#86648 = CARTESIAN_POINT ( 'NONE',  ( 15.39793903038207823, 9.389686005666812108, -49.17284350635129897 ) ) ;
#86650 = CARTESIAN_POINT ( 'NONE',  ( 21.12400222705963415, 67.22148809293538818, -191.2731074845244166 ) ) ;
#86651 = EDGE_LOOP ( 'NONE', ( #38732, #181746, #129200, #206444, #120782, #175373, #59722, #103508, #13259, #38666, #215743, #46498 ) ) ;
#86652 = AXIS2_PLACEMENT_3D ( 'NONE', #166972, #168263, #160849 ) ;
#86653 = VERTEX_POINT ( 'NONE', #53097 ) ;
#86654 = EDGE_CURVE ( 'NONE', #52, #189967, #130528, .T. ) ;
#86655 = DIRECTION ( 'NONE',  ( 0.5735764363510460484, 0.8191520442889919096, 0.000000000000000000 ) ) ;
#86656 = DIRECTION ( 'NONE',  ( 0.000000000000000000, 0.9999176327611370985, -0.01283462868041289687 ) ) ;
#86657 =( BOUNDED_SURFACE ( )  B_SPLINE_SURFACE ( 3, 2, ( 
 ( #124021, #122749, #139698 ),
 ( #40667, #143570, #4054 ),
 ( #58869, #160599, #219244 ),
 ( #2758, #120197, #101849 ),
 ( #82281, #180146, #199718 ),
 ( #21086, #161877, #83562 ) ),
 .UNSPECIFIED., .F., .F., .F. ) 
 B_SPLINE_SURFACE_WITH_KNOTS ( ( 4, 2, 4 ),
 ( 3, 3 ),
 ( 0.0001792624049599542612, 0.0003686986002124735670, 0.0005581347954649928727 ),
 ( 0.000000000000000000, 1.000000000000000000 ),
 .UNSPECIFIED. ) 
 GEOMETRIC_REPRESENTATION_ITEM ( )  RATIONAL_B_SPLINE_SURFACE ( (
 ( 1.000000000000000000, 0.9238795325112985068, 1.000000000000000000),
 ( 1.000000000000000000, 0.9229318695241288673, 1.000000000000000000),
 ( 1.000000000000000000, 0.8926288119226872819, 1.000000000000000000),
 ( 1.000000000000000000, 0.8123777807275367469, 1.000000000000000000),
 ( 1.000000000000000000, 0.7629087100928569898, 1.000000000000000000),
 ( 1.000000000000000000, 0.7071067811865475727, 1.000000000000000000) ) ) 
 REPRESENTATION_ITEM ( '' )  SURFACE ( )  );
#86658 = DIRECTION ( 'NONE',  ( 1.000000000000000000, 0.000000000000000000, 0.000000000000000000 ) ) ;
#86659 = EDGE_CURVE ( 'NONE', #155996, #11174, #72285, .T. ) ;
#86660 = CARTESIAN_POINT ( 'NONE',  ( -18.50000000000000000, 64.35000000001198828, -115.1731074845243796 ) ) ;
#86661 = DIRECTION ( 'NONE',  ( 0.000000000000000000, 0.000000000000000000, 1.000000000000000000 ) ) ;
#86662 = DIRECTION ( 'NONE',  ( 0.000000000000000000, -0.9651348961777157509, 0.2617529984165031243 ) ) ;
#86663 = EDGE_LOOP ( 'NONE', ( #250544, #50284, #117290 ) ) ;
#86664 = DIRECTION ( 'NONE',  ( -0.000000000000000000, 0.000000000000000000, -1.000000000000000000 ) ) ;
#86665 = CARTESIAN_POINT ( 'NONE',  ( -22.50000000000000000, -3.140208063160686791, -228.2318569537739847 ) ) ;
#86667 = CARTESIAN_POINT ( 'NONE',  ( -18.59999999999999787, 11.75000000001115197, -88.75000000000004263 ) ) ;
#86666 = PRODUCT_DEFINITION ( 'UNKNOWN', '', #182049, #3538 ) ;
#86668 = DIRECTION ( 'NONE',  ( 1.000000000000000000, 0.000000000000000000, 0.000000000000000000 ) ) ;
#86669 = CIRCLE ( 'NONE', #195061, 0.1000000000000028644 ) ;
#86670 = EDGE_LOOP ( 'NONE', ( #125520, #112091, #211763, #128032 ) ) ;
#86671 = CARTESIAN_POINT ( 'NONE',  ( 18.55807992284871588, 10.32898536001801659, -106.0826683222764899 ) ) ;
#86672 = ORIENTED_EDGE ( 'NONE', *, *, #252273, .T. ) ;
#86673 = CARTESIAN_POINT ( 'NONE',  ( 12.93225390519044637, 9.417651958852159666, -115.8587873924405045 ) ) ;
#86674 = AXIS2_PLACEMENT_3D ( 'NONE', #159522, #241612, #257267 ) ;
#86675 = ORIENTED_EDGE ( 'NONE', *, *, #201292, .T. ) ;
#86676 = VECTOR ( 'NONE', #68952, 1000.000000000000000 ) ;
#86677 =( BOUNDED_CURVE ( )  B_SPLINE_CURVE ( 3, ( #14298, #251597, #232054, #18118 ),
 .UNSPECIFIED., .F., .F. ) 
 B_SPLINE_CURVE_WITH_KNOTS ( ( 4, 4 ),
 ( 1.570796326794896558, 3.141592653589793116 ),
 .UNSPECIFIED. ) 
 CURVE ( )  GEOMETRIC_REPRESENTATION_ITEM ( )  RATIONAL_B_SPLINE_CURVE ( ( 1.000000000000000000, 0.8047378541243649375, 0.8047378541243649375, 1.000000000000000000 ) ) 
 REPRESENTATION_ITEM ( '' )  );
#86678 = CARTESIAN_POINT ( 'NONE',  ( -23.15000000000000213, 1.115626384983466744E-11, -98.40000000000004832 ) ) ;
#86679 = CARTESIAN_POINT ( 'NONE',  ( 18.49999999999999645, 74.36282728704118483, -57.94095411905231430 ) ) ;
#86680 = EDGE_CURVE ( 'NONE', #60900, #147515, #197163, .T. ) ;
#86681 = VERTEX_POINT ( 'NONE', #37412 ) ;
#86682 = ORIENTED_EDGE ( 'NONE', *, *, #194129, .F. ) ;
#86684 = VERTEX_POINT ( 'NONE', #196456 ) ;
#86683 = CARTESIAN_POINT ( 'NONE',  ( 23.14999999999999858, 76.00000000001213607, -136.5231074845242745 ) ) ;
#86685 = EDGE_CURVE ( 'NONE', #125866, #83776, #175637, .T. ) ;
#86686 = DIRECTION ( 'NONE',  ( 0.000000000000000000, 0.000000000000000000, 1.000000000000000000 ) ) ;
#86687 = ORIENTED_EDGE ( 'NONE', *, *, #213467, .F. ) ;
#86688 = EDGE_CURVE ( 'NONE', #29064, #11395, #209653, .T. ) ;
#86689 = AXIS2_PLACEMENT_3D ( 'NONE', #242746, #4143, #122834 ) ;
#86690 = DIRECTION ( 'NONE',  ( -1.000000000000000000, -0.000000000000000000, -0.000000000000000000 ) ) ;
#86691 = DIRECTION ( 'NONE',  ( 3.697785493223492838E-32, -0.2128009952263605065, 0.9770955615653315052 ) ) ;
#86692 = EDGE_LOOP ( 'NONE', ( #120829, #122108, #334, #49214, #225896, #131006 ) ) ;
#86693 = FACE_OUTER_BOUND ( 'NONE', #33108, .T. ) ;
#86694 = PLANE ( 'NONE',  #86589 ) ;
#86695 = AXIS2_PLACEMENT_3D ( 'NONE', #160783, #98169, #1659 ) ;
#86696 = VECTOR ( 'NONE', #154210, 1000.000000000000000 ) ;
#86698 = ORIENTED_EDGE ( 'NONE', *, *, #195095, .T. ) ;
#86697 = AXIS2_PLACEMENT_3D ( 'NONE', #4514, #237988, #198871 ) ;
#86699 =( BOUNDED_CURVE ( )  B_SPLINE_CURVE ( 3, ( #61442, #200948, #144808, #159275 ),
 .UNSPECIFIED., .F., .F. ) 
 B_SPLINE_CURVE_WITH_KNOTS ( ( 4, 4 ),
 ( 2.589852378279005496, 2.850972632318389710 ),
 .UNSPECIFIED. ) 
 CURVE ( )  GEOMETRIC_REPRESENTATION_ITEM ( )  RATIONAL_B_SPLINE_CURVE ( ( 1.000000000000000000, 0.9943260843901261525, 0.9943260843901261525, 1.000000000000000000 ) ) 
 REPRESENTATION_ITEM ( '' )  );
#86701 = CARTESIAN_POINT ( 'NONE',  ( 19.99999999999998934, 61.47936603916259202, -212.1738987416902376 ) ) ;
#86700 = CIRCLE ( 'NONE', #232508, 0.09999999999999939493 ) ;
#86702 = CARTESIAN_POINT ( 'NONE',  ( -22.59999999999999787, 76.00000000001165290, -69.52310748452431710 ) ) ;
#86704 = VERTEX_POINT ( 'NONE', #154804 ) ;
#86703 = CARTESIAN_POINT ( 'NONE',  ( -16.85312841634287651, 9.913606177331356406, -46.39717313329252590 ) ) ;
#86706 = CIRCLE ( 'NONE', #232523, 0.1999999999999938494 ) ;
#86705 = CARTESIAN_POINT ( 'NONE',  ( -21.05000000000000071, 46.45388641681647357, -243.1520440498138385 ) ) ;
#86707 = FACE_OUTER_BOUND ( 'NONE', #31142, .T. ) ;
#86709 = EDGE_CURVE ( 'NONE', #200535, #197481, #210896, .T. ) ;
#86708 = CARTESIAN_POINT ( 'NONE',  ( 20.94999999999999929, 4.850467289730772791, -179.5342674090016430 ) ) ;
#86711 = CARTESIAN_POINT ( 'NONE',  ( 23.25000000000000355, -22.45632476061176774, -40.29389844773160689 ) ) ;
#86710 = CARTESIAN_POINT ( 'NONE',  ( -16.98495255085919453, 10.00556436600593280, -154.8653827937795029 ) ) ;
#86712 = CARTESIAN_POINT ( 'NONE',  ( -20.88420186297724257, 65.66974365629718591, -164.4360145562605453 ) ) ;
#86713 = CARTESIAN_POINT ( 'NONE',  ( 23.14999999999999858, 53.66153320161009788, -235.9075159595686841 ) ) ;
#86714 = CIRCLE ( 'NONE', #132537, 0.09999999999999939493 ) ;
#86715 = CARTESIAN_POINT ( 'NONE',  ( -23.15000000000000213, 66.45861426436469799, -222.8494355952551018 ) ) ;
#86716 = CARTESIAN_POINT ( 'NONE',  ( 23.15000000000000213, -11.64999999998883595, -63.89999999999999858 ) ) ;
#86717 = CIRCLE ( 'NONE', #231954, 0.1000000000000028644 ) ;
#86718 = ORIENTED_EDGE ( 'NONE', *, *, #148157, .T. ) ;
#86719 = AXIS2_PLACEMENT_3D ( 'NONE', #91593, #74640, #250646 ) ;
#86720 = TOROIDAL_SURFACE ( 'NONE', #165886, 0.2000000000000000111, 0.1000000000000000056 ) ;
#86721 = AXIS2_PLACEMENT_3D ( 'NONE', #70465, #95122, #174712 ) ;
#86722 = CIRCLE ( 'NONE', #95134, 0.1000000000000105804 ) ;
#86723 = VERTEX_POINT ( 'NONE', #195215 ) ;
#86724 = EDGE_CURVE ( 'NONE', #111193, #235470, #231757, .T. ) ;
#86725 = DIRECTION ( 'NONE',  ( 1.000000000000000000, 0.000000000000000000, 0.000000000000000000 ) ) ;
#86726 = EDGE_LOOP ( 'NONE', ( #229614, #226558, #8822, #232597, #148053, #165167, #102882, #185174, #122730, #52478 ) ) ;
#86727 = AXIS2_PLACEMENT_3D ( 'NONE', #94257, #74748, #254597 ) ;
#86728 = CARTESIAN_POINT ( 'NONE',  ( -21.05000000000000071, 64.40000000001219860, -143.4513107147999449 ) ) ;
#86729 = EDGE_CURVE ( 'NONE', #16521, #241094, #213456, .T. ) ;
#86730 = ORIENTED_EDGE ( 'NONE', *, *, #110135, .T. ) ;
#86731 = CARTESIAN_POINT ( 'NONE',  ( 18.59999999999999076, 64.25000000001196554, -111.6731074845243796 ) ) ;
#86732 = LINE ( 'NONE', #139336, #133157 ) ;
#86733 = PRODUCT ( 'Snap Open Cable Crossbars 15', 'Snap Open Cable Crossbars 15', '', ( #252986 ) ) ;
#86734 = ORIENTED_EDGE ( 'NONE', *, *, #241913, .F. ) ;
#86735 = CARTESIAN_POINT ( 'NONE',  ( -23.25000000000000000, 11.75000000001115552, -21.75000000000000355 ) ) ;
#86736 = VERTEX_POINT ( 'NONE', #116931 ) ;
#86737 = AXIS2_PLACEMENT_3D ( 'NONE', #81832, #118452, #161434 ) ;
#86738 = CIRCLE ( 'NONE', #128294, 0.2000000000000057288 ) ;
#86739 = ORIENTED_EDGE ( 'NONE', *, *, #178282, .T. ) ;
#86740 = ADVANCED_FACE ( 'NONE', ( #212197 ), #33593, .T. ) ;
#86741 = CARTESIAN_POINT ( 'NONE',  ( 18.59999999999999076, 74.16465844978765176, -124.9679561919613207 ) ) ;
#86742 = LINE ( 'NONE', #166340, #34437 ) ;
#86745 = ADVANCED_FACE ( 'NONE', ( #13991 ), #156091, .T. ) ;
#86744 = ORIENTED_EDGE ( 'NONE', *, *, #78888, .T. ) ;
#86743 = CARTESIAN_POINT ( 'NONE',  ( 21.13461538461538680, 67.11458296203711882, -57.27310748452438816 ) ) ;
#86746 = CARTESIAN_POINT ( 'NONE',  ( 20.94983749550516450, 65.70233904877009934, -97.54874109119680270 ) ) ;
#86748 = ORIENTED_EDGE ( 'NONE', *, *, #114301, .T. ) ;
#86747 = DIRECTION ( 'NONE',  ( -3.890533409366484652E-14, -0.1298341882520124002, -0.9915357197604841577 ) ) ;
#86749 = DIRECTION ( 'NONE',  ( -1.836970198721029934E-16, 1.000000000000000000, 0.000000000000000000 ) ) ;
#86750 = DIRECTION ( 'NONE',  ( -1.000000000000000000, 0.000000000000000000, -0.000000000000000000 ) ) ;
#86752 = ORIENTED_EDGE ( 'NONE', *, *, #64122, .F. ) ;
#86751 = FACE_OUTER_BOUND ( 'NONE', #207645, .T. ) ;
#86753 = TOROIDAL_SURFACE ( 'NONE', #24258, 0.4000000000000009104, 0.1000000000000000056 ) ;
#86754 = CARTESIAN_POINT ( 'NONE',  ( 18.49999999999999289, 10.29270135741298731, -172.9573618871519614 ) ) ;
#86755 = DIRECTION ( 'NONE',  ( -0.000000000000000000, -1.000000000000000000, 6.308085367188393199E-16 ) ) ;
#86756 = AXIS2_PLACEMENT_3D ( 'NONE', #18791, #98296, #239137 ) ;
#86757 = DIRECTION ( 'NONE',  ( -1.000000000000000000, 0.000000000000000000, 0.000000000000000000 ) ) ;
#86759 = CARTESIAN_POINT ( 'NONE',  ( 20.94999999999999929, 67.23127455305835554, -235.8551265064784559 ) ) ;
#86758 = DIRECTION ( 'NONE',  ( -1.000000000000000000, 0.000000000000000000, 0.000000000000000000 ) ) ;
#86760 = DIRECTION ( 'NONE',  ( -1.000000000000000000, -0.000000000000000000, 0.000000000000000000 ) ) ;
#86761 = CARTESIAN_POINT ( 'NONE',  ( 18.44208962362762705, 85.55234049692037956, -163.1809344290608976 ) ) ;
#86762 = EDGE_CURVE ( 'NONE', #207164, #100804, #201256, .T. ) ;
#86763 = CARTESIAN_POINT ( 'NONE',  ( 21.05000000000002203, 1.363275264940671860, -230.6442496871288768 ) ) ;
#86764 = CARTESIAN_POINT ( 'NONE',  ( -23.39999999999994529, 74.16448838626247664, -47.52760213295649550 ) ) ;
#86765 = EDGE_CURVE ( 'NONE', #198700, #125678, #51385, .T. ) ;
#86766 = ORIENTED_EDGE ( 'NONE', *, *, #78976, .T. ) ;
#86767 = EDGE_LOOP ( 'NONE', ( #144970, #172197, #240699, #1909 ) ) ;
#86769 = VERTEX_POINT ( 'NONE', #173104 ) ;
#86768 = AXIS2_PLACEMENT_3D ( 'NONE', #30045, #52129, #53430 ) ;
#86770 = DIRECTION ( 'NONE',  ( 0.000000000000000000, 0.4999999999999348299, -0.8660254037844762331 ) ) ;
#86771 = ORIENTED_EDGE ( 'NONE', *, *, #45037, .F. ) ;
#86772 = DIRECTION ( 'NONE',  ( -1.000000000000000000, 7.492892343619937423E-30, -1.073024830501117725E-15 ) ) ;
#86773 = EDGE_LOOP ( 'NONE', ( #136959, #256057, #146965, #133662 ) ) ;
#86774 = EDGE_CURVE ( 'NONE', #25427, #35607, #193089, .T. ) ;
#86775 = CARTESIAN_POINT ( 'NONE',  ( -18.43569575749025446, -7.817436562502987130, -209.8389866834998827 ) ) ;
#86776 = CARTESIAN_POINT ( 'NONE',  ( -16.94107738177415712, 10.01423928514777728, -113.0500000000000398 ) ) ;
#86777 = VECTOR ( 'NONE', #124143, 1000.000000000000000 ) ;
#86778 = AXIS2_PLACEMENT_3D ( 'NONE', #47055, #164463, #142311 ) ;
#86779 = ADVANCED_FACE ( 'NONE', ( #73990 ), #153543, .F. ) ;
#86780 = ORIENTED_EDGE ( 'NONE', *, *, #190359, .T. ) ;
#86781 = AXIS2_PLACEMENT_3D ( 'NONE', #51376, #189648, #249630 ) ;
#86782 = CARTESIAN_POINT ( 'NONE',  ( 12.84435279558020504, 9.410708747058237122, -152.0692084058441367 ) ) ;
#86783 = EDGE_CURVE ( 'NONE', #55133, #213315, #109673, .T. ) ;
#86784 = VECTOR ( 'NONE', #92483, 1000.000000000000000 ) ;
#86785 = ORIENTED_EDGE ( 'NONE', *, *, #56070, .T. ) ;
#86786 = EDGE_LOOP ( 'NONE', ( #62309, #130754 ) ) ;
#86787 = EDGE_LOOP ( 'NONE', ( #42297, #204380 ) ) ;
#86788 = CARTESIAN_POINT ( 'NONE',  ( -20.54999999999999716, 85.40000000001252545, -179.9170766071767389 ) ) ;
#86789 = CARTESIAN_POINT ( 'NONE',  ( -23.15000000000000213, 85.00000000001149658, -45.91707660717669626 ) ) ;
#86790 = CARTESIAN_POINT ( 'NONE',  ( 18.54999999999999716, 9.950000000011153034, -180.1499999999999204 ) ) ;
#86791 = LINE ( 'NONE', #64676, #3029 ) ;
#86792 = CARTESIAN_POINT ( 'NONE',  ( -21.05000000000000071, 78.47509609352879068, -238.9045489380306435 ) ) ;
#86793 = LINE ( 'NONE', #15981, #251115 ) ;
#86795 = FACE_OUTER_BOUND ( 'NONE', #194797, .T. ) ;
#86794 = CARTESIAN_POINT ( 'NONE',  ( -16.27683809663750480, 19.69766786220170829, -229.8585047820796490 ) ) ;
#86796 = DIRECTION ( 'NONE',  ( 0.000000000000000000, 1.000000000000000000, 0.000000000000000000 ) ) ;
#86798 = VERTEX_POINT ( 'NONE', #119512 ) ;
#86797 = CARTESIAN_POINT ( 'NONE',  ( -18.40000000000000213, 64.52683809664982562, -157.4145288407617613 ) ) ;
#86800 = DIRECTION ( 'NONE',  ( 0.000000000000000000, -0.9126074666063545004, -0.4088369013363783999 ) ) ;
#86799 = DIRECTION ( 'NONE',  ( 0.000000000000000000, 1.000000000000000000, 0.000000000000000000 ) ) ;
#86801 = EDGE_CURVE ( 'NONE', #28426, #194531, #93109, .T. ) ;
#86802 = DIRECTION ( 'NONE',  ( -1.000000000000000000, -0.000000000000000000, -0.000000000000000000 ) ) ;
#86803 = EDGE_CURVE ( 'NONE', #442, #88307, #226364, .T. ) ;
#86804 = ORIENTED_EDGE ( 'NONE', *, *, #8418, .T. ) ;
#86805 = DIRECTION ( 'NONE',  ( 0.000000000000000000, -6.853228547068871147E-15, 1.000000000000000000 ) ) ;
#86806 = AXIS2_PLACEMENT_3D ( 'NONE', #227719, #127348, #225139 ) ;
#86807 = CARTESIAN_POINT ( 'NONE',  ( 22.59999985501178799, 64.25013020700896504, -103.0887061543238303 ) ) ;
#86808 = CARTESIAN_POINT ( 'NONE',  ( 20.04142135623731136, 64.25000000001148237, -44.87310748452440379 ) ) ;
#86809 = VERTEX_POINT ( 'NONE', #199038 ) ;
#86810 = LINE ( 'NONE', #217653, #249425 ) ;
#86811 = FACE_OUTER_BOUND ( 'NONE', #100284, .T. ) ;
#86812 = DIRECTION ( 'NONE',  ( 0.000000000000000000, -0.9908441862701782288, 0.1350103645450542456 ) ) ;
#86813 = EDGE_LOOP ( 'NONE', ( #146921, #105022, #181129, #90215 ) ) ;
#86814 = EDGE_LOOP ( 'NONE', ( #130008, #66456, #180484, #200668 ) ) ;
#86815 = DIRECTION ( 'NONE',  ( 1.000000000000000000, -0.000000000000000000, 0.000000000000000000 ) ) ;
#86816 = VERTEX_POINT ( 'NONE', #42517 ) ;
#86817 = CARTESIAN_POINT ( 'NONE',  ( 20.94999999999999929, 0.000000000000000000, -33.50000000000000000 ) ) ;
#86818 = CARTESIAN_POINT ( 'NONE',  ( -18.59999994787167310, -9.523637689750707125, -174.3824495347721779 ) ) ;
#86819 = DIRECTION ( 'NONE',  ( 1.000000000000000000, 0.000000000000000000, 0.000000000000000000 ) ) ;
#86820 = ORIENTED_EDGE ( 'NONE', *, *, #90882, .T. ) ;
#86821 = DIRECTION ( 'NONE',  ( 0.000000000000000000, -1.000000000000000000, 0.000000000000000000 ) ) ;
#86822 = DIRECTION ( 'NONE',  ( 0.000000000000000000, 0.000000000000000000, -1.000000000000000000 ) ) ;
#86823 = CARTESIAN_POINT ( 'NONE',  ( 18.52928932188133970, 10.27928932189250055, -192.1499999999999488 ) ) ;
#86824 = DIRECTION ( 'NONE',  ( 0.000000000000000000, -7.056502275159890832E-15, 1.000000000000000000 ) ) ;
#86825 = TOROIDAL_SURFACE ( 'NONE', #45153, 0.2000000000000000111, 0.1000000000000000056 ) ;
#86826 = AXIS2_PLACEMENT_3D ( 'NONE', #5380, #26270, #164503 ) ;
#86827 = EDGE_CURVE ( 'NONE', #18395, #184009, #255375, .T. ) ;
#86828 = ORIENTED_EDGE ( 'NONE', *, *, #202515, .T. ) ;
#86829 = CARTESIAN_POINT ( 'NONE',  ( -20.94999999999999929, -11.74999999998884448, -164.4000000000000057 ) ) ;
#86831 = VERTEX_POINT ( 'NONE', #63356 ) ;
#86830 = FACE_OUTER_BOUND ( 'NONE', #20324, .T. ) ;
#86832 = AXIS2_PLACEMENT_3D ( 'NONE', #229878, #189472, #31706 ) ;
#86833 = CARTESIAN_POINT ( 'NONE',  ( 23.40000000000005542, 74.16448838626247664, -47.52760213295649550 ) ) ;
#86834 = DIRECTION ( 'NONE',  ( -1.000000000000000000, 3.151514657663852580E-16, -8.547182517843351137E-17 ) ) ;
#86835 = CARTESIAN_POINT ( 'NONE',  ( -20.54999999999999716, -6.488386256076843495, -212.2361678873109838 ) ) ;
#86836 = CARTESIAN_POINT ( 'NONE',  ( 18.49999999999999645, 62.13039908340535078, -248.0610840288475174 ) ) ;
#86837 = FACE_OUTER_BOUND ( 'NONE', #123631, .T. ) ;
#86838 = CARTESIAN_POINT ( 'NONE',  ( -23.25000000000000000, 76.00000000001213607, -136.5231074845242745 ) ) ;
#86839 = CARTESIAN_POINT ( 'NONE',  ( 21.00000000000000000, 61.02768354592784306, -221.4801322937404393 ) ) ;
#86840 = ORIENTED_EDGE ( 'NONE', *, *, #217978, .T. ) ;
#86841 = DIRECTION ( 'NONE',  ( -1.000000000000000000, -0.000000000000000000, 0.000000000000000000 ) ) ;
#86842 = CARTESIAN_POINT ( 'NONE',  ( 21.14999999999999503, 11.38316329224760892, -198.5208684056144079 ) ) ;
#86843 = AXIS2_PLACEMENT_3D ( 'NONE', #38287, #117811, #158271 ) ;
#86844 = AXIS2_PLACEMENT_3D ( 'NONE', #251644, #91294, #52142 ) ;
#86845 = DIRECTION ( 'NONE',  ( 0.000000000000000000, 0.2617529984165152257, 0.9651348961777124202 ) ) ;
#86846 = AXIS2_PLACEMENT_3D ( 'NONE', #234780, #50976, #14477 ) ;
#86847 = EDGE_CURVE ( 'NONE', #171323, #59375, #19107, .T. ) ;
#86848 = CARTESIAN_POINT ( 'NONE',  ( 22.60000000000000142, 76.00000000001267608, -203.5231074845243597 ) ) ;
#86849 = CYLINDRICAL_SURFACE ( 'NONE', #144907, 0.1000000000000028644 ) ;
#86850 = CIRCLE ( 'NONE', #182578, 0.09999999999999123479 ) ;
#86851 = ORIENTED_EDGE ( 'NONE', *, *, #71346, .T. ) ;
#86852 = VERTEX_POINT ( 'NONE', #62097 ) ;
#86853 = CARTESIAN_POINT ( 'NONE',  ( -18.59999999999999787, 77.26327546522934142, -128.6212428177779543 ) ) ;
#86854 = DIRECTION ( 'NONE',  ( 1.000000000000000000, 0.000000000000000000, 0.000000000000000000 ) ) ;
#86855 = CARTESIAN_POINT ( 'NONE',  ( 18.49999999999999645, 77.36242903720497566, -61.63422623660309796 ) ) ;
#86856 = LINE ( 'NONE', #184686, #5850 ) ;
#86857 = DIRECTION ( 'NONE',  ( 1.000000000000000000, 0.000000000000000000, 0.000000000000000000 ) ) ;
#86858 = CARTESIAN_POINT ( 'NONE',  ( -18.59999999999999787, 77.16412189325286874, -61.60825939895269698 ) ) ;
#86859 = CARTESIAN_POINT ( 'NONE',  ( -21.05000000000000071, -1.249999999999999334, -8.000000000000000000 ) ) ;
#86860 = AXIS2_PLACEMENT_3D ( 'NONE', #47668, #12438, #69844 ) ;
#86861 = AXIS2_PLACEMENT_3D ( 'NONE', #19705, #199638, #80928 ) ;
#86862 = VECTOR ( 'NONE', #167745, 1000.000000000000227 ) ;
#86863 = ORIENTED_EDGE ( 'NONE', *, *, #245568, .F. ) ;
#86864 = CARTESIAN_POINT ( 'NONE',  ( -18.54118089899631983, 85.46353763185970820, -62.47452988665613560 ) ) ;
#86865 = EDGE_LOOP ( 'NONE', ( #66928, #19618, #35739, #162552 ) ) ;
#86866 = LINE ( 'NONE', #146844, #130739 ) ;
#86867 = DIRECTION ( 'NONE',  ( -0.000000000000000000, -0.2128009952263603677, 0.9770955615653313941 ) ) ;
#86868 = VECTOR ( 'NONE', #12713, 999.9999999999998863 ) ;
#86869 = CARTESIAN_POINT ( 'NONE',  ( 20.94999999999999574, 1.250000000011155299, -141.9000000000000341 ) ) ;
#86870 = DIRECTION ( 'NONE',  ( 1.000000000000000000, 0.000000000000000000, 0.000000000000000000 ) ) ;
#86871 = DIRECTION ( 'NONE',  ( 1.000000000000000000, -7.304098846218133681E-16, 0.000000000000000000 ) ) ;
#86872 = DIRECTION ( 'NONE',  ( 0.000000000000000000, 0.000000000000000000, 1.000000000000000000 ) ) ;
#86873 = DIRECTION ( 'NONE',  ( 0.000000000000000000, -5.551115123125777653E-14, 1.000000000000000000 ) ) ;
#86874 = VERTEX_POINT ( 'NONE', #197745 ) ;
#86875 = CARTESIAN_POINT ( 'NONE',  ( -16.93255653858138388, 22.94068984415941159, -230.8600761695373080 ) ) ;
#86876 = DIRECTION ( 'NONE',  ( 1.000000000000000000, 1.734723475976817507E-14, 0.000000000000000000 ) ) ;
#86878 = EDGE_CURVE ( 'NONE', #65312, #69180, #188800, .T. ) ;
#86877 = FACE_OUTER_BOUND ( 'NONE', #221607, .T. ) ;
#86879 = CARTESIAN_POINT ( 'NONE',  ( 18.46905048506369695, -9.473744257382394451, -40.17598629225540208 ) ) ;
#86880 = CIRCLE ( 'NONE', #57286, 0.09999999999999939493 ) ;
#86881 = CIRCLE ( 'NONE', #70376, 4.150000000000001243 ) ;
#86882 = CIRCLE ( 'NONE', #16203, 0.09999999999999939493 ) ;
#86883 = CARTESIAN_POINT ( 'NONE',  ( 18.60000000000000497, 85.52394631232958488, -96.14107948918599789 ) ) ;
#86884 = DIRECTION ( 'NONE',  ( 0.000000000000000000, -0.5954378521545836689, -0.8034013718071036925 ) ) ;
#86885 = AXIS2_PLACEMENT_3D ( 'NONE', #10256, #187618, #228010 ) ;
#86886 = VERTEX_POINT ( 'NONE', #161200 ) ;
#86887 = CARTESIAN_POINT ( 'NONE',  ( 23.14999999999998437, 76.00000000001165290, -69.52310748452431710 ) ) ;
#86889 = ADVANCED_FACE ( 'NONE', ( #79055 ), #142977, .T. ) ;
#86888 = CARTESIAN_POINT ( 'NONE',  ( -20.94999999999999929, 68.96868720525648655, -65.91395654629705803 ) ) ;
#86890 = EDGE_LOOP ( 'NONE', ( #237165, #94800, #44100, #86638 ) ) ;
#86892 = EDGE_CURVE ( 'NONE', #171186, #41545, #30599, .T. ) ;
#86891 = DIRECTION ( 'NONE',  ( 1.000000000000000000, 0.000000000000000000, 0.000000000000000000 ) ) ;
#86893 = CARTESIAN_POINT ( 'NONE',  ( 21.06277459767474980, 11.26665768069844553, -211.0363194868302799 ) ) ;
#86894 = CIRCLE ( 'NONE', #75055, 0.09999999999999939493 ) ;
#86895 = ORIENTED_EDGE ( 'NONE', *, *, #201011, .F. ) ;
#86896 = CARTESIAN_POINT ( 'NONE',  ( 18.41815437325346849, -9.498709853130273828, -174.1039458388020194 ) ) ;
#86897 = DIRECTION ( 'NONE',  ( -4.336808689942017736E-16, 0.000000000000000000, -1.000000000000000000 ) ) ;
#86899 = EDGE_CURVE ( 'NONE', #138896, #243619, #151404, .T. ) ;
#86898 = AXIS2_PLACEMENT_3D ( 'NONE', #141760, #204298, #240884 ) ;
#86900 = ORIENTED_EDGE ( 'NONE', *, *, #84739, .T. ) ;
#86901 = CIRCLE ( 'NONE', #11952, 0.1000000000000028644 ) ;
#86902 = AXIS2_PLACEMENT_3D ( 'NONE', #135515, #215070, #53432 ) ;
#86903 = AXIS2_PLACEMENT_3D ( 'NONE', #132964, #149964, #228206 ) ;
#86904 = CARTESIAN_POINT ( 'NONE',  ( -21.05000000000000071, 75.90220970870321082, -109.2809220950004203 ) ) ;
#86905 = EDGE_LOOP ( 'NONE', ( #231850, #11359, #177184, #222698 ) ) ;
#86906 = AXIS2_PLACEMENT_3D ( 'NONE', #116580, #59130, #96967 ) ;
#86908 = ADVANCED_FACE ( 'NONE', ( #24268 ), #168368, .T. ) ;
#86907 = CARTESIAN_POINT ( 'NONE',  ( -20.64999999999999858, 7.128833340093095217, -233.7327013124392749 ) ) ;
#86909 = CARTESIAN_POINT ( 'NONE',  ( -21.05000000000000071, 1.250000000011155299, -108.5000000000000426 ) ) ;
#86910 = CARTESIAN_POINT ( 'NONE',  ( 22.10000000000000142, -11.65000000000000036, 32.89999999999999858 ) ) ;
#86912 = UNCERTAINTY_MEASURE_WITH_UNIT (LENGTH_MEASURE( 1.000000000000000082E-05 ), #166978, 'distance_accuracy_value', 'NONE');
#86911 = DIRECTION ( 'NONE',  ( -1.000000000000000000, -0.000000000000000000, -0.000000000000000000 ) ) ;
#86913 = DIRECTION ( 'NONE',  ( -1.000000000000000000, 0.000000000000000000, 0.000000000000000000 ) ) ;
#86914 = CARTESIAN_POINT ( 'NONE',  ( -21.05000000000000071, 36.65892442174472876, -249.5511627012454596 ) ) ;
#86915 = LINE ( 'NONE', #167794, #101366 ) ;
#86917 = ORIENTED_EDGE ( 'NONE', *, *, #53881, .T. ) ;
#86916 = CARTESIAN_POINT ( 'NONE',  ( 20.94999999999999574, 1.835341550235567887, -112.0551512925630249 ) ) ;
#86918 = ORIENTED_EDGE ( 'NONE', *, *, #173568, .T. ) ;
#86920 = CARTESIAN_POINT ( 'NONE',  ( -15.57281606413133979, 9.370655051134635372, -84.52582325598092439 ) ) ;
#86919 = DIRECTION ( 'NONE',  ( 0.000000000000000000, 0.000000000000000000, 1.000000000000000000 ) ) ;
#86922 = EDGE_LOOP ( 'NONE', ( #212496, #155563, #103060, #159980 ) ) ;
#86921 = CARTESIAN_POINT ( 'NONE',  ( 23.14999999999999147, 76.00000000001237765, -170.0231074845243597 ) ) ;
#86923 = VERTEX_POINT ( 'NONE', #140327 ) ;
#86924 = PLANE ( 'NONE',  #129016 ) ;
#86925 = AXIS2_PLACEMENT_3D ( 'NONE', #4114, #82339, #2820 ) ;
#86926 = CARTESIAN_POINT ( 'NONE',  ( 20.95512820512820440, 67.12384868372375024, -90.87310748452436826 ) ) ;
#86927 = AXIS2_PLACEMENT_3D ( 'NONE', #166848, #67707, #128977 ) ;
#86928 = LINE ( 'NONE', #21855, #150736 ) ;
#86929 = CARTESIAN_POINT ( 'NONE',  ( 20.94999999999999929, -9.499999999988844479, -157.6060308773475640 ) ) ;
#86930 = CARTESIAN_POINT ( 'NONE',  ( -20.64999999999999858, 71.65000000001259650, -191.1731074845243654 ) ) ;
#86931 = AXIS2_PLACEMENT_3D ( 'NONE', #17525, #61810, #80043 ) ;
#86932 = DIRECTION ( 'NONE',  ( 1.000000000000000000, -0.000000000000000000, -0.000000000000000000 ) ) ;
#86933 = VERTEX_POINT ( 'NONE', #3379 ) ;
#86934 = ORIENTED_EDGE ( 'NONE', *, *, #92875, .T. ) ;
#86935 = CARTESIAN_POINT ( 'NONE',  ( -21.05000000000000071, 68.11887992016828264, -227.8068560890360175 ) ) ;
#86936 = ORIENTED_EDGE ( 'NONE', *, *, #163176, .T. ) ;
#86937 = CARTESIAN_POINT ( 'NONE',  ( -21.05000000000000071, 70.10000000001235776, -159.8040077198679683 ) ) ;
#86938 = EDGE_LOOP ( 'NONE', ( #173091, #200245, #108424, #117501 ) ) ;
#86939 = CARTESIAN_POINT ( 'NONE',  ( -23.25000000000000000, 82.09643798151613225, -215.4278993322501208 ) ) ;
#86940 = CIRCLE ( 'NONE', #49564, 0.5000000000000004441 ) ;
#86941 = EDGE_CURVE ( 'NONE', #193742, #104543, #26690, .T. ) ;
#86942 = DIRECTION ( 'NONE',  ( 0.000000000000000000, 1.000000000000000000, 1.387778780781444413E-14 ) ) ;
#86943 = CARTESIAN_POINT ( 'NONE',  ( -23.25000000000000000, 77.16412189325305349, -95.10825939895268277 ) ) ;
#86944 = CARTESIAN_POINT ( 'NONE',  ( -21.08376601933334271, 75.93622398908284765, -209.8650547558000881 ) ) ;
#86945 = ORIENTED_EDGE ( 'NONE', *, *, #186548, .T. ) ;
#86947 = ADVANCED_FACE ( 'NONE', ( #157376 ), #217289, .T. ) ;
#86946 = CARTESIAN_POINT ( 'NONE',  ( -20.64999999999999858, 68.85000000001228670, -157.7731074845244166 ) ) ;
#86948 = VERTEX_POINT ( 'NONE', #58215 ) ;
#86949 = DIRECTION ( 'NONE',  ( -0.7071067811865460184, -0.6824534298470606997, 0.1850873201761399356 ) ) ;
#86950 = AXIS2_PLACEMENT_3D ( 'NONE', #63771, #222835, #203285 ) ;
#86952 = DIRECTION ( 'NONE',  ( 1.000000000000000000, 5.603460673774838784E-17, 1.046060675573451523E-16 ) ) ;
#86951 = VECTOR ( 'NONE', #201997, 1000.000000000000000 ) ;
#86953 = CARTESIAN_POINT ( 'NONE',  ( -18.59999999999999787, 77.16412189325360771, -162.1082593989527254 ) ) ;
#86954 = AXIS2_PLACEMENT_3D ( 'NONE', #189349, #150234, #208900 ) ;
#86955 = CARTESIAN_POINT ( 'NONE',  ( -21.05000000000000071, 87.48912529308769592, -66.52310748452423184 ) ) ;
#86956 = EDGE_CURVE ( 'NONE', #18621, #123416, #43241, .T. ) ;
#86957 = VERTEX_POINT ( 'NONE', #98603 ) ;
#86958 = DIRECTION ( 'NONE',  ( 1.000000000000000000, 7.304098846218135653E-16, 5.311601492717085047E-30 ) ) ;
#86959 = EDGE_LOOP ( 'NONE', ( #229431, #44309, #136845, #101431 ) ) ;
#86962 = ORIENTED_EDGE ( 'NONE', *, *, #236960, .F. ) ;
#86961 = CARTESIAN_POINT ( 'NONE',  ( -23.15000000000000213, 1.115651490242849210E-11, -62.85000000000004405 ) ) ;
#86960 = DIRECTION ( 'NONE',  ( 0.000000000000000000, 0.6728971962617172897, -0.7397360091702445128 ) ) ;
#86963 = DIRECTION ( 'NONE',  ( -1.000000000000000000, 0.000000000000000000, 0.000000000000000000 ) ) ;
#86964 = ORIENTED_EDGE ( 'NONE', *, *, #242563, .F. ) ;
#86965 = LINE ( 'NONE', #107840, #117159 ) ;
#86966 = ORIENTED_EDGE ( 'NONE', *, *, #25651, .T. ) ;
#86968 = EDGE_CURVE ( 'NONE', #80243, #90604, #151598, .T. ) ;
#86967 = FACE_OUTER_BOUND ( 'NONE', #257352, .T. ) ;
#86969 = CARTESIAN_POINT ( 'NONE',  ( 23.14999999999999503, 11.65000000001116298, -122.2500000000000284 ) ) ;
#86970 = CARTESIAN_POINT ( 'NONE',  ( -18.40000000000000213, 64.52683809664929981, -78.84905355133234650 ) ) ;
#86971 = AXIS2_PLACEMENT_3D ( 'NONE', #182198, #3539, #162635 ) ;
#86972 = ADVANCED_FACE ( 'NONE', ( #20415 ), #80334, .F. ) ;
#86973 = EDGE_CURVE ( 'NONE', #244742, #127799, #97367, .T. ) ;
#86974 = DIRECTION ( 'NONE',  ( 1.734723475976817507E-14, 0.000000000000000000, -1.000000000000000000 ) ) ;
#86975 = ORIENTED_EDGE ( 'NONE', *, *, #54698, .T. ) ;
#86976 = DIRECTION ( 'NONE',  ( 0.000000000000000000, 1.000000000000000000, -0.000000000000000000 ) ) ;
#86977 = DIRECTION ( 'NONE',  ( -1.000000000000000000, 0.000000000000000000, 0.000000000000000000 ) ) ;
#86978 = CARTESIAN_POINT ( 'NONE',  ( -12.25000000000000355, 66.65000000001229807, -153.5045385271217526 ) ) ;
#86979 = ORIENTED_EDGE ( 'NONE', *, *, #218430, .T. ) ;
#86980 = CARTESIAN_POINT ( 'NONE',  ( -23.39999999999994529, 87.50449464844290048, -34.18759587077607165 ) ) ;
#86981 = ORIENTED_EDGE ( 'NONE', *, *, #116517, .F. ) ;
#86982 = CARTESIAN_POINT ( 'NONE',  ( 21.09610168723073542, 30.82370917696424328, -252.1284611548308874 ) ) ;
#86983 = EDGE_CURVE ( 'NONE', #87387, #193635, #143169, .T. ) ;
#86984 = CARTESIAN_POINT ( 'NONE',  ( 20.94999999999999574, 72.02722222756958104, -225.1832529173024398 ) ) ;
#86985 = PLANE ( 'NONE',  #122875 ) ;
#86986 = B_SPLINE_CURVE_WITH_KNOTS ( 'NONE', 3,
 ( #235084, #175152, #193402, #197225, #79824, #301, #53874, #218052, #39478, #76001 ),
 .UNSPECIFIED., .F., .F.,
 ( 4, 3, 3, 4 ),
 ( 0.000000000000000000, 0.0002000000000008585893, 0.001000000000082977483, 0.001967863649483336721 ),
 .UNSPECIFIED. ) ;
#86988 = ORIENTED_EDGE ( 'NONE', *, *, #154775, .F. ) ;
#86987 = CARTESIAN_POINT ( 'NONE',  ( 20.94999999999999929, 76.00000000001142553, -36.02310748452432421 ) ) ;
#86989 = ADVANCED_FACE ( 'NONE', ( #227575 ), #50209, .F. ) ;
#86990 = DIRECTION ( 'NONE',  ( 0.000000000000000000, -0.4088369013363783999, 0.9126074666063545004 ) ) ;
#86991 = EDGE_CURVE ( 'NONE', #222371, #12431, #139059, .T. ) ;
#86992 = LINE ( 'NONE', #46588, #85832 ) ;
#86993 = ORIENTED_EDGE ( 'NONE', *, *, #183914, .T. ) ;
#86994 = CIRCLE ( 'NONE', #182904, 0.09999999999999036049 ) ;
#86996 = AXIS2_PLACEMENT_3D ( 'NONE', #167286, #168592, #188105 ) ;
#86995 = DIRECTION ( 'NONE',  ( 0.000000000000000000, 0.000000000000000000, 1.000000000000000000 ) ) ;
#86997 = CARTESIAN_POINT ( 'NONE',  ( -18.50000000000000000, 66.85000000001173248, -81.27310748452438816 ) ) ;
#86998 = ORIENTED_EDGE ( 'NONE', *, *, #47788, .T. ) ;
#86999 = VECTOR ( 'NONE', #83621, 1000.000000000000000 ) ;
#87001 = CARTESIAN_POINT ( 'NONE',  ( 18.59999999999999432, 14.81796439977981272, -236.5325475414793743 ) ) ;
#87000 = AXIS2_PLACEMENT_3D ( 'NONE', #69188, #187845, #148711 ) ;
#87002 = ORIENTED_EDGE ( 'NONE', *, *, #16392, .F. ) ;
#87003 = LINE ( 'NONE', #64895, #216700 ) ;
#87004 = AXIS2_PLACEMENT_3D ( 'NONE', #23698, #60209, #83598 ) ;
#87006 = VERTEX_POINT ( 'NONE', #209296 ) ;
#87005 = DIRECTION ( 'NONE',  ( 0.000000000000000000, 0.3738317757009942399, -0.9274965247785252886 ) ) ;
#87007 = EDGE_CURVE ( 'NONE', #181065, #225548, #172461, .T. ) ;
#87008 = EDGE_CURVE ( 'NONE', #25173, #212362, #1707, .T. ) ;
#87011 = ORIENTED_EDGE ( 'NONE', *, *, #96733, .F. ) ;
#87010 = ORIENTED_EDGE ( 'NONE', *, *, #224557, .T. ) ;
#87009 = FACE_OUTER_BOUND ( 'NONE', #102631, .T. ) ;
#87013 = CIRCLE ( 'NONE', #116290, 0.4000000000000121791 ) ;
#87012 = DIRECTION ( 'NONE',  ( 0.000000000000000000, -6.308085367188393199E-16, -1.000000000000000000 ) ) ;
#87014 = AXIS2_PLACEMENT_3D ( 'NONE', #91330, #230855, #71781 ) ;
#87015 = DIRECTION ( 'NONE',  ( 0.000000000000000000, 0.9126074666063769270, 0.4088369013363280513 ) ) ;
#87017 = EDGE_CURVE ( 'NONE', #113112, #97927, #176527, .T. ) ;
#87016 = CARTESIAN_POINT ( 'NONE',  ( 21.14999999999999858, 76.00000000001222134, -148.1726782920690937 ) ) ;
#87018 = CIRCLE ( 'NONE', #24530, 11.64999999999999325 ) ;
#87020 = CARTESIAN_POINT ( 'NONE',  ( -12.92414019175885898, 66.58236703690523939, -51.37415901879212754 ) ) ;
#87019 = LINE ( 'NONE', #47906, #19177 ) ;
#87021 = DIRECTION ( 'NONE',  ( 1.000000000000000000, 0.000000000000000000, 0.000000000000000000 ) ) ;
#87022 = DIRECTION ( 'NONE',  ( 0.000000000000000000, -0.8660254037844419273, 0.4999999999999942824 ) ) ;
#87023 = DIRECTION ( 'NONE',  ( 0.000000000000000000, 0.2128009952263485993, -0.9770955615653341697 ) ) ;
#87024 = CARTESIAN_POINT ( 'NONE',  ( 21.05000000000000071, 1.115649653272650466E-11, -196.9999999999999432 ) ) ;
#87025 = AXIS2_PLACEMENT_3D ( 'NONE', #25228, #163440, #26509 ) ;
#87026 = DIRECTION ( 'NONE',  ( 1.000000000000000000, 0.000000000000000000, 0.000000000000000000 ) ) ;
#87027 = ORIENTED_EDGE ( 'NONE', *, *, #226142, .T. ) ;
#87028 = ORIENTED_EDGE ( 'NONE', *, *, #241275, .F. ) ;
#87029 = CARTESIAN_POINT ( 'NONE',  ( -21.05000000000000071, 64.40000000001175806, -76.45131071479988805 ) ) ;
#87031 = ORIENTED_EDGE ( 'NONE', *, *, #240229, .T. ) ;
#87030 = CYLINDRICAL_SURFACE ( 'NONE', #16185, 0.09999999999999939493 ) ;
#87032 = ORIENTED_EDGE ( 'NONE', *, *, #73781, .F. ) ;
#87033 = DIRECTION ( 'NONE',  ( -1.000000000000000000, 2.952720810173289112E-16, 2.061873921506763405E-30 ) ) ;
#87034 = ORIENTED_EDGE ( 'NONE', *, *, #45912, .T. ) ;
#87035 = CARTESIAN_POINT ( 'NONE',  ( -21.05000000000000071, 69.58633726514295859, -136.4375146211624497 ) ) ;
#87036 = EDGE_CURVE ( 'NONE', #256686, #229236, #39164, .T. ) ;
#87037 = EDGE_LOOP ( 'NONE', ( #14618, #89137, #139610, #174531 ) ) ;
#87038 =( LENGTH_UNIT ( ) NAMED_UNIT ( * ) SI_UNIT ( .MILLI., .METRE. ) );
#87040 = EDGE_CURVE ( 'NONE', #80924, #90864, #183327, .T. ) ;
#87039 = DIRECTION ( 'NONE',  ( 1.000000000000000000, -2.849773892568378313E-16, 7.728835255496647986E-17 ) ) ;
#87041 = CIRCLE ( 'NONE', #232838, 0.1000000000000066530 ) ;
#87042 = VECTOR ( 'NONE', #238621, 1000.000000000000000 ) ;
#87044 = ORIENTED_EDGE ( 'NONE', *, *, #213326, .F. ) ;
#87043 = VERTEX_POINT ( 'NONE', #5941 ) ;
#87045 = ORIENTED_EDGE ( 'NONE', *, *, #6491, .F. ) ;
#87046 = CARTESIAN_POINT ( 'NONE',  ( 21.12769345151713196, 10.71928767695172624, -45.74748034619748438 ) ) ;
#87047 = ORIENTED_EDGE ( 'NONE', *, *, #234542, .F. ) ;
#87048 = EDGE_LOOP ( 'NONE', ( #178829, #42341, #255200, #54043 ) ) ;
#87049 = EDGE_CURVE ( 'NONE', #229766, #237818, #206733, .T. ) ;
#87050 = CARTESIAN_POINT ( 'NONE',  ( -20.64999999999999858, 2.399999999999999467, -20.27537807723789953 ) ) ;
#87051 = CARTESIAN_POINT ( 'NONE',  ( -22.39999999999999858, -0.1008583690875579364, -55.25043287651065782 ) ) ;
#87054 = ADVANCED_FACE ( 'NONE', ( #89336 ), #84159, .T. ) ;
#87053 = ORIENTED_EDGE ( 'NONE', *, *, #153324, .F. ) ;
#87052 = LINE ( 'NONE', #190033, #220824 ) ;
#87055 = TOROIDAL_SURFACE ( 'NONE', #66239, 0.9750000000000019762, 0.1000000000000000056 ) ;
#87056 = DIRECTION ( 'NONE',  ( 2.978066053179066272E-16, 1.000000000000000000, 7.147358527629759053E-15 ) ) ;
#87057 = DIRECTION ( 'NONE',  ( 0.000000000000000000, 0.9126074666063770380, 0.4088369013363281068 ) ) ;
#87059 = EDGE_LOOP ( 'NONE', ( #148596, #26448, #178548, #242955 ) ) ;
#87058 = LINE ( 'NONE', #166656, #214001 ) ;
#87060 = CARTESIAN_POINT ( 'NONE',  ( -21.05000000000000071, 70.56573376625485139, -228.3808404818380779 ) ) ;
#87061 = ORIENTED_EDGE ( 'NONE', *, *, #75840, .F. ) ;
#87062 = EDGE_CURVE ( 'NONE', #34161, #1847, #185881, .T. ) ;
#87063 = DIRECTION ( 'NONE',  ( 1.000000000000000000, 0.000000000000000000, 0.000000000000000000 ) ) ;
#87064 = ORIENTED_EDGE ( 'NONE', *, *, #191823, .F. ) ;
#87065 = DIRECTION ( 'NONE',  ( 2.952720810173289112E-16, 0.4088369013363266635, -0.9126074666063777041 ) ) ;
#87066 = ORIENTED_EDGE ( 'NONE', *, *, #228883, .T. ) ;
#87069 = CARTESIAN_POINT ( 'NONE',  ( 22.48660254037844197, 11.65000000001116298, -133.9500000000000171 ) ) ;
#87068 = DIRECTION ( 'NONE',  ( -1.000000000000000000, 0.000000000000000000, 0.000000000000000000 ) ) ;
#87067 = TOROIDAL_SURFACE ( 'NONE', #32980, 11.65000000000000036, 0.1000000000000000056 ) ;
#87070 = VECTOR ( 'NONE', #180232, 1000.000000000000000 ) ;
#87071 = ADVANCED_FACE ( 'NONE', ( #247129 ), #45093, .T. ) ;
#87072 = CARTESIAN_POINT ( 'NONE',  ( 23.24999999999997513, 64.35000000001146248, -43.03791325517834565 ) ) ;
#87073 = DIRECTION ( 'NONE',  ( 0.000000000000000000, -0.2128009952263485993, 0.9770955615653341697 ) ) ;
#87075 = ADVANCED_FACE ( 'NONE', ( #88038 ), #8538, .F. ) ;
#87074 = CIRCLE ( 'NONE', #57851, 0.09999999999999939493 ) ;
#87076 = ORIENTED_EDGE ( 'NONE', *, *, #40060, .T. ) ;
#87077 = ORIENTED_EDGE ( 'NONE', *, *, #176685, .T. ) ;
#87078 = DIRECTION ( 'NONE',  ( 0.000000000000000000, 0.000000000000000000, -1.000000000000000000 ) ) ;
#87079 = DIRECTION ( 'NONE',  ( 0.000000000000000000, 0.000000000000000000, -1.000000000000000000 ) ) ;
#87080 = VERTEX_POINT ( 'NONE', #165040 ) ;
#87081 = DIRECTION ( 'NONE',  ( 0.000000000000000000, -0.01283462868041981321, -0.9999176327611367654 ) ) ;
#87082 = ORIENTED_EDGE ( 'NONE', *, *, #247800, .T. ) ;
#87083 = ADVANCED_FACE ( 'NONE', ( #245864 ), #47635, .T. ) ;
#87084 = CARTESIAN_POINT ( 'NONE',  ( -22.59999999999999787, 11.74987124438766273, -66.93457040898637445 ) ) ;
#87085 = ORIENTED_EDGE ( 'NONE', *, *, #161719, .F. ) ;
#87086 = DIRECTION ( 'NONE',  ( -1.000000000000000000, -2.952720810173289112E-16, 0.000000000000000000 ) ) ;
#87087 = CIRCLE ( 'NONE', #120457, 0.09999999999998898659 ) ;
#87088 = AXIS2_PLACEMENT_3D ( 'NONE', #198167, #42956, #40421 ) ;
#87089 = CARTESIAN_POINT ( 'NONE',  ( -23.25000000000000000, -0.1008583690875562017, -155.7504328765105868 ) ) ;
#87090 = CARTESIAN_POINT ( 'NONE',  ( 18.59999999999999787, -1.263275465206102233, -141.9018646667464338 ) ) ;
#87091 = ORIENTED_EDGE ( 'NONE', *, *, #124523, .T. ) ;
#87092 = CARTESIAN_POINT ( 'NONE',  ( 18.50000000000000355, -9.399999999988830623, -207.8820418481726620 ) ) ;
#87093 =( NAMED_UNIT ( * ) SI_UNIT ( $, .STERADIAN. ) SOLID_ANGLE_UNIT ( ) );
#87094 = EDGE_CURVE ( 'NONE', #236288, #97847, #148051, .T. ) ;
#87095 = ADVANCED_FACE ( 'NONE', ( #85461 ), #186515, .T. ) ;
#87097 = EDGE_LOOP ( 'NONE', ( #105599, #13150, #133480, #6142 ) ) ;
#87096 = AXIS2_PLACEMENT_3D ( 'NONE', #115679, #56949, #140358 ) ;
#87098 = VERTEX_POINT ( 'NONE', #13668 ) ;
#87099 = AXIS2_PLACEMENT_3D ( 'NONE', #87191, #166787, #246295 ) ;
#87100 = CIRCLE ( 'NONE', #16398, 0.09999999999999939493 ) ;
#87101 = ORIENTED_EDGE ( 'NONE', *, *, #182108, .T. ) ;
#87102 = AXIS2_PLACEMENT_3D ( 'NONE', #78091, #157692, #237189 ) ;
#87103 = ADVANCED_FACE ( 'NONE', ( #214426 ), #155693, .F. ) ;
#87104 = CARTESIAN_POINT ( 'NONE',  ( -14.00000000000000178, 9.850000000011133849, -83.75000000000004263 ) ) ;
#87105 = CARTESIAN_POINT ( 'NONE',  ( -20.64999999999999858, 65.77012247227901298, -213.5448142138000378 ) ) ;
#87106 = DIRECTION ( 'NONE',  ( 1.000000000000000000, 2.952720810173289112E-16, -0.000000000000000000 ) ) ;
#87107 = DIRECTION ( 'NONE',  ( 0.000000000000000000, -1.000000000000000000, 0.000000000000000000 ) ) ;
#87108 = DIRECTION ( 'NONE',  ( 1.000000000000000000, 0.000000000000000000, 0.000000000000000000 ) ) ;
#87109 = AXIS2_PLACEMENT_3D ( 'NONE', #117556, #251928, #112436 ) ;
#87111 = LINE ( 'NONE', #150957, #95077 ) ;
#87110 = DIRECTION ( 'NONE',  ( -0.000000000000000000, -0.9984213852963228497, -0.05616704890745022327 ) ) ;
#87112 = EDGE_CURVE ( 'NONE', #257455, #87436, #73675, .T. ) ;
#87114 = VERTEX_POINT ( 'NONE', #34541 ) ;
#87113 = DIRECTION ( 'NONE',  ( -0.000000000000000000, -0.6132151058540604716, 0.7899159663865477077 ) ) ;
#87115 = DIRECTION ( 'NONE',  ( 3.616040088954490704E-32, 7.105427357601001859E-15, -1.000000000000000000 ) ) ;
#87116 = ORIENTED_EDGE ( 'NONE', *, *, #1258, .F. ) ;
#87117 = DIRECTION ( 'NONE',  ( 0.000000000000000000, -6.982962677686266711E-15, 1.000000000000000000 ) ) ;
#87118 = EDGE_CURVE ( 'NONE', #8311, #142060, #115330, .T. ) ;
#87119 = ORIENTED_EDGE ( 'NONE', *, *, #239870, .T. ) ;
#87120 = EDGE_LOOP ( 'NONE', ( #119304, #127208, #57486, #179450 ) ) ;
#87121 = DIRECTION ( 'NONE',  ( 1.000000000000000000, 0.000000000000000000, -0.000000000000000000 ) ) ;
#87122 = CARTESIAN_POINT ( 'NONE',  ( -18.50000000000000000, 36.65892442174472876, -249.5511627012454596 ) ) ;
#87123 = CARTESIAN_POINT ( 'NONE',  ( -21.09096482362091507, 75.96055172123860189, -209.8866518499290521 ) ) ;
#87124 = DIRECTION ( 'NONE',  ( 0.000000000000000000, 0.3738317757009225195, 0.9274965247785541544 ) ) ;
#87125 = VECTOR ( 'NONE', #32070, 1000.000000000000000 ) ;
#87126 = CARTESIAN_POINT ( 'NONE',  ( -20.94999999999999929, 68.87972903831452243, -132.8635444426850825 ) ) ;
#87127 = ORIENTED_EDGE ( 'NONE', *, *, #34723, .T. ) ;
#87128 = EDGE_LOOP ( 'NONE', ( #203514, #249606, #51424, #68870 ) ) ;
#87129 = CARTESIAN_POINT ( 'NONE',  ( -23.25000000000000000, 71.85000000001198828, -115.2731074845243171 ) ) ;
#87131 = EDGE_CURVE ( 'NONE', #187124, #39261, #72473, .T. ) ;
#87130 = VERTEX_POINT ( 'NONE', #114038 ) ;
#87132 = DIRECTION ( 'NONE',  ( -1.000000000000000000, 0.000000000000000000, 0.000000000000000000 ) ) ;
#87133 = ORIENTED_EDGE ( 'NONE', *, *, #34969, .T. ) ;
#87134 = CYLINDRICAL_SURFACE ( 'NONE', #132091, 0.09999999999999939493 ) ;
#87135 = DIRECTION ( 'NONE',  ( 0.000000000000000000, 0.2128009952263603677, -0.9770955615653313941 ) ) ;
#87136 = PLANE ( 'NONE',  #53073 ) ;
#87137 = DIRECTION ( 'NONE',  ( 0.000000000000000000, -7.304098846218085561E-15, 1.000000000000000000 ) ) ;
#87138 = ORIENTED_EDGE ( 'NONE', *, *, #205326, .T. ) ;
#87139 = DIRECTION ( 'NONE',  ( 2.827886303505249259E-16, 0.8660254037844377084, 0.5000000000000016653 ) ) ;
#87140 = CIRCLE ( 'NONE', #253537, 0.1000000000000028644 ) ;
#87141 = DIRECTION ( 'NONE',  ( 1.000000000000000000, 0.000000000000000000, 0.000000000000000000 ) ) ;
#87142 = DIRECTION ( 'NONE',  ( 1.000000000000000000, 0.000000000000000000, 0.000000000000000000 ) ) ;
#87143 = CIRCLE ( 'NONE', #183024, 0.09999999999999939493 ) ;
#87145 = ADVANCED_FACE ( 'NONE', ( #16268 ), #91912, .F. ) ;
#87144 = CARTESIAN_POINT ( 'NONE',  ( -23.15000000000000213, 71.85000000001276987, -215.2731074845243882 ) ) ;
#87146 = DIRECTION ( 'NONE',  ( 0.000000000000000000, 1.000000000000000000, 6.352154140967427193E-15 ) ) ;
#87147 = CARTESIAN_POINT ( 'NONE',  ( 18.49505816908823164, 77.27516569126373724, -241.6972430987673022 ) ) ;
#87148 = AXIS2_PLACEMENT_3D ( 'NONE', #64356, #128180, #104716 ) ;
#87149 = EDGE_LOOP ( 'NONE', ( #117793, #22849, #244485, #244556 ) ) ;
#87150 = EDGE_CURVE ( 'NONE', #150222, #156295, #188993, .T. ) ;
#87151 = VERTEX_POINT ( 'NONE', #189742 ) ;
#87152 = FACE_OUTER_BOUND ( 'NONE', #96999, .T. ) ;
#87153 = CARTESIAN_POINT ( 'NONE',  ( -20.54999999999999716, 1.115600667400684642E-11, -200.9999999999999432 ) ) ;
#87154 = CARTESIAN_POINT ( 'NONE',  ( -23.49999999999994316, 76.00000000001119815, -36.02310748452479316 ) ) ;
#87155 = CARTESIAN_POINT ( 'NONE',  ( 20.22483756094572271, 66.49809532114194610, -161.8835683558092171 ) ) ;
#87156 = AXIS2_PLACEMENT_3D ( 'NONE', #123442, #223808, #20509 ) ;
#87157 = VERTEX_POINT ( 'NONE', #95754 ) ;
#87158 = CARTESIAN_POINT ( 'NONE',  ( -20.85000000000000142, 87.75000000001172396, -69.52310748452423184 ) ) ;
#87159 = DIRECTION ( 'NONE',  ( 0.000000000000000000, -6.467318590049456648E-15, 1.000000000000000000 ) ) ;
#87160 = CARTESIAN_POINT ( 'NONE',  ( -18.69999999999999929, -9.849999999999996092, 31.39999999999999858 ) ) ;
#87161 = CARTESIAN_POINT ( 'NONE',  ( 18.59999999999999076, 65.79142135624879018, -44.87310748452438958 ) ) ;
#87162 = EDGE_CURVE ( 'NONE', #251301, #137039, #197344, .T. ) ;
#87163 = DIRECTION ( 'NONE',  ( 0.000000000000000000, 1.000000000000000000, 2.891205793294679805E-16 ) ) ;
#87164 = AXIS2_PLACEMENT_3D ( 'NONE', #42096, #184138, #19957 ) ;
#87165 = DIRECTION ( 'NONE',  ( 1.000000000000000000, 0.000000000000000000, 0.000000000000000000 ) ) ;
#87166 = ORIENTED_EDGE ( 'NONE', *, *, #70773, .F. ) ;
#87167 = ORIENTED_EDGE ( 'NONE', *, *, #126187, .F. ) ;
#87168 = LINE ( 'NONE', #250114, #245807 ) ;
#87169 = DIRECTION ( 'NONE',  ( 0.000000000000000000, 0.000000000000000000, 1.000000000000000000 ) ) ;
#87170 = LINE ( 'NONE', #166763, #25821 ) ;
#87171 = DIRECTION ( 'NONE',  ( -3.265361837132813093E-16, -1.000000000000000000, 7.445645354460596589E-46 ) ) ;
#87172 = CARTESIAN_POINT ( 'NONE',  ( -16.86757978335471719, 44.08163191180170770, -235.3059065703284318 ) ) ;
#87173 = ORIENTED_EDGE ( 'NONE', *, *, #239903, .T. ) ;
#87174 = CARTESIAN_POINT ( 'NONE',  ( -20.94999999999999929, -1.835859311432479268, -78.50443916879852679 ) ) ;
#87175 = ITEM_DEFINED_TRANSFORMATION ( 'NONE', 'NONE', #52846,  #2425 ) ;
#87176 = DIRECTION ( 'NONE',  ( 0.000000000000000000, 0.2617529984165031243, 0.9651348961777157509 ) ) ;
#87177 = ORIENTED_EDGE ( 'NONE', *, *, #128898, .F. ) ;
#87178 = CARTESIAN_POINT ( 'NONE',  ( -20.64999999999999858, 4.250000000011156409, -79.35000000000005116 ) ) ;
#87179 = VERTEX_POINT ( 'NONE', #11108 ) ;
#87180 = ORIENTED_EDGE ( 'NONE', *, *, #243426, .F. ) ;
#87181 = ORIENTED_EDGE ( 'NONE', *, *, #226906, .F. ) ;
#87182 = CARTESIAN_POINT ( 'NONE',  ( 21.05000000000000426, 10.62950747927179407, -74.62797939999673247 ) ) ;
#87183 = PLANE ( 'NONE',  #154767 ) ;
#87184 = DIRECTION ( 'NONE',  ( -7.304098846218201720E-16, 1.000000000000000000, 0.000000000000000000 ) ) ;
#87185 = CARTESIAN_POINT ( 'NONE',  ( -21.10257677756356642, 69.60161825747921682, -103.0480582340923092 ) ) ;
#87186 = CARTESIAN_POINT ( 'NONE',  ( -20.54999999999999716, 76.00000000001142553, -36.02310748452432421 ) ) ;
#87187 = DIRECTION ( 'NONE',  ( 0.000000000000000000, 0.000000000000000000, 1.000000000000000000 ) ) ;
#87188 = EDGE_CURVE ( 'NONE', #201200, #38057, #192314, .T. ) ;
#87189 = DIRECTION ( 'NONE',  ( 1.000000000000000000, 0.000000000000000000, 0.000000000000000000 ) ) ;
#87191 = CARTESIAN_POINT ( 'NONE',  ( -18.59999999999999787, 69.15387683765952431, -132.7853812176745407 ) ) ;
#87190 = DIRECTION ( 'NONE',  ( 0.000000000000000000, 0.4999999999999956701, -0.8660254037844411501 ) ) ;
#87192 = CIRCLE ( 'NONE', #137278, 0.09999999999999907574 ) ;
#87193 = DIRECTION ( 'NONE',  ( 6.938893903907991995E-14, 0.000000000000000000, -1.000000000000000000 ) ) ;
#87194 = CIRCLE ( 'NONE', #232979, 0.2000000000000057288 ) ;
#87195 = DIRECTION ( 'NONE',  ( 1.000000000000000000, 0.000000000000000000, 0.000000000000000000 ) ) ;
#87196 = CARTESIAN_POINT ( 'NONE',  ( -20.54999999999999716, 54.34471204062663219, -239.4366250215122420 ) ) ;
#87197 = TOROIDAL_SURFACE ( 'NONE', #145462, 11.65000000000000036, 0.1000000000000000056 ) ;
#87199 = CARTESIAN_POINT ( 'NONE',  ( 18.59999999999999432, 77.16270174994961906, -61.42310748452431568 ) ) ;
#87198 = TOROIDAL_SURFACE ( 'NONE', #237258, 4.149999999999999467, 0.1000000000000000056 ) ;
#87200 = EDGE_LOOP ( 'NONE', ( #181046, #229423, #188750, #35383 ) ) ;
#87201 = EDGE_LOOP ( 'NONE', ( #30831, #155606, #229770, #85561 ) ) ;
#87202 = CARTESIAN_POINT ( 'NONE',  ( -21.05000000000000071, 11.65000000001115588, -134.1000000000000227 ) ) ;
#87203 = CARTESIAN_POINT ( 'NONE',  ( -23.25000000000000000, 64.25313205997782973, -247.2214437328673853 ) ) ;
#87205 = CARTESIAN_POINT ( 'NONE',  ( 20.85000000000000142, 0.000000000000000000, -33.50000000000000000 ) ) ;
#87204 = LINE ( 'NONE', #213247, #4856 ) ;
#87206 = AXIS2_PLACEMENT_3D ( 'NONE', #62497, #239852, #221531 ) ;
#87207 = CARTESIAN_POINT ( 'NONE',  ( 21.05000000000000071, 76.00000000001213607, -136.5231074845243313 ) ) ;
#87209 = ADVANCED_FACE ( 'NONE', ( #170233 ), #147471, .T. ) ;
#87208 = CYLINDRICAL_SURFACE ( 'NONE', #170914, 0.1000000000000028644 ) ;
#87210 = CARTESIAN_POINT ( 'NONE',  ( -23.25000000000000000, 11.75000000001115552, -79.15000000000004832 ) ) ;
#87211 = VERTEX_POINT ( 'NONE', #254792 ) ;
#87212 = ORIENTED_EDGE ( 'NONE', *, *, #252110, .F. ) ;
#87213 = ADVANCED_FACE ( 'NONE', ( #193598 ), #14970, .T. ) ;
#87214 = CIRCLE ( 'NONE', #220522, 0.2000000000000057288 ) ;
#87215 = VECTOR ( 'NONE', #63744, 1000.000000000000000 ) ;
#87217 = AXIS2_PLACEMENT_3D ( 'NONE', #90780, #171659, #29576 ) ;
#87216 = CYLINDRICAL_SURFACE ( 'NONE', #30430, 0.09999999999998898659 ) ;
#87218 = ORIENTED_EDGE ( 'NONE', *, *, #47273, .F. ) ;
#87219 = CARTESIAN_POINT ( 'NONE',  ( 18.59999999999999432, 45.93315328338058379, -256.6017782078560003 ) ) ;
#87220 = EDGE_CURVE ( 'NONE', #194844, #171093, #122346, .T. ) ;
#87221 = AXIS2_PLACEMENT_3D ( 'NONE', #181436, #200984, #43199 ) ;
#87222 = EDGE_CURVE ( 'NONE', #89391, #77509, #84888, .T. ) ;
#87223 = EDGE_CURVE ( 'NONE', #204755, #84823, #1792, .T. ) ;
#87224 = VERTEX_POINT ( 'NONE', #102160 ) ;
#87225 = CARTESIAN_POINT ( 'NONE',  ( -20.94999999999999929, 7.128833340094563376, -233.7327013124401276 ) ) ;
#87226 = ORIENTED_EDGE ( 'NONE', *, *, #76250, .F. ) ;
#87227 = ADVANCED_FACE ( 'NONE', ( #82592 ), #117896, .T. ) ;
#87228 = CARTESIAN_POINT ( 'NONE',  ( -20.64999999999999858, 76.00000000001189449, -101.0231074845243029 ) ) ;
#87229 = LINE ( 'NONE', #148515, #112069 ) ;
#87230 = DIRECTION ( 'NONE',  ( 0.000000000000000000, -0.2128009952263605065, 0.9770955615653315052 ) ) ;
#87231 = DIRECTION ( 'NONE',  ( 0.000000000000000000, -0.9501938099239353175, 0.3116596277708039708 ) ) ;
#87232 = DIRECTION ( 'NONE',  ( 1.000000000000000000, 0.000000000000000000, 0.000000000000000000 ) ) ;
#87233 = CARTESIAN_POINT ( 'NONE',  ( -21.05000000000000071, 64.35000000001161879, -62.73924182154625129 ) ) ;
#87234 = EDGE_CURVE ( 'NONE', #99302, #18158, #51570, .T. ) ;
#87235 = DIRECTION ( 'NONE',  ( 0.000000000000000000, -0.9856811345164803173, -0.1686199900910455851 ) ) ;
#87236 = CARTESIAN_POINT ( 'NONE',  ( -22.39999999999999858, 0.1000000000111554016, -126.2092204016266379 ) ) ;
#87238 = ORIENTED_EDGE ( 'NONE', *, *, #8687, .T. ) ;
#87237 = CARTESIAN_POINT ( 'NONE',  ( 18.44206774312973351, -0.7347395580569413553, -242.2268588646078626 ) ) ;
#87239 = LINE ( 'NONE', #242470, #176946 ) ;
#87240 = ORIENTED_EDGE ( 'NONE', *, *, #38010, .T. ) ;
#87242 = VERTEX_POINT ( 'NONE', #138711 ) ;
#87241 = CARTESIAN_POINT ( 'NONE',  ( -23.15000000000000213, 64.25000000001222134, -148.2731074845243882 ) ) ;
#87243 = TOROIDAL_SURFACE ( 'NONE', #41489, 12.77499999999999858, 0.1000000000000000056 ) ;
#87244 = VERTEX_POINT ( 'NONE', #200020 ) ;
#87245 = CARTESIAN_POINT ( 'NONE',  ( -18.39999999999999858, 85.40000000001222702, -148.2731074845242460 ) ) ;
#87246 = CARTESIAN_POINT ( 'NONE',  ( -21.05000000000000071, 1.835341550235567887, -145.6551512925629766 ) ) ;
#87247 = CARTESIAN_POINT ( 'NONE',  ( 21.05000000000000071, 0.03201369319901656296, -127.7411572764626584 ) ) ;
#87248 = CARTESIAN_POINT ( 'NONE',  ( -18.59999999999999787, 64.35000000001203091, -114.7731074845243882 ) ) ;
#87249 = TOROIDAL_SURFACE ( 'NONE', #49847, 0.4000000000000012990, 0.1000000000000000056 ) ;
#87250 = DIRECTION ( 'NONE',  ( 1.000000000000000000, 0.000000000000000000, 0.000000000000000000 ) ) ;
#87251 = CARTESIAN_POINT ( 'NONE',  ( 18.60000000000000142, -9.399999999988782662, -141.2972597596633193 ) ) ;
#87252 = DIRECTION ( 'NONE',  ( -1.000000000000000000, 0.000000000000000000, 0.000000000000000000 ) ) ;
#87254 = EDGE_CURVE ( 'NONE', #95552, #190717, #81311, .T. ) ;
#87253 = PLANE ( 'NONE',  #214926 ) ;
#87255 = DIRECTION ( 'NONE',  ( 0.000000000000000000, 0.000000000000000000, 1.000000000000000000 ) ) ;
#87256 = ORIENTED_EDGE ( 'NONE', *, *, #102025, .T. ) ;
#87257 = ORIENTED_EDGE ( 'NONE', *, *, #196047, .F. ) ;
#87258 = CARTESIAN_POINT ( 'NONE',  ( -16.90257928357874562, 9.954106821116520010, -180.1362854301136451 ) ) ;
#87259 = AXIS2_PLACEMENT_3D ( 'NONE', #256820, #194370, #78232 ) ;
#87260 = ORIENTED_EDGE ( 'NONE', *, *, #157529, .T. ) ;
#87261 = LINE ( 'NONE', #166859, #63346 ) ;
#87263 = EDGE_LOOP ( 'NONE', ( #28167, #104527, #244080, #148897 ) ) ;
#87262 = CIRCLE ( 'NONE', #91390, 0.1000000000000013933 ) ;
#87264 = DIRECTION ( 'NONE',  ( -0.000000000000000000, -2.891205793294679805E-16, 1.000000000000000000 ) ) ;
#87265 = EDGE_CURVE ( 'NONE', #123343, #94806, #89857, .T. ) ;
#87266 = TOROIDAL_SURFACE ( 'NONE', #249784, 11.65000000000000036, 0.1000000000000000056 ) ;
#87267 = FACE_OUTER_BOUND ( 'NONE', #146055, .T. ) ;
#87268 = FACE_OUTER_BOUND ( 'NONE', #200102, .T. ) ;
#87269 = DIRECTION ( 'NONE',  ( 0.000000000000000000, -1.000000000000000000, -6.982962677686265922E-15 ) ) ;
#87270 = CARTESIAN_POINT ( 'NONE',  ( -20.94999999999999929, 1.115600667400684642E-11, -67.00000000000000000 ) ) ;
#87271 = ORIENTED_EDGE ( 'NONE', *, *, #245568, .T. ) ;
#87272 = CIRCLE ( 'NONE', #133093, 0.5000000000000007772 ) ;
#87273 = CIRCLE ( 'NONE', #174646, 0.6000000000000033085 ) ;
#87274 = CARTESIAN_POINT ( 'NONE',  ( 21.05000000000000071, 71.00000000001180922, -81.92837350343744163 ) ) ;
#87275 = DIRECTION ( 'NONE',  ( 1.000000000000000000, 0.000000000000000000, 0.000000000000000000 ) ) ;
#87276 = LINE ( 'NONE', #24789, #203011 ) ;
#87278 = EDGE_CURVE ( 'NONE', #37616, #30650, #101836, .T. ) ;
#87277 = CARTESIAN_POINT ( 'NONE',  ( -18.50000000000000000, 67.23127455305835554, -235.8551265064784559 ) ) ;
#87279 = VERTEX_POINT ( 'NONE', #215701 ) ;
#87281 = LINE ( 'NONE', #7775, #243914 ) ;
#87280 = DIRECTION ( 'NONE',  ( 0.000000000000000000, -1.000000000000000000, -6.982962677686265922E-15 ) ) ;
#87282 = ORIENTED_EDGE ( 'NONE', *, *, #113254, .F. ) ;
#87284 = ORIENTED_EDGE ( 'NONE', *, *, #142939, .F. ) ;
#87283 = CARTESIAN_POINT ( 'NONE',  ( -16.87372397896795562, 51.19159386254698774, -232.2139266409263598 ) ) ;
#87285 = EDGE_CURVE ( 'NONE', #76379, #127210, #201290, .T. ) ;
#87286 = AXIS2_PLACEMENT_3D ( 'NONE', #250999, #192339, #252288 ) ;
#87287 = ORIENTED_EDGE ( 'NONE', *, *, #78548, .T. ) ;
#87288 = DIRECTION ( 'NONE',  ( -0.000000000000000000, 0.000000000000000000, 1.000000000000000000 ) ) ;
#87289 = VECTOR ( 'NONE', #115763, 1000.000000000000000 ) ;
#87290 = STYLED_ITEM ( 'NONE', ( #65329 ), #112300 ) ;
#87291 = MECHANICAL_DESIGN_GEOMETRIC_PRESENTATION_REPRESENTATION (  '', ( #220586 ), #149873 ) ;
#87292 = CIRCLE ( 'NONE', #58244, 0.1999999999999987899 ) ;
#87293 = CARTESIAN_POINT ( 'NONE',  ( -18.40000000000000213, 5.650000000011139001, -79.65000000000004832 ) ) ;
#87294 = CARTESIAN_POINT ( 'NONE',  ( -18.50000000000000000, 85.40000000001187175, -96.14106563635156988 ) ) ;
#87295 = ORIENTED_EDGE ( 'NONE', *, *, #5749, .F. ) ;
#87296 = LINE ( 'NONE', #243815, #134536 ) ;
#87297 = AXIS2_PLACEMENT_3D ( 'NONE', #209292, #50205, #111483 ) ;
#87299 = EDGE_CURVE ( 'NONE', #235880, #182847, #216987, .T. ) ;
#87298 = DIRECTION ( 'NONE',  ( 1.000000000000000000, 0.000000000000000000, 0.000000000000000000 ) ) ;
#87301 = DIRECTION ( 'NONE',  ( 0.000000000000000000, -0.8777080977375132376, 0.4791956752371582251 ) ) ;
#87300 = CARTESIAN_POINT ( 'NONE',  ( -22.57320508075687115, 11.75000000000000000, -3.083226800830041490E-14 ) ) ;
#87303 = VERTEX_POINT ( 'NONE', #80025 ) ;
#87302 = CARTESIAN_POINT ( 'NONE',  ( 23.24999999999999645, 11.75000000001113953, -42.75000000000000000 ) ) ;
#87304 = ADVANCED_FACE ( 'NONE', ( #38375 ), #218266, .F. ) ;
#87305 = EDGE_CURVE ( 'NONE', #116282, #241842, #158356, .T. ) ;
#87306 = EDGE_LOOP ( 'NONE', ( #71871, #142509, #224844, #196759 ) ) ;
#87307 = CARTESIAN_POINT ( 'NONE',  ( 21.97500000000000497, 12.15477401631902232, -210.9923204818763622 ) ) ;
#87308 = CIRCLE ( 'NONE', #37271, 0.1000000000000001860 ) ;
#87309 = CARTESIAN_POINT ( 'NONE',  ( -18.38639463286148867, 11.48019957384713230, -176.7499999999999716 ) ) ;
#87310 = CARTESIAN_POINT ( 'NONE',  ( 20.94999999999999929, -9.499999999988844479, -157.6060308773475640 ) ) ;
#87311 = ORIENTED_EDGE ( 'NONE', *, *, #104114, .F. ) ;
#87312 = CARTESIAN_POINT ( 'NONE',  ( 23.14999999999999503, 6.550000000011156231, -188.7499999999999716 ) ) ;
#87313 = EDGE_CURVE ( 'NONE', #30570, #96530, #20103, .T. ) ;
#87314 = DIRECTION ( 'NONE',  ( -0.000000000000000000, -1.000000000000000000, -6.982962677686266711E-15 ) ) ;
#87315 = FACE_OUTER_BOUND ( 'NONE', #165049, .T. ) ;
#87316 = ORIENTED_EDGE ( 'NONE', *, *, #128591, .F. ) ;
#87317 = CYLINDRICAL_SURFACE ( 'NONE', #225046, 0.09999999999999939493 ) ;
#87318 = CIRCLE ( 'NONE', #195698, 4.049999999999998934 ) ;
#87319 = AXIS2_PLACEMENT_3D ( 'NONE', #188572, #129873, #206857 ) ;
#87320 = VERTEX_POINT ( 'NONE', #159611 ) ;
#87321 = CYLINDRICAL_SURFACE ( 'NONE', #168960, 0.1000000000000013933 ) ;
#87322 = AXIS2_PLACEMENT_3D ( 'NONE', #258043, #95167, #255471 ) ;
#87323 = EDGE_LOOP ( 'NONE', ( #178373, #167262, #80358, #5050 ) ) ;
#87324 = ORIENTED_EDGE ( 'NONE', *, *, #168618, .T. ) ;
#87325 = SPHERICAL_SURFACE ( 'NONE', #249836, 0.1000000000000000056 ) ;
#87326 = EDGE_LOOP ( 'NONE', ( #233369, #126040, #146523, #184395 ) ) ;
#87328 = EDGE_LOOP ( 'NONE', ( #130833, #171601, #257495, #115169 ) ) ;
#87327 = CARTESIAN_POINT ( 'NONE',  ( 18.49999999999998934, 19.85039924724470950, -35.78030305780136189 ) ) ;
#87329 = ADVANCED_FACE ( 'NONE', ( #239141 ), #22781, .F. ) ;
#87330 = EDGE_CURVE ( 'NONE', #210865, #127472, #89199, .T. ) ;
#87331 = ORIENTED_EDGE ( 'NONE', *, *, #5341, .F. ) ;
#87332 = AXIS2_PLACEMENT_3D ( 'NONE', #35916, #137542, #197522 ) ;
#87334 = ORIENTED_EDGE ( 'NONE', *, *, #121587, .T. ) ;
#87333 = ORIENTED_EDGE ( 'NONE', *, *, #209519, .F. ) ;
#87335 = AXIS2_PLACEMENT_3D ( 'NONE', #223008, #9120, #106916 ) ;
#87337 = EDGE_CURVE ( 'NONE', #241566, #8126, #83827, .T. ) ;
#87336 = PLANE ( 'NONE',  #35698 ) ;
#87338 = EDGE_LOOP ( 'NONE', ( #121675, #683, #232743, #204093 ) ) ;
#87339 = DIRECTION ( 'NONE',  ( 1.000000000000000000, 0.000000000000000000, 0.000000000000000000 ) ) ;
#87340 = CARTESIAN_POINT ( 'NONE',  ( -21.05000000000000426, -1.476035864388226537, -194.6925666612220027 ) ) ;
#87341 = AXIS2_PLACEMENT_3D ( 'NONE', #219531, #123025, #121753 ) ;
#87342 = DIRECTION ( 'NONE',  ( 0.000000000000000000, 0.000000000000000000, -1.000000000000000000 ) ) ;
#87343 = LINE ( 'NONE', #26117, #26201 ) ;
#87344 = VERTEX_POINT ( 'NONE', #23967 ) ;
#87345 = EDGE_LOOP ( 'NONE', ( #230373, #10967, #246770, #254919 ) ) ;
#87346 = DIRECTION ( 'NONE',  ( -1.000000000000000000, 0.000000000000000000, 0.000000000000000000 ) ) ;
#87348 = ORIENTED_EDGE ( 'NONE', *, *, #128349, .T. ) ;
#87347 = CARTESIAN_POINT ( 'NONE',  ( -22.39999999999999858, 0.1000000000111554016, -126.2092204016266379 ) ) ;
#87349 = LINE ( 'NONE', #88625, #213230 ) ;
#87351 = EDGE_LOOP ( 'NONE', ( #27021, #228580, #55356, #108581 ) ) ;
#87350 = FACE_OUTER_BOUND ( 'NONE', #22039, .T. ) ;
#87352 = VERTEX_POINT ( 'NONE', #103456 ) ;
#87353 = DIRECTION ( 'NONE',  ( -1.836970198721029934E-16, 1.000000000000000000, 0.000000000000000000 ) ) ;
#87354 = ORIENTED_EDGE ( 'NONE', *, *, #104635, .F. ) ;
#87355 = ORIENTED_EDGE ( 'NONE', *, *, #235951, .F. ) ;
#87356 = AXIS2_PLACEMENT_3D ( 'NONE', #110351, #172945, #34696 ) ;
#87357 = AXIS2_PLACEMENT_3D ( 'NONE', #78611, #155633, #17376 ) ;
#87358 = CARTESIAN_POINT ( 'NONE',  ( 23.14999999999999503, 64.35000000001197407, -115.2731074845243739 ) ) ;
#87360 = EDGE_CURVE ( 'NONE', #167384, #41308, #222454, .T. ) ;
#87359 = CARTESIAN_POINT ( 'NONE',  ( 23.24999999999999645, 79.90000000001141700, -36.02310748452429578 ) ) ;
#87361 = B_SPLINE_CURVE_WITH_KNOTS ( 'NONE', 3,
 ( #210297, #111188, #36820, #57612, #19809, #117605, #53775, #115038, #116336, #118907, #193303, #113743, #134575 ),
 .UNSPECIFIED., .F., .F.,
 ( 4, 3, 3, 3, 4 ),
 ( -3.224855718275878119E-06, 0.000000000000000000, 6.199515528665969596E-06, 4.034952380127732529E-05, 7.452715123699841550E-05 ),
 .UNSPECIFIED. ) ;
#87363 = ORIENTED_EDGE ( 'NONE', *, *, #24600, .T. ) ;
#87362 = EDGE_LOOP ( 'NONE', ( #68246, #48939, #149531, #146014 ) ) ;
#87364 = ORIENTED_EDGE ( 'NONE', *, *, #169896, .T. ) ;
#87365 = CARTESIAN_POINT ( 'NONE',  ( 22.88900146558018989, 67.29609520889950147, -160.7731074845244166 ) ) ;
#87366 = ORIENTED_EDGE ( 'NONE', *, *, #160647, .F. ) ;
#87367 = EDGE_LOOP ( 'NONE', ( #247677, #112783, #101825, #19045 ) ) ;
#87368 = DIRECTION ( 'NONE',  ( -2.940209281316619043E-16, -0.4088369013363290505, 0.9126074666063767049 ) ) ;
#87371 = EDGE_CURVE ( 'NONE', #80209, #173183, #1881, .T. ) ;
#87370 = ORIENTED_EDGE ( 'NONE', *, *, #121316, .T. ) ;
#87369 = CARTESIAN_POINT ( 'NONE',  ( -20.94999999999994600, 65.25000000001119815, -4.423107484524790856 ) ) ;
#87372 = CARTESIAN_POINT ( 'NONE',  ( 18.49999999999999289, 64.25000000001277556, -215.2731074845244450 ) ) ;
#87374 = DIRECTION ( 'NONE',  ( 0.000000000000000000, 0.000000000000000000, 1.000000000000000000 ) ) ;
#87373 = DIRECTION ( 'NONE',  ( 0.000000000000000000, 0.000000000000000000, -1.000000000000000000 ) ) ;
#87375 = CARTESIAN_POINT ( 'NONE',  ( -21.05000000000000071, 76.10000000001245724, -181.6731074845243654 ) ) ;
#87376 = DIRECTION ( 'NONE',  ( 0.000000000000000000, 1.776356839400306474E-15, 1.000000000000000000 ) ) ;
#87377 = ORIENTED_EDGE ( 'NONE', *, *, #143768, .T. ) ;
#87378 = ADVANCED_FACE ( 'NONE', ( #163458 ), #168555, .F. ) ;
#87379 = VERTEX_POINT ( 'NONE', #203856 ) ;
#87381 = CIRCLE ( 'NONE', #233171, 0.1000000000000043771 ) ;
#87380 = CARTESIAN_POINT ( 'NONE',  ( -20.54999999999999716, 11.60596396992030144, -220.2204734678737168 ) ) ;
#87382 = DIRECTION ( 'NONE',  ( 1.000000000000000000, 0.000000000000000000, 0.000000000000000000 ) ) ;
#87383 = CIRCLE ( 'NONE', #125017, 0.1000000000000124678 ) ;
#87384 = EDGE_CURVE ( 'NONE', #97414, #246455, #9508, .T. ) ;
#87385 = AXIS2_PLACEMENT_3D ( 'NONE', #257452, #80116, #78854 ) ;
#87386 = VECTOR ( 'NONE', #174423, 1000.000000000000000 ) ;
#87387 = VERTEX_POINT ( 'NONE', #207740 ) ;
#87388 = EDGE_CURVE ( 'NONE', #255690, #71995, #26529, .T. ) ;
#87389 = CIRCLE ( 'NONE', #116626, 0.6000000000000033085 ) ;
#87390 = CARTESIAN_POINT ( 'NONE',  ( 18.59999999999999787, -1.249999999999999334, -41.30048075441506938 ) ) ;
#87392 = EDGE_CURVE ( 'NONE', #128506, #224580, #239234, .T. ) ;
#87391 = ADVANCED_FACE ( 'NONE', ( #89042 ), #25249, .T. ) ;
#87393 = VERTEX_POINT ( 'NONE', #66920 ) ;
#87394 = VERTEX_POINT ( 'NONE', #64361 ) ;
#87395 = DIRECTION ( 'NONE',  ( -1.000000000000000000, -0.000000000000000000, -0.000000000000000000 ) ) ;
#87396 = CARTESIAN_POINT ( 'NONE',  ( -18.50000000000000000, 102.4393534156127572, -84.88159887701665696 ) ) ;
#87397 = VERTEX_POINT ( 'NONE', #188162 ) ;
#87398 = CARTESIAN_POINT ( 'NONE',  ( -17.11825945287481332, 10.05000000001113847, -154.7500000000000284 ) ) ;
#87399 = LINE ( 'NONE', #166991, #39475 ) ;
#87400 = EDGE_LOOP ( 'NONE', ( #11128, #39157, #85984, #253916 ) ) ;
#87401 = FACE_OUTER_BOUND ( 'NONE', #130332, .T. ) ;
#87402 = PLANE ( 'NONE',  #141370 ) ;
#87404 = CARTESIAN_POINT ( 'NONE',  ( -21.05000000000000071, 6.413759733821438935, -67.08561306080399333 ) ) ;
#87403 = DIRECTION ( 'NONE',  ( 0.000000000000000000, -0.9126074666063545004, -0.4088369013363783999 ) ) ;
#87405 = CARTESIAN_POINT ( 'NONE',  ( -18.40000000000000213, 33.92263863280957992, -235.0698407953532012 ) ) ;
#87407 = DIRECTION ( 'NONE',  ( 0.000000000000000000, -0.4721928772777242433, -0.8814952561688484955 ) ) ;
#87406 = TOROIDAL_SURFACE ( 'NONE', #162442, 0.2000000000000000111, 0.1000000000000000056 ) ;
#87408 = CARTESIAN_POINT ( 'NONE',  ( 18.44364597020194196, -9.490487317151110602, -174.5579778896838263 ) ) ;
#87409 = AXIS2_PLACEMENT_3D ( 'NONE', #65158, #149861, #104274 ) ;
#87410 = CARTESIAN_POINT ( 'NONE',  ( 20.94999999999999929, 87.48912529308779540, -72.42310748452423752 ) ) ;
#87411 = EDGE_LOOP ( 'NONE', ( #150773, #232740, #89751, #97193 ) ) ;
#87413 = EDGE_CURVE ( 'NONE', #165636, #5450, #242980, .T. ) ;
#87412 = AXIS2_PLACEMENT_3D ( 'NONE', #183363, #46389, #107658 ) ;
#87414 = EDGE_CURVE ( 'NONE', #23909, #56118, #114331, .T. ) ;
#87416 = VERTEX_POINT ( 'NONE', #104722 ) ;
#87415 = ORIENTED_EDGE ( 'NONE', *, *, #238036, .F. ) ;
#87417 = ORIENTED_EDGE ( 'NONE', *, *, #195762, .T. ) ;
#87418 = EDGE_CURVE ( 'NONE', #227800, #115127, #147655, .T. ) ;
#87419 = CARTESIAN_POINT ( 'NONE',  ( 23.15000000000000213, 85.50000000001149658, -45.91707660717669626 ) ) ;
#87420 =( BOUNDED_SURFACE ( )  B_SPLINE_SURFACE ( 3, 2, ( 
 ( #55801, #57095, #217457 ),
 ( #136644, #17985, #98774 ),
 ( #195376, #177099, #79230 ),
 ( #194091, #35035, #58374 ),
 ( #137923, #114534, #15450 ),
 ( #16730, #135360, #214910 ),
 ( #6115, #223877, #103921 ),
 ( #165208, #221307, #220049 ),
 ( #143058, #201759, #42691 ),
 ( #183494, #123517, #244727 ),
 ( #199210, #4820, #122238 ),
 ( #83060, #66105, #222586 ) ),
 .UNSPECIFIED., .F., .F., .F. ) 
 B_SPLINE_SURFACE_WITH_KNOTS ( ( 4, 2, 2, 2, 2, 4 ),
 ( 3, 3 ),
 ( 3.174653483277205090, 3.943930578431714018, 4.713207673586222946, 5.482484768740731873, 5.867123316317986337, 6.251761863895240801 ),
 ( 0.000000000000000000, 1.000000000000000000 ),
 .UNSPECIFIED. ) 
 GEOMETRIC_REPRESENTATION_ITEM ( )  RATIONAL_B_SPLINE_SURFACE ( (
 ( 1.000000000000000000, 0.8659465255642228021, 1.000000000000000000),
 ( 1.000000000000000000, 0.8648614068488911233, 1.000000000000000000),
 ( 1.000000000000000000, 0.8489031841323105843, 1.000000000000000000),
 ( 1.000000000000000000, 0.7927507630162217156, 1.000000000000000000),
 ( 1.000000000000000000, 0.7523013858916698382, 1.000000000000000000),
 ( 1.000000000000000000, 0.6616226951289214675, 1.000000000000000000),
 ( 1.000000000000000000, 0.6112214368573144485, 1.000000000000000000),
 ( 1.000000000000000000, 0.5507684314573975115, 1.000000000000000000),
 ( 1.000000000000000000, 0.5333267243152293169, 1.000000000000000000),
 ( 1.000000000000000000, 0.5084565446480597828, 1.000000000000000000),
 ( 1.000000000000000000, 0.5010722703450565252, 1.000000000000000000),
 ( 1.000000000000000000, 0.5001234037138694299, 1.000000000000000000) ) ) 
 REPRESENTATION_ITEM ( '' )  SURFACE ( )  );
#87421 = DIRECTION ( 'NONE',  ( -0.000000000000000000, 0.4721928772777345684, 0.8814952561688429444 ) ) ;
#87423 = CARTESIAN_POINT ( 'NONE',  ( -17.11825945287482753, 9.950000000011138823, -146.7500000000000284 ) ) ;
#87422 = LINE ( 'NONE', #223085, #99387 ) ;
#87424 = FACE_OUTER_BOUND ( 'NONE', #224210, .T. ) ;
#87425 = ORIENTED_EDGE ( 'NONE', *, *, #113552, .T. ) ;
#87426 = EDGE_CURVE ( 'NONE', #47971, #228818, #85157, .T. ) ;
#87427 = CARTESIAN_POINT ( 'NONE',  ( -21.13422380239050824, -7.589415207398531038E-16, 6.493326514805533911 ) ) ;
#87428 = DIRECTION ( 'NONE',  ( 0.000000000000000000, -0.9118278131605103143, 0.4105728183244983232 ) ) ;
#87429 = EDGE_CURVE ( 'NONE', #17720, #197918, #151779, .T. ) ;
#87430 = FACE_OUTER_BOUND ( 'NONE', #98408, .T. ) ;
#87431 = ORIENTED_EDGE ( 'NONE', *, *, #222375, .F. ) ;
#87432 = AXIS2_PLACEMENT_3D ( 'NONE', #95905, #55467, #97153 ) ;
#87433 = CARTESIAN_POINT ( 'NONE',  ( -18.40000000000000213, 13.88102806299823833, -210.8210490262177359 ) ) ;
#87434 = CYLINDRICAL_SURFACE ( 'NONE', #192286, 0.5000000000000004441 ) ;
#87435 = ORIENTED_EDGE ( 'NONE', *, *, #105893, .F. ) ;
#87436 = VERTEX_POINT ( 'NONE', #34252 ) ;
#87437 = FACE_OUTER_BOUND ( 'NONE', #13296, .T. ) ;
#87438 = DIRECTION ( 'NONE',  ( -0.000000000000000000, -0.9876197685951252359, -0.1568667991644863424 ) ) ;
#87439 = CIRCLE ( 'NONE', #170900, 0.1999999999999996503 ) ;
#87440 = CARTESIAN_POINT ( 'NONE',  ( 23.14999999999999503, 6.650000000011155876, -88.15000000000004832 ) ) ;
#87441 = EDGE_CURVE ( 'NONE', #209609, #691, #171211, .T. ) ;
#87442 = CARTESIAN_POINT ( 'NONE',  ( -18.59999999999999787, 6.933893972137497030, -70.78564583437358237 ) ) ;
#87443 = LINE ( 'NONE', #228264, #6844 ) ;
#87444 = DIRECTION ( 'NONE',  ( 1.000000000000000000, 0.000000000000000000, 0.000000000000000000 ) ) ;
#87445 = ORIENTED_EDGE ( 'NONE', *, *, #185104, .T. ) ;
#87446 = DIRECTION ( 'NONE',  ( 0.000000000000000000, -1.000000000000000000, 0.000000000000000000 ) ) ;
#87447 = CARTESIAN_POINT ( 'NONE',  ( 21.05000000000000071, 11.90759680182680924, -206.0382519879416918 ) ) ;
#87449 = DIRECTION ( 'NONE',  ( -1.000000000000000000, 0.000000000000000000, 0.000000000000000000 ) ) ;
#87448 = CARTESIAN_POINT ( 'NONE',  ( -16.93344882324368683, 9.996588767299030565, -87.91302569480497198 ) ) ;
#87450 = DIRECTION ( 'NONE',  ( 0.7071067811865475727, -0.6824534298470373850, 0.1850873201762208153 ) ) ;
#87451 = EDGE_CURVE ( 'NONE', #229356, #187889, #53778, .T. ) ;
#87452 = CARTESIAN_POINT ( 'NONE',  ( 20.94999999999999929, 65.27628289530476025, -157.8731074845244393 ) ) ;
#87453 = CARTESIAN_POINT ( 'NONE',  ( -20.94999999999999929, -11.74999999998884448, -137.1000000000000227 ) ) ;
#87454 = CIRCLE ( 'NONE', #95809, 0.1000000000000028644 ) ;
#87456 = ORIENTED_EDGE ( 'NONE', *, *, #195356, .T. ) ;
#87455 = CARTESIAN_POINT ( 'NONE',  ( 22.39999999999999503, 29.54900078958455367, -252.7363208912387620 ) ) ;
#87457 = AXIS2_PLACEMENT_3D ( 'NONE', #109923, #91658, #188195 ) ;
#87458 = EDGE_CURVE ( 'NONE', #244617, #257624, #97549, .T. ) ;
#87459 = TOROIDAL_SURFACE ( 'NONE', #233249, 0.6000000000000006439, 0.1000000000000000056 ) ;
#87460 = CIRCLE ( 'NONE', #120822, 0.1000000000000028644 ) ;
#87461 = FACE_OUTER_BOUND ( 'NONE', #68004, .T. ) ;
#87462 = DIRECTION ( 'NONE',  ( 1.000000000000000000, 0.000000000000000000, 0.000000000000000000 ) ) ;
#87463 = DIRECTION ( 'NONE',  ( 0.000000000000000000, -0.2128009952263603954, 0.9770955615653315052 ) ) ;
#87464 = ORIENTED_EDGE ( 'NONE', *, *, #200912, .F. ) ;
#87465 = AXIS2_PLACEMENT_3D ( 'NONE', #100887, #180481, #81336 ) ;
#87466 = DIRECTION ( 'NONE',  ( 0.000000000000000000, 0.2128009952263485993, -0.9770955615653341697 ) ) ;
#87467 = CIRCLE ( 'NONE', #124906, 0.1000000000000028644 ) ;
#87468 = VECTOR ( 'NONE', #53479, 1000.000000000000000 ) ;
#87469 = DIRECTION ( 'NONE',  ( -1.020425574104004196E-15, -6.982962677686266711E-15, 1.000000000000000000 ) ) ;
#87470 = CARTESIAN_POINT ( 'NONE',  ( -18.50000000000000000, 65.70729864261004138, -97.56574559737242680 ) ) ;
#87471 = AXIS2_PLACEMENT_3D ( 'NONE', #245557, #188146, #190743 ) ;
#87472 = CIRCLE ( 'NONE', #50067, 0.1000000000000028644 ) ;
#87473 = ORIENTED_EDGE ( 'NONE', *, *, #201813, .T. ) ;
#87474 = DIRECTION ( 'NONE',  ( 1.000000000000000000, 0.000000000000000000, 0.000000000000000000 ) ) ;
#87476 = EDGE_LOOP ( 'NONE', ( #107951, #227417, #180577, #132572 ) ) ;
#87475 = CARTESIAN_POINT ( 'NONE',  ( -16.82542659449977762, 9.934499891438612451, -188.2553643999739847 ) ) ;
#87477 = CARTESIAN_POINT ( 'NONE',  ( -16.94107738177414291, 63.04990807712500356, -213.0142932718104021 ) ) ;
#87478 = CIRCLE ( 'NONE', #53613, 12.77499999999999503 ) ;
#87479 = DIRECTION ( 'NONE',  ( 0.000000000000000000, 0.000000000000000000, 1.000000000000000000 ) ) ;
#87480 = ORIENTED_EDGE ( 'NONE', *, *, #89774, .T. ) ;
#87481 = DIRECTION ( 'NONE',  ( -0.000000000000000000, -0.9651348961777157509, 0.2617529984165031243 ) ) ;
#87482 = DIRECTION ( 'NONE',  ( 1.000000000000000000, 0.000000000000000000, 0.000000000000000000 ) ) ;
#87483 = CARTESIAN_POINT ( 'NONE',  ( -20.87600722750343252, 65.66887361445314752, -63.93298459182691573 ) ) ;
#87484 = DIRECTION ( 'NONE',  ( 0.000000000000000000, 0.1495327102803792052, -0.9887567792719320625 ) ) ;
#87485 = DIRECTION ( 'NONE',  ( 0.000000000000000000, -6.982962677686266711E-15, 1.000000000000000000 ) ) ;
#87486 = VERTEX_POINT ( 'NONE', #250687 ) ;
#87487 = CARTESIAN_POINT ( 'NONE',  ( 20.94999999999999929, 69.15387683765929694, -99.28538121767448388 ) ) ;
#87488 = CARTESIAN_POINT ( 'NONE',  ( -22.39999999999999858, 0.1000000000111554016, -33.50000000000000000 ) ) ;
#87489 = B_SPLINE_CURVE_WITH_KNOTS ( 'NONE', 3,
 ( #146425, #47326, #208989, #172487, #13369, #34241, #51168, #227262, #171198, #249415, #212853, #48625, #30373, #70795, #193295, #229839, #12103, #147742, #89032, #129457, #112475, #32972, #232432, #113739, #168639, #189439, #248112, #52464, #128176, #14676 ),
 .UNSPECIFIED., .F., .F.,
 ( 4, 2, 2, 2, 2, 2, 2, 2, 2, 2, 2, 2, 2, 2, 4 ),
 ( 0.000000000000000000, 0.0003422764154113352953, 0.0006845528308226705907, 0.001026829246234005778, 0.001369105661645341181, 0.002053658492468005484, 0.002738211323290670220, 0.003080487738702004756, 0.003422764154113338859, 0.003765040569524673829, 0.004107316984936008365, 0.004449593400347343769, 0.004791869815758677438, 0.005134146231170012842, 0.005476422646581347378 ),
 .UNSPECIFIED. ) ;
#87490 = CARTESIAN_POINT ( 'NONE',  ( -23.25000000000000000, -11.38316329222462464, -203.4791315943886048 ) ) ;
#87491 = ORIENTED_EDGE ( 'NONE', *, *, #52682, .T. ) ;
#87492 = VERTEX_POINT ( 'NONE', #30384 ) ;
#87493 = CARTESIAN_POINT ( 'NONE',  ( -23.25000000000000000, 1.115600667400684642E-11, -134.0000000000000000 ) ) ;
#87494 = CIRCLE ( 'NONE', #195874, 0.09999999999999939493 ) ;
#87495 = CARTESIAN_POINT ( 'NONE',  ( 18.49999999999999289, 65.50857864377418593, -44.67310748452439384 ) ) ;
#87496 = SPHERICAL_SURFACE ( 'NONE', #123325, 0.1000000000000000056 ) ;
#87497 = CARTESIAN_POINT ( 'NONE',  ( 21.14999999999999858, 13.07482039728799528, -210.6896000549707537 ) ) ;
#87498 = CARTESIAN_POINT ( 'NONE',  ( 18.50000000000000000, 86.35479209693788505, -176.2665665014505407 ) ) ;
#87499 = EDGE_CURVE ( 'NONE', #41846, #26102, #130748, .T. ) ;
#87501 = DIRECTION ( 'NONE',  ( 1.000000000000000000, 7.304098846218105085E-16, 4.217023435051676515E-16 ) ) ;
#87500 = DIRECTION ( 'NONE',  ( 0.000000000000000000, 1.897661533703519897E-16, -1.000000000000000000 ) ) ;
#87502 = DIRECTION ( 'NONE',  ( 1.000000000000000000, 0.000000000000000000, 0.000000000000000000 ) ) ;
#87503 = CARTESIAN_POINT ( 'NONE',  ( -23.15000000000000213, 1.925233644870967487, -188.2697564668738153 ) ) ;
#87504 = DIRECTION ( 'NONE',  ( 2.952720810173289112E-16, 1.000000000000000000, 6.982962677686266711E-15 ) ) ;
#87505 = LINE ( 'NONE', #246590, #127370 ) ;
#87506 = CIRCLE ( 'NONE', #70807, 0.09999999999998986089 ) ;
#87508 = ORIENTED_EDGE ( 'NONE', *, *, #86287, .T. ) ;
#87507 = CARTESIAN_POINT ( 'NONE',  ( 13.99999999999999822, 9.849999999999981881, -16.74999999999999645 ) ) ;
#87509 = CARTESIAN_POINT ( 'NONE',  ( 21.14250536705908345, 69.48182782313165262, -170.0231074845243882 ) ) ;
#87510 = FACE_OUTER_BOUND ( 'NONE', #85394, .T. ) ;
#87512 = CARTESIAN_POINT ( 'NONE',  ( 23.15000000000000213, -11.64999999998883595, -164.4000000000000057 ) ) ;
#87511 = CARTESIAN_POINT ( 'NONE',  ( 23.15000000000000213, 28.50120599808395028, -258.2149742250584268 ) ) ;
#87513 =( BOUNDED_CURVE ( )  B_SPLINE_CURVE ( 3, ( #179146, #236509, #57860, #117846 ),
 .UNSPECIFIED., .F., .F. ) 
 B_SPLINE_CURVE_WITH_KNOTS ( ( 4, 4 ),
 ( 3.192897208853993085, 4.712388980384689674 ),
 .UNSPECIFIED. ) 
 CURVE ( )  GEOMETRIC_REPRESENTATION_ITEM ( )  RATIONAL_B_SPLINE_CURVE ( ( 1.000000000000000000, 0.8166740347213228279, 0.8166740347213228279, 1.000000000000000000 ) ) 
 REPRESENTATION_ITEM ( '' )  );
#87514 = ORIENTED_EDGE ( 'NONE', *, *, #99196, .T. ) ;
#87515 = LINE ( 'NONE', #49692, #110040 ) ;
#87516 = CARTESIAN_POINT ( 'NONE',  ( -16.87036670365549895, 9.989418819312803066, -113.0204398826979855 ) ) ;
#87517 = CARTESIAN_POINT ( 'NONE',  ( -20.85000000000000142, 76.00000000001244871, -170.0231074845243597 ) ) ;
#87518 = DIRECTION ( 'NONE',  ( -1.073024830501117725E-15, 0.2617529984165031243, 0.9651348961777157509 ) ) ;
#87519 = CARTESIAN_POINT ( 'NONE',  ( 22.59999999999999432, 12.58798907299599001, -223.3278890275437050 ) ) ;
#87520 = EDGE_LOOP ( 'NONE', ( #183102, #126840, #250135, #123329 ) ) ;
#87522 = ORIENTED_EDGE ( 'NONE', *, *, #194495, .F. ) ;
#87521 = AXIS2_PLACEMENT_3D ( 'NONE', #227365, #109980, #48723 ) ;
#87523 = EDGE_CURVE ( 'NONE', #128325, #161509, #155004, .T. ) ;
#87524 = CIRCLE ( 'NONE', #12739, 11.75000000000000000 ) ;
#87525 = CARTESIAN_POINT ( 'NONE',  ( 19.99999999999998934, 31.49702336731128582, -233.4564499823349877 ) ) ;
#87526 = EDGE_LOOP ( 'NONE', ( #181061, #216219, #223680, #58561, #228717, #37980 ) ) ;
#87527 = DIRECTION ( 'NONE',  ( 0.000000000000000000, 0.9126074666063773710, 0.4088369013363274962 ) ) ;
#87528 = ORIENTED_EDGE ( 'NONE', *, *, #6673, .T. ) ;
#87529 = CIRCLE ( 'NONE', #29323, 0.09999999999999971412 ) ;
#87530 = DIRECTION ( 'NONE',  ( 1.000000000000000000, 0.000000000000000000, 0.000000000000000000 ) ) ;
#87531 = DIRECTION ( 'NONE',  ( 0.000000000000000000, 0.000000000000000000, -1.000000000000000000 ) ) ;
#87532 = ADVANCED_FACE ( 'NONE', ( #95469 ), #251976, .T. ) ;
#87534 = EDGE_CURVE ( 'NONE', #153680, #43270, #173787, .T. ) ;
#87533 = DIRECTION ( 'NONE',  ( 1.000000000000000000, 0.000000000000000000, 0.000000000000000000 ) ) ;
#87535 = EDGE_LOOP ( 'NONE', ( #121710, #131009, #135672, #203163 ) ) ;
#87536 = EDGE_CURVE ( 'NONE', #38206, #33088, #193464, .T. ) ;
#87537 = CARTESIAN_POINT ( 'NONE',  ( -20.64999999999999858, 74.00000000001223555, -149.7477294072864709 ) ) ;
#87538 = CARTESIAN_POINT ( 'NONE',  ( -21.05000000000000071, 65.55628185913181483, -241.9744003048582215 ) ) ;
#87539 = CARTESIAN_POINT ( 'NONE',  ( -18.55807992284872299, 68.10318897902124036, -224.1464165264002588 ) ) ;
#87540 = DIRECTION ( 'NONE',  ( -1.000000000000000000, 0.000000000000000000, 0.000000000000000000 ) ) ;
#87541 = DIRECTION ( 'NONE',  ( 1.734723475976817507E-14, -6.982962677686266711E-15, 1.000000000000000000 ) ) ;
#87542 = DIRECTION ( 'NONE',  ( 1.000000000000000000, 0.000000000000000000, 0.000000000000000000 ) ) ;
#87543 = EDGE_CURVE ( 'NONE', #161554, #21663, #210300, .T. ) ;
#87544 = CIRCLE ( 'NONE', #229233, 0.1999999999999997335 ) ;
#87545 = DIRECTION ( 'NONE',  ( 1.000000000000000000, 0.000000000000000000, 0.000000000000000000 ) ) ;
#87546 = VERTEX_POINT ( 'NONE', #73378 ) ;
#87548 = CARTESIAN_POINT ( 'NONE',  ( -22.47886152344871036, 75.96249906115107819, -215.1730961275723075 ) ) ;
#87547 = CARTESIAN_POINT ( 'NONE',  ( -16.97683809663752186, 66.05000000001207638, -123.1207434663278804 ) ) ;
#87549 = ORIENTED_EDGE ( 'NONE', *, *, #122678, .T. ) ;
#87551 = ORIENTED_EDGE ( 'NONE', *, *, #203800, .T. ) ;
#87550 = DIRECTION ( 'NONE',  ( 0.000000000000000000, 0.000000000000000000, -1.000000000000000000 ) ) ;
#87552 = VERTEX_POINT ( 'NONE', #209002 ) ;
#87553 = FACE_OUTER_BOUND ( 'NONE', #107555, .T. ) ;
#87554 = EDGE_CURVE ( 'NONE', #179043, #78788, #183169, .T. ) ;
#87555 = CARTESIAN_POINT ( 'NONE',  ( -18.59999999999999787, 43.63140573099096287, -239.9077968784524444 ) ) ;
#87556 = DIRECTION ( 'NONE',  ( -1.000000000000000000, -0.000000000000000000, -0.000000000000000000 ) ) ;
#87557 = CARTESIAN_POINT ( 'NONE',  ( 21.05000000000000071, 65.51540711881749246, -129.0663939139408285 ) ) ;
#87558 = EDGE_LOOP ( 'NONE', ( #79946, #7373 ) ) ;
#87559 = LINE ( 'NONE', #148854, #30743 ) ;
#87560 = CARTESIAN_POINT ( 'NONE',  ( -18.50000000000000000, 8.882751598337863541, -187.0399955572217721 ) ) ;
#87561 = VERTEX_POINT ( 'NONE', #154216 ) ;
#87563 = EDGE_CURVE ( 'NONE', #110507, #165216, #189449, .T. ) ;
#87562 = CYLINDRICAL_SURFACE ( 'NONE', #69223, 0.1000000000000028644 ) ;
#87564 = VECTOR ( 'NONE', #45239, 1000.000000000000114 ) ;
#87565 = AXIS2_PLACEMENT_3D ( 'NONE', #122755, #204, #241408 ) ;
#87566 = TOROIDAL_SURFACE ( 'NONE', #112535, 11.65000000000000036, 0.1000000000000000056 ) ;
#87568 = AXIS2_PLACEMENT_3D ( 'NONE', #232767, #33308, #155808 ) ;
#87567 = CARTESIAN_POINT ( 'NONE',  ( 18.59999999999999787, -10.35479209692539548, -27.25654098307376216 ) ) ;
#87569 = VERTEX_POINT ( 'NONE', #150329 ) ;
#87570 = LINE ( 'NONE', #230975, #101794 ) ;
#87571 = VERTEX_POINT ( 'NONE', #233718 ) ;
#87572 = AXIS2_PLACEMENT_3D ( 'NONE', #71166, #232808, #209368 ) ;
#87573 = CARTESIAN_POINT ( 'NONE',  ( 21.14999999999999858, 41.42187432231294508, -260.1830396872097140 ) ) ;
#87574 = EDGE_LOOP ( 'NONE', ( #150963, #34732, #3434, #102350 ) ) ;
#87575 = DIRECTION ( 'NONE',  ( 0.000000000000000000, 1.000000000000000000, 0.000000000000000000 ) ) ;
#87576 = CARTESIAN_POINT ( 'NONE',  ( 20.99749315643147440, 64.25000000001175238, -76.53791325328415951 ) ) ;
#87577 = CARTESIAN_POINT ( 'NONE',  ( 21.04999999999999716, 76.03753606329739512, -75.85537975845998915 ) ) ;
#87578 = CARTESIAN_POINT ( 'NONE',  ( -21.64999999999999858, 11.70367352607683564, -220.1991933683510467 ) ) ;
#87579 = CIRCLE ( 'NONE', #95952, 7.899999999999990585 ) ;
#87580 = VECTOR ( 'NONE', #234282, 1000.000000000000000 ) ;
#87581 = FACE_OUTER_BOUND ( 'NONE', #79094, .T. ) ;
#87582 = DIRECTION ( 'NONE',  ( 0.000000000000000000, 1.000000000000000000, 0.000000000000000000 ) ) ;
#87583 = CARTESIAN_POINT ( 'NONE',  ( 20.91682497891422798, 10.32263460347359363, -72.56059579686719019 ) ) ;
#87584 = ORIENTED_EDGE ( 'NONE', *, *, #116209, .F. ) ;
#87586 = LINE ( 'NONE', #189289, #146110 ) ;
#87585 = CARTESIAN_POINT ( 'NONE',  ( 20.73486653747088582, 68.75000000001229239, -160.7731074845244166 ) ) ;
#87587 = ADVANCED_FACE ( 'NONE', ( #51179 ), #31684, .F. ) ;
#87588 = ORIENTED_EDGE ( 'NONE', *, *, #201878, .T. ) ;
#87589 = EDGE_CURVE ( 'NONE', #229059, #112606, #118446, .T. ) ;
#87590 = LINE ( 'NONE', #101021, #151394 ) ;
#87591 = LINE ( 'NONE', #88873, #251881 ) ;
#87592 = DIRECTION ( 'NONE',  ( 0.000000000000000000, -1.000000000000000000, 0.000000000000000000 ) ) ;
#87594 = VERTEX_POINT ( 'NONE', #91625 ) ;
#87593 = CARTESIAN_POINT ( 'NONE',  ( -18.58744394320977378, -9.566385154537556446, -207.8228480538757594 ) ) ;
#87596 = ORIENTED_EDGE ( 'NONE', *, *, #57661, .F. ) ;
#87595 = CARTESIAN_POINT ( 'NONE',  ( -20.94999999999999929, 7.070967871798842452, -37.24656422186831151 ) ) ;
#87597 = EDGE_CURVE ( 'NONE', #172515, #147359, #211580, .T. ) ;
#87599 = ADVANCED_FACE ( 'NONE', ( #39389 ), #178905, .F. ) ;
#87598 = LINE ( 'NONE', #216210, #67355 ) ;
#87600 = DIRECTION ( 'NONE',  ( -1.000000000000000000, 0.000000000000000000, 0.000000000000000000 ) ) ;
#87602 = EDGE_LOOP ( 'NONE', ( #233732, #148659, #116362, #139460, #188482, #225935, #199639, #149033, #29799, #174093, #123065, #95039, #191473, #157104, #114325, #130082, #33469, #159351 ) ) ;
#87601 = LINE ( 'NONE', #28983, #3074 ) ;
#87603 = ADVANCED_FACE ( 'NONE', ( #217964 ), #56048, .T. ) ;
#87604 = VECTOR ( 'NONE', #25395, 1000.000000000000000 ) ;
#87605 = EDGE_CURVE ( 'NONE', #159875, #58200, #18479, .T. ) ;
#87606 = EDGE_CURVE ( 'NONE', #105369, #5646, #51762, .T. ) ;
#87607 = DIRECTION ( 'NONE',  ( 0.000000000000000000, 0.000000000000000000, -1.000000000000000000 ) ) ;
#87608 = DIRECTION ( 'NONE',  ( -1.000000000000000000, 0.000000000000000000, 0.000000000000000000 ) ) ;
#87609 = ORIENTED_EDGE ( 'NONE', *, *, #124061, .T. ) ;
#87610 = DIRECTION ( 'NONE',  ( 1.000000000000000000, 0.000000000000000000, 0.000000000000000000 ) ) ;
#87611 = ORIENTED_EDGE ( 'NONE', *, *, #118019, .T. ) ;
#87612 = EDGE_CURVE ( 'NONE', #132438, #226125, #58411, .T. ) ;
#87613 = AXIS2_PLACEMENT_3D ( 'NONE', #127552, #70172, #89689 ) ;
#87614 = LINE ( 'NONE', #151488, #232497 ) ;
#87615 = DIRECTION ( 'NONE',  ( 1.000000000000000000, 0.000000000000000000, 0.000000000000000000 ) ) ;
#87616 = ORIENTED_EDGE ( 'NONE', *, *, #197486, .T. ) ;
#87617 = FACE_OUTER_BOUND ( 'NONE', #2959, .T. ) ;
#87618 = ADVANCED_FACE ( 'NONE', ( #100575 ), #226753, .T. ) ;
#87619 = CARTESIAN_POINT ( 'NONE',  ( 20.94999999999999929, -8.999999999988844479, -143.8939691226524644 ) ) ;
#87620 = ORIENTED_EDGE ( 'NONE', *, *, #131989, .T. ) ;
#87621 = EDGE_CURVE ( 'NONE', #76842, #77103, #185062, .T. ) ;
#87622 = AXIS2_PLACEMENT_3D ( 'NONE', #89466, #248550, #127328 ) ;
#87623 = CARTESIAN_POINT ( 'NONE',  ( -18.59999999999999787, 3.912899247244609580, -145.4818229730109920 ) ) ;
#87624 = AXIS2_PLACEMENT_3D ( 'NONE', #86914, #227724, #107784 ) ;
#87625 = EDGE_CURVE ( 'NONE', #72694, #89956, #251707, .T. ) ;
#87626 = ORIENTED_EDGE ( 'NONE', *, *, #20164, .F. ) ;
#87627 = ORIENTED_EDGE ( 'NONE', *, *, #63780, .F. ) ;
#87628 = CARTESIAN_POINT ( 'NONE',  ( -18.43459694179558284, -9.494210124986880217, -73.61700520266094827 ) ) ;
#87629 = CIRCLE ( 'NONE', #250157, 11.75000000000000000 ) ;
#87630 = ORIENTED_EDGE ( 'NONE', *, *, #104793, .T. ) ;
#87631 = CARTESIAN_POINT ( 'NONE',  ( 18.59999999999999787, -0.7124699236739290287, -242.4838055749970351 ) ) ;
#87632 = ORIENTED_EDGE ( 'NONE', *, *, #43437, .T. ) ;
#87634 = ORIENTED_EDGE ( 'NONE', *, *, #94478, .T. ) ;
#87633 = FACE_OUTER_BOUND ( 'NONE', #173847, .T. ) ;
#87635 = EDGE_CURVE ( 'NONE', #76480, #72649, #201810, .T. ) ;
#87636 = EDGE_CURVE ( 'NONE', #65743, #66990, #137168, .T. ) ;
#87637 = AXIS2_PLACEMENT_3D ( 'NONE', #117641, #195913, #57647 ) ;
#87638 = CIRCLE ( 'NONE', #8552, 0.09999999999999735489 ) ;
#87639 = DIRECTION ( 'NONE',  ( 1.000000000000000000, 0.000000000000000000, 0.000000000000000000 ) ) ;
#87640 = ORIENTED_EDGE ( 'NONE', *, *, #88560, .T. ) ;
#87641 = DIRECTION ( 'NONE',  ( 1.000000000000000000, 0.000000000000000000, 0.000000000000000000 ) ) ;
#87642 = ORIENTED_EDGE ( 'NONE', *, *, #144235, .F. ) ;
#87645 = EDGE_LOOP ( 'NONE', ( #218505, #107269, #170274, #46653 ) ) ;
#87644 = ORIENTED_EDGE ( 'NONE', *, *, #230383, .F. ) ;
#87643 = CARTESIAN_POINT ( 'NONE',  ( -16.94037747912386394, 65.98646061752525327, -56.97197652654890021 ) ) ;
#87646 = FACE_OUTER_BOUND ( 'NONE', #119883, .T. ) ;
#87647 = DIRECTION ( 'NONE',  ( 0.000000000000000000, 0.06835365183351375939, -0.9976611540402997580 ) ) ;
#87648 = EDGE_LOOP ( 'NONE', ( #156581, #178968, #56054, #31787 ) ) ;
#87649 = AXIS2_PLACEMENT_3D ( 'NONE', #62169, #36202, #195281 ) ;
#87650 = AXIS2_PLACEMENT_3D ( 'NONE', #23818, #85010, #125463 ) ;
#87651 = AXIS2_PLACEMENT_3D ( 'NONE', #145833, #105402, #68899 ) ;
#87652 = AXIS2_PLACEMENT_3D ( 'NONE', #250671, #255452, #61157 ) ;
#87653 = CIRCLE ( 'NONE', #233446, 2.700000000000001066 ) ;
#87654 = ORIENTED_EDGE ( 'NONE', *, *, #53357, .T. ) ;
#87655 = FACE_OUTER_BOUND ( 'NONE', #166794, .T. ) ;
#87656 = DIRECTION ( 'NONE',  ( 0.000000000000000000, 6.982962677686267499E-15, -1.000000000000000000 ) ) ;
#87658 = EDGE_LOOP ( 'NONE', ( #10740, #108781, #40130 ) ) ;
#87657 = DIRECTION ( 'NONE',  ( 0.000000000000000000, 1.734723475976817507E-14, -1.000000000000000000 ) ) ;
#87659 = CYLINDRICAL_SURFACE ( 'NONE', #23157, 4.049999999999995381 ) ;
#87660 = VERTEX_POINT ( 'NONE', #219264 ) ;
#87661 = CARTESIAN_POINT ( 'NONE',  ( -23.25000000000000000, 74.00000000001205080, -123.2984855617622060 ) ) ;
#87662 = CYLINDRICAL_SURFACE ( 'NONE', #256283, 0.1000000000000028644 ) ;
#87663 = VERTEX_POINT ( 'NONE', #1499 ) ;
#87664 = DIRECTION ( 'NONE',  ( 0.000000000000000000, 4.163336342344333240E-14, -1.000000000000000000 ) ) ;
#87665 = AXIS2_PLACEMENT_3D ( 'NONE', #146052, #100791, #66535 ) ;
#87666 = CARTESIAN_POINT ( 'NONE',  ( 20.73486653747088582, 62.65526179112259086, -225.0299194783148664 ) ) ;
#87668 = ORIENTED_EDGE ( 'NONE', *, *, #34162, .F. ) ;
#87667 = B_SPLINE_CURVE_WITH_KNOTS ( 'NONE', 3,
 ( #38840, #79214, #942, #218722, #20568, #100051, #179639, #160081, #120958, #200472, #21837, #101307, #180910, #85611, #148190, #105165, #23136, #246016, #64797 ),
 .UNSPECIFIED., .F., .F.,
 ( 4, 3, 3, 3, 3, 3, 4 ),
 ( 0.000000000000000000, 7.110282409890261485E-05, 0.0001508797727291307672, 0.0002027344179858337034, 0.0002343294522348885335, 0.0002454816334821149936, 0.0002619873080085548971 ),
 .UNSPECIFIED. ) ;
#87670 = ORIENTED_EDGE ( 'NONE', *, *, #251975, .T. ) ;
#87669 = FACE_OUTER_BOUND ( 'NONE', #148703, .T. ) ;
#87672 = EDGE_LOOP ( 'NONE', ( #16371, #48737, #193166, #183540 ) ) ;
#87671 = ORIENTED_EDGE ( 'NONE', *, *, #128569, .T. ) ;
#87673 = VERTEX_POINT ( 'NONE', #160617 ) ;
#87674 = CARTESIAN_POINT ( 'NONE',  ( 18.54999999999999716, 9.950000000011153034, -154.8500000000000796 ) ) ;
#87675 = EDGE_LOOP ( 'NONE', ( #154070, #95145, #3394, #246875 ) ) ;
#87676 = DIRECTION ( 'NONE',  ( 0.000000000000000000, 6.982962677686266711E-15, -1.000000000000000000 ) ) ;
#87677 = VERTEX_POINT ( 'NONE', #257064 ) ;
#87678 = CYLINDRICAL_SURFACE ( 'NONE', #94033, 0.1000000000000028644 ) ;
#87679 = DIRECTION ( 'NONE',  ( -0.000000000000000000, 1.000000000000000000, 7.172728831056617961E-15 ) ) ;
#87680 = ORIENTED_EDGE ( 'NONE', *, *, #25799, .F. ) ;
#87681 = ADVANCED_FACE ( 'NONE', ( #81025 ), #216704, .T. ) ;
#87682 = AXIS2_PLACEMENT_3D ( 'NONE', #66190, #246119, #165287 ) ;
#87683 = ORIENTED_EDGE ( 'NONE', *, *, #139127, .F. ) ;
#87684 = EDGE_CURVE ( 'NONE', #232784, #493, #52435, .T. ) ;
#87685 = B_SPLINE_CURVE_WITH_KNOTS ( 'NONE', 3,
 ( #168887, #30640, #248381, #151878 ),
 .UNSPECIFIED., .F., .F.,
 ( 4, 4 ),
 ( 0.000000000000000000, 0.0002118541922231799543 ),
 .UNSPECIFIED. ) ;
#87686 = ORIENTED_EDGE ( 'NONE', *, *, #235472, .F. ) ;
#87687 = AXIS2_PLACEMENT_3D ( 'NONE', #222322, #5857, #202790 ) ;
#87688 = ADVANCED_FACE ( 'NONE', ( #221815, #241418 ), #2777, .T. ) ;
#87689 = DIRECTION ( 'NONE',  ( 0.000000000000000000, -0.000000000000000000, 1.000000000000000000 ) ) ;
#87690 = ADVANCED_FACE ( 'NONE', ( #48338 ), #207437, .T. ) ;
#87691 = ORIENTED_EDGE ( 'NONE', *, *, #59752, .F. ) ;
#87692 = CARTESIAN_POINT ( 'NONE',  ( -18.59999999999999787, 11.65000000001115232, -45.65000000000000568 ) ) ;
#87694 = ORIENTED_EDGE ( 'NONE', *, *, #119658, .F. ) ;
#87693 = FACE_OUTER_BOUND ( 'NONE', #205026, .T. ) ;
#87695 = CARTESIAN_POINT ( 'NONE',  ( -20.94999999999999929, -12.41227409413852811, -64.00000000000000000 ) ) ;
#87696 = DIRECTION ( 'NONE',  ( 1.000000000000000000, -0.000000000000000000, -0.000000000000000000 ) ) ;
#87697 = FACE_OUTER_BOUND ( 'NONE', #183816, .T. ) ;
#87698 = CARTESIAN_POINT ( 'NONE',  ( -18.42554971533676778, 85.49715966945035461, -196.4832805709756656 ) ) ;
#87699 = AXIS2_PLACEMENT_3D ( 'NONE', #49860, #9453, #214080 ) ;
#87701 = DIRECTION ( 'NONE',  ( 3.265361837132813093E-16, -1.000000000000000000, -0.000000000000000000 ) ) ;
#87700 = CARTESIAN_POINT ( 'NONE',  ( -23.15000000000000213, 28.50120599808395028, -258.2149742250584268 ) ) ;
#87702 = CARTESIAN_POINT ( 'NONE',  ( -20.85000000000000142, 69.15387683765929694, -99.28538121767448388 ) ) ;
#87703 = CARTESIAN_POINT ( 'NONE',  ( 18.59999999999999076, 7.070967871809997973, -171.2465642218683115 ) ) ;
#87704 = CARTESIAN_POINT ( 'NONE',  ( -21.59142135623730852, 7.850000000011158718, -146.3500000000000227 ) ) ;
#87705 = AXIS2_PLACEMENT_3D ( 'NONE', #69192, #190418, #189114 ) ;
#87706 = ORIENTED_EDGE ( 'NONE', *, *, #217126, .T. ) ;
#87707 = TOROIDAL_SURFACE ( 'NONE', #233501, 0.2000000000000000111, 0.1000000000000000056 ) ;
#87708 = ADVANCED_FACE ( 'NONE', ( #86151 ), #142298, .T. ) ;
#87709 = TOROIDAL_SURFACE ( 'NONE', #21122, 0.2000000000000000111, 0.1000000000000000056 ) ;
#87710 = ORIENTED_EDGE ( 'NONE', *, *, #44094, .T. ) ;
#87712 = ORIENTED_EDGE ( 'NONE', *, *, #125617, .T. ) ;
#87711 = DIRECTION ( 'NONE',  ( 0.000000000000000000, -1.000000000000000000, 0.000000000000000000 ) ) ;
#87713 = ORIENTED_EDGE ( 'NONE', *, *, #246795, .F. ) ;
#87714 = CARTESIAN_POINT ( 'NONE',  ( 23.50000000000005684, 64.25000000001119815, -51.02310748452479316 ) ) ;
#87715 = CARTESIAN_POINT ( 'NONE',  ( 20.73486653747090003, 7.250000000011182166, -121.3500000000000227 ) ) ;
#87717 = CARTESIAN_POINT ( 'NONE',  ( 21.05000000000000071, 71.18691588786300883, -181.9646252410481964 ) ) ;
#87716 = CARTESIAN_POINT ( 'NONE',  ( -18.59999999999999787, 64.40000000001161595, -62.59490425424885274 ) ) ;
#87718 = ORIENTED_EDGE ( 'NONE', *, *, #214896, .T. ) ;
#87719 = SURFACE_SIDE_STYLE ('',( #244226 ) ) ;
#87720 = ADVANCED_FACE ( 'NONE', ( #246535 ), #177578, .T. ) ;
#87721 = DIRECTION ( 'NONE',  ( 0.000000000000000000, 1.000000000000000000, 0.000000000000000000 ) ) ;
#87722 = AXIS2_PLACEMENT_3D ( 'NONE', #208563, #226815, #127733 ) ;
#87723 = EDGE_CURVE ( 'NONE', #18470, #114980, #114992, .T. ) ;
#87724 = LINE ( 'NONE', #168621, #153958 ) ;
#87725 = ORIENTED_EDGE ( 'NONE', *, *, #251258, .F. ) ;
#87726 = DIRECTION ( 'NONE',  ( 0.000000000000000000, 0.9274965247785529332, 0.3738317757009255171 ) ) ;
#87727 = CARTESIAN_POINT ( 'NONE',  ( -16.79139129368503802, 9.944944162472834748, -180.1702446328257849 ) ) ;
#87728 = CARTESIAN_POINT ( 'NONE',  ( 21.00000000000000000, 66.25000000001253397, -182.3731074845244393 ) ) ;
#87729 = CARTESIAN_POINT ( 'NONE',  ( 20.95262331984758575, 65.49584273722187788, -61.96221915493101307 ) ) ;
#87730 = CARTESIAN_POINT ( 'NONE',  ( -21.14999999999999858, 64.25000000001232081, -163.2392418215462726 ) ) ;
#87732 = ORIENTED_EDGE ( 'NONE', *, *, #70967, .F. ) ;
#87731 = CARTESIAN_POINT ( 'NONE',  ( -20.85000000000000142, 67.49222854868494892, -195.4187676019683693 ) ) ;
#87733 = CARTESIAN_POINT ( 'NONE',  ( 22.88900146558018989, 8.703904791123973084, -42.75000000000000000 ) ) ;
#87734 = EDGE_CURVE ( 'NONE', #217025, #149752, #219031, .T. ) ;
#87735 = CARTESIAN_POINT ( 'NONE',  ( 20.85000000000000142, 14.86477715130881272, -235.7932433709592601 ) ) ;
#87736 = FACE_OUTER_BOUND ( 'NONE', #197723, .T. ) ;
#87737 = CARTESIAN_POINT ( 'NONE',  ( 18.49999999999997868, 85.32100840337321301, -95.78716923544641304 ) ) ;
#87738 = ORIENTED_EDGE ( 'NONE', *, *, #127080, .F. ) ;
#87739 = DIRECTION ( 'NONE',  ( 0.000000000000000000, -6.467318590049456648E-15, 1.000000000000000000 ) ) ;
#87740 = EDGE_CURVE ( 'NONE', #211554, #252276, #23446, .T. ) ;
#87741 = CARTESIAN_POINT ( 'NONE',  ( -20.64999999999999858, 7.250000000011155521, -179.7499999999999716 ) ) ;
#87742 = AXIS2_PLACEMENT_3D ( 'NONE', #46506, #145607, #169078 ) ;
#87745 = DIRECTION ( 'NONE',  ( 1.000000000000000000, 7.304098846218133681E-16, -4.607487905232622991E-31 ) ) ;
#87744 = AXIS2_PLACEMENT_3D ( 'NONE', #148420, #183696, #186264 ) ;
#87743 = DIRECTION ( 'NONE',  ( -2.952720810173289112E-16, 1.000000000000000000, 0.000000000000000000 ) ) ;
#87746 = CARTESIAN_POINT ( 'NONE',  ( 20.94999999999999929, 10.72371710471867701, -74.66491356908764487 ) ) ;
#87747 = DIRECTION ( 'NONE',  ( 0.000000000000000000, -0.9553114395363127009, 0.2956011730204364252 ) ) ;
#87748 = CIRCLE ( 'NONE', #220847, 0.1000000000000106498 ) ;
#87750 = EDGE_CURVE ( 'NONE', #215192, #181648, #169183, .T. ) ;
#87749 = CARTESIAN_POINT ( 'NONE',  ( 23.24999999999999645, 70.40000000001207070, -124.1178414656112352 ) ) ;
#87751 = LINE ( 'NONE', #167334, #131143 ) ;
#87752 = CARTESIAN_POINT ( 'NONE',  ( -23.15000000000000213, 66.26558728512915764, -222.7970849955717938 ) ) ;
#87753 = CARTESIAN_POINT ( 'NONE',  ( -16.80117486205003630, 9.949657268323468529, -87.84885487292552853 ) ) ;
#87754 = ORIENTED_EDGE ( 'NONE', *, *, #59711, .F. ) ;
#87755 = AXIS2_PLACEMENT_3D ( 'NONE', #66986, #202639, #104791 ) ;
#87756 = ORIENTED_EDGE ( 'NONE', *, *, #143802, .T. ) ;
#87757 = EDGE_LOOP ( 'NONE', ( #142705, #62631, #57897, #166218 ) ) ;
#87758 = DIRECTION ( 'NONE',  ( 1.000000000000000000, 0.000000000000000000, 0.000000000000000000 ) ) ;
#87759 = LINE ( 'NONE', #232450, #206838 ) ;
#87760 = EDGE_LOOP ( 'NONE', ( #62320, #81220, #55432, #18981, #150018, #15614, #227539, #44282, #204434, #250554, #198993, #27424, #117096, #237474 ) ) ;
#87761 = EDGE_CURVE ( 'NONE', #11395, #63728, #94139, .T. ) ;
#87762 = ORIENTED_EDGE ( 'NONE', *, *, #70850, .F. ) ;
#87763 = EDGE_CURVE ( 'NONE', #132550, #80211, #204832, .T. ) ;
#87764 = ORIENTED_EDGE ( 'NONE', *, *, #1364, .T. ) ;
#87765 = CARTESIAN_POINT ( 'NONE',  ( -18.59999999999999787, -1.835859311432481045, -112.0044391687985694 ) ) ;
#87766 = VERTEX_POINT ( 'NONE', #24952 ) ;
#87767 = DIRECTION ( 'NONE',  ( 1.000000000000000000, 0.000000000000000000, 0.000000000000000000 ) ) ;
#87768 = CARTESIAN_POINT ( 'NONE',  ( 21.05000000000000071, 20.66107731230508548, -234.7421556583769302 ) ) ;
#87769 = CARTESIAN_POINT ( 'NONE',  ( -21.07933241753356413, 1.594255136103273296, -230.6620461068241923 ) ) ;
#87770 = CARTESIAN_POINT ( 'NONE',  ( 21.05000000000000071, 76.00000000001213607, -136.5231074845243313 ) ) ;
#87771 = DIRECTION ( 'NONE',  ( 0.000000000000000000, 1.000000000000000000, -3.469446951953635015E-14 ) ) ;
#87773 = ORIENTED_EDGE ( 'NONE', *, *, #240521, .F. ) ;
#87772 = CARTESIAN_POINT ( 'NONE',  ( 21.09546886439575886, 44.19670749624917505, -236.4455533064239319 ) ) ;
#87775 = DIRECTION ( 'NONE',  ( -1.000000000000000000, -0.000000000000000000, 0.000000000000000000 ) ) ;
#87774 = LINE ( 'NONE', #85188, #92085 ) ;
#87777 = CYLINDRICAL_SURFACE ( 'NONE', #48565, 0.5000000000000004441 ) ;
#87776 = AXIS2_PLACEMENT_3D ( 'NONE', #83943, #162270, #222192 ) ;
#87778 = ORIENTED_EDGE ( 'NONE', *, *, #107926, .F. ) ;
#87779 = DIRECTION ( 'NONE',  ( 0.000000000000000000, -0.9126074666063660468, -0.4088369013363524762 ) ) ;
#87780 = CARTESIAN_POINT ( 'NONE',  ( -14.45443560709635911, 9.450592112144855506, -115.5561883188084096 ) ) ;
#87781 = CARTESIAN_POINT ( 'NONE',  ( -23.15000000000000213, 73.40000000001181490, -82.74772940728642823 ) ) ;
#87782 = EDGE_LOOP ( 'NONE', ( #32832, #228140, #30054, #111504 ) ) ;
#87783 = CIRCLE ( 'NONE', #225142, 0.09999999999999939493 ) ;
#87784 = DIRECTION ( 'NONE',  ( 1.000000000000000000, 0.000000000000000000, -0.000000000000000000 ) ) ;
#87785 = CIRCLE ( 'NONE', #46104, 0.09999999999999939493 ) ;
#87786 = CARTESIAN_POINT ( 'NONE',  ( -16.87998658237740912, 66.05000000001182059, -82.38674705226230799 ) ) ;
#87787 = ORIENTED_EDGE ( 'NONE', *, *, #140070, .F. ) ;
#87788 = CARTESIAN_POINT ( 'NONE',  ( 21.00000000000000000, 9.749999999999998224, -21.25000000000000000 ) ) ;
#87790 = CARTESIAN_POINT ( 'NONE',  ( -23.15000000000000213, 76.00000000001193712, -106.9231074845242944 ) ) ;
#87789 = AXIS2_PLACEMENT_3D ( 'NONE', #116352, #56342, #115056 ) ;
#87791 = DIRECTION ( 'NONE',  ( -0.000000000000000000, -0.000000000000000000, -1.000000000000000000 ) ) ;
#87792 = ORIENTED_EDGE ( 'NONE', *, *, #183077, .F. ) ;
#87793 = ORIENTED_EDGE ( 'NONE', *, *, #180063, .F. ) ;
#87794 = DIRECTION ( 'NONE',  ( 0.000000000000000000, 0.000000000000000000, 1.000000000000000000 ) ) ;
#87795 = CARTESIAN_POINT ( 'NONE',  ( 21.05000000000000071, 10.48443348965288990, -40.95680580149191030 ) ) ;
#87796 = CARTESIAN_POINT ( 'NONE',  ( -21.05000000000000071, 77.83534155023700407, -191.9679561919613491 ) ) ;
#87797 = EDGE_CURVE ( 'NONE', #205018, #12615, #182736, .T. ) ;
#87798 = CARTESIAN_POINT ( 'NONE',  ( -21.05000000000000071, 1.162701749949165642, -41.50000000000000000 ) ) ;
#87799 = CARTESIAN_POINT ( 'NONE',  ( -18.50000000000000000, 42.94327155031035659, -233.8606566173841372 ) ) ;
#87801 = CARTESIAN_POINT ( 'NONE',  ( -20.12071067811865888, 9.320710678129810134, -79.35000000000005116 ) ) ;
#87800 = CIRCLE ( 'NONE', #104551, 0.1999999999999945155 ) ;
#87802 = ORIENTED_EDGE ( 'NONE', *, *, #148203, .T. ) ;
#87803 = DIRECTION ( 'NONE',  ( -0.000000000000000000, 0.000000000000000000, 1.000000000000000000 ) ) ;
#87804 = AXIS2_PLACEMENT_3D ( 'NONE', #218100, #240266, #39521 ) ;
#87806 = ORIENTED_EDGE ( 'NONE', *, *, #91931, .F. ) ;
#87805 = CARTESIAN_POINT ( 'NONE',  ( -23.15000000000000213, 76.00000000001213607, -136.5231074845243313 ) ) ;
#87807 = DIRECTION ( 'NONE',  ( 0.000000000000000000, 1.000000000000000000, 0.000000000000000000 ) ) ;
#87808 = CARTESIAN_POINT ( 'NONE',  ( -16.80621392010908011, 66.05779742250405207, -90.33351551910763533 ) ) ;
#87809 = CYLINDRICAL_SURFACE ( 'NONE', #71220, 0.09999999999999939493 ) ;
#87810 = CARTESIAN_POINT ( 'NONE',  ( -16.87998658237755834, 66.05000000001207638, -123.6594679167868236 ) ) ;
#87811 = EDGE_CURVE ( 'NONE', #88928, #13286, #56691, .T. ) ;
#87813 = ORIENTED_EDGE ( 'NONE', *, *, #144447, .T. ) ;
#87812 = CARTESIAN_POINT ( 'NONE',  ( -23.25000000000000000, 4.350000000011156054, -54.84999999999999432 ) ) ;
#87814 = CARTESIAN_POINT ( 'NONE',  ( -18.39999999999999858, -9.682403433465239573, -174.1568433774127982 ) ) ;
#87815 = CARTESIAN_POINT ( 'NONE',  ( -23.15000000000000213, 76.00000000001156764, -56.74810748452433273 ) ) ;
#87816 = CARTESIAN_POINT ( 'NONE',  ( -23.15000000000000213, 76.00000000001237765, -170.0231074845243597 ) ) ;
#87817 = CARTESIAN_POINT ( 'NONE',  ( -21.14999999999999858, 64.27847795353595473, -247.1247091181747066 ) ) ;
#87818 = ORIENTED_EDGE ( 'NONE', *, *, #218833, .F. ) ;
#87819 = CARTESIAN_POINT ( 'NONE',  ( 18.49999999999996803, 67.75954444190071513, -227.8703747234148693 ) ) ;
#87820 = CARTESIAN_POINT ( 'NONE',  ( -16.80070461187894892, 66.05000000001203375, -115.6700713136833798 ) ) ;
#87821 = ADVANCED_FACE ( 'NONE', ( #26228 ), #206137, .F. ) ;
#87822 = EDGE_CURVE ( 'NONE', #44761, #128947, #248268, .T. ) ;
#87823 = CYLINDRICAL_SURFACE ( 'NONE', #192059, 0.09999999999999939493 ) ;
#87824 = CARTESIAN_POINT ( 'NONE',  ( -16.87331047859649757, 9.950000000011138823, -121.3500000000000369 ) ) ;
#87825 = VERTEX_POINT ( 'NONE', #87453 ) ;
#87826 = FACE_OUTER_BOUND ( 'NONE', #230882, .T. ) ;
#87827 = AXIS2_PLACEMENT_3D ( 'NONE', #128031, #172334, #251814 ) ;
#87828 = VECTOR ( 'NONE', #13724, 1000.000000000000000 ) ;
#87829 = ORIENTED_EDGE ( 'NONE', *, *, #149191, .F. ) ;
#87830 = AXIS2_PLACEMENT_3D ( 'NONE', #63398, #240777, #5988 ) ;
#87831 = AXIS2_PLACEMENT_3D ( 'NONE', #144546, #105395, #201975 ) ;
#87832 = FACE_OUTER_BOUND ( 'NONE', #121356, .T. ) ;
#87833 = FACE_OUTER_BOUND ( 'NONE', #231297, .T. ) ;
#87834 = EDGE_CURVE ( 'NONE', #85698, #51100, #67904, .T. ) ;
#87835 = CARTESIAN_POINT ( 'NONE',  ( 20.94999999999999929, 84.66355140188177586, -193.9990063664569959 ) ) ;
#87836 = CARTESIAN_POINT ( 'NONE',  ( -23.39999999999994529, 77.16254490893143725, -43.92310748452479885 ) ) ;
#87837 = ORIENTED_EDGE ( 'NONE', *, *, #210687, .T. ) ;
#87838 = CARTESIAN_POINT ( 'NONE',  ( 20.94999999999999929, 71.00000000001151079, -48.42837350343745584 ) ) ;
#87839 = AXIS2_PLACEMENT_3D ( 'NONE', #181049, #59769, #239729 ) ;
#87840 = DIRECTION ( 'NONE',  ( -0.000000000000000000, 6.982962677686266711E-15, -1.000000000000000000 ) ) ;
#87841 = CARTESIAN_POINT ( 'NONE',  ( 22.57856590037848932, -0.004128330064331048668, 11.75005846267545273 ) ) ;
#87842 = CARTESIAN_POINT ( 'NONE',  ( -22.39999999999999858, 11.65000000001115588, -100.6000000000000369 ) ) ;
#87843 = CARTESIAN_POINT ( 'NONE',  ( 20.27550659511089037, 66.78395627750315100, -115.6731074845243654 ) ) ;
#87844 = ORIENTED_EDGE ( 'NONE', *, *, #11649, .F. ) ;
#87846 = EDGE_LOOP ( 'NONE', ( #205090, #48170, #161409, #198601 ) ) ;
#87845 = DIRECTION ( 'NONE',  ( 0.000000000000000000, -7.429790795770647916E-15, 1.000000000000000000 ) ) ;
#87847 = EDGE_LOOP ( 'NONE', ( #7044, #134411, #133219, #32108 ) ) ;
#87848 = DIRECTION ( 'NONE',  ( -1.000000000000000000, -8.674042436075324885E-17, -1.619280515896126624E-16 ) ) ;
#87849 = ORIENTED_EDGE ( 'NONE', *, *, #238980, .F. ) ;
#87850 = EDGE_CURVE ( 'NONE', #44347, #72194, #156726, .T. ) ;
#87851 = CARTESIAN_POINT ( 'NONE',  ( -20.94999999999999929, 87.65000000001212754, -133.5231074845242176 ) ) ;
#87852 = CARTESIAN_POINT ( 'NONE',  ( 21.05000000000000071, 6.650000000011155876, -110.3438220896831581 ) ) ;
#87853 = CARTESIAN_POINT ( 'NONE',  ( 23.24999999999999289, 70.05000000001177796, -79.82880978955917328 ) ) ;
#87854 = ORIENTED_EDGE ( 'NONE', *, *, #158165, .T. ) ;
#87855 = CARTESIAN_POINT ( 'NONE',  ( -16.94389599338511943, 66.00880201025701410, -123.9154626827141215 ) ) ;
#87856 = DIRECTION ( 'NONE',  ( 0.000000000000000000, -0.4721928772777346239, -0.8814952561688430555 ) ) ;
#87857 = DIRECTION ( 'NONE',  ( 0.000000000000000000, -1.000000000000000000, 0.000000000000000000 ) ) ;
#87859 = VERTEX_POINT ( 'NONE', #108324 ) ;
#87858 = CIRCLE ( 'NONE', #217037, 0.1000000000000124678 ) ;
#87860 = DIRECTION ( 'NONE',  ( -1.000000000000000000, 0.000000000000000000, -0.000000000000000000 ) ) ;
#87862 = EDGE_LOOP ( 'NONE', ( #46902, #174677, #79025, #121362 ) ) ;
#87861 = CARTESIAN_POINT ( 'NONE',  ( -23.15000000000000213, 36.65892442174472876, -249.5511627012454596 ) ) ;
#87863 = DIRECTION ( 'NONE',  ( -1.000000000000000000, -7.049440681616513945E-16, 1.911869773728115701E-16 ) ) ;
#87865 = ADVANCED_FACE ( 'NONE', ( #232133 ), #102478, .F. ) ;
#87864 = CARTESIAN_POINT ( 'NONE',  ( 20.94999999999999929, 76.00000000001213607, -136.5231074845243313 ) ) ;
#87866 = VECTOR ( 'NONE', #40885, 999.9999999999998863 ) ;
#87867 = VERTEX_POINT ( 'NONE', #31389 ) ;
#87868 = CARTESIAN_POINT ( 'NONE',  ( 18.49999999999999289, 63.86149674585136893, -209.2793526595898470 ) ) ;
#87869 = CARTESIAN_POINT ( 'NONE',  ( -13.88555196119804158, 66.54256847116315043, -121.5231905466247753 ) ) ;
#87870 = VECTOR ( 'NONE', #188471, 1000.000000000000000 ) ;
#87871 = LINE ( 'NONE', #185724, #60159 ) ;
#87872 = ORIENTED_EDGE ( 'NONE', *, *, #192110, .F. ) ;
#87873 = DIRECTION ( 'NONE',  ( 0.000000000000000000, 0.8814952561688436106, -0.4721928772777334027 ) ) ;
#87874 = PLANE ( 'NONE',  #238852 ) ;
#87875 = ORIENTED_EDGE ( 'NONE', *, *, #178998, .F. ) ;
#87876 = CIRCLE ( 'NONE', #50461, 0.1999999999999987899 ) ;
#87877 = CIRCLE ( 'NONE', #242022, 0.1000000000000028644 ) ;
#87879 = ORIENTED_EDGE ( 'NONE', *, *, #146925, .F. ) ;
#87878 = AXIS2_PLACEMENT_3D ( 'NONE', #32472, #9021, #29894 ) ;
#87880 = CARTESIAN_POINT ( 'NONE',  ( 21.14999999999999858, 65.28660755661270798, -191.2731074845244166 ) ) ;
#87881 = EDGE_CURVE ( 'NONE', #181648, #215192, #227410, .T. ) ;
#87882 = EDGE_CURVE ( 'NONE', #109044, #12223, #99072, .T. ) ;
#87883 = ORIENTED_EDGE ( 'NONE', *, *, #192106, .F. ) ;
#87884 = CARTESIAN_POINT ( 'NONE',  ( -16.93388492042257809, 9.988541822527057690, -188.4005451231861628 ) ) ;
#87885 = CARTESIAN_POINT ( 'NONE',  ( -16.92280123533733871, 66.05000000001255955, -182.8737397986104725 ) ) ;
#87887 = ORIENTED_EDGE ( 'NONE', *, *, #67864, .T. ) ;
#87886 = CYLINDRICAL_SURFACE ( 'NONE', #108475, 0.09999999999999939493 ) ;
#87888 = DIRECTION ( 'NONE',  ( 1.000000000000000000, 0.000000000000000000, 0.000000000000000000 ) ) ;
#87889 = CARTESIAN_POINT ( 'NONE',  ( -18.59999999999999787, 68.97833521811233481, -166.2895420826271220 ) ) ;
#87891 = EDGE_CURVE ( 'NONE', #78167, #252512, #206572, .T. ) ;
#87890 = DIRECTION ( 'NONE',  ( -0.000000000000000000, 6.982962677686266711E-15, -1.000000000000000000 ) ) ;
#87893 = EDGE_CURVE ( 'NONE', #242585, #134549, #54752, .T. ) ;
#87892 = CYLINDRICAL_SURFACE ( 'NONE', #200451, 0.09999999999999939493 ) ;
#87894 = FACE_OUTER_BOUND ( 'NONE', #148379, .T. ) ;
#87895 = CARTESIAN_POINT ( 'NONE',  ( -16.92209698673727303, 9.950000000011138823, -79.71063556705212250 ) ) ;
#87896 = DIRECTION ( 'NONE',  ( 0.000000000000000000, -0.4721928772777346239, -0.8814952561688430555 ) ) ;
#87898 = ORIENTED_EDGE ( 'NONE', *, *, #215880, .F. ) ;
#87897 = CARTESIAN_POINT ( 'NONE',  ( -22.49072729836729678, 75.94351806727840426, -114.6731157336792535 ) ) ;
#87899 = CARTESIAN_POINT ( 'NONE',  ( -17.11825945287482753, 10.05000000001113847, -146.7500000000000284 ) ) ;
#87900 = VECTOR ( 'NONE', #29624, 1000.000000000000000 ) ;
#87902 = EDGE_LOOP ( 'NONE', ( #242904, #196965, #197941, #26820 ) ) ;
#87901 = EDGE_CURVE ( 'NONE', #140569, #206400, #92591, .T. ) ;
#87903 = ADVANCED_FACE ( 'NONE', ( #93884 ), #160812, .F. ) ;
#87905 = EDGE_CURVE ( 'NONE', #193233, #14270, #144187, .T. ) ;
#87904 = ADVANCED_FACE ( 'NONE', ( #13089 ), #172194, .T. ) ;
#87906 = PLANE ( 'NONE',  #126632 ) ;
#87907 = DIRECTION ( 'NONE',  ( 1.000000000000000000, 0.000000000000000000, 0.000000000000000000 ) ) ;
#87908 = EDGE_CURVE ( 'NONE', #156407, #207108, #77546, .T. ) ;
#87909 = DIRECTION ( 'NONE',  ( 1.000000000000000000, 0.000000000000000000, -0.000000000000000000 ) ) ;
#87910 = DIRECTION ( 'NONE',  ( -1.000000000000000000, -0.000000000000000000, -0.000000000000000000 ) ) ;
#87911 = ORIENTED_EDGE ( 'NONE', *, *, #29868, .F. ) ;
#87912 = LINE ( 'NONE', #47513, #18853 ) ;
#87913 = AXIS2_PLACEMENT_3D ( 'NONE', #26680, #125744, #7084 ) ;
#87914 = ADVANCED_FACE ( 'NONE', ( #11816 ), #193000, .F. ) ;
#87915 = AXIS2_PLACEMENT_3D ( 'NONE', #94843, #206642, #48844 ) ;
#87916 = AXIS2_PLACEMENT_3D ( 'NONE', #16703, #111957, #135330 ) ;
#87917 = CARTESIAN_POINT ( 'NONE',  ( -23.15000000000000213, 64.35000000001258513, -191.2731074845244450 ) ) ;
#87918 = ORIENTED_EDGE ( 'NONE', *, *, #37636, .T. ) ;
#87919 = EDGE_CURVE ( 'NONE', #152168, #153892, #213835, .T. ) ;
#87920 = EDGE_CURVE ( 'NONE', #152615, #195996, #244154, .T. ) ;
#87921 = DIRECTION ( 'NONE',  ( 0.000000000000000000, 0.2965989261549202283, 0.9550021345545507412 ) ) ;
#87922 = DIRECTION ( 'NONE',  ( -0.000000000000000000, -0.000000000000000000, -1.000000000000000000 ) ) ;
#87923 = ADVANCED_FACE ( 'NONE', ( #255476 ), #23036, .F. ) ;
#87924 = ORIENTED_EDGE ( 'NONE', *, *, #174992, .T. ) ;
#87925 = CARTESIAN_POINT ( 'NONE',  ( -20.64999999999999858, 74.07476635515273244, -182.7533510176504876 ) ) ;
#87926 = ORIENTED_EDGE ( 'NONE', *, *, #163894, .T. ) ;
#87927 = CARTESIAN_POINT ( 'NONE',  ( 21.06280952165553444, 65.37286769941074738, -124.3190535977457500 ) ) ;
#87928 = ORIENTED_EDGE ( 'NONE', *, *, #207935, .F. ) ;
#87929 = EDGE_CURVE ( 'NONE', #224443, #256147, #19311, .T. ) ;
#87930 = AXIS2_PLACEMENT_3D ( 'NONE', #112225, #42943, #39110 ) ;
#87931 = CARTESIAN_POINT ( 'NONE',  ( -23.49999999999994316, 74.16448838626247664, -47.52760213295649550 ) ) ;
#87932 = LINE ( 'NONE', #249616, #226273 ) ;
#87934 = VERTEX_POINT ( 'NONE', #76880 ) ;
#87933 = EDGE_CURVE ( 'NONE', #79539, #143129, #165056, .T. ) ;
#87935 = ORIENTED_EDGE ( 'NONE', *, *, #196211, .T. ) ;
#87936 = CARTESIAN_POINT ( 'NONE',  ( -20.54999999999999716, 7.368416211812038874, -223.5546256078887097 ) ) ;
#87938 = ORIENTED_EDGE ( 'NONE', *, *, #188443, .T. ) ;
#87937 = CARTESIAN_POINT ( 'NONE',  ( 14.45204356427542081, 9.450668889178686527, -48.55554649020735525 ) ) ;
#87939 = FACE_OUTER_BOUND ( 'NONE', #128862, .T. ) ;
#87940 = ORIENTED_EDGE ( 'NONE', *, *, #124699, .F. ) ;
#87941 = VERTEX_POINT ( 'NONE', #3427 ) ;
#87942 = EDGE_CURVE ( 'NONE', #14615, #12920, #231530, .T. ) ;
#87943 = DIRECTION ( 'NONE',  ( -1.000000000000000000, 0.000000000000000000, 0.000000000000000000 ) ) ;
#87945 = DIRECTION ( 'NONE',  ( 1.000000000000000000, 0.000000000000000000, 0.000000000000000000 ) ) ;
#87944 = AXIS2_PLACEMENT_3D ( 'NONE', #80773, #178651, #79497 ) ;
#87946 = CARTESIAN_POINT ( 'NONE',  ( -20.64999999999999858, 7.150000000011155876, -88.25000000000005684 ) ) ;
#87947 = DIRECTION ( 'NONE',  ( -1.000000000000000000, 0.000000000000000000, 0.000000000000000000 ) ) ;
#87948 = DIRECTION ( 'NONE',  ( -0.000000000000000000, -0.000000000000000000, -1.000000000000000000 ) ) ;
#87949 = DIRECTION ( 'NONE',  ( 0.000000000000000000, 0.2128009952263403282, -0.9770955615653358350 ) ) ;
#87950 = CIRCLE ( 'NONE', #58740, 0.1000000000000001721 ) ;
#87951 = ORIENTED_EDGE ( 'NONE', *, *, #194452, .F. ) ;
#87952 = CARTESIAN_POINT ( 'NONE',  ( 20.94999999999999929, 4.850467289730776344, -155.4657325909983570 ) ) ;
#87953 = DIRECTION ( 'NONE',  ( 0.000000000000000000, 0.000000000000000000, -1.000000000000000000 ) ) ;
#87954 = DIRECTION ( 'NONE',  ( 0.000000000000000000, -7.026728003956695223E-15, 1.000000000000000000 ) ) ;
#87955 = DIRECTION ( 'NONE',  ( 0.000000000000000000, -0.000000000000000000, -1.000000000000000000 ) ) ;
#87956 = AXIS2_PLACEMENT_3D ( 'NONE', #144055, #3261, #26722 ) ;
#87957 = ORIENTED_EDGE ( 'NONE', *, *, #45902, .F. ) ;
#87958 = DIRECTION ( 'NONE',  ( -1.000000000000000000, 0.000000000000000000, -0.000000000000000000 ) ) ;
#87959 = EDGE_LOOP ( 'NONE', ( #149498, #116075, #83480, #216670 ) ) ;
#87960 = DIRECTION ( 'NONE',  ( -1.000000000000000000, -0.000000000000000000, -0.000000000000000000 ) ) ;
#87961 = ORIENTED_EDGE ( 'NONE', *, *, #93825, .F. ) ;
#87962 = CIRCLE ( 'NONE', #17278, 0.1999999999999987899 ) ;
#87963 = CARTESIAN_POINT ( 'NONE',  ( -15.75000000000000355, 26.30888228346803004, -233.3999513616626587 ) ) ;
#87964 = DIRECTION ( 'NONE',  ( 0.000000000000000000, -6.608470384673558123E-15, 1.000000000000000000 ) ) ;
#87965 = ORIENTED_EDGE ( 'NONE', *, *, #100054, .T. ) ;
#87966 = AXIS2_PLACEMENT_3D ( 'NONE', #9221, #168352, #150044 ) ;
#87967 = ORIENTED_EDGE ( 'NONE', *, *, #124542, .F. ) ;
#87969 = ORIENTED_EDGE ( 'NONE', *, *, #8165, .T. ) ;
#87968 = DIRECTION ( 'NONE',  ( 0.7071067811865463515, 0.6824534298470384952, -0.1850873201762213149 ) ) ;
#87970 = CARTESIAN_POINT ( 'NONE',  ( -23.15000000000000213, 76.00000000001195133, -103.0231074845243171 ) ) ;
#87971 = ORIENTED_EDGE ( 'NONE', *, *, #109759, .F. ) ;
#87972 = CARTESIAN_POINT ( 'NONE',  ( -18.59999999999999787, 9.250000000011157297, -45.85000000000000142 ) ) ;
#87973 = AXIS2_PLACEMENT_3D ( 'NONE', #190734, #229822, #227250 ) ;
#87974 = DIRECTION ( 'NONE',  ( 1.000000000000000000, 0.000000000000000000, 0.000000000000000000 ) ) ;
#87975 = ORIENTED_EDGE ( 'NONE', *, *, #229030, .F. ) ;
#87976 = ADVANCED_FACE ( 'NONE', ( #254224 ), #82942, .T. ) ;
#87977 = DIRECTION ( 'NONE',  ( -0.000000000000000000, 0.8660254037844424824, 0.4999999999999934497 ) ) ;
#87978 = LINE ( 'NONE', #167573, #65955 ) ;
#87979 = AXIS2_PLACEMENT_3D ( 'NONE', #181258, #2584, #215230 ) ;
#87980 = EDGE_CURVE ( 'NONE', #177802, #124483, #185731, .T. ) ;
#87981 = CIRCLE ( 'NONE', #104723, 12.87499999999999822 ) ;
#87982 = ORIENTED_EDGE ( 'NONE', *, *, #40436, .F. ) ;
#87983 = DIRECTION ( 'NONE',  ( 0.000000000000000000, -1.000000000000000000, 0.000000000000000000 ) ) ;
#87984 = EDGE_CURVE ( 'NONE', #237421, #83796, #15053, .T. ) ;
#87985 = CARTESIAN_POINT ( 'NONE',  ( 20.94999999999999929, 70.60000000001228670, -157.6178414656113205 ) ) ;
#87986 = EDGE_CURVE ( 'NONE', #116802, #152824, #61686, .T. ) ;
#87987 = VECTOR ( 'NONE', #249580, 1000.000000000000000 ) ;
#87988 = CARTESIAN_POINT ( 'NONE',  ( -23.25000000000000000, 4.150000000011156764, -54.75000000000000711 ) ) ;
#87990 = EDGE_LOOP ( 'NONE', ( #40879, #25453, #146270, #177215 ) ) ;
#87989 = DIRECTION ( 'NONE',  ( 1.000000000000000000, 0.000000000000000000, 0.000000000000000000 ) ) ;
#87991 = EDGE_CURVE ( 'NONE', #143019, #143516, #52625, .T. ) ;
#87992 = FACE_OUTER_BOUND ( 'NONE', #177112, .T. ) ;
#87993 = CARTESIAN_POINT ( 'NONE',  ( -22.49544290803746094, 12.61946619309018303, -223.3444065952058395 ) ) ;
#87994 = DIRECTION ( 'NONE',  ( 0.000000000000000000, -7.272083257015735086E-15, 1.000000000000000000 ) ) ;
#87996 = FACE_OUTER_BOUND ( 'NONE', #37776, .T. ) ;
#87995 = DIRECTION ( 'NONE',  ( 1.000000000000000000, -0.000000000000000000, -0.000000000000000000 ) ) ;
#87997 = CARTESIAN_POINT ( 'NONE',  ( 20.95512820512820085, 39.31056039967181448, -236.7220595557971023 ) ) ;
#87998 = DIRECTION ( 'NONE',  ( 0.000000000000000000, 0.5795995782408065455, 0.8149014228132623883 ) ) ;
#87999 = CARTESIAN_POINT ( 'NONE',  ( -21.05000000000000071, 75.90220970870393558, -209.7809220950004772 ) ) ;
#88000 = VECTOR ( 'NONE', #25994, 1000.000000000000000 ) ;
#88001 = DIRECTION ( 'NONE',  ( 1.000000000000000000, 0.000000000000000000, 0.000000000000000000 ) ) ;
#88002 = VECTOR ( 'NONE', #74202, 1000.000000000000000 ) ;
#88003 = AXIS2_PLACEMENT_3D ( 'NONE', #559, #224435, #217038 ) ;
#88005 = ORIENTED_EDGE ( 'NONE', *, *, #201811, .F. ) ;
#88004 = AXIS2_PLACEMENT_3D ( 'NONE', #79184, #252690, #233173 ) ;
#88006 = EDGE_CURVE ( 'NONE', #252613, #114500, #177313, .T. ) ;
#88007 = VERTEX_POINT ( 'NONE', #64698 ) ;
#88008 = VERTEX_POINT ( 'NONE', #135566 ) ;
#88009 = CARTESIAN_POINT ( 'NONE',  ( -20.96428641294245310, 64.25000000001219291, -143.3482143065823209 ) ) ;
#88010 = DIRECTION ( 'NONE',  ( -0.000000000000000000, -1.897661533703519897E-16, 1.000000000000000000 ) ) ;
#88011 = ORIENTED_EDGE ( 'NONE', *, *, #191434, .T. ) ;
#88012 = FILL_AREA_STYLE ('',( #48906 ) ) ;
#88013 = CARTESIAN_POINT ( 'NONE',  ( 23.14999999999999858, 69.35000000001156195, -57.17310748452436542 ) ) ;
#88014 = DIRECTION ( 'NONE',  ( 0.000000000000000000, 0.000000000000000000, 1.000000000000000000 ) ) ;
#88015 = ADVANCED_FACE ( 'NONE', ( #144218 ), #69404, .F. ) ;
#88016 = CARTESIAN_POINT ( 'NONE',  ( 12.25000000000000000, 9.850000000011137402, -83.75000000000004263 ) ) ;
#88017 = VERTEX_POINT ( 'NONE', #16931 ) ;
#88018 = ORIENTED_EDGE ( 'NONE', *, *, #145660, .T. ) ;
#88019 = DIRECTION ( 'NONE',  ( 1.000000000000000000, 0.000000000000000000, 0.000000000000000000 ) ) ;
#88020 = DIRECTION ( 'NONE',  ( 0.000000000000000000, -0.2128009952263604232, 0.9770955615653316162 ) ) ;
#88021 = VERTEX_POINT ( 'NONE', #95173 ) ;
#88022 = CARTESIAN_POINT ( 'NONE',  ( -18.50000000000000000, 77.36242903720467723, -28.13422623660311217 ) ) ;
#88024 = VERTEX_POINT ( 'NONE', #8584 ) ;
#88023 = CARTESIAN_POINT ( 'NONE',  ( 18.59999999999997655, 43.08613539620618837, -254.3146655184800409 ) ) ;
#88025 = CYLINDRICAL_SURFACE ( 'NONE', #237060, 0.09999999999999939493 ) ;
#88026 = LINE ( 'NONE', #7221, #187367 ) ;
#88027 = EDGE_CURVE ( 'NONE', #94061, #214758, #231453, .T. ) ;
#88028 = VECTOR ( 'NONE', #84089, 1000.000000000000000 ) ;
#88029 = ORIENTED_EDGE ( 'NONE', *, *, #167170, .F. ) ;
#88030 = LINE ( 'NONE', #250966, #116533 ) ;
#88031 = CARTESIAN_POINT ( 'NONE',  ( 20.94999999999999929, 64.25000000001219291, -143.3069731475025321 ) ) ;
#88032 = EDGE_CURVE ( 'NONE', #225035, #149877, #102666, .T. ) ;
#88033 = CARTESIAN_POINT ( 'NONE',  ( 18.49999999999999289, 69.55000000001261640, -193.5060803140843859 ) ) ;
#88035 = CARTESIAN_POINT ( 'NONE',  ( 21.05000000000000071, 70.15000000001221281, -146.6556047088023149 ) ) ;
#88034 = DIRECTION ( 'NONE',  ( -1.000000000000000000, 0.000000000000000000, 0.000000000000000000 ) ) ;
#88036 = CARTESIAN_POINT ( 'NONE',  ( 18.50000000000022382, 10.37342005529079536, -91.76578812462599899 ) ) ;
#88037 = DIRECTION ( 'NONE',  ( -1.000000000000000000, -0.000000000000000000, -0.000000000000000000 ) ) ;
#88038 = FACE_OUTER_BOUND ( 'NONE', #142988, .T. ) ;
#88039 = DIRECTION ( 'NONE',  ( 0.000000000000000000, 6.467318590049456648E-15, -1.000000000000000000 ) ) ;
#88040 = ORIENTED_EDGE ( 'NONE', *, *, #143188, .F. ) ;
#88041 = ORIENTED_EDGE ( 'NONE', *, *, #212801, .T. ) ;
#88042 = VERTEX_POINT ( 'NONE', #166404 ) ;
#88043 = EDGE_CURVE ( 'NONE', #169886, #208902, #23637, .T. ) ;
#88044 = CARTESIAN_POINT ( 'NONE',  ( -23.49999999999994316, 74.94272479589878344, -3.023107484524792277 ) ) ;
#88045 = VERTEX_POINT ( 'NONE', #226314 ) ;
#88046 = CARTESIAN_POINT ( 'NONE',  ( 19.58285714285715073, 10.38499851036257837, -74.62968466739000917 ) ) ;
#88047 = ORIENTED_EDGE ( 'NONE', *, *, #222637, .F. ) ;
#88048 = CARTESIAN_POINT ( 'NONE',  ( 18.39999999999999503, 64.52683809664972614, -145.7731074845244450 ) ) ;
#88049 = CARTESIAN_POINT ( 'NONE',  ( -23.15000000000000213, 76.00000000001165290, -69.52310748452431710 ) ) ;
#88050 = ADVANCED_FACE ( 'NONE', ( #86811 ), #244613, .F. ) ;
#88051 = ADVANCED_FACE ( 'NONE', ( #46405 ), #89386, .F. ) ;
#88052 = ORIENTED_EDGE ( 'NONE', *, *, #181840, .F. ) ;
#88053 = EDGE_CURVE ( 'NONE', #9029, #222564, #44461, .T. ) ;
#88054 = CARTESIAN_POINT ( 'NONE',  ( 12.25000000000000178, 9.350000000011140955, -150.8642676076161138 ) ) ;
#88056 = ORIENTED_EDGE ( 'NONE', *, *, #207179, .F. ) ;
#88055 = AXIS2_PLACEMENT_3D ( 'NONE', #186866, #185561, #162170 ) ;
#88057 = ORIENTED_EDGE ( 'NONE', *, *, #124046, .T. ) ;
#88058 = ORIENTED_EDGE ( 'NONE', *, *, #46749, .F. ) ;
#88059 = AXIS2_PLACEMENT_3D ( 'NONE', #140781, #102911, #243732 ) ;
#88060 = DIRECTION ( 'NONE',  ( 0.000000000000000000, 0.8814952561688442767, -0.4721928772777322925 ) ) ;
#88061 = CARTESIAN_POINT ( 'NONE',  ( 20.95512820512820440, 65.37615131630019505, -128.8581939154367717 ) ) ;
#88062 = CARTESIAN_POINT ( 'NONE',  ( -23.15000000000000213, 2.000000000011154189, -188.2753780772378889 ) ) ;
#88063 = DIRECTION ( 'NONE',  ( 0.000000000000000000, 0.000000000000000000, 1.000000000000000000 ) ) ;
#88064 = DIRECTION ( 'NONE',  ( 3.265361837132813093E-16, 1.000000000000000000, 6.982962677686266711E-15 ) ) ;
#88065 = CARTESIAN_POINT ( 'NONE',  ( -23.15000000000000213, 19.16534496950139399, -238.0132401564540032 ) ) ;
#88066 = EDGE_CURVE ( 'NONE', #211628, #200753, #167678, .T. ) ;
#88068 = DIRECTION ( 'NONE',  ( 1.000000000000000000, 1.836970198721029934E-16, 0.000000000000000000 ) ) ;
#88067 = PLANE ( 'NONE',  #41530 ) ;
#88069 = DIRECTION ( 'NONE',  ( 0.000000000000000000, 0.9553114395362829470, -0.2956011730205325705 ) ) ;
#88071 = ORIENTED_EDGE ( 'NONE', *, *, #231947, .T. ) ;
#88070 = LINE ( 'NONE', #208071, #23207 ) ;
#88073 = DIRECTION ( 'NONE',  ( 0.000000000000000000, -1.000000000000000000, -2.891205793294679805E-16 ) ) ;
#88072 = CARTESIAN_POINT ( 'NONE',  ( 20.12518398540832365, 9.975088720679844201, -74.99666825246995927 ) ) ;
#88074 = CARTESIAN_POINT ( 'NONE',  ( -19.99999999999999645, 1.350000000000000089, 22.00000000000000355 ) ) ;
#88075 = EDGE_LOOP ( 'NONE', ( #100097, #23537, #222785, #236821 ) ) ;
#88076 = SPHERICAL_SURFACE ( 'NONE', #242201, 0.1000000000000000056 ) ;
#88077 = DIRECTION ( 'NONE',  ( -1.000000000000000000, 0.000000000000000000, 0.000000000000000000 ) ) ;
#88078 = FACE_OUTER_BOUND ( 'NONE', #215021, .T. ) ;
#88079 = ORIENTED_EDGE ( 'NONE', *, *, #154436, .T. ) ;
#88080 = AXIS2_PLACEMENT_3D ( 'NONE', #60902, #37516, #238258 ) ;
#88081 = CARTESIAN_POINT ( 'NONE',  ( 20.85000000000000142, 64.25000000001215028, -136.5231074845244166 ) ) ;
#88082 = DIRECTION ( 'NONE',  ( 0.000000000000000000, 0.000000000000000000, 1.000000000000000000 ) ) ;
#88083 = CARTESIAN_POINT ( 'NONE',  ( 21.05000000000000071, 1.115600667400684642E-11, -167.4999999999999716 ) ) ;
#88084 = EDGE_LOOP ( 'NONE', ( #101074, #91414, #120277, #128873 ) ) ;
#88085 = ORIENTED_EDGE ( 'NONE', *, *, #125863, .F. ) ;
#88086 = CARTESIAN_POINT ( 'NONE',  ( -23.15000000000000213, 23.47541653617480861, -229.1594947991076197 ) ) ;
#88087 = ORIENTED_EDGE ( 'NONE', *, *, #172754, .F. ) ;
#88088 = CARTESIAN_POINT ( 'NONE',  ( -18.50000324121759121, 10.29307482169070731, -172.9586421466940465 ) ) ;
#88089 = PLANE ( 'NONE',  #90673 ) ;
#88090 = CARTESIAN_POINT ( 'NONE',  ( -20.94403535211772294, 10.30632246271647467, -206.5041836778895288 ) ) ;
#88091 = ORIENTED_EDGE ( 'NONE', *, *, #110966, .T. ) ;
#88092 = DIRECTION ( 'NONE',  ( -0.000000000000000000, 1.000000000000000000, 0.000000000000000000 ) ) ;
#88093 = CIRCLE ( 'NONE', #142293, 0.09999999999999564793 ) ;
#88095 = CARTESIAN_POINT ( 'NONE',  ( 21.05000000000000071, -9.399999999988846611, -110.3939691226524786 ) ) ;
#88094 = AXIS2_PLACEMENT_3D ( 'NONE', #86848, #6033, #47726 ) ;
#88096 = TOROIDAL_SURFACE ( 'NONE', #242237, 3.899999999999999467, 0.1000000000000000056 ) ;
#88097 = CARTESIAN_POINT ( 'NONE',  ( -18.40000000000000213, 15.65609082920797412, -218.9714148105434788 ) ) ;
#88098 = DIRECTION ( 'NONE',  ( 1.000000000000000000, 0.000000000000000000, 0.000000000000000000 ) ) ;
#88099 = EDGE_CURVE ( 'NONE', #23382, #78723, #127652, .T. ) ;
#88100 = ORIENTED_EDGE ( 'NONE', *, *, #14600, .T. ) ;
#88101 = LINE ( 'NONE', #167701, #200923 ) ;
#88103 = ORIENTED_EDGE ( 'NONE', *, *, #120714, .F. ) ;
#88102 = FACE_OUTER_BOUND ( 'NONE', #9653, .T. ) ;
#88104 = CARTESIAN_POINT ( 'NONE',  ( -16.93344882324368683, 9.996588767299030565, -121.4130256948049578 ) ) ;
#88105 = DIRECTION ( 'NONE',  ( 0.000000000000000000, -0.2617529984165031243, -0.9651348961777157509 ) ) ;
#88106 = CARTESIAN_POINT ( 'NONE',  ( -20.54999999999999716, 73.50000000001259082, -190.2984855617622770 ) ) ;
#88107 = ADVANCED_FACE ( 'NONE', ( #145511 ), #240087, .T. ) ;
#88108 = CARTESIAN_POINT ( 'NONE',  ( -16.92973740335348509, 9.992503814478576274, -87.90605903520246045 ) ) ;
#88109 = DIRECTION ( 'NONE',  ( 1.000000000000000000, -1.836970198721029934E-16, -1.282749433769087582E-30 ) ) ;
#88110 = CARTESIAN_POINT ( 'NONE',  ( 18.59999999999999787, 16.44800918141279311, -240.8068063186265135 ) ) ;
#88111 = CARTESIAN_POINT ( 'NONE',  ( -23.15000000000000213, 11.75000000001115552, -122.2500000000000284 ) ) ;
#88112 = CIRCLE ( 'NONE', #213035, 12.87499999999999822 ) ;
#88113 = VERTEX_POINT ( 'NONE', #247176 ) ;
#88114 = DIRECTION ( 'NONE',  ( -1.000000000000000000, 0.000000000000000000, 0.000000000000000000 ) ) ;
#88115 = CARTESIAN_POINT ( 'NONE',  ( -21.05000000000000071, 16.52766025697963315, -240.8672687545768270 ) ) ;
#88117 = ADVANCED_FACE ( 'NONE', ( #185930 ), #190201, .T. ) ;
#88116 = DIRECTION ( 'NONE',  ( 0.7071067811865487940, 8.659560562354918067E-17, 0.7071067811865463515 ) ) ;
#88118 = ADVANCED_FACE ( 'NONE', ( #108950 ), #146779, .F. ) ;
#88119 = CARTESIAN_POINT ( 'NONE',  ( -21.44999999999999929, 68.85000000001259934, -191.2731074845244166 ) ) ;
#88120 = LINE ( 'NONE', #166443, #34006 ) ;
#88121 = DIRECTION ( 'NONE',  ( 0.000000000000000000, 0.1335171055202901691, 0.9910465087640861759 ) ) ;
#88122 = ORIENTED_EDGE ( 'NONE', *, *, #60527, .F. ) ;
#88123 = ORIENTED_EDGE ( 'NONE', *, *, #248299, .F. ) ;
#88124 = CARTESIAN_POINT ( 'NONE',  ( 23.14999999999999858, 4.999999999999997335, -21.59473398108690390 ) ) ;
#88125 = DIRECTION ( 'NONE',  ( 0.000000000000000000, -1.000000000000000000, 0.000000000000000000 ) ) ;
#88126 = CARTESIAN_POINT ( 'NONE',  ( -21.05000000000000071, -0.9150442794618510733, -196.7984890852706030 ) ) ;
#88127 = ADVANCED_FACE ( 'NONE', ( #68562 ), #148097, .T. ) ;
#88128 = AXIS2_PLACEMENT_3D ( 'NONE', #251872, #12013, #189352 ) ;
#88129 = CARTESIAN_POINT ( 'NONE',  ( -21.04999999999994387, 82.64476912853859858, -26.37791261425322986 ) ) ;
#88130 = DIRECTION ( 'NONE',  ( -1.000000000000000000, -2.952720810173289112E-16, 0.000000000000000000 ) ) ;
#88131 = CIRCLE ( 'NONE', #54831, 1.500000000000001332 ) ;
#88132 = FACE_OUTER_BOUND ( 'NONE', #78433, .T. ) ;
#88133 = CARTESIAN_POINT ( 'NONE',  ( -16.94389599338512298, 9.991197989755043807, -12.60764480181024538 ) ) ;
#88134 = AXIS2_PLACEMENT_3D ( 'NONE', #230899, #49670, #194348 ) ;
#88135 = AXIS2_PLACEMENT_3D ( 'NONE', #56041, #75658, #255502 ) ;
#88136 = ORIENTED_EDGE ( 'NONE', *, *, #14765, .T. ) ;
#88137 = CARTESIAN_POINT ( 'NONE',  ( -18.46902351632713746, 85.50947011869244818, -62.53665355026694073 ) ) ;
#88138 = CIRCLE ( 'NONE', #179778, 0.1000000000000055844 ) ;
#88139 = VERTEX_POINT ( 'NONE', #208085 ) ;
#88140 = ADVANCED_FACE ( 'NONE', ( #188497 ), #209338, .F. ) ;
#88141 = DIRECTION ( 'NONE',  ( -1.000000000000000000, -0.000000000000000000, 0.000000000000000000 ) ) ;
#88142 = EDGE_CURVE ( 'NONE', #52520, #91770, #228917, .T. ) ;
#88143 = CARTESIAN_POINT ( 'NONE',  ( 20.94999999999999929, 65.27628289530404970, -57.37310748452439668 ) ) ;
#88144 = CARTESIAN_POINT ( 'NONE',  ( 21.10710606213542206, 8.776894023904366904, -79.24099652639947067 ) ) ;
#88145 = CARTESIAN_POINT ( 'NONE',  ( 23.14999999999998437, 76.00000000001240608, -174.0731074845243711 ) ) ;
#88146 = DIRECTION ( 'NONE',  ( -0.000000000000000000, 0.9651348961777155289, -0.2617529984165036794 ) ) ;
#88148 = CARTESIAN_POINT ( 'NONE',  ( 18.59999999999999076, 65.50857864377520912, -178.7731074845244450 ) ) ;
#88147 = AXIS2_PLACEMENT_3D ( 'NONE', #62435, #141954, #221475 ) ;
#88149 = CARTESIAN_POINT ( 'NONE',  ( 18.49999999999999289, 11.75000000001115907, -75.10000000000003695 ) ) ;
#88150 = ORIENTED_EDGE ( 'NONE', *, *, #159936, .F. ) ;
#88151 = CARTESIAN_POINT ( 'NONE',  ( -16.93970660449832621, 22.92160253073273424, -230.8335271541670295 ) ) ;
#88152 = CIRCLE ( 'NONE', #9083, 0.09999999999998898659 ) ;
#88153 = DIRECTION ( 'NONE',  ( 0.000000000000000000, 1.000000000000000000, 0.000000000000000000 ) ) ;
#88154 = DIRECTION ( 'NONE',  ( -0.000000000000000000, 0.9651348961777157509, -0.2617529984165031243 ) ) ;
#88156 = EDGE_CURVE ( 'NONE', #50839, #251180, #98549, .T. ) ;
#88155 = CARTESIAN_POINT ( 'NONE',  ( 18.59999999999999076, -1.851617760457748618, -145.6031897196037050 ) ) ;
#88157 = TOROIDAL_SURFACE ( 'NONE', #92461, 0.4000000000000005773, 0.1000000000000000056 ) ;
#88158 = AXIS2_PLACEMENT_3D ( 'NONE', #84357, #2291, #221335 ) ;
#88159 = CARTESIAN_POINT ( 'NONE',  ( -20.00857864376270001, 9.150000000011157653, -112.8500000000000369 ) ) ;
#88160 = FACE_OUTER_BOUND ( 'NONE', #100718, .T. ) ;
#88161 = VERTEX_POINT ( 'NONE', #33319 ) ;
#88162 = CIRCLE ( 'NONE', #104902, 0.09999999999999939493 ) ;
#88163 = CARTESIAN_POINT ( 'NONE',  ( 18.45139536634708222, 85.48608172029329921, -129.8825958667136433 ) ) ;
#88164 = CARTESIAN_POINT ( 'NONE',  ( -23.15000000000000213, -11.48912529306489994, -130.9000000000000341 ) ) ;
#88165 = ORIENTED_EDGE ( 'NONE', *, *, #198043, .F. ) ;
#88166 = EDGE_LOOP ( 'NONE', ( #11884, #189243, #3989, #41862 ) ) ;
#88167 = DIRECTION ( 'NONE',  ( 0.000000000000000000, 6.982962677686266711E-15, -1.000000000000000000 ) ) ;
#88168 = CARTESIAN_POINT ( 'NONE',  ( 21.13920837816993270, 67.21675294989238125, -157.7731074845244166 ) ) ;
#88169 = EDGE_CURVE ( 'NONE', #168409, #74676, #193639, .T. ) ;
#88170 = CARTESIAN_POINT ( 'NONE',  ( -20.64999999999999858, -8.730841121484171907, -110.0980747189843640 ) ) ;
#88171 = ORIENTED_EDGE ( 'NONE', *, *, #86576, .T. ) ;
#88172 = CARTESIAN_POINT ( 'NONE',  ( 20.94999999999999929, 64.36312671090679771, -42.84486669784945434 ) ) ;
#88173 = CARTESIAN_POINT ( 'NONE',  ( 23.24999999999999289, 64.04577702392042227, -222.1950530992138226 ) ) ;
#88174 = VECTOR ( 'NONE', #255907, 1000.000000000000000 ) ;
#88175 = ORIENTED_EDGE ( 'NONE', *, *, #141181, .T. ) ;
#88176 = AXIS2_PLACEMENT_3D ( 'NONE', #194337, #37829, #153948 ) ;
#88177 = AXIS2_PLACEMENT_3D ( 'NONE', #234109, #136271, #93319 ) ;
#88178 = CIRCLE ( 'NONE', #138092, 0.1000000000000028644 ) ;
#88179 = CARTESIAN_POINT ( 'NONE',  ( -21.05000000000000071, 1.115600667400684642E-11, -100.5000000000000426 ) ) ;
#88180 = EDGE_CURVE ( 'NONE', #251640, #141132, #231707, .T. ) ;
#88181 = EDGE_LOOP ( 'NONE', ( #61465, #210259, #2101, #135394 ) ) ;
#88182 = CYLINDRICAL_SURFACE ( 'NONE', #9912, 0.09999999999999982514 ) ;
#88183 = CARTESIAN_POINT ( 'NONE',  ( 20.94999999999999574, 18.52348994230296242, -223.9544021632493127 ) ) ;
#88185 =( BOUNDED_CURVE ( )  B_SPLINE_CURVE ( 3, ( #195341, #16694, #233186, #96196 ),
 .UNSPECIFIED., .F., .F. ) 
 B_SPLINE_CURVE_WITH_KNOTS ( ( 4, 4 ),
 ( 0.3000847527772402823, 0.5517402753107897295 ),
 .UNSPECIFIED. ) 
 CURVE ( )  GEOMETRIC_REPRESENTATION_ITEM ( )  RATIONAL_B_SPLINE_CURVE ( ( 1.000000000000000000, 0.9947294176030464508, 0.9947294176030464508, 1.000000000000000000 ) ) 
 REPRESENTATION_ITEM ( '' )  );
#88184 = CARTESIAN_POINT ( 'NONE',  ( 20.84999999999998721, -11.74999999998884448, -200.9999999999999432 ) ) ;
#88186 = CARTESIAN_POINT ( 'NONE',  ( -20.64999999999999858, 54.18213181965657554, -236.9344197582443883 ) ) ;
#88187 = CYLINDRICAL_SURFACE ( 'NONE', #145253, 0.09999999999999939493 ) ;
#88188 = ADVANCED_FACE ( 'NONE', ( #151969 ), #6842, .T. ) ;
#88190 = EDGE_CURVE ( 'NONE', #200635, #187737, #196199, .T. ) ;
#88189 = CARTESIAN_POINT ( 'NONE',  ( -22.00356870141228427, 68.74575763752110902, -203.5231074845244450 ) ) ;
#88191 = DIRECTION ( 'NONE',  ( 1.000000000000000000, -0.000000000000000000, -0.000000000000000000 ) ) ;
#88192 = CARTESIAN_POINT ( 'NONE',  ( -16.81744102076749314, 66.05000000001261640, -190.8731074845244393 ) ) ;
#88193 = CARTESIAN_POINT ( 'NONE',  ( -23.25000000000000000, 36.65892442174472876, -249.5511627012454596 ) ) ;
#88194 = CARTESIAN_POINT ( 'NONE',  ( -18.59999999999999787, 51.38014393322265505, -230.1906178717505611 ) ) ;
#88196 = VERTEX_POINT ( 'NONE', #252305 ) ;
#88195 = CARTESIAN_POINT ( 'NONE',  ( 18.48197441911338501, 86.98964386969565510, -199.3644769928878588 ) ) ;
#88197 = ORIENTED_EDGE ( 'NONE', *, *, #174089, .T. ) ;
#88199 = DIRECTION ( 'NONE',  ( 0.000000000000000000, 0.000000000000000000, 1.000000000000000000 ) ) ;
#88198 = CARTESIAN_POINT ( 'NONE',  ( -22.39999999999999858, 76.00000000001165290, -69.52310748452431710 ) ) ;
#88201 = VERTEX_POINT ( 'NONE', #234036 ) ;
#88200 = FACE_OUTER_BOUND ( 'NONE', #168497, .T. ) ;
#88202 = EDGE_LOOP ( 'NONE', ( #244887, #187973, #158919, #111255 ) ) ;
#88203 = FACE_OUTER_BOUND ( 'NONE', #53741, .T. ) ;
#88204 = AXIS2_PLACEMENT_3D ( 'NONE', #110178, #150608, #135838 ) ;
#88205 = DIRECTION ( 'NONE',  ( 1.000000000000000000, 0.000000000000000000, 0.000000000000000000 ) ) ;
#88206 = EDGE_CURVE ( 'NONE', #12223, #173371, #235966, .T. ) ;
#88207 = EDGE_CURVE ( 'NONE', #175419, #76430, #11123, .T. ) ;
#88208 =( BOUNDED_SURFACE ( )  B_SPLINE_SURFACE ( 3, 2, ( 
 ( #174737, #73059, #152589 ),
 ( #252925, #58566, #216370 ),
 ( #195556, #153893, #116013 ),
 ( #114711, #55991, #156445 ),
 ( #136831, #215092, #232109 ),
 ( #14356, #92563, #57277 ) ),
 .UNSPECIFIED., .F., .F., .F. ) 
 B_SPLINE_SURFACE_WITH_KNOTS ( ( 4, 2, 4 ),
 ( 3, 3 ),
 ( 0.0001300404313046710908, 0.0003183318589266704419, 0.0005066232865486697658 ),
 ( 0.000000000000000000, 1.000000000000000000 ),
 .UNSPECIFIED. ) 
 GEOMETRIC_REPRESENTATION_ITEM ( )  RATIONAL_B_SPLINE_SURFACE ( (
 ( 1.000000000000000000, 0.7071067811865597852, 1.000000000000000000),
 ( 1.000000000000000000, 0.7625113560540824897, 1.000000000000000000),
 ( 1.000000000000000000, 0.8126073484687461601, 1.000000000000000000),
 ( 1.000000000000000000, 0.8923049332733758998, 1.000000000000000000),
 ( 1.000000000000000000, 0.9231914937768594953, 1.000000000000000000),
 ( 1.000000000000000000, 0.9238795325112947321, 1.000000000000000000) ) ) 
 REPRESENTATION_ITEM ( '' )  SURFACE ( )  );
#88209 = CARTESIAN_POINT ( 'NONE',  ( -18.59999999999999787, 31.44980407958351165, -233.5445995079518866 ) ) ;
#88210 = CARTESIAN_POINT ( 'NONE',  ( -20.85882249326303040, 10.33248238083634796, -173.0948465439131496 ) ) ;
#88211 = DIRECTION ( 'NONE',  ( 1.000000000000000000, -0.000000000000000000, -0.000000000000000000 ) ) ;
#88212 = ADVANCED_FACE ( 'NONE', ( #132377 ), #210629, .F. ) ;
#88213 = CARTESIAN_POINT ( 'NONE',  ( -23.25000000000000000, 11.65000000001115588, -54.75000000000000000 ) ) ;
#88214 = DIRECTION ( 'NONE',  ( 0.000000000000000000, 0.9651348961777160840, -0.2617529984165015700 ) ) ;
#88216 = ORIENTED_EDGE ( 'NONE', *, *, #47606, .F. ) ;
#88215 = EDGE_CURVE ( 'NONE', #177869, #114655, #156901, .T. ) ;
#88217 = ORIENTED_EDGE ( 'NONE', *, *, #215826, .T. ) ;
#88218 = DIRECTION ( 'NONE',  ( 0.000000000000000000, 0.2617529984165031243, 0.9651348961777157509 ) ) ;
#88219 = EDGE_LOOP ( 'NONE', ( #100139, #108522, #135707, #179451 ) ) ;
#88220 = EDGE_CURVE ( 'NONE', #319, #208145, #175386, .T. ) ;
#88221 = CARTESIAN_POINT ( 'NONE',  ( 18.54999999999999716, 41.52322060116084401, -237.7841060310786077 ) ) ;
#88223 = EDGE_CURVE ( 'NONE', #59872, #13799, #77728, .T. ) ;
#88222 = ORIENTED_EDGE ( 'NONE', *, *, #143173, .F. ) ;
#88224 =( BOUNDED_CURVE ( )  B_SPLINE_CURVE ( 3, ( #212443, #192875, #254103, #93756 ),
 .UNSPECIFIED., .F., .F. ) 
 B_SPLINE_CURVE_WITH_KNOTS ( ( 4, 4 ),
 ( 0.06456096931748350753, 3.077031684272309775 ),
 .UNSPECIFIED. ) 
 CURVE ( )  GEOMETRIC_REPRESENTATION_ITEM ( )  RATIONAL_B_SPLINE_CURVE ( ( 1.000000000000000000, 0.3763440860215095940, 0.3763440860215095940, 1.000000000000000000 ) ) 
 REPRESENTATION_ITEM ( '' )  );
#88225 = CIRCLE ( 'NONE', #188218, 0.09999999999999939493 ) ;
#88226 = DIRECTION ( 'NONE',  ( 1.000000000000000000, 0.000000000000000000, 0.000000000000000000 ) ) ;
#88227 = EDGE_CURVE ( 'NONE', #14219, #81578, #219220, .T. ) ;
#88228 = CYLINDRICAL_SURFACE ( 'NONE', #206633, 0.09999999999999939493 ) ;
#88229 = CARTESIAN_POINT ( 'NONE',  ( -18.59999999999999787, 64.35000000001187459, -90.87310748452438247 ) ) ;
#88230 = EDGE_LOOP ( 'NONE', ( #175473, #160575, #168088 ) ) ;
#88231 = DIRECTION ( 'NONE',  ( -1.000000000000000000, 0.000000000000000000, 0.000000000000000000 ) ) ;
#88232 = EDGE_LOOP ( 'NONE', ( #206116, #233959 ) ) ;
#88233 = ADVANCED_FACE ( 'NONE', ( #174118 ), #131089, .F. ) ;
#88234 = DIRECTION ( 'NONE',  ( 0.000000000000000000, 0.2617529984164506107, 0.9651348961777299618 ) ) ;
#88235 = DIRECTION ( 'NONE',  ( 0.000000000000000000, 6.982962677686266711E-15, -1.000000000000000000 ) ) ;
#88236 = EDGE_CURVE ( 'NONE', #38559, #120435, #27731, .T. ) ;
#88237 = CARTESIAN_POINT ( 'NONE',  ( 18.52165635395190435, 8.844262510478683836, -245.4073689581170186 ) ) ;
#88239 = ORIENTED_EDGE ( 'NONE', *, *, #223133, .T. ) ;
#88238 = ADVANCED_FACE ( 'NONE', ( #37148 ), #131924, .T. ) ;
#88241 = DIRECTION ( 'NONE',  ( -1.000000000000000000, -0.000000000000000000, -0.000000000000000000 ) ) ;
#88240 = AXIS2_PLACEMENT_3D ( 'NONE', #190459, #170926, #107024 ) ;
#88242 = ORIENTED_EDGE ( 'NONE', *, *, #190179, .T. ) ;
#88245 = VERTEX_POINT ( 'NONE', #75000 ) ;
#88244 = CARTESIAN_POINT ( 'NONE',  ( 15.74999999999999645, 62.59162599727320497, -217.2417264603073477 ) ) ;
#88243 = DIRECTION ( 'NONE',  ( 0.000000000000000000, -0.3280696808754172689, -0.9446535261620007118 ) ) ;
#88246 = AXIS2_PLACEMENT_3D ( 'NONE', #2431, #123692, #40336 ) ;
#88247 = DIRECTION ( 'NONE',  ( 0.000000000000000000, 0.000000000000000000, -1.000000000000000000 ) ) ;
#88248 = ORIENTED_EDGE ( 'NONE', *, *, #114492, .T. ) ;
#88249 = AXIS2_PLACEMENT_3D ( 'NONE', #65438, #201101, #62874 ) ;
#88250 = CARTESIAN_POINT ( 'NONE',  ( -20.54999999999999716, 25.94586868676353575, -241.5435999122864530 ) ) ;
#88251 = ORIENTED_EDGE ( 'NONE', *, *, #165556, .T. ) ;
#88252 = DIRECTION ( 'NONE',  ( 0.000000000000000000, 0.000000000000000000, -1.000000000000000000 ) ) ;
#88253 = EDGE_CURVE ( 'NONE', #236445, #140955, #94316, .T. ) ;
#88254 = DIRECTION ( 'NONE',  ( 0.000000000000000000, -0.4856429311786307212, -0.8741572761215384846 ) ) ;
#88255 = EDGE_CURVE ( 'NONE', #224848, #2364, #214469, .T. ) ;
#88256 = CARTESIAN_POINT ( 'NONE',  ( -23.25000000000000000, 76.00000000001236344, -165.8731074845243825 ) ) ;
#88257 = DIRECTION ( 'NONE',  ( 0.000000000000000000, -1.000000000000000000, 0.000000000000000000 ) ) ;
#88258 = AXIS2_PLACEMENT_3D ( 'NONE', #244831, #204417, #225253 ) ;
#88259 = ORIENTED_EDGE ( 'NONE', *, *, #224691, .F. ) ;
#88260 = LINE ( 'NONE', #248645, #19246 ) ;
#88261 = DIRECTION ( 'NONE',  ( 0.000000000000000000, 0.9616958981405249185, -0.2741185865637159602 ) ) ;
#88262 = DIRECTION ( 'NONE',  ( 1.000000000000000000, 0.000000000000000000, 0.000000000000000000 ) ) ;
#88263 = EDGE_LOOP ( 'NONE', ( #50101, #91107, #209579, #64234 ) ) ;
#88264 = DIRECTION ( 'NONE',  ( 0.000000000000000000, 1.000000000000000000, 1.224646799147353207E-16 ) ) ;
#88265 = ORIENTED_EDGE ( 'NONE', *, *, #129836, .T. ) ;
#88266 = CARTESIAN_POINT ( 'NONE',  ( 21.14999999999999858, 30.68987205111126926, -252.2252246220829193 ) ) ;
#88267 = DIRECTION ( 'NONE',  ( 0.000000000000000000, -0.2617529984165152257, -0.9651348961777124202 ) ) ;
#88268 = CARTESIAN_POINT ( 'NONE',  ( -23.25000000000000000, 6.933893972137497030, -171.2856458343736108 ) ) ;
#88270 = VERTEX_POINT ( 'NONE', #176659 ) ;
#88269 = CARTESIAN_POINT ( 'NONE',  ( -16.92280123533699054, 44.31858025389571054, -235.2169057130089129 ) ) ;
#88271 = CARTESIAN_POINT ( 'NONE',  ( 18.50000000000000000, -9.399999999988843058, -107.7972597596633193 ) ) ;
#88272 = CARTESIAN_POINT ( 'NONE',  ( -12.26136940704871847, 62.65035202501400846, -217.0198313409406978 ) ) ;
#88273 = AXIS2_PLACEMENT_3D ( 'NONE', #229375, #92405, #33775 ) ;
#88274 = AXIS2_PLACEMENT_3D ( 'NONE', #206517, #226040, #121854 ) ;
#88275 = LINE ( 'NONE', #143125, #231197 ) ;
#88276 = ORIENTED_EDGE ( 'NONE', *, *, #89002, .F. ) ;
#88277 = TOROIDAL_SURFACE ( 'NONE', #146559, 0.2000000000000000111, 0.1000000000000000056 ) ;
#88278 = EDGE_CURVE ( 'NONE', #57631, #14587, #119283, .T. ) ;
#88279 = DIRECTION ( 'NONE',  ( 1.000000000000000000, 0.000000000000000000, 0.000000000000000000 ) ) ;
#88280 = DIRECTION ( 'NONE',  ( -1.000000000000000000, -1.646408749285562691E-14, 1.073024830501117725E-15 ) ) ;
#88281 = ORIENTED_EDGE ( 'NONE', *, *, #87313, .T. ) ;
#88282 = DIRECTION ( 'NONE',  ( 1.000000000000000000, 0.000000000000000000, 0.000000000000000000 ) ) ;
#88283 = ADVANCED_FACE ( 'NONE', ( #218305 ), #117940, .T. ) ;
#88284 = VERTEX_POINT ( 'NONE', #142625 ) ;
#88285 = CARTESIAN_POINT ( 'NONE',  ( -21.05000000000000071, -11.64999999998884483, -137.0000000000000000 ) ) ;
#88287 = VERTEX_POINT ( 'NONE', #222154 ) ;
#88286 = CARTESIAN_POINT ( 'NONE',  ( 19.75857864376268935, 64.25000000001250555, -178.6731074845244507 ) ) ;
#88288 = TOROIDAL_SURFACE ( 'NONE', #254686, 0.4000000000000015210, 0.1000000000000000056 ) ;
#88291 = ORIENTED_EDGE ( 'NONE', *, *, #54244, .F. ) ;
#88290 = ORIENTED_EDGE ( 'NONE', *, *, #79891, .T. ) ;
#88289 = CARTESIAN_POINT ( 'NONE',  ( -18.59999999999999787, 0.000000000000000000, -33.50000000000000000 ) ) ;
#88292 = CARTESIAN_POINT ( 'NONE',  ( -20.64999999999999858, 2.000000000011154189, -147.2246219227621111 ) ) ;
#88293 = DIRECTION ( 'NONE',  ( 1.000000000000000000, 0.000000000000000000, 0.000000000000000000 ) ) ;
#88294 = DIRECTION ( 'NONE',  ( 0.000000000000000000, -0.2617529984165365975, -0.9651348961777066471 ) ) ;
#88296 = CARTESIAN_POINT ( 'NONE',  ( -13.54036565897075306, 66.54845833862601978, -51.06923198569381128 ) ) ;
#88295 = CARTESIAN_POINT ( 'NONE',  ( -21.65000000000000213, 66.05000000001230376, -157.2731074845244166 ) ) ;
#88298 = EDGE_CURVE ( 'NONE', #49254, #171051, #39527, .T. ) ;
#88297 = CARTESIAN_POINT ( 'NONE',  ( -20.64999999999999858, 68.85000000001205933, -124.1731074845243370 ) ) ;
#88299 = CARTESIAN_POINT ( 'NONE',  ( -20.64999999999999858, 1.115600667400684642E-11, -33.50000000000000000 ) ) ;
#88300 = DIRECTION ( 'NONE',  ( 1.000000000000000000, 0.000000000000000000, 0.000000000000000000 ) ) ;
#88301 = TOROIDAL_SURFACE ( 'NONE', #9784, 11.90000000000000213, 0.1000000000000000056 ) ;
#88302 = CARTESIAN_POINT ( 'NONE',  ( -22.49231231312463208, 11.64998490368843953, -33.43894711239862971 ) ) ;
#88303 = VERTEX_POINT ( 'NONE', #201337 ) ;
#88304 = ORIENTED_EDGE ( 'NONE', *, *, #102023, .T. ) ;
#88305 = CARTESIAN_POINT ( 'NONE',  ( 21.05000000000000071, -1.162701749926853712, -41.60000000000000142 ) ) ;
#88307 = VERTEX_POINT ( 'NONE', #179232 ) ;
#88306 = FACE_OUTER_BOUND ( 'NONE', #123944, .T. ) ;
#88308 = ORIENTED_EDGE ( 'NONE', *, *, #28171, .F. ) ;
#88310 = FACE_OUTER_BOUND ( 'NONE', #68875, .T. ) ;
#88309 = VECTOR ( 'NONE', #43115, 1000.000000000000114 ) ;
#88311 = ORIENTED_EDGE ( 'NONE', *, *, #202973, .T. ) ;
#88312 = DIRECTION ( 'NONE',  ( 1.000000000000000000, 0.000000000000000000, 0.000000000000000000 ) ) ;
#88313 = CIRCLE ( 'NONE', #104875, 0.09999999999998898659 ) ;
#88314 = VERTEX_POINT ( 'NONE', #1830 ) ;
#88315 = AXIS2_PLACEMENT_3D ( 'NONE', #71925, #172348, #223576 ) ;
#88317 = AXIS2_PLACEMENT_3D ( 'NONE', #239876, #116077, #199474 ) ;
#88316 = CARTESIAN_POINT ( 'NONE',  ( 18.59999999999996945, 67.49222854868494892, -195.4187676019683693 ) ) ;
#88318 = AXIS2_PLACEMENT_3D ( 'NONE', #48562, #131952, #8170 ) ;
#88320 = ORIENTED_EDGE ( 'NONE', *, *, #12892, .T. ) ;
#88319 = ORIENTED_EDGE ( 'NONE', *, *, #250664, .F. ) ;
#88321 = ORIENTED_EDGE ( 'NONE', *, *, #41883, .F. ) ;
#88323 = CARTESIAN_POINT ( 'NONE',  ( 21.07189867249812210, 10.72498027010430377, -45.71245144227673762 ) ) ;
#88322 = CIRCLE ( 'NONE', #92447, 0.5000000000000044409 ) ;
#88324 = ORIENTED_EDGE ( 'NONE', *, *, #44947, .T. ) ;
#88325 = VERTEX_POINT ( 'NONE', #24007 ) ;
#88326 = CARTESIAN_POINT ( 'NONE',  ( -16.89268316805465986, 14.16190809729244648, -219.2603268738197073 ) ) ;
#88327 = DIRECTION ( 'NONE',  ( -1.000000000000000000, -0.000000000000000000, -0.000000000000000000 ) ) ;
#88328 = FACE_BOUND ( 'NONE', #52982, .T. ) ;
#88330 = ORIENTED_EDGE ( 'NONE', *, *, #71738, .F. ) ;
#88329 = DIRECTION ( 'NONE',  ( 0.000000000000000000, -0.1568667991644714932, 0.9876197685951274563 ) ) ;
#88331 = CARTESIAN_POINT ( 'NONE',  ( -18.40000000000000213, 16.38400329561159907, -222.2501914957450424 ) ) ;
#88332 = CARTESIAN_POINT ( 'NONE',  ( 20.85000000000000142, 69.01799029515522932, -65.82695536626806643 ) ) ;
#88334 = ORIENTED_EDGE ( 'NONE', *, *, #114845, .F. ) ;
#88333 = DIRECTION ( 'NONE',  ( 0.000000000000000000, 0.1290532225515364506, 0.9916376685811525427 ) ) ;
#88335 = SPHERICAL_SURFACE ( 'NONE', #171929, 0.1000000000000000056 ) ;
#88336 = ORIENTED_EDGE ( 'NONE', *, *, #211550, .F. ) ;
#88337 = DIRECTION ( 'NONE',  ( 1.000000000000000000, 0.000000000000000000, 0.000000000000000000 ) ) ;
#88338 = CIRCLE ( 'NONE', #196689, 4.150000000000001243 ) ;
#88339 = ADVANCED_FACE ( 'NONE', ( #21443 ), #137488, .F. ) ;
#88340 = ORIENTED_EDGE ( 'NONE', *, *, #154758, .F. ) ;
#88341 = AXIS2_PLACEMENT_3D ( 'NONE', #26556, #106046, #146465 ) ;
#88342 = DIRECTION ( 'NONE',  ( 0.000000000000000000, 6.982962677686266711E-15, -1.000000000000000000 ) ) ;
#88343 = LINE ( 'NONE', #71400, #103848 ) ;
#88344 = EDGE_CURVE ( 'NONE', #85650, #40168, #194314, .T. ) ;
#88346 = ORIENTED_EDGE ( 'NONE', *, *, #178761, .T. ) ;
#88345 = AXIS2_PLACEMENT_3D ( 'NONE', #129918, #71268, #252431 ) ;
#88348 = DIRECTION ( 'NONE',  ( -1.000000000000000000, -0.000000000000000000, -0.000000000000000000 ) ) ;
#88347 = DIRECTION ( 'NONE',  ( 1.000000000000000000, 0.000000000000000000, 0.000000000000000000 ) ) ;
#88349 = CIRCLE ( 'NONE', #238399, 0.1000000000000028644 ) ;
#88350 = CARTESIAN_POINT ( 'NONE',  ( -21.05000000000000071, 1.115600667400684642E-11, -134.0000000000000000 ) ) ;
#88351 = CARTESIAN_POINT ( 'NONE',  ( 18.52928932188133970, 65.72071067813013201, -44.87310748452439668 ) ) ;
#88352 = CARTESIAN_POINT ( 'NONE',  ( 21.05000000000000426, 18.88693907895052249, -227.8658253555367992 ) ) ;
#88353 = VERTEX_POINT ( 'NONE', #181779 ) ;
#88354 = ORIENTED_EDGE ( 'NONE', *, *, #87017, .F. ) ;
#88355 = CIRCLE ( 'NONE', #17632, 0.1000000000000072220 ) ;
#88356 = ADVANCED_FACE ( 'NONE', ( #202620 ), #239693, .T. ) ;
#88357 = CARTESIAN_POINT ( 'NONE',  ( 20.94999999999999929, -8.999999999988842703, -157.6060308773475640 ) ) ;
#88358 = CARTESIAN_POINT ( 'NONE',  ( -20.54999999999999716, 76.00000000001237765, -170.0231074845243597 ) ) ;
#88359 = ORIENTED_EDGE ( 'NONE', *, *, #99329, .T. ) ;
#88360 = DIRECTION ( 'NONE',  ( 0.000000000000000000, -0.9999176327611369874, 0.01283462868041984617 ) ) ;
#88361 = ORIENTED_EDGE ( 'NONE', *, *, #223133, .F. ) ;
#88362 = DIRECTION ( 'NONE',  ( -1.020425574104004196E-15, 0.000000000000000000, 1.000000000000000000 ) ) ;
#88363 = AXIS2_PLACEMENT_3D ( 'NONE', #180955, #84355, #4842 ) ;
#88364 = VERTEX_POINT ( 'NONE', #120542 ) ;
#88365 = EDGE_CURVE ( 'NONE', #54771, #130997, #162237, .T. ) ;
#88366 = LINE ( 'NONE', #87089, #182481 ) ;
#88367 = CARTESIAN_POINT ( 'NONE',  ( 18.50000000000000000, 85.50000000001185185, -96.42291809330220076 ) ) ;
#88368 = ORIENTED_EDGE ( 'NONE', *, *, #214270, .T. ) ;
#88369 = ADVANCED_FACE ( 'NONE', ( #80062 ), #177937, .F. ) ;
#88370 = CARTESIAN_POINT ( 'NONE',  ( -16.80117486205003274, 63.08576339494070595, -213.1288165000758568 ) ) ;
#88371 = CIRCLE ( 'NONE', #234130, 11.70000000000000995 ) ;
#88372 = TOROIDAL_SURFACE ( 'NONE', #100822, 12.77499999999999858, 0.1000000000000000056 ) ;
#88373 = ORIENTED_EDGE ( 'NONE', *, *, #225496, .T. ) ;
#88375 = ORIENTED_EDGE ( 'NONE', *, *, #124761, .T. ) ;
#88374 = CIRCLE ( 'NONE', #175732, 2.000000000000002665 ) ;
#88376 = ORIENTED_EDGE ( 'NONE', *, *, #164431, .F. ) ;
#88377 = DIRECTION ( 'NONE',  ( 7.304098846218134667E-16, 1.000000000000000000, 6.982962677686267499E-15 ) ) ;
#88378 = DIRECTION ( 'NONE',  ( 0.000000000000000000, -1.000000000000000000, -0.000000000000000000 ) ) ;
#88379 = CARTESIAN_POINT ( 'NONE',  ( -21.08078803292166725, 0.07918598716886143807, -127.6669870355628973 ) ) ;
#88380 = CARTESIAN_POINT ( 'NONE',  ( 20.94999999999999929, 8.776282895303628706, -109.0586289951409924 ) ) ;
#88381 = CARTESIAN_POINT ( 'NONE',  ( -16.88460203013675454, 9.954759003235713166, -20.86589180953822975 ) ) ;
#88382 = EDGE_CURVE ( 'NONE', #51736, #190222, #138752, .T. ) ;
#88384 = DIRECTION ( 'NONE',  ( 0.000000000000000000, 0.2617529984165152257, 0.9651348961777124202 ) ) ;
#88383 = CARTESIAN_POINT ( 'NONE',  ( -22.50000000000000000, 1.115600667400684642E-11, -67.00000000000004263 ) ) ;
#88386 = ORIENTED_EDGE ( 'NONE', *, *, #236932, .F. ) ;
#88385 = CYLINDRICAL_SURFACE ( 'NONE', #93914, 0.09999999999999781286 ) ;
#88387 = DIRECTION ( 'NONE',  ( 0.000000000000000000, 0.8814952561688437216, -0.4721928772777334582 ) ) ;
#88388 = EDGE_LOOP ( 'NONE', ( #254441, #54657 ) ) ;
#88389 = DIRECTION ( 'NONE',  ( 0.000000000000000000, 1.000000000000000000, -0.000000000000000000 ) ) ;
#88390 = ORIENTED_EDGE ( 'NONE', *, *, #213553, .F. ) ;
#88391 = ORIENTED_EDGE ( 'NONE', *, *, #206301, .F. ) ;
#88392 = CARTESIAN_POINT ( 'NONE',  ( 18.59999999999999076, 77.14957036958705316, -28.20719500002235236 ) ) ;
#88393 = CYLINDRICAL_SURFACE ( 'NONE', #6132, 0.09999999999999568956 ) ;
#88394 = CARTESIAN_POINT ( 'NONE',  ( 20.94999999999999574, 64.21185867012613357, -224.4479740254296303 ) ) ;
#88395 = CARTESIAN_POINT ( 'NONE',  ( -20.85000000000000142, 36.22724532936083364, -235.9903003947922286 ) ) ;
#88396 = TOROIDAL_SURFACE ( 'NONE', #192477, 6.258578643762700899, 0.1000000000000000056 ) ;
#88397 = DIRECTION ( 'NONE',  ( 0.000000000000000000, -1.000000000000000000, 0.000000000000000000 ) ) ;
#88398 = ORIENTED_EDGE ( 'NONE', *, *, #110503, .F. ) ;
#88400 = VERTEX_POINT ( 'NONE', #239179 ) ;
#88399 = B_SPLINE_CURVE_WITH_KNOTS ( 'NONE', 3,
 ( #83594, #23692, #184011, #201021, #225676, #43230 ),
 .UNSPECIFIED., .F., .F.,
 ( 4, 2, 4 ),
 ( 0.000000000000000000, 0.0001497467027049268525, 0.0002994934054098537051 ),
 .UNSPECIFIED. ) ;
#88401 = DIRECTION ( 'NONE',  ( 0.000000000000000000, -1.000000000000000000, 0.000000000000000000 ) ) ;
#88402 = VERTEX_POINT ( 'NONE', #217028 ) ;
#88403 = CARTESIAN_POINT ( 'NONE',  ( -22.42357213249529480, 0.09908696401271366305, -126.3270676136400965 ) ) ;
#88404 = CARTESIAN_POINT ( 'NONE',  ( 21.14999999999999858, 1.115600667400684642E-11, -160.9593430482987344 ) ) ;
#88405 = ORIENTED_EDGE ( 'NONE', *, *, #55797, .T. ) ;
#88406 = CARTESIAN_POINT ( 'NONE',  ( 20.94999999999999929, 85.00000000001179501, -79.41707660717668205 ) ) ;
#88407 = DIRECTION ( 'NONE',  ( -1.000000000000000000, 0.000000000000000000, 0.000000000000000000 ) ) ;
#88408 = CARTESIAN_POINT ( 'NONE',  ( 21.15000000000005542, 64.35000000001120668, -3.123107484524795474 ) ) ;
#88409 = DIRECTION ( 'NONE',  ( 0.000000000000000000, 0.4721928772777346239, 0.8814952561688430555 ) ) ;
#88410 = ORIENTED_EDGE ( 'NONE', *, *, #163298, .F. ) ;
#88411 = DIRECTION ( 'NONE',  ( 1.000000000000000000, 0.000000000000000000, 0.000000000000000000 ) ) ;
#88412 = DIRECTION ( 'NONE',  ( 1.000000000000000000, 7.304098846218135653E-16, 0.000000000000000000 ) ) ;
#88413 = CARTESIAN_POINT ( 'NONE',  ( -18.50000000000000000, 10.29270135740182823, -38.95736188715194714 ) ) ;
#88414 = CARTESIAN_POINT ( 'NONE',  ( -22.50000000000000000, 1.115600667400684642E-11, -167.3999999999999773 ) ) ;
#88415 = CARTESIAN_POINT ( 'NONE',  ( -21.05000000000000071, -11.48912529306490349, -136.9000000000000341 ) ) ;
#88416 = CARTESIAN_POINT ( 'NONE',  ( 21.14999999999999858, 8.985508020264692419, -211.4778645542876347 ) ) ;
#88417 = ADVANCED_FACE ( 'NONE', ( #257393 ), #54756, .F. ) ;
#88418 = ORIENTED_EDGE ( 'NONE', *, *, #30630, .F. ) ;
#88419 = EDGE_LOOP ( 'NONE', ( #204192, #140301, #249781, #14976 ) ) ;
#88420 = EDGE_CURVE ( 'NONE', #19526, #74676, #173681, .T. ) ;
#88421 = FACE_OUTER_BOUND ( 'NONE', #4901, .T. ) ;
#88422 = DIRECTION ( 'NONE',  ( 0.000000000000000000, 0.000000000000000000, 1.000000000000000000 ) ) ;
#88423 = CARTESIAN_POINT ( 'NONE',  ( 21.06277459767443005, 61.86219876617301594, -221.7541226652555224 ) ) ;
#88424 = DIRECTION ( 'NONE',  ( 1.000000000000000000, -0.000000000000000000, -0.000000000000000000 ) ) ;
#88425 = ORIENTED_EDGE ( 'NONE', *, *, #146712, .F. ) ;
#88426 = CARTESIAN_POINT ( 'NONE',  ( 20.94999999999999929, 1.115600667400684642E-11, -100.5000000000000426 ) ) ;
#88427 = LINE ( 'NONE', #109288, #73379 ) ;
#88428 = ADVANCED_FACE ( 'NONE', ( #9547 ), #168997, .F. ) ;
#88429 = EDGE_CURVE ( 'NONE', #230164, #257624, #227209, .T. ) ;
#88430 = CARTESIAN_POINT ( 'NONE',  ( 18.39999999999999858, 78.24072131640578220, -231.5548844243369047 ) ) ;
#88431 = CARTESIAN_POINT ( 'NONE',  ( -20.54999999999999716, 68.75000000001151079, -48.27310748452437394 ) ) ;
#88432 = TOROIDAL_SURFACE ( 'NONE', #155139, 1.900000000000002576, 0.1000000000000000056 ) ;
#88434 = CARTESIAN_POINT ( 'NONE',  ( -23.15000000000000213, -9.499999999988848032, -76.89396912265249284 ) ) ;
#88433 = AXIS2_PLACEMENT_3D ( 'NONE', #117409, #199538, #256863 ) ;
#88435 = ORIENTED_EDGE ( 'NONE', *, *, #129617, .F. ) ;
#88436 = ORIENTED_EDGE ( 'NONE', *, *, #58117, .T. ) ;
#88437 = SPHERICAL_SURFACE ( 'NONE', #208221, 0.1000000000000000056 ) ;
#88439 = DIRECTION ( 'NONE',  ( -1.000000000000000000, -0.000000000000000000, -0.000000000000000000 ) ) ;
#88438 = VECTOR ( 'NONE', #144512, 1000.000000000000000 ) ;
#88440 = DIRECTION ( 'NONE',  ( 0.000000000000000000, 0.1298341882519953583, 0.9915357197604862671 ) ) ;
#88441 = FACE_OUTER_BOUND ( 'NONE', #18940, .T. ) ;
#88442 = ADVANCED_FACE ( 'NONE', ( #248170 ), #244302, .T. ) ;
#88443 = ORIENTED_EDGE ( 'NONE', *, *, #142114, .T. ) ;
#88444 = DIRECTION ( 'NONE',  ( -1.000000000000000000, -0.000000000000000000, -0.000000000000000000 ) ) ;
#88445 = EDGE_CURVE ( 'NONE', #91362, #1674, #48673, .T. ) ;
#88446 = ITEM_DEFINED_TRANSFORMATION ( 'NONE', 'NONE', #177785,  #2425 ) ;
#88447 = DIRECTION ( 'NONE',  ( -0.000000000000000000, 0.2617529984165031243, 0.9651348961777157509 ) ) ;
#88448 = VECTOR ( 'NONE', #50172, 1000.000000000000000 ) ;
#88449 = ORIENTED_EDGE ( 'NONE', *, *, #158933, .F. ) ;
#88450 = CIRCLE ( 'NONE', #46771, 0.1000000000000055844 ) ;
#88451 = DIRECTION ( 'NONE',  ( 1.000000000000000000, 3.265361837132813093E-16, -0.000000000000000000 ) ) ;
#88452 = EDGE_LOOP ( 'NONE', ( #2407, #21029, #118762, #46155 ) ) ;
#88453 = ORIENTED_EDGE ( 'NONE', *, *, #160687, .T. ) ;
#88454 = ADVANCED_FACE ( 'NONE', ( #5674 ), #168684, .F. ) ;
#88455 = AXIS2_PLACEMENT_3D ( 'NONE', #102979, #60002, #220392 ) ;
#88456 = EDGE_LOOP ( 'NONE', ( #68739, #149107, #157701, #223964, #236799 ) ) ;
#88457 = ADVANCED_FACE ( 'NONE', ( #228622 ), #205168, .T. ) ;
#88458 = CARTESIAN_POINT ( 'NONE',  ( -22.50000000000094147, 75.89914163091340527, -114.7726746080137303 ) ) ;
#88459 = ADVANCED_FACE ( 'NONE', ( #83907 ), #163497, .T. ) ;
#88460 = DIRECTION ( 'NONE',  ( 0.000000000000000000, -6.982962677686266711E-15, 1.000000000000000000 ) ) ;
#88461 = CARTESIAN_POINT ( 'NONE',  ( 23.15000000000000213, 87.65000000001246860, -173.1231074845242688 ) ) ;
#88462 = CARTESIAN_POINT ( 'NONE',  ( -23.15000000000000213, 70.10000000001251408, -180.2422072491807796 ) ) ;
#88464 = AXIS2_PLACEMENT_3D ( 'NONE', #133676, #56670, #57970 ) ;
#88463 = DIRECTION ( 'NONE',  ( -2.489438768765009500E-17, -0.1686199900910313187, 0.9856811345164828708 ) ) ;
#88466 = CARTESIAN_POINT ( 'NONE',  ( -21.05000000000000071, -1.835341550213255957, -78.65515129256301918 ) ) ;
#88465 = AXIS2_PLACEMENT_3D ( 'NONE', #235767, #19298, #54565 ) ;
#88467 = AXIS2_PLACEMENT_3D ( 'NONE', #31460, #110958, #254299 ) ;
#88468 = CARTESIAN_POINT ( 'NONE',  ( -16.93772744219066340, 9.993541108752353352, -12.59806197196970068 ) ) ;
#88471 = FACE_OUTER_BOUND ( 'NONE', #178676, .T. ) ;
#88470 = CIRCLE ( 'NONE', #229973, 0.1000000000000024342 ) ;
#88469 = CARTESIAN_POINT ( 'NONE',  ( -23.15000000000000213, 68.69389471299010097, -223.1641309873017462 ) ) ;
#88472 = CARTESIAN_POINT ( 'NONE',  ( 21.05000000000000426, -1.300211140951535116, -194.8661069862146178 ) ) ;
#88473 = CARTESIAN_POINT ( 'NONE',  ( -16.88560720703333473, 9.950564843760847822, -113.1481119208637551 ) ) ;
#88474 = CARTESIAN_POINT ( 'NONE',  ( -21.14999999999999858, -2.576749817950532595, -189.6385361693310756 ) ) ;
#88475 = CARTESIAN_POINT ( 'NONE',  ( 20.95052659398289308, 18.75486878932230184, -228.0717596309566204 ) ) ;
#88476 = VERTEX_POINT ( 'NONE', #143921 ) ;
#88477 = VERTEX_POINT ( 'NONE', #223451 ) ;
#88478 = CARTESIAN_POINT ( 'NONE',  ( -18.40904629823847216, -9.500000000000007105, -40.10018956248171662 ) ) ;
#88479 = DIRECTION ( 'NONE',  ( -1.000000000000000000, -0.000000000000000000, -0.000000000000000000 ) ) ;
#88481 = CARTESIAN_POINT ( 'NONE',  ( -14.77538296656415007, 13.11968191886198376, -216.8952266020228308 ) ) ;
#88480 = CARTESIAN_POINT ( 'NONE',  ( -16.97092634996668181, 10.00088896635978486, -154.8698572337025325 ) ) ;
#88482 = ADVANCED_FACE ( 'NONE', ( #185629 ), #104767, .T. ) ;
#88483 = CARTESIAN_POINT ( 'NONE',  ( 20.95132126680579887, 39.27898052006931806, -236.8829280990189829 ) ) ;
#88484 = DIRECTION ( 'NONE',  ( 2.952720810173289112E-16, 0.4088369013363287729, -0.9126074666063767049 ) ) ;
#88485 = CARTESIAN_POINT ( 'NONE',  ( -21.14999999999999858, 6.390846877240202950, -199.6081416912452653 ) ) ;
#88486 = ORIENTED_EDGE ( 'NONE', *, *, #83230, .T. ) ;
#88487 = VERTEX_POINT ( 'NONE', #166098 ) ;
#88488 = EDGE_CURVE ( 'NONE', #224829, #2708, #245607, .T. ) ;
#88489 = DIRECTION ( 'NONE',  ( -0.000000000000000000, -0.000000000000000000, -1.000000000000000000 ) ) ;
#88490 = VERTEX_POINT ( 'NONE', #210337 ) ;
#88491 = DIRECTION ( 'NONE',  ( -1.000000000000000000, -7.136802563874199107E-16, -1.554319503706929991E-16 ) ) ;
#88492 = AXIS2_PLACEMENT_3D ( 'NONE', #36090, #70946, #30522 ) ;
#88493 = AXIS2_PLACEMENT_3D ( 'NONE', #247762, #204769, #224343 ) ;
#88494 = DIRECTION ( 'NONE',  ( 0.000000000000000000, 0.000000000000000000, 1.000000000000000000 ) ) ;
#88495 = ORIENTED_EDGE ( 'NONE', *, *, #145357, .F. ) ;
#88496 = CARTESIAN_POINT ( 'NONE',  ( -18.50596464788227635, 18.37039103902859694, -236.9176190769589141 ) ) ;
#88497 = ADVANCED_FACE ( 'NONE', ( #229892 ), #231195, .F. ) ;
#88498 = CIRCLE ( 'NONE', #59258, 0.09999999999999459321 ) ;
#88499 = ORIENTED_EDGE ( 'NONE', *, *, #146802, .F. ) ;
#88500 = LINE ( 'NONE', #105490, #91371 ) ;
#88501 = LINE ( 'NONE', #190211, #253508 ) ;
#88503 = AXIS2_PLACEMENT_3D ( 'NONE', #257718, #235637, #60848 ) ;
#88502 = DIRECTION ( 'NONE',  ( 4.336808689942128965E-15, -0.8660254037844367092, 0.5000000000000037748 ) ) ;
#88504 = EDGE_CURVE ( 'NONE', #211450, #218485, #135625, .T. ) ;
#88505 = DIRECTION ( 'NONE',  ( 0.000000000000000000, -1.000000000000000000, 0.000000000000000000 ) ) ;
#88506 = FACE_OUTER_BOUND ( 'NONE', #233101, .T. ) ;
#88507 = DIRECTION ( 'NONE',  ( 0.000000000000000000, -1.000000000000000000, -6.982962677686266711E-15 ) ) ;
#88508 = CIRCLE ( 'NONE', #184386, 0.1000000000000106498 ) ;
#88509 = CARTESIAN_POINT ( 'NONE',  ( 23.14999999999998437, 4.050000000011155343, -33.50000000000000000 ) ) ;
#88511 = CARTESIAN_POINT ( 'NONE',  ( 23.15000000000000213, 87.39257802171711376, -39.09705706435617856 ) ) ;
#88510 = TOROIDAL_SURFACE ( 'NONE', #176059, 0.9750000000000019762, 0.1000000000000000056 ) ;
#88512 = EDGE_CURVE ( 'NONE', #50036, #103521, #240271, .T. ) ;
#88513 = AXIS2_PLACEMENT_3D ( 'NONE', #174681, #254145, #75551 ) ;
#88515 = ORIENTED_EDGE ( 'NONE', *, *, #141510, .F. ) ;
#88514 = CARTESIAN_POINT ( 'NONE',  ( 20.97250901189795513, 65.37543196631021658, -128.8585617675573758 ) ) ;
#88517 = FACE_OUTER_BOUND ( 'NONE', #137197, .T. ) ;
#88516 = CARTESIAN_POINT ( 'NONE',  ( -21.05000000000000071, 77.83534155023627932, -91.46795619196132066 ) ) ;
#88518 = ORIENTED_EDGE ( 'NONE', *, *, #34849, .F. ) ;
#88520 = ORIENTED_EDGE ( 'NONE', *, *, #221203, .F. ) ;
#88519 = DIRECTION ( 'NONE',  ( 0.000000000000000000, 6.982962677686266711E-15, -1.000000000000000000 ) ) ;
#88521 = ORIENTED_EDGE ( 'NONE', *, *, #163325, .F. ) ;
#88522 = FACE_OUTER_BOUND ( 'NONE', #49598, .T. ) ;
#88523 = CIRCLE ( 'NONE', #196868, 2.000000000000001776 ) ;
#88524 = DIRECTION ( 'NONE',  ( 0.000000000000000000, 0.000000000000000000, 1.000000000000000000 ) ) ;
#88525 = VECTOR ( 'NONE', #185105, 1000.000000000000000 ) ;
#88526 = EDGE_CURVE ( 'NONE', #30427, #33613, #81438, .T. ) ;
#88527 = ADVANCED_FACE ( 'NONE', ( #33024 ), #95508, .T. ) ;
#88528 = DIRECTION ( 'NONE',  ( 0.000000000000000000, 0.000000000000000000, -1.000000000000000000 ) ) ;
#88529 = CARTESIAN_POINT ( 'NONE',  ( -18.59999999999999787, 77.83585931145600512, -158.5186683157258187 ) ) ;
#88530 = DIRECTION ( 'NONE',  ( 1.000000000000000000, 0.000000000000000000, 0.000000000000000000 ) ) ;
#88531 = CARTESIAN_POINT ( 'NONE',  ( -23.25000000000000000, 4.349999999999999645, -12.15000000000000391 ) ) ;
#88532 = CIRCLE ( 'NONE', #200808, 0.09999999999999939493 ) ;
#88533 = CARTESIAN_POINT ( 'NONE',  ( -18.37013991200266005, 13.19560622132187078, -207.5489386142775174 ) ) ;
#88534 = CARTESIAN_POINT ( 'NONE',  ( 23.15000000000000213, 87.65000000001192859, -106.0231074845242176 ) ) ;
#88535 = AXIS2_PLACEMENT_3D ( 'NONE', #230878, #52200, #15693 ) ;
#88536 = CARTESIAN_POINT ( 'NONE',  ( -23.15000000000000213, -11.48912529306489994, -197.9999999999999432 ) ) ;
#88537 = AXIS2_PLACEMENT_3D ( 'NONE', #198058, #83217, #80658 ) ;
#88538 = VERTEX_POINT ( 'NONE', #154253 ) ;
#88539 = ORIENTED_EDGE ( 'NONE', *, *, #31581, .F. ) ;
#88540 = DIRECTION ( 'NONE',  ( 0.000000000000000000, 0.9126074666063783702, 0.4088369013363252757 ) ) ;
#88541 = ADVANCED_FACE ( 'NONE', ( #235035 ), #233754, .T. ) ;
#88543 = ORIENTED_EDGE ( 'NONE', *, *, #76129, .F. ) ;
#88542 = B_SPLINE_CURVE_WITH_KNOTS ( 'NONE', 3,
 ( #254666, #93062, #232611, #175226, #172663, #55191, #211749 ),
 .UNSPECIFIED., .F., .F.,
 ( 4, 3, 4 ),
 ( 0.000000000000000000, 3.882884552234292441E-05, 5.798605692158292918E-05 ),
 .UNSPECIFIED. ) ;
#88544 = DIRECTION ( 'NONE',  ( -0.000000000000000000, 0.9770955615653313941, 0.2128009952263603954 ) ) ;
#88546 = ADVANCED_FACE ( 'NONE', ( #253290 ), #134615, .F. ) ;
#88545 = ORIENTED_EDGE ( 'NONE', *, *, #52927, .T. ) ;
#88548 = CIRCLE ( 'NONE', #138592, 0.09999999999998807065 ) ;
#88547 = CARTESIAN_POINT ( 'NONE',  ( -20.94999999999999929, -1.162701749926853712, -41.60000000000000142 ) ) ;
#88549 = DIRECTION ( 'NONE',  ( -1.000000000000000000, 0.000000000000000000, 0.000000000000000000 ) ) ;
#88550 = CARTESIAN_POINT ( 'NONE',  ( -20.94999999999999929, -10.72348020702290583, -206.5081278352411402 ) ) ;
#88551 = ADVANCED_FACE ( 'NONE', ( #171251 ), #94493, .T. ) ;
#88552 = AXIS2_PLACEMENT_3D ( 'NONE', #241983, #180740, #140299 ) ;
#88553 = DIRECTION ( 'NONE',  ( 0.000000000000000000, -0.8660254037844411501, -0.4999999999999956146 ) ) ;
#88554 = LINE ( 'NONE', #14200, #24652 ) ;
#88555 = ORIENTED_EDGE ( 'NONE', *, *, #191298, .T. ) ;
#88556 = CARTESIAN_POINT ( 'NONE',  ( -20.94999999999999929, 76.00000000001190870, -103.0231074845243029 ) ) ;
#88557 = CARTESIAN_POINT ( 'NONE',  ( -18.40000000000000213, 13.78091005366907140, -222.8171174488881832 ) ) ;
#88558 = LINE ( 'NONE', #105537, #211223 ) ;
#88559 = FACE_OUTER_BOUND ( 'NONE', #20577, .T. ) ;
#88561 = VERTEX_POINT ( 'NONE', #72115 ) ;
#88560 = EDGE_CURVE ( 'NONE', #102673, #138714, #89831, .T. ) ;
#88563 = DIRECTION ( 'NONE',  ( -1.000000000000000000, 0.000000000000000000, 0.000000000000000000 ) ) ;
#88562 = FACE_OUTER_BOUND ( 'NONE', #72888, .T. ) ;
#88564 = AXIS2_PLACEMENT_3D ( 'NONE', #257763, #141714, #79164 ) ;
#88565 = ORIENTED_EDGE ( 'NONE', *, *, #147777, .T. ) ;
#88568 = VERTEX_POINT ( 'NONE', #151670 ) ;
#88567 = DIRECTION ( 'NONE',  ( 1.000000000000000000, 0.000000000000000000, 0.000000000000000000 ) ) ;
#88566 = CARTESIAN_POINT ( 'NONE',  ( -18.59999999999999787, 46.45388641681647357, -243.1520440498138385 ) ) ;
#88569 = CIRCLE ( 'NONE', #167722, 4.000000000000003553 ) ;
#88570 = ORIENTED_EDGE ( 'NONE', *, *, #114393, .T. ) ;
#88571 = DIRECTION ( 'NONE',  ( 1.000000000000000000, 0.000000000000000000, 0.000000000000000000 ) ) ;
#88572 = AXIS2_PLACEMENT_3D ( 'NONE', #26891, #148098, #85509 ) ;
#88573 = DIRECTION ( 'NONE',  ( -1.000000000000000000, 0.000000000000000000, 0.000000000000000000 ) ) ;
#88574 = ADVANCED_FACE ( 'NONE', ( #254554 ), #75955, .T. ) ;
#88575 = CARTESIAN_POINT ( 'NONE',  ( 23.14999999999999503, 11.65000000001116298, -188.8499999999999659 ) ) ;
#88576 = VERTEX_POINT ( 'NONE', #214182 ) ;
#88577 = DIRECTION ( 'NONE',  ( 0.000000000000000000, 1.000000000000000000, -6.308085367188393199E-16 ) ) ;
#88578 = DIRECTION ( 'NONE',  ( -0.000000000000000000, 0.9126074666063770380, 0.4088369013363281068 ) ) ;
#88580 = FACE_OUTER_BOUND ( 'NONE', #142747, .T. ) ;
#88579 = DIRECTION ( 'NONE',  ( 0.000000000000000000, 0.000000000000000000, -1.000000000000000000 ) ) ;
#88581 = EDGE_CURVE ( 'NONE', #136977, #182052, #57061, .T. ) ;
#88583 = ORIENTED_EDGE ( 'NONE', *, *, #23722, .T. ) ;
#88582 = DIRECTION ( 'NONE',  ( 0.000000000000000000, 0.8814952561688430555, -0.4721928772777346239 ) ) ;
#88584 = ORIENTED_EDGE ( 'NONE', *, *, #103385, .F. ) ;
#88585 = CARTESIAN_POINT ( 'NONE',  ( 20.04142135623731136, 64.25000000001176659, -78.37310748452439668 ) ) ;
#88586 = DIRECTION ( 'NONE',  ( 0.000000000000000000, -0.9651348961777157509, 0.2617529984165028467 ) ) ;
#88587 = DIRECTION ( 'NONE',  ( 0.000000000000000000, 0.000000000000000000, -1.000000000000000000 ) ) ;
#88588 = ORIENTED_EDGE ( 'NONE', *, *, #229983, .T. ) ;
#88589 = FACE_OUTER_BOUND ( 'NONE', #128284, .T. ) ;
#88590 = AXIS2_PLACEMENT_3D ( 'NONE', #133086, #169683, #212628 ) ;
#88591 = EDGE_CURVE ( 'NONE', #143659, #86809, #35569, .T. ) ;
#88592 = DIRECTION ( 'NONE',  ( 1.000000000000000000, 0.000000000000000000, 0.000000000000000000 ) ) ;
#88593 = CARTESIAN_POINT ( 'NONE',  ( 23.24999999999999645, 1.148907358139439339E-11, -201.0000000000015064 ) ) ;
#88594 = ORIENTED_EDGE ( 'NONE', *, *, #5128, .T. ) ;
#88595 = DIRECTION ( 'NONE',  ( 1.000000000000000000, 0.000000000000000000, 0.000000000000000000 ) ) ;
#88596 = EDGE_LOOP ( 'NONE', ( #46948, #95529, #177254, #63517 ) ) ;
#88597 = CARTESIAN_POINT ( 'NONE',  ( 0.9000000000000014655, -11.75000000000000000, 28.70000000000000284 ) ) ;
#88598 = DIRECTION ( 'NONE',  ( 0.000000000000000000, 0.000000000000000000, 1.000000000000000000 ) ) ;
#88600 = ORIENTED_EDGE ( 'NONE', *, *, #128672, .F. ) ;
#88599 = CIRCLE ( 'NONE', #172051, 4.100000000000006750 ) ;
#88601 = ORIENTED_EDGE ( 'NONE', *, *, #44171, .T. ) ;
#88602 = CARTESIAN_POINT ( 'NONE',  ( 18.39999999999997371, 64.25000000001161027, -60.27310748452440947 ) ) ;
#88603 = EDGE_CURVE ( 'NONE', #247441, #64278, #82002, .T. ) ;
#88604 = ORIENTED_EDGE ( 'NONE', *, *, #33601, .F. ) ;
#88606 = ORIENTED_EDGE ( 'NONE', *, *, #66657, .T. ) ;
#88605 = CARTESIAN_POINT ( 'NONE',  ( -22.50047199487879368, 0.04490605193130675632, -155.7499525810887633 ) ) ;
#88607 = SHAPE_REPRESENTATION ( 'Injection Molded Chain Links 5', ( #2425 ), #193986 ) ;
#88608 = ORIENTED_EDGE ( 'NONE', *, *, #115274, .F. ) ;
#88610 = ORIENTED_EDGE ( 'NONE', *, *, #8157, .T. ) ;
#88609 = ORIENTED_EDGE ( 'NONE', *, *, #137613, .F. ) ;
#88611 = DIRECTION ( 'NONE',  ( 0.000000000000000000, -1.000000000000000000, -6.982962677686266711E-15 ) ) ;
#88612 = VECTOR ( 'NONE', #131119, 1000.000000000000227 ) ;
#88613 = ORIENTED_EDGE ( 'NONE', *, *, #70333, .F. ) ;
#88614 = DIRECTION ( 'NONE',  ( 0.000000000000000000, -3.447762908503805145E-13, 1.000000000000000000 ) ) ;
#88616 = EDGE_CURVE ( 'NONE', #247736, #242182, #219393, .T. ) ;
#88615 = CARTESIAN_POINT ( 'NONE',  ( -21.04999999999999716, -1.448645706476685335, -194.7513245572836809 ) ) ;
#88617 = CARTESIAN_POINT ( 'NONE',  ( 20.94999999999999929, -3.770473190032740174, -225.9805569534692324 ) ) ;
#88618 = CARTESIAN_POINT ( 'NONE',  ( -18.50000000000001066, 86.96699927712943179, -199.3055931863049466 ) ) ;
#88619 = EDGE_LOOP ( 'NONE', ( #18016, #157721, #177555, #175563 ) ) ;
#88620 = EDGE_LOOP ( 'NONE', ( #5064, #29695, #236619 ) ) ;
#88621 = CIRCLE ( 'NONE', #176164, 0.09999999999999939493 ) ;
#88622 = DIRECTION ( 'NONE',  ( 1.000000000000000000, 0.000000000000000000, 0.000000000000000000 ) ) ;
#88624 = EDGE_LOOP ( 'NONE', ( #63971, #178533, #128785, #41249 ) ) ;
#88623 = CARTESIAN_POINT ( 'NONE',  ( 18.49999999999999289, 63.83083047455526327, -209.3924252461221158 ) ) ;
#88625 = CARTESIAN_POINT ( 'NONE',  ( -23.15000000000000213, 87.41227409416215721, -173.0231074845243029 ) ) ;
#88627 = ORIENTED_EDGE ( 'NONE', *, *, #11629, .T. ) ;
#88626 = CARTESIAN_POINT ( 'NONE',  ( 18.39999999999999858, -9.599999999988842347, -174.5320693966996259 ) ) ;
#88628 = ORIENTED_EDGE ( 'NONE', *, *, #77324, .F. ) ;
#88629 = DIRECTION ( 'NONE',  ( -1.000000000000000000, 0.000000000000000000, 0.000000000000000000 ) ) ;
#88630 = CIRCLE ( 'NONE', #172088, 0.09999999999999939493 ) ;
#88631 = VECTOR ( 'NONE', #182274, 1000.000000000000000 ) ;
#88632 = EDGE_LOOP ( 'NONE', ( #208623, #195354 ) ) ;
#88634 = CARTESIAN_POINT ( 'NONE',  ( 23.15000000000000213, -8.999999999988842703, -124.1060308773475924 ) ) ;
#88633 = ADVANCED_BREP_SHAPE_REPRESENTATION ( '', ( #110572, #2425 ), #252581 ) ;
#88635 = CYLINDRICAL_SURFACE ( 'NONE', #6961, 12.87499999999999822 ) ;
#88636 = B_SPLINE_CURVE_WITH_KNOTS ( 'NONE', 3,
 ( #184343, #87795, #49971, #5686, #85214, #106069 ),
 .UNSPECIFIED., .F., .F.,
 ( 4, 2, 4 ),
 ( 0.000000000000000000, 0.0002113392456165986782, 0.0004226784912331973563 ),
 .UNSPECIFIED. ) ;
#88638 = ORIENTED_EDGE ( 'NONE', *, *, #230374, .T. ) ;
#88637 = VERTEX_POINT ( 'NONE', #252011 ) ;
#88639 = ORIENTED_EDGE ( 'NONE', *, *, #246872, .T. ) ;
#88640 = LINE ( 'NONE', #87365, #140334 ) ;
#88641 = ORIENTED_EDGE ( 'NONE', *, *, #206696, .F. ) ;
#88642 = VERTEX_POINT ( 'NONE', #90367 ) ;
#88644 = CARTESIAN_POINT ( 'NONE',  ( -23.49999999999994316, 77.83551161375991967, -47.52760213295649550 ) ) ;
#88643 = VECTOR ( 'NONE', #75269, 1000.000000000000000 ) ;
#88646 = ORIENTED_EDGE ( 'NONE', *, *, #104890, .F. ) ;
#88645 = DIRECTION ( 'NONE',  ( 1.000000000000000000, 0.000000000000000000, 0.000000000000000000 ) ) ;
#88647 = CARTESIAN_POINT ( 'NONE',  ( 20.94999999999999929, -1.835341550213257733, -45.05515129256298223 ) ) ;
#88648 = DIRECTION ( 'NONE',  ( -1.000000000000000000, 3.469446951953635015E-14, 0.000000000000000000 ) ) ;
#88649 = LINE ( 'NONE', #28758, #61574 ) ;
#88650 = CARTESIAN_POINT ( 'NONE',  ( -18.59999999999999787, 74.73788286442776041, -233.7359682632885267 ) ) ;
#88651 = ORIENTED_EDGE ( 'NONE', *, *, #157153, .F. ) ;
#88652 = VECTOR ( 'NONE', #249486, 1000.000000000000000 ) ;
#88653 = AXIS2_PLACEMENT_3D ( 'NONE', #254960, #76374, #155957 ) ;
#88654 = EDGE_CURVE ( 'NONE', #111853, #45933, #249467, .T. ) ;
#88655 = ORIENTED_EDGE ( 'NONE', *, *, #198879, .F. ) ;
#88656 = AXIS2_PLACEMENT_3D ( 'NONE', #164064, #182350, #241038 ) ;
#88657 = DIRECTION ( 'NONE',  ( -1.000000000000000000, -0.000000000000000000, -0.000000000000000000 ) ) ;
#88658 = CARTESIAN_POINT ( 'NONE',  ( 21.05000000000000071, 85.00000000001197975, -112.4170766071766678 ) ) ;
#88659 = ORIENTED_EDGE ( 'NONE', *, *, #149868, .F. ) ;
#88660 = DIRECTION ( 'NONE',  ( 0.000000000000000000, -7.116814260417668513E-15, 1.000000000000000000 ) ) ;
#88661 = VERTEX_POINT ( 'NONE', #180200 ) ;
#88662 = ORIENTED_EDGE ( 'NONE', *, *, #102171, .T. ) ;
#88663 = EDGE_CURVE ( 'NONE', #227765, #202185, #119459, .T. ) ;
#88664 = DIRECTION ( 'NONE',  ( 1.000000000000000000, -0.000000000000000000, -0.000000000000000000 ) ) ;
#88665 = LINE ( 'NONE', #247766, #244475 ) ;
#88666 = VERTEX_POINT ( 'NONE', #141067 ) ;
#88667 = FACE_OUTER_BOUND ( 'NONE', #92127, .T. ) ;
#88668 = DIRECTION ( 'NONE',  ( -0.000000000000000000, 0.4721928772777345684, 0.8814952561688429444 ) ) ;
#88669 = ORIENTED_EDGE ( 'NONE', *, *, #246642, .T. ) ;
#88670 = FACE_OUTER_BOUND ( 'NONE', #94841, .T. ) ;
#88671 = CARTESIAN_POINT ( 'NONE',  ( -20.54999999999999716, 1.999999999999998224, -20.27537807723789953 ) ) ;
#88673 = DIRECTION ( 'NONE',  ( -1.836970198721029934E-16, 1.000000000000000000, 0.000000000000000000 ) ) ;
#88672 = DIRECTION ( 'NONE',  ( -0.000000000000000000, 1.000000000000000000, -0.000000000000000000 ) ) ;
#88674 = EDGE_CURVE ( 'NONE', #165639, #184724, #116374, .T. ) ;
#88675 = CARTESIAN_POINT ( 'NONE',  ( -22.20000000000000284, 10.88519226655716565, -15.14794223642649840 ) ) ;
#88676 = DIRECTION ( 'NONE',  ( 0.000000000000000000, 0.000000000000000000, 1.000000000000000000 ) ) ;
#88677 = CARTESIAN_POINT ( 'NONE',  ( 18.49999999999999289, -9.419209763398093571, -174.7477694627588392 ) ) ;
#88678 = DIRECTION ( 'NONE',  ( -0.000000000000000000, 1.000000000000000000, 6.982962677686266711E-15 ) ) ;
#88679 = AXIS2_PLACEMENT_3D ( 'NONE', #10787, #242958, #64337 ) ;
#88680 = ADVANCED_FACE ( 'NONE', ( #96762 ), #138461, .F. ) ;
#88681 = EDGE_LOOP ( 'NONE', ( #15059, #194332, #157657 ) ) ;
#88683 = ORIENTED_EDGE ( 'NONE', *, *, #191308, .F. ) ;
#88682 = ORIENTED_EDGE ( 'NONE', *, *, #87313, .F. ) ;
#88684 = ORIENTED_EDGE ( 'NONE', *, *, #167765, .F. ) ;
#88685 = VECTOR ( 'NONE', #99815, 999.9999999999998863 ) ;
#88686 = CYLINDRICAL_SURFACE ( 'NONE', #57354, 0.1000000000000013933 ) ;
#88687 = AXIS2_PLACEMENT_3D ( 'NONE', #17185, #72018, #253199 ) ;
#88688 = DIRECTION ( 'NONE',  ( 1.000000000000000000, -0.000000000000000000, 0.000000000000000000 ) ) ;
#88689 = EDGE_CURVE ( 'NONE', #18989, #72387, #199773, .T. ) ;
#88691 = CARTESIAN_POINT ( 'NONE',  ( -22.50000000000000000, 11.64957080755595520, -33.40000000000000568 ) ) ;
#88690 = FACE_OUTER_BOUND ( 'NONE', #143241, .T. ) ;
#88692 = DIRECTION ( 'NONE',  ( 0.000000000000000000, 0.000000000000000000, -1.000000000000000000 ) ) ;
#88693 = ORIENTED_EDGE ( 'NONE', *, *, #125000, .F. ) ;
#88694 = AXIS2_PLACEMENT_3D ( 'NONE', #237898, #175395, #45802 ) ;
#88695 = CARTESIAN_POINT ( 'NONE',  ( -22.49533356619864577, 11.65000000631534149, -100.4348774196772638 ) ) ;
#88696 = ORIENTED_EDGE ( 'NONE', *, *, #183595, .T. ) ;
#88697 = DIRECTION ( 'NONE',  ( -0.000000000000000000, -0.6132151058540604716, 0.7899159663865477077 ) ) ;
#88699 = EDGE_CURVE ( 'NONE', #72750, #229354, #127847, .T. ) ;
#88698 = VECTOR ( 'NONE', #198927, 1000.000000000000000 ) ;
#88700 = CARTESIAN_POINT ( 'NONE',  ( 18.49999999999999645, 1.866714910068465239, -112.2526752462820525 ) ) ;
#88701 = VECTOR ( 'NONE', #225900, 1000.000000000000000 ) ;
#88702 = CIRCLE ( 'NONE', #92805, 0.9000000000000014655 ) ;
#88703 = CARTESIAN_POINT ( 'NONE',  ( -21.05000000000000071, 1.599488064139765742, -230.7125547273896586 ) ) ;
#88704 = EDGE_LOOP ( 'NONE', ( #77370, #53536, #54421, #201209 ) ) ;
#88705 = CARTESIAN_POINT ( 'NONE',  ( 22.16821283564876666, 7.558973340791918183, -134.0000000000000000 ) ) ;
#88706 = AXIS2_PLACEMENT_3D ( 'NONE', #66126, #128683, #86942 ) ;
#88707 = DIRECTION ( 'NONE',  ( -0.000000000000000000, 1.000000000000000000, 6.982962677686266711E-15 ) ) ;
#88708 = ORIENTED_EDGE ( 'NONE', *, *, #25549, .F. ) ;
#88709 = EDGE_LOOP ( 'NONE', ( #239066, #223549, #41668, #161002 ) ) ;
#88710 = CARTESIAN_POINT ( 'NONE',  ( -21.29999999999995808, 1.115600667400684642E-11, -134.0000000000000000 ) ) ;
#88711 = CARTESIAN_POINT ( 'NONE',  ( 23.15000000000000213, 87.48912529308852015, -173.1231074845242688 ) ) ;
#88712 = FACE_OUTER_BOUND ( 'NONE', #226183, .T. ) ;
#88713 = DIRECTION ( 'NONE',  ( 0.000000000000000000, 0.000000000000000000, 1.000000000000000000 ) ) ;
#88714 = DIRECTION ( 'NONE',  ( 0.000000000000000000, -1.000000000000000000, 0.000000000000000000 ) ) ;
#88716 = AXIS2_PLACEMENT_3D ( 'NONE', #235297, #533, #77486 ) ;
#88715 = CARTESIAN_POINT ( 'NONE',  ( -21.05000000000000071, 6.258842723537645369, 0.03201369318776357137 ) ) ;
#88717 = EDGE_LOOP ( 'NONE', ( #13428, #229931, #251410, #61116 ) ) ;
#88718 = FACE_OUTER_BOUND ( 'NONE', #246789, .T. ) ;
#88720 = EDGE_CURVE ( 'NONE', #62297, #215522, #255823, .T. ) ;
#88719 = DIRECTION ( 'NONE',  ( 0.000000000000000000, -0.2128009952263604232, 0.9770955615653316162 ) ) ;
#88721 = AXIS2_PLACEMENT_3D ( 'NONE', #4533, #84030, #198893 ) ;
#88723 = CARTESIAN_POINT ( 'NONE',  ( -21.04999999999999361, 11.75000000001115374, -174.2838656629781156 ) ) ;
#88722 = CARTESIAN_POINT ( 'NONE',  ( -16.94107738177414291, 10.01423928514777373, -87.95000000000004547 ) ) ;
#88724 = CARTESIAN_POINT ( 'NONE',  ( -20.54999999999999716, 4.250000000011156409, -45.75000000000000711 ) ) ;
#88725 = DIRECTION ( 'NONE',  ( 0.000000000000000000, -7.086529944415886769E-15, 1.000000000000000000 ) ) ;
#88726 = AXIS2_PLACEMENT_3D ( 'NONE', #55543, #136365, #114272 ) ;
#88727 = CARTESIAN_POINT ( 'NONE',  ( -20.85000000000000142, 1.115600667400684642E-11, -141.9000000000000341 ) ) ;
#88728 = CARTESIAN_POINT ( 'NONE',  ( 20.94999999999999929, 10.29270135741298731, -139.4573618871519614 ) ) ;
#88730 = EDGE_LOOP ( 'NONE', ( #248080, #167610, #245214, #154363 ) ) ;
#88729 = CARTESIAN_POINT ( 'NONE',  ( 21.07094088545368393, 30.85066122990914650, -252.0448291528320510 ) ) ;
#88731 = CIRCLE ( 'NONE', #188695, 0.1000000000000026007 ) ;
#88732 = AXIS2_PLACEMENT_3D ( 'NONE', #38160, #55103, #117677 ) ;
#88733 = AXIS2_PLACEMENT_3D ( 'NONE', #29936, #70355, #188988 ) ;
#88734 = EDGE_CURVE ( 'NONE', #109895, #84132, #115346, .T. ) ;
#88735 = AXIS2_PLACEMENT_3D ( 'NONE', #103196, #142331, #79775 ) ;
#88736 = EDGE_CURVE ( 'NONE', #160738, #100104, #235290, .T. ) ;
#88737 = CARTESIAN_POINT ( 'NONE',  ( -18.59999999999999787, 77.83585931145546510, -91.51866831572576189 ) ) ;
#88738 = EDGE_CURVE ( 'NONE', #70690, #9758, #36270, .T. ) ;
#88739 = DIRECTION ( 'NONE',  ( 1.000000000000000000, 0.000000000000000000, 0.000000000000000000 ) ) ;
#88740 = VECTOR ( 'NONE', #40527, 1000.000000000000000 ) ;
#88741 = VERTEX_POINT ( 'NONE', #79772 ) ;
#88742 = AXIS2_PLACEMENT_3D ( 'NONE', #50355, #208191, #246023 ) ;
#88743 = EDGE_CURVE ( 'NONE', #25751, #228703, #216737, .T. ) ;
#88744 = AXIS2_PLACEMENT_3D ( 'NONE', #166559, #209499, #244766 ) ;
#88746 = CARTESIAN_POINT ( 'NONE',  ( 0.8999999999999993561, -11.65000000000000036, 23.40000000000000568 ) ) ;
#88745 = AXIS2_PLACEMENT_3D ( 'NONE', #57953, #137490, #117941 ) ;
#88747 = CARTESIAN_POINT ( 'NONE',  ( -16.27683809663751191, 66.65000000001191438, -93.77310748452441658 ) ) ;
#88748 = PLANE ( 'NONE',  #94476 ) ;
#88749 = ORIENTED_EDGE ( 'NONE', *, *, #134778, .F. ) ;
#88750 = DIRECTION ( 'NONE',  ( -0.000000000000000000, 1.000000000000000000, -1.224646799147352961E-16 ) ) ;
#88752 = ORIENTED_EDGE ( 'NONE', *, *, #252105, .T. ) ;
#88751 = CARTESIAN_POINT ( 'NONE',  ( -16.83558968593874638, 9.950000000011137047, -188.3376948123832619 ) ) ;
#88753 = CARTESIAN_POINT ( 'NONE',  ( -20.54999999999999716, 84.73084112150739600, -126.9250327655398962 ) ) ;
#88754 = EDGE_CURVE ( 'NONE', #61360, #188240, #18552, .T. ) ;
#88755 = CARTESIAN_POINT ( 'NONE',  ( -16.27683809663751191, 9.350000000011132073, -113.0500000000000398 ) ) ;
#88756 = VERTEX_POINT ( 'NONE', #98042 ) ;
#88757 = DIRECTION ( 'NONE',  ( 1.000000000000000000, 0.000000000000000000, 0.000000000000000000 ) ) ;
#88758 = EDGE_CURVE ( 'NONE', #100756, #254423, #177652, .T. ) ;
#88759 = APPLICATION_PROTOCOL_DEFINITION ( 'draft international standard', 'automotive_design', 1998, #207378 ) ;
#88760 = CARTESIAN_POINT ( 'NONE',  ( -20.94999675878240808, 65.70692517833212776, -64.06446533783034170 ) ) ;
#88761 = ADVANCED_FACE ( 'NONE', ( #139750 ), #219304, .T. ) ;
#88762 = CARTESIAN_POINT ( 'NONE',  ( -20.85000000000000142, 74.86109765932731364, -233.8067614591677454 ) ) ;
#88763 = DIRECTION ( 'NONE',  ( 0.000000000000000000, -0.6728388485993130885, 0.7397890806274115549 ) ) ;
#88764 = ORIENTED_EDGE ( 'NONE', *, *, #235884, .F. ) ;
#88765 = CARTESIAN_POINT ( 'NONE',  ( 21.14999999999999858, 6.257814610476124528, 0.09779029130879343668 ) ) ;
#88766 = DIRECTION ( 'NONE',  ( 0.000000000000000000, 6.982962677686266711E-15, -1.000000000000000000 ) ) ;
#88767 = ADVANCED_FACE ( 'NONE', ( #115918 ), #95056, .F. ) ;
#88768 = DIRECTION ( 'NONE',  ( 0.000000000000000000, -0.2128009952263602289, 0.9770955615653315052 ) ) ;
#88769 = VERTEX_POINT ( 'NONE', #156354 ) ;
#88770 = EDGE_LOOP ( 'NONE', ( #164717, #37987, #17246, #200721 ) ) ;
#88771 = EDGE_CURVE ( 'NONE', #17857, #83361, #212459, .T. ) ;
#88772 = EDGE_CURVE ( 'NONE', #165247, #7336, #84767, .T. ) ;
#88773 = CARTESIAN_POINT ( 'NONE',  ( 21.08804281139605408, 65.37816569817088919, -124.1731075171459082 ) ) ;
#88774 = CARTESIAN_POINT ( 'NONE',  ( -21.78635804494510708, 68.96433851485876687, -103.1221125500320426 ) ) ;
#88775 = FACE_OUTER_BOUND ( 'NONE', #151068, .T. ) ;
#88776 = FACE_OUTER_BOUND ( 'NONE', #76987, .T. ) ;
#88777 = LINE ( 'NONE', #227021, #211832 ) ;
#88779 = CARTESIAN_POINT ( 'NONE',  ( 21.05000000000000071, 6.257814610487280937, -33.40220970869120265 ) ) ;
#88778 = SPHERICAL_SURFACE ( 'NONE', #190825, 0.1000000000000000056 ) ;
#88780 = CARTESIAN_POINT ( 'NONE',  ( 21.05000000000000071, 76.00000000001242029, -166.0231074845243597 ) ) ;
#88781 = DIRECTION ( 'NONE',  ( 0.000000000000000000, 6.982962677686266711E-15, -1.000000000000000000 ) ) ;
#88783 = DIRECTION ( 'NONE',  ( 0.000000000000000000, 0.000000000000000000, -1.000000000000000000 ) ) ;
#88782 = CIRCLE ( 'NONE', #247007, 0.2000000000000057288 ) ;
#88784 = CIRCLE ( 'NONE', #26462, 0.2000000000000048683 ) ;
#88786 = ORIENTED_EDGE ( 'NONE', *, *, #234621, .F. ) ;
#88785 = LINE ( 'NONE', #228332, #57155 ) ;
#88787 = FACE_OUTER_BOUND ( 'NONE', #221418, .T. ) ;
#88788 = CARTESIAN_POINT ( 'NONE',  ( 18.49999999999999289, 33.67810952736942198, -236.3734420906320395 ) ) ;
#88790 = DIRECTION ( 'NONE',  ( 0.000000000000000000, 0.000000000000000000, 1.000000000000000000 ) ) ;
#88789 = CARTESIAN_POINT ( 'NONE',  ( 20.85000000000000142, 87.65000000001215597, -139.4231074845242802 ) ) ;
#88791 = ADVANCED_FACE ( 'NONE', ( #54638 ), #235844, .F. ) ;
#88792 = EDGE_LOOP ( 'NONE', ( #127988, #28528, #58146, #159379, #14530 ) ) ;
#88793 = DIRECTION ( 'NONE',  ( -1.000000000000000000, 0.000000000000000000, 0.000000000000000000 ) ) ;
#88795 = EDGE_CURVE ( 'NONE', #152727, #213696, #118122, .T. ) ;
#88794 = CARTESIAN_POINT ( 'NONE',  ( 19.90621891164687440, 64.25000000001196554, -111.6946622066469672 ) ) ;
#88796 = CARTESIAN_POINT ( 'NONE',  ( -18.50000000000000000, 16.60731133254646963, -240.9277311905271688 ) ) ;
#88797 = DIRECTION ( 'NONE',  ( 1.000000000000000000, 0.000000000000000000, 0.000000000000000000 ) ) ;
#88798 = CARTESIAN_POINT ( 'NONE',  ( -18.59999999999999787, 68.97833521811131163, -32.38954208262708079 ) ) ;
#88799 = ORIENTED_EDGE ( 'NONE', *, *, #23208, .F. ) ;
#88800 = ORIENTED_EDGE ( 'NONE', *, *, #67605, .T. ) ;
#88801 = EDGE_CURVE ( 'NONE', #186491, #203708, #22289, .T. ) ;
#88803 = AXIS2_PLACEMENT_3D ( 'NONE', #211667, #92977, #253332 ) ;
#88802 = DIRECTION ( 'NONE',  ( 0.7071067811865473507, 0.3338907855510733769, 0.6233112732207618523 ) ) ;
#88804 = ORIENTED_EDGE ( 'NONE', *, *, #90601, .T. ) ;
#88805 = CARTESIAN_POINT ( 'NONE',  ( 21.04999999999999716, 65.31569084252679147, -95.49641069419752171 ) ) ;
#88806 = ORIENTED_EDGE ( 'NONE', *, *, #133522, .T. ) ;
#88807 = AXIS2_PLACEMENT_3D ( 'NONE', #209464, #32143, #46526 ) ;
#88808 = FACE_OUTER_BOUND ( 'NONE', #51110, .T. ) ;
#88809 = DIRECTION ( 'NONE',  ( 1.000000000000000000, 0.000000000000000000, 0.000000000000000000 ) ) ;
#88810 = CIRCLE ( 'NONE', #255364, 1.900000000000000799 ) ;
#88811 = CARTESIAN_POINT ( 'NONE',  ( -23.49999999999994316, 79.88763423575340994, -7.282924647898262549 ) ) ;
#88812 = EDGE_LOOP ( 'NONE', ( #117073, #28413, #131568, #186568 ) ) ;
#88813 = CARTESIAN_POINT ( 'NONE',  ( 18.39999999999999503, 70.35000000001222986, -145.7731074845243882 ) ) ;
#88814 = AXIS2_PLACEMENT_3D ( 'NONE', #230462, #51798, #252577 ) ;
#88815 = EDGE_CURVE ( 'NONE', #253894, #53634, #163920, .T. ) ;
#88817 = DIRECTION ( 'NONE',  ( 0.000000000000000000, 0.000000000000000000, 1.000000000000000000 ) ) ;
#88816 = CIRCLE ( 'NONE', #43066, 0.09999999999999749367 ) ;
#88818 = CARTESIAN_POINT ( 'NONE',  ( -20.94999999999999929, 1.115600667400684642E-11, -67.00000000000000000 ) ) ;
#88820 = AXIS2_PLACEMENT_3D ( 'NONE', #69617, #52595, #13493 ) ;
#88819 = CARTESIAN_POINT ( 'NONE',  ( 21.05000000000000071, 78.50726470275242264, -228.6618886302502176 ) ) ;
#88821 = DIRECTION ( 'NONE',  ( 1.000000000000000000, 7.304098846218105085E-16, 4.217023435051677501E-16 ) ) ;
#88822 = ADVANCED_FACE ( 'NONE', ( #131617 ), #97227, .T. ) ;
#88823 = VERTEX_POINT ( 'NONE', #57192 ) ;
#88825 = CARTESIAN_POINT ( 'NONE',  ( -16.97683809663752186, 9.950000000011138823, -180.9023640181964652 ) ) ;
#88824 = CARTESIAN_POINT ( 'NONE',  ( -21.44999999999999929, 7.250000000011155521, -112.8500000000000369 ) ) ;
#88826 = ORIENTED_EDGE ( 'NONE', *, *, #210836, .F. ) ;
#88828 = ORIENTED_EDGE ( 'NONE', *, *, #240711, .T. ) ;
#88827 = FACE_OUTER_BOUND ( 'NONE', #66708, .T. ) ;
#88829 = VERTEX_POINT ( 'NONE', #194185 ) ;
#88830 = FACE_OUTER_BOUND ( 'NONE', #164250, .T. ) ;
#88831 = CARTESIAN_POINT ( 'NONE',  ( 12.26145404764308999, 66.64858632091086577, -153.0427639169754173 ) ) ;
#88832 = CYLINDRICAL_SURFACE ( 'NONE', #155521, 0.09999999999999939493 ) ;
#88833 = VECTOR ( 'NONE', #48940, 1000.000000000000000 ) ;
#88834 = FACE_OUTER_BOUND ( 'NONE', #185447, .T. ) ;
#88835 = ORIENTED_EDGE ( 'NONE', *, *, #43480, .F. ) ;
#88836 = EDGE_CURVE ( 'NONE', #82861, #33906, #255360, .T. ) ;
#88837 = DIRECTION ( 'NONE',  ( -0.7071067811865475727, 0.7071067811865475727, 4.937700262164531476E-15 ) ) ;
#88838 = CARTESIAN_POINT ( 'NONE',  ( 18.49999999999999289, 10.34378108836433263, -158.8284452778770230 ) ) ;
#88839 = VECTOR ( 'NONE', #164509, 1000.000000000000000 ) ;
#88840 = EDGE_CURVE ( 'NONE', #214650, #106794, #180496, .T. ) ;
#88841 = ORIENTED_EDGE ( 'NONE', *, *, #65571, .T. ) ;
#88842 = CIRCLE ( 'NONE', #184326, 0.1999999999999996503 ) ;
#88843 = TOROIDAL_SURFACE ( 'NONE', #172118, 11.65000000000000036, 0.1000000000000000056 ) ;
#88844 = EDGE_CURVE ( 'NONE', #221948, #215622, #51452, .T. ) ;
#88845 = DIRECTION ( 'NONE',  ( -0.000000000000000000, -0.1350103645451904977, 0.9908441862701596881 ) ) ;
#88846 = ORIENTED_EDGE ( 'NONE', *, *, #249591, .T. ) ;
#88847 = DIRECTION ( 'NONE',  ( -0.000000000000000000, -0.4721928772777346239, -0.8814952561688430555 ) ) ;
#88848 = EDGE_CURVE ( 'NONE', #244974, #100799, #254120, .T. ) ;
#88849 = ORIENTED_EDGE ( 'NONE', *, *, #126438, .T. ) ;
#88850 = CARTESIAN_POINT ( 'NONE',  ( 18.50000324121758055, 65.70692517833211355, -97.56446533783039854 ) ) ;
#88853 = EDGE_CURVE ( 'NONE', #127618, #113007, #216279, .T. ) ;
#88852 = EDGE_CURVE ( 'NONE', #213807, #89961, #96323, .T. ) ;
#88851 = EDGE_LOOP ( 'NONE', ( #31652, #59568, #12976, #227685 ) ) ;
#88854 = DIRECTION ( 'NONE',  ( 0.000000000000000000, 1.000000000000000000, 0.000000000000000000 ) ) ;
#88855 = CARTESIAN_POINT ( 'NONE',  ( 21.05000000000000071, 64.25000000001175238, -76.53791325517833855 ) ) ;
#88856 = CARTESIAN_POINT ( 'NONE',  ( -23.25000000000000355, 70.35000000001224407, -149.1731074845243938 ) ) ;
#88857 = FACE_OUTER_BOUND ( 'NONE', #91140, .T. ) ;
#88858 = CIRCLE ( 'NONE', #13870, 0.1000000000000002554 ) ;
#88859 = AXIS2_PLACEMENT_3D ( 'NONE', #26205, #126577, #223096 ) ;
#88860 = LINE ( 'NONE', #184125, #182185 ) ;
#88861 = CARTESIAN_POINT ( 'NONE',  ( -18.59999999999999787, 7.675662554762638479, -241.7139905447625381 ) ) ;
#88862 = AXIS2_PLACEMENT_3D ( 'NONE', #127980, #10602, #172281 ) ;
#88864 = ORIENTED_EDGE ( 'NONE', *, *, #228388, .F. ) ;
#88863 = EDGE_CURVE ( 'NONE', #89516, #146851, #47191, .T. ) ;
#88866 = EDGE_CURVE ( 'NONE', #53690, #33906, #222152, .T. ) ;
#88865 = DIRECTION ( 'NONE',  ( -1.000000000000000000, 2.952720810173289112E-16, 2.061873921506763405E-30 ) ) ;
#88867 = VERTEX_POINT ( 'NONE', #112075 ) ;
#88869 = CARTESIAN_POINT ( 'NONE',  ( 21.05000000000000071, 10.72371710471867701, -33.50000000000000000 ) ) ;
#88868 = CARTESIAN_POINT ( 'NONE',  ( -18.59999999999999787, 85.32100840337318459, -95.78716923544635620 ) ) ;
#88870 = ORIENTED_EDGE ( 'NONE', *, *, #192649, .T. ) ;
#88871 = FACE_OUTER_BOUND ( 'NONE', #206775, .T. ) ;
#88872 = AXIS2_PLACEMENT_3D ( 'NONE', #95686, #257283, #136080 ) ;
#88873 = CARTESIAN_POINT ( 'NONE',  ( -20.54999999999999716, 4.350000000011156054, -150.7500000000000284 ) ) ;
#88874 = ADVANCED_FACE ( 'NONE', ( #234568 ), #191635, .T. ) ;
#88875 = CARTESIAN_POINT ( 'NONE',  ( 21.05000000000000071, 65.27628289530437655, -95.35819391543677170 ) ) ;
#88876 = AXIS2_PLACEMENT_3D ( 'NONE', #49572, #148688, #103100 ) ;
#88877 = EDGE_LOOP ( 'NONE', ( #173124, #77439 ) ) ;
#88879 = VERTEX_POINT ( 'NONE', #53369 ) ;
#88878 = FACE_OUTER_BOUND ( 'NONE', #103938, .T. ) ;
#88880 = DIRECTION ( 'NONE',  ( 0.000000000000000000, 1.000000000000000000, 1.387778780781444413E-14 ) ) ;
#88881 = EDGE_CURVE ( 'NONE', #199335, #89573, #159649, .T. ) ;
#88882 = AXIS2_PLACEMENT_3D ( 'NONE', #10238, #65059, #246275 ) ;
#88884 = CARTESIAN_POINT ( 'NONE',  ( 18.50000000000062883, 15.26868426882366592, -222.9405159379593613 ) ) ;
#88883 = CARTESIAN_POINT ( 'NONE',  ( -18.59999999999999787, -1.249999999988843369, -175.4999999999999716 ) ) ;
#88885 = ADVANCED_FACE ( 'NONE', ( #62361 ), #251403, .T. ) ;
#88887 = ORIENTED_EDGE ( 'NONE', *, *, #20427, .T. ) ;
#88886 = CARTESIAN_POINT ( 'NONE',  ( 22.19999999999999929, -11.75000000000000355, 12.09999999999999609 ) ) ;
#88888 = AXIS2_PLACEMENT_3D ( 'NONE', #184190, #104627, #246732 ) ;
#88889 = AXIS2_PLACEMENT_3D ( 'NONE', #184236, #128127, #108559 ) ;
#88890 = TOROIDAL_SURFACE ( 'NONE', #9786, 0.4000000000000017431, 0.1000000000000000056 ) ;
#88891 = AXIS2_PLACEMENT_3D ( 'NONE', #172444, #254471, #154166 ) ;
#88892 = PRODUCT_DEFINITION_SHAPE ( 'NONE', 'NONE',  #236527 ) ;
#88893 = VERTEX_POINT ( 'NONE', #198000 ) ;
#88894 = CIRCLE ( 'NONE', #234665, 0.1999999999999996503 ) ;
#88895 = FACE_OUTER_BOUND ( 'NONE', #30854, .T. ) ;
#88896 = LINE ( 'NONE', #145022, #26337 ) ;
#88897 = ORIENTED_EDGE ( 'NONE', *, *, #50551, .T. ) ;
#88898 = FACE_OUTER_BOUND ( 'NONE', #18983, .T. ) ;
#88899 = ORIENTED_EDGE ( 'NONE', *, *, #228999, .T. ) ;
#88901 = ADVANCED_FACE ( 'NONE', ( #3652 ), #83157, .T. ) ;
#88900 = DIRECTION ( 'NONE',  ( 0.000000000000000000, 1.000000000000000000, 0.000000000000000000 ) ) ;
#88902 = CARTESIAN_POINT ( 'NONE',  ( 20.12500000000000000, 18.88320179786139619, -228.9684431863134932 ) ) ;
#88903 = CIRCLE ( 'NONE', #155415, 0.3999999999999975797 ) ;
#88904 = VERTEX_POINT ( 'NONE', #41531 ) ;
#88905 = EDGE_CURVE ( 'NONE', #21530, #90111, #34768, .T. ) ;
#88906 = AXIS2_PLACEMENT_3D ( 'NONE', #199632, #41843, #219151 ) ;
#88907 = ORIENTED_EDGE ( 'NONE', *, *, #99690, .T. ) ;
#88908 = CARTESIAN_POINT ( 'NONE',  ( 23.14999999999999503, 11.65000000000000746, -21.25000000000000000 ) ) ;
#88909 = VECTOR ( 'NONE', #119451, 1000.000000000000000 ) ;
#88910 = CIRCLE ( 'NONE', #34997, 0.1000000000000052097 ) ;
#88911 = ORIENTED_EDGE ( 'NONE', *, *, #62588, .T. ) ;
#88912 = CIRCLE ( 'NONE', #109766, 0.5000000000000004441 ) ;
#88913 = EDGE_LOOP ( 'NONE', ( #205010, #217469, #9125, #79841 ) ) ;
#88914 = DIRECTION ( 'NONE',  ( 0.000000000000000000, -0.2700277750006208621, -0.9628525332200221776 ) ) ;
#88915 = ORIENTED_EDGE ( 'NONE', *, *, #150753, .T. ) ;
#88917 = EDGE_CURVE ( 'NONE', #244346, #14172, #147167, .T. ) ;
#88916 = DIRECTION ( 'NONE',  ( 1.836970198721029934E-16, -1.000000000000000000, -0.000000000000000000 ) ) ;
#88918 = EDGE_LOOP ( 'NONE', ( #196373, #8542, #82159 ) ) ;
#88920 = ORIENTED_EDGE ( 'NONE', *, *, #251710, .F. ) ;
#88919 = CARTESIAN_POINT ( 'NONE',  ( -20.94999999999999929, 87.65000000001163016, -66.62310748452424036 ) ) ;
#88921 = CARTESIAN_POINT ( 'NONE',  ( -20.94999999999999929, 11.60000000001115339, -73.92820323027561358 ) ) ;
#88922 = ORIENTED_EDGE ( 'NONE', *, *, #218301, .T. ) ;
#88923 = DIRECTION ( 'NONE',  ( 0.000000000000000000, 0.000000000000000000, 1.000000000000000000 ) ) ;
#88924 = ORIENTED_EDGE ( 'NONE', *, *, #132063, .T. ) ;
#88925 = B_SPLINE_CURVE_WITH_KNOTS ( 'NONE', 3,
 ( #170945, #250420, #88760, #187898, #151349, #247858, #230887, #146180, #206168, #28863, #69241, #9242, #27569, #186618, #109621, #87483, #167073, #189176, #67934 ),
 .UNSPECIFIED., .F., .F.,
 ( 4, 3, 3, 3, 3, 3, 4 ),
 ( -2.000416914659873068E-06, 0.000000000000000000, 4.714008503744566487E-05, 9.979203887777271477E-05, 0.0001372215519229485938, 0.0001635031576220933387, 0.0001900083748504131887 ),
 .UNSPECIFIED. ) ;
#88928 = VERTEX_POINT ( 'NONE', #21958 ) ;
#88927 = ORIENTED_EDGE ( 'NONE', *, *, #243235, .T. ) ;
#88926 = CARTESIAN_POINT ( 'NONE',  ( -18.50000000000000000, -1.736257131586239844, -179.0686523290174819 ) ) ;
#88929 = FACE_OUTER_BOUND ( 'NONE', #3431, .T. ) ;
#88930 = LINE ( 'NONE', #10703, #189752 ) ;
#88932 = EDGE_LOOP ( 'NONE', ( #168250, #148982, #119362, #31600 ) ) ;
#88931 = AXIS2_PLACEMENT_3D ( 'NONE', #175244, #119084, #18689 ) ;
#88933 = VECTOR ( 'NONE', #25403, 1000.000000000000000 ) ;
#88934 = CIRCLE ( 'NONE', #39091, 0.09999999999999939493 ) ;
#88935 = CIRCLE ( 'NONE', #51319, 0.09999999999999939493 ) ;
#88936 = VERTEX_POINT ( 'NONE', #119786 ) ;
#88937 = DIRECTION ( 'NONE',  ( 1.000000000000000000, 0.000000000000000000, 0.000000000000000000 ) ) ;
#88938 = CARTESIAN_POINT ( 'NONE',  ( -21.44999999999999929, 68.65000000001199965, -115.2731074845243455 ) ) ;
#88939 =( BOUNDED_SURFACE ( )  B_SPLINE_SURFACE ( 3, 2, ( 
 ( #228172, #89920, #88623 ),
 ( #168232, #49529, #66528 ),
 ( #48236, #245164, #207333 ),
 ( #189039, #129067, #146045 ),
 ( #204729, #29993, #169517 ),
 ( #247722, #224305, #186475 ) ),
 .UNSPECIFIED., .F., .F., .F. ) 
 B_SPLINE_SURFACE_WITH_KNOTS ( ( 4, 2, 4 ),
 ( 3, 3 ),
 ( 3.141592653589827755, 3.926990816987264932, 4.712388980384702108 ),
 ( 0.000000000000000000, 1.000000000000000000 ),
 .UNSPECIFIED. ) 
 GEOMETRIC_REPRESENTATION_ITEM ( )  RATIONAL_B_SPLINE_SURFACE ( (
 ( 1.000000000000000000, 0.9238795325112765244, 1.000000000000000000),
 ( 1.000000000000000000, 0.9240297172240848900, 1.000000000000000000),
 ( 1.000000000000000000, 0.9038128468042962993, 1.000000000000000000),
 ( 1.000000000000000000, 0.8282379607645715680, 1.000000000000000000),
 ( 1.000000000000000000, 0.7727932973494031632, 1.000000000000000000),
 ( 1.000000000000000000, 0.7071067811866299513, 1.000000000000000000) ) ) 
 REPRESENTATION_ITEM ( '' )  SURFACE ( )  );
#88941 = ORIENTED_EDGE ( 'NONE', *, *, #202551, .T. ) ;
#88940 = FACE_OUTER_BOUND ( 'NONE', #210725, .T. ) ;
#88942 = DIRECTION ( 'NONE',  ( 1.000000000000000000, 0.000000000000000000, 0.000000000000000000 ) ) ;
#88943 = VERTEX_POINT ( 'NONE', #201863 ) ;
#88944 = PLANE ( 'NONE',  #95241 ) ;
#88945 = DIRECTION ( 'NONE',  ( -1.000000000000000000, -2.885090398161910739E-16, -6.283419270304611573E-17 ) ) ;
#88946 = ORIENTED_EDGE ( 'NONE', *, *, #155913, .F. ) ;
#88947 = DIRECTION ( 'NONE',  ( 0.000000000000000000, -0.2617529984165033463, -0.9651348961777156399 ) ) ;
#88948 = CYLINDRICAL_SURFACE ( 'NONE', #257204, 0.5000000000000004441 ) ;
#88949 = VERTEX_POINT ( 'NONE', #178479 ) ;
#88951 = VERTEX_POINT ( 'NONE', #139298 ) ;
#88950 = CARTESIAN_POINT ( 'NONE',  ( -23.25000000000000000, 28.51339163295720169, -258.4040038037771865 ) ) ;
#88952 = CARTESIAN_POINT ( 'NONE',  ( -16.87036670365548474, 14.22508806334145959, -219.3732768077300932 ) ) ;
#88954 = VERTEX_POINT ( 'NONE', #42793 ) ;
#88953 = EDGE_LOOP ( 'NONE', ( #114255, #130269, #225090, #133829 ) ) ;
#88955 = TOROIDAL_SURFACE ( 'NONE', #155650, 0.9750000000000019762, 0.1000000000000000056 ) ;
#88956 = ORIENTED_EDGE ( 'NONE', *, *, #154099, .F. ) ;
#88957 = CARTESIAN_POINT ( 'NONE',  ( -22.50000000000000000, 12.62988036037870998, -223.4632815780722410 ) ) ;
#88958 = ORIENTED_EDGE ( 'NONE', *, *, #191934, .T. ) ;
#88959 = VERTEX_POINT ( 'NONE', #222691 ) ;
#88960 = CYLINDRICAL_SURFACE ( 'NONE', #159120, 0.5000000000000004441 ) ;
#88961 = ORIENTED_EDGE ( 'NONE', *, *, #142983, .T. ) ;
#88962 = DIRECTION ( 'NONE',  ( 0.000000000000000000, 0.000000000000000000, -1.000000000000000000 ) ) ;
#88963 = CARTESIAN_POINT ( 'NONE',  ( 18.49999999999998934, 34.44688795055758135, -235.1500552906961730 ) ) ;
#88964 = ORIENTED_EDGE ( 'NONE', *, *, #65252, .T. ) ;
#88965 = EDGE_CURVE ( 'NONE', #120146, #210220, #138018, .T. ) ;
#88966 = ORIENTED_EDGE ( 'NONE', *, *, #9637, .T. ) ;
#88967 = CARTESIAN_POINT ( 'NONE',  ( -14.00000000000000178, 9.850000000011133849, -184.2499999999999716 ) ) ;
#88968 = AXIS2_PLACEMENT_3D ( 'NONE', #155653, #197299, #137319 ) ;
#88969 = ORIENTED_EDGE ( 'NONE', *, *, #131215, .T. ) ;
#88970 = AXIS2_PLACEMENT_3D ( 'NONE', #71551, #49402, #70276 ) ;
#88971 = CIRCLE ( 'NONE', #138837, 0.1000000000000009354 ) ;
#88972 = DIRECTION ( 'NONE',  ( 0.000000000000000000, -0.9126074666063660468, -0.4088369013363524762 ) ) ;
#88973 = VERTEX_POINT ( 'NONE', #18085 ) ;
#88974 = EDGE_CURVE ( 'NONE', #195545, #163442, #113850, .T. ) ;
#88975 = FACE_OUTER_BOUND ( 'NONE', #163102, .T. ) ;
#88977 = ORIENTED_EDGE ( 'NONE', *, *, #184782, .F. ) ;
#88976 = CARTESIAN_POINT ( 'NONE',  ( 22.39999999999999858, 0.1000000000111554016, -159.7092204016265669 ) ) ;
#88978 = DIRECTION ( 'NONE',  ( 0.000000000000000000, 0.7397360091702755991, -0.6728971962616832059 ) ) ;
#88979 = DIRECTION ( 'NONE',  ( 2.952720810173289112E-16, 1.000000000000000000, 7.086529944415894657E-15 ) ) ;
#88980 = CARTESIAN_POINT ( 'NONE',  ( 18.49999999999999645, 70.05000000001165006, -59.21740517948951066 ) ) ;
#88981 = CARTESIAN_POINT ( 'NONE',  ( -21.10257677756355932, 6.398381742543874928, -133.9750492504320221 ) ) ;
#88982 = ADVANCED_FACE ( 'NONE', ( #217554 ), #38955, .F. ) ;
#88983 = DIRECTION ( 'NONE',  ( 1.734723475976817507E-14, -6.982962677686266711E-15, 1.000000000000000000 ) ) ;
#88984 = DIRECTION ( 'NONE',  ( 0.000000000000000000, 0.000000000000000000, 1.000000000000000000 ) ) ;
#88985 = DIRECTION ( 'NONE',  ( 0.000000000000000000, 0.000000000000000000, -1.000000000000000000 ) ) ;
#88986 = CARTESIAN_POINT ( 'NONE',  ( 18.48197441912073558, 38.23830283804237951, -261.1947035615960431 ) ) ;
#88987 = VECTOR ( 'NONE', #94312, 1000.000000000000000 ) ;
#88988 = CARTESIAN_POINT ( 'NONE',  ( 21.05000000000000071, 76.00000000001126921, -203.5231074845248997 ) ) ;
#88989 = EDGE_CURVE ( 'NONE', #127486, #189010, #155588, .T. ) ;
#88990 = TOROIDAL_SURFACE ( 'NONE', #143152, 11.65000000000000036, 0.1000000000000000056 ) ;
#88991 = ORIENTED_EDGE ( 'NONE', *, *, #204191, .T. ) ;
#88992 = AXIS2_PLACEMENT_3D ( 'NONE', #210769, #174261, #111669 ) ;
#88993 = AXIS2_PLACEMENT_3D ( 'NONE', #166914, #67773, #229425 ) ;
#88994 = ADVANCED_FACE ( 'NONE', ( #239715 ), #102733, .F. ) ;
#88995 = VERTEX_POINT ( 'NONE', #200578 ) ;
#88997 = ORIENTED_EDGE ( 'NONE', *, *, #217181, .T. ) ;
#88996 = CARTESIAN_POINT ( 'NONE',  ( 23.15000000000000213, 23.68770167995059239, -252.8127582590406348 ) ) ;
#88998 = EDGE_CURVE ( 'NONE', #71933, #19770, #256642, .T. ) ;
#88999 = ORIENTED_EDGE ( 'NONE', *, *, #147746, .T. ) ;
#89000 = CARTESIAN_POINT ( 'NONE',  ( -23.15000000000000213, 74.08971962618021223, -115.6544753397232626 ) ) ;
#89001 = CARTESIAN_POINT ( 'NONE',  ( -23.25000000000000355, 7.488999128699433072, -208.8358083214519070 ) ) ;
#89002 = EDGE_CURVE ( 'NONE', #50885, #248097, #242260, .T. ) ;
#89004 = FACE_OUTER_BOUND ( 'NONE', #131892, .T. ) ;
#89003 = DIRECTION ( 'NONE',  ( 0.1538461538461484146, -0.9880948137434723000, 0.000000000000000000 ) ) ;
#89005 = VERTEX_POINT ( 'NONE', #63634 ) ;
#89006 = ORIENTED_EDGE ( 'NONE', *, *, #210732, .T. ) ;
#89007 = AXIS2_PLACEMENT_3D ( 'NONE', #136150, #30694, #110190 ) ;
#89009 = CIRCLE ( 'NONE', #14036, 12.87499999999999822 ) ;
#89008 = FILL_AREA_STYLE ('',( #66892 ) ) ;
#89011 = AXIS2_PLACEMENT_3D ( 'NONE', #134380, #154022, #96534 ) ;
#89010 = DIRECTION ( 'NONE',  ( 0.7071067811865388020, -0.7071067811865561215, 0.000000000000000000 ) ) ;
#89012 = EDGE_CURVE ( 'NONE', #241241, #103333, #182319, .T. ) ;
#89013 = DIRECTION ( 'NONE',  ( 1.000000000000000000, -0.000000000000000000, -0.000000000000000000 ) ) ;
#89014 = VERTEX_POINT ( 'NONE', #79329 ) ;
#89015 = ORIENTED_EDGE ( 'NONE', *, *, #142126, .F. ) ;
#89016 = CARTESIAN_POINT ( 'NONE',  ( -20.54999999999999716, 2.000000000011154189, -120.7753780772379315 ) ) ;
#89017 = DIRECTION ( 'NONE',  ( 1.000000000000000000, 0.000000000000000000, 0.000000000000000000 ) ) ;
#89019 = EDGE_CURVE ( 'NONE', #172220, #224786, #158912, .T. ) ;
#89018 = FACE_OUTER_BOUND ( 'NONE', #184187, .T. ) ;
#89020 = DIRECTION ( 'NONE',  ( 0.000000000000000000, 0.000000000000000000, 1.000000000000000000 ) ) ;
#89021 = AXIS2_PLACEMENT_3D ( 'NONE', #104302, #204691, #189957 ) ;
#89022 = CARTESIAN_POINT ( 'NONE',  ( -18.59999999999999787, 1.115600667400684642E-11, -67.00000000000000000 ) ) ;
#89024 = VERTEX_POINT ( 'NONE', #242422 ) ;
#89023 = DIRECTION ( 'NONE',  ( -0.000000000000000000, -0.000000000000000000, 1.000000000000000000 ) ) ;
#89025 = EDGE_CURVE ( 'NONE', #145735, #179299, #182480, .T. ) ;
#89026 = DIRECTION ( 'NONE',  ( 1.000000000000000000, -1.186688945009010077E-16, -8.286604613020808509E-31 ) ) ;
#89027 = AXIS2_PLACEMENT_3D ( 'NONE', #14438, #32731, #56076 ) ;
#89028 = CARTESIAN_POINT ( 'NONE',  ( -20.54999999999999716, -8.663551401858004652, -76.52410111806734960 ) ) ;
#89029 = CARTESIAN_POINT ( 'NONE',  ( 18.49351773456776016, 85.44302569515703283, -95.83778195849694725 ) ) ;
#89031 = EDGE_LOOP ( 'NONE', ( #197554, #198998, #90161, #194548, #186418 ) ) ;
#89030 = VECTOR ( 'NONE', #159142, 1000.000000000000000 ) ;
#89032 = CARTESIAN_POINT ( 'NONE',  ( 13.12229106158773639, 66.56936289831510578, -84.75484686646345267 ) ) ;
#89034 = EDGE_CURVE ( 'NONE', #251858, #136324, #160364, .T. ) ;
#89033 = DIRECTION ( 'NONE',  ( 0.000000000000000000, 0.2128009952263568982, -0.9770955615653323934 ) ) ;
#89035 = AXIS2_PLACEMENT_3D ( 'NONE', #96475, #236002, #57350 ) ;
#89037 = DIRECTION ( 'NONE',  ( 0.000000000000000000, 0.9651348961777148627, -0.2617529984165062329 ) ) ;
#89036 = CARTESIAN_POINT ( 'NONE',  ( -22.50000000000000000, 0.1000000000111554016, -100.5000000000000284 ) ) ;
#89038 = FACE_OUTER_BOUND ( 'NONE', #47838, .T. ) ;
#89039 = CARTESIAN_POINT ( 'NONE',  ( -16.80891096016331687, 9.950000000011137047, -54.36766280726798328 ) ) ;
#89040 = DIRECTION ( 'NONE',  ( 1.000000000000000000, -7.304098846218134667E-16, -4.217023435051625732E-16 ) ) ;
#89041 = DIRECTION ( 'NONE',  ( -7.304098846218134667E-16, -1.000000000000000000, 0.000000000000000000 ) ) ;
#89042 = FACE_OUTER_BOUND ( 'NONE', #146191, .T. ) ;
#89043 = ORIENTED_EDGE ( 'NONE', *, *, #197330, .F. ) ;
#89044 = ORIENTED_EDGE ( 'NONE', *, *, #228009, .T. ) ;
#89045 =( BOUNDED_CURVE ( )  B_SPLINE_CURVE ( 3, ( #165158, #166470, #67335, #88148 ),
 .UNSPECIFIED., .F., .F. ) 
 B_SPLINE_CURVE_WITH_KNOTS ( ( 4, 4 ),
 ( 3.141592653589778461, 4.712388980384686121 ),
 .UNSPECIFIED. ) 
 CURVE ( )  GEOMETRIC_REPRESENTATION_ITEM ( )  RATIONAL_B_SPLINE_CURVE ( ( 1.000000000000000000, 0.8047378541243622729, 0.8047378541243622729, 1.000000000000000000 ) ) 
 REPRESENTATION_ITEM ( '' )  );
#89046 = ORIENTED_EDGE ( 'NONE', *, *, #81496, .T. ) ;
#89047 = ADVANCED_FACE ( 'NONE', ( #144599 ), #83325, .T. ) ;
#89048 = CARTESIAN_POINT ( 'NONE',  ( 20.22516295850462598, 66.10063570456303239, -95.11304177243273728 ) ) ;
#89049 = DIRECTION ( 'NONE',  ( 0.000000000000000000, 0.000000000000000000, 1.000000000000000000 ) ) ;
#89050 = ORIENTED_EDGE ( 'NONE', *, *, #46727, .F. ) ;
#89051 = ORIENTED_EDGE ( 'NONE', *, *, #219712, .F. ) ;
#89052 = AXIS2_PLACEMENT_3D ( 'NONE', #158786, #19243, #101288 ) ;
#89053 = CIRCLE ( 'NONE', #213974, 0.09999999999999939493 ) ;
#89054 = VERTEX_POINT ( 'NONE', #222862 ) ;
#89055 = CIRCLE ( 'NONE', #243179, 0.1000000000000054040 ) ;
#89056 = CARTESIAN_POINT ( 'NONE',  ( 21.05000000000010374, 75.98528214348843335, -109.3678308886146056 ) ) ;
#89057 = ORIENTED_EDGE ( 'NONE', *, *, #78356, .T. ) ;
#89058 = ADVANCED_FACE ( 'NONE', ( #20847 ), #88890, .F. ) ;
#89059 = CARTESIAN_POINT ( 'NONE',  ( -21.44999999999999929, 9.614325556249161409, -211.5456030694648746 ) ) ;
#89060 = PLANE ( 'NONE',  #82309 ) ;
#89061 = CARTESIAN_POINT ( 'NONE',  ( -21.08198257630413508, 1.577455038876691917, -230.6765707231475631 ) ) ;
#89062 = VECTOR ( 'NONE', #82433, 1000.000000000000000 ) ;
#89063 = CIRCLE ( 'NONE', #122406, 0.09999999999999939493 ) ;
#89064 = CARTESIAN_POINT ( 'NONE',  ( -20.54999999999999716, 84.73084112150721126, -93.42503276553991043 ) ) ;
#89065 = CARTESIAN_POINT ( 'NONE',  ( 23.24999999999999645, 76.00000000001244871, -170.0231074845243597 ) ) ;
#89067 = ORIENTED_EDGE ( 'NONE', *, *, #128632, .T. ) ;
#89066 = CARTESIAN_POINT ( 'NONE',  ( 21.04105312098505465, 44.28144824342318486, -236.4111193842065006 ) ) ;
#89069 = FACE_OUTER_BOUND ( 'NONE', #26301, .T. ) ;
#89068 = CARTESIAN_POINT ( 'NONE',  ( 20.95512820512820440, 65.37615131629972609, -61.85819391543678591 ) ) ;
#89070 = CARTESIAN_POINT ( 'NONE',  ( -16.86379686415369150, 9.975217759264314310, -154.9333898890903072 ) ) ;
#89071 = ADVANCED_FACE ( 'NONE', ( #162923 ), #100328, .F. ) ;
#89072 = VERTEX_POINT ( 'NONE', #1234 ) ;
#89073 = DIRECTION ( 'NONE',  ( 0.000000000000000000, -0.2617529984164856383, -0.9651348961777204138 ) ) ;
#89074 = CIRCLE ( 'NONE', #238937, 0.1000000000000002554 ) ;
#89075 = CARTESIAN_POINT ( 'NONE',  ( -16.86133551771148475, 66.05000000001182059, -82.22176404997772181 ) ) ;
#89076 = CARTESIAN_POINT ( 'NONE',  ( 21.05000000000000426, -0.09999999998884513686, -60.52295361821018105 ) ) ;
#89077 = ORIENTED_EDGE ( 'NONE', *, *, #188131, .T. ) ;
#89078 = CIRCLE ( 'NONE', #234846, 0.5000000000000004441 ) ;
#89079 = EDGE_CURVE ( 'NONE', #136601, #134956, #209718, .T. ) ;
#89080 = DIRECTION ( 'NONE',  ( 0.000000000000000000, 0.000000000000000000, 1.000000000000000000 ) ) ;
#89081 = EDGE_CURVE ( 'NONE', #87080, #130316, #93001, .T. ) ;
#89082 = AXIS2_PLACEMENT_3D ( 'NONE', #171927, #251420, #212313 ) ;
#89083 = B_SPLINE_CURVE_WITH_KNOTS ( 'NONE', 3,
 ( #8641, #169037, #88137, #248531, #86864, #167740, #110302, #231548 ),
 .UNSPECIFIED., .F., .F.,
 ( 4, 2, 2, 4 ),
 ( 0.000000000000000000, 0.0001049670497870057353, 0.0002099340995740114706, 0.0004198681991480003898 ),
 .UNSPECIFIED. ) ;
#89084 = VECTOR ( 'NONE', #230459, 1000.000000000000227 ) ;
#89085 = CARTESIAN_POINT ( 'NONE',  ( -20.54999999999999716, 2.399999999999999467, -23.60603087734756045 ) ) ;
#89086 = EDGE_CURVE ( 'NONE', #245346, #67371, #203869, .T. ) ;
#89087 = ORIENTED_EDGE ( 'NONE', *, *, #163574, .F. ) ;
#89088 = AXIS2_PLACEMENT_3D ( 'NONE', #18054, #1026, #162719 ) ;
#89089 = DIRECTION ( 'NONE',  ( 1.000000000000000000, 0.000000000000000000, 0.000000000000000000 ) ) ;
#89090 = DIRECTION ( 'NONE',  ( 0.000000000000000000, 0.000000000000000000, -1.000000000000000000 ) ) ;
#89091 = EDGE_CURVE ( 'NONE', #17731, #251883, #221560, .T. ) ;
#89092 = DIRECTION ( 'NONE',  ( 1.000000000000000000, 0.000000000000000000, 0.000000000000000000 ) ) ;
#89093 = DIRECTION ( 'NONE',  ( -1.000000000000000000, 0.000000000000000000, -0.000000000000000000 ) ) ;
#89094 = EDGE_LOOP ( 'NONE', ( #61264, #15789, #100927, #249736, #205503, #124066, #205733, #254720, #153151, #171779, #205861, #159511, #78343, #157974 ) ) ;
#89095 = CIRCLE ( 'NONE', #59858, 0.1000000000000001027 ) ;
#89096 = ORIENTED_EDGE ( 'NONE', *, *, #35056, .F. ) ;
#89097 = CARTESIAN_POINT ( 'NONE',  ( 20.94999999999999929, 69.45000000001259366, -191.2731074845244166 ) ) ;
#89099 = CIRCLE ( 'NONE', #68265, 6.258578643762710669 ) ;
#89098 = CARTESIAN_POINT ( 'NONE',  ( 21.04999999999999716, 10.68430915748508347, -7.526696790326847797 ) ) ;
#89100 = DIRECTION ( 'NONE',  ( -0.000000000000000000, -0.2128009952263607285, 0.9770955615653316162 ) ) ;
#89101 = DIRECTION ( 'NONE',  ( 0.000000000000000000, -1.000000000000000000, -6.982962677686265922E-15 ) ) ;
#89102 = DIRECTION ( 'NONE',  ( 0.000000000000000000, -1.000000000000000000, 0.000000000000000000 ) ) ;
#89103 = CARTESIAN_POINT ( 'NONE',  ( 21.05000000000000071, 5.000000000011153745, -121.5947339810869465 ) ) ;
#89104 = DIRECTION ( 'NONE',  ( 0.000000000000000000, 1.000000000000000000, 1.734723475976807292E-15 ) ) ;
#89105 = DIRECTION ( 'NONE',  ( -1.000000000000000000, 3.265361837132813093E-16, 2.280189983783949500E-30 ) ) ;
#89106 = VECTOR ( 'NONE', #50155, 1000.000000000000000 ) ;
#89107 = B_SPLINE_CURVE_WITH_KNOTS ( 'NONE', 3,
 ( #256709, #20738, #122392, #161531, #200646, #76836, #181096, #19443, #62420, #140658, #2417, #218902, #37743, #157711, #57253, #81932, #141942, #241066, #59815 ),
 .UNSPECIFIED., .F., .F.,
 ( 4, 3, 3, 3, 3, 3, 4 ),
 ( -2.000416914665993304E-06, 0.000000000000000000, 4.714008503744424863E-05, 9.979203887778155101E-05, 0.0001372215519229429831, 0.0001635031576221004132, 0.0001900083748504148421 ),
 .UNSPECIFIED. ) ;
#89108 = ORIENTED_EDGE ( 'NONE', *, *, #234861, .F. ) ;
#89109 = DIRECTION ( 'NONE',  ( 1.000000000000000000, 0.000000000000000000, 0.000000000000000000 ) ) ;
#89110 = AXIS2_PLACEMENT_3D ( 'NONE', #231046, #66815, #168529 ) ;
#89111 = ADVANCED_FACE ( 'NONE', ( #203314 ), #238751, .F. ) ;
#89113 = ORIENTED_EDGE ( 'NONE', *, *, #78192, .T. ) ;
#89112 = FACE_OUTER_BOUND ( 'NONE', #79351, .T. ) ;
#89114 = CIRCLE ( 'NONE', #143459, 0.1999999999999987899 ) ;
#89115 = CARTESIAN_POINT ( 'NONE',  ( 21.93340585971889212, 68.67585297715739046, -170.0231074845244166 ) ) ;
#89116 = DIRECTION ( 'NONE',  ( 0.000000000000000000, 0.000000000000000000, -1.000000000000000000 ) ) ;
#89117 = LINE ( 'NONE', #109960, #216931 ) ;
#89118 = CARTESIAN_POINT ( 'NONE',  ( -16.87683809663750623, 66.05000000001206217, -123.1207434663278946 ) ) ;
#89119 = EDGE_CURVE ( 'NONE', #189189, #225321, #219009, .T. ) ;
#89120 = CARTESIAN_POINT ( 'NONE',  ( 20.99749315643151348, 11.75000000001115907, -193.9851942312420192 ) ) ;
#89122 = ORIENTED_EDGE ( 'NONE', *, *, #53293, .T. ) ;
#89121 = FACE_OUTER_BOUND ( 'NONE', #135473, .T. ) ;
#89123 = CARTESIAN_POINT ( 'NONE',  ( 20.12500000000000000, 66.25000000001227818, -148.8731074845244393 ) ) ;
#89125 = EDGE_CURVE ( 'NONE', #192475, #224260, #151667, .T. ) ;
#89124 = LINE ( 'NONE', #128261, #66254 ) ;
#89126 = CARTESIAN_POINT ( 'NONE',  ( -20.94999999999999929, -11.48912529306490349, -70.10000000000005116 ) ) ;
#89127 = FACE_OUTER_BOUND ( 'NONE', #65504, .T. ) ;
#89128 = VERTEX_POINT ( 'NONE', #122501 ) ;
#89129 = CARTESIAN_POINT ( 'NONE',  ( -15.69373346032657679, 66.64320997496638199, -152.8182809759103975 ) ) ;
#89130 = ORIENTED_EDGE ( 'NONE', *, *, #168349, .F. ) ;
#89131 = CARTESIAN_POINT ( 'NONE',  ( 21.00000000000000000, 9.750000000011153745, -146.2500000000000284 ) ) ;
#89133 = ORIENTED_EDGE ( 'NONE', *, *, #187616, .T. ) ;
#89132 = AXIS2_PLACEMENT_3D ( 'NONE', #4219, #202437, #2934 ) ;
#89134 = DIRECTION ( 'NONE',  ( 3.469446951953634384E-14, -0.8814952561688430555, 0.4721928772777346239 ) ) ;
#89135 = AXIS2_PLACEMENT_3D ( 'NONE', #205598, #27006, #229041 ) ;
#89136 = AXIS2_PLACEMENT_3D ( 'NONE', #141566, #221095, #64590 ) ;
#89137 = ORIENTED_EDGE ( 'NONE', *, *, #222477, .F. ) ;
#89138 = DIRECTION ( 'NONE',  ( -0.000000000000000000, 0.9126074666063771490, 0.4088369013363281623 ) ) ;
#89139 = FACE_OUTER_BOUND ( 'NONE', #157774, .T. ) ;
#89140 = ORIENTED_EDGE ( 'NONE', *, *, #166328, .T. ) ;
#89141 = ADVANCED_FACE ( 'NONE', ( #23421 ), #104188, .T. ) ;
#89142 = DIRECTION ( 'NONE',  ( -1.000000000000000000, 0.000000000000000000, 0.000000000000000000 ) ) ;
#89143 = CARTESIAN_POINT ( 'NONE',  ( 14.45963434102923983, 9.451541661385506998, -18.45387549883058398 ) ) ;
#89144 = CARTESIAN_POINT ( 'NONE',  ( 23.14999999999999858, -2.099999999988846344, -134.0000000000000284 ) ) ;
#89145 = ORIENTED_EDGE ( 'NONE', *, *, #1272, .T. ) ;
#89147 = VERTEX_POINT ( 'NONE', #183751 ) ;
#89146 = DIRECTION ( 'NONE',  ( 0.7071067811865493491, -0.7071067811865456854, -4.937700262164518065E-15 ) ) ;
#89148 = EDGE_LOOP ( 'NONE', ( #118620, #103613, #140634, #203866 ) ) ;
#89149 = CIRCLE ( 'NONE', #105694, 0.1000000000000075273 ) ;
#89150 = DIRECTION ( 'NONE',  ( -3.265361837132813586E-16, 0.4721928772777344019, 0.8814952561688430555 ) ) ;
#89151 = ORIENTED_EDGE ( 'NONE', *, *, #206914, .F. ) ;
#89152 = FACE_OUTER_BOUND ( 'NONE', #226853, .T. ) ;
#89153 = DIRECTION ( 'NONE',  ( 1.000000000000000000, 7.304098846218134667E-16, 0.000000000000000000 ) ) ;
#89154 = DIRECTION ( 'NONE',  ( 0.000000000000000000, -6.982962677686266711E-15, 1.000000000000000000 ) ) ;
#89155 = EDGE_LOOP ( 'NONE', ( #58799, #37891, #94782, #50545 ) ) ;
#89156 = DIRECTION ( 'NONE',  ( 0.000000000000000000, -0.7049548389605068133, 0.7092521942342977503 ) ) ;
#89157 = CARTESIAN_POINT ( 'NONE',  ( 22.39999999999999503, 11.50215294792677767, -198.5972978622482970 ) ) ;
#89158 = LINE ( 'NONE', #27948, #231066 ) ;
#89159 = ORIENTED_EDGE ( 'NONE', *, *, #163935, .F. ) ;
#89160 = EDGE_CURVE ( 'NONE', #135358, #95624, #60042, .T. ) ;
#89162 = EDGE_LOOP ( 'NONE', ( #231327, #64837, #254022, #201561 ) ) ;
#89161 = CARTESIAN_POINT ( 'NONE',  ( 21.14999999999999503, 1.115600667400684642E-11, -167.4999999999999716 ) ) ;
#89163 = FACE_OUTER_BOUND ( 'NONE', #186800, .T. ) ;
#89164 = CARTESIAN_POINT ( 'NONE',  ( 18.49999999999999645, 77.29973367124354411, -213.4949779616549392 ) ) ;
#89165 = EDGE_CURVE ( 'NONE', #256420, #202021, #143254, .T. ) ;
#89166 = CIRCLE ( 'NONE', #51723, 0.1000000000000028644 ) ;
#89167 = AXIS2_PLACEMENT_3D ( 'NONE', #28272, #166496, #247266 ) ;
#89168 = VERTEX_POINT ( 'NONE', #91064 ) ;
#89169 = CIRCLE ( 'NONE', #168344, 0.09999999999998898659 ) ;
#89171 = DIRECTION ( 'NONE',  ( 0.000000000000000000, 0.000000000000000000, 1.000000000000000000 ) ) ;
#89170 = TOROIDAL_SURFACE ( 'NONE', #218325, 11.65000000000000036, 0.1000000000000000056 ) ;
#89173 = ADVANCED_FACE ( 'NONE', ( #68957 ), #169360, .T. ) ;
#89172 = CARTESIAN_POINT ( 'NONE',  ( -17.78241384948270110, 41.57411277420364826, -235.4540984113116906 ) ) ;
#89174 = DIRECTION ( 'NONE',  ( 0.000000000000000000, 0.2128009952263485993, -0.9770955615653341697 ) ) ;
#89176 = ADVANCED_FACE ( 'NONE', ( #46783 ), #27278, .T. ) ;
#89175 = ORIENTED_EDGE ( 'NONE', *, *, #41995, .T. ) ;
#89177 = PLANE ( 'NONE',  #129889 ) ;
#89178 = CARTESIAN_POINT ( 'NONE',  ( 20.90000000000000213, 1.885425182446133885, -11.59641995933507808 ) ) ;
#89179 = EDGE_LOOP ( 'NONE', ( #249663, #203783, #245090, #31756 ) ) ;
#89180 = AXIS2_PLACEMENT_3D ( 'NONE', #5463, #141162, #21240 ) ;
#89181 = AXIS2_PLACEMENT_3D ( 'NONE', #165114, #88105, #49009 ) ;
#89182 = EDGE_CURVE ( 'NONE', #82768, #60760, #228836, .T. ) ;
#89183 = EDGE_CURVE ( 'NONE', #116440, #123667, #147348, .T. ) ;
#89184 = CIRCLE ( 'NONE', #10083, 0.09999999999999520384 ) ;
#89185 = ORIENTED_EDGE ( 'NONE', *, *, #138444, .F. ) ;
#89186 = CARTESIAN_POINT ( 'NONE',  ( -20.64999999999999858, -9.499999999988846255, -124.1060308773475924 ) ) ;
#89187 = AXIS2_PLACEMENT_3D ( 'NONE', #24199, #3308, #219801 ) ;
#89188 = AXIS2_PLACEMENT_3D ( 'NONE', #50949, #88793, #168410 ) ;
#89189 = VERTEX_POINT ( 'NONE', #50631 ) ;
#89190 = FACE_OUTER_BOUND ( 'NONE', #127482, .T. ) ;
#89191 = CARTESIAN_POINT ( 'NONE',  ( -16.92778301347272674, 10.00094491684634868, -79.57148189203122968 ) ) ;
#89193 = ORIENTED_EDGE ( 'NONE', *, *, #201740, .T. ) ;
#89192 = DIRECTION ( 'NONE',  ( -1.000000000000000000, 0.000000000000000000, 0.000000000000000000 ) ) ;
#89194 = CARTESIAN_POINT ( 'NONE',  ( 20.04142135623730070, 11.75000000001115907, -125.1500000000000341 ) ) ;
#89195 = CARTESIAN_POINT ( 'NONE',  ( 21.09696443733127325, 65.27599011609309798, -57.28832995747617218 ) ) ;
#89196 = CARTESIAN_POINT ( 'NONE',  ( -20.54999999999999716, 49.36776662947724503, -253.7196102226803021 ) ) ;
#89197 = CARTESIAN_POINT ( 'NONE',  ( 19.90000000000000568, 1.250000000000000000, 21.90000000000000213 ) ) ;
#89198 = DIRECTION ( 'NONE',  ( 3.469446951953728416E-14, -0.8660254037844309360, 0.5000000000000134337 ) ) ;
#89199 = CIRCLE ( 'NONE', #47679, 0.4000000000000010214 ) ;
#89200 = CARTESIAN_POINT ( 'NONE',  ( -17.04295772865440028, 10.02489942527099842, -79.65000000000004832 ) ) ;
#89201 = CIRCLE ( 'NONE', #5989, 0.2000000000000057288 ) ;
#89203 = EDGE_CURVE ( 'NONE', #251152, #84962, #49374, .T. ) ;
#89202 = DIRECTION ( 'NONE',  ( 0.000000000000000000, 0.8814952561688476074, -0.4721928772777262417 ) ) ;
#89205 = ORIENTED_EDGE ( 'NONE', *, *, #199378, .F. ) ;
#89204 = DIRECTION ( 'NONE',  ( 0.000000000000000000, -0.9126074666064696306, -0.4088369013361213278 ) ) ;
#89207 = CARTESIAN_POINT ( 'NONE',  ( -21.05000000000000071, 11.59999999999999964, -26.57179676972449656 ) ) ;
#89206 = VECTOR ( 'NONE', #19605, 1000.000000000000000 ) ;
#89208 = ADVANCED_FACE ( 'NONE', ( #106761 ), #114011, .F. ) ;
#89209 = CARTESIAN_POINT ( 'NONE',  ( 11.60000000000006004, 64.35000000001120668, -21.02310748452479316 ) ) ;
#89210 = AXIS2_PLACEMENT_3D ( 'NONE', #94691, #75167, #137652 ) ;
#89211 = DIRECTION ( 'NONE',  ( 0.000000000000000000, -0.1298341882519953583, -0.9915357197604861561 ) ) ;
#89213 = EDGE_CURVE ( 'NONE', #29274, #164555, #45518, .T. ) ;
#89212 = CARTESIAN_POINT ( 'NONE',  ( 20.86036036209898015, 65.37895722344167382, -195.8567590660222208 ) ) ;
#89214 = DIRECTION ( 'NONE',  ( -1.000000000000000000, 0.000000000000000000, 0.000000000000000000 ) ) ;
#89215 = CIRCLE ( 'NONE', #5811, 0.2000000000000058675 ) ;
#89216 = ORIENTED_EDGE ( 'NONE', *, *, #121954, .F. ) ;
#89218 = AXIS2_PLACEMENT_3D ( 'NONE', #15388, #12829, #72809 ) ;
#89217 = DIRECTION ( 'NONE',  ( -1.000000000000000000, 1.207181226542539700E-16, -2.694675058168174199E-16 ) ) ;
#89219 = DIRECTION ( 'NONE',  ( 0.000000000000000000, 0.000000000000000000, 1.000000000000000000 ) ) ;
#89220 = CARTESIAN_POINT ( 'NONE',  ( 23.14999999999999858, 2.000000000000002665, -33.50000000000000000 ) ) ;
#89221 = EDGE_CURVE ( 'NONE', #132077, #46773, #155755, .T. ) ;
#89222 = VERTEX_POINT ( 'NONE', #170654 ) ;
#89223 = LINE ( 'NONE', #47516, #85120 ) ;
#89224 = CARTESIAN_POINT ( 'NONE',  ( -16.94107738177415712, 10.01423928514777728, -79.55000000000005400 ) ) ;
#89225 = VERTEX_POINT ( 'NONE', #250142 ) ;
#89226 = DIRECTION ( 'NONE',  ( 0.000000000000000000, 0.9908441862701596881, 0.1350103645451904977 ) ) ;
#89227 = ORIENTED_EDGE ( 'NONE', *, *, #168780, .T. ) ;
#89228 = EDGE_CURVE ( 'NONE', #82975, #92271, #5858, .T. ) ;
#89229 = DIRECTION ( 'NONE',  ( 0.000000000000000000, -0.4999999999999673039, -0.8660254037844573594 ) ) ;
#89230 = ORIENTED_EDGE ( 'NONE', *, *, #102012, .T. ) ;
#89231 = FACE_BOUND ( 'NONE', #237178, .T. ) ;
#89232 = AXIS2_PLACEMENT_3D ( 'NONE', #13176, #229651, #50977 ) ;
#89233 = DIRECTION ( 'NONE',  ( -0.000000000000000000, -0.000000000000000000, -1.000000000000000000 ) ) ;
#89234 = VERTEX_POINT ( 'NONE', #6387 ) ;
#89235 = AXIS2_PLACEMENT_3D ( 'NONE', #154060, #135711, #171055 ) ;
#89236 = ORIENTED_EDGE ( 'NONE', *, *, #30374, .F. ) ;
#89237 = DIRECTION ( 'NONE',  ( 1.000000000000000000, 3.265361837132813093E-16, -0.000000000000000000 ) ) ;
#89239 = ORIENTED_EDGE ( 'NONE', *, *, #38869, .F. ) ;
#89238 = DIRECTION ( 'NONE',  ( 1.000000000000000000, 0.000000000000000000, 0.000000000000000000 ) ) ;
#89240 = CIRCLE ( 'NONE', #205771, 0.09999999999999939493 ) ;
#89241 = CARTESIAN_POINT ( 'NONE',  ( 20.94999675878240808, 65.70692517833212776, -64.06446533783034170 ) ) ;
#89242 = VERTEX_POINT ( 'NONE', #67646 ) ;
#89243 = AXIS2_PLACEMENT_3D ( 'NONE', #161728, #183830, #27370 ) ;
#89244 = TOROIDAL_SURFACE ( 'NONE', #235016, 0.6000000000000009770, 0.1000000000000000056 ) ;
#89245 = ORIENTED_EDGE ( 'NONE', *, *, #225238, .T. ) ;
#89246 = FACE_OUTER_BOUND ( 'NONE', #10012, .T. ) ;
#89247 = LINE ( 'NONE', #125807, #172163 ) ;
#89248 = CIRCLE ( 'NONE', #197581, 0.1000000000000075273 ) ;
#89249 = CARTESIAN_POINT ( 'NONE',  ( -20.64999999999999858, -9.499999999988846255, -191.1060308773475356 ) ) ;
#89250 = CARTESIAN_POINT ( 'NONE',  ( 21.04116576186320842, 65.37533692126021378, -57.19452571589663847 ) ) ;
#89251 = FACE_OUTER_BOUND ( 'NONE', #177828, .T. ) ;
#89252 = VECTOR ( 'NONE', #12393, 1000.000000000000000 ) ;
#89253 = VERTEX_POINT ( 'NONE', #147181 ) ;
#89254 = CARTESIAN_POINT ( 'NONE',  ( 21.05000000000000071, 85.50000000001232081, -160.1291383618718385 ) ) ;
#89255 = CIRCLE ( 'NONE', #31057, 0.1000000000000054040 ) ;
#89256 = CARTESIAN_POINT ( 'NONE',  ( -21.45000000000000284, 7.708578643773852157, -179.8499999999999943 ) ) ;
#89257 = CARTESIAN_POINT ( 'NONE',  ( 20.95289811251229750, 67.10683199555347755, -128.0212979906058308 ) ) ;
#89259 = DIRECTION ( 'NONE',  ( 1.000000000000000000, 0.000000000000000000, 0.000000000000000000 ) ) ;
#89258 = AXIS2_PLACEMENT_3D ( 'NONE', #239139, #194893, #100858 ) ;
#89260 = ORIENTED_EDGE ( 'NONE', *, *, #233497, .T. ) ;
#89261 = FACE_OUTER_BOUND ( 'NONE', #210283, .T. ) ;
#89262 = ORIENTED_EDGE ( 'NONE', *, *, #223657, .T. ) ;
#89263 = CARTESIAN_POINT ( 'NONE',  ( -18.59999999999999787, 77.25000000001185185, -95.22262673010921219 ) ) ;
#89264 = ORIENTED_EDGE ( 'NONE', *, *, #239262, .T. ) ;
#89265 = CARTESIAN_POINT ( 'NONE',  ( 23.14999999999999503, 69.35000000001259934, -191.3731074845244109 ) ) ;
#89266 = CARTESIAN_POINT ( 'NONE',  ( -23.25000000000000000, 19.98118924431957311, -235.6825596947570602 ) ) ;
#89267 = VERTEX_POINT ( 'NONE', #225417 ) ;
#89268 = EDGE_LOOP ( 'NONE', ( #110127, #29828, #83111 ) ) ;
#89270 = EDGE_LOOP ( 'NONE', ( #215642, #70910, #127743, #62071 ) ) ;
#89269 = DIRECTION ( 'NONE',  ( 1.000000000000000000, 7.304098846218134667E-16, 5.100424963727256530E-30 ) ) ;
#89271 = DIRECTION ( 'NONE',  ( 1.000000000000000000, 3.265361837132813093E-16, -0.000000000000000000 ) ) ;
#89272 = ORIENTED_EDGE ( 'NONE', *, *, #52909, .F. ) ;
#89273 = AXIS2_PLACEMENT_3D ( 'NONE', #60550, #140080, #120564 ) ;
#89274 = LINE ( 'NONE', #91855, #139618 ) ;
#89275 = FILL_AREA_STYLE_COLOUR ( '', #106246 ) ;
#89276 = EDGE_LOOP ( 'NONE', ( #35463, #27209, #52081, #192881 ) ) ;
#89277 = CIRCLE ( 'NONE', #235046, 2.000000000000001776 ) ;
#89278 = DIRECTION ( 'NONE',  ( 0.000000000000000000, 0.000000000000000000, -1.000000000000000000 ) ) ;
#89279 = EDGE_CURVE ( 'NONE', #117008, #188047, #48080, .T. ) ;
#89280 = DIRECTION ( 'NONE',  ( -1.000000000000000000, 0.000000000000000000, 0.000000000000000000 ) ) ;
#89282 = VERTEX_POINT ( 'NONE', #28578 ) ;
#89281 = VECTOR ( 'NONE', #169221, 1000.000000000000114 ) ;
#89283 = AXIS2_PLACEMENT_3D ( 'NONE', #198997, #93466, #255050 ) ;
#89284 = AXIS2_PLACEMENT_3D ( 'NONE', #254611, #5413, #161980 ) ;
#89285 = CYLINDRICAL_SURFACE ( 'NONE', #47399, 1.500000000000001332 ) ;
#89287 = EDGE_CURVE ( 'NONE', #89282, #152832, #118326, .T. ) ;
#89286 = CARTESIAN_POINT ( 'NONE',  ( -22.50000000000000000, 75.90000000001172964, -81.17267829206912211 ) ) ;
#89288 = DIRECTION ( 'NONE',  ( 1.000000000000000000, 0.000000000000000000, 0.000000000000000000 ) ) ;
#89290 = VERTEX_POINT ( 'NONE', #75380 ) ;
#89289 = DIRECTION ( 'NONE',  ( -1.000000000000000000, 0.000000000000000000, 0.000000000000000000 ) ) ;
#89291 = EDGE_CURVE ( 'NONE', #234652, #142813, #9975, .T. ) ;
#89292 = CARTESIAN_POINT ( 'NONE',  ( -22.59999999999999787, 11.74987124438766273, -133.9345704089863318 ) ) ;
#89293 = DIRECTION ( 'NONE',  ( -0.000000000000000000, -0.7049548389605067023, 0.7092521942342977503 ) ) ;
#89295 = FACE_OUTER_BOUND ( 'NONE', #146260, .T. ) ;
#89294 = CARTESIAN_POINT ( 'NONE',  ( -18.43707690579159930, -9.682403433465241349, -140.6568433774128266 ) ) ;
#89296 = FACE_OUTER_BOUND ( 'NONE', #202506, .T. ) ;
#89297 = DIRECTION ( 'NONE',  ( 0.000000000000000000, 0.01562500000001058528, 0.9998779222360095753 ) ) ;
#89298 = CARTESIAN_POINT ( 'NONE',  ( 22.39999999999999503, 11.65000000001116298, -66.90000000000004832 ) ) ;
#89299 = CYLINDRICAL_SURFACE ( 'NONE', #238506, 0.09999999999999939493 ) ;
#89300 = AXIS2_PLACEMENT_3D ( 'NONE', #92841, #236208, #254460 ) ;
#89301 = EDGE_LOOP ( 'NONE', ( #174948, #43583, #171811, #183665 ) ) ;
#89302 = ORIENTED_EDGE ( 'NONE', *, *, #196568, .T. ) ;
#89303 = EDGE_CURVE ( 'NONE', #238843, #251548, #230587, .T. ) ;
#89304 = TOROIDAL_SURFACE ( 'NONE', #43542, 11.90000000000000213, 0.1000000000000000056 ) ;
#89305 = ORIENTED_EDGE ( 'NONE', *, *, #156993, .F. ) ;
#89306 = EDGE_CURVE ( 'NONE', #142842, #71479, #184955, .T. ) ;
#89307 = DIRECTION ( 'NONE',  ( -4.336808689942052446E-15, 0.8660254037844445918, 0.4999999999999896194 ) ) ;
#89308 = ADVANCED_FACE ( 'NONE', ( #76627 ), #231882, .F. ) ;
#89309 = CARTESIAN_POINT ( 'NONE',  ( -18.59999999999999787, 64.35000000001234355, -163.0083017138704236 ) ) ;
#89310 = EDGE_LOOP ( 'NONE', ( #71489, #43315, #219266, #109218 ) ) ;
#89311 = DIRECTION ( 'NONE',  ( -0.000000000000000000, 0.000000000000000000, -1.000000000000000000 ) ) ;
#89312 = CARTESIAN_POINT ( 'NONE',  ( 20.89192007715127986, 10.32898536001801304, -206.5826683222763904 ) ) ;
#89313 = ORIENTED_EDGE ( 'NONE', *, *, #250555, .T. ) ;
#89314 = ORIENTED_EDGE ( 'NONE', *, *, #166573, .F. ) ;
#89315 = DIRECTION ( 'NONE',  ( 0.5932847527679310229, -0.8049926720990042694, 0.000000000000000000 ) ) ;
#89316 = LINE ( 'NONE', #168918, #167709 ) ;
#89317 = ORIENTED_EDGE ( 'NONE', *, *, #221324, .F. ) ;
#89318 = EDGE_CURVE ( 'NONE', #257030, #100823, #72535, .T. ) ;
#89319 = DIRECTION ( 'NONE',  ( -1.000000000000000000, 3.265361837132813093E-16, 2.280189983783949500E-30 ) ) ;
#89321 = VERTEX_POINT ( 'NONE', #94901 ) ;
#89320 = DIRECTION ( 'NONE',  ( -1.000000000000000000, 0.000000000000000000, 0.000000000000000000 ) ) ;
#89322 = DIRECTION ( 'NONE',  ( -1.000000000000000000, -0.000000000000000000, -0.000000000000000000 ) ) ;
#89323 = DIRECTION ( 'NONE',  ( 1.000000000000000000, 0.000000000000000000, 0.000000000000000000 ) ) ;
#89325 = ORIENTED_EDGE ( 'NONE', *, *, #146075, .T. ) ;
#89324 = DIRECTION ( 'NONE',  ( 0.000000000000000000, 0.000000000000000000, -1.000000000000000000 ) ) ;
#89326 = CARTESIAN_POINT ( 'NONE',  ( -18.51697539158856998, 10.31565961587945779, -72.53641941191783360 ) ) ;
#89327 = CARTESIAN_POINT ( 'NONE',  ( -17.01473183483382101, 9.950000000011138823, -46.25000000000000000 ) ) ;
#89328 = CARTESIAN_POINT ( 'NONE',  ( 18.49999999999998934, 10.24999999999999822, -24.65000000000000213 ) ) ;
#89330 = ADVANCED_FACE ( 'NONE', ( #135306 ), #64154, .F. ) ;
#89329 = DIRECTION ( 'NONE',  ( -0.000000000000000000, -0.9371753822965315228, 0.3488585713686134238 ) ) ;
#89332 = CARTESIAN_POINT ( 'NONE',  ( 21.05000005001280172, 8.871279691782062216, -179.6779475882455870 ) ) ;
#89331 = CARTESIAN_POINT ( 'NONE',  ( -16.97683809663752186, 9.950000000011137047, -154.0976359818037054 ) ) ;
#89333 = LINE ( 'NONE', #204146, #253388 ) ;
#89334 = VECTOR ( 'NONE', #112044, 1000.000000000000114 ) ;
#89335 = DIRECTION ( 'NONE',  ( 0.000000000000000000, 0.000000000000000000, 1.000000000000000000 ) ) ;
#89336 = FACE_OUTER_BOUND ( 'NONE', #174908, .T. ) ;
#89337 = CARTESIAN_POINT ( 'NONE',  ( 20.94999999999999574, 1.736257131608553550, -112.0686523290175245 ) ) ;
#89338 = EDGE_LOOP ( 'NONE', ( #255865, #104837, #18697, #235150 ) ) ;
#89339 = AXIS2_PLACEMENT_3D ( 'NONE', #149706, #227935, #10178 ) ;
#89340 = EDGE_LOOP ( 'NONE', ( #165121, #176620, #250025 ) ) ;
#89341 = VECTOR ( 'NONE', #124469, 1000.000000000000000 ) ;
#89342 = CARTESIAN_POINT ( 'NONE',  ( 18.79999999999999716, 5.488301202077012775, 16.40000000000000213 ) ) ;
#89343 = ORIENTED_EDGE ( 'NONE', *, *, #85305, .F. ) ;
#89344 = DIRECTION ( 'NONE',  ( 1.000000000000000000, -0.000000000000000000, -0.000000000000000000 ) ) ;
#89345 = ORIENTED_EDGE ( 'NONE', *, *, #137705, .F. ) ;
#89346 = LINE ( 'NONE', #112785, #235957 ) ;
#89347 =( NAMED_UNIT ( * ) SI_UNIT ( $, .STERADIAN. ) SOLID_ANGLE_UNIT ( ) );
#89348 = ORIENTED_EDGE ( 'NONE', *, *, #21791, .T. ) ;
#89349 = AXIS2_PLACEMENT_3D ( 'NONE', #108140, #49449, #27362 ) ;
#89350 = DIRECTION ( 'NONE',  ( 0.000000000000000000, 0.000000000000000000, 1.000000000000000000 ) ) ;
#89351 = FILL_AREA_STYLE_COLOUR ( '', #169059 ) ;
#89352 = VECTOR ( 'NONE', #149653, 1000.000000000000000 ) ;
#89353 = EDGE_LOOP ( 'NONE', ( #54342, #220095, #191287, #122976 ) ) ;
#89354 = EDGE_LOOP ( 'NONE', ( #173316, #185481, #107007, #222425 ) ) ;
#89355 = ORIENTED_EDGE ( 'NONE', *, *, #235771, .T. ) ;
#89356 = AXIS2_PLACEMENT_3D ( 'NONE', #23597, #144759, #84772 ) ;
#89357 = EDGE_CURVE ( 'NONE', #31810, #3980, #194039, .T. ) ;
#89358 = LINE ( 'NONE', #125920, #237733 ) ;
#89359 = CARTESIAN_POINT ( 'NONE',  ( 21.14999999999998082, 87.75000000001193712, -103.0231074845242318 ) ) ;
#89360 = CARTESIAN_POINT ( 'NONE',  ( 18.59999999999997655, 76.00000000001126921, -203.5231074845248997 ) ) ;
#89362 = ADVANCED_FACE ( 'NONE', ( #175758 ), #255215, .T. ) ;
#89361 = AXIS2_PLACEMENT_3D ( 'NONE', #65095, #51926, #211032 ) ;
#89363 = DIRECTION ( 'NONE',  ( 1.000000000000000000, 0.000000000000000000, 0.000000000000000000 ) ) ;
#89364 = LINE ( 'NONE', #51505, #15031 ) ;
#89365 = CARTESIAN_POINT ( 'NONE',  ( 20.94999999999999929, 76.00000000001243450, -168.1231074845243540 ) ) ;
#89366 = CARTESIAN_POINT ( 'NONE',  ( -12.60206096961791822, 9.389686005666813884, -82.67284350635138424 ) ) ;
#89368 = ORIENTED_EDGE ( 'NONE', *, *, #90551, .F. ) ;
#89367 = CARTESIAN_POINT ( 'NONE',  ( -20.64999999999999858, 71.75000000001156764, -57.27310748452435263 ) ) ;
#89370 = DIRECTION ( 'NONE',  ( -1.000000000000000000, 0.000000000000000000, 0.000000000000000000 ) ) ;
#89369 = CARTESIAN_POINT ( 'NONE',  ( 20.22483756094572271, 9.501904678882469923, -75.13953912871474472 ) ) ;
#89371 = EDGE_CURVE ( 'NONE', #238125, #59420, #239114, .T. ) ;
#89372 = DIRECTION ( 'NONE',  ( -0.7071067811865456854, -0.7071067811865493491, -4.937700262164544098E-15 ) ) ;
#89373 = ADVANCED_FACE ( 'NONE', ( #177045 ), #132780, .F. ) ;
#89374 = ORIENTED_EDGE ( 'NONE', *, *, #72392, .T. ) ;
#89375 = CARTESIAN_POINT ( 'NONE',  ( -20.85000000000000142, -11.64999999998884483, -134.0000000000000284 ) ) ;
#89376 = AXIS2_PLACEMENT_3D ( 'NONE', #15414, #14138, #93649 ) ;
#89377 = DIRECTION ( 'NONE',  ( 0.000000000000000000, 0.2617529984165031243, 0.9651348961777157509 ) ) ;
#89378 = LINE ( 'NONE', #48978, #121213 ) ;
#89379 = TOROIDAL_SURFACE ( 'NONE', #189358, 0.2000000000000000111, 0.1000000000000000056 ) ;
#89380 = ORIENTED_EDGE ( 'NONE', *, *, #113272, .F. ) ;
#89381 = CIRCLE ( 'NONE', #147661, 0.09999999999999939493 ) ;
#89382 = EDGE_CURVE ( 'NONE', #190151, #149752, #126691, .T. ) ;
#89383 = CARTESIAN_POINT ( 'NONE',  ( 20.94999999999999574, 10.42338541492406279, -141.4920519238701218 ) ) ;
#89384 = TOROIDAL_SURFACE ( 'NONE', #156061, 0.2000000000000000111, 0.1000000000000000056 ) ;
#89385 = ADVANCED_FACE ( 'NONE', ( #173223 ), #126503, .T. ) ;
#89386 = CYLINDRICAL_SURFACE ( 'NONE', #173497, 0.1000000000000028644 ) ;
#89387 = DIRECTION ( 'NONE',  ( -0.8049926720990042694, 0.5932847527679310229, 4.142885285818786163E-15 ) ) ;
#89389 = EDGE_CURVE ( 'NONE', #91807, #114829, #97448, .T. ) ;
#89388 = EDGE_CURVE ( 'NONE', #159212, #13871, #14098, .T. ) ;
#89390 = ORIENTED_EDGE ( 'NONE', *, *, #144390, .T. ) ;
#89391 = VERTEX_POINT ( 'NONE', #12834 ) ;
#89392 = VECTOR ( 'NONE', #29632, 1000.000000000000000 ) ;
#89393 = DIRECTION ( 'NONE',  ( -0.000000000000000000, -0.9876197685951252359, -0.1568667991644863424 ) ) ;
#89394 = DIRECTION ( 'NONE',  ( -1.836970198721029934E-16, 0.9770955615653316162, 0.2128009952263604232 ) ) ;
#89395 = DIRECTION ( 'NONE',  ( -0.000000000000000000, 0.000000000000000000, 1.000000000000000000 ) ) ;
#89396 = DIRECTION ( 'NONE',  ( 0.000000000000000000, 0.9999631594459055250, 0.008583690987131395445 ) ) ;
#89397 = ORIENTED_EDGE ( 'NONE', *, *, #135283, .F. ) ;
#89398 = CIRCLE ( 'NONE', #105951, 11.90000000000000746 ) ;
#89399 = AXIS2_PLACEMENT_3D ( 'NONE', #231940, #53289, #205938 ) ;
#89400 = CARTESIAN_POINT ( 'NONE',  ( -12.25000000000000178, 9.350000000011139178, -117.2500000000000284 ) ) ;
#89401 = EDGE_CURVE ( 'NONE', #1366, #70072, #209908, .T. ) ;
#89402 = CARTESIAN_POINT ( 'NONE',  ( 18.59999999999999076, 65.50857864377491069, -145.2731074845244450 ) ) ;
#89403 = DIRECTION ( 'NONE',  ( 0.000000000000000000, 0.000000000000000000, 1.000000000000000000 ) ) ;
#89404 = DIRECTION ( 'NONE',  ( 1.000000000000000000, 0.000000000000000000, 0.000000000000000000 ) ) ;
#89405 = EDGE_CURVE ( 'NONE', #88007, #105461, #43310, .T. ) ;
#89406 = EDGE_CURVE ( 'NONE', #191384, #135942, #34984, .T. ) ;
#89407 = ORIENTED_EDGE ( 'NONE', *, *, #101559, .T. ) ;
#89408 = CARTESIAN_POINT ( 'NONE',  ( 20.89192007715127986, 10.32898536000685574, -39.08266832227643306 ) ) ;
#89409 = EDGE_CURVE ( 'NONE', #145844, #127497, #134843, .T. ) ;
#89411 = EDGE_LOOP ( 'NONE', ( #53104, #195543, #117130 ) ) ;
#89410 = CYLINDRICAL_SURFACE ( 'NONE', #42035, 0.09999999999999543976 ) ;
#89412 = CARTESIAN_POINT ( 'NONE',  ( -20.85000000000000142, 77.14957036958755054, -95.20719500002232394 ) ) ;
#89413 = DIRECTION ( 'NONE',  ( -1.000000000000000000, 0.000000000000000000, 0.000000000000000000 ) ) ;
#89414 = FACE_OUTER_BOUND ( 'NONE', #165030, .T. ) ;
#89415 = SPHERICAL_SURFACE ( 'NONE', #175356, 0.1000000000000000056 ) ;
#89416 = CYLINDRICAL_SURFACE ( 'NONE', #50505, 0.1000000000000028644 ) ;
#89417 = ADVANCED_FACE ( 'NONE', ( #122191 ), #143000, .T. ) ;
#89418 = CARTESIAN_POINT ( 'NONE',  ( 18.39999999999998082, 11.47316190336247033, -9.250000000000000000 ) ) ;
#89419 = CYLINDRICAL_SURFACE ( 'NONE', #102893, 0.1000000000000028644 ) ;
#89420 = ORIENTED_EDGE ( 'NONE', *, *, #166125, .T. ) ;
#89421 = FACE_OUTER_BOUND ( 'NONE', #229161, .T. ) ;
#89422 = AXIS2_PLACEMENT_3D ( 'NONE', #175802, #57089, #114528 ) ;
#89423 = CARTESIAN_POINT ( 'NONE',  ( -20.64999999999999858, 68.75000000001253397, -182.2731074845244166 ) ) ;
#89424 = DIRECTION ( 'NONE',  ( 1.000000000000000000, 7.304098846218133681E-16, 5.311601492717083645E-30 ) ) ;
#89426 = CIRCLE ( 'NONE', #93711, 0.1000000000000000333 ) ;
#89425 = CARTESIAN_POINT ( 'NONE',  ( -18.40000000000000213, 11.33174054713633261, -188.3499999999999659 ) ) ;
#89427 = AXIS2_PLACEMENT_3D ( 'NONE', #119352, #197583, #201440 ) ;
#89428 = FACE_OUTER_BOUND ( 'NONE', #15166, .T. ) ;
#89429 = CARTESIAN_POINT ( 'NONE',  ( 21.05000000000000071, 11.65000000001115943, -100.6000000000000369 ) ) ;
#89430 = ORIENTED_EDGE ( 'NONE', *, *, #114229, .T. ) ;
#89431 = EDGE_LOOP ( 'NONE', ( #208743, #242886, #124885, #154427 ) ) ;
#89432 = CIRCLE ( 'NONE', #205969, 6.258578643762724880 ) ;
#89433 = LINE ( 'NONE', #96795, #130885 ) ;
#89434 = CARTESIAN_POINT ( 'NONE',  ( -18.50000000000000000, 64.25000000001186606, -90.87310748452439668 ) ) ;
#89435 = VECTOR ( 'NONE', #21092, 1000.000000000000000 ) ;
#89436 = DIRECTION ( 'NONE',  ( 1.000000000000000000, -7.304098846218133681E-16, -2.111765289898285610E-31 ) ) ;
#89437 = CARTESIAN_POINT ( 'NONE',  ( 21.05000000000000071, 70.15000000001163016, -59.39061026024639034 ) ) ;
#89439 = CIRCLE ( 'NONE', #222704, 0.2000000000000057288 ) ;
#89438 = DIRECTION ( 'NONE',  ( 0.000000000000000000, 0.000000000000000000, -1.000000000000000000 ) ) ;
#89440 = CARTESIAN_POINT ( 'NONE',  ( 18.49999999999999289, 66.40155400966892785, -213.5088390336144073 ) ) ;
#89441 = AXIS2_PLACEMENT_3D ( 'NONE', #53572, #212656, #253045 ) ;
#89442 = CIRCLE ( 'NONE', #235210, 0.09999999999999939493 ) ;
#89443 = CARTESIAN_POINT ( 'NONE',  ( -20.85000000106584750, 17.15319076756266981, -224.5445635972164951 ) ) ;
#89444 = CARTESIAN_POINT ( 'NONE',  ( -20.94999999999999929, 74.75000000001189449, -95.02310748452431710 ) ) ;
#89445 = ORIENTED_EDGE ( 'NONE', *, *, #6655, .F. ) ;
#89446 = PLANE ( 'NONE',  #106688 ) ;
#89447 = EDGE_LOOP ( 'NONE', ( #168504, #246441, #120601, #90241 ) ) ;
#89448 = CARTESIAN_POINT ( 'NONE',  ( 20.84999999999999432, -1.164121893230052995, -141.9148480855716343 ) ) ;
#89449 = CARTESIAN_POINT ( 'NONE',  ( -23.15000000000000213, 1.115600667400684642E-11, -67.00000000000004263 ) ) ;
#89451 = CIRCLE ( 'NONE', #68625, 4.049999999999998046 ) ;
#89450 = DIRECTION ( 'NONE',  ( 0.000000000000000000, 0.000000000000000000, 1.000000000000000000 ) ) ;
#89452 = CARTESIAN_POINT ( 'NONE',  ( -22.50000000000000000, 11.64957080754479968, 0.09999999999999592548 ) ) ;
#89453 = DIRECTION ( 'NONE',  ( 0.000000000000000000, -0.9651348961777157509, 0.2617529984165031243 ) ) ;
#89454 = CARTESIAN_POINT ( 'NONE',  ( 18.41832399655377372, 85.68240326668576756, -62.86626386449687942 ) ) ;
#89455 = DIRECTION ( 'NONE',  ( -0.000000000000000000, -0.1350103645451876666, -0.9908441862701600211 ) ) ;
#89456 = VERTEX_POINT ( 'NONE', #21807 ) ;
#89457 = DIRECTION ( 'NONE',  ( 0.000000000000000000, 0.8814952561688437216, -0.4721928772777334582 ) ) ;
#89458 = EDGE_CURVE ( 'NONE', #241192, #117897, #239564, .T. ) ;
#89459 = CARTESIAN_POINT ( 'NONE',  ( -18.59999999999999787, 47.95459712139159336, -246.5019368548292675 ) ) ;
#89460 = FACE_OUTER_BOUND ( 'NONE', #133787, .T. ) ;
#89461 = ADVANCED_FACE ( 'NONE', ( #139140 ), #217409, .T. ) ;
#89462 = DIRECTION ( 'NONE',  ( 0.000000000000000000, -6.853228547068871147E-15, 1.000000000000000000 ) ) ;
#89463 = AXIS2_PLACEMENT_3D ( 'NONE', #173064, #76471, #73951 ) ;
#89464 = VERTEX_POINT ( 'NONE', #80442 ) ;
#89465 = DIRECTION ( 'NONE',  ( 0.000000000000000000, 0.8814952561688476074, -0.4721928772777262417 ) ) ;
#89467 = EDGE_CURVE ( 'NONE', #116008, #47209, #230755, .T. ) ;
#89466 = CARTESIAN_POINT ( 'NONE',  ( -37.88850191057539973, 11.75000000000000000, 31.50000000000000000 ) ) ;
#89469 = EDGE_CURVE ( 'NONE', #206042, #82519, #51633, .T. ) ;
#89468 = ORIENTED_EDGE ( 'NONE', *, *, #19513, .F. ) ;
#89470 = ORIENTED_EDGE ( 'NONE', *, *, #143324, .F. ) ;
#89471 = DIRECTION ( 'NONE',  ( -1.000000000000000000, 0.000000000000000000, 0.000000000000000000 ) ) ;
#89472 = CARTESIAN_POINT ( 'NONE',  ( -18.59999999999999787, 70.05000000001165006, -59.21740517948951066 ) ) ;
#89473 = ORIENTED_EDGE ( 'NONE', *, *, #155932, .T. ) ;
#89474 = CARTESIAN_POINT ( 'NONE',  ( 21.02374657821574644, 64.39999999919136542, -42.95131071432642500 ) ) ;
#89475 = DIRECTION ( 'NONE',  ( 1.000000000000000000, 2.952720810173289112E-16, -0.000000000000000000 ) ) ;
#89476 = ORIENTED_EDGE ( 'NONE', *, *, #73537, .T. ) ;
#89477 = TOROIDAL_SURFACE ( 'NONE', #118564, 0.9750000000000019762, 0.1000000000000000056 ) ;
#89478 = ADVANCED_FACE ( 'NONE', ( #200435 ), #180877, .T. ) ;
#89479 = ADVANCED_FACE ( 'NONE', ( #238264 ), #10180, .F. ) ;
#89480 = DIRECTION ( 'NONE',  ( 0.000000000000000000, 0.000000000000000000, -1.000000000000000000 ) ) ;
#89481 = AXIS2_PLACEMENT_3D ( 'NONE', #173536, #195635, #233477 ) ;
#89482 = ORIENTED_EDGE ( 'NONE', *, *, #43435, .T. ) ;
#89483 = DIRECTION ( 'NONE',  ( 0.000000000000000000, 0.8814952561688432775, -0.4721928772777344019 ) ) ;
#89484 = LINE ( 'NONE', #4801, #21153 ) ;
#89486 = VERTEX_POINT ( 'NONE', #908 ) ;
#89485 = CARTESIAN_POINT ( 'NONE',  ( -23.25000000000000355, 59.20211495293902004, -220.5705723384363921 ) ) ;
#89487 = DIRECTION ( 'NONE',  ( 0.000000000000000000, 0.000000000000000000, -1.000000000000000000 ) ) ;
#89489 = UNCERTAINTY_MEASURE_WITH_UNIT (LENGTH_MEASURE( 1.000000000000000082E-05 ), #53275, 'distance_accuracy_value', 'NONE');
#89488 = DIRECTION ( 'NONE',  ( -1.836970198721029934E-16, 0.9770955615653316162, 0.2128009952263604232 ) ) ;
#89490 = DIRECTION ( 'NONE',  ( -0.000000000000000000, 0.9770955615653313941, 0.2128009952263603677 ) ) ;
#89491 = DIRECTION ( 'NONE',  ( -1.000000000000000000, -0.000000000000000000, -0.000000000000000000 ) ) ;
#89492 = PLANE ( 'NONE',  #75196 ) ;
#89493 = DIRECTION ( 'NONE',  ( 0.000000000000000000, 0.9126074666063781482, 0.4088369013363255533 ) ) ;
#89496 = ORIENTED_EDGE ( 'NONE', *, *, #188211, .T. ) ;
#89495 = ADVANCED_FACE ( 'NONE', ( #137869 ), #59606, .T. ) ;
#89494 = DIRECTION ( 'NONE',  ( -1.000000000000000000, 0.000000000000000000, -0.000000000000000000 ) ) ;
#89497 = VERTEX_POINT ( 'NONE', #161322 ) ;
#89499 = CARTESIAN_POINT ( 'NONE',  ( -14.45422546970483957, 9.450602096099682825, -85.44389596309675028 ) ) ;
#89498 = CARTESIAN_POINT ( 'NONE',  ( -21.33487959338958362, 69.27444184810046579, -69.52310748452435973 ) ) ;
#89501 = ORIENTED_EDGE ( 'NONE', *, *, #251423, .F. ) ;
#89500 = CARTESIAN_POINT ( 'NONE',  ( 20.95443524775735256, 8.878554263883966513, -109.0337222756001836 ) ) ;
#89502 = ORIENTED_EDGE ( 'NONE', *, *, #9222, .F. ) ;
#89503 = EDGE_CURVE ( 'NONE', #3167, #236242, #64328, .T. ) ;
#89504 = DIRECTION ( 'NONE',  ( 0.000000000000000000, -0.9654727137038715545, 0.2605042016806676242 ) ) ;
#89505 = CARTESIAN_POINT ( 'NONE',  ( 18.49999999999999289, 69.55000000001246008, -181.7731074845244166 ) ) ;
#89506 = VECTOR ( 'NONE', #107863, 1000.000000000000000 ) ;
#89507 = AXIS2_PLACEMENT_3D ( 'NONE', #134731, #179052, #18658 ) ;
#89508 = CARTESIAN_POINT ( 'NONE',  ( -23.25000000000000000, 64.25000000001170974, -69.52310748452438816 ) ) ;
#89509 = DIRECTION ( 'NONE',  ( 0.000000000000000000, 0.000000000000000000, 1.000000000000000000 ) ) ;
#89510 = DIRECTION ( 'NONE',  ( -0.000000000000000000, 0.9916376685811522096, -0.1290532225515392817 ) ) ;
#89512 = ADVANCED_FACE ( 'NONE', ( #19227 ), #103870, .T. ) ;
#89511 = FACE_OUTER_BOUND ( 'NONE', #12513, .T. ) ;
#89513 = EDGE_CURVE ( 'NONE', #80704, #197421, #163721, .T. ) ;
#89514 = B_SPLINE_CURVE_WITH_KNOTS ( 'NONE', 3,
 ( #192697, #252644, #91021, #231832, #125343, #71485, #152310, #104461, #32368, #72779, #203588, #24979, #250100, #164474 ),
 .UNSPECIFIED., .F., .F.,
 ( 4, 2, 2, 2, 2, 2, 4 ),
 ( 1.387778780781445676E-17, 0.0003823333598417443468, 0.0005735000397626304793, 0.0006690833797230903235, 0.0007168750497033217093, 0.0007407708846934326317, 0.0007646667196835435542 ),
 .UNSPECIFIED. ) ;
#89515 = CARTESIAN_POINT ( 'NONE',  ( -20.94999999999999929, -1.736257131586239844, -179.0686523290174819 ) ) ;
#89516 = VERTEX_POINT ( 'NONE', #178330 ) ;
#89517 = ORIENTED_EDGE ( 'NONE', *, *, #145301, .F. ) ;
#89518 = CARTESIAN_POINT ( 'NONE',  ( -18.59999999999999787, 16.00289399696429271, -219.2628689893550700 ) ) ;
#89519 = AXIS2_PLACEMENT_3D ( 'NONE', #123273, #25468, #39911 ) ;
#89520 = ADVANCED_FACE ( 'NONE', ( #20533 ), #158768, .T. ) ;
#89521 = EDGE_LOOP ( 'NONE', ( #112521, #11021, #63319, #227819 ) ) ;
#89522 = CARTESIAN_POINT ( 'NONE',  ( 19.99999999999998934, 11.75000000000000000, -21.35000000000000142 ) ) ;
#89523 = ORIENTED_EDGE ( 'NONE', *, *, #122964, .T. ) ;
#89524 = CARTESIAN_POINT ( 'NONE',  ( -21.55000000000000071, 7.350000000011155166, -88.15000000000004832 ) ) ;
#89525 = CIRCLE ( 'NONE', #222805, 0.8750000000000007772 ) ;
#89526 = AXIS2_PLACEMENT_3D ( 'NONE', #146135, #148726, #4058 ) ;
#89527 = CARTESIAN_POINT ( 'NONE',  ( 21.72449340488910252, 65.71604372252076587, -93.77310748452438816 ) ) ;
#89528 =( GEOMETRIC_REPRESENTATION_CONTEXT ( 3 ) GLOBAL_UNCERTAINTY_ASSIGNED_CONTEXT ( ( #230290 ) ) GLOBAL_UNIT_ASSIGNED_CONTEXT ( ( #198401, #219236, #176293 ) ) REPRESENTATION_CONTEXT ( 'NONE', 'WORKASPACE' ) );
#89529 = CARTESIAN_POINT ( 'NONE',  ( 20.94999999999997442, -1.263275465217258198, -41.40186466674640542 ) ) ;
#89530 = EDGE_LOOP ( 'NONE', ( #234268, #84127, #37835, #113989 ) ) ;
#89531 = EDGE_CURVE ( 'NONE', #89486, #80723, #197587, .T. ) ;
#89532 = DIRECTION ( 'NONE',  ( 0.000000000000000000, 0.2128009952263604787, -0.9770955615653313941 ) ) ;
#89533 = EDGE_LOOP ( 'NONE', ( #123689, #254718, #213122 ) ) ;
#89534 = CARTESIAN_POINT ( 'NONE',  ( -20.64999999999999858, 4.349999999999999645, -12.35000000000000142 ) ) ;
#89535 = CARTESIAN_POINT ( 'NONE',  ( -16.87665923198281348, 9.950000000011138823, -87.85000000000005116 ) ) ;
#89536 = DIRECTION ( 'NONE',  ( 0.000000000000000000, 0.000000000000000000, -1.000000000000000000 ) ) ;
#89537 = EDGE_CURVE ( 'NONE', #71510, #8323, #243385, .T. ) ;
#89538 = ORIENTED_EDGE ( 'NONE', *, *, #141766, .T. ) ;
#89539 = LINE ( 'NONE', #209496, #202591 ) ;
#89540 = EDGE_LOOP ( 'NONE', ( #242869, #249428, #188796, #141016, #221748, #217134 ) ) ;
#89543 = ORIENTED_EDGE ( 'NONE', *, *, #24231, .F. ) ;
#89542 = DIRECTION ( 'NONE',  ( 2.952720810173289112E-16, 1.000000000000000000, 6.982962677686266711E-15 ) ) ;
#89541 = DIRECTION ( 'NONE',  ( 0.000000000000000000, 0.000000000000000000, 1.000000000000000000 ) ) ;
#89544 = DIRECTION ( 'NONE',  ( -1.000000000000000000, 0.000000000000000000, -0.000000000000000000 ) ) ;
#89546 = VERTEX_POINT ( 'NONE', #109016 ) ;
#89545 = AXIS2_PLACEMENT_3D ( 'NONE', #46897, #245122, #66483 ) ;
#89547 = AXIS2_PLACEMENT_3D ( 'NONE', #156371, #54658, #118516 ) ;
#89548 = LINE ( 'NONE', #169138, #4527 ) ;
#89549 = VERTEX_POINT ( 'NONE', #245982 ) ;
#89550 = AXIS2_PLACEMENT_3D ( 'NONE', #242128, #63483, #12535 ) ;
#89551 = ADVANCED_FACE ( 'NONE', ( #25650 ), #165159, .T. ) ;
#89552 = DIRECTION ( 'NONE',  ( 1.000000000000000000, 0.000000000000000000, 0.000000000000000000 ) ) ;
#89553 = PLANE ( 'NONE',  #234451 ) ;
#89554 = CARTESIAN_POINT ( 'NONE',  ( -18.59999999999999787, -9.321008403350132809, -74.23593824907793248 ) ) ;
#89555 = AXIS2_PLACEMENT_3D ( 'NONE', #210728, #255909, #248565 ) ;
#89556 = CIRCLE ( 'NONE', #152139, 0.1000000000000028644 ) ;
#89557 = DIRECTION ( 'NONE',  ( 0.000000000000000000, -6.240597636138643358E-14, -1.000000000000000000 ) ) ;
#89558 = AXIS2_PLACEMENT_3D ( 'NONE', #35679, #76051, #156909 ) ;
#89559 = VERTEX_POINT ( 'NONE', #7360 ) ;
#89560 = SPHERICAL_SURFACE ( 'NONE', #123304, 0.1000000000000000056 ) ;
#89561 = CARTESIAN_POINT ( 'NONE',  ( -16.80100914604133067, 14.14529455580030515, -219.2243293987745858 ) ) ;
#89562 = LINE ( 'NONE', #169149, #184416 ) ;
#89563 = EDGE_LOOP ( 'NONE', ( #7160, #101283, #194411, #143055 ) ) ;
#89564 = DIRECTION ( 'NONE',  ( 0.000000000000000000, 0.8496786552930076786, 0.5273008465188218086 ) ) ;
#89565 = ORIENTED_EDGE ( 'NONE', *, *, #79417, .T. ) ;
#89566 = LINE ( 'NONE', #223940, #172992 ) ;
#89567 = ORIENTED_EDGE ( 'NONE', *, *, #171773, .T. ) ;
#89568 = AXIS2_PLACEMENT_3D ( 'NONE', #68731, #208251, #111703 ) ;
#89569 = AXIS2_PLACEMENT_3D ( 'NONE', #197547, #18911, #98405 ) ;
#89570 = CARTESIAN_POINT ( 'NONE',  ( -20.00857864376270001, 9.150000000000002132, -12.34999999999999964 ) ) ;
#89571 = DIRECTION ( 'NONE',  ( 1.000000000000000000, 0.000000000000000000, 0.000000000000000000 ) ) ;
#89573 = VERTEX_POINT ( 'NONE', #29528 ) ;
#89572 = CARTESIAN_POINT ( 'NONE',  ( -16.80891096016330977, 44.11936249622485917, -235.3061528139998586 ) ) ;
#89574 = CARTESIAN_POINT ( 'NONE',  ( 18.52928932188133970, 63.77791826721860957, -209.3173802208384018 ) ) ;
#89575 = CIRCLE ( 'NONE', #251901, 11.79999999999999716 ) ;
#89576 = CIRCLE ( 'NONE', #64479, 0.1000000000000028644 ) ;
#89577 = DIRECTION ( 'NONE',  ( 1.836970198721029441E-16, -0.4721928772777346239, -0.8814952561688430555 ) ) ;
#89578 = DIRECTION ( 'NONE',  ( 1.000000000000000000, 0.000000000000000000, 0.000000000000000000 ) ) ;
#89579 = ORIENTED_EDGE ( 'NONE', *, *, #53249, .T. ) ;
#89580 = CARTESIAN_POINT ( 'NONE',  ( -22.50000000000000000, 11.75000000001115552, -134.0000000000000284 ) ) ;
#89581 = FACE_OUTER_BOUND ( 'NONE', #98521, .T. ) ;
#89582 = ORIENTED_EDGE ( 'NONE', *, *, #131852, .F. ) ;
#89583 = DIRECTION ( 'NONE',  ( 1.000000000000000000, 0.000000000000000000, 0.000000000000000000 ) ) ;
#89584 = ORIENTED_EDGE ( 'NONE', *, *, #62914, .T. ) ;
#89585 = CARTESIAN_POINT ( 'NONE',  ( 15.73863059295127798, 9.351403174152808973, -117.4795304368385018 ) ) ;
#89586 = DIRECTION ( 'NONE',  ( 0.000000000000000000, 0.000000000000000000, -1.000000000000000000 ) ) ;
#89587 = ADVANCED_FACE ( 'NONE', ( #225101 ), #229912, .T. ) ;
#89590 = ORIENTED_EDGE ( 'NONE', *, *, #106181, .T. ) ;
#89589 = VERTEX_POINT ( 'NONE', #6067 ) ;
#89588 = DIRECTION ( 'NONE',  ( 0.000000000000000000, -0.9651348961777157509, 0.2617529984165031243 ) ) ;
#89591 = VECTOR ( 'NONE', #184127, 1000.000000000000000 ) ;
#89592 = EDGE_CURVE ( 'NONE', #123054, #170816, #8649, .T. ) ;
#89593 = CARTESIAN_POINT ( 'NONE',  ( -33.72168855820452649, 11.47316190337362940, -124.7500000000000426 ) ) ;
#89594 = ADVANCED_FACE ( 'NONE', ( #64764 ), #68630, .F. ) ;
#89595 = CARTESIAN_POINT ( 'NONE',  ( -21.05000000000000071, 1.835341550235567887, -112.0551512925630249 ) ) ;
#89596 = VECTOR ( 'NONE', #150815, 1000.000000000000000 ) ;
#89597 = DIRECTION ( 'NONE',  ( 0.000000000000000000, -5.551115123125777653E-14, 1.000000000000000000 ) ) ;
#89599 = CARTESIAN_POINT ( 'NONE',  ( -21.05000000000000071, 1.115600667400684642E-11, -67.00000000000004263 ) ) ;
#89598 = CARTESIAN_POINT ( 'NONE',  ( 22.46250603428203618, 0.02114417614996233138, -88.85013690265994057 ) ) ;
#89600 = CARTESIAN_POINT ( 'NONE',  ( -21.14999999999994174, 77.83551161375991967, -47.52760213295649550 ) ) ;
#89601 = CIRCLE ( 'NONE', #27109, 2.000000000000001776 ) ;
#89602 = CARTESIAN_POINT ( 'NONE',  ( -20.64999999999999858, 47.74660456829661825, -241.9541913331436263 ) ) ;
#89603 = DIRECTION ( 'NONE',  ( 1.000000000000000000, -1.207181226542539700E-16, 2.694675058168174199E-16 ) ) ;
#89604 = CARTESIAN_POINT ( 'NONE',  ( -22.49436431346200038, 11.64995094766461392, -33.43309647027773934 ) ) ;
#89605 = ORIENTED_EDGE ( 'NONE', *, *, #161349, .T. ) ;
#89607 = ORIENTED_EDGE ( 'NONE', *, *, #117958, .F. ) ;
#89606 = VECTOR ( 'NONE', #212740, 1000.000000000000000 ) ;
#89608 = DIRECTION ( 'NONE',  ( 0.000000000000000000, -0.9550021345545507412, 0.2965989261549202283 ) ) ;
#89609 = CIRCLE ( 'NONE', #235363, 0.1000000000000124678 ) ;
#89611 = VERTEX_POINT ( 'NONE', #184709 ) ;
#89610 = DIRECTION ( 'NONE',  ( 0.000000000000000000, 1.000000000000000000, 6.982962677686267499E-15 ) ) ;
#89612 = ORIENTED_EDGE ( 'NONE', *, *, #86466, .F. ) ;
#89613 = EDGE_CURVE ( 'NONE', #122037, #115921, #205547, .T. ) ;
#89614 = CARTESIAN_POINT ( 'NONE',  ( 21.13736287352038445, 8.046642376383999817, -12.65000000000000568 ) ) ;
#89615 = ORIENTED_EDGE ( 'NONE', *, *, #243585, .F. ) ;
#89616 = CARTESIAN_POINT ( 'NONE',  ( 21.05000000000000071, 0.000000000000000000, 0.000000000000000000 ) ) ;
#89617 = AXIS2_PLACEMENT_3D ( 'NONE', #211561, #112468, #129449 ) ;
#89618 = EDGE_LOOP ( 'NONE', ( #148182, #68714, #206449, #78546 ) ) ;
#89619 = CIRCLE ( 'NONE', #222901, 0.1000000000000030170 ) ;
#89620 = CARTESIAN_POINT ( 'NONE',  ( -18.59999999999999787, -6.696875742858878766, -214.8933205276707099 ) ) ;
#89622 = ORIENTED_EDGE ( 'NONE', *, *, #161503, .F. ) ;
#89621 = VERTEX_POINT ( 'NONE', #85573 ) ;
#89623 = ORIENTED_EDGE ( 'NONE', *, *, #217922, .T. ) ;
#89624 = FACE_OUTER_BOUND ( 'NONE', #146133, .T. ) ;
#89625 = ORIENTED_EDGE ( 'NONE', *, *, #141863, .T. ) ;
#89626 = ORIENTED_EDGE ( 'NONE', *, *, #22937, .T. ) ;
#89627 = CARTESIAN_POINT ( 'NONE',  ( 21.09696443733127325, 43.44010277435545930, -234.7623226765231266 ) ) ;
#89628 = DIRECTION ( 'NONE',  ( 0.000000000000000000, 0.000000000000000000, 1.000000000000000000 ) ) ;
#89629 = VERTEX_POINT ( 'NONE', #49051 ) ;
#89630 = EDGE_CURVE ( 'NONE', #46680, #150422, #26943, .T. ) ;
#89631 = ADVANCED_FACE ( 'NONE', ( #84273 ), #169045, .T. ) ;
#89632 = CONICAL_SURFACE ( 'NONE', #189617, 4.000000000000000000, 0.7853981633974487231 ) ;
#89633 = CARTESIAN_POINT ( 'NONE',  ( 20.94999999999999929, -11.48912529306489994, -197.9999999999999432 ) ) ;
#89634 = SPHERICAL_SURFACE ( 'NONE', #253268, 0.1000000000000000056 ) ;
#89636 = ORIENTED_EDGE ( 'NONE', *, *, #234855, .T. ) ;
#89635 = CARTESIAN_POINT ( 'NONE',  ( -22.50000000000000000, 65.59531831295525706, -241.8872196075891168 ) ) ;
#89637 = CARTESIAN_POINT ( 'NONE',  ( -23.25000000000000000, 0.000000000000000000, 0.000000000000000000 ) ) ;
#89638 = EDGE_LOOP ( 'NONE', ( #218165, #25512, #15897, #216555 ) ) ;
#89639 = CARTESIAN_POINT ( 'NONE',  ( -23.15000000000000213, -11.65000000000000036, -30.39999999999999858 ) ) ;
#89640 = EDGE_LOOP ( 'NONE', ( #65511, #18303, #71059 ) ) ;
#89641 = LINE ( 'NONE', #107935, #130499 ) ;
#89642 = CARTESIAN_POINT ( 'NONE',  ( -16.94878442675511465, 30.25972311995205288, -234.7883080098580990 ) ) ;
#89643 = EDGE_CURVE ( 'NONE', #186334, #73251, #230950, .T. ) ;
#89644 = VERTEX_POINT ( 'NONE', #189853 ) ;
#89646 = DIRECTION ( 'NONE',  ( -1.000000000000000000, -0.000000000000000000, -0.000000000000000000 ) ) ;
#89645 = FACE_BOUND ( 'NONE', #141262, .T. ) ;
#89647 = DIRECTION ( 'NONE',  ( -0.000000000000000000, -0.1298341882519805091, -0.9915357197604881545 ) ) ;
#89648 = CARTESIAN_POINT ( 'NONE',  ( -20.94999999999999929, 1.115650877919449575E-11, -71.09999999999999432 ) ) ;
#89649 = AXIS2_PLACEMENT_3D ( 'NONE', #5758, #61910, #180575 ) ;
#89650 = CARTESIAN_POINT ( 'NONE',  ( 21.14999999999998082, 1.580567032079710055, -244.0902705724231794 ) ) ;
#89651 = ORIENTED_EDGE ( 'NONE', *, *, #127357, .F. ) ;
#89652 = ORIENTED_EDGE ( 'NONE', *, *, #97280, .T. ) ;
#89653 = CARTESIAN_POINT ( 'NONE',  ( 21.14999999999999858, 70.41157348381892689, -224.1287375179191201 ) ) ;
#89654 = ORIENTED_EDGE ( 'NONE', *, *, #158322, .T. ) ;
#89655 = CARTESIAN_POINT ( 'NONE',  ( -22.59999999999999787, 55.86495732666938352, -232.8769840133977880 ) ) ;
#89656 = ORIENTED_EDGE ( 'NONE', *, *, #231633, .F. ) ;
#89657 = CARTESIAN_POINT ( 'NONE',  ( 20.94999999999999929, 82.48249193998721296, -215.5326005316167084 ) ) ;
#89658 = LINE ( 'NONE', #169254, #54403 ) ;
#89659 = CARTESIAN_POINT ( 'NONE',  ( -20.99142135623731420, 64.40000000001147384, -42.95131071479990226 ) ) ;
#89660 = ADVANCED_FACE ( 'NONE', ( #163883 ), #243402, .F. ) ;
#89661 = ORIENTED_EDGE ( 'NONE', *, *, #191434, .F. ) ;
#89662 = CARTESIAN_POINT ( 'NONE',  ( -16.80468759584937644, 66.05784632487846864, -190.8330886183227335 ) ) ;
#89663 =( NAMED_UNIT ( * ) SI_UNIT ( $, .STERADIAN. ) SOLID_ANGLE_UNIT ( ) );
#89664 = AXIS2_PLACEMENT_3D ( 'NONE', #111476, #188435, #89324 ) ;
#89665 = ORIENTED_EDGE ( 'NONE', *, *, #145996, .F. ) ;
#89666 = ORIENTED_EDGE ( 'NONE', *, *, #82411, .F. ) ;
#89667 = ORIENTED_EDGE ( 'NONE', *, *, #160740, .T. ) ;
#89668 = ADVANCED_FACE ( 'NONE', ( #251091 ), #170340, .T. ) ;
#89669 = CYLINDRICAL_SURFACE ( 'NONE', #191801, 0.1000000000000028644 ) ;
#89670 = DIRECTION ( 'NONE',  ( 0.000000000000000000, 1.000000000000000000, -0.000000000000000000 ) ) ;
#89671 = CIRCLE ( 'NONE', #14708, 0.09999999999998898659 ) ;
#89672 = DIRECTION ( 'NONE',  ( 0.000000000000000000, -1.000000000000000000, -6.982962677686265922E-15 ) ) ;
#89673 = CARTESIAN_POINT ( 'NONE',  ( 23.15000000000000213, -11.64999999998883595, -197.8999999999999773 ) ) ;
#89674 = DIRECTION ( 'NONE',  ( 0.000000000000000000, -0.8814952561688476074, 0.4721928772777262417 ) ) ;
#89676 = CARTESIAN_POINT ( 'NONE',  ( 21.10710606213542206, 8.776894023893211383, -12.24099652639942271 ) ) ;
#89675 = FACE_OUTER_BOUND ( 'NONE', #17224, .T. ) ;
#89678 = ORIENTED_EDGE ( 'NONE', *, *, #181020, .F. ) ;
#89677 = DIRECTION ( 'NONE',  ( 1.040834085586049673E-13, 0.7899159663865300551, 0.6132151058540831201 ) ) ;
#89679 = DIRECTION ( 'NONE',  ( 1.000000000000000000, 0.000000000000000000, 0.000000000000000000 ) ) ;
#89680 = ORIENTED_EDGE ( 'NONE', *, *, #102924, .F. ) ;
#89681 = EDGE_CURVE ( 'NONE', #44979, #209410, #80882, .T. ) ;
#89682 = DIRECTION ( 'NONE',  ( 0.000000000000000000, -0.9908441862701596881, 0.1350103645451899148 ) ) ;
#89683 = EDGE_CURVE ( 'NONE', #224804, #204844, #201695, .T. ) ;
#89684 = EDGE_LOOP ( 'NONE', ( #132044, #191975, #249343, #160498 ) ) ;
#89685 = ORIENTED_EDGE ( 'NONE', *, *, #45698, .T. ) ;
#89686 = LINE ( 'NONE', #47999, #407 ) ;
#89687 = DIRECTION ( 'NONE',  ( 1.000000000000000000, 0.000000000000000000, 0.000000000000000000 ) ) ;
#89688 = CARTESIAN_POINT ( 'NONE',  ( -18.59999999999999787, 64.35000000001203091, -114.7731074845243882 ) ) ;
#89689 = DIRECTION ( 'NONE',  ( -1.000000000000000000, 0.000000000000000000, 0.000000000000000000 ) ) ;
#89690 = ADVANCED_FACE ( 'NONE', ( #237655 ), #39421, .T. ) ;
#89691 = VECTOR ( 'NONE', #207137, 1000.000000000000000 ) ;
#89692 = DIRECTION ( 'NONE',  ( 0.000000000000000000, 0.000000000000000000, -1.000000000000000000 ) ) ;
#89693 = ADVANCED_FACE ( 'NONE', ( #112886 ), #92029, .T. ) ;
#89694 = ORIENTED_EDGE ( 'NONE', *, *, #498, .T. ) ;
#89695 = ORIENTED_EDGE ( 'NONE', *, *, #63929, .F. ) ;
#89696 = DIRECTION ( 'NONE',  ( 0.000000000000000000, 0.000000000000000000, -1.000000000000000000 ) ) ;
#89697 = EDGE_LOOP ( 'NONE', ( #6087, #64607, #51070, #213244 ) ) ;
#89698 = DIRECTION ( 'NONE',  ( 0.000000000000000000, -0.8814952561688438326, 0.4721928772777330696 ) ) ;
#89699 = CYLINDRICAL_SURFACE ( 'NONE', #156903, 0.5000000000000009992 ) ;
#89700 = EDGE_LOOP ( 'NONE', ( #205658, #59463, #28490, #189971 ) ) ;
#89701 = DIRECTION ( 'NONE',  ( 0.000000000000000000, -1.000000000000000000, 0.000000000000000000 ) ) ;
#89703 = EDGE_CURVE ( 'NONE', #147060, #73870, #131157, .T. ) ;
#89702 = CARTESIAN_POINT ( 'NONE',  ( -23.25000000000000000, 7.021664781900089913, -37.33356540189728889 ) ) ;
#89704 = LINE ( 'NONE', #10199, #15519 ) ;
#89705 = DIRECTION ( 'NONE',  ( 1.000000000000000000, -0.000000000000000000, 0.000000000000000000 ) ) ;
#89706 = VERTEX_POINT ( 'NONE', #179002 ) ;
#89707 = CARTESIAN_POINT ( 'NONE',  ( 22.39999999999999503, 76.00000000001219291, -144.3138870828976792 ) ) ;
#89708 = DIRECTION ( 'NONE',  ( 0.000000000000000000, 0.000000000000000000, 1.000000000000000000 ) ) ;
#89709 = CYLINDRICAL_SURFACE ( 'NONE', #170931, 0.1000000000000028644 ) ;
#89710 = ADVANCED_FACE ( 'NONE', ( #150730 ), #180863, .T. ) ;
#89711 = CARTESIAN_POINT ( 'NONE',  ( 22.50000000000000000, 76.00000000001267608, -203.5231074845243597 ) ) ;
#89712 = VECTOR ( 'NONE', #205353, 1000.000000000000000 ) ;
#89713 = CARTESIAN_POINT ( 'NONE',  ( 18.46905048506371116, 77.19704573657351432, -241.7715467033954440 ) ) ;
#89714 = AXIS2_PLACEMENT_3D ( 'NONE', #49114, #111662, #247313 ) ;
#89715 = EDGE_CURVE ( 'NONE', #232170, #14704, #130965, .T. ) ;
#89716 = ADVANCED_FACE ( 'NONE', ( #210698 ), #78566, .T. ) ;
#89717 = AXIS2_PLACEMENT_3D ( 'NONE', #155516, #254545, #5040 ) ;
#89718 = AXIS2_PLACEMENT_3D ( 'NONE', #178800, #198314, #237448 ) ;
#89719 = ORIENTED_EDGE ( 'NONE', *, *, #41460, .T. ) ;
#89720 = STYLED_ITEM ( 'NONE', ( #79075 ), #144531 ) ;
#89721 = EDGE_CURVE ( 'NONE', #148820, #110439, #185138, .T. ) ;
#89722 = VERTEX_POINT ( 'NONE', #32088 ) ;
#89723 = FACE_OUTER_BOUND ( 'NONE', #69472, .T. ) ;
#89724 = EDGE_CURVE ( 'NONE', #46709, #182231, #89255, .T. ) ;
#89725 = DIRECTION ( 'NONE',  ( -0.000000000000000000, 0.2617529984165031243, 0.9651348961777157509 ) ) ;
#89726 = DIRECTION ( 'NONE',  ( 0.000000000000000000, 0.1350103645451974088, -0.9908441862701587999 ) ) ;
#89727 = CARTESIAN_POINT ( 'NONE',  ( 20.74625933824083290, 67.11708647892803015, -161.4679364604013188 ) ) ;
#89728 = EDGE_CURVE ( 'NONE', #136766, #96347, #105992, .T. ) ;
#89729 = ORIENTED_EDGE ( 'NONE', *, *, #254472, .T. ) ;
#89730 = CARTESIAN_POINT ( 'NONE',  ( 20.27550659511088682, 9.216043722520002035, -146.6500000000000341 ) ) ;
#89732 = EDGE_CURVE ( 'NONE', #28264, #41050, #251768, .T. ) ;
#89731 = CARTESIAN_POINT ( 'NONE',  ( -20.54999999999999716, 71.65000000001253966, -182.2731074845243882 ) ) ;
#89733 = DIRECTION ( 'NONE',  ( 0.000000000000000000, 0.2128009952263613391, -0.9770955615653312831 ) ) ;
#89734 = CIRCLE ( 'NONE', #235473, 0.1000000000000055705 ) ;
#89735 = CARTESIAN_POINT ( 'NONE',  ( -20.94999999999999929, -0.2561057920922211739, 0.03489644167229202787 ) ) ;
#89736 = AXIS2_PLACEMENT_3D ( 'NONE', #174588, #59686, #137947 ) ;
#89737 = ORIENTED_EDGE ( 'NONE', *, *, #164334, .T. ) ;
#89738 = VERTEX_POINT ( 'NONE', #111604 ) ;
#89739 = CARTESIAN_POINT ( 'NONE',  ( -21.00000000000000000, 6.356682116888462630, 11.91686199900910381 ) ) ;
#89740 = LINE ( 'NONE', #49344, #230895 ) ;
#89741 = CARTESIAN_POINT ( 'NONE',  ( 22.59080734064468032, 11.75000000001115552, -33.46925029190293088 ) ) ;
#89742 = AXIS2_PLACEMENT_3D ( 'NONE', #109685, #169718, #249221 ) ;
#89743 = ADVANCED_FACE ( 'NONE', ( #191161 ), #239298, .F. ) ;
#89744 =( BOUNDED_CURVE ( )  B_SPLINE_CURVE ( 3, ( #204617, #166829, #44289, #145930 ),
 .UNSPECIFIED., .F., .F. ) 
 B_SPLINE_CURVE_WITH_KNOTS ( ( 4, 4 ),
 ( 3.752122642744643688, 4.712388980384671910 ),
 .UNSPECIFIED. ) 
 CURVE ( )  GEOMETRIC_REPRESENTATION_ITEM ( )  RATIONAL_B_SPLINE_CURVE ( ( 1.000000000000000000, 0.9246222802177312960, 0.9246222802177312960, 1.000000000000000000 ) ) 
 REPRESENTATION_ITEM ( '' )  );
#89745 = ORIENTED_EDGE ( 'NONE', *, *, #120084, .T. ) ;
#89746 = CARTESIAN_POINT ( 'NONE',  ( 22.49999999999999645, 11.64987090377453605, -33.41748010912699129 ) ) ;
#89747 = AXIS2_PLACEMENT_3D ( 'NONE', #117418, #58698, #157872 ) ;
#89748 = ITEM_DEFINED_TRANSFORMATION ( 'NONE', 'NONE', #227636,  #2425 ) ;
#89749 = CIRCLE ( 'NONE', #102194, 7.900000000000003908 ) ;
#89750 = LINE ( 'NONE', #70233, #67550 ) ;
#89751 = ORIENTED_EDGE ( 'NONE', *, *, #139178, .T. ) ;
#89752 = DIRECTION ( 'NONE',  ( 0.000000000000000000, 0.000000000000000000, 1.000000000000000000 ) ) ;
#89753 = AXIS2_PLACEMENT_3D ( 'NONE', #57821, #237765, #173990 ) ;
#89754 = ORIENTED_EDGE ( 'NONE', *, *, #10705, .F. ) ;
#89756 = VERTEX_POINT ( 'NONE', #11223 ) ;
#89755 = AXIS2_PLACEMENT_3D ( 'NONE', #102075, #236472, #237760 ) ;
#89757 = ORIENTED_EDGE ( 'NONE', *, *, #128335, .T. ) ;
#89758 = CIRCLE ( 'NONE', #235508, 0.1000000000000000056 ) ;
#89759 = CARTESIAN_POINT ( 'NONE',  ( -20.65000000000000568, 9.957490673325212427, -220.1701168356097469 ) ) ;
#89760 = CARTESIAN_POINT ( 'NONE',  ( 18.49999999999999645, 77.36242903720570041, -162.1342262366031548 ) ) ;
#89761 = AXIS2_PLACEMENT_3D ( 'NONE', #161071, #61966, #141489 ) ;
#89762 = DIRECTION ( 'NONE',  ( 0.000000000000000000, -1.000000000000000000, 0.000000000000000000 ) ) ;
#89763 = CARTESIAN_POINT ( 'NONE',  ( -21.05000000000000071, 74.16465844978819177, -191.9679561919613775 ) ) ;
#89764 = LINE ( 'NONE', #96178, #149487 ) ;
#89765 = CARTESIAN_POINT ( 'NONE',  ( -16.93583594267724379, 10.00862343505220053, -12.55939083932076272 ) ) ;
#89767 = CARTESIAN_POINT ( 'NONE',  ( 21.72449340488910252, 10.28395627749112151, -12.65000000000000568 ) ) ;
#89766 = DIRECTION ( 'NONE',  ( 1.000000000000000000, 0.000000000000000000, 0.000000000000000000 ) ) ;
#89768 = ADVANCED_FACE ( 'NONE', ( #71208 ), #235032, .F. ) ;
#89769 = CARTESIAN_POINT ( 'NONE',  ( 21.14999999999999858, 20.97908333644147660, -233.6079013178409411 ) ) ;
#89770 = FACE_OUTER_BOUND ( 'NONE', #85053, .T. ) ;
#89771 = DIRECTION ( 'NONE',  ( -1.000000000000000000, -0.000000000000000000, -0.000000000000000000 ) ) ;
#89772 = DIRECTION ( 'NONE',  ( 1.000000000000000000, 0.000000000000000000, 0.000000000000000000 ) ) ;
#89773 = ORIENTED_EDGE ( 'NONE', *, *, #154758, .T. ) ;
#89774 = EDGE_CURVE ( 'NONE', #197213, #225207, #93552, .T. ) ;
#89775 = ORIENTED_EDGE ( 'NONE', *, *, #238215, .T. ) ;
#89776 = CARTESIAN_POINT ( 'NONE',  ( -18.40000000000000213, -9.500000000000007105, -40.42214984933044519 ) ) ;
#89777 = DIRECTION ( 'NONE',  ( -0.000000000000000000, 1.000000000000000000, -0.000000000000000000 ) ) ;
#89779 = CARTESIAN_POINT ( 'NONE',  ( -23.25000000000000355, 11.69051004343035771, -207.9207640419785719 ) ) ;
#89778 = PLANE ( 'NONE',  #121454 ) ;
#89780 =( BOUNDED_CURVE ( )  B_SPLINE_CURVE ( 3, ( #76802, #212486, #113372, #135479 ),
 .UNSPECIFIED., .F., .T. ) 
 B_SPLINE_CURVE_WITH_KNOTS ( ( 4, 4 ),
 ( 0.06456096931748350753, 3.077031684272309775 ),
 .UNSPECIFIED. ) 
 CURVE ( )  GEOMETRIC_REPRESENTATION_ITEM ( )  RATIONAL_B_SPLINE_CURVE ( ( 1.000000000000000000, 0.3763440860215095940, 0.3763440860215095940, 1.000000000000000000 ) ) 
 REPRESENTATION_ITEM ( '' )  );
#89781 = FACE_OUTER_BOUND ( 'NONE', #130266, .T. ) ;
#89782 = DIRECTION ( 'NONE',  ( 1.000000000000000000, 0.000000000000000000, 0.000000000000000000 ) ) ;
#89783 = DIRECTION ( 'NONE',  ( -1.000000000000000000, 0.000000000000000000, -0.000000000000000000 ) ) ;
#89784 = ORIENTED_EDGE ( 'NONE', *, *, #99604, .T. ) ;
#89785 = EDGE_LOOP ( 'NONE', ( #10454, #232298, #32901, #155887 ) ) ;
#89786 = CIRCLE ( 'NONE', #64839, 0.09999999999999609201 ) ;
#89787 = DIRECTION ( 'NONE',  ( 1.000000000000000000, 0.000000000000000000, 0.000000000000000000 ) ) ;
#89788 = ORIENTED_EDGE ( 'NONE', *, *, #6665, .F. ) ;
#89789 = EDGE_CURVE ( 'NONE', #132941, #180362, #14470, .T. ) ;
#89790 = CARTESIAN_POINT ( 'NONE',  ( -18.59999999999999787, -1.164121893230052995, -175.4148480855716059 ) ) ;
#89791 = AXIS2_PLACEMENT_3D ( 'NONE', #132532, #212082, #77663 ) ;
#89792 = B_SPLINE_CURVE_WITH_KNOTS ( 'NONE', 3,
 ( #18123, #36434, #96355, #175945, #196752, #97632, #177229, #38988, #118533, #198034, #59787, #128454, #208007, #179782, #247094, #62389, #220182, #29390, #218873, #222725, #41564, #9779 ),
 .UNSPECIFIED., .F., .F.,
 ( 4, 3, 3, 3, 3, 3, 3, 4 ),
 ( 0.000000000000000000, 7.307836821087015899E-06, 4.161455748548358328E-05, 7.576591810647013904E-05, 0.0001098090429817646371, 0.0001438003617351047054, 0.0001777914035423499054, 0.0002117966137402968007 ),
 .UNSPECIFIED. ) ;
#89793 = LINE ( 'NONE', #213271, #146632 ) ;
#89794 = ORIENTED_EDGE ( 'NONE', *, *, #98194, .T. ) ;
#89795 = DIRECTION ( 'NONE',  ( 0.000000000000000000, 0.8814952561688476074, -0.4721928772777262417 ) ) ;
#89796 = ORIENTED_EDGE ( 'NONE', *, *, #15470, .F. ) ;
#89798 = AXIS2_PLACEMENT_3D ( 'NONE', #225615, #46985, #126550 ) ;
#89797 = DIRECTION ( 'NONE',  ( 1.000000000000000000, 0.000000000000000000, 0.000000000000000000 ) ) ;
#89800 = AXIS2_PLACEMENT_3D ( 'NONE', #47670, #106357, #65973 ) ;
#89799 = PLANE ( 'NONE',  #20303 ) ;
#89801 = DIRECTION ( 'NONE',  ( 0.000000000000000000, 0.8660254037844420383, -0.4999999999999941713 ) ) ;
#89802 = FACE_OUTER_BOUND ( 'NONE', #208974, .T. ) ;
#89803 = DIRECTION ( 'NONE',  ( -1.073024830501117725E-15, -6.982962677686266711E-15, 1.000000000000000000 ) ) ;
#89804 = CARTESIAN_POINT ( 'NONE',  ( 23.14999999999998437, 64.25000000001195133, -103.0231074845244024 ) ) ;
#89805 = VECTOR ( 'NONE', #115089, 1000.000000000000000 ) ;
#89806 = CARTESIAN_POINT ( 'NONE',  ( -20.00857864376270001, 9.150000000000002132, -12.25000000000000000 ) ) ;
#89807 = CARTESIAN_POINT ( 'NONE',  ( -22.39999999999999858, 67.20509925321675837, -235.9516399960961337 ) ) ;
#89809 = EDGE_LOOP ( 'NONE', ( #152403, #145042, #98489, #214069 ) ) ;
#89808 = CARTESIAN_POINT ( 'NONE',  ( -20.64999999999999858, 85.00000000001149658, -45.41707660717669626 ) ) ;
#89811 = DIRECTION ( 'NONE',  ( 0.000000000000000000, 0.000000000000000000, 1.000000000000000000 ) ) ;
#89810 = DIRECTION ( 'NONE',  ( 0.000000000000000000, -6.938893903907222067E-15, 1.000000000000000000 ) ) ;
#89812 = VERTEX_POINT ( 'NONE', #81124 ) ;
#89814 = ORIENTED_EDGE ( 'NONE', *, *, #54123, .F. ) ;
#89813 = FACE_OUTER_BOUND ( 'NONE', #57784, .T. ) ;
#89815 = ORIENTED_EDGE ( 'NONE', *, *, #142678, .F. ) ;
#89816 = CARTESIAN_POINT ( 'NONE',  ( 20.85000000000000142, 7.128833340094563376, -233.7327013124401276 ) ) ;
#89817 = FACE_OUTER_BOUND ( 'NONE', #191901, .T. ) ;
#89818 = DIRECTION ( 'NONE',  ( 1.000000000000000000, 0.000000000000000000, 0.000000000000000000 ) ) ;
#89819 = LINE ( 'NONE', #110682, #164183 ) ;
#89821 = FACE_OUTER_BOUND ( 'NONE', #197283, .T. ) ;
#89820 = VECTOR ( 'NONE', #113335, 1000.000000000000114 ) ;
#89822 = DIRECTION ( 'NONE',  ( 1.186688945009009831E-16, 1.000000000000000000, 6.982962677686266711E-15 ) ) ;
#89824 = EDGE_CURVE ( 'NONE', #8358, #163693, #20560, .T. ) ;
#89823 = LINE ( 'NONE', #92394, #62968 ) ;
#89825 = CARTESIAN_POINT ( 'NONE',  ( -16.78270389226387138, 51.61191257970394020, -231.9524616731252138 ) ) ;
#89826 = EDGE_CURVE ( 'NONE', #151773, #246470, #14283, .T. ) ;
#89827 = DIRECTION ( 'NONE',  ( 1.000000000000000000, 0.000000000000000000, 0.000000000000000000 ) ) ;
#89828 = ORIENTED_EDGE ( 'NONE', *, *, #208230, .T. ) ;
#89829 = ORIENTED_EDGE ( 'NONE', *, *, #160278, .T. ) ;
#89830 = CARTESIAN_POINT ( 'NONE',  ( -16.89268316805466341, 9.951721813253341153, -180.1442475214544174 ) ) ;
#89831 = CIRCLE ( 'NONE', #140267, 0.1000000000000035444 ) ;
#89832 = AXIS2_PLACEMENT_3D ( 'NONE', #158975, #179807, #79387 ) ;
#89833 = EDGE_LOOP ( 'NONE', ( #15102, #172502, #90429, #241384, #57501 ) ) ;
#89834 = VECTOR ( 'NONE', #129282, 1000.000000000000000 ) ;
#89836 = CARTESIAN_POINT ( 'NONE',  ( -18.50000000000000000, 2.272311100394797556, -217.9150152700588876 ) ) ;
#89835 = AXIS2_PLACEMENT_3D ( 'NONE', #238199, #205160, #126933 ) ;
#89837 = ORIENTED_EDGE ( 'NONE', *, *, #4964, .F. ) ;
#89838 = CARTESIAN_POINT ( 'NONE',  ( 20.85000000000000142, 36.65892442174935439, -249.5511627012433848 ) ) ;
#89839 = ADVANCED_FACE ( 'NONE', ( #25049 ), #185378, .F. ) ;
#89840 = CARTESIAN_POINT ( 'NONE',  ( 20.00000000000000355, 11.75000000000000711, -24.65000000000000213 ) ) ;
#89841 = CARTESIAN_POINT ( 'NONE',  ( -20.64999999999999858, -8.999999999988846255, -143.8939691226524644 ) ) ;
#89842 = DIRECTION ( 'NONE',  ( -1.000000000000000000, -0.000000000000000000, -0.000000000000000000 ) ) ;
#89843 = EDGE_CURVE ( 'NONE', #136089, #186480, #156132, .T. ) ;
#89844 = DIRECTION ( 'NONE',  ( 0.000000000000000000, -0.2128009952263604232, 0.9770955615653316162 ) ) ;
#89845 = ORIENTED_EDGE ( 'NONE', *, *, #94539, .T. ) ;
#89846 = EDGE_CURVE ( 'NONE', #231604, #87043, #1383, .T. ) ;
#89847 = CARTESIAN_POINT ( 'NONE',  ( -21.59142135623730852, 7.850000000011158718, -45.75000000000000000 ) ) ;
#89848 = DIRECTION ( 'NONE',  ( 0.000000000000000000, 6.982962677686266711E-15, -1.000000000000000000 ) ) ;
#89849 = DIRECTION ( 'NONE',  ( 0.7071067811865475727, -0.2890913453342130457, 0.6453109281988448354 ) ) ;
#89850 = EDGE_CURVE ( 'NONE', #90961, #70645, #247085, .T. ) ;
#89851 = LINE ( 'NONE', #172014, #182376 ) ;
#89852 = CARTESIAN_POINT ( 'NONE',  ( 18.49999999999999289, 6.650000000011155876, -155.3500000000000227 ) ) ;
#89853 = VERTEX_POINT ( 'NONE', #124138 ) ;
#89854 = AXIS2_PLACEMENT_3D ( 'NONE', #132017, #192017, #108600 ) ;
#89856 = CARTESIAN_POINT ( 'NONE',  ( -21.14999999999999858, 76.10000000001170406, -75.77310748452431710 ) ) ;
#89855 = FACE_OUTER_BOUND ( 'NONE', #149652, .T. ) ;
#89858 = VERTEX_POINT ( 'NONE', #201088 ) ;
#89857 = B_SPLINE_CURVE_WITH_KNOTS ( 'NONE', 3,
 ( #506, #98300, #240425, #196156, #241707, #97015, #220850, #177898, #57911, #237853, #22686, #60482, #180453, #77465, #120507, #21403, #61786, #17510, #42230 ),
 .UNSPECIFIED., .F., .F.,
 ( 4, 3, 3, 3, 3, 3, 4 ),
 ( 0.000000000000000000, 7.110282409888900811E-05, 0.0001508797727291396576, 0.0002027344179858381486, 0.0002343294522348978305, 0.0002454816334821145599, 0.0002619873080085490967 ),
 .UNSPECIFIED. ) ;
#89861 = ORIENTED_EDGE ( 'NONE', *, *, #138898, .F. ) ;
#89860 = DIRECTION ( 'NONE',  ( 0.000000000000000000, 0.1480365673253017378, -0.9889818879709282307 ) ) ;
#89859 = CARTESIAN_POINT ( 'NONE',  ( -18.59999999999999787, 68.97833521811131163, -32.18954208262707795 ) ) ;
#89862 = DIRECTION ( 'NONE',  ( -1.000000000000000000, -0.000000000000000000, -0.000000000000000000 ) ) ;
#89863 = DIRECTION ( 'NONE',  ( 0.000000000000000000, -1.000000000000000000, 0.000000000000000000 ) ) ;
#89864 = DIRECTION ( 'NONE',  ( 0.000000000000000000, 1.000000000000000000, -6.308085367188393199E-16 ) ) ;
#89865 = AXIS2_PLACEMENT_3D ( 'NONE', #89459, #148158, #206854 ) ;
#89866 = ORIENTED_EDGE ( 'NONE', *, *, #20351, .F. ) ;
#89867 = DIRECTION ( 'NONE',  ( 0.000000000000000000, 0.000000000000000000, 1.000000000000000000 ) ) ;
#89868 = EDGE_CURVE ( 'NONE', #50671, #224268, #104523, .T. ) ;
#89869 = DIRECTION ( 'NONE',  ( 1.000000000000000000, -2.952720810173289112E-16, -2.061873921506763405E-30 ) ) ;
#89871 = CARTESIAN_POINT ( 'NONE',  ( -23.15000000000000213, 74.00000000001259082, -190.2984855617622770 ) ) ;
#89870 = DIRECTION ( 'NONE',  ( 1.000000000000000000, -0.000000000000000000, -0.000000000000000000 ) ) ;
#89873 = VERTEX_POINT ( 'NONE', #23773 ) ;
#89872 = CARTESIAN_POINT ( 'NONE',  ( -18.60000000000001563, 47.04011997029079595, -255.1614879447985800 ) ) ;
#89874 = VERTEX_POINT ( 'NONE', #62860 ) ;
#89875 = CARTESIAN_POINT ( 'NONE',  ( -18.59999999999999787, 11.65000000001115232, -74.01480577065404987 ) ) ;
#89876 = CARTESIAN_POINT ( 'NONE',  ( -20.54999999999999716, -8.730841121495325652, -23.90192528101566793 ) ) ;
#89877 = VECTOR ( 'NONE', #190683, 1000.000000000000000 ) ;
#89878 = AXIS2_PLACEMENT_3D ( 'NONE', #30440, #29187, #209061 ) ;
#89879 = DIRECTION ( 'NONE',  ( 0.000000000000000000, 0.8814952561688437216, -0.4721928772777334582 ) ) ;
#89880 = EDGE_LOOP ( 'NONE', ( #45403, #200934, #242712, #123592 ) ) ;
#89881 = DIRECTION ( 'NONE',  ( -1.000000000000000000, 0.000000000000000000, -0.000000000000000000 ) ) ;
#89882 = DIRECTION ( 'NONE',  ( 1.000000000000000000, 0.000000000000000000, 0.000000000000000000 ) ) ;
#89883 = FACE_OUTER_BOUND ( 'NONE', #165013, .T. ) ;
#89884 = ORIENTED_EDGE ( 'NONE', *, *, #140979, .F. ) ;
#89885 = CARTESIAN_POINT ( 'NONE',  ( 20.75572585718487773, 60.88282358376731196, -225.3291528674897677 ) ) ;
#89886 = ORIENTED_EDGE ( 'NONE', *, *, #199612, .T. ) ;
#89887 = VECTOR ( 'NONE', #210719, 1000.000000000000000 ) ;
#89888 = CARTESIAN_POINT ( 'NONE',  ( 18.59999999999999787, -1.851028230140860487, -11.65391326942249250 ) ) ;
#89889 = CARTESIAN_POINT ( 'NONE',  ( -18.50000000000000000, 7.128833340093095217, -233.7327013124392749 ) ) ;
#89890 = AXIS2_PLACEMENT_3D ( 'NONE', #167508, #112648, #132205 ) ;
#89891 = CIRCLE ( 'NONE', #119139, 0.1000000000000028644 ) ;
#89892 = CIRCLE ( 'NONE', #6702, 0.1000000000000024342 ) ;
#89893 = ADVANCED_FACE ( 'NONE', ( #83667 ), #64153, .F. ) ;
#89894 = ORIENTED_EDGE ( 'NONE', *, *, #245017, .F. ) ;
#89895 = VERTEX_POINT ( 'NONE', #61582 ) ;
#89896 = STYLED_ITEM ( 'NONE', ( #18810 ), #225623 ) ;
#89897 = DIRECTION ( 'NONE',  ( 2.259780016855445309E-14, -0.2599159095383298257, 0.9656312546561772736 ) ) ;
#89898 = VERTEX_POINT ( 'NONE', #26315 ) ;
#89900 = ORIENTED_EDGE ( 'NONE', *, *, #169046, .F. ) ;
#89899 = CARTESIAN_POINT ( 'NONE',  ( 22.50046968638039857, 25.91727838046696064, -254.3137924129949567 ) ) ;
#89901 = ADVANCED_FACE ( 'NONE', ( #242772 ), #224499, .F. ) ;
#89902 = VERTEX_POINT ( 'NONE', #21204 ) ;
#89905 = ORIENTED_EDGE ( 'NONE', *, *, #205750, .F. ) ;
#89904 = VERTEX_POINT ( 'NONE', #42036 ) ;
#89903 = CARTESIAN_POINT ( 'NONE',  ( 20.99999999999999645, 9.750000000011137757, -180.1499999999999773 ) ) ;
#89906 = ADVANCED_FACE ( 'NONE', ( #182840 ), #143675, .F. ) ;
#89907 = EDGE_CURVE ( 'NONE', #95398, #26294, #130570, .T. ) ;
#89908 = CARTESIAN_POINT ( 'NONE',  ( -18.59999999999999787, 18.62343931468261360, -223.9512205031617498 ) ) ;
#89909 = VERTEX_POINT ( 'NONE', #2871 ) ;
#89910 = CARTESIAN_POINT ( 'NONE',  ( 21.14999999999999858, -0.09999999998884338825, -67.00000000000004263 ) ) ;
#89911 = DIRECTION ( 'NONE',  ( 0.000000000000000000, 6.938893903907234689E-15, -1.000000000000000000 ) ) ;
#89912 = AXIS2_PLACEMENT_3D ( 'NONE', #118130, #197653, #119425 ) ;
#89913 = CARTESIAN_POINT ( 'NONE',  ( -20.64999999999999858, 74.00000000001199396, -116.2477294072864140 ) ) ;
#89914 =( GEOMETRIC_REPRESENTATION_CONTEXT ( 3 ) GLOBAL_UNCERTAINTY_ASSIGNED_CONTEXT ( ( #34688 ) ) GLOBAL_UNIT_ASSIGNED_CONTEXT ( ( #476, #22655, #159578 ) ) REPRESENTATION_CONTEXT ( 'NONE', 'WORKASPACE' ) );
#89915 = CARTESIAN_POINT ( 'NONE',  ( -17.71734398241073905, 65.15764277154701745, -59.24824573752999157 ) ) ;
#89916 = AXIS2_PLACEMENT_3D ( 'NONE', #86943, #70006, #149545 ) ;
#89917 = ORIENTED_EDGE ( 'NONE', *, *, #27266, .T. ) ;
#89918 = ORIENTED_EDGE ( 'NONE', *, *, #38795, .F. ) ;
#89919 = CARTESIAN_POINT ( 'NONE',  ( -21.59142135623730852, 68.15000000001199965, -115.2731074845243455 ) ) ;
#89921 = ORIENTED_EDGE ( 'NONE', *, *, #233725, .F. ) ;
#89920 = CARTESIAN_POINT ( 'NONE',  ( 18.49999999999999289, 63.79085327820362039, -209.3815830819284827 ) ) ;
#89922 = CARTESIAN_POINT ( 'NONE',  ( -20.94999999999999929, 1.162701749938009677, -8.099999999999999645 ) ) ;
#89924 = ORIENTED_EDGE ( 'NONE', *, *, #3429, .T. ) ;
#89923 = CYLINDRICAL_SURFACE ( 'NONE', #210705, 0.09999999999999939493 ) ;
#89925 = ADVANCED_FACE ( 'NONE', ( #161991 ), #134660, .T. ) ;
#89926 = ORIENTED_EDGE ( 'NONE', *, *, #151323, .T. ) ;
#89927 = CARTESIAN_POINT ( 'NONE',  ( -20.54999999999999716, 2.500000000011154633, -53.77537807723790309 ) ) ;
#89928 = CIRCLE ( 'NONE', #164944, 0.09999999999999982514 ) ;
#89929 = EDGE_CURVE ( 'NONE', #11679, #66389, #101297, .T. ) ;
#89930 = AXIS2_PLACEMENT_3D ( 'NONE', #194222, #35161, #3342 ) ;
#89932 = VERTEX_POINT ( 'NONE', #70599 ) ;
#89931 = PRODUCT_RELATED_PRODUCT_CATEGORY ( 'part', '', ( #205405 ) ) ;
#89933 = LINE ( 'NONE', #208629, #256083 ) ;
#89934 = CARTESIAN_POINT ( 'NONE',  ( 21.05000000000000071, 19.09887790564731702, -232.6007267402957837 ) ) ;
#89936 = VERTEX_POINT ( 'NONE', #211370 ) ;
#89935 = VERTEX_POINT ( 'NONE', #8039 ) ;
#89937 = ORIENTED_EDGE ( 'NONE', *, *, #35904, .T. ) ;
#89938 = CARTESIAN_POINT ( 'NONE',  ( -18.35663730107557257, 13.17951322611091491, -207.5964750249841302 ) ) ;
#89939 = EDGE_LOOP ( 'NONE', ( #137729, #154297, #140017, #93819 ) ) ;
#89940 = AXIS2_PLACEMENT_3D ( 'NONE', #163224, #107080, #184053 ) ;
#89941 = EDGE_LOOP ( 'NONE', ( #47183, #76330, #38918, #161671 ) ) ;
#89942 = EDGE_CURVE ( 'NONE', #57410, #45783, #91421, .T. ) ;
#89943 = DIRECTION ( 'NONE',  ( 1.000000000000000000, 0.000000000000000000, -0.000000000000000000 ) ) ;
#89945 = ORIENTED_EDGE ( 'NONE', *, *, #40273, .F. ) ;
#89944 = FACE_OUTER_BOUND ( 'NONE', #78132, .T. ) ;
#89946 = EDGE_CURVE ( 'NONE', #39697, #175208, #101899, .T. ) ;
#89947 = DIRECTION ( 'NONE',  ( 1.000000000000000000, -0.000000000000000000, -0.000000000000000000 ) ) ;
#89948 = EDGE_CURVE ( 'NONE', #210671, #138899, #97209, .T. ) ;
#89949 = AXIS2_PLACEMENT_3D ( 'NONE', #186346, #89783, #147203 ) ;
#89950 = AXIS2_PLACEMENT_3D ( 'NONE', #153947, #35273, #155214 ) ;
#89952 = CARTESIAN_POINT ( 'NONE',  ( 20.95512820512820085, 11.26905698129511357, -211.0318809171001249 ) ) ;
#89951 = DIRECTION ( 'NONE',  ( -2.827886303505249259E-16, 0.8660254037844412611, 0.4999999999999956701 ) ) ;
#89953 = CARTESIAN_POINT ( 'NONE',  ( 21.05000000000000071, -11.48912529306489994, -130.9000000000000341 ) ) ;
#89954 = CARTESIAN_POINT ( 'NONE',  ( -20.64999999999999858, 2.400000000011155432, -120.7753780772379315 ) ) ;
#89955 = ORIENTED_EDGE ( 'NONE', *, *, #81258, .F. ) ;
#89956 = VERTEX_POINT ( 'NONE', #126690 ) ;
#89957 = DIRECTION ( 'NONE',  ( 0.000000000000000000, 0.000000000000000000, 1.000000000000000000 ) ) ;
#89958 = CARTESIAN_POINT ( 'NONE',  ( 20.94999999999999929, 1.115600667400684642E-11, -100.5000000000000426 ) ) ;
#89959 = ORIENTED_EDGE ( 'NONE', *, *, #248886, .T. ) ;
#89960 = CARTESIAN_POINT ( 'NONE',  ( 20.94999999999999574, 8.926614585087095932, -8.471683019223121391 ) ) ;
#89961 = VERTEX_POINT ( 'NONE', #52263 ) ;
#89962 = EDGE_LOOP ( 'NONE', ( #28096, #225867, #31093, #215154 ) ) ;
#89963 = CARTESIAN_POINT ( 'NONE',  ( 23.14999999999999858, 87.75000000001222134, -148.2731074845242176 ) ) ;
#89964 = DIRECTION ( 'NONE',  ( -1.000000000000000000, 0.000000000000000000, 0.000000000000000000 ) ) ;
#89965 = EDGE_LOOP ( 'NONE', ( #52367, #190635, #166290, #15792 ) ) ;
#89966 = CARTESIAN_POINT ( 'NONE',  ( -20.00857864376270001, 66.75000000001199396, -115.3731074845243683 ) ) ;
#89967 = ORIENTED_EDGE ( 'NONE', *, *, #95491, .F. ) ;
#89968 = CARTESIAN_POINT ( 'NONE',  ( -21.05000000000000071, 6.258316057343176197, -100.4342983896779344 ) ) ;
#89969 = DIRECTION ( 'NONE',  ( -1.000000000000000000, 0.000000000000000000, -0.000000000000000000 ) ) ;
#89971 = DIRECTION ( 'NONE',  ( 1.000000000000000000, 0.000000000000000000, 0.000000000000000000 ) ) ;
#89970 = DIRECTION ( 'NONE',  ( -0.000000000000000000, -0.8814952561688430555, 0.4721928772777346239 ) ) ;
#89972 = FACE_OUTER_BOUND ( 'NONE', #140282, .T. ) ;
#89973 = AXIS2_PLACEMENT_3D ( 'NONE', #202119, #242519, #226806 ) ;
#89974 = DIRECTION ( 'NONE',  ( -1.000000000000000000, -0.000000000000000000, 0.000000000000000000 ) ) ;
#89975 = DIRECTION ( 'NONE',  ( 2.952720810173289112E-16, 1.000000000000000000, 6.308085367188367561E-15 ) ) ;
#89976 = CIRCLE ( 'NONE', #235717, 0.1999999999999987899 ) ;
#89977 = EDGE_CURVE ( 'NONE', #68680, #179358, #209699, .T. ) ;
#89978 = LINE ( 'NONE', #151265, #216102 ) ;
#89979 = AXIS2_PLACEMENT_3D ( 'NONE', #46674, #190060, #29733 ) ;
#89980 = CIRCLE ( 'NONE', #69174, 0.1000000000000075273 ) ;
#89982 = ORIENTED_EDGE ( 'NONE', *, *, #95562, .T. ) ;
#89981 = CARTESIAN_POINT ( 'NONE',  ( 20.94999999999999574, 1.115600667400684642E-11, -67.00000000000004263 ) ) ;
#89983 = AXIS2_PLACEMENT_3D ( 'NONE', #72622, #107868, #67459 ) ;
#89985 = EDGE_LOOP ( 'NONE', ( #132684, #149900, #52619, #98049 ) ) ;
#89984 = VERTEX_POINT ( 'NONE', #71866 ) ;
#89986 = VERTEX_POINT ( 'NONE', #230949 ) ;
#89987 = ADVANCED_FACE ( 'NONE', ( #148834 ), #30178, .T. ) ;
#89988 = DIRECTION ( 'NONE',  ( 0.000000000000000000, 7.086529944415886769E-15, -1.000000000000000000 ) ) ;
#89989 = DIRECTION ( 'NONE',  ( 1.000000000000000000, 0.000000000000000000, 0.000000000000000000 ) ) ;
#89990 = CIRCLE ( 'NONE', #235729, 0.1000000000000055844 ) ;
#89992 = DIRECTION ( 'NONE',  ( 0.000000000000000000, -0.2617529984165067880, -0.9651348961777146407 ) ) ;
#89991 = LINE ( 'NONE', #172154, #78554 ) ;
#89993 = CARTESIAN_POINT ( 'NONE',  ( -22.39999999999999858, 76.00000000001169553, -75.77310748452431710 ) ) ;
#89994 = EDGE_LOOP ( 'NONE', ( #76197, #199857, #178080, #191702 ) ) ;
#89995 = EDGE_CURVE ( 'NONE', #44654, #75742, #227061, .T. ) ;
#89996 = CARTESIAN_POINT ( 'NONE',  ( -22.59999999999999787, 11.74956712350054566, -100.3991416309013260 ) ) ;
#89997 = ORIENTED_EDGE ( 'NONE', *, *, #98701, .F. ) ;
#89998 = AXIS2_PLACEMENT_3D ( 'NONE', #9562, #249478, #185643 ) ;
#89999 = CARTESIAN_POINT ( 'NONE',  ( -22.49917693094574389, 0.08522996423282762357, -88.85020421546937541 ) ) ;
#90000 = EDGE_CURVE ( 'NONE', #213681, #185072, #10369, .T. ) ;
#90001 = CARTESIAN_POINT ( 'NONE',  ( 22.39999999999999858, 68.20922040163875977, -136.6231074845243540 ) ) ;
#90002 = ORIENTED_EDGE ( 'NONE', *, *, #196554, .T. ) ;
#90003 = DIRECTION ( 'NONE',  ( 0.000000000000000000, 0.2617529984165152257, 0.9651348961777124202 ) ) ;
#90004 = EDGE_CURVE ( 'NONE', #41107, #130397, #201307, .T. ) ;
#90005 = DIRECTION ( 'NONE',  ( 0.000000000000000000, -6.853228547068871147E-15, 1.000000000000000000 ) ) ;
#90006 = EDGE_CURVE ( 'NONE', #44033, #85055, #56113, .T. ) ;
#90007 = EDGE_LOOP ( 'NONE', ( #108939, #214679, #179115, #112909 ) ) ;
#90008 = ORIENTED_EDGE ( 'NONE', *, *, #135401, .F. ) ;
#90009 = CARTESIAN_POINT ( 'NONE',  ( 19.97071067811865319, 64.27928932189311695, -78.31452884076171017 ) ) ;
#90010 = FACE_OUTER_BOUND ( 'NONE', #119202, .T. ) ;
#90011 = CIRCLE ( 'NONE', #173280, 1.749999999999998002 ) ;
#90012 = DIRECTION ( 'NONE',  ( 0.000000000000000000, 0.000000000000000000, -1.000000000000000000 ) ) ;
#90013 = DIRECTION ( 'NONE',  ( 0.000000000000000000, 0.000000000000000000, -1.000000000000000000 ) ) ;
#90014 = CARTESIAN_POINT ( 'NONE',  ( -20.54999999999999716, -11.74999999998884448, -184.2499999999999716 ) ) ;
#90015 = ORIENTED_EDGE ( 'NONE', *, *, #256879, .F. ) ;
#90016 = DIRECTION ( 'NONE',  ( 1.000000000000000000, 2.885090398161910739E-16, 6.283419270304611573E-17 ) ) ;
#90017 = LINE ( 'NONE', #108316, #241608 ) ;
#90019 = CARTESIAN_POINT ( 'NONE',  ( -21.00219873199047171, 11.60538868788763089, -174.4126474282949744 ) ) ;
#90018 = DIRECTION ( 'NONE',  ( 3.616040088954490704E-32, 7.105427357601001859E-15, -1.000000000000000000 ) ) ;
#90020 = CARTESIAN_POINT ( 'NONE',  ( -18.50000000000000000, 68.68284540823283635, -224.2482512540334767 ) ) ;
#90021 = B_SPLINE_CURVE_WITH_KNOTS ( 'NONE', 3,
 ( #50242, #32007, #47673, #90658 ),
 .UNSPECIFIED., .F., .F.,
 ( 4, 4 ),
 ( 0.000000000000000000, 0.001767853679387121216 ),
 .UNSPECIFIED. ) ;
#90022 = DIRECTION ( 'NONE',  ( 1.000000000000000000, 0.000000000000000000, 0.000000000000000000 ) ) ;
#90023 = CARTESIAN_POINT ( 'NONE',  ( 20.10000000000000853, 4.645987002755569861, 21.91686199900910736 ) ) ;
#90024 = CARTESIAN_POINT ( 'NONE',  ( 20.84999999999998721, 10.33248238083634440, -139.5948465439131780 ) ) ;
#90025 = AXIS2_PLACEMENT_3D ( 'NONE', #16912, #63383, #140355 ) ;
#90027 = ORIENTED_EDGE ( 'NONE', *, *, #45469, .F. ) ;
#90026 = DIRECTION ( 'NONE',  ( 0.000000000000000000, 0.7397890806274222131, 0.6728388485993012091 ) ) ;
#90028 = EDGE_CURVE ( 'NONE', #172105, #138363, #193522, .T. ) ;
#90029 = AXIS2_PLACEMENT_3D ( 'NONE', #254336, #135676, #95284 ) ;
#90030 = EDGE_CURVE ( 'NONE', #96167, #200257, #11901, .T. ) ;
#90031 = EDGE_CURVE ( 'NONE', #56183, #257629, #43669, .T. ) ;
#90032 = CARTESIAN_POINT ( 'NONE',  ( -21.64999999999999858, 44.38078384682074784, -235.8464960865713067 ) ) ;
#90033 = EDGE_CURVE ( 'NONE', #215553, #177416, #22842, .T. ) ;
#90034 = AXIS2_PLACEMENT_3D ( 'NONE', #212568, #14381, #247827 ) ;
#90035 = EDGE_CURVE ( 'NONE', #217909, #70167, #197221, .T. ) ;
#90036 = DIRECTION ( 'NONE',  ( -1.000000000000000000, -7.304098846218133681E-16, 4.217023435051677994E-16 ) ) ;
#90037 = AXIS2_PLACEMENT_3D ( 'NONE', #79724, #78453, #158055 ) ;
#90038 = ORIENTED_EDGE ( 'NONE', *, *, #242805, .F. ) ;
#90039 = CARTESIAN_POINT ( 'NONE',  ( -18.40000000000000213, 64.52683809665003878, -179.2731074845244450 ) ) ;
#90040 = LINE ( 'NONE', #169641, #41222 ) ;
#90041 = CARTESIAN_POINT ( 'NONE',  ( 21.05000000000000071, 1.115600667400684642E-11, -138.1000000000000227 ) ) ;
#90042 = EDGE_CURVE ( 'NONE', #159998, #43292, #189418, .T. ) ;
#90043 = AXIS2_PLACEMENT_3D ( 'NONE', #180574, #138830, #158468 ) ;
#90044 = ORIENTED_EDGE ( 'NONE', *, *, #59317, .T. ) ;
#90045 = CARTESIAN_POINT ( 'NONE',  ( -16.88495309932520883, 12.41526644790654288, -211.2268068864140105 ) ) ;
#90047 = ORIENTED_EDGE ( 'NONE', *, *, #53040, .T. ) ;
#90046 = DIRECTION ( 'NONE',  ( 0.000000000000000000, 0.000000000000000000, 1.000000000000000000 ) ) ;
#90048 = DIRECTION ( 'NONE',  ( -0.000000000000000000, -0.4721928772777346239, -0.8814952561688430555 ) ) ;
#90049 = CARTESIAN_POINT ( 'NONE',  ( -20.64999999999999858, 74.00000000001199396, -116.2477294072864140 ) ) ;
#90050 = EDGE_LOOP ( 'NONE', ( #214258, #17163, #148030, #139161 ) ) ;
#90051 = CARTESIAN_POINT ( 'NONE',  ( -16.96982749440708815, 66.05000000001261640, -190.3983290757135194 ) ) ;
#90052 = EDGE_CURVE ( 'NONE', #45320, #139155, #69299, .T. ) ;
#90053 = PRODUCT_CONTEXT ( 'NONE', #43997, 'mechanical' ) ;
#90054 = DIRECTION ( 'NONE',  ( 0.000000000000000000, 0.2128009952263603677, -0.9770955615653313941 ) ) ;
#90055 = DIRECTION ( 'NONE',  ( -1.000000000000000000, 0.000000000000000000, 0.000000000000000000 ) ) ;
#90056 = CARTESIAN_POINT ( 'NONE',  ( -18.40000000000000213, 85.51932773110434027, -96.05013110796491560 ) ) ;
#90057 = VERTEX_POINT ( 'NONE', #254314 ) ;
#90058 = DIRECTION ( 'NONE',  ( 0.000000000000000000, 7.056502275159890832E-15, -1.000000000000000000 ) ) ;
#90059 = LINE ( 'NONE', #69246, #129931 ) ;
#90060 = AXIS2_PLACEMENT_3D ( 'NONE', #21028, #114965, #15896 ) ;
#90061 = DIRECTION ( 'NONE',  ( 1.000000000000000000, 0.000000000000000000, 0.000000000000000000 ) ) ;
#90062 = ORIENTED_EDGE ( 'NONE', *, *, #167827, .T. ) ;
#90063 = VERTEX_POINT ( 'NONE', #54833 ) ;
#90064 = DIRECTION ( 'NONE',  ( 2.952720810173289112E-16, -1.000000000000000000, 0.000000000000000000 ) ) ;
#90065 = CARTESIAN_POINT ( 'NONE',  ( -20.64999999999999858, 68.85000000001259934, -191.1731074845243938 ) ) ;
#90066 = DIRECTION ( 'NONE',  ( 1.000000000000000000, 0.000000000000000000, 0.000000000000000000 ) ) ;
#90067 = CARTESIAN_POINT ( 'NONE',  ( 20.95512820512820440, 8.876151316299269567, -146.1500000000000341 ) ) ;
#90070 = DIRECTION ( 'NONE',  ( -0.000000000000000000, -6.982962677686266711E-15, 1.000000000000000000 ) ) ;
#90069 = VECTOR ( 'NONE', #236321, 1000.000000000000000 ) ;
#90068 = DIRECTION ( 'NONE',  ( 1.000000000000000000, 0.000000000000000000, 0.000000000000000000 ) ) ;
#90071 = LINE ( 'NONE', #249177, #56729 ) ;
#90072 = FACE_OUTER_BOUND ( 'NONE', #96977, .T. ) ;
#90073 = DIRECTION ( 'NONE',  ( 0.000000000000000000, -1.000000000000000000, 0.000000000000000000 ) ) ;
#90074 = AXIS2_PLACEMENT_3D ( 'NONE', #16338, #73748, #254862 ) ;
#90075 = EDGE_LOOP ( 'NONE', ( #78119, #241498 ) ) ;
#90076 = AXIS2_PLACEMENT_3D ( 'NONE', #115589, #96015, #175584 ) ;
#90077 = EDGE_CURVE ( 'NONE', #247118, #67101, #55524, .T. ) ;
#90079 = ORIENTED_EDGE ( 'NONE', *, *, #316, .F. ) ;
#90078 = CARTESIAN_POINT ( 'NONE',  ( -16.88560720703333473, 12.41418354840153526, -211.2409239182446470 ) ) ;
#90080 = CARTESIAN_POINT ( 'NONE',  ( -17.11825945287481332, 9.950000000011138823, -87.75000000000005684 ) ) ;
#90081 = CARTESIAN_POINT ( 'NONE',  ( 21.05000000000000071, 70.50000000001253397, -182.4283735034374843 ) ) ;
#90083 = CARTESIAN_POINT ( 'NONE',  ( -11.59999999999994458, 67.65000000001118963, -21.02310748452479316 ) ) ;
#90082 = CARTESIAN_POINT ( 'NONE',  ( -21.45000000000000284, 65.32753222054176945, -213.4247798787853867 ) ) ;
#90084 = PRESENTATION_LAYER_ASSIGNMENT (  '', '', ( #127516 ) ) ;
#90085 = ORIENTED_EDGE ( 'NONE', *, *, #40311, .F. ) ;
#90086 = CARTESIAN_POINT ( 'NONE',  ( -17.11825945287482753, 65.95000000001208207, -123.8731074845243683 ) ) ;
#90087 = LINE ( 'NONE', #189213, #233048 ) ;
#90088 = CARTESIAN_POINT ( 'NONE',  ( 18.49999999999999645, -1.135018845899022466, -108.2169768834323662 ) ) ;
#90089 = FACE_OUTER_BOUND ( 'NONE', #32458, .T. ) ;
#90090 = ORIENTED_EDGE ( 'NONE', *, *, #165318, .T. ) ;
#90091 = ORIENTED_EDGE ( 'NONE', *, *, #184433, .T. ) ;
#90092 = CARTESIAN_POINT ( 'NONE',  ( 20.94999999999999929, 1.115600667400684642E-11, -74.80000000000001137 ) ) ;
#90093 = VERTEX_POINT ( 'NONE', #136951 ) ;
#90094 = EDGE_CURVE ( 'NONE', #191176, #209877, #135010, .T. ) ;
#90095 = CARTESIAN_POINT ( 'NONE',  ( -23.25000000000000000, -1.736705739456431807, -212.5174225876236846 ) ) ;
#90096 = TOROIDAL_SURFACE ( 'NONE', #139967, 7.800000000000000711, 0.1000000000000000056 ) ;
#90097 =( BOUNDED_SURFACE ( )  B_SPLINE_SURFACE ( 3, 2, ( 
 ( #163885, #62212, #144277 ),
 ( #201712, #66048, #42639 ),
 ( #204265, #43923, #102581 ),
 ( #123466, #25652, #105133 ) ),
 .UNSPECIFIED., .F., .F., .T. ) 
 B_SPLINE_SURFACE_WITH_KNOTS ( ( 4, 4 ),
 ( 3, 3 ),
 ( 0.04058434257139457990, 0.04256401539001584966 ),
 ( 0.000000000000000000, 1.000000000000000000 ),
 .UNSPECIFIED. ) 
 GEOMETRIC_REPRESENTATION_ITEM ( )  RATIONAL_B_SPLINE_SURFACE ( (
 ( 1.000000000000000000, 0.7103081912008297749, 1.000000000000000000),
 ( 1.000000000000000000, 0.7104998333555360146, 1.000000000000000000),
 ( 1.000000000000000000, 0.7107238315755094460, 1.000000000000000000),
 ( 1.000000000000000000, 0.7110073749539291832, 1.000000000000000000) ) ) 
 REPRESENTATION_ITEM ( '' )  SURFACE ( )  );
#90098 = AXIS2_PLACEMENT_3D ( 'NONE', #120690, #138897, #218455 ) ;
#90099 = DIRECTION ( 'NONE',  ( 1.000000000000000000, 0.000000000000000000, 0.000000000000000000 ) ) ;
#90100 = DIRECTION ( 'NONE',  ( -1.000000000000000000, 0.000000000000000000, 0.000000000000000000 ) ) ;
#90102 = VERTEX_POINT ( 'NONE', #97796 ) ;
#90101 = CIRCLE ( 'NONE', #135884, 0.3999999999999994671 ) ;
#90103 = VECTOR ( 'NONE', #214596, 1000.000000000000114 ) ;
#90104 = DIRECTION ( 'NONE',  ( 0.000000000000000000, 1.000000000000000000, 6.982962677686266711E-15 ) ) ;
#90105 = AXIS2_PLACEMENT_3D ( 'NONE', #139977, #470, #120477 ) ;
#90106 = CARTESIAN_POINT ( 'NONE',  ( 20.04999999999999716, 52.10946721379481517, -233.0415979755771900 ) ) ;
#90107 = CYLINDRICAL_SURFACE ( 'NONE', #144789, 11.75000000000001066 ) ;
#90108 = CARTESIAN_POINT ( 'NONE',  ( 20.89999999999999858, -11.65000000000000036, -15.00000000000000000 ) ) ;
#90109 = CARTESIAN_POINT ( 'NONE',  ( 23.14999999999999503, 69.35000000001222986, -148.8731074845244109 ) ) ;
#90110 = DIRECTION ( 'NONE',  ( 1.000000000000000000, 0.000000000000000000, 0.000000000000000000 ) ) ;
#90111 = VERTEX_POINT ( 'NONE', #176110 ) ;
#90113 = DIRECTION ( 'NONE',  ( -1.073024830501117725E-15, -0.000000000000000000, -1.000000000000000000 ) ) ;
#90112 = CARTESIAN_POINT ( 'NONE',  ( -17.04761207306819770, 10.02645087339777241, -12.65000000000000213 ) ) ;
#90114 = ORIENTED_EDGE ( 'NONE', *, *, #145117, .T. ) ;
#90116 = EDGE_LOOP ( 'NONE', ( #45472, #39058, #154432, #237649 ) ) ;
#90115 = CARTESIAN_POINT ( 'NONE',  ( 18.69999999999999929, 1.149999999999999911, 21.90000000000000213 ) ) ;
#90117 = AXIS2_PLACEMENT_3D ( 'NONE', #256314, #77726, #37357 ) ;
#90118 = VERTEX_POINT ( 'NONE', #236053 ) ;
#90119 = CARTESIAN_POINT ( 'NONE',  ( -18.38817693311004575, 11.48149151591092476, -91.25000000000005684 ) ) ;
#90120 = AXIS2_PLACEMENT_3D ( 'NONE', #227587, #51491, #148062 ) ;
#90121 = DIRECTION ( 'NONE',  ( 1.000000000000000000, 0.000000000000000000, -0.000000000000000000 ) ) ;
#90122 = CARTESIAN_POINT ( 'NONE',  ( 23.14999999999999858, 1.115600667400684642E-11, -71.00000000000001421 ) ) ;
#90123 = DIRECTION ( 'NONE',  ( 0.000000000000000000, -1.000000000000000000, -7.272083257015735086E-15 ) ) ;
#90124 = ORIENTED_EDGE ( 'NONE', *, *, #20822, .F. ) ;
#90125 = CARTESIAN_POINT ( 'NONE',  ( 21.05000000000000071, 5.849999999999949019, -10.13249722427796762 ) ) ;
#90126 = DIRECTION ( 'NONE',  ( -1.000000000000000000, -2.952720810173289112E-16, 0.000000000000000000 ) ) ;
#90127 = EDGE_LOOP ( 'NONE', ( #98234, #251138, #175848, #22866 ) ) ;
#90128 = CYLINDRICAL_SURFACE ( 'NONE', #44058, 0.09999999999998898659 ) ;
#90129 = ADVANCED_FACE ( 'NONE', ( #116123 ), #96600, .T. ) ;
#90130 = AXIS2_PLACEMENT_3D ( 'NONE', #38631, #175587, #154748 ) ;
#90131 = CARTESIAN_POINT ( 'NONE',  ( 18.59999999999999076, 69.35000000001254250, -182.3731074845244109 ) ) ;
#90132 = ORIENTED_EDGE ( 'NONE', *, *, #524, .T. ) ;
#90133 = FACE_OUTER_BOUND ( 'NONE', #172810, .T. ) ;
#90134 = B_SPLINE_CURVE_WITH_KNOTS ( 'NONE', 3,
 ( #221253, #179601, #178326, #137866, #199147, #83008, #160044, #140439, #122184, #81724, #119623, #904, #3495, #201707, #23097, #80435, #79176, #120921, #38796 ),
 .UNSPECIFIED., .F., .F.,
 ( 4, 3, 3, 3, 3, 3, 4 ),
 ( -2.000416914649330048E-06, 0.000000000000000000, 4.714008503747417261E-05, 9.979203887780082271E-05, 0.0001372215519229642606, 0.0001635031576221119057, 0.0001900083748504280965 ),
 .UNSPECIFIED. ) ;
#90135 = ORIENTED_EDGE ( 'NONE', *, *, #69453, .T. ) ;
#90136 = DIRECTION ( 'NONE',  ( 1.000000000000000000, 0.000000000000000000, 0.000000000000000000 ) ) ;
#90137 = ORIENTED_EDGE ( 'NONE', *, *, #133513, .T. ) ;
#90138 = CARTESIAN_POINT ( 'NONE',  ( 21.05000000000000071, 76.10000000001240039, -176.5001538663141503 ) ) ;
#90139 = EDGE_CURVE ( 'NONE', #70632, #116539, #99086, .T. ) ;
#90140 = CARTESIAN_POINT ( 'NONE',  ( 21.05000000000000071, 6.257814610487280937, -133.9022097086912311 ) ) ;
#90141 = DIRECTION ( 'NONE',  ( -0.000000000000000000, 1.000000000000000000, -0.000000000000000000 ) ) ;
#90142 = SHAPE_REPRESENTATION ( 'Injection Molded Chain Links 9', ( #2425 ), #231953 ) ;
#90143 = ADVANCED_FACE ( 'NONE', ( #79526 ), #159113, .T. ) ;
#90144 = FACE_OUTER_BOUND ( 'NONE', #35356, .T. ) ;
#90145 = VECTOR ( 'NONE', #154712, 1000.000000000000000 ) ;
#90146 = AXIS2_PLACEMENT_3D ( 'NONE', #83759, #396, #218152 ) ;
#90147 = ADVANCED_FACE ( 'NONE', ( #34045 ), #113542, .F. ) ;
#90148 = CARTESIAN_POINT ( 'NONE',  ( 23.04999999999999716, 8.822561741666397950, -9.250000000000001776 ) ) ;
#90149 = DIRECTION ( 'NONE',  ( -1.000000000000000000, 0.000000000000000000, -0.000000000000000000 ) ) ;
#90150 = ORIENTED_EDGE ( 'NONE', *, *, #115188, .F. ) ;
#90151 = CARTESIAN_POINT ( 'NONE',  ( -21.55000000000000071, 63.46669608621377279, -222.0380013001639270 ) ) ;
#90152 = ORIENTED_EDGE ( 'NONE', *, *, #6666, .F. ) ;
#90154 = CARTESIAN_POINT ( 'NONE',  ( -22.50000000000000000, 1.115600667400684642E-11, -27.25000000000000355 ) ) ;
#90153 = CARTESIAN_POINT ( 'NONE',  ( 23.50000000000005684, 76.00000000001119815, -31.87310748452479459 ) ) ;
#90155 = AXIS2_PLACEMENT_3D ( 'NONE', #210222, #113664, #193220 ) ;
#90156 = ORIENTED_EDGE ( 'NONE', *, *, #225162, .T. ) ;
#90157 = DIRECTION ( 'NONE',  ( 0.000000000000000000, 0.000000000000000000, -1.000000000000000000 ) ) ;
#90158 = LINE ( 'NONE', #91472, #201427 ) ;
#90159 = DIRECTION ( 'NONE',  ( -0.000000000000000000, 0.9770955615653313941, 0.2128009952263603954 ) ) ;
#90160 = CARTESIAN_POINT ( 'NONE',  ( -20.85000000000000142, 76.00000000001190870, -103.0231074845243029 ) ) ;
#90161 = ORIENTED_EDGE ( 'NONE', *, *, #9559, .F. ) ;
#90163 = EDGE_LOOP ( 'NONE', ( #137920, #87551, #165855, #224633 ) ) ;
#90162 = CARTESIAN_POINT ( 'NONE',  ( -18.40000000000000213, 64.25000000001207923, -123.8731074845243683 ) ) ;
#90164 = EDGE_CURVE ( 'NONE', #56894, #178238, #1945, .T. ) ;
#90166 = DIRECTION ( 'NONE',  ( 0.000000000000000000, -0.8660254037844377084, -0.5000000000000016653 ) ) ;
#90165 = CIRCLE ( 'NONE', #65057, 0.09999999999999939493 ) ;
#90168 = CARTESIAN_POINT ( 'NONE',  ( -16.87036670365549895, 66.01058118071094327, -191.0026676018264595 ) ) ;
#90167 = CARTESIAN_POINT ( 'NONE',  ( 20.94999999999999929, 21.02001357433058004, -233.7432701311855965 ) ) ;
#90169 = CIRCLE ( 'NONE', #36032, 0.09999999999998898659 ) ;
#90171 = ORIENTED_EDGE ( 'NONE', *, *, #206946, .F. ) ;
#90170 = CARTESIAN_POINT ( 'NONE',  ( -20.54999999999999716, -11.74999999998884448, -188.6499999999999488 ) ) ;
#90172 = AXIS2_PLACEMENT_3D ( 'NONE', #180213, #98052, #2824 ) ;
#90173 = ORIENTED_EDGE ( 'NONE', *, *, #256831, .T. ) ;
#90174 = SPHERICAL_SURFACE ( 'NONE', #14421, 0.1000000000000000056 ) ;
#90175 = DIRECTION ( 'NONE',  ( 0.000000000000000000, -1.000000000000000000, 0.000000000000000000 ) ) ;
#90176 = EDGE_LOOP ( 'NONE', ( #127966, #108543, #110917, #213287 ) ) ;
#90177 = FACE_OUTER_BOUND ( 'NONE', #236343, .T. ) ;
#90178 = EDGE_LOOP ( 'NONE', ( #205012, #213837, #102681, #201844 ) ) ;
#90179 = CIRCLE ( 'NONE', #135977, 0.09999999999998898659 ) ;
#90180 = CARTESIAN_POINT ( 'NONE',  ( -20.00857864376270001, 66.85000000001156195, -57.17310748452438673 ) ) ;
#90181 = DIRECTION ( 'NONE',  ( 0.000000000000000000, -1.000000000000000000, -0.000000000000000000 ) ) ;
#90182 = ORIENTED_EDGE ( 'NONE', *, *, #109317, .T. ) ;
#90183 = CARTESIAN_POINT ( 'NONE',  ( -23.15000000000000213, 71.75000000001223555, -148.8731074845244109 ) ) ;
#90184 = ADVANCED_FACE ( 'NONE', ( #155273 ), #233510, .T. ) ;
#90185 = ORIENTED_EDGE ( 'NONE', *, *, #120897, .F. ) ;
#90186 = VECTOR ( 'NONE', #14998, 1000.000000000000000 ) ;
#90187 = CIRCLE ( 'NONE', #40171, 12.87500000000000178 ) ;
#90188 = FACE_OUTER_BOUND ( 'NONE', #151942, .T. ) ;
#90189 = AXIS2_PLACEMENT_3D ( 'NONE', #119357, #35975, #197590 ) ;
#90190 = ADVANCED_FACE ( 'NONE', ( #15761 ), #95261, .F. ) ;
#90191 = ORIENTED_EDGE ( 'NONE', *, *, #233408, .T. ) ;
#90192 = ORIENTED_EDGE ( 'NONE', *, *, #57024, .F. ) ;
#90193 = CARTESIAN_POINT ( 'NONE',  ( -20.54999999999999716, 11.48697431424113446, -220.1440440112397994 ) ) ;
#90194 = EDGE_LOOP ( 'NONE', ( #251812, #159224, #38416, #77818, #50693 ) ) ;
#90195 = DIRECTION ( 'NONE',  ( 2.952720810173289112E-16, -1.000000000000000000, -0.000000000000000000 ) ) ;
#90196 = ORIENTED_EDGE ( 'NONE', *, *, #95897, .F. ) ;
#90198 = ORIENTED_EDGE ( 'NONE', *, *, #52889, .F. ) ;
#90197 = DIRECTION ( 'NONE',  ( 0.000000000000000000, -0.8814952561688430555, 0.4721928772777346239 ) ) ;
#90199 = EDGE_CURVE ( 'NONE', #243905, #79646, #23464, .T. ) ;
#90200 = ORIENTED_EDGE ( 'NONE', *, *, #201423, .T. ) ;
#90201 = DIRECTION ( 'NONE',  ( 0.000000000000000000, -0.6626775042260681925, -0.7489048840758811831 ) ) ;
#90202 = ORIENTED_EDGE ( 'NONE', *, *, #139211, .T. ) ;
#90205 = ORIENTED_EDGE ( 'NONE', *, *, #202590, .T. ) ;
#90204 = ORIENTED_EDGE ( 'NONE', *, *, #191196, .F. ) ;
#90203 = CARTESIAN_POINT ( 'NONE',  ( 21.97500000000000497, 66.25000000001260503, -191.1731074845244223 ) ) ;
#90206 = FACE_OUTER_BOUND ( 'NONE', #62372, .T. ) ;
#90207 = AXIS2_PLACEMENT_3D ( 'NONE', #65984, #245915, #189788 ) ;
#90208 = ADVANCED_FACE ( 'NONE', ( #202071 ), #161679, .T. ) ;
#90209 = CARTESIAN_POINT ( 'NONE',  ( 17.74533788810830970, 62.85906666726748426, -210.6453698753407480 ) ) ;
#90210 = CIRCLE ( 'NONE', #165241, 11.75000000000000000 ) ;
#90212 = ORIENTED_EDGE ( 'NONE', *, *, #253740, .F. ) ;
#90211 = B_SPLINE_CURVE_WITH_KNOTS ( 'NONE', 3,
 ( #165757, #5343, #144871, #125329, #201015, #245281, #4085, #240144, #204841, #160628 ),
 .UNSPECIFIED., .F., .F.,
 ( 4, 3, 3, 4 ),
 ( 0.000000000000000000, 0.0002000000000008511354, 0.001000000000082984205, 0.001967863649483301593 ),
 .UNSPECIFIED. ) ;
#90213 = CIRCLE ( 'NONE', #2740, 2.000000000000001776 ) ;
#90214 = FACE_OUTER_BOUND ( 'NONE', #171060, .T. ) ;
#90215 = ORIENTED_EDGE ( 'NONE', *, *, #1497, .T. ) ;
#90216 = CARTESIAN_POINT ( 'NONE',  ( -21.05000000000000071, 69.45934304831143891, -203.4231074845244223 ) ) ;
#90217 = ADVANCED_FACE ( 'NONE', ( #104227 ), #59962, .T. ) ;
#90219 = ORIENTED_EDGE ( 'NONE', *, *, #254605, .T. ) ;
#90218 = CYLINDRICAL_SURFACE ( 'NONE', #153392, 11.75000000000001066 ) ;
#90220 = CARTESIAN_POINT ( 'NONE',  ( 23.14999999999999858, 1.115600667400684642E-11, -67.00000000000000000 ) ) ;
#90221 = ORIENTED_EDGE ( 'NONE', *, *, #191194, .T. ) ;
#90222 = DIRECTION ( 'NONE',  ( 0.000000000000000000, -0.9126074666063844765, -0.4088369013363114535 ) ) ;
#90223 = CARTESIAN_POINT ( 'NONE',  ( 18.49999999999999289, 65.76093837589047553, -111.7687100499271651 ) ) ;
#90225 = ORIENTED_EDGE ( 'NONE', *, *, #242478, .T. ) ;
#90224 = EDGE_CURVE ( 'NONE', #208604, #220305, #100819, .T. ) ;
#90226 = ADVANCED_FACE ( 'NONE', ( #85933 ), #80810, .F. ) ;
#90227 = FACE_OUTER_BOUND ( 'NONE', #165381, .T. ) ;
#90228 = ORIENTED_EDGE ( 'NONE', *, *, #235057, .F. ) ;
#90230 = ORIENTED_EDGE ( 'NONE', *, *, #33406, .T. ) ;
#90229 = CARTESIAN_POINT ( 'NONE',  ( 19.87657994472052536, 54.45653398996847017, -228.7028568925953778 ) ) ;
#90231 = DIRECTION ( 'NONE',  ( 0.7071067811865214825, -0.7071067811865735520, 0.000000000000000000 ) ) ;
#90232 = AXIS2_PLACEMENT_3D ( 'NONE', #234600, #16858, #217582 ) ;
#90233 = EDGE_CURVE ( 'NONE', #15098, #40541, #51612, .T. ) ;
#90235 = EDGE_LOOP ( 'NONE', ( #153448, #111027, #76419, #208319 ) ) ;
#90234 = ORIENTED_EDGE ( 'NONE', *, *, #207417, .F. ) ;
#90236 = VERTEX_POINT ( 'NONE', #222899 ) ;
#90237 = LINE ( 'NONE', #88957, #128275 ) ;
#90238 = ORIENTED_EDGE ( 'NONE', *, *, #184356, .T. ) ;
#90239 = ORIENTED_EDGE ( 'NONE', *, *, #145313, .F. ) ;
#90240 = DIRECTION ( 'NONE',  ( -0.000000000000000000, 0.1298341882520022694, 0.9915357197604853789 ) ) ;
#90241 = ORIENTED_EDGE ( 'NONE', *, *, #193121, .F. ) ;
#90242 = EDGE_CURVE ( 'NONE', #202597, #126077, #222306, .T. ) ;
#90243 = DIRECTION ( 'NONE',  ( 1.000000000000000000, 0.000000000000000000, 0.000000000000000000 ) ) ;
#90244 = EDGE_CURVE ( 'NONE', #27420, #237840, #159816, .T. ) ;
#90245 = AXIS2_PLACEMENT_3D ( 'NONE', #51207, #173816, #72105 ) ;
#90246 = FACE_OUTER_BOUND ( 'NONE', #89270, .T. ) ;
#90247 = ORIENTED_EDGE ( 'NONE', *, *, #147667, .F. ) ;
#90248 = VERTEX_POINT ( 'NONE', #142080 ) ;
#90249 = AXIS2_PLACEMENT_3D ( 'NONE', #13772, #1888, #60585 ) ;
#90250 = DIRECTION ( 'NONE',  ( 1.000000000000000000, 3.265361837132813093E-16, -0.000000000000000000 ) ) ;
#90251 = ORIENTED_EDGE ( 'NONE', *, *, #83230, .F. ) ;
#90252 = VECTOR ( 'NONE', #160546, 1000.000000000000114 ) ;
#90253 = CIRCLE ( 'NONE', #44509, 0.1000000000000002554 ) ;
#90254 = LINE ( 'NONE', #207673, #76237 ) ;
#90255 = EDGE_CURVE ( 'NONE', #219226, #120146, #189031, .T. ) ;
#90256 = ORIENTED_EDGE ( 'NONE', *, *, #41132, .F. ) ;
#90257 = EDGE_CURVE ( 'NONE', #205409, #8169, #84638, .T. ) ;
#90258 = CARTESIAN_POINT ( 'NONE',  ( 5.899999999999995914, -11.34999999999999964, 10.10000000000000142 ) ) ;
#90260 = ORIENTED_EDGE ( 'NONE', *, *, #251581, .T. ) ;
#90259 = DIRECTION ( 'NONE',  ( -0.9880948137434723000, 0.1538461538461483591, -0.000000000000000000 ) ) ;
#90261 = FACE_OUTER_BOUND ( 'NONE', #98666, .T. ) ;
#90262 = CARTESIAN_POINT ( 'NONE',  ( -23.25000000000000000, 68.97833521811131163, -32.18954208262707795 ) ) ;
#90263 = CARTESIAN_POINT ( 'NONE',  ( 18.49999999999999289, 33.69766839675185821, -236.3369293616048310 ) ) ;
#90264 = CARTESIAN_POINT ( 'NONE',  ( -21.13614978966382196, 6.499104701844944820, -134.0000000000000284 ) ) ;
#90265 = CARTESIAN_POINT ( 'NONE',  ( 20.94999999999999929, 1.835341550235569663, -78.55515129256303908 ) ) ;
#90266 = B_SPLINE_CURVE_WITH_KNOTS ( 'NONE', 3,
 ( #127832, #207374, #110817, #86090, #9160, #49570, #190386 ),
 .UNSPECIFIED., .F., .F.,
 ( 4, 3, 4 ),
 ( 0.000000000000000000, 4.520325912680430423E-05, 5.794988040901246848E-05 ),
 .UNSPECIFIED. ) ;
#90267 = LINE ( 'NONE', #109836, #78562 ) ;
#90268 = CARTESIAN_POINT ( 'NONE',  ( 21.30740335185486245, 10.13763019447862668, -227.9063222794615342 ) ) ;
#90269 = CARTESIAN_POINT ( 'NONE',  ( 22.40000000000010516, 76.00000000001340084, -181.6726782920694632 ) ) ;
#90270 = EDGE_CURVE ( 'NONE', #187404, #16838, #89055, .T. ) ;
#90271 = DIRECTION ( 'NONE',  ( -0.7071067811865388020, 0.7071067811865561215, 0.000000000000000000 ) ) ;
#90272 = CIRCLE ( 'NONE', #115234, 0.1000000000000064587 ) ;
#90273 = B_SPLINE_CURVE_WITH_KNOTS ( 'NONE', 3,
 ( #26456, #6874, #164676, #47265, #125540, #86379 ),
 .UNSPECIFIED., .F., .F.,
 ( 4, 2, 4 ),
 ( 0.000000000000000000, 0.0001497467027049168508, 0.0002994934054098337016 ),
 .UNSPECIFIED. ) ;
#90274 = ORIENTED_EDGE ( 'NONE', *, *, #104628, .T. ) ;
#90275 = AXIS2_PLACEMENT_3D ( 'NONE', #29645, #247365, #148279 ) ;
#90277 = ORIENTED_EDGE ( 'NONE', *, *, #239841, .T. ) ;
#90276 = AXIS2_PLACEMENT_3D ( 'NONE', #204821, #26219, #185282 ) ;
#90279 = ORIENTED_EDGE ( 'NONE', *, *, #2840, .T. ) ;
#90278 = DIRECTION ( 'NONE',  ( -1.000000000000000000, -0.000000000000000000, -0.000000000000000000 ) ) ;
#90280 = AXIS2_PLACEMENT_3D ( 'NONE', #127681, #108115, #187670 ) ;
#90281 = ORIENTED_EDGE ( 'NONE', *, *, #183862, .T. ) ;
#90282 = CARTESIAN_POINT ( 'NONE',  ( 23.24999999999997513, 64.35000000001218723, -143.5379132551784096 ) ) ;
#90283 = CARTESIAN_POINT ( 'NONE',  ( 20.97250901189795513, 10.62456803371303593, -141.6645457169670124 ) ) ;
#90284 = AXIS2_PLACEMENT_3D ( 'NONE', #12274, #91789, #171373 ) ;
#90285 = AXIS2_PLACEMENT_3D ( 'NONE', #34215, #233680, #253220 ) ;
#90286 = FACE_OUTER_BOUND ( 'NONE', #133485, .T. ) ;
#90287 = ORIENTED_EDGE ( 'NONE', *, *, #156048, .T. ) ;
#90288 = VERTEX_POINT ( 'NONE', #219045 ) ;
#90289 = EDGE_CURVE ( 'NONE', #149075, #123919, #155740, .T. ) ;
#90290 = CARTESIAN_POINT ( 'NONE',  ( 18.47073956224751257, -9.471729412460696551, -40.60868575281791237 ) ) ;
#90291 = EDGE_CURVE ( 'NONE', #153129, #26109, #44288, .T. ) ;
#90292 = DIRECTION ( 'NONE',  ( 0.000000000000000000, 0.000000000000000000, 1.000000000000000000 ) ) ;
#90293 = VERTEX_POINT ( 'NONE', #185065 ) ;
#90294 = ORIENTED_EDGE ( 'NONE', *, *, #233150, .F. ) ;
#90295 = VECTOR ( 'NONE', #91574, 1000.000000000000000 ) ;
#90296 = B_SPLINE_CURVE_WITH_KNOTS ( 'NONE', 3,
 ( #228014, #105457, #48084, #88473, #169365, #144603, #247573, #27283, #68962, #166789 ),
 .UNSPECIFIED., .F., .F.,
 ( 4, 3, 3, 4 ),
 ( 1.957469226477651626E-15, 8.145022132832446376E-06, 1.905645951092389470E-05, 2.061107371225767530E-05 ),
 .UNSPECIFIED. ) ;
#90297 = CARTESIAN_POINT ( 'NONE',  ( -16.87372386987899020, 9.880600233647918174, -180.6492698718663519 ) ) ;
#90298 = CIRCLE ( 'NONE', #44541, 0.1000000000000013933 ) ;
#90299 = LINE ( 'NONE', #8225, #116387 ) ;
#90300 = DIRECTION ( 'NONE',  ( -0.000000000000000000, -0.4721928772777346239, -0.8814952561688430555 ) ) ;
#90301 = AXIS2_PLACEMENT_3D ( 'NONE', #120600, #237946, #41068 ) ;
#90302 = EDGE_CURVE ( 'NONE', #7208, #64566, #205570, .T. ) ;
#90303 = CARTESIAN_POINT ( 'NONE',  ( -21.06715728752538652, 64.25000000001233502, -163.0083017138703951 ) ) ;
#90305 = ORIENTED_EDGE ( 'NONE', *, *, #237096, .T. ) ;
#90304 = CARTESIAN_POINT ( 'NONE',  ( 20.94999999999999574, 77.16270174994990327, -94.92310748452430857 ) ) ;
#90306 = DIRECTION ( 'NONE',  ( -1.000000000000000000, -0.000000000000000000, -0.000000000000000000 ) ) ;
#90307 = DIRECTION ( 'NONE',  ( 0.000000000000000000, 0.000000000000000000, -1.000000000000000000 ) ) ;
#90309 = EDGE_CURVE ( 'NONE', #252199, #16613, #160401, .T. ) ;
#90308 = DIRECTION ( 'NONE',  ( -1.000000000000000000, 0.000000000000000000, -0.000000000000000000 ) ) ;
#90310 = DIRECTION ( 'NONE',  ( -1.000000000000000000, -0.000000000000000000, -0.000000000000000000 ) ) ;
#90311 = VERTEX_POINT ( 'NONE', #220358 ) ;
#90312 = CARTESIAN_POINT ( 'NONE',  ( -20.94999999999999929, 7.021664781911246322, -104.1335654018973287 ) ) ;
#90314 = CYLINDRICAL_SURFACE ( 'NONE', #216267, 4.000000000000003553 ) ;
#90313 = CARTESIAN_POINT ( 'NONE',  ( 20.94999999999999929, 1.835341550224413698, -11.55515129256298401 ) ) ;
#90316 = EDGE_CURVE ( 'NONE', #198523, #136731, #72337, .T. ) ;
#90315 = CYLINDRICAL_SURFACE ( 'NONE', #232930, 7.900000000000000355 ) ;
#90317 = CARTESIAN_POINT ( 'NONE',  ( -16.93710578446422588, 9.950000000011137047, -54.08119601620066419 ) ) ;
#90318 = AXIS2_PLACEMENT_3D ( 'NONE', #1746, #82549, #242935 ) ;
#90319 = CARTESIAN_POINT ( 'NONE',  ( 18.59999999999997655, 64.25000000001190870, -103.0231074845243882 ) ) ;
#90320 = LINE ( 'NONE', #149047, #197786 ) ;
#90321 = CARTESIAN_POINT ( 'NONE',  ( -20.54999999999999716, -11.74999999998884448, -121.6500000000000341 ) ) ;
#90322 = CARTESIAN_POINT ( 'NONE',  ( 5.899999999999995914, -11.25000000000000000, 10.00000000000000178 ) ) ;
#90323 = EDGE_LOOP ( 'NONE', ( #216326, #96155, #214902, #105739 ) ) ;
#90324 = ADVANCED_FACE ( 'NONE', ( #43000 ), #218049, .T. ) ;
#90326 = ADVANCED_FACE ( 'NONE', ( #31173 ), #149815, .F. ) ;
#90325 = EDGE_CURVE ( 'NONE', #135756, #227551, #130761, .T. ) ;
#90327 = VERTEX_POINT ( 'NONE', #8999 ) ;
#90328 = ORIENTED_EDGE ( 'NONE', *, *, #65809, .T. ) ;
#90329 = DIRECTION ( 'NONE',  ( 0.000000000000000000, 0.000000000000000000, -1.000000000000000000 ) ) ;
#90330 = CARTESIAN_POINT ( 'NONE',  ( -23.15000000000000213, 43.07541598710462694, -233.9110336739111347 ) ) ;
#90331 = ORIENTED_EDGE ( 'NONE', *, *, #14271, .T. ) ;
#90332 = EDGE_CURVE ( 'NONE', #31299, #7157, #255612, .T. ) ;
#90333 = CIRCLE ( 'NONE', #102792, 11.75000000000000000 ) ;
#90334 = AXIS2_PLACEMENT_3D ( 'NONE', #59391, #214645, #198932 ) ;
#90335 = VERTEX_POINT ( 'NONE', #250182 ) ;
#90336 = TOROIDAL_SURFACE ( 'NONE', #94615, 11.65000000000000036, 0.1000000000000000056 ) ;
#90337 = AXIS2_PLACEMENT_3D ( 'NONE', #89673, #252602, #114391 ) ;
#90338 = ORIENTED_EDGE ( 'NONE', *, *, #43177, .T. ) ;
#90339 = ADVANCED_FACE ( 'NONE', ( #128955 ), #169401, .F. ) ;
#90340 = CARTESIAN_POINT ( 'NONE',  ( -23.15000000000000213, 64.25000000001260503, -191.3731074845244393 ) ) ;
#90341 = EDGE_CURVE ( 'NONE', #255841, #167682, #247610, .T. ) ;
#90342 = ORIENTED_EDGE ( 'NONE', *, *, #3574, .F. ) ;
#90343 = VECTOR ( 'NONE', #45683, 1000.000000000000000 ) ;
#90344 = CARTESIAN_POINT ( 'NONE',  ( -16.80939487329394666, 66.05000000001182059, -82.17310748452349856 ) ) ;
#90345 = CARTESIAN_POINT ( 'NONE',  ( -23.15000000000000213, 82.09643798151613225, -215.4278993322501208 ) ) ;
#90346 = DIRECTION ( 'NONE',  ( -0.000000000000000000, -0.1686199900910463068, 0.9856811345164802063 ) ) ;
#90347 = EDGE_CURVE ( 'NONE', #10818, #199162, #1578, .T. ) ;
#90348 = DIRECTION ( 'NONE',  ( -2.827886303505248766E-16, -0.8103668758649577031, 0.5859227990963212784 ) ) ;
#90349 = CARTESIAN_POINT ( 'NONE',  ( 22.39999999999999503, 29.58621655554530250, -252.7196486866020280 ) ) ;
#90351 = ORIENTED_EDGE ( 'NONE', *, *, #47979, .F. ) ;
#90350 = CARTESIAN_POINT ( 'NONE',  ( -16.84793658983391396, 30.13259441044248277, -234.7675476393297345 ) ) ;
#90353 = CARTESIAN_POINT ( 'NONE',  ( 20.94999999999999574, 77.16270174994961906, -61.42310748452431568 ) ) ;
#90352 = CARTESIAN_POINT ( 'NONE',  ( 20.94999999999999574, -11.48912529306490349, -103.4000000000000341 ) ) ;
#90354 = CARTESIAN_POINT ( 'NONE',  ( -16.86337532320261090, 9.979967204235514089, -154.9489244689828524 ) ) ;
#90355 = AXIS2_PLACEMENT_3D ( 'NONE', #1784, #218257, #180445 ) ;
#90356 = EDGE_CURVE ( 'NONE', #130340, #181022, #134830, .T. ) ;
#90357 = ORIENTED_EDGE ( 'NONE', *, *, #80175, .F. ) ;
#90358 = CARTESIAN_POINT ( 'NONE',  ( 15.39793903038207823, 66.61031399435637468, -120.8502639781730750 ) ) ;
#90359 = DIRECTION ( 'NONE',  ( 7.304098846218134667E-16, -1.000000000000000000, 0.000000000000000000 ) ) ;
#90360 = DIRECTION ( 'NONE',  ( 1.000000000000000000, 0.000000000000000000, 0.000000000000000000 ) ) ;
#90362 = ORIENTED_EDGE ( 'NONE', *, *, #82000, .F. ) ;
#90361 = CIRCLE ( 'NONE', #248579, 0.09999999999999939493 ) ;
#90363 = ADVANCED_FACE ( 'NONE', ( #12876 ), #234820, .T. ) ;
#90364 = VECTOR ( 'NONE', #123777, 1000.000000000000000 ) ;
#90365 =( NAMED_UNIT ( * ) PLANE_ANGLE_UNIT ( ) SI_UNIT ( $, .RADIAN. ) );
#90366 = CARTESIAN_POINT ( 'NONE',  ( -20.54999999999999716, 60.76440593117145994, -251.6273999706070583 ) ) ;
#90367 = CARTESIAN_POINT ( 'NONE',  ( -21.14999999999994174, 77.26165318615413469, -44.00978271863746016 ) ) ;
#90368 = ORIENTED_EDGE ( 'NONE', *, *, #223848, .T. ) ;
#90369 = AXIS2_PLACEMENT_3D ( 'NONE', #96830, #194712, #235103 ) ;
#90370 = CARTESIAN_POINT ( 'NONE',  ( 22.57320508075687115, 64.25000000001165290, -69.52310748452440237 ) ) ;
#90371 = CARTESIAN_POINT ( 'NONE',  ( 23.24999999999999289, 64.25000000001220712, -148.2731074845243882 ) ) ;
#90372 = EDGE_CURVE ( 'NONE', #192073, #175406, #106801, .T. ) ;
#90373 = EDGE_LOOP ( 'NONE', ( #123510, #244166, #73478, #209341 ) ) ;
#90374 = ORIENTED_EDGE ( 'NONE', *, *, #44668, .T. ) ;
#90376 = ADVANCED_FACE ( 'NONE', ( #109361 ), #248906, .T. ) ;
#90375 = DIRECTION ( 'NONE',  ( 0.000000000000000000, -6.982962677686266711E-15, 1.000000000000000000 ) ) ;
#90377 = CARTESIAN_POINT ( 'NONE',  ( -18.59999999999999787, -1.293555411365099994, -227.7000673772910204 ) ) ;
#90378 = CARTESIAN_POINT ( 'NONE',  ( 21.05000000000000071, 87.48912529308749697, -39.12310748452424747 ) ) ;
#90379 = CARTESIAN_POINT ( 'NONE',  ( -16.89268316805466341, 9.951721813253341153, -146.6442475214544743 ) ) ;
#90381 = LINE ( 'NONE', #252029, #170 ) ;
#90380 = DIRECTION ( 'NONE',  ( 0.000000000000000000, 0.000000000000000000, -1.000000000000000000 ) ) ;
#90382 = CIRCLE ( 'NONE', #186071, 0.09999999999999491240 ) ;
#90383 = VECTOR ( 'NONE', #77193, 1000.000000000000000 ) ;
#90384 = CARTESIAN_POINT ( 'NONE',  ( -20.94999999999999929, 87.65000000001235492, -167.0231074845242460 ) ) ;
#90386 = CIRCLE ( 'NONE', #48878, 0.1000000000000028644 ) ;
#90385 = DIRECTION ( 'NONE',  ( -1.000000000000000000, -0.000000000000000000, 0.000000000000000000 ) ) ;
#90387 = AXIS2_PLACEMENT_3D ( 'NONE', #134883, #220565, #174090 ) ;
#90388 = CARTESIAN_POINT ( 'NONE',  ( 19.99999999999998934, 11.65000000001115943, -88.25000000000005684 ) ) ;
#90389 = ORIENTED_EDGE ( 'NONE', *, *, #193809, .T. ) ;
#90390 = CARTESIAN_POINT ( 'NONE',  ( -20.88420186297724257, 65.66974365629666011, -97.43601455626048846 ) ) ;
#90392 = EDGE_LOOP ( 'NONE', ( #242700, #174962, #17394, #231908 ) ) ;
#90391 = LINE ( 'NONE', #249490, #142153 ) ;
#90393 = DIRECTION ( 'NONE',  ( 0.000000000000000000, -6.467318590049456648E-15, 1.000000000000000000 ) ) ;
#90394 = DIRECTION ( 'NONE',  ( 1.000000000000000000, 0.000000000000000000, 0.000000000000000000 ) ) ;
#90395 = DIRECTION ( 'NONE',  ( 2.952720810173289112E-16, 1.000000000000000000, -6.088138035986627436E-46 ) ) ;
#90396 = CARTESIAN_POINT ( 'NONE',  ( -16.82542659449982736, 66.06550010858471467, -123.7784718844978897 ) ) ;
#90397 = ADVANCED_FACE ( 'NONE', ( #88506 ), #147222, .F. ) ;
#90398 = CARTESIAN_POINT ( 'NONE',  ( 21.04386569057696121, 11.75000000001181988, -194.1428373517797468 ) ) ;
#90400 = ORIENTED_EDGE ( 'NONE', *, *, #84968, .F. ) ;
#90399 = CARTESIAN_POINT ( 'NONE',  ( 21.05000000000000071, 71.00000000001253397, -182.4283735034374843 ) ) ;
#90401 = DIRECTION ( 'NONE',  ( 0.000000000000000000, -1.000000000000000000, 0.000000000000000000 ) ) ;
#90402 = DIRECTION ( 'NONE',  ( 0.000000000000000000, 6.467318590049456648E-15, -1.000000000000000000 ) ) ;
#90403 = FACE_OUTER_BOUND ( 'NONE', #130196, .T. ) ;
#90404 = CARTESIAN_POINT ( 'NONE',  ( -21.05000000000000071, 70.97296516614450468, -234.1788952109995137 ) ) ;
#90405 = ORIENTED_EDGE ( 'NONE', *, *, #77853, .T. ) ;
#90406 = CARTESIAN_POINT ( 'NONE',  ( 18.43579564894472966, -7.817436314305575173, -209.8389869030123407 ) ) ;
#90407 = ORIENTED_EDGE ( 'NONE', *, *, #105872, .F. ) ;
#90408 = AXIS2_PLACEMENT_3D ( 'NONE', #171862, #33645, #157432 ) ;
#90410 = CIRCLE ( 'NONE', #119465, 0.2000000000000005107 ) ;
#90409 = PLANE ( 'NONE',  #21682 ) ;
#90411 = ORIENTED_EDGE ( 'NONE', *, *, #12403, .F. ) ;
#90412 = EDGE_CURVE ( 'NONE', #168199, #152727, #193136, .T. ) ;
#90413 = DIRECTION ( 'NONE',  ( 0.000000000000000000, 0.000000000000000000, -1.000000000000000000 ) ) ;
#90414 = ORIENTED_EDGE ( 'NONE', *, *, #37189, .T. ) ;
#90416 = CARTESIAN_POINT ( 'NONE',  ( -20.64999999999999858, 49.57218508014541669, -254.1759139559835035 ) ) ;
#90415 = CIRCLE ( 'NONE', #202838, 0.09999999999999939493 ) ;
#90417 = CARTESIAN_POINT ( 'NONE',  ( -20.85000000000000142, -1.362429037182151470, -175.3888812479212334 ) ) ;
#90418 = ORIENTED_EDGE ( 'NONE', *, *, #213710, .F. ) ;
#90419 = DIRECTION ( 'NONE',  ( 1.000000000000000000, 0.000000000000000000, 0.000000000000000000 ) ) ;
#90420 = CARTESIAN_POINT ( 'NONE',  ( -20.65000000000000568, 9.052352027203962592, -208.4953267290897543 ) ) ;
#90421 = CARTESIAN_POINT ( 'NONE',  ( -18.79999999999999716, 0.000000000000000000, 0.000000000000000000 ) ) ;
#90422 = CARTESIAN_POINT ( 'NONE',  ( 12.42718393586866554, 9.370655051123481627, -17.52582325598087820 ) ) ;
#90423 = FACE_OUTER_BOUND ( 'NONE', #72297, .T. ) ;
#90424 = TOROIDAL_SURFACE ( 'NONE', #123768, 4.149999999999999467, 0.1000000000000000056 ) ;
#90425 = CARTESIAN_POINT ( 'NONE',  ( 20.94999999999999929, 64.35000000001146248, -42.80697314750249660 ) ) ;
#90426 = VERTEX_POINT ( 'NONE', #51952 ) ;
#90428 = ORIENTED_EDGE ( 'NONE', *, *, #192352, .T. ) ;
#90427 = FACE_OUTER_BOUND ( 'NONE', #71732, .T. ) ;
#90429 = ORIENTED_EDGE ( 'NONE', *, *, #254698, .F. ) ;
#90430 = CYLINDRICAL_SURFACE ( 'NONE', #103019, 0.09999999999999939493 ) ;
#90431 = ORIENTED_EDGE ( 'NONE', *, *, #189237, .T. ) ;
#90432 = FACE_OUTER_BOUND ( 'NONE', #214760, .T. ) ;
#90433 = PLANE ( 'NONE',  #151408 ) ;
#90434 = FACE_BOUND ( 'NONE', #236372, .T. ) ;
#90435 = ORIENTED_EDGE ( 'NONE', *, *, #53342, .F. ) ;
#90436 = CARTESIAN_POINT ( 'NONE',  ( -23.15000000000000213, 85.50000000001251976, -179.9170766071767389 ) ) ;
#90437 = FACE_OUTER_BOUND ( 'NONE', #210044, .T. ) ;
#90438 = CIRCLE ( 'NONE', #207167, 11.64999999999999325 ) ;
#90439 = DIRECTION ( 'NONE',  ( 0.000000000000000000, 0.000000000000000000, -1.000000000000000000 ) ) ;
#90440 = EDGE_LOOP ( 'NONE', ( #37025, #70578, #227584, #137144 ) ) ;
#90442 = ORIENTED_EDGE ( 'NONE', *, *, #89357, .T. ) ;
#90441 = CARTESIAN_POINT ( 'NONE',  ( -20.94999999999999929, -1.162701749938009677, -8.000000000000000000 ) ) ;
#90443 = EDGE_CURVE ( 'NONE', #109375, #152727, #131509, .T. ) ;
#90444 = CARTESIAN_POINT ( 'NONE',  ( -21.05000000000000071, 64.25000000001249134, -177.0379132551784096 ) ) ;
#90445 = DIRECTION ( 'NONE',  ( 0.000000000000000000, 0.000000000000000000, -1.000000000000000000 ) ) ;
#90446 = AXIS2_PLACEMENT_3D ( 'NONE', #21207, #156865, #221911 ) ;
#90447 = CIRCLE ( 'NONE', #94535, 12.87499999999999822 ) ;
#90448 = VECTOR ( 'NONE', #181692, 1000.000000000000000 ) ;
#90449 = ORIENTED_EDGE ( 'NONE', *, *, #225000, .T. ) ;
#90451 = DIRECTION ( 'NONE',  ( 0.000000000000000000, -0.8814952561688430555, 0.4721928772777346239 ) ) ;
#90450 = PRODUCT_DEFINITION_FORMATION_WITH_SPECIFIED_SOURCE ( 'ANY', '', #7676, .NOT_KNOWN. ) ;
#90452 = CARTESIAN_POINT ( 'NONE',  ( 18.59999999999999076, 61.95000000001189733, -97.50941241376342816 ) ) ;
#90453 = CARTESIAN_POINT ( 'NONE',  ( 21.05000000000000071, 87.75000000001190870, -105.9231074845242091 ) ) ;
#90455 = VERTEX_POINT ( 'NONE', #126377 ) ;
#90454 = VECTOR ( 'NONE', #72993, 1000.000000000000114 ) ;
#90456 = CYLINDRICAL_SURFACE ( 'NONE', #221464, 0.1000000000000106914 ) ;
#90457 = EDGE_CURVE ( 'NONE', #147707, #10477, #176574, .T. ) ;
#90458 = AXIS2_PLACEMENT_3D ( 'NONE', #54432, #188811, #153593 ) ;
#90459 = DIRECTION ( 'NONE',  ( -1.000000000000000000, 0.000000000000000000, 0.000000000000000000 ) ) ;
#90460 = EDGE_CURVE ( 'NONE', #27216, #31477, #168224, .T. ) ;
#90461 = DIRECTION ( 'NONE',  ( -0.000000000000000000, -0.000000000000000000, -1.000000000000000000 ) ) ;
#90462 = ORIENTED_EDGE ( 'NONE', *, *, #153315, .F. ) ;
#90464 = ADVANCED_FACE ( 'NONE', ( #187660 ), #118378, .T. ) ;
#90463 = AXIS2_PLACEMENT_3D ( 'NONE', #133070, #35290, #136909 ) ;
#90465 = AXIS2_PLACEMENT_3D ( 'NONE', #129692, #87968, #30617 ) ;
#90466 = ORIENTED_EDGE ( 'NONE', *, *, #57803, .T. ) ;
#90467 = CARTESIAN_POINT ( 'NONE',  ( -23.25000000000000355, 64.25000000001264766, -194.2731074845244450 ) ) ;
#90468 = EDGE_CURVE ( 'NONE', #196735, #163267, #256449, .T. ) ;
#90469 = VERTEX_POINT ( 'NONE', #33746 ) ;
#90470 = EDGE_CURVE ( 'NONE', #121939, #241985, #255251, .T. ) ;
#90471 = CIRCLE ( 'NONE', #169646, 0.09999999999998898659 ) ;
#90472 = DIRECTION ( 'NONE',  ( -0.000000000000000000, 1.000000000000000000, 6.982962677686266711E-15 ) ) ;
#90475 = ORIENTED_EDGE ( 'NONE', *, *, #6008, .T. ) ;
#90474 = CARTESIAN_POINT ( 'NONE',  ( -16.81744102076749314, 44.13548170601895038, -235.2989316066074821 ) ) ;
#90473 =( BOUNDED_CURVE ( )  B_SPLINE_CURVE ( 3, ( #129145, #208700, #150011, #130417 ),
 .UNSPECIFIED., .F., .F. ) 
 B_SPLINE_CURVE_WITH_KNOTS ( ( 4, 4 ),
 ( 2.589852378279005496, 2.850972632318389710 ),
 .UNSPECIFIED. ) 
 CURVE ( )  GEOMETRIC_REPRESENTATION_ITEM ( )  RATIONAL_B_SPLINE_CURVE ( ( 1.000000000000000000, 0.9943260843901261525, 0.9943260843901261525, 1.000000000000000000 ) ) 
 REPRESENTATION_ITEM ( '' )  );
#90476 = FACE_OUTER_BOUND ( 'NONE', #32715, .T. ) ;
#90478 = TOROIDAL_SURFACE ( 'NONE', #161237, 12.97499999999999787, 0.1000000000000000056 ) ;
#90477 = CARTESIAN_POINT ( 'NONE',  ( 21.13507111622889667, 65.28231661301319377, -57.27393889816360684 ) ) ;
#90479 = EDGE_CURVE ( 'NONE', #251858, #14355, #14080, .T. ) ;
#90480 = CARTESIAN_POINT ( 'NONE',  ( -20.94999999999999929, -1.162701749926853712, -75.10000000000003695 ) ) ;
#90481 = DIRECTION ( 'NONE',  ( 0.000000000000000000, 1.000000000000000000, 0.000000000000000000 ) ) ;
#90482 = DIRECTION ( 'NONE',  ( 1.734723475976817507E-14, 0.9651348961777157509, -0.2617529984165031243 ) ) ;
#90483 = DIRECTION ( 'NONE',  ( -1.000000000000000000, 0.000000000000000000, 0.000000000000000000 ) ) ;
#90484 = CARTESIAN_POINT ( 'NONE',  ( 18.59999999999999076, 18.62343931468261715, -223.9512205031617214 ) ) ;
#90486 = ORIENTED_EDGE ( 'NONE', *, *, #1010, .T. ) ;
#90485 = CARTESIAN_POINT ( 'NONE',  ( 18.59999999999999787, -10.84999999999999076, 32.89999999999999858 ) ) ;
#90487 = ADVANCED_FACE ( 'NONE', ( #153705 ), #174548, .T. ) ;
#90488 = VECTOR ( 'NONE', #126548, 1000.000000000000000 ) ;
#90489 = AXIS2_PLACEMENT_3D ( 'NONE', #57675, #42004, #116396 ) ;
#90490 = TOROIDAL_SURFACE ( 'NONE', #86194, 11.70000000000000639, 0.1000000000000000056 ) ;
#90491 = LINE ( 'NONE', #170087, #239065 ) ;
#90492 = CARTESIAN_POINT ( 'NONE',  ( -18.59999999999999787, 36.65892442174935439, -249.5511627012433848 ) ) ;
#90493 = DIRECTION ( 'NONE',  ( 0.000000000000000000, -6.938893903907222067E-15, 1.000000000000000000 ) ) ;
#90494 = DIRECTION ( 'NONE',  ( -1.836970198721029934E-16, 1.000000000000000000, 0.000000000000000000 ) ) ;
#90495 = EDGE_LOOP ( 'NONE', ( #104234, #183314, #176902, #27365 ) ) ;
#90496 = EDGE_CURVE ( 'NONE', #13684, #60684, #234449, .T. ) ;
#90497 = LINE ( 'NONE', #205303, #19175 ) ;
#90498 = TOROIDAL_SURFACE ( 'NONE', #123848, 2.100000000000002309, 0.1000000000000000056 ) ;
#90499 = CARTESIAN_POINT ( 'NONE',  ( -23.25000000000000000, 67.49222854868494892, -195.4187676019683693 ) ) ;
#90500 = ORIENTED_EDGE ( 'NONE', *, *, #28695, .F. ) ;
#90501 = CARTESIAN_POINT ( 'NONE',  ( -20.54999999999999716, -9.399999999988846611, -124.1060308773475924 ) ) ;
#90503 = DIRECTION ( 'NONE',  ( 0.000000000000000000, 1.000000000000000000, 0.000000000000000000 ) ) ;
#90502 = AXIS2_PLACEMENT_3D ( 'NONE', #81568, #101108, #257610 ) ;
#90504 = EDGE_CURVE ( 'NONE', #106612, #221154, #18338, .T. ) ;
#90505 = VERTEX_POINT ( 'NONE', #93668 ) ;
#90506 = CARTESIAN_POINT ( 'NONE',  ( 18.59999999999999076, 66.54223038922117439, -213.7542166125332415 ) ) ;
#90507 = VERTEX_POINT ( 'NONE', #15434 ) ;
#90509 = ORIENTED_EDGE ( 'NONE', *, *, #156896, .F. ) ;
#90508 = PLANE ( 'NONE',  #180541 ) ;
#90510 = VECTOR ( 'NONE', #168535, 1000.000000000000000 ) ;
#90511 = CARTESIAN_POINT ( 'NONE',  ( -22.48660254037843487, 11.37252324248628632, -198.4720136275361710 ) ) ;
#90512 = AXIS2_PLACEMENT_3D ( 'NONE', #129677, #252181, #87953 ) ;
#90513 = ORIENTED_EDGE ( 'NONE', *, *, #107044, .F. ) ;
#90514 = CARTESIAN_POINT ( 'NONE',  ( -23.15000000000000213, 2.319530388122572617, -217.8268657444419887 ) ) ;
#90515 = AXIS2_PLACEMENT_3D ( 'NONE', #24638, #44183, #100265 ) ;
#90516 = AXIS2_PLACEMENT_3D ( 'NONE', #140354, #219904, #221173 ) ;
#90517 = ORIENTED_EDGE ( 'NONE', *, *, #9111, .T. ) ;
#90518 = ORIENTED_EDGE ( 'NONE', *, *, #51761, .F. ) ;
#90519 = CARTESIAN_POINT ( 'NONE',  ( -23.25000000000000000, 84.59626168225520360, -145.9732350016745954 ) ) ;
#90521 = ORIENTED_EDGE ( 'NONE', *, *, #244267, .F. ) ;
#90520 = DIRECTION ( 'NONE',  ( 0.000000000000000000, 0.9876197685951252359, -0.1568667991644863424 ) ) ;
#90522 = DIRECTION ( 'NONE',  ( 1.000000000000000000, -0.000000000000000000, -0.000000000000000000 ) ) ;
#90523 = ORIENTED_EDGE ( 'NONE', *, *, #91503, .T. ) ;
#90524 = VECTOR ( 'NONE', #84448, 1000.000000000000000 ) ;
#90525 = EDGE_CURVE ( 'NONE', #68538, #127360, #233207, .T. ) ;
#90526 = EDGE_LOOP ( 'NONE', ( #198124, #256001, #250692, #15982 ) ) ;
#90527 = DIRECTION ( 'NONE',  ( 1.000000000000000000, 1.836970198721029934E-16, -0.000000000000000000 ) ) ;
#90528 = CARTESIAN_POINT ( 'NONE',  ( -21.05000000000000071, 14.05000000001115623, -173.0136950707609458 ) ) ;
#90529 = EDGE_CURVE ( 'NONE', #40138, #91949, #97410, .T. ) ;
#90530 = DIRECTION ( 'NONE',  ( 0.000000000000000000, 0.2617529984165033463, 0.9651348961777157509 ) ) ;
#90531 = ORIENTED_EDGE ( 'NONE', *, *, #63166, .T. ) ;
#90532 = CARTESIAN_POINT ( 'NONE',  ( 21.05000000000000071, 13.96869538424789070, -210.3925794786331949 ) ) ;
#90533 = DIRECTION ( 'NONE',  ( 1.441126678808781001E-14, 0.9876197685951252359, 0.1568667991644863424 ) ) ;
#90534 = CARTESIAN_POINT ( 'NONE',  ( -23.15000000000000213, 11.75000000001115552, -79.15000000000004832 ) ) ;
#90535 = AXIS2_PLACEMENT_3D ( 'NONE', #253968, #128912, #72813 ) ;
#90537 = ORIENTED_EDGE ( 'NONE', *, *, #106016, .T. ) ;
#90536 = EDGE_CURVE ( 'NONE', #189932, #176334, #180652, .T. ) ;
#90539 = EDGE_CURVE ( 'NONE', #102379, #133216, #171965, .T. ) ;
#90538 = CARTESIAN_POINT ( 'NONE',  ( -21.33487959338958362, 60.74020368437641082, -234.0946914941910677 ) ) ;
#90540 = DIRECTION ( 'NONE',  ( 0.000000000000000000, 0.000000000000000000, 1.000000000000000000 ) ) ;
#90541 = DIRECTION ( 'NONE',  ( -0.000000000000000000, -0.01283462868040327436, 0.9999176327611370985 ) ) ;
#90542 = CARTESIAN_POINT ( 'NONE',  ( 23.14999999999999503, 52.91185528119409298, -244.1460391050142675 ) ) ;
#90543 = ORIENTED_EDGE ( 'NONE', *, *, #5548, .T. ) ;
#90544 = CARTESIAN_POINT ( 'NONE',  ( -21.05000000000000071, 77.83534155023700407, -191.8679561919613832 ) ) ;
#90545 = VERTEX_POINT ( 'NONE', #152392 ) ;
#90546 = DIRECTION ( 'NONE',  ( 1.000000000000000000, 0.000000000000000000, 0.000000000000000000 ) ) ;
#90548 = ORIENTED_EDGE ( 'NONE', *, *, #183826, .T. ) ;
#90547 = CIRCLE ( 'NONE', #248981, 0.09999999999998900047 ) ;
#90549 = DIRECTION ( 'NONE',  ( 0.000000000000000000, 0.7071067811865472397, -0.7071067811865479058 ) ) ;
#90550 = DIRECTION ( 'NONE',  ( 1.000000000000000000, 0.000000000000000000, 0.000000000000000000 ) ) ;
#90551 = EDGE_CURVE ( 'NONE', #58688, #172629, #17969, .T. ) ;
#90552 = ORIENTED_EDGE ( 'NONE', *, *, #100240, .T. ) ;
#90553 = VERTEX_POINT ( 'NONE', #97484 ) ;
#90554 = CARTESIAN_POINT ( 'NONE',  ( -21.14999999999999858, 76.10000000001245724, -181.6726782920691505 ) ) ;
#90555 = LINE ( 'NONE', #127124, #75626 ) ;
#90556 = ORIENTED_EDGE ( 'NONE', *, *, #254163, .T. ) ;
#90557 = DIRECTION ( 'NONE',  ( 0.000000000000000000, -0.1480365673253065117, 0.9889818879709273425 ) ) ;
#90558 = SURFACE_STYLE_USAGE ( .BOTH. , #74895 ) ;
#90559 = ORIENTED_EDGE ( 'NONE', *, *, #127696, .T. ) ;
#90560 = CARTESIAN_POINT ( 'NONE',  ( -16.93658211146646408, 9.994108662352344297, -180.0957049300442918 ) ) ;
#90561 = CIRCLE ( 'NONE', #123910, 0.09999999999999939493 ) ;
#90562 = CIRCLE ( 'NONE', #119634, 4.099999999999992539 ) ;
#90563 = AXIS2_PLACEMENT_3D ( 'NONE', #19498, #216399, #119901 ) ;
#90564 = ORIENTED_EDGE ( 'NONE', *, *, #7938, .F. ) ;
#90565 = CARTESIAN_POINT ( 'NONE',  ( -18.59999999999999787, 11.65000000001115232, -179.7499999999999716 ) ) ;
#90566 =( BOUNDED_SURFACE ( )  B_SPLINE_SURFACE ( 3, 2, ( 
 ( #164284, #243805, #224233 ),
 ( #185119, #85981, #15487 ),
 ( #132862, #250225, #110715 ),
 ( #214947, #114570, #54584 ) ),
 .UNSPECIFIED., .F., .F., .T. ) 
 B_SPLINE_SURFACE_WITH_KNOTS ( ( 4, 4 ),
 ( 3, 3 ),
 ( 0.04058434257139457990, 0.04256401539001584966 ),
 ( 0.000000000000000000, 1.000000000000000000 ),
 .UNSPECIFIED. ) 
 GEOMETRIC_REPRESENTATION_ITEM ( )  RATIONAL_B_SPLINE_SURFACE ( (
 ( 1.000000000000000000, 0.7103081912007872534, 1.000000000000000000),
 ( 1.000000000000000000, 0.7104998333556717949, 1.000000000000000000),
 ( 1.000000000000000000, 0.7107238315754015323, 1.000000000000000000),
 ( 1.000000000000000000, 0.7110073749539779220, 1.000000000000000000) ) ) 
 REPRESENTATION_ITEM ( '' )  SURFACE ( )  );
#90567 = CARTESIAN_POINT ( 'NONE',  ( -16.77828822508139694, 22.98741874091696147, -230.9443501695940313 ) ) ;
#90568 = EDGE_CURVE ( 'NONE', #238808, #187977, #135011, .T. ) ;
#90569 = EDGE_CURVE ( 'NONE', #43432, #104140, #55902, .T. ) ;
#90570 = DIRECTION ( 'NONE',  ( -1.000000000000000000, -0.000000000000000000, 0.000000000000000000 ) ) ;
#90572 = ORIENTED_EDGE ( 'NONE', *, *, #114556, .F. ) ;
#90571 = DIRECTION ( 'NONE',  ( 0.000000000000000000, 0.7092521942343974484, 0.7049548389604062271 ) ) ;
#90573 = DIRECTION ( 'NONE',  ( 0.000000000000000000, 1.000000000000000000, 1.156482317317864980E-14 ) ) ;
#90574 = CARTESIAN_POINT ( 'NONE',  ( 21.72449340488909897, 65.71604372252141957, -182.6731074845244223 ) ) ;
#90575 = DIRECTION ( 'NONE',  ( 0.000000000000000000, 0.000000000000000000, 1.000000000000000000 ) ) ;
#90578 = DIRECTION ( 'NONE',  ( -2.557131231893036985E-16, 0.8660254037844384856, -0.5000000000000002220 ) ) ;
#90577 = VECTOR ( 'NONE', #228415, 1000.000000000000000 ) ;
#90576 = DIRECTION ( 'NONE',  ( 0.000000000000000000, 0.000000000000000000, -1.000000000000000000 ) ) ;
#90579 = DIRECTION ( 'NONE',  ( -0.000000000000000000, 0.8660254037844411501, 0.4999999999999956701 ) ) ;
#90580 = CARTESIAN_POINT ( 'NONE',  ( 18.49505832270840955, -9.438028062771739002, -107.6984731748938771 ) ) ;
#90581 = EDGE_CURVE ( 'NONE', #51812, #21148, #184930, .T. ) ;
#90582 = AXIS2_PLACEMENT_3D ( 'NONE', #25354, #36256, #255222 ) ;
#90583 = DIRECTION ( 'NONE',  ( 1.000000000000000000, 0.000000000000000000, 0.000000000000000000 ) ) ;
#90584 = FACE_OUTER_BOUND ( 'NONE', #131076, .T. ) ;
#90585 = ORIENTED_EDGE ( 'NONE', *, *, #209757, .F. ) ;
#90586 = AXIS2_PLACEMENT_3D ( 'NONE', #228743, #185747, #223563 ) ;
#90587 = EDGE_LOOP ( 'NONE', ( #131705, #189273, #164605, #32891, #15508, #213441, #147349, #34164, #151272, #220175 ) ) ;
#90588 = ORIENTED_EDGE ( 'NONE', *, *, #161485, .F. ) ;
#90589 = DIRECTION ( 'NONE',  ( 0.000000000000000000, -0.1298341882520022694, -0.9915357197604852679 ) ) ;
#90590 = FACE_OUTER_BOUND ( 'NONE', #235139, .T. ) ;
#90591 = ORIENTED_EDGE ( 'NONE', *, *, #15585, .T. ) ;
#90592 = DIRECTION ( 'NONE',  ( 0.000000000000000000, 0.000000000000000000, 1.000000000000000000 ) ) ;
#90593 = CARTESIAN_POINT ( 'NONE',  ( 20.84999999999998721, 10.33248238083634440, -206.5948465439131496 ) ) ;
#90594 = EDGE_CURVE ( 'NONE', #101672, #24943, #201678, .T. ) ;
#90595 = CYLINDRICAL_SURFACE ( 'NONE', #107924, 0.1000000000000098310 ) ;
#90596 = EDGE_LOOP ( 'NONE', ( #161556, #83262, #35798, #50796 ) ) ;
#90597 = ORIENTED_EDGE ( 'NONE', *, *, #67063, .T. ) ;
#90598 = CARTESIAN_POINT ( 'NONE',  ( 21.09696443733127325, 60.08364808979766991, -221.2398740259893657 ) ) ;
#90599 = DIRECTION ( 'NONE',  ( -0.000000000000000000, -0.8814952561688430555, 0.4721928772777346239 ) ) ;
#90600 = EDGE_LOOP ( 'NONE', ( #82839, #153594, #232746, #29902 ) ) ;
#90601 = EDGE_CURVE ( 'NONE', #76888, #224580, #14263, .T. ) ;
#90602 = CARTESIAN_POINT ( 'NONE',  ( 20.99999999999999645, 9.750000000011137757, -109.7500000000000426 ) ) ;
#90604 = VERTEX_POINT ( 'NONE', #141764 ) ;
#90603 = CARTESIAN_POINT ( 'NONE',  ( 23.14999999999998437, 40.35498466150056629, -247.8953732508333587 ) ) ;
#90605 = DIRECTION ( 'NONE',  ( 1.000000000000000000, -0.000000000000000000, -0.000000000000000000 ) ) ;
#90607 = CARTESIAN_POINT ( 'NONE',  ( -18.50000000000000000, 67.23127455305835554, -235.8551265064784559 ) ) ;
#90606 = AXIS2_PLACEMENT_3D ( 'NONE', #131117, #112847, #93274 ) ;
#90609 = ORIENTED_EDGE ( 'NONE', *, *, #122468, .T. ) ;
#90608 = DIRECTION ( 'NONE',  ( 1.000000000000000000, 7.304098846218105085E-16, 4.217023435051677501E-16 ) ) ;
#90610 = EDGE_CURVE ( 'NONE', #49667, #179995, #4807, .T. ) ;
#90611 = CARTESIAN_POINT ( 'NONE',  ( -21.05000000000000071, 2.838478681111047841, -208.5693404029859437 ) ) ;
#90612 = CARTESIAN_POINT ( 'NONE',  ( -23.15000000000000213, 36.65892442174935439, -249.5511627012433848 ) ) ;
#90613 = DIRECTION ( 'NONE',  ( 0.000000000000000000, 0.000000000000000000, -1.000000000000000000 ) ) ;
#90614 = AXIS2_PLACEMENT_3D ( 'NONE', #138220, #59965, #196925 ) ;
#90616 = CARTESIAN_POINT ( 'NONE',  ( 20.97250901189795513, 10.62456803371303593, -108.1645457169670266 ) ) ;
#90615 = CARTESIAN_POINT ( 'NONE',  ( 18.59999999999999076, 64.35000000001220144, -145.1731074845244507 ) ) ;
#90618 = ADVANCED_FACE ( 'NONE', ( #220034 ), #158805, .T. ) ;
#90617 = DIRECTION ( 'NONE',  ( -1.000000000000000000, 0.000000000000000000, 0.000000000000000000 ) ) ;
#90619 = DIRECTION ( 'NONE',  ( 0.000000000000000000, -1.000000000000000000, 0.000000000000000000 ) ) ;
#90620 = CIRCLE ( 'NONE', #190615, 11.74999999999999645 ) ;
#90621 = AXIS2_PLACEMENT_3D ( 'NONE', #145767, #62402, #3698 ) ;
#90622 = DIRECTION ( 'NONE',  ( -1.000000000000000000, -0.000000000000000000, -0.000000000000000000 ) ) ;
#90623 = DIRECTION ( 'NONE',  ( -0.000000000000000000, 0.8660254037844377084, 0.5000000000000016653 ) ) ;
#90624 = AXIS2_PLACEMENT_3D ( 'NONE', #234139, #111634, #72527 ) ;
#90625 = ORIENTED_EDGE ( 'NONE', *, *, #235756, .F. ) ;
#90626 = EDGE_CURVE ( 'NONE', #116221, #253858, #114188, .T. ) ;
#90627 = DIRECTION ( 'NONE',  ( 1.000000000000000000, 0.000000000000000000, 0.000000000000000000 ) ) ;
#90628 = ADVANCED_FACE ( 'NONE', ( #63510 ), #20570, .T. ) ;
#90629 = ORIENTED_EDGE ( 'NONE', *, *, #166810, .F. ) ;
#90630 = DIRECTION ( 'NONE',  ( -1.000000000000000000, -2.952720810173289112E-16, 0.000000000000000000 ) ) ;
#90631 = ORIENTED_EDGE ( 'NONE', *, *, #6709, .T. ) ;
#90633 = CARTESIAN_POINT ( 'NONE',  ( -23.15000000000000213, 2.600000000011156054, -113.7246219227621395 ) ) ;
#90632 = AXIS2_PLACEMENT_3D ( 'NONE', #103791, #106362, #9851 ) ;
#90634 = DIRECTION ( 'NONE',  ( 1.000000000000000000, 0.000000000000000000, 0.000000000000000000 ) ) ;
#90635 = ORIENTED_EDGE ( 'NONE', *, *, #17661, .T. ) ;
#90636 = DIRECTION ( 'NONE',  ( -1.000000000000000000, 0.000000000000000000, 0.000000000000000000 ) ) ;
#90637 = CIRCLE ( 'NONE', #44877, 0.09999999999999939493 ) ;
#90638 = EDGE_LOOP ( 'NONE', ( #246712, #33401, #46290 ) ) ;
#90639 = ADVANCED_FACE ( 'NONE', ( #119663 ), #179641, .F. ) ;
#90641 = ADVANCED_FACE ( 'NONE', ( #102619 ), #120960, .F. ) ;
#90640 = AXIS2_PLACEMENT_3D ( 'NONE', #26767, #127121, #189671 ) ;
#90642 = ORIENTED_EDGE ( 'NONE', *, *, #149212, .F. ) ;
#90644 = LINE ( 'NONE', #145491, #108745 ) ;
#90643 = CIRCLE ( 'NONE', #232339, 7.791421356237338003 ) ;
#90645 = CARTESIAN_POINT ( 'NONE',  ( 23.25000000000000000, 45.25174493058054281, -238.5244480634700324 ) ) ;
#90646 = CARTESIAN_POINT ( 'NONE',  ( 18.59999999999999787, 42.94477010600542854, -254.3363632230312703 ) ) ;
#90647 = AXIS2_PLACEMENT_3D ( 'NONE', #246742, #25168, #143793 ) ;
#90648 = CARTESIAN_POINT ( 'NONE',  ( 12.25000000000000000, 26.40960863751538312, -233.4539077120826107 ) ) ;
#90649 = CARTESIAN_POINT ( 'NONE',  ( -21.44999999999999929, 7.350000000011155166, -88.25000000000005684 ) ) ;
#90650 = AXIS2_PLACEMENT_3D ( 'NONE', #159167, #202121, #58723 ) ;
#90651 = EDGE_CURVE ( 'NONE', #162196, #13073, #183480, .T. ) ;
#90653 = CARTESIAN_POINT ( 'NONE',  ( -18.38817693311004575, 11.48149151591092476, -57.75000000000000000 ) ) ;
#90652 = CARTESIAN_POINT ( 'NONE',  ( -18.59999999999999787, 7.128833340093095217, -233.7327013124392749 ) ) ;
#90654 = CARTESIAN_POINT ( 'NONE',  ( 18.52928932188133970, 10.27928932189250055, -58.15000000000000568 ) ) ;
#90656 = ORIENTED_EDGE ( 'NONE', *, *, #95664, .F. ) ;
#90655 = CARTESIAN_POINT ( 'NONE',  ( 21.72449340488910252, 65.71604372252093640, -123.8731074845243683 ) ) ;
#90658 = CARTESIAN_POINT ( 'NONE',  ( 21.14999999999999858, 1.115600667400684642E-11, -160.9593430482987344 ) ) ;
#90657 = CARTESIAN_POINT ( 'NONE',  ( -18.59999999999999787, 66.75000000001151079, -48.27310748452438816 ) ) ;
#90659 = AXIS2_PLACEMENT_3D ( 'NONE', #131575, #211115, #87298 ) ;
#90660 = CARTESIAN_POINT ( 'NONE',  ( 21.05000000000000071, 54.36558989155976462, -236.3448031251562327 ) ) ;
#90661 = EDGE_LOOP ( 'NONE', ( #145859, #220717, #149650 ) ) ;
#90662 = DIRECTION ( 'NONE',  ( 0.000000000000000000, 0.000000000000000000, -1.000000000000000000 ) ) ;
#90663 = FACE_OUTER_BOUND ( 'NONE', #248731, .T. ) ;
#90664 = FACE_OUTER_BOUND ( 'NONE', #145235, .T. ) ;
#90665 = VERTEX_POINT ( 'NONE', #200474 ) ;
#90666 = ADVANCED_FACE ( 'NONE', ( #221292 ), #42675, .T. ) ;
#90667 = CARTESIAN_POINT ( 'NONE',  ( -16.78493832629888871, 60.94702803318471496, -221.0293550571836363 ) ) ;
#90668 = EDGE_CURVE ( 'NONE', #57200, #185004, #43962, .T. ) ;
#90669 = CIRCLE ( 'NONE', #211310, 0.2000000000000057288 ) ;
#90670 = CARTESIAN_POINT ( 'NONE',  ( -18.50000000000000000, 11.40444339177023458, -198.6185779617709670 ) ) ;
#90671 = CARTESIAN_POINT ( 'NONE',  ( 18.59999999999999432, -1.162701749926853712, -41.60000000000000142 ) ) ;
#90672 = AXIS2_PLACEMENT_3D ( 'NONE', #204930, #121654, #36986 ) ;
#90674 = VERTEX_POINT ( 'NONE', #243440 ) ;
#90673 = AXIS2_PLACEMENT_3D ( 'NONE', #142937, #167689, #46416 ) ;
#90675 = EDGE_LOOP ( 'NONE', ( #133865, #59454, #172332 ) ) ;
#90676 = CARTESIAN_POINT ( 'NONE',  ( 21.05000000000000071, 1.115649653272650466E-11, -163.5000000000000284 ) ) ;
#90677 = CARTESIAN_POINT ( 'NONE',  ( -18.55121869061588669, 10.32747123227773045, -173.0774032850249569 ) ) ;
#90678 = CARTESIAN_POINT ( 'NONE',  ( 23.24999999999999289, 28.81810206650552075, -238.0339362645743222 ) ) ;
#90680 = ADVANCED_FACE ( 'NONE', ( #180913 ), #248195, .F. ) ;
#90679 = CARTESIAN_POINT ( 'NONE',  ( -20.85000000000000142, 10.33248238083634440, -206.5948465439131496 ) ) ;
#90681 = ORIENTED_EDGE ( 'NONE', *, *, #250917, .T. ) ;
#90682 = CARTESIAN_POINT ( 'NONE',  ( 23.25000000000000000, -4.356730526971940520, -226.1082375506050539 ) ) ;
#90683 = TOROIDAL_SURFACE ( 'NONE', #32474, 0.2000000000000000111, 0.1000000000000000056 ) ;
#90684 = CARTESIAN_POINT ( 'NONE',  ( 23.24999999999999645, 34.81737220036617941, -252.9889942003018461 ) ) ;
#90685 = AXIS2_PLACEMENT_3D ( 'NONE', #175971, #33921, #113406 ) ;
#90687 = EDGE_CURVE ( 'NONE', #241247, #188351, #31030, .T. ) ;
#90686 = DIRECTION ( 'NONE',  ( 0.000000000000000000, 0.9908441862701791170, -0.1350103645450472789 ) ) ;
#90688 = CARTESIAN_POINT ( 'NONE',  ( -20.64999999999999858, 11.48697431424113446, -220.1440440112397994 ) ) ;
#90689 = VECTOR ( 'NONE', #256126, 1000.000000000000114 ) ;
#90690 = VERTEX_POINT ( 'NONE', #149508 ) ;
#90691 = CARTESIAN_POINT ( 'NONE',  ( -20.94999999999999929, 77.16412189325286874, -61.60825939895269698 ) ) ;
#90692 = VECTOR ( 'NONE', #191004, 1000.000000000000000 ) ;
#90694 = ORIENTED_EDGE ( 'NONE', *, *, #199429, .T. ) ;
#90693 = CARTESIAN_POINT ( 'NONE',  ( -16.91256925476571737, 66.01426884188440170, -190.9907499735297165 ) ) ;
#90695 = CARTESIAN_POINT ( 'NONE',  ( -20.94999999999999929, 74.83729825007431202, -162.0231074845243597 ) ) ;
#90696 = DIRECTION ( 'NONE',  ( -0.7071067811865475727, 0.6824534298470373850, -0.1850873201762210096 ) ) ;
#90697 = DIRECTION ( 'NONE',  ( 0.000000000000000000, 0.000000000000000000, 1.000000000000000000 ) ) ;
#90698 = ADVANCED_FACE ( 'NONE', ( #225141 ), #247282, .T. ) ;
#90699 = DIRECTION ( 'NONE',  ( -1.000000000000000000, 0.000000000000000000, 0.000000000000000000 ) ) ;
#90700 = ORIENTED_EDGE ( 'NONE', *, *, #143868, .F. ) ;
#90701 = CARTESIAN_POINT ( 'NONE',  ( 21.14999999999999858, 8.786607556600111835, -12.25000000000000000 ) ) ;
#90702 = VECTOR ( 'NONE', #111733, 1000.000000000000000 ) ;
#90703 = DIRECTION ( 'NONE',  ( -0.000000000000000000, 1.000000000000000000, 6.982962677686266711E-15 ) ) ;
#90704 = CARTESIAN_POINT ( 'NONE',  ( 20.85882249326303040, 67.49222854868494892, -195.4187676019683693 ) ) ;
#90705 = ORIENTED_EDGE ( 'NONE', *, *, #207305, .T. ) ;
#90706 = CARTESIAN_POINT ( 'NONE',  ( 20.94999999999999574, 74.15091558138558980, -191.8670969630772447 ) ) ;
#90707 = FACE_OUTER_BOUND ( 'NONE', #225524, .T. ) ;
#90708 = CYLINDRICAL_SURFACE ( 'NONE', #229680, 0.1000000000000028644 ) ;
#90709 = CIRCLE ( 'NONE', #61677, 0.2000000000000057288 ) ;
#90710 = DIRECTION ( 'NONE',  ( 0.000000000000000000, -0.2128009952263485993, 0.9770955615653341697 ) ) ;
#90711 = CARTESIAN_POINT ( 'NONE',  ( 21.04999999999999716, 6.496686585778529199, -167.5146561185098619 ) ) ;
#90712 = VECTOR ( 'NONE', #248403, 1000.000000000000000 ) ;
#90713 = CARTESIAN_POINT ( 'NONE',  ( 12.25000000000000355, 9.350000000011142731, -184.3642676076160569 ) ) ;
#90714 = ORIENTED_EDGE ( 'NONE', *, *, #165084, .T. ) ;
#90715 = ORIENTED_EDGE ( 'NONE', *, *, #180707, .F. ) ;
#90716 = DIRECTION ( 'NONE',  ( 0.000000000000000000, 0.000000000000000000, 1.000000000000000000 ) ) ;
#90717 = CARTESIAN_POINT ( 'NONE',  ( -20.54999999999999716, 9.350000000011156942, -155.1500000000000057 ) ) ;
#90718 = DIRECTION ( 'NONE',  ( 1.000000000000000000, -0.000000000000000000, 0.000000000000000000 ) ) ;
#90719 = CARTESIAN_POINT ( 'NONE',  ( -20.94999999999999929, 38.25685495413521409, -235.9601135138701693 ) ) ;
#90720 = LINE ( 'NONE', #175433, #251578 ) ;
#90721 = CARTESIAN_POINT ( 'NONE',  ( 22.47071067811865319, 7.720074744498043096, 0.09909245470260744093 ) ) ;
#90722 = DIRECTION ( 'NONE',  ( 1.000000000000000000, 0.000000000000000000, 0.000000000000000000 ) ) ;
#90723 = CARTESIAN_POINT ( 'NONE',  ( 22.39999999999999858, 29.50811709945092076, -252.6450601445781103 ) ) ;
#90724 = VECTOR ( 'NONE', #122558, 1000.000000000000114 ) ;
#90725 = DIRECTION ( 'NONE',  ( 0.000000000000000000, 0.000000000000000000, 1.000000000000000000 ) ) ;
#90726 = ORIENTED_EDGE ( 'NONE', *, *, #177322, .T. ) ;
#90727 = DIRECTION ( 'NONE',  ( -0.000000000000000000, 6.982962677686266711E-15, -1.000000000000000000 ) ) ;
#90728 = ORIENTED_EDGE ( 'NONE', *, *, #255105, .T. ) ;
#90729 = CARTESIAN_POINT ( 'NONE',  ( -20.64999999999999858, 73.50000000001259082, -190.2984855617622770 ) ) ;
#90730 = FACE_OUTER_BOUND ( 'NONE', #184799, .T. ) ;
#90731 = CARTESIAN_POINT ( 'NONE',  ( 21.11747605621531321, 8.778708005504054057, -79.24456316978982784 ) ) ;
#90732 = DIRECTION ( 'NONE',  ( 0.000000000000000000, 0.9999176327611370985, -0.01283462868041289687 ) ) ;
#90733 = CARTESIAN_POINT ( 'NONE',  ( 20.04142135623730070, 64.25000000001151079, -48.17310748452440805 ) ) ;
#90734 = DIRECTION ( 'NONE',  ( 1.000000000000000000, 1.110223024625155531E-13, 0.000000000000000000 ) ) ;
#90735 = DIRECTION ( 'NONE',  ( 0.000000000000000000, -0.9908441862701596881, -0.1350103645451901924 ) ) ;
#90736 = VERTEX_POINT ( 'NONE', #148195 ) ;
#90737 = CARTESIAN_POINT ( 'NONE',  ( 18.49999999999998934, 69.45000000001222418, -148.8731074845244109 ) ) ;
#90738 = FACE_OUTER_BOUND ( 'NONE', #126247, .T. ) ;
#90739 = EDGE_CURVE ( 'NONE', #210883, #171697, #197570, .T. ) ;
#90740 = CARTESIAN_POINT ( 'NONE',  ( -16.98495255085919098, 65.99443563401679569, -56.88849027830389105 ) ) ;
#90741 = CARTESIAN_POINT ( 'NONE',  ( -18.59999999999999787, 9.150000000011157653, -155.7499999999999716 ) ) ;
#90742 = AXIS2_PLACEMENT_3D ( 'NONE', #59539, #139075, #239507 ) ;
#90743 = AXIS2_PLACEMENT_3D ( 'NONE', #46426, #28195, #187252 ) ;
#90744 = DIRECTION ( 'NONE',  ( 0.000000000000000000, 0.2617529984165027912, 0.9651348961777157509 ) ) ;
#90745 = ORIENTED_EDGE ( 'NONE', *, *, #147994, .T. ) ;
#90746 = DIRECTION ( 'NONE',  ( 1.000000000000000000, 0.000000000000000000, -0.000000000000000000 ) ) ;
#90747 = DIRECTION ( 'NONE',  ( -1.000000000000000000, -0.000000000000000000, 0.000000000000000000 ) ) ;
#90748 = ORIENTED_EDGE ( 'NONE', *, *, #153013, .T. ) ;
#90749 = EDGE_LOOP ( 'NONE', ( #134433, #16934, #161383 ) ) ;
#90750 = CARTESIAN_POINT ( 'NONE',  ( -16.92563707711778065, 51.63916908934552907, -231.9165628382792761 ) ) ;
#90751 = DIRECTION ( 'NONE',  ( 0.000000000000000000, 0.2617529984165031243, 0.9651348961777157509 ) ) ;
#90752 = ADVANCED_FACE ( 'NONE', ( #49086 ), #128648, .T. ) ;
#90753 = EDGE_CURVE ( 'NONE', #22444, #20758, #66090, .T. ) ;
#90754 = ORIENTED_EDGE ( 'NONE', *, *, #181861, .T. ) ;
#90755 = AXIS2_PLACEMENT_3D ( 'NONE', #146938, #83092, #225187 ) ;
#90756 = CARTESIAN_POINT ( 'NONE',  ( -20.94999999999999929, 70.44746257310249860, -228.4383880063670347 ) ) ;
#90757 = CARTESIAN_POINT ( 'NONE',  ( 23.15000000000000213, -8.999999999988842703, -57.10603087734755690 ) ) ;
#90758 = TOROIDAL_SURFACE ( 'NONE', #128201, 0.2000000000000000111, 0.1000000000000000056 ) ;
#90759 = ORIENTED_EDGE ( 'NONE', *, *, #196399, .F. ) ;
#90760 = AXIS2_PLACEMENT_3D ( 'NONE', #48266, #148667, #127816 ) ;
#90761 = FACE_OUTER_BOUND ( 'NONE', #66063, .T. ) ;
#90762 = EDGE_CURVE ( 'NONE', #12568, #82203, #89240, .T. ) ;
#90763 = ORIENTED_EDGE ( 'NONE', *, *, #88905, .F. ) ;
#90764 = EDGE_CURVE ( 'NONE', #120409, #2697, #18523, .T. ) ;
#90765 = CYLINDRICAL_SURFACE ( 'NONE', #18293, 0.09999999999998898659 ) ;
#90766 = FACE_OUTER_BOUND ( 'NONE', #241479, .T. ) ;
#90768 = VERTEX_POINT ( 'NONE', #248580 ) ;
#90767 = CARTESIAN_POINT ( 'NONE',  ( 23.24999999999999289, 64.35000000001201670, -114.7731074845243882 ) ) ;
#90769 = DIRECTION ( 'NONE',  ( 0.000000000000000000, -1.000000000000000000, -6.982962677686266711E-15 ) ) ;
#90770 = CARTESIAN_POINT ( 'NONE',  ( -22.49806830649814415, 11.64988965485023620, -133.9225356836745107 ) ) ;
#90771 = EDGE_CURVE ( 'NONE', #130496, #24262, #122593, .T. ) ;
#90772 = CARTESIAN_POINT ( 'NONE',  ( -22.49999999999999289, 11.45898712536581066, -198.4011321578509808 ) ) ;
#90773 = DIRECTION ( 'NONE',  ( 0.000000000000000000, -0.8777080977375132376, 0.4791956752371582251 ) ) ;
#90774 = DIRECTION ( 'NONE',  ( 0.000000000000000000, -6.982962677686266711E-15, 1.000000000000000000 ) ) ;
#90775 = CARTESIAN_POINT ( 'NONE',  ( -21.55000000000000426, 7.708578643773852157, -121.6500000000000341 ) ) ;
#90776 = CARTESIAN_POINT ( 'NONE',  ( -16.79814274880124358, 66.05072745733498607, -157.3706744474764321 ) ) ;
#90778 = ORIENTED_EDGE ( 'NONE', *, *, #151864, .F. ) ;
#90777 = DIRECTION ( 'NONE',  ( -0.000000000000000000, 0.01283462868039629209, -0.9999176327611372095 ) ) ;
#90779 = ORIENTED_EDGE ( 'NONE', *, *, #213737, .F. ) ;
#90781 = CARTESIAN_POINT ( 'NONE',  ( -20.85000000000000142, 68.11287320386161070, -224.1382462126928488 ) ) ;
#90780 = CARTESIAN_POINT ( 'NONE',  ( -21.45000000000000284, 7.708578643762696636, -21.15000000000000213 ) ) ;
#90782 = EDGE_CURVE ( 'NONE', #142904, #119168, #130948, .T. ) ;
#90784 = ORIENTED_EDGE ( 'NONE', *, *, #108525, .F. ) ;
#90783 = DIRECTION ( 'NONE',  ( 0.000000000000000000, 0.000000000000000000, -1.000000000000000000 ) ) ;
#90785 = AXIS2_PLACEMENT_3D ( 'NONE', #210927, #226622, #247482 ) ;
#90786 = ORIENTED_EDGE ( 'NONE', *, *, #211589, .F. ) ;
#90787 = CARTESIAN_POINT ( 'NONE',  ( -21.53752568622134334, 1.193029429793917684, -230.4407734565325825 ) ) ;
#90789 = DIRECTION ( 'NONE',  ( -1.000000000000000000, -0.000000000000000000, 0.000000000000000000 ) ) ;
#90788 = AXIS2_PLACEMENT_3D ( 'NONE', #148950, #129367, #208901 ) ;
#90790 = TOROIDAL_SURFACE ( 'NONE', #182594, 11.90000000000000213, 0.1000000000000000056 ) ;
#90791 = ADVANCED_FACE ( 'NONE', ( #26995 ), #249865, .F. ) ;
#90792 = CARTESIAN_POINT ( 'NONE',  ( 18.59999999999999076, 69.35000000001200249, -115.3731074845243398 ) ) ;
#90793 = FACE_OUTER_BOUND ( 'NONE', #228456, .T. ) ;
#90795 = DIRECTION ( 'NONE',  ( -1.000000000000000000, -3.265361837132813093E-16, 0.000000000000000000 ) ) ;
#90794 = CIRCLE ( 'NONE', #99167, 0.09999999999998898659 ) ;
#90796 = CARTESIAN_POINT ( 'NONE',  ( -21.98333005346336577, 76.00000000001219291, -143.8971828135809972 ) ) ;
#90797 = ADVANCED_FACE ( 'NONE', ( #126047 ), #230292, .T. ) ;
#90798 = DIRECTION ( 'NONE',  ( 0.000000000000000000, 0.000000000000000000, 1.000000000000000000 ) ) ;
#90799 = ORIENTED_EDGE ( 'NONE', *, *, #81264, .F. ) ;
#90800 = ORIENTED_EDGE ( 'NONE', *, *, #154187, .F. ) ;
#90801 = CARTESIAN_POINT ( 'NONE',  ( -18.59999999999999787, 1.866714910068465239, -145.7526752462820241 ) ) ;
#90802 = TOROIDAL_SURFACE ( 'NONE', #236554, 14.20833333333334103, 0.1000000000000000056 ) ;
#90803 = VECTOR ( 'NONE', #228865, 1000.000000000000000 ) ;
#90804 = ORIENTED_EDGE ( 'NONE', *, *, #104139, .F. ) ;
#90805 = CARTESIAN_POINT ( 'NONE',  ( -18.69999999999999929, 8.000000000000000000, 1.212568896937007867 ) ) ;
#90806 = ORIENTED_EDGE ( 'NONE', *, *, #76418, .T. ) ;
#90808 = LINE ( 'NONE', #153412, #172446 ) ;
#90807 = AXIS2_PLACEMENT_3D ( 'NONE', #51328, #16114, #14834 ) ;
#90809 = AXIS2_PLACEMENT_3D ( 'NONE', #66680, #101916, #43264 ) ;
#90810 = CARTESIAN_POINT ( 'NONE',  ( -23.15000000000000213, 4.350000000011156054, -112.8500000000000369 ) ) ;
#90811 = CARTESIAN_POINT ( 'NONE',  ( 18.59999999999998366, 76.00000000001142553, -36.02310748452432421 ) ) ;
#90812 = ORIENTED_EDGE ( 'NONE', *, *, #94872, .T. ) ;
#90813 =( REPRESENTATION_RELATIONSHIP ('NONE','NONE', #36900, #168659 ) REPRESENTATION_RELATIONSHIP_WITH_TRANSFORMATION ( #3810 )SHAPE_REPRESENTATION_RELATIONSHIP( ) );
#90814 = CARTESIAN_POINT ( 'NONE',  ( -23.15000000000000213, 74.08971962618051066, -157.3917396293254285 ) ) ;
#90815 = ORIENTED_EDGE ( 'NONE', *, *, #76895, .F. ) ;
#90816 = CARTESIAN_POINT ( 'NONE',  ( -23.25000000000000355, 43.39957528361355799, -233.6562381667159798 ) ) ;
#90817 = CARTESIAN_POINT ( 'NONE',  ( 21.05000000000000071, 8.872080675389215187, -109.0210474188294114 ) ) ;
#90818 = VERTEX_POINT ( 'NONE', #6101 ) ;
#90819 = DIRECTION ( 'NONE',  ( -1.000000000000000000, 3.151514657663852580E-16, -8.547182517843351137E-17 ) ) ;
#90820 = AXIS2_PLACEMENT_3D ( 'NONE', #242111, #63470, #98716 ) ;
#90821 = ORIENTED_EDGE ( 'NONE', *, *, #254212, .F. ) ;
#90824 = ORIENTED_EDGE ( 'NONE', *, *, #7065, .F. ) ;
#90823 = DIRECTION ( 'NONE',  ( 0.000000000000000000, 1.224646799142015331E-16, 1.000000000000000000 ) ) ;
#90822 = CARTESIAN_POINT ( 'NONE',  ( -21.65000000000000213, 68.75000000001233502, -160.7731074845244166 ) ) ;
#90825 = FACE_OUTER_BOUND ( 'NONE', #40432, .T. ) ;
#90826 = TOROIDAL_SURFACE ( 'NONE', #236569, 0.6000000000000017542, 0.1000000000000000056 ) ;
#90827 = ORIENTED_EDGE ( 'NONE', *, *, #175726, .T. ) ;
#90828 = EDGE_CURVE ( 'NONE', #173825, #12431, #85117, .T. ) ;
#90829 = AXIS2_PLACEMENT_3D ( 'NONE', #214109, #173753, #35506 ) ;
#90830 = DIRECTION ( 'NONE',  ( -1.000000000000000000, 0.000000000000000000, 0.000000000000000000 ) ) ;
#90831 = VERTEX_POINT ( 'NONE', #145613 ) ;
#90833 = EDGE_CURVE ( 'NONE', #74336, #108268, #155926, .T. ) ;
#90832 = AXIS2_PLACEMENT_3D ( 'NONE', #213023, #215467, #219319 ) ;
#90834 = AXIS2_PLACEMENT_3D ( 'NONE', #251501, #194131, #95000 ) ;
#90835 = CARTESIAN_POINT ( 'NONE',  ( 20.94999999999999929, 1.115600667400684642E-11, -104.6000000000000512 ) ) ;
#90836 = VERTEX_POINT ( 'NONE', #56762 ) ;
#90838 = CIRCLE ( 'NONE', #144824, 0.1999999999999918510 ) ;
#90837 = DIRECTION ( 'NONE',  ( -0.000000000000000000, -0.9550021345545507412, 0.2965989261549202838 ) ) ;
#90839 = EDGE_CURVE ( 'NONE', #230182, #214984, #212041, .T. ) ;
#90840 = CARTESIAN_POINT ( 'NONE',  ( 21.13461538461538325, 8.885417037985616773, -179.8499999999999943 ) ) ;
#90841 = ADVANCED_FACE ( 'NONE', ( #175484 ), #231599, .F. ) ;
#90842 = CARTESIAN_POINT ( 'NONE',  ( -18.50000000000000000, 29.81973725181492085, -263.0247672247078867 ) ) ;
#90843 = CARTESIAN_POINT ( 'NONE',  ( -16.89318236219977010, 66.04846474213692886, -123.8782371166302312 ) ) ;
#90845 = EDGE_LOOP ( 'NONE', ( #189053, #246978, #69316, #42058, #200021, #215131, #44409, #64583, #114618, #72623 ) ) ;
#90844 = EDGE_CURVE ( 'NONE', #9861, #77283, #218220, .T. ) ;
#90846 = CARTESIAN_POINT ( 'NONE',  ( -18.59999999999999787, 68.97833521811159585, -65.68954208262705663 ) ) ;
#90847 = FACE_OUTER_BOUND ( 'NONE', #56709, .T. ) ;
#90848 = LINE ( 'NONE', #12630, #55381 ) ;
#90849 = ADVANCED_FACE ( 'NONE', ( #115480 ), #254934, .F. ) ;
#90850 = ORIENTED_EDGE ( 'NONE', *, *, #163109, .T. ) ;
#90851 = DIRECTION ( 'NONE',  ( 0.000000000000000000, 0.000000000000000000, -1.000000000000000000 ) ) ;
#90854 = ADVANCED_FACE ( 'NONE', ( #76340 ), #52939, .T. ) ;
#90853 = EDGE_LOOP ( 'NONE', ( #120376, #51958, #147983, #231023 ) ) ;
#90852 = AXIS2_PLACEMENT_3D ( 'NONE', #87619, #147610, #186759 ) ;
#90856 = AXIS2_PLACEMENT_3D ( 'NONE', #136198, #20152, #38420 ) ;
#90855 = DIRECTION ( 'NONE',  ( 0.000000000000000000, -1.265107689135680095E-16, 1.000000000000000000 ) ) ;
#90857 = ORIENTED_EDGE ( 'NONE', *, *, #214227, .F. ) ;
#90858 = DIRECTION ( 'NONE',  ( 0.000000000000000000, 0.9915357197604849349, -0.1298341882520056834 ) ) ;
#90859 = FACE_OUTER_BOUND ( 'NONE', #124003, .T. ) ;
#90860 = EDGE_CURVE ( 'NONE', #185160, #162338, #32128, .T. ) ;
#90862 = ORIENTED_EDGE ( 'NONE', *, *, #119316, .T. ) ;
#90861 = CARTESIAN_POINT ( 'NONE',  ( -16.83233564386408787, 44.25808114483436384, -235.2656807595939767 ) ) ;
#90863 = LINE ( 'NONE', #189977, #208318 ) ;
#90864 = VERTEX_POINT ( 'NONE', #174224 ) ;
#90865 = CARTESIAN_POINT ( 'NONE',  ( -20.99780126800958513, 36.04544038259461303, -236.0569647481114259 ) ) ;
#90866 = AXIS2_PLACEMENT_3D ( 'NONE', #209638, #132676, #173129 ) ;
#90867 = EDGE_CURVE ( 'NONE', #147247, #133820, #80858, .T. ) ;
#90868 = VECTOR ( 'NONE', #26525, 1000.000000000000000 ) ;
#90869 = ORIENTED_EDGE ( 'NONE', *, *, #69215, .F. ) ;
#90870 = CARTESIAN_POINT ( 'NONE',  ( 21.07094088545303734, 69.67983277809619835, -203.6220011870766200 ) ) ;
#90871 = LINE ( 'NONE', #68757, #119043 ) ;
#90872 = AXIS2_PLACEMENT_3D ( 'NONE', #144917, #165809, #22446 ) ;
#90874 = VERTEX_POINT ( 'NONE', #112925 ) ;
#90873 = ADVANCED_FACE ( 'NONE', ( #75111 ), #116770, .T. ) ;
#90876 = ADVANCED_FACE ( 'NONE', ( #135025 ), #251125, .F. ) ;
#90875 = CARTESIAN_POINT ( 'NONE',  ( 20.94999999999999574, 77.34908441863890971, -95.03660852097883094 ) ) ;
#90877 = ORIENTED_EDGE ( 'NONE', *, *, #103176, .T. ) ;
#90878 = AXIS2_PLACEMENT_3D ( 'NONE', #137129, #236216, #40635 ) ;
#90879 = EDGE_CURVE ( 'NONE', #183416, #20030, #13577, .T. ) ;
#90880 = CARTESIAN_POINT ( 'NONE',  ( 15.66039659514495774, 9.360749169926259938, -117.8145701406072874 ) ) ;
#90881 = CARTESIAN_POINT ( 'NONE',  ( 20.04142135623730070, 64.35000000001254250, -182.2731074845244450 ) ) ;
#90882 = EDGE_CURVE ( 'NONE', #214712, #108130, #60200, .T. ) ;
#90883 = EDGE_CURVE ( 'NONE', #101793, #62395, #210076, .T. ) ;
#90884 = CIRCLE ( 'NONE', #170059, 0.1000000000000002692 ) ;
#90887 = ORIENTED_EDGE ( 'NONE', *, *, #8112, .T. ) ;
#90886 = ORIENTED_EDGE ( 'NONE', *, *, #93092, .F. ) ;
#90885 = CARTESIAN_POINT ( 'NONE',  ( -20.64999999999999858, 85.50000000001251976, -179.9170766071767389 ) ) ;
#90888 = DIRECTION ( 'NONE',  ( 0.000000000000000000, 0.2128009952263403282, -0.9770955615653358350 ) ) ;
#90889 = AXIS2_PLACEMENT_3D ( 'NONE', #157098, #254834, #76246 ) ;
#90890 = CARTESIAN_POINT ( 'NONE',  ( -18.59999999999999787, 9.350000000011156942, -179.7499999999999716 ) ) ;
#90891 = CIRCLE ( 'NONE', #116051, 11.64999999999999325 ) ;
#90893 = DIRECTION ( 'NONE',  ( -1.000000000000000000, -0.000000000000000000, -0.000000000000000000 ) ) ;
#90892 = DIRECTION ( 'NONE',  ( 0.000000000000000000, -1.000000000000000000, 6.308085367188393199E-16 ) ) ;
#90894 = DIRECTION ( 'NONE',  ( 0.000000000000000000, 0.4930308989875575865, 0.8700118002898125091 ) ) ;
#90895 = CARTESIAN_POINT ( 'NONE',  ( 21.05000000000000071, 76.00000000001165290, -69.52310748452431710 ) ) ;
#90896 = CARTESIAN_POINT ( 'NONE',  ( 23.14999999999999858, 53.86595165227826243, -236.3638196928718855 ) ) ;
#90897 = VECTOR ( 'NONE', #131613, 1000.000000000000227 ) ;
#90898 = DIRECTION ( 'NONE',  ( -1.000000000000000000, 0.000000000000000000, -0.000000000000000000 ) ) ;
#90899 = B_SPLINE_CURVE_WITH_KNOTS ( 'NONE', 3,
 ( #20861, #3840, #165493, #202042, #183762, #1246, #25979, #119966 ),
 .UNSPECIFIED., .F., .F.,
 ( 4, 2, 2, 4 ),
 ( 0.000000000000000000, 9.550056980124262422E-05, 0.0001910011396024852484, 0.0003820022792049918557 ),
 .UNSPECIFIED. ) ;
#90900 = ORIENTED_EDGE ( 'NONE', *, *, #152044, .F. ) ;
#90901 = ORIENTED_EDGE ( 'NONE', *, *, #110300, .F. ) ;
#90902 = CARTESIAN_POINT ( 'NONE',  ( 21.05000000000000071, 0.000000000000000000, 0.000000000000000000 ) ) ;
#90904 = VERTEX_POINT ( 'NONE', #58059 ) ;
#90903 = CARTESIAN_POINT ( 'NONE',  ( -18.34374000495059676, 33.92263863280957281, -235.0698407953532296 ) ) ;
#90905 = ORIENTED_EDGE ( 'NONE', *, *, #53689, .T. ) ;
#90906 = LINE ( 'NONE', #72657, #243410 ) ;
#90907 = ORIENTED_EDGE ( 'NONE', *, *, #17235, .T. ) ;
#90908 = DIRECTION ( 'NONE',  ( 0.000000000000000000, 0.000000000000000000, -1.000000000000000000 ) ) ;
#90909 = VECTOR ( 'NONE', #196921, 1000.000000000000000 ) ;
#90910 = VERTEX_POINT ( 'NONE', #80177 ) ;
#90911 = CARTESIAN_POINT ( 'NONE',  ( -16.89268316805465986, 66.04827818677006235, -149.1673550059788909 ) ) ;
#90912 = DIRECTION ( 'NONE',  ( 1.000000000000000000, -0.000000000000000000, -0.000000000000000000 ) ) ;
#90914 = ORIENTED_EDGE ( 'NONE', *, *, #256288, .T. ) ;
#90913 = ORIENTED_EDGE ( 'NONE', *, *, #97469, .T. ) ;
#90915 = ORIENTED_EDGE ( 'NONE', *, *, #193075, .T. ) ;
#90916 = ORIENTED_EDGE ( 'NONE', *, *, #110149, .F. ) ;
#90917 = ORIENTED_EDGE ( 'NONE', *, *, #179878, .F. ) ;
#90918 = FACE_OUTER_BOUND ( 'NONE', #50905, .T. ) ;
#90919 = DIRECTION ( 'NONE',  ( 0.000000000000000000, -0.8700118002898354908, 0.4930308989875170078 ) ) ;
#90920 = CARTESIAN_POINT ( 'NONE',  ( -14.56336952470180002, 9.446645344706398717, -185.9108064561001470 ) ) ;
#90922 = ORIENTED_EDGE ( 'NONE', *, *, #240187, .T. ) ;
#90921 = CARTESIAN_POINT ( 'NONE',  ( -23.15000000000000213, 49.36776662947724503, -253.7196102226803021 ) ) ;
#90923 = FACE_OUTER_BOUND ( 'NONE', #221137, .T. ) ;
#90924 = FACE_OUTER_BOUND ( 'NONE', #236599, .T. ) ;
#90926 = VERTEX_POINT ( 'NONE', #200171 ) ;
#90925 = DIRECTION ( 'NONE',  ( 0.000000000000000000, 0.000000000000000000, 1.000000000000000000 ) ) ;
#90927 = DIRECTION ( 'NONE',  ( 1.000000000000000000, 0.000000000000000000, 0.000000000000000000 ) ) ;
#90928 = ORIENTED_EDGE ( 'NONE', *, *, #229534, .F. ) ;
#90929 = FACE_OUTER_BOUND ( 'NONE', #249776, .T. ) ;
#90930 = ORIENTED_EDGE ( 'NONE', *, *, #86878, .T. ) ;
#90931 = DIRECTION ( 'NONE',  ( 0.000000000000000000, -7.147358527629762208E-15, 1.000000000000000000 ) ) ;
#90933 = EDGE_CURVE ( 'NONE', #140695, #35438, #60012, .T. ) ;
#90932 = FACE_OUTER_BOUND ( 'NONE', #48808, .T. ) ;
#90934 = VERTEX_POINT ( 'NONE', #39834 ) ;
#90935 = CIRCLE ( 'NONE', #61723, 0.9750000000000036415 ) ;
#90936 = CIRCLE ( 'NONE', #136717, 2.699999999999999289 ) ;
#90938 = DIRECTION ( 'NONE',  ( 0.000000000000000000, -0.9651348961777157509, 0.2617529984165031243 ) ) ;
#90937 = DIRECTION ( 'NONE',  ( 0.000000000000000000, -1.000000000000000000, -6.982962677686266711E-15 ) ) ;
#90939 = EDGE_CURVE ( 'NONE', #203639, #218161, #139296, .T. ) ;
#90940 = CIRCLE ( 'NONE', #145095, 0.1000000000000052097 ) ;
#90941 = DIRECTION ( 'NONE',  ( 2.952720810173289112E-16, 0.4088369013363280513, -0.9126074666063769270 ) ) ;
#90942 = DIRECTION ( 'NONE',  ( 0.000000000000000000, 0.000000000000000000, -1.000000000000000000 ) ) ;
#90943 = DIRECTION ( 'NONE',  ( 0.000000000000000000, -0.9908441862701420355, -0.1350103645453197554 ) ) ;
#90944 = VERTEX_POINT ( 'NONE', #138862 ) ;
#90945 = ORIENTED_EDGE ( 'NONE', *, *, #163347, .T. ) ;
#90946 = EDGE_CURVE ( 'NONE', #100003, #54863, #218404, .T. ) ;
#90947 = FACE_OUTER_BOUND ( 'NONE', #144268, .T. ) ;
#90948 = B_SPLINE_CURVE_WITH_KNOTS ( 'NONE', 3,
 ( #42643, #186008, #7364, #123470, #86879, #103877, #3504, #183451, #166477, #245989 ),
 .UNSPECIFIED., .F., .F.,
 ( 4, 2, 2, 2, 4 ),
 ( 0.000000000000000000, 0.0001660831991682258321, 0.0002491247987523387752, 0.0002906455985443952197, 0.0003321663983364516641 ),
 .UNSPECIFIED. ) ;
#90950 = EDGE_CURVE ( 'NONE', #107898, #245381, #41115, .T. ) ;
#90949 = DIRECTION ( 'NONE',  ( 0.000000000000000000, 0.04908394489122551441, 0.9987946567507833828 ) ) ;
#90951 = ORIENTED_EDGE ( 'NONE', *, *, #70378, .T. ) ;
#90952 = FACE_OUTER_BOUND ( 'NONE', #177549, .T. ) ;
#90953 = EDGE_LOOP ( 'NONE', ( #82516, #95895, #102744, #167968, #133903, #167596, #57451, #241078 ) ) ;
#90954 = DIRECTION ( 'NONE',  ( 0.000000000000000000, 0.2617529984165152257, 0.9651348961777124202 ) ) ;
#90955 = DIRECTION ( 'NONE',  ( -1.000000000000000000, 0.000000000000000000, 0.000000000000000000 ) ) ;
#90956 = DIRECTION ( 'NONE',  ( 1.000000000000000000, 2.952720810173289112E-16, -0.000000000000000000 ) ) ;
#90957 = AXIS2_PLACEMENT_3D ( 'NONE', #82653, #1841, #257412 ) ;
#90958 = ORIENTED_EDGE ( 'NONE', *, *, #13878, .T. ) ;
#90959 = VECTOR ( 'NONE', #54839, 1000.000000000000000 ) ;
#90960 = DIRECTION ( 'NONE',  ( 1.000000000000000000, 0.000000000000000000, 0.000000000000000000 ) ) ;
#90961 = VERTEX_POINT ( 'NONE', #645 ) ;
#90962 = VECTOR ( 'NONE', #239747, 1000.000000000000227 ) ;
#90963 = ORIENTED_EDGE ( 'NONE', *, *, #111371, .F. ) ;
#90964 = EDGE_CURVE ( 'NONE', #53966, #173788, #239294, .T. ) ;
#90965 = EDGE_LOOP ( 'NONE', ( #182079, #19272, #251202, #160835 ) ) ;
#90966 = CARTESIAN_POINT ( 'NONE',  ( 22.59999999999999432, 64.25043287652275126, -136.6239658536231047 ) ) ;
#90967 = CARTESIAN_POINT ( 'NONE',  ( -21.14999999999999858, 79.33069327855442054, -236.1318330389568985 ) ) ;
#90968 = CARTESIAN_POINT ( 'NONE',  ( -21.08134388332232589, 0.07581891751813471525, -127.6653194194820600 ) ) ;
#90969 = DIRECTION ( 'NONE',  ( 0.000000000000000000, 0.000000000000000000, 1.000000000000000000 ) ) ;
#90970 = DIRECTION ( 'NONE',  ( 1.000000000000000000, 3.265361837132813093E-16, -0.000000000000000000 ) ) ;
#90972 = DIRECTION ( 'NONE',  ( 0.000000000000000000, -0.000000000000000000, 1.000000000000000000 ) ) ;
#90971 = DIRECTION ( 'NONE',  ( 1.000000000000000000, 0.000000000000000000, 0.000000000000000000 ) ) ;
#90974 = ORIENTED_EDGE ( 'NONE', *, *, #74811, .T. ) ;
#90973 = CARTESIAN_POINT ( 'NONE',  ( 20.99999999999999645, 9.750000000011137757, -79.65000000000004832 ) ) ;
#90975 = CARTESIAN_POINT ( 'NONE',  ( 18.52928932188133970, 15.31067260432008403, -222.9956721508274029 ) ) ;
#90976 = ORIENTED_EDGE ( 'NONE', *, *, #47881, .T. ) ;
#90977 = ORIENTED_EDGE ( 'NONE', *, *, #149438, .F. ) ;
#90978 = ORIENTED_EDGE ( 'NONE', *, *, #131986, .F. ) ;
#90979 = DIRECTION ( 'NONE',  ( 1.000000000000000000, -7.125593699324843413E-30, 1.020425574104004196E-15 ) ) ;
#90980 = CARTESIAN_POINT ( 'NONE',  ( -16.93339986808596365, 10.00510392857707664, -46.06599367181285487 ) ) ;
#90981 = LINE ( 'NONE', #113121, #162693 ) ;
#90982 = ADVANCED_FACE ( 'NONE', ( #220995 ), #218417, .T. ) ;
#90983 = DIRECTION ( 'NONE',  ( 0.000000000000000000, 0.000000000000000000, 1.000000000000000000 ) ) ;
#90984 = AXIS2_PLACEMENT_3D ( 'NONE', #180794, #140359, #102494 ) ;
#90985 = EDGE_CURVE ( 'NONE', #84702, #216494, #76962, .T. ) ;
#90986 = TOROIDAL_SURFACE ( 'NONE', #86861, 0.2000000000000000111, 0.1000000000000000056 ) ;
#90987 = AXIS2_PLACEMENT_3D ( 'NONE', #62856, #142389, #232848 ) ;
#90988 = DIRECTION ( 'NONE',  ( 0.000000000000000000, -0.1350103645451807555, -0.9908441862701610203 ) ) ;
#90989 = VERTEX_POINT ( 'NONE', #102307 ) ;
#90990 = ORIENTED_EDGE ( 'NONE', *, *, #116594, .F. ) ;
#90991 = DIRECTION ( 'NONE',  ( 0.000000000000000000, 0.4999999999999689138, 0.8660254037844565822 ) ) ;
#90992 = ORIENTED_EDGE ( 'NONE', *, *, #249540, .T. ) ;
#90993 = DIRECTION ( 'NONE',  ( -0.000000000000000000, 1.000000000000000000, 0.000000000000000000 ) ) ;
#90994 = DIRECTION ( 'NONE',  ( 1.000000000000000000, 0.000000000000000000, 0.000000000000000000 ) ) ;
#90995 = ORIENTED_EDGE ( 'NONE', *, *, #112856, .F. ) ;
#90997 = CARTESIAN_POINT ( 'NONE',  ( 23.25000000000000000, -8.999999999988842703, -157.6060308773475640 ) ) ;
#90996 = TOROIDAL_SURFACE ( 'NONE', #124318, 11.70000000000000639, 0.1000000000000000056 ) ;
#90998 = DIRECTION ( 'NONE',  ( -1.000000000000000000, -0.000000000000000000, -0.000000000000000000 ) ) ;
#90999 = FACE_OUTER_BOUND ( 'NONE', #25339, .T. ) ;
#91001 = ADVANCED_FACE ( 'NONE', ( #140167 ), #98444, .T. ) ;
#91000 = CARTESIAN_POINT ( 'NONE',  ( 21.05000000000000071, 65.27628289530476025, -157.8731074845244393 ) ) ;
#91002 = ORIENTED_EDGE ( 'NONE', *, *, #177946, .T. ) ;
#91003 = DIRECTION ( 'NONE',  ( 0.000000000000000000, 0.3738317757009942399, -0.9274965247785252886 ) ) ;
#91004 = FACE_OUTER_BOUND ( 'NONE', #119525, .T. ) ;
#91005 = DIRECTION ( 'NONE',  ( 0.000000000000000000, 0.9915357197604982575, -0.1298341882519033486 ) ) ;
#91006 = EDGE_CURVE ( 'NONE', #239652, #96700, #22825, .T. ) ;
#91007 = CARTESIAN_POINT ( 'NONE',  ( -23.25000000000000000, -0.09999999998884338825, -55.35042919245524473 ) ) ;
#91008 = DIRECTION ( 'NONE',  ( 0.000000000000000000, 0.000000000000000000, -1.000000000000000000 ) ) ;
#91009 = ADVANCED_FACE ( 'NONE', ( #178051 ), #210258, .F. ) ;
#91010 = AXIS2_PLACEMENT_3D ( 'NONE', #117480, #217829, #236133 ) ;
#91011 = DIRECTION ( 'NONE',  ( -1.000000000000000000, 0.000000000000000000, 0.000000000000000000 ) ) ;
#91012 = CIRCLE ( 'NONE', #203442, 12.87499999999999822 ) ;
#91013 = CIRCLE ( 'NONE', #99175, 0.9750000000000036415 ) ;
#91014 = ORIENTED_EDGE ( 'NONE', *, *, #163624, .T. ) ;
#91015 = TOROIDAL_SURFACE ( 'NONE', #45215, 4.149999999999999467, 0.1000000000000000056 ) ;
#91016 = CARTESIAN_POINT ( 'NONE',  ( -22.00356870141341759, 68.74575763752174851, -136.5231074845243882 ) ) ;
#91017 = VERTEX_POINT ( 'NONE', #81463 ) ;
#91018 = PLANE ( 'NONE',  #14010 ) ;
#91019 = EDGE_CURVE ( 'NONE', #132009, #109794, #110274, .T. ) ;
#91020 = DIRECTION ( 'NONE',  ( 0.000000000000000000, 0.000000000000000000, -1.000000000000000000 ) ) ;
#91021 = CARTESIAN_POINT ( 'NONE',  ( -16.87372397896796272, 66.11940046337004162, -82.67238297448861317 ) ) ;
#91022 = CARTESIAN_POINT ( 'NONE',  ( 23.24999999999999645, 8.822561741677553471, -143.2500000000000284 ) ) ;
#91023 = SPHERICAL_SURFACE ( 'NONE', #63238, 0.1000000000000000056 ) ;
#91024 = CARTESIAN_POINT ( 'NONE',  ( -23.25000000000000000, 6.933893972137497030, -204.7856458343735255 ) ) ;
#91025 = AXIS2_PLACEMENT_3D ( 'NONE', #9263, #10563, #185337 ) ;
#91026 = ORIENTED_EDGE ( 'NONE', *, *, #232511, .F. ) ;
#91027 = DIRECTION ( 'NONE',  ( -1.000000000000000000, 3.448943450116724061E-16, 6.438528483529607644E-16 ) ) ;
#91028 = EDGE_CURVE ( 'NONE', #240784, #162878, #190946, .T. ) ;
#91029 = DIRECTION ( 'NONE',  ( -1.000000000000000000, 0.000000000000000000, -0.000000000000000000 ) ) ;
#91030 = CARTESIAN_POINT ( 'NONE',  ( 18.59999999999999787, 1.115600667400684642E-11, -134.0000000000000000 ) ) ;
#91031 = CARTESIAN_POINT ( 'NONE',  ( -23.25000000000000000, 6.982009704867601307, -204.6961521182562649 ) ) ;
#91032 = AXIS2_PLACEMENT_3D ( 'NONE', #160396, #42997, #3862 ) ;
#91033 = DIRECTION ( 'NONE',  ( -0.7071067811865474617, -0.6909108974501236844, -0.1504730267678055788 ) ) ;
#91034 = AXIS2_PLACEMENT_3D ( 'NONE', #17211, #97984, #176289 ) ;
#91035 = VECTOR ( 'NONE', #189199, 1000.000000000000000 ) ;
#91037 = ORIENTED_EDGE ( 'NONE', *, *, #108531, .F. ) ;
#91036 = VECTOR ( 'NONE', #56286, 1000.000000000000114 ) ;
#91038 = ORIENTED_EDGE ( 'NONE', *, *, #47253, .F. ) ;
#91039 = FACE_OUTER_BOUND ( 'NONE', #4673, .T. ) ;
#91040 = AXIS2_PLACEMENT_3D ( 'NONE', #139645, #195819, #155421 ) ;
#91041 = CARTESIAN_POINT ( 'NONE',  ( 21.05000000000000071, 2.817198581588411077, -208.4716308468294130 ) ) ;
#91042 = FACE_OUTER_BOUND ( 'NONE', #26140, .T. ) ;
#91043 = CARTESIAN_POINT ( 'NONE',  ( -22.00356870141227006, 68.74575763752082480, -170.0231074845244450 ) ) ;
#91044 = VECTOR ( 'NONE', #201543, 1000.000000000000114 ) ;
#91045 = VERTEX_POINT ( 'NONE', #59328 ) ;
#91046 = LINE ( 'NONE', #132761, #1397 ) ;
#91047 = CONTEXT_DEPENDENT_SHAPE_REPRESENTATION ( #14327, #20518 ) ;
#91048 = CARTESIAN_POINT ( 'NONE',  ( 18.49999999999999289, 68.87972903831379767, -32.36354444268504693 ) ) ;
#91049 = ORIENTED_EDGE ( 'NONE', *, *, #126555, .T. ) ;
#91050 = CARTESIAN_POINT ( 'NONE',  ( 18.59999999999999432, 74.36282728704149747, -91.44095411905230719 ) ) ;
#91051 = PRODUCT_DEFINITION_SHAPE ( 'NONE', 'NONE',  #29336 ) ;
#91052 =( GEOMETRIC_REPRESENTATION_CONTEXT ( 3 ) GLOBAL_UNCERTAINTY_ASSIGNED_CONTEXT ( ( #158863 ) ) GLOBAL_UNIT_ASSIGNED_CONTEXT ( ( #45316, #247355, #149575 ) ) REPRESENTATION_CONTEXT ( 'NONE', 'WORKASPACE' ) );
#91053 = VECTOR ( 'NONE', #187905, 1000.000000000000000 ) ;
#91054 = VECTOR ( 'NONE', #230645, 1000.000000000000000 ) ;
#91055 = ORIENTED_EDGE ( 'NONE', *, *, #31803, .F. ) ;
#91056 = ORIENTED_EDGE ( 'NONE', *, *, #188648, .T. ) ;
#91057 = ORIENTED_EDGE ( 'NONE', *, *, #200445, .F. ) ;
#91058 = CARTESIAN_POINT ( 'NONE',  ( -16.97683809663752186, 9.950000000011138823, -154.0976359818037054 ) ) ;
#91059 = LINE ( 'NONE', #109316, #149275 ) ;
#91060 = CYLINDRICAL_SURFACE ( 'NONE', #173915, 0.5000000000000004441 ) ;
#91062 = AXIS2_PLACEMENT_3D ( 'NONE', #166075, #83889, #243000 ) ;
#91061 = DIRECTION ( 'NONE',  ( 0.000000000000000000, 0.000000000000000000, -1.000000000000000000 ) ) ;
#91063 = DIRECTION ( 'NONE',  ( 0.000000000000000000, 1.000000000000000000, 0.000000000000000000 ) ) ;
#91064 = CARTESIAN_POINT ( 'NONE',  ( 20.94999999999999574, 77.85102823015292017, -124.8691942151017855 ) ) ;
#91065 = AXIS2_PLACEMENT_3D ( 'NONE', #211401, #151443, #53612 ) ;
#91067 = CARTESIAN_POINT ( 'NONE',  ( -23.25000000000000000, 1.115600667400684642E-11, -100.5000000000000426 ) ) ;
#91066 = CARTESIAN_POINT ( 'NONE',  ( -23.25000000000000000, 11.75000000001115552, -167.5000000000000284 ) ) ;
#91068 = DIRECTION ( 'NONE',  ( 0.000000000000000000, -0.9908441862701420355, -0.1350103645453197554 ) ) ;
#91069 = ADVANCED_FACE ( 'NONE', ( #43665 ), #202728, .F. ) ;
#91070 = CIRCLE ( 'NONE', #174322, 0.1000000000000028644 ) ;
#91071 = CARTESIAN_POINT ( 'NONE',  ( 21.06086055315984140, 22.02847682286311937, -231.7596878716482820 ) ) ;
#91072 = CARTESIAN_POINT ( 'NONE',  ( -18.40000000000000213, 11.47867410001105881, -91.22530678365944823 ) ) ;
#91073 = CARTESIAN_POINT ( 'NONE',  ( 18.59999999999999787, 77.35494420175977837, -241.6200040285045532 ) ) ;
#91074 = EDGE_LOOP ( 'NONE', ( #65469, #179845, #42766 ) ) ;
#91075 = CARTESIAN_POINT ( 'NONE',  ( -18.31331870001055862, -9.536294719180791191, -40.36857869098546558 ) ) ;
#91076 = DIRECTION ( 'NONE',  ( -1.000000000000000000, 0.000000000000000000, 0.000000000000000000 ) ) ;
#91077 = DIRECTION ( 'NONE',  ( 0.000000000000000000, 0.7397360091702755991, -0.6728971962616832059 ) ) ;
#91078 = CIRCLE ( 'NONE', #161833, 1.749999999999999778 ) ;
#91079 = CARTESIAN_POINT ( 'NONE',  ( 22.50000000000000000, 76.00000000001267608, -203.5231074845243597 ) ) ;
#91080 = CARTESIAN_POINT ( 'NONE',  ( -33.72168855820452649, 64.52683809664972614, -145.7731074845244450 ) ) ;
#91082 = ADVANCED_FACE ( 'NONE', ( #4518 ), #10963, .F. ) ;
#91081 = CARTESIAN_POINT ( 'NONE',  ( 21.07928932188134397, 6.328516656404459262, -66.90110485434564680 ) ) ;
#91083 = VECTOR ( 'NONE', #107292, 1000.000000000000000 ) ;
#91084 = VERTEX_POINT ( 'NONE', #50077 ) ;
#91085 = ORIENTED_EDGE ( 'NONE', *, *, #174180, .T. ) ;
#91086 = ADVANCED_FACE ( 'NONE', ( #48791 ), #26688, .F. ) ;
#91088 = EDGE_CURVE ( 'NONE', #97606, #21107, #35319, .T. ) ;
#91087 = CIRCLE ( 'NONE', #103700, 0.1000000000000050293 ) ;
#91089 = AXIS2_PLACEMENT_3D ( 'NONE', #47712, #218979, #199449 ) ;
#91090 = LINE ( 'NONE', #145913, #130364 ) ;
#91091 = CIRCLE ( 'NONE', #228668, 3.899999999999993694 ) ;
#91092 = VERTEX_POINT ( 'NONE', #7093 ) ;
#91093 = CARTESIAN_POINT ( 'NONE',  ( 18.39999999999999858, 85.50000000001209344, -129.9229180933022576 ) ) ;
#91094 = ORIENTED_EDGE ( 'NONE', *, *, #94922, .F. ) ;
#91095 = EDGE_CURVE ( 'NONE', #241360, #59439, #126853, .T. ) ;
#91096 = VERTEX_POINT ( 'NONE', #86610 ) ;
#91097 = CARTESIAN_POINT ( 'NONE',  ( -18.59999999999999787, 11.64999999999999680, -12.25000000000000000 ) ) ;
#91098 = DIRECTION ( 'NONE',  ( 0.000000000000000000, -6.982962677686266711E-15, 1.000000000000000000 ) ) ;
#91100 = CARTESIAN_POINT ( 'NONE',  ( 21.05000000000000071, 67.22371710471941242, -94.46447848938342418 ) ) ;
#91099 = VECTOR ( 'NONE', #54535, 1000.000000000000000 ) ;
#91101 = CARTESIAN_POINT ( 'NONE',  ( 18.39999999999999503, 11.47316190336248454, -12.65000000000000213 ) ) ;
#91102 = DIRECTION ( 'NONE',  ( 1.000000000000000000, 0.000000000000000000, 0.000000000000000000 ) ) ;
#91103 = DIRECTION ( 'NONE',  ( -1.000000000000000000, 0.000000000000000000, 0.000000000000000000 ) ) ;
#91104 = CARTESIAN_POINT ( 'NONE',  ( 23.14999999999999858, 71.00000000001223555, -148.9283735034374843 ) ) ;
#91105 = CARTESIAN_POINT ( 'NONE',  ( 21.05000000000000071, -8.999999999988844479, -110.3939691226524786 ) ) ;
#91107 = ORIENTED_EDGE ( 'NONE', *, *, #257731, .T. ) ;
#91106 = DIRECTION ( 'NONE',  ( 0.000000000000000000, 0.000000000000000000, -1.000000000000000000 ) ) ;
#91109 = FACE_OUTER_BOUND ( 'NONE', #136764, .T. ) ;
#91108 = CARTESIAN_POINT ( 'NONE',  ( -20.85000000000000142, 80.69087520990402140, -192.8618289658565743 ) ) ;
#91110 = ORIENTED_EDGE ( 'NONE', *, *, #183934, .F. ) ;
#91112 = ORIENTED_EDGE ( 'NONE', *, *, #211141, .F. ) ;
#91111 = CARTESIAN_POINT ( 'NONE',  ( -23.25000000000000000, 2.600000000000000089, -13.22462192276210224 ) ) ;
#91113 = VERTEX_POINT ( 'NONE', #206586 ) ;
#91114 = DIRECTION ( 'NONE',  ( 1.000000000000000000, 0.000000000000000000, 0.000000000000000000 ) ) ;
#91115 = SPHERICAL_SURFACE ( 'NONE', #225974, 0.1000000000000000056 ) ;
#91116 = ADVANCED_FACE ( 'NONE', ( #204011 ), #151820, .T. ) ;
#91118 = EDGE_CURVE ( 'NONE', #16708, #255384, #105978, .T. ) ;
#91117 = CARTESIAN_POINT ( 'NONE',  ( -17.01825945287482966, 65.95000000001159890, -56.87310748452438958 ) ) ;
#91119 = LINE ( 'NONE', #247626, #47443 ) ;
#91120 = DIRECTION ( 'NONE',  ( -3.265361837132813093E-16, -0.4088369013363280513, 0.9126074666063769270 ) ) ;
#91121 = CARTESIAN_POINT ( 'NONE',  ( -21.44999999999999929, 7.350000000011155166, -188.6499999999999488 ) ) ;
#91122 = DIRECTION ( 'NONE',  ( 1.224646799147353207E-16, 1.000000000000000000, 0.000000000000000000 ) ) ;
#91123 = DIRECTION ( 'NONE',  ( 1.000000000000000000, -0.000000000000000000, 0.000000000000000000 ) ) ;
#91124 = ADVANCED_FACE ( 'NONE', ( #87894 ), #172694, .T. ) ;
#91125 = CARTESIAN_POINT ( 'NONE',  ( 18.59999999999997655, 77.16412189325330928, -128.6082593989527254 ) ) ;
#91126 = AXIS2_PLACEMENT_3D ( 'NONE', #13144, #212629, #193068 ) ;
#91127 = VERTEX_POINT ( 'NONE', #167487 ) ;
#91128 = VERTEX_POINT ( 'NONE', #248285 ) ;
#91129 = AXIS2_PLACEMENT_3D ( 'NONE', #28779, #249079, #165697 ) ;
#91130 = CARTESIAN_POINT ( 'NONE',  ( 17.23472005113827166, 65.69211804551174794, -181.4765306244557621 ) ) ;
#91131 = EDGE_LOOP ( 'NONE', ( #136527, #2348, #166122, #43698 ) ) ;
#91132 = CYLINDRICAL_SURFACE ( 'NONE', #88273, 0.09999999999999939493 ) ;
#91133 = VERTEX_POINT ( 'NONE', #129624 ) ;
#91134 = DIRECTION ( 'NONE',  ( 1.000000000000000000, 0.000000000000000000, 0.000000000000000000 ) ) ;
#91135 = CIRCLE ( 'NONE', #236875, 12.87499999999999822 ) ;
#91136 = CARTESIAN_POINT ( 'NONE',  ( -20.64999999999999858, 73.60000000001157616, -56.29848556176223440 ) ) ;
#91137 = FACE_OUTER_BOUND ( 'NONE', #230847, .T. ) ;
#91138 = CARTESIAN_POINT ( 'NONE',  ( -21.04999999999999716, 1.434589632855153063, -230.7797184520195231 ) ) ;
#91139 = DIRECTION ( 'NONE',  ( -1.000000000000000000, 0.000000000000000000, 0.000000000000000000 ) ) ;
#91140 = EDGE_LOOP ( 'NONE', ( #117680, #59841, #209914, #174985 ) ) ;
#91141 = LINE ( 'NONE', #170740, #53602 ) ;
#91142 = AXIS2_PLACEMENT_3D ( 'NONE', #21316, #23885, #239050 ) ;
#91143 = CIRCLE ( 'NONE', #240990, 7.800000000000001599 ) ;
#91144 = DIRECTION ( 'NONE',  ( 1.000000000000000000, 0.000000000000000000, 0.000000000000000000 ) ) ;
#91146 = CIRCLE ( 'NONE', #120410, 0.09999999999999939493 ) ;
#91145 = DIRECTION ( 'NONE',  ( 0.000000000000000000, -0.1335171055202901413, 0.9910465087640860649 ) ) ;
#91147 = DIRECTION ( 'NONE',  ( 1.000000000000000000, 0.000000000000000000, 0.000000000000000000 ) ) ;
#91148 = DIRECTION ( 'NONE',  ( 0.000000000000000000, 0.2617529984165503087, 0.9651348961777028723 ) ) ;
#91149 = ORIENTED_EDGE ( 'NONE', *, *, #77941, .F. ) ;
#91151 = DIRECTION ( 'NONE',  ( 0.000000000000000000, 0.9889818879709272315, 0.1480365673253073999 ) ) ;
#91150 = CARTESIAN_POINT ( 'NONE',  ( 21.05000000000005400, 74.94272479589878344, -8.023107484524793165 ) ) ;
#91152 = EDGE_LOOP ( 'NONE', ( #177800, #217399, #217359, #84525 ) ) ;
#91155 = ORIENTED_EDGE ( 'NONE', *, *, #247066, .T. ) ;
#91154 = CARTESIAN_POINT ( 'NONE',  ( 20.95159278453404283, 67.09210366206326626, -161.5383872994151773 ) ) ;
#91153 = LINE ( 'NONE', #250228, #7454 ) ;
#91156 = CIRCLE ( 'NONE', #3653, 4.041421356237310469 ) ;
#91157 = DIRECTION ( 'NONE',  ( 0.000000000000000000, -0.5907332058517320572, 0.8068669527896995541 ) ) ;
#91158 = LINE ( 'NONE', #87293, #198385 ) ;
#91159 = EDGE_CURVE ( 'NONE', #17866, #1479, #209146, .T. ) ;
#91160 = CARTESIAN_POINT ( 'NONE',  ( -18.49513951962167724, 85.43772502668957713, -96.24503490949508944 ) ) ;
#91161 = VERTEX_POINT ( 'NONE', #127050 ) ;
#91163 = EDGE_CURVE ( 'NONE', #107334, #258000, #246987, .T. ) ;
#91162 = DIRECTION ( 'NONE',  ( 0.000000000000000000, -0.9875102702516471709, 0.1575546449569757979 ) ) ;
#91164 = CARTESIAN_POINT ( 'NONE',  ( -23.25000000000000000, 0.8618440306782485516, -204.9572370243411115 ) ) ;
#91165 = ADVANCED_FACE ( 'NONE', ( #185743, #147912 ), #67079, .F. ) ;
#91167 = CARTESIAN_POINT ( 'NONE',  ( 20.85000000000000142, 6.933893972137497030, -171.2856458343736108 ) ) ;
#91166 = FACE_OUTER_BOUND ( 'NONE', #28147, .T. ) ;
#91168 = EDGE_CURVE ( 'NONE', #123166, #160843, #18702, .T. ) ;
#91170 = ORIENTED_EDGE ( 'NONE', *, *, #197516, .F. ) ;
#91169 = CARTESIAN_POINT ( 'NONE',  ( 20.99749315643149217, 11.75000000001115907, -93.48519423124028549 ) ) ;
#91171 = VERTEX_POINT ( 'NONE', #146585 ) ;
#91172 = DIRECTION ( 'NONE',  ( 1.000000000000000000, -0.000000000000000000, -0.000000000000000000 ) ) ;
#91173 = CARTESIAN_POINT ( 'NONE',  ( 22.57320508075688537, 64.35000000001238618, -170.0231074845244166 ) ) ;
#91174 = CIRCLE ( 'NONE', #128587, 0.1000000000000013933 ) ;
#91175 = CIRCLE ( 'NONE', #236916, 0.09999999999998898659 ) ;
#91176 = ADVANCED_FACE ( 'NONE', ( #149205 ), #64509, .T. ) ;
#91177 = FACE_OUTER_BOUND ( 'NONE', #246747, .T. ) ;
#91180 = EDGE_CURVE ( 'NONE', #40998, #162117, #5789, .T. ) ;
#91179 = ADVANCED_FACE ( 'NONE', ( #104873 ), #244423, .T. ) ;
#91178 = ORIENTED_EDGE ( 'NONE', *, *, #65097, .T. ) ;
#91181 = DIRECTION ( 'NONE',  ( 0.000000000000000000, 0.8814952561688430555, -0.4721928772777346239 ) ) ;
#91182 = DIRECTION ( 'NONE',  ( 1.000000000000000000, 0.000000000000000000, 0.000000000000000000 ) ) ;
#91183 = CARTESIAN_POINT ( 'NONE',  ( 18.52130828395271678, -9.481395502614628157, -141.0245067238836327 ) ) ;
#91184 = CIRCLE ( 'NONE', #187063, 0.09999999999998898659 ) ;
#91185 = ADVANCED_FACE ( 'NONE', ( #17382 ), #72232, .F. ) ;
#91186 = ORIENTED_EDGE ( 'NONE', *, *, #82417, .T. ) ;
#91187 = CARTESIAN_POINT ( 'NONE',  ( 20.84451136049846554, 58.94296221207902420, -225.8426244149431454 ) ) ;
#91188 = DIRECTION ( 'NONE',  ( 1.000000000000000000, 0.000000000000000000, 0.000000000000000000 ) ) ;
#91189 = EDGE_CURVE ( 'NONE', #2313, #83334, #6214, .T. ) ;
#91190 = ORIENTED_EDGE ( 'NONE', *, *, #214708, .F. ) ;
#91191 = AXIS2_PLACEMENT_3D ( 'NONE', #230056, #108811, #11007 ) ;
#91193 = AXIS2_PLACEMENT_3D ( 'NONE', #5993, #165083, #185929 ) ;
#91192 = CARTESIAN_POINT ( 'NONE',  ( -20.85000000000000142, 79.14291928130900544, -196.3819507745080557 ) ) ;
#91194 = FACE_OUTER_BOUND ( 'NONE', #178535, .T. ) ;
#91195 = ADVANCED_FACE ( 'NONE', ( #233861 ), #85307, .T. ) ;
#91196 = ADVANCED_FACE ( 'NONE', ( #112630 ), #141560, .T. ) ;
#91197 = AXIS2_PLACEMENT_3D ( 'NONE', #105534, #2609, #5156 ) ;
#91198 = ORIENTED_EDGE ( 'NONE', *, *, #204368, .F. ) ;
#91199 = ORIENTED_EDGE ( 'NONE', *, *, #110570, .F. ) ;
#91200 = EDGE_CURVE ( 'NONE', #151453, #29169, #214339, .T. ) ;
#91201 = LINE ( 'NONE', #63617, #166852 ) ;
#91202 = ORIENTED_EDGE ( 'NONE', *, *, #243846, .F. ) ;
#91204 = ORIENTED_EDGE ( 'NONE', *, *, #142740, .F. ) ;
#91203 = CARTESIAN_POINT ( 'NONE',  ( -22.45437739390954590, 1.115488181425289271E-11, -155.8504291884057693 ) ) ;
#91206 = EDGE_CURVE ( 'NONE', #44801, #257362, #152012, .T. ) ;
#91205 = EDGE_LOOP ( 'NONE', ( #103062, #206416, #86227, #28361 ) ) ;
#91207 = AXIS2_PLACEMENT_3D ( 'NONE', #251971, #254514, #53773 ) ;
#91208 = CIRCLE ( 'NONE', #241069, 14.30833333333333890 ) ;
#91211 = ORIENTED_EDGE ( 'NONE', *, *, #227413, .F. ) ;
#91210 = ORIENTED_EDGE ( 'NONE', *, *, #186769, .T. ) ;
#91209 = CARTESIAN_POINT ( 'NONE',  ( -23.25000000000000000, 77.83585931145498193, -24.41866831572578533 ) ) ;
#91212 = EDGE_CURVE ( 'NONE', #60425, #165019, #14839, .T. ) ;
#91213 = DIRECTION ( 'NONE',  ( 0.000000000000000000, 0.9908441862701782288, -0.1350103645450542456 ) ) ;
#91215 = ORIENTED_EDGE ( 'NONE', *, *, #179815, .F. ) ;
#91214 = AXIS2_PLACEMENT_3D ( 'NONE', #98755, #221289, #158802 ) ;
#91216 = DIRECTION ( 'NONE',  ( 0.000000000000000000, -0.5773469543544729188, -0.8164989248600478255 ) ) ;
#91217 = CARTESIAN_POINT ( 'NONE',  ( -17.11825945287481332, 51.52760218553060412, -231.9873527057832234 ) ) ;
#91218 = CARTESIAN_POINT ( 'NONE',  ( 20.94999999999999574, 74.83729825007360148, -61.42310748452432989 ) ) ;
#91219 = CIRCLE ( 'NONE', #149494, 0.09999999999998898659 ) ;
#91220 = DIRECTION ( 'NONE',  ( 0.000000000000000000, 0.000000000000000000, -1.000000000000000000 ) ) ;
#91221 = CARTESIAN_POINT ( 'NONE',  ( -22.50000000000093436, 25.89494711235937530, -254.2627752153468919 ) ) ;
#91223 = ORIENTED_EDGE ( 'NONE', *, *, #227348, .T. ) ;
#91222 = VECTOR ( 'NONE', #102900, 1000.000000000000000 ) ;
#91224 = CIRCLE ( 'NONE', #236965, 0.1999999999999987899 ) ;
#91225 = VERTEX_POINT ( 'NONE', #130898 ) ;
#91226 = AXIS2_PLACEMENT_3D ( 'NONE', #31317, #187802, #173412 ) ;
#91227 = VERTEX_POINT ( 'NONE', #196029 ) ;
#91228 = CARTESIAN_POINT ( 'NONE',  ( 21.05000000000000071, 87.65000000001246860, -172.9231074845242802 ) ) ;
#91229 =( BOUNDED_SURFACE ( )  B_SPLINE_SURFACE ( 3, 2, ( 
 ( #64784, #223847, #45227 ),
 ( #85596, #165178, #106453 ),
 ( #86896, #127335, #206872 ),
 ( #107766, #75096, #193732 ),
 ( #154634, #15099, #234127 ),
 ( #132471, #94614, #112910 ),
 ( #131176, #153365, #210722 ),
 ( #150751, #171630, #54206 ),
 ( #133745, #214562, #12545 ),
 ( #11243, #35952, #213276 ) ),
 .UNSPECIFIED., .F., .F., .F. ) 
 B_SPLINE_SURFACE_WITH_KNOTS ( ( 4, 2, 2, 2, 4 ),
 ( 3, 3 ),
 ( 0.0001701955120502345899, 0.0002247052511886165759, 0.0002792149903269985889, 0.0003882344686037626151, 0.0006062734251572906132 ),
 ( 0.000000000000000000, 1.000000000000000000 ),
 .UNSPECIFIED. ) 
 GEOMETRIC_REPRESENTATION_ITEM ( )  RATIONAL_B_SPLINE_SURFACE ( (
 ( 1.000000000000000000, 0.2966190024560962923, 1.000000000000000000),
 ( 1.000000000000000000, 0.2964522492709221746, 1.000000000000000000),
 ( 1.000000000000000000, 0.3059923531885490600, 1.000000000000000000),
 ( 1.000000000000000000, 0.3355751146947310581, 1.000000000000000000),
 ( 1.000000000000000000, 0.3550672384961548467, 1.000000000000000000),
 ( 1.000000000000000000, 0.4157034672184251600, 1.000000000000000000),
 ( 1.000000000000000000, 0.4588031877658517166, 1.000000000000000000),
 ( 1.000000000000000000, 0.5771441759652446990, 1.000000000000000000),
 ( 1.000000000000000000, 0.6469377121778305817, 1.000000000000000000),
 ( 1.000000000000000000, 0.7071067811865524577, 1.000000000000000000) ) ) 
 REPRESENTATION_ITEM ( '' )  SURFACE ( )  );
#91231 = VERTEX_POINT ( 'NONE', #134733 ) ;
#91230 = DIRECTION ( 'NONE',  ( 1.000000000000000000, -2.952720810173289112E-16, -2.061873921506763405E-30 ) ) ;
#91232 = CARTESIAN_POINT ( 'NONE',  ( 18.59999999999999076, 6.650000000011155876, -121.6500000000000341 ) ) ;
#91234 = EDGE_LOOP ( 'NONE', ( #175241, #82851, #128823, #108738 ) ) ;
#91233 = DIRECTION ( 'NONE',  ( 0.000000000000000000, -0.2617529984165032908, -0.9651348961777156399 ) ) ;
#91235 = EDGE_CURVE ( 'NONE', #47981, #163656, #39588, .T. ) ;
#91236 = AXIS2_PLACEMENT_3D ( 'NONE', #74913, #172747, #175301 ) ;
#91237 = ORIENTED_EDGE ( 'NONE', *, *, #145676, .T. ) ;
#91238 = PLANE ( 'NONE',  #216678 ) ;
#91239 = EDGE_LOOP ( 'NONE', ( #210519, #49519, #251841, #33094 ) ) ;
#91240 = CARTESIAN_POINT ( 'NONE',  ( -16.84981964351498007, 9.917318234109993469, -180.3696016140194445 ) ) ;
#91241 = DIRECTION ( 'NONE',  ( 0.000000000000000000, 0.8814952561688476074, -0.4721928772777262417 ) ) ;
#91242 = CIRCLE ( 'NONE', #49541, 11.74999999999999645 ) ;
#91244 = ORIENTED_EDGE ( 'NONE', *, *, #192882, .F. ) ;
#91243 = ORIENTED_EDGE ( 'NONE', *, *, #49262, .T. ) ;
#91245 = ORIENTED_EDGE ( 'NONE', *, *, #156704, .T. ) ;
#91246 = DIRECTION ( 'NONE',  ( 0.000000000000000000, 0.000000000000000000, -1.000000000000000000 ) ) ;
#91247 = ORIENTED_EDGE ( 'NONE', *, *, #227533, .T. ) ;
#91248 = ORIENTED_EDGE ( 'NONE', *, *, #82285, .T. ) ;
#91249 = CARTESIAN_POINT ( 'NONE',  ( -21.04999999999999716, -9.599999999988844124, -74.03206939669971121 ) ) ;
#91251 = ORIENTED_EDGE ( 'NONE', *, *, #8709, .F. ) ;
#91250 = CARTESIAN_POINT ( 'NONE',  ( 20.94999999999999929, 85.40000000001252545, -179.9170766071767389 ) ) ;
#91252 = DIRECTION ( 'NONE',  ( 0.000000000000000000, -1.000000000000000000, 0.000000000000000000 ) ) ;
#91254 = DIRECTION ( 'NONE',  ( -0.000000000000000000, -6.982962677686266711E-15, 1.000000000000000000 ) ) ;
#91253 = DIRECTION ( 'NONE',  ( 1.000000000000000000, -2.952720810173289112E-16, -2.061873921506763405E-30 ) ) ;
#91255 = LINE ( 'NONE', #92516, #128207 ) ;
#91256 = CARTESIAN_POINT ( 'NONE',  ( -18.40000000000000213, 11.48667500176882861, -191.7499999999999716 ) ) ;
#91257 = ORIENTED_EDGE ( 'NONE', *, *, #4195, .T. ) ;
#91258 = VECTOR ( 'NONE', #141995, 1000.000000000000000 ) ;
#91259 = EDGE_LOOP ( 'NONE', ( #212513, #11946, #57261 ) ) ;
#91260 = CARTESIAN_POINT ( 'NONE',  ( -18.50000000000000000, 77.83534155023627932, -91.46795619196132066 ) ) ;
#91262 = EDGE_CURVE ( 'NONE', #94765, #13299, #16691, .T. ) ;
#91261 = DIRECTION ( 'NONE',  ( 0.000000000000000000, 0.000000000000000000, -1.000000000000000000 ) ) ;
#91263 = AXIS2_PLACEMENT_3D ( 'NONE', #31144, #8970, #91076 ) ;
#91264 = ORIENTED_EDGE ( 'NONE', *, *, #127896, .F. ) ;
#91265 = ADVANCED_FACE ( 'NONE', ( #173935 ), #31836, .T. ) ;
#91266 = VECTOR ( 'NONE', #56603, 1000.000000000000114 ) ;
#91267 = CARTESIAN_POINT ( 'NONE',  ( 18.59999999999999076, 76.00000000001142553, -36.02310748452432421 ) ) ;
#91268 = LINE ( 'NONE', #229494, #221770 ) ;
#91269 = ORIENTED_EDGE ( 'NONE', *, *, #129776, .T. ) ;
#91270 = VERTEX_POINT ( 'NONE', #230000 ) ;
#91271 = EDGE_CURVE ( 'NONE', #84975, #101180, #16120, .T. ) ;
#91272 = DIRECTION ( 'NONE',  ( 0.000000000000000000, -0.2128009952263604232, 0.9770955615653316162 ) ) ;
#91274 = EDGE_CURVE ( 'NONE', #127648, #113736, #201861, .T. ) ;
#91273 = CARTESIAN_POINT ( 'NONE',  ( -21.14999999999999858, 6.540656951712397138, -100.5000000000000284 ) ) ;
#91275 = EDGE_LOOP ( 'NONE', ( #69735, #237432, #61978, #5998 ) ) ;
#91276 = LINE ( 'NONE', #134227, #34754 ) ;
#91277 = EDGE_LOOP ( 'NONE', ( #190638, #106173 ) ) ;
#91278 = CARTESIAN_POINT ( 'NONE',  ( -23.25000000000000000, 64.25000000001146816, -43.03791325517834565 ) ) ;
#91279 = CARTESIAN_POINT ( 'NONE',  ( -21.55000000000000071, 7.349999999999998757, -12.34999999999999964 ) ) ;
#91281 = DIRECTION ( 'NONE',  ( 0.000000000000000000, 0.000000000000000000, 1.000000000000000000 ) ) ;
#91280 = DIRECTION ( 'NONE',  ( 6.938893903907222067E-15, 1.000000000000000000, 6.982962677686266711E-15 ) ) ;
#91282 = CARTESIAN_POINT ( 'NONE',  ( -17.04295772865488345, 10.02489942527116007, -87.85000000000003695 ) ) ;
#91284 = AXIS2_PLACEMENT_3D ( 'NONE', #98697, #177028, #134010 ) ;
#91283 = CARTESIAN_POINT ( 'NONE',  ( 20.84999999999999787, 64.25000000001146816, -42.94225473048309993 ) ) ;
#91285 = FACE_OUTER_BOUND ( 'NONE', #170594, .T. ) ;
#91286 = CARTESIAN_POINT ( 'NONE',  ( 20.85000000000000142, 77.83585931145600512, -158.5186683157258187 ) ) ;
#91287 = AXIS2_PLACEMENT_3D ( 'NONE', #215319, #231059, #133220 ) ;
#91289 = VERTEX_POINT ( 'NONE', #220712 ) ;
#91288 = DIRECTION ( 'NONE',  ( 1.000000000000000000, 0.000000000000000000, 0.000000000000000000 ) ) ;
#91291 = VERTEX_POINT ( 'NONE', #137309 ) ;
#91290 = ORIENTED_EDGE ( 'NONE', *, *, #226265, .F. ) ;
#91292 = ORIENTED_EDGE ( 'NONE', *, *, #161393, .T. ) ;
#91293 = CARTESIAN_POINT ( 'NONE',  ( -16.77779411503079388, 60.94653821389059090, -221.0301460241443010 ) ) ;
#91294 = DIRECTION ( 'NONE',  ( -1.000000000000000000, -0.000000000000000000, -0.000000000000000000 ) ) ;
#91295 =( BOUNDED_SURFACE ( )  B_SPLINE_SURFACE ( 3, 2, ( 
 ( #33520, #113014, #192557 ),
 ( #246112, #146981, #217223 ),
 ( #214668, #236795, #256299 ),
 ( #36055, #98530, #95995 ) ),
 .UNSPECIFIED., .F., .F., .F. ) 
 B_SPLINE_SURFACE_WITH_KNOTS ( ( 4, 4 ),
 ( 3, 3 ),
 ( -1.992221491942114397E-18, 0.0003124336117481551524 ),
 ( 0.000000000000000000, 1.000000000000000000 ),
 .UNSPECIFIED. ) 
 GEOMETRIC_REPRESENTATION_ITEM ( )  RATIONAL_B_SPLINE_SURFACE ( (
 ( 1.000000000000000000, 0.7040654476016252605, 1.000000000000000000),
 ( 1.000000000000000000, 0.7039193538783552473, 1.000000000000000000),
 ( 1.000000000000000000, 0.7089171279143997584, 1.000000000000000000),
 ( 1.000000000000000000, 0.7071067811865408004, 1.000000000000000000) ) ) 
 REPRESENTATION_ITEM ( '' )  SURFACE ( )  );
#91297 = CARTESIAN_POINT ( 'NONE',  ( -22.50014994444008565, 11.74971973190325158, -33.41691984328069509 ) ) ;
#91296 = DIRECTION ( 'NONE',  ( -1.000000000000000000, 0.000000000000000000, 0.000000000000000000 ) ) ;
#91298 = LINE ( 'NONE', #169594, #91501 ) ;
#91299 = ORIENTED_EDGE ( 'NONE', *, *, #104138, .F. ) ;
#91300 = FACE_OUTER_BOUND ( 'NONE', #205556, .T. ) ;
#91301 = EDGE_LOOP ( 'NONE', ( #52530, #183593, #137113, #65429 ) ) ;
#91302 = VERTEX_POINT ( 'NONE', #139871 ) ;
#91303 = CARTESIAN_POINT ( 'NONE',  ( 21.05000000000000071, 34.01125473725045367, -243.8802146427659352 ) ) ;
#91304 = DIRECTION ( 'NONE',  ( 1.186688945009009831E-16, 0.9651348961777157509, -0.2617529984165031243 ) ) ;
#91305 = CARTESIAN_POINT ( 'NONE',  ( -21.05000000000000071, 77.26178616857765746, -195.4366085209788935 ) ) ;
#91306 = AXIS2_PLACEMENT_3D ( 'NONE', #136632, #949, #137913 ) ;
#91307 = VERTEX_POINT ( 'NONE', #57770 ) ;
#91308 = EDGE_CURVE ( 'NONE', #130466, #203569, #205942, .T. ) ;
#91309 = DIRECTION ( 'NONE',  ( -1.000000000000000000, -0.000000000000000000, 0.000000000000000000 ) ) ;
#91310 = LINE ( 'NONE', #156450, #238047 ) ;
#91311 = ORIENTED_EDGE ( 'NONE', *, *, #168054, .F. ) ;
#91312 = ORIENTED_EDGE ( 'NONE', *, *, #93795, .T. ) ;
#91313 = DIRECTION ( 'NONE',  ( -1.000000000000000000, 0.000000000000000000, -0.000000000000000000 ) ) ;
#91314 = CARTESIAN_POINT ( 'NONE',  ( 23.14999999999999858, 0.000000000000000000, -37.50000000000000000 ) ) ;
#91315 = FACE_OUTER_BOUND ( 'NONE', #170579, .T. ) ;
#91316 = DIRECTION ( 'NONE',  ( 0.000000000000000000, 0.9126074666063660468, 0.4088369013363524762 ) ) ;
#91317 = CARTESIAN_POINT ( 'NONE',  ( -20.90000000000000213, 11.49641995933507843, -1.885425182446133885 ) ) ;
#91318 = SPHERICAL_SURFACE ( 'NONE', #237793, 0.1000000000000000056 ) ;
#91319 = ORIENTED_EDGE ( 'NONE', *, *, #125382, .F. ) ;
#91321 = EDGE_CURVE ( 'NONE', #119361, #177518, #189399, .T. ) ;
#91320 = FACE_OUTER_BOUND ( 'NONE', #245488, .T. ) ;
#91322 = DIRECTION ( 'NONE',  ( -1.000000000000000000, 0.000000000000000000, 0.000000000000000000 ) ) ;
#91324 = DIRECTION ( 'NONE',  ( 0.000000000000000000, 0.000000000000000000, 1.000000000000000000 ) ) ;
#91323 = CARTESIAN_POINT ( 'NONE',  ( -23.25000000000000000, 7.128833340093095217, -233.7327013124392749 ) ) ;
#91325 = DIRECTION ( 'NONE',  ( 1.000000000000000000, 3.190570557967288949E-16, 6.948722487160392945E-17 ) ) ;
#91326 = EDGE_CURVE ( 'NONE', #170888, #3167, #21261, .T. ) ;
#91327 = CARTESIAN_POINT ( 'NONE',  ( -20.85000000000000142, 77.36242903720497566, -61.63422623660309796 ) ) ;
#91328 = AXIS2_PLACEMENT_3D ( 'NONE', #256498, #916, #80449 ) ;
#91329 = CIRCLE ( 'NONE', #237057, 0.1000000000000028644 ) ;
#91330 = CARTESIAN_POINT ( 'NONE',  ( -23.15000000000000213, -11.64999999998884483, -197.8999999999999773 ) ) ;
#91331 = CARTESIAN_POINT ( 'NONE',  ( 20.90851465518105812, 10.32532329027886320, -139.5699343018359855 ) ) ;
#91332 = VECTOR ( 'NONE', #50307, 1000.000000000000000 ) ;
#91333 = AXIS2_PLACEMENT_3D ( 'NONE', #128468, #89322, #210575 ) ;
#91335 = ORIENTED_EDGE ( 'NONE', *, *, #117763, .F. ) ;
#91334 = FACE_BOUND ( 'NONE', #88388, .T. ) ;
#91336 =( BOUNDED_CURVE ( )  B_SPLINE_CURVE ( 3, ( #23213, #226490, #66161, #106547 ),
 .UNSPECIFIED., .F., .F. ) 
 B_SPLINE_CURVE_WITH_KNOTS ( ( 4, 4 ),
 ( 0.3000847527772391721, 0.5517402753107903957 ),
 .UNSPECIFIED. ) 
 CURVE ( )  GEOMETRIC_REPRESENTATION_ITEM ( )  RATIONAL_B_SPLINE_CURVE ( ( 1.000000000000000000, 0.9947294176030464508, 0.9947294176030464508, 1.000000000000000000 ) ) 
 REPRESENTATION_ITEM ( '' )  );
#91337 = EDGE_CURVE ( 'NONE', #185693, #236168, #60340, .T. ) ;
#91338 = CIRCLE ( 'NONE', #49630, 0.4999999999999978351 ) ;
#91339 = FACE_OUTER_BOUND ( 'NONE', #120246, .T. ) ;
#91340 = ADVANCED_FACE ( 'NONE', ( #181603 ), #2933, .T. ) ;
#91341 = ADVANCED_FACE ( 'NONE', ( #99454 ), #240288, .F. ) ;
#91342 = CARTESIAN_POINT ( 'NONE',  ( -21.29999999999995808, 1.115650265596050101E-11, -96.45000000000003126 ) ) ;
#91343 = AXIS2_PLACEMENT_3D ( 'NONE', #52383, #235837, #237136 ) ;
#91344 = CIRCLE ( 'NONE', #220342, 0.09999999999999939493 ) ;
#91346 = AXIS2_PLACEMENT_3D ( 'NONE', #158505, #218426, #235427 ) ;
#91345 = CARTESIAN_POINT ( 'NONE',  ( 23.24999999999999289, 11.65000000001116298, -45.65000000000000568 ) ) ;
#91347 = EDGE_CURVE ( 'NONE', #12734, #66731, #122910, .T. ) ;
#91348 = CARTESIAN_POINT ( 'NONE',  ( 21.08489247129321242, 8.877675190881227252, -45.85000000000000853 ) ) ;
#91349 = DIRECTION ( 'NONE',  ( 0.000000000000000000, 0.000000000000000000, 1.000000000000000000 ) ) ;
#91350 = B_SPLINE_CURVE_WITH_KNOTS ( 'NONE', 3,
 ( #29744, #10151, #152251, #71423, #89662, #50528, #154819, #252591, #34873, #74009, #230479, #169259, #233067, #209629 ),
 .UNSPECIFIED., .F., .F.,
 ( 4, 2, 2, 2, 2, 2, 4 ),
 ( 0.000000000000000000, 2.389617747641766606E-05, 4.779235495283533212E-05, 9.558470990574123225E-05, 0.0001911694198115613131, 0.0003823388396232054050, 0.0007646776792464113522 ),
 .UNSPECIFIED. ) ;
#91351 = AXIS2_PLACEMENT_3D ( 'NONE', #193285, #94160, #173769 ) ;
#91352 = DIRECTION ( 'NONE',  ( 0.000000000000000000, -0.8660254037844419273, 0.4999999999999942824 ) ) ;
#91353 = CARTESIAN_POINT ( 'NONE',  ( 21.14999999999999858, 52.91185528119409298, -244.1460391050142675 ) ) ;
#91354 = CARTESIAN_POINT ( 'NONE',  ( -16.94225986326250677, 66.05000000001157900, -56.57638810891648973 ) ) ;
#91355 = ORIENTED_EDGE ( 'NONE', *, *, #1434, .T. ) ;
#91356 = CYLINDRICAL_SURFACE ( 'NONE', #78992, 2.000000000000001776 ) ;
#91358 = ORIENTED_EDGE ( 'NONE', *, *, #151039, .T. ) ;
#91357 = DIRECTION ( 'NONE',  ( 0.000000000000000000, 1.000000000000000000, 0.000000000000000000 ) ) ;
#91359 = CARTESIAN_POINT ( 'NONE',  ( 20.94999999999999929, 70.15000000001178648, -79.65560470880227228 ) ) ;
#91360 = ADVANCED_FACE ( 'NONE', ( #78617 ), #62922, .T. ) ;
#91361 = LINE ( 'NONE', #204856, #75200 ) ;
#91362 = VERTEX_POINT ( 'NONE', #96870 ) ;
#91363 = DIRECTION ( 'NONE',  ( 1.000000000000000000, 0.000000000000000000, -0.000000000000000000 ) ) ;
#91364 = SHAPE_DEFINITION_REPRESENTATION ( #124202, #223420 ) ;
#91365 = DIRECTION ( 'NONE',  ( 0.000000000000000000, 2.891205793294679805E-16, -1.000000000000000000 ) ) ;
#91366 = DIRECTION ( 'NONE',  ( 0.5000000000001141309, 0.000000000000000000, -0.8660254037843729824 ) ) ;
#91367 = CARTESIAN_POINT ( 'NONE',  ( -18.48550754432041288, 85.46339977857189751, -95.97431773210885808 ) ) ;
#91368 = ORIENTED_EDGE ( 'NONE', *, *, #125671, .F. ) ;
#91369 = DIRECTION ( 'NONE',  ( 0.000000000000000000, 0.000000000000000000, 1.000000000000000000 ) ) ;
#91370 = CARTESIAN_POINT ( 'NONE',  ( 23.24999999999999289, 5.950000000011163692, -123.6942976949652149 ) ) ;
#91371 = VECTOR ( 'NONE', #6418, 1000.000000000000000 ) ;
#91372 = CARTESIAN_POINT ( 'NONE',  ( 20.95289811251229750, 8.893168004469748311, -176.0018094939185005 ) ) ;
#91373 = EDGE_LOOP ( 'NONE', ( #121426, #131092, #251314, #67822 ) ) ;
#91374 = CIRCLE ( 'NONE', #174803, 0.4000000000000114575 ) ;
#91375 = ORIENTED_EDGE ( 'NONE', *, *, #73916, .F. ) ;
#91376 = CARTESIAN_POINT ( 'NONE',  ( 20.94999999999999929, 71.18691588786300883, -181.9646252410481964 ) ) ;
#91377 = CARTESIAN_POINT ( 'NONE',  ( 18.44444291854882323, 85.49010118095512212, -96.39420351963327960 ) ) ;
#91378 = DIRECTION ( 'NONE',  ( 0.000000000000000000, 1.776356839400254803E-15, -1.000000000000000000 ) ) ;
#91380 = LINE ( 'NONE', #134329, #3529 ) ;
#91379 = DIRECTION ( 'NONE',  ( -1.000000000000000000, 0.000000000000000000, 0.000000000000000000 ) ) ;
#91382 = CARTESIAN_POINT ( 'NONE',  ( -21.09316766718153247, 75.96073659769774622, -176.3932607969990727 ) ) ;
#91381 = VECTOR ( 'NONE', #128529, 1000.000000000000000 ) ;
#91383 = CARTESIAN_POINT ( 'NONE',  ( -18.37013991200266005, 64.50025238380001724, -112.2300844740072705 ) ) ;
#91384 = CIRCLE ( 'NONE', #153788, 0.09999999999999939493 ) ;
#91385 = ORIENTED_EDGE ( 'NONE', *, *, #116881, .F. ) ;
#91386 = EDGE_CURVE ( 'NONE', #51112, #201670, #176473, .T. ) ;
#91388 = VERTEX_POINT ( 'NONE', #156918 ) ;
#91387 = DIRECTION ( 'NONE',  ( -1.000000000000000000, 0.000000000000000000, -0.000000000000000000 ) ) ;
#91389 = CARTESIAN_POINT ( 'NONE',  ( -16.77683809663752257, 44.14991418685006153, -235.2970290647049580 ) ) ;
#91390 = AXIS2_PLACEMENT_3D ( 'NONE', #1594, #255877, #240237 ) ;
#91391 = CARTESIAN_POINT ( 'NONE',  ( -21.09316766718152891, -1.317210868494001375, -194.7673961808032459 ) ) ;
#91393 = LINE ( 'NONE', #14443, #249359 ) ;
#91392 = DIRECTION ( 'NONE',  ( 1.000000000000000000, 0.000000000000000000, 0.000000000000000000 ) ) ;
#91394 = ORIENTED_EDGE ( 'NONE', *, *, #101472, .F. ) ;
#91395 = FACE_OUTER_BOUND ( 'NONE', #83545, .T. ) ;
#91396 = CARTESIAN_POINT ( 'NONE',  ( 20.04142135391667168, 64.25000000001196554, -111.8206006188945025 ) ) ;
#91397 = CARTESIAN_POINT ( 'NONE',  ( -21.14999999999999858, 69.45934304831071415, -103.0231074845243597 ) ) ;
#91399 = EDGE_CURVE ( 'NONE', #236473, #43709, #147894, .T. ) ;
#91398 = CYLINDRICAL_SURFACE ( 'NONE', #97936, 0.09999999999999609201 ) ;
#91400 = ORIENTED_EDGE ( 'NONE', *, *, #2726, .T. ) ;
#91401 = AXIS2_PLACEMENT_3D ( 'NONE', #3768, #161583, #221509 ) ;
#91402 = TOROIDAL_SURFACE ( 'NONE', #20669, 11.90000000000000391, 0.1000000000000000056 ) ;
#91403 = VERTEX_POINT ( 'NONE', #237713 ) ;
#91404 = EDGE_CURVE ( 'NONE', #99703, #172803, #197291, .T. ) ;
#91405 = EDGE_CURVE ( 'NONE', #22307, #111909, #44854, .T. ) ;
#91406 = LINE ( 'NONE', #87525, #242607 ) ;
#91407 = VERTEX_POINT ( 'NONE', #59031 ) ;
#91408 = CARTESIAN_POINT ( 'NONE',  ( 21.04999999999999716, 10.68430915749623367, -141.5266967903268664 ) ) ;
#91409 = CIRCLE ( 'NONE', #37244, 0.1999999999999997335 ) ;
#91411 = AXIS2_PLACEMENT_3D ( 'NONE', #193595, #124964, #204478 ) ;
#91410 = CARTESIAN_POINT ( 'NONE',  ( -21.11927991906891222, 65.53459516797913409, -242.0764145625574315 ) ) ;
#91412 = AXIS2_PLACEMENT_3D ( 'NONE', #130051, #47950, #170536 ) ;
#91413 = DIRECTION ( 'NONE',  ( 1.000000000000000000, -0.000000000000000000, -0.000000000000000000 ) ) ;
#91414 = ORIENTED_EDGE ( 'NONE', *, *, #63698, .T. ) ;
#91415 = CARTESIAN_POINT ( 'NONE',  ( 20.84999999999998721, 18.60970618848720903, -231.2322896185303875 ) ) ;
#91416 = ADVANCED_FACE ( 'NONE', ( #65482 ), #151133, .T. ) ;
#91417 = ADVANCED_FACE ( 'NONE', ( #104585 ), #68775, .F. ) ;
#91418 = CARTESIAN_POINT ( 'NONE',  ( -20.64999999999999858, 1.940186915899004161, -54.17088078894667547 ) ) ;
#91419 = LINE ( 'NONE', #249210, #24411 ) ;
#91420 = CARTESIAN_POINT ( 'NONE',  ( 20.94999999999999929, 76.00000000001190870, -103.0231074845243029 ) ) ;
#91421 = LINE ( 'NONE', #48425, #35331 ) ;
#91422 = DIRECTION ( 'NONE',  ( -1.000000000000000000, 2.952720810173289112E-16, 2.061873921506763405E-30 ) ) ;
#91423 = DIRECTION ( 'NONE',  ( 1.000000000000000000, 0.000000000000000000, 0.000000000000000000 ) ) ;
#91424 = ORIENTED_EDGE ( 'NONE', *, *, #186537, .T. ) ;
#91426 = CARTESIAN_POINT ( 'NONE',  ( -16.97683809663752896, 9.950000000011140600, -180.7715247686699627 ) ) ;
#91425 = LINE ( 'NONE', #172289, #90959 ) ;
#91427 = AXIS2_PLACEMENT_3D ( 'NONE', #225614, #143531, #35192 ) ;
#91428 = VERTEX_POINT ( 'NONE', #229387 ) ;
#91430 = EDGE_LOOP ( 'NONE', ( #74850, #5417, #98567, #62300 ) ) ;
#91429 = DIRECTION ( 'NONE',  ( 0.000000000000000000, 0.000000000000000000, 1.000000000000000000 ) ) ;
#91431 = EDGE_LOOP ( 'NONE', ( #81592, #65100, #182382, #130852 ) ) ;
#91432 = CARTESIAN_POINT ( 'NONE',  ( -16.86445178670583545, 9.962211629127152079, -146.6092225618827172 ) ) ;
#91433 = DIRECTION ( 'NONE',  ( 0.000000000000000000, 0.2128009952263600346, -0.9770955615653315052 ) ) ;
#91434 = CARTESIAN_POINT ( 'NONE',  ( 5.551115123125782702E-14, 64.35000000001120668, -3.123107484524795474 ) ) ;
#91435 = EDGE_CURVE ( 'NONE', #75064, #148589, #118867, .T. ) ;
#91436 = CARTESIAN_POINT ( 'NONE',  ( -16.94107738177415712, 10.01423928514777728, -46.04999999999999716 ) ) ;
#91437 = ORIENTED_EDGE ( 'NONE', *, *, #256145, .T. ) ;
#91438 = EDGE_CURVE ( 'NONE', #219596, #28335, #251934, .T. ) ;
#91439 = EDGE_CURVE ( 'NONE', #80890, #221156, #10342, .T. ) ;
#91440 = DIRECTION ( 'NONE',  ( -0.7071067811865474617, 0.7071067811865474617, 4.937700262164531476E-15 ) ) ;
#91441 = DIRECTION ( 'NONE',  ( -0.000000000000000000, -0.2128009952263603677, 0.9770955615653313941 ) ) ;
#91442 = EDGE_LOOP ( 'NONE', ( #108862, #101505, #44419, #252996 ) ) ;
#91443 = AXIS2_PLACEMENT_3D ( 'NONE', #55197, #214315, #56493 ) ;
#91444 = CARTESIAN_POINT ( 'NONE',  ( 23.14999999999999503, 69.35000000001200249, -115.3731074845243398 ) ) ;
#91445 = AXIS2_PLACEMENT_3D ( 'NONE', #88159, #225112, #247252 ) ;
#91446 = ADVANCED_FACE ( 'NONE', ( #172012 ), #250221, .F. ) ;
#91447 = DIRECTION ( 'NONE',  ( 0.000000000000000000, -6.467318590049456648E-15, 1.000000000000000000 ) ) ;
#91448 = VERTEX_POINT ( 'NONE', #64210 ) ;
#91450 = DIRECTION ( 'NONE',  ( 0.000000000000000000, -1.000000000000000000, -8.717686153663073805E-15 ) ) ;
#91449 = B_SPLINE_CURVE_WITH_KNOTS ( 'NONE', 3,
 ( #81870, #41525, #80596, #255353, #79320, #235838, #76767, #117191, #13285, #37674, #238416, #196714, #119779, #59748, #161468, #18079, #139290, #20674, #141875 ),
 .UNSPECIFIED., .F., .F.,
 ( 4, 3, 3, 3, 3, 3, 4 ),
 ( 0.000000000000000000, 1.655171619026302737E-05, 2.773500582847661863E-05, 5.941817267377570179E-05, 0.0001114174635873301661, 0.0001914169455916044462, 0.0002627181070750214849 ),
 .UNSPECIFIED. ) ;
#91451 = TOROIDAL_SURFACE ( 'NONE', #237193, 12.97499999999999609, 0.1000000000000000056 ) ;
#91452 = ORIENTED_EDGE ( 'NONE', *, *, #159550, .F. ) ;
#91453 = ORIENTED_EDGE ( 'NONE', *, *, #180410, .T. ) ;
#91454 = CARTESIAN_POINT ( 'NONE',  ( -22.60000000000080789, 75.95218301954709261, -181.7731299156771172 ) ) ;
#91455 = LINE ( 'NONE', #255601, #73231 ) ;
#91456 = DIRECTION ( 'NONE',  ( 0.000000000000000000, -0.8700118002898321601, 0.4930308989875230030 ) ) ;
#91457 = CYLINDRICAL_SURFACE ( 'NONE', #216134, 9.500000000000001776 ) ;
#91458 = CIRCLE ( 'NONE', #216345, 0.09999999999999986677 ) ;
#91459 = ADVANCED_FACE ( 'NONE', ( #5486 ), #203721, .T. ) ;
#91460 = VECTOR ( 'NONE', #28728, 1000.000000000000227 ) ;
#91461 = FACE_OUTER_BOUND ( 'NONE', #70977, .T. ) ;
#91462 = CARTESIAN_POINT ( 'NONE',  ( 18.50000000000000355, -9.421074344976016590, -73.82447205943003610 ) ) ;
#91463 = DIRECTION ( 'NONE',  ( -1.000000000000000000, 0.000000000000000000, 0.000000000000000000 ) ) ;
#91464 = ORIENTED_EDGE ( 'NONE', *, *, #44551, .F. ) ;
#91466 = CARTESIAN_POINT ( 'NONE',  ( 20.94999999999999574, -1.360870587180885716, -175.5729979270909382 ) ) ;
#91465 = CIRCLE ( 'NONE', #49760, 0.09999999999999939493 ) ;
#91467 = EDGE_LOOP ( 'NONE', ( #24138, #77385, #5532, #118181 ) ) ;
#91469 = DIRECTION ( 'NONE',  ( 0.000000000000000000, 0.2128009952263601734, -0.9770955615653315052 ) ) ;
#91468 = CARTESIAN_POINT ( 'NONE',  ( -21.04999999999999716, 69.69982018209549324, -170.0745903664056016 ) ) ;
#91470 = VERTEX_POINT ( 'NONE', #4218 ) ;
#91471 = CARTESIAN_POINT ( 'NONE',  ( 21.30000000000002558, 7.128833340093095217, -233.7327013124392749 ) ) ;
#91472 = CARTESIAN_POINT ( 'NONE',  ( 20.94999999999999929, 76.00000000001229239, -157.1481074845243882 ) ) ;
#91473 = DIRECTION ( 'NONE',  ( -0.000000000000000000, -0.000000000000000000, 1.000000000000000000 ) ) ;
#91474 = ADVANCED_FACE ( 'NONE', ( #32500 ), #50704, .T. ) ;
#91475 = CARTESIAN_POINT ( 'NONE',  ( 20.73486653747088937, 18.94215925855735705, -231.2688971919497760 ) ) ;
#91476 = ORIENTED_EDGE ( 'NONE', *, *, #33406, .F. ) ;
#91478 = VERTEX_POINT ( 'NONE', #152434 ) ;
#91477 = CARTESIAN_POINT ( 'NONE',  ( -21.05000000000000071, 87.41227409416235616, -200.5231074845242745 ) ) ;
#91479 = EDGE_CURVE ( 'NONE', #80932, #9718, #89601, .T. ) ;
#91481 = DIRECTION ( 'NONE',  ( 0.000000000000000000, 0.2617529984165031243, 0.9651348961777157509 ) ) ;
#91480 = DIRECTION ( 'NONE',  ( 0.000000000000000000, 0.000000000000000000, 1.000000000000000000 ) ) ;
#91483 = ORIENTED_EDGE ( 'NONE', *, *, #234520, .T. ) ;
#91482 = DIRECTION ( 'NONE',  ( 0.000000000000000000, 1.000000000000000000, 0.000000000000000000 ) ) ;
#91484 = CIRCLE ( 'NONE', #104111, 0.5000000000000004441 ) ;
#91485 = ORIENTED_EDGE ( 'NONE', *, *, #49592, .F. ) ;
#91487 = ADVANCED_FACE ( 'NONE', ( #223266 ), #156294, .T. ) ;
#91486 = CARTESIAN_POINT ( 'NONE',  ( 23.14999999999999503, 9.028068219309963283, -211.6732836666006961 ) ) ;
#91488 = DIRECTION ( 'NONE',  ( 0.000000000000000000, 0.000000000000000000, 1.000000000000000000 ) ) ;
#91490 = EDGE_CURVE ( 'NONE', #23645, #166894, #231290, .T. ) ;
#91489 = VERTEX_POINT ( 'NONE', #31218 ) ;
#91491 = VERTEX_POINT ( 'NONE', #132856 ) ;
#91492 = FACE_OUTER_BOUND ( 'NONE', #208878, .T. ) ;
#91493 = FACE_OUTER_BOUND ( 'NONE', #144416, .T. ) ;
#91494 = ORIENTED_EDGE ( 'NONE', *, *, #157329, .F. ) ;
#91495 = DIRECTION ( 'NONE',  ( 0.000000000000000000, 0.000000000000000000, -1.000000000000000000 ) ) ;
#91496 = AXIS2_PLACEMENT_3D ( 'NONE', #25642, #26953, #166466 ) ;
#91497 = EDGE_CURVE ( 'NONE', #68843, #205409, #97971, .T. ) ;
#91498 = AXIS2_PLACEMENT_3D ( 'NONE', #183948, #146097, #206085 ) ;
#91499 = VERTEX_POINT ( 'NONE', #44651 ) ;
#91500 = AXIS2_PLACEMENT_3D ( 'NONE', #239239, #41064, #100952 ) ;
#91501 = VECTOR ( 'NONE', #133000, 1000.000000000000000 ) ;
#91502 = DIRECTION ( 'NONE',  ( 0.000000000000000000, 0.000000000000000000, 1.000000000000000000 ) ) ;
#91503 = EDGE_CURVE ( 'NONE', #168221, #138337, #172878, .T. ) ;
#91504 = EDGE_LOOP ( 'NONE', ( #12759, #174468, #249871, #158278, #19689 ) ) ;
#91505 = CIRCLE ( 'NONE', #24892, 0.4000000000000044631 ) ;
#91506 = ORIENTED_EDGE ( 'NONE', *, *, #235136, .F. ) ;
#91507 = CARTESIAN_POINT ( 'NONE',  ( 20.75572585718056473, 18.81329300187470821, -229.9153261448354613 ) ) ;
#91508 = VERTEX_POINT ( 'NONE', #45925 ) ;
#91509 = EDGE_CURVE ( 'NONE', #68843, #50987, #18880, .T. ) ;
#91510 = DIRECTION ( 'NONE',  ( 1.000000000000000000, 0.000000000000000000, 0.000000000000000000 ) ) ;
#91511 = EDGE_LOOP ( 'NONE', ( #25260, #142855, #114963, #1836 ) ) ;
#91513 = ORIENTED_EDGE ( 'NONE', *, *, #220957, .T. ) ;
#91512 = DIRECTION ( 'NONE',  ( 1.000000000000000000, 0.000000000000000000, 0.000000000000000000 ) ) ;
#91514 = ORIENTED_EDGE ( 'NONE', *, *, #249128, .F. ) ;
#91515 = DIRECTION ( 'NONE',  ( -0.000000000000000000, 6.982962677686266711E-15, -1.000000000000000000 ) ) ;
#91516 = AXIS2_PLACEMENT_3D ( 'NONE', #135252, #229253, #131412 ) ;
#91518 = VERTEX_POINT ( 'NONE', #35065 ) ;
#91517 = EDGE_CURVE ( 'NONE', #169022, #136640, #202057, .T. ) ;
#91521 = ORIENTED_EDGE ( 'NONE', *, *, #220734, .F. ) ;
#91520 = EDGE_LOOP ( 'NONE', ( #193417, #208605, #28951, #206323 ) ) ;
#91519 = CARTESIAN_POINT ( 'NONE',  ( 23.15000000000000213, 85.00000000001251976, -179.9170766071767389 ) ) ;
#91522 = VECTOR ( 'NONE', #233553, 1000.000000000000000 ) ;
#91523 = EDGE_CURVE ( 'NONE', #112086, #56955, #6411, .T. ) ;
#91524 = CARTESIAN_POINT ( 'NONE',  ( 16.87683809663749557, 63.08573235307424198, -213.1276215869287967 ) ) ;
#91525 = EDGE_LOOP ( 'NONE', ( #176807, #154837, #159488, #174042 ) ) ;
#91526 = DIRECTION ( 'NONE',  ( 0.000000000000000000, 0.000000000000000000, -1.000000000000000000 ) ) ;
#91527 = ORIENTED_EDGE ( 'NONE', *, *, #94340, .F. ) ;
#91528 = FACE_OUTER_BOUND ( 'NONE', #68013, .T. ) ;
#91530 = ORIENTED_EDGE ( 'NONE', *, *, #136993, .T. ) ;
#91529 = CARTESIAN_POINT ( 'NONE',  ( 21.14999999999999858, 76.00000000001165290, -69.42310748452432279 ) ) ;
#91531 = CYLINDRICAL_SURFACE ( 'NONE', #167300, 11.80000000000000426 ) ;
#91532 = ORIENTED_EDGE ( 'NONE', *, *, #186012, .F. ) ;
#91534 = EDGE_CURVE ( 'NONE', #65772, #99108, #212396, .T. ) ;
#91533 = B_SPLINE_CURVE_WITH_KNOTS ( 'NONE', 3,
 ( #116457, #176442, #60308, #139844, #180278, #255899, #156887 ),
 .UNSPECIFIED., .F., .F.,
 ( 4, 3, 4 ),
 ( 0.000000000000000000, 0.0007844235214594269838, 0.001767853679404345069 ),
 .UNSPECIFIED. ) ;
#91535 = CARTESIAN_POINT ( 'NONE',  ( 21.05000000000000071, 65.43728505328341782, -95.56630537887993171 ) ) ;
#91536 = CARTESIAN_POINT ( 'NONE',  ( 18.49999999999999289, 65.55993210786772352, -111.7559897356389911 ) ) ;
#91537 = EDGE_CURVE ( 'NONE', #162728, #194468, #193682, .T. ) ;
#91538 = EDGE_LOOP ( 'NONE', ( #74492, #98581, #154153, #95692, #145860, #5253 ) ) ;
#91539 = FACE_OUTER_BOUND ( 'NONE', #134200, .T. ) ;
#91540 = DIRECTION ( 'NONE',  ( 1.000000000000000000, 0.000000000000000000, 0.000000000000000000 ) ) ;
#91541 = ORIENTED_EDGE ( 'NONE', *, *, #165798, .T. ) ;
#91543 = ORIENTED_EDGE ( 'NONE', *, *, #209895, .F. ) ;
#91542 = CARTESIAN_POINT ( 'NONE',  ( -20.94999999999999929, 74.16465844978715438, -57.96795619196134908 ) ) ;
#91544 = DIRECTION ( 'NONE',  ( 1.000000000000000000, 0.000000000000000000, 0.000000000000000000 ) ) ;
#91546 = ORIENTED_EDGE ( 'NONE', *, *, #59474, .T. ) ;
#91545 = ORIENTED_EDGE ( 'NONE', *, *, #114109, .T. ) ;
#91547 = ORIENTED_EDGE ( 'NONE', *, *, #166193, .F. ) ;
#91548 = DIRECTION ( 'NONE',  ( -1.020425574104004196E-15, -1.210927747993693964E-31, 1.000000000000000000 ) ) ;
#91549 = ORIENTED_EDGE ( 'NONE', *, *, #239549, .T. ) ;
#91550 = VERTEX_POINT ( 'NONE', #213662 ) ;
#91551 = DIRECTION ( 'NONE',  ( 1.000000000000000000, 0.000000000000000000, -0.000000000000000000 ) ) ;
#91552 = VERTEX_POINT ( 'NONE', #196652 ) ;
#91553 = DIRECTION ( 'NONE',  ( 0.000000000000000000, 0.000000000000000000, 1.000000000000000000 ) ) ;
#91554 = CYLINDRICAL_SURFACE ( 'NONE', #40037, 0.1000000000000028644 ) ;
#91555 = ORIENTED_EDGE ( 'NONE', *, *, #7249, .F. ) ;
#91556 = ORIENTED_EDGE ( 'NONE', *, *, #122807, .F. ) ;
#91557 = CARTESIAN_POINT ( 'NONE',  ( 20.94999999999999929, -3.664072692419559907, -226.4691047342518857 ) ) ;
#91559 = VERTEX_POINT ( 'NONE', #75465 ) ;
#91558 = AXIS2_PLACEMENT_3D ( 'NONE', #201065, #141102, #160691 ) ;
#91560 = ADVANCED_FACE ( 'NONE', ( #257867 ), #157585, .T. ) ;
#91561 = VECTOR ( 'NONE', #5110, 1000.000000000000000 ) ;
#91562 = CARTESIAN_POINT ( 'NONE',  ( -18.59999999999999787, 74.16465844978715438, -57.96795619196135618 ) ) ;
#91563 = EDGE_LOOP ( 'NONE', ( #150523, #188996, #32876, #44871, #5511 ) ) ;
#91564 = VECTOR ( 'NONE', #184638, 1000.000000000000000 ) ;
#91565 = LINE ( 'NONE', #188100, #225068 ) ;
#91567 = ORIENTED_EDGE ( 'NONE', *, *, #16429, .T. ) ;
#91566 = CARTESIAN_POINT ( 'NONE',  ( -20.94999999999999929, 1.115600667400684642E-11, -55.30000000000000426 ) ) ;
#91568 = DIRECTION ( 'NONE',  ( -1.000000000000000000, -0.000000000000000000, -0.000000000000000000 ) ) ;
#91569 = CARTESIAN_POINT ( 'NONE',  ( 20.94999999999999929, 10.29270135741298731, -172.9573618871519329 ) ) ;
#91570 = VECTOR ( 'NONE', #100902, 1000.000000000000114 ) ;
#91571 = CYLINDRICAL_SURFACE ( 'NONE', #31262, 0.09999999999999939493 ) ;
#91573 = CIRCLE ( 'NONE', #253870, 0.1000000000000028644 ) ;
#91572 = CARTESIAN_POINT ( 'NONE',  ( 18.49999999999808864, 33.89065584167517642, -236.2246875831560260 ) ) ;
#91574 = DIRECTION ( 'NONE',  ( 0.000000000000000000, -1.000000000000000000, 0.000000000000000000 ) ) ;
#91575 = LINE ( 'NONE', #92845, #148086 ) ;
#91576 = FACE_OUTER_BOUND ( 'NONE', #147463, .T. ) ;
#91577 = DIRECTION ( 'NONE',  ( 1.734723475976817507E-14, 0.000000000000000000, -1.000000000000000000 ) ) ;
#91578 = CARTESIAN_POINT ( 'NONE',  ( 22.40000000000020819, 76.10085836911211743, -181.7726746080140572 ) ) ;
#91579 = DIRECTION ( 'NONE',  ( -0.7071067811865412445, -0.2890913453339235550, 0.6453109281989813928 ) ) ;
#91580 = EDGE_CURVE ( 'NONE', #74710, #166612, #252771, .T. ) ;
#91581 = ORIENTED_EDGE ( 'NONE', *, *, #153874, .F. ) ;
#91582 = CIRCLE ( 'NONE', #24967, 0.09999999999999939493 ) ;
#91583 = CIRCLE ( 'NONE', #66642, 0.09999999999999939493 ) ;
#91584 = AXIS2_PLACEMENT_3D ( 'NONE', #234995, #56326, #103158 ) ;
#91585 = CIRCLE ( 'NONE', #249806, 0.1000000000000009492 ) ;
#91586 = CIRCLE ( 'NONE', #153998, 0.09999999999999939493 ) ;
#91588 = ORIENTED_EDGE ( 'NONE', *, *, #31493, .T. ) ;
#91587 = EDGE_LOOP ( 'NONE', ( #35200, #5784, #124641, #237084 ) ) ;
#91589 = ORIENTED_EDGE ( 'NONE', *, *, #42483, .F. ) ;
#91590 = AXIS2_PLACEMENT_3D ( 'NONE', #794, #79051, #94789 ) ;
#91591 = CARTESIAN_POINT ( 'NONE',  ( -20.65000000000000568, 68.75000000001209344, -127.2731074845243597 ) ) ;
#91592 = CARTESIAN_POINT ( 'NONE',  ( -23.25000000000000000, 10.33248238083634440, -139.5948465439131780 ) ) ;
#91594 = DIRECTION ( 'NONE',  ( 0.000000000000000000, 0.000000000000000000, -1.000000000000000000 ) ) ;
#91593 = CARTESIAN_POINT ( 'NONE',  ( 22.39999999999999858, 76.00000000001237765, -170.0231074845243597 ) ) ;
#91595 = EDGE_LOOP ( 'NONE', ( #150880, #239354, #214987 ) ) ;
#91596 = ORIENTED_EDGE ( 'NONE', *, *, #79182, .T. ) ;
#91597 =( NAMED_UNIT ( * ) SI_UNIT ( $, .STERADIAN. ) SOLID_ANGLE_UNIT ( ) );
#91598 = CARTESIAN_POINT ( 'NONE',  ( 22.39999999999999503, 64.35000000001237197, -170.1231074845244393 ) ) ;
#91599 = DIRECTION ( 'NONE',  ( 0.000000000000000000, -1.734723475976811630E-15, 1.000000000000000000 ) ) ;
#91600 = DIRECTION ( 'NONE',  ( 0.000000000000000000, -7.086529944415894657E-15, 1.000000000000000000 ) ) ;
#91601 = VERTEX_POINT ( 'NONE', #216212 ) ;
#91602 = VERTEX_POINT ( 'NONE', #58405 ) ;
#91603 = CARTESIAN_POINT ( 'NONE',  ( 20.73486653747088937, 68.25000000001205080, -127.2731074845243597 ) ) ;
#91604 = DIRECTION ( 'NONE',  ( 0.000000000000000000, 0.8814952561688442767, -0.4721928772777324035 ) ) ;
#91605 = DIRECTION ( 'NONE',  ( -1.000000000000000000, -0.000000000000000000, -0.000000000000000000 ) ) ;
#91607 = ORIENTED_EDGE ( 'NONE', *, *, #233730, .T. ) ;
#91606 = DIRECTION ( 'NONE',  ( -0.000000000000000000, -1.000000000000000000, 0.000000000000000000 ) ) ;
#91608 = DIRECTION ( 'NONE',  ( -0.7071067811865474617, 0.7071067811865474617, 4.937700262164531476E-15 ) ) ;
#91609 = CARTESIAN_POINT ( 'NONE',  ( -23.15000000000000213, 48.79765034352288922, -253.5326144460178170 ) ) ;
#91610 = CARTESIAN_POINT ( 'NONE',  ( 23.15000000000000213, 85.00000000001197975, -112.9170766071766820 ) ) ;
#91611 = CARTESIAN_POINT ( 'NONE',  ( 18.46947024752537203, 85.50929715716800672, -96.03641803582634395 ) ) ;
#91612 = ORIENTED_EDGE ( 'NONE', *, *, #175632, .T. ) ;
#91613 = DIRECTION ( 'NONE',  ( -0.000000000000000000, -0.000000000000000000, 1.000000000000000000 ) ) ;
#91614 = VECTOR ( 'NONE', #189316, 1000.000000000000000 ) ;
#91615 = DIRECTION ( 'NONE',  ( 0.000000000000000000, 0.000000000000000000, 1.000000000000000000 ) ) ;
#91617 = DIRECTION ( 'NONE',  ( 0.000000000000000000, 0.000000000000000000, -1.000000000000000000 ) ) ;
#91616 = CARTESIAN_POINT ( 'NONE',  ( -23.15000000000000213, -9.499999999988846255, -191.1060308773475356 ) ) ;
#91618 = CYLINDRICAL_SURFACE ( 'NONE', #95531, 0.09999999999999939493 ) ;
#91619 = CIRCLE ( 'NONE', #137391, 0.1000000000000028644 ) ;
#91621 = EDGE_CURVE ( 'NONE', #192597, #220241, #239470, .T. ) ;
#91620 = CARTESIAN_POINT ( 'NONE',  ( -18.59999999999999787, -1.835859311432481045, -145.5044391687985694 ) ) ;
#91622 = DIRECTION ( 'NONE',  ( 4.239556034732056743E-17, -0.1298341882520022972, -0.9915357197604853789 ) ) ;
#91623 = CARTESIAN_POINT ( 'NONE',  ( -16.81744102076748959, 66.05000000001153637, -48.67310748452439384 ) ) ;
#91624 = CARTESIAN_POINT ( 'NONE',  ( -18.39999999999999858, 64.52132590001305346, -160.7484142681837795 ) ) ;
#91625 = CARTESIAN_POINT ( 'NONE',  ( 18.49999999999999645, 1.162701749938009677, -8.099999999999999645 ) ) ;
#91627 = ORIENTED_EDGE ( 'NONE', *, *, #180719, .T. ) ;
#91626 = AXIS2_PLACEMENT_3D ( 'NONE', #195573, #235950, #217657 ) ;
#91628 = EDGE_LOOP ( 'NONE', ( #139557, #224809, #82403, #19094 ) ) ;
#91629 = VERTEX_POINT ( 'NONE', #94991 ) ;
#91630 = EDGE_CURVE ( 'NONE', #100213, #71501, #164645, .T. ) ;
#91631 = CARTESIAN_POINT ( 'NONE',  ( -21.14999999999999858, 1.115600667400684642E-11, -160.9593430482987344 ) ) ;
#91632 = CYLINDRICAL_SURFACE ( 'NONE', #140180, 0.09999999999999810429 ) ;
#91633 = EDGE_LOOP ( 'NONE', ( #96630, #65248 ) ) ;
#91634 = EDGE_CURVE ( 'NONE', #87151, #234897, #135393, .T. ) ;
#91635 = AXIS2_PLACEMENT_3D ( 'NONE', #47734, #106414, #110284 ) ;
#91636 = ORIENTED_EDGE ( 'NONE', *, *, #183118, .T. ) ;
#91637 = AXIS2_PLACEMENT_3D ( 'NONE', #59762, #62369, #161482 ) ;
#91638 =( NAMED_UNIT ( * ) PLANE_ANGLE_UNIT ( ) SI_UNIT ( $, .RADIAN. ) );
#91639 = EDGE_CURVE ( 'NONE', #260, #94806, #214511, .T. ) ;
#91640 = ORIENTED_EDGE ( 'NONE', *, *, #210026, .T. ) ;
#91641 = CYLINDRICAL_SURFACE ( 'NONE', #79422, 0.09999999999998898659 ) ;
#91642 = AXIS2_PLACEMENT_3D ( 'NONE', #35513, #133296, #234968 ) ;
#91643 = ORIENTED_EDGE ( 'NONE', *, *, #107843, .T. ) ;
#91644 =( BOUNDED_SURFACE ( )  B_SPLINE_SURFACE ( 3, 2, ( 
 ( #211103, #32507, #112018 ),
 ( #191566, #252777, #153753 ),
 ( #172017, #54585, #36333 ),
 ( #217494, #174604, #115853 ),
 ( #175844, #214948, #993 ),
 ( #234502, #195414, #238353 ),
 ( #216218, #256587, #257872 ),
 ( #75471, #213667, #194128 ),
 ( #77990, #79262, #19315 ),
 ( #16769, #197940, #98811 ) ),
 .UNSPECIFIED., .F., .F., .T. ) 
 B_SPLINE_SURFACE_WITH_KNOTS ( ( 4, 2, 2, 2, 4 ),
 ( 3, 3 ),
 ( 0.0001836757140119196091, 0.0004000170051583634982, 0.0005081876507315854835, 0.0005622729735181964490, 0.0006163582963048074145 ),
 ( 0.000000000000000000, 1.000000000000000000 ),
 .UNSPECIFIED. ) 
 GEOMETRIC_REPRESENTATION_ITEM ( )  RATIONAL_B_SPLINE_SURFACE ( (
 ( 1.000000000000000000, 0.7071067811865079378, 1.000000000000000000),
 ( 1.000000000000000000, 0.6461995200025473229, 1.000000000000000000),
 ( 1.000000000000000000, 0.5776453529555616306, 1.000000000000000000),
 ( 1.000000000000000000, 0.4585233068348677499, 1.000000000000000000),
 ( 1.000000000000000000, 0.4154092989938408254, 1.000000000000000000),
 ( 1.000000000000000000, 0.3550093145837127095, 1.000000000000000000),
 ( 1.000000000000000000, 0.3354498651688673228, 1.000000000000000000),
 ( 1.000000000000000000, 0.3060347992253271698, 1.000000000000000000),
 ( 1.000000000000000000, 0.2963555829628214955, 1.000000000000000000),
 ( 1.000000000000000000, 0.2966190024561043415, 1.000000000000000000) ) ) 
 REPRESENTATION_ITEM ( '' )  SURFACE ( )  );
#91645 = DIRECTION ( 'NONE',  ( -4.408576920032448588E-17, 0.8490545835447252943, 0.5283051335749948674 ) ) ;
#91646 = DIRECTION ( 'NONE',  ( 1.000000000000000000, 0.000000000000000000, 0.000000000000000000 ) ) ;
#91647 = DIRECTION ( 'NONE',  ( 2.952720810173289112E-16, 1.000000000000000000, 6.938893903907229955E-15 ) ) ;
#91648 = CARTESIAN_POINT ( 'NONE',  ( -20.64999999999999858, 1.115600667400684642E-11, -188.1249999999999716 ) ) ;
#91649 = CARTESIAN_POINT ( 'NONE',  ( 23.24999999999999645, 4.775700934579435675, -21.65123189595403375 ) ) ;
#91651 = VERTEX_POINT ( 'NONE', #114564 ) ;
#91650 = CARTESIAN_POINT ( 'NONE',  ( 23.14999999999999503, 61.90000000001248992, -175.6234050956638271 ) ) ;
#91653 = CARTESIAN_POINT ( 'NONE',  ( 21.97500000000000497, 66.25000000001151079, -48.27310748452438816 ) ) ;
#91652 = DIRECTION ( 'NONE',  ( 1.000000000000000000, -1.207181226542539700E-16, 2.694675058168174199E-16 ) ) ;
#91654 = EDGE_CURVE ( 'NONE', #217170, #92859, #60386, .T. ) ;
#91655 = DIRECTION ( 'NONE',  ( 0.000000000000000000, -1.000000000000000000, 0.000000000000000000 ) ) ;
#91656 = DIRECTION ( 'NONE',  ( 1.000000000000000000, 0.000000000000000000, 0.000000000000000000 ) ) ;
#91657 = CARTESIAN_POINT ( 'NONE',  ( 18.59999999999999076, 52.81534179157633702, -244.1198638051726277 ) ) ;
#91658 = DIRECTION ( 'NONE',  ( 0.000000000000000000, 0.8490545835447238510, 0.5283051335749973099 ) ) ;
#91659 = ORIENTED_EDGE ( 'NONE', *, *, #128994, .F. ) ;
#91660 = DIRECTION ( 'NONE',  ( 0.000000000000000000, 0.000000000000000000, -1.000000000000000000 ) ) ;
#91661 = AXIS2_PLACEMENT_3D ( 'NONE', #45918, #22526, #204969 ) ;
#91662 = DIRECTION ( 'NONE',  ( 0.000000000000000000, 0.8814952561688444987, -0.4721928772777320149 ) ) ;
#91663 = ORIENTED_EDGE ( 'NONE', *, *, #189185, .T. ) ;
#91664 = CARTESIAN_POINT ( 'NONE',  ( 18.59999999999999076, 74.16465844978787914, -158.4679561919613775 ) ) ;
#91665 = DIRECTION ( 'NONE',  ( 0.000000000000000000, -1.000000000000000000, 0.000000000000000000 ) ) ;
#91666 = DIRECTION ( 'NONE',  ( 1.000000000000000000, -7.304098846218133681E-16, -2.111765289898285610E-31 ) ) ;
#91667 = ORIENTED_EDGE ( 'NONE', *, *, #100010, .F. ) ;
#91668 = B_SPLINE_CURVE_WITH_KNOTS ( 'NONE', 3,
 ( #170289, #251045, #189813, #194960, #253609, #54131, #193661, #210651, #112835, #11173, #13734, #249780, #191115, #75023, #12470, #172859 ),
 .UNSPECIFIED., .F., .F.,
 ( 4, 3, 3, 3, 3, 4 ),
 ( 0.000000000000000000, 1.810570668009477602E-05, 2.740575833571357316E-05, 4.256816319435821725E-05, 5.213463471025588320E-05, 6.641585710718402133E-05 ),
 .UNSPECIFIED. ) ;
#91669 = EDGE_LOOP ( 'NONE', ( #235656, #125860, #232702, #239762 ) ) ;
#91670 = CARTESIAN_POINT ( 'NONE',  ( -21.05000000000000071, 1.835341550235567887, -112.0551512925630249 ) ) ;
#91671 = DIRECTION ( 'NONE',  ( -1.000000000000000000, -0.000000000000000000, -0.000000000000000000 ) ) ;
#91672 = VECTOR ( 'NONE', #72190, 999.9999999999998863 ) ;
#91673 = CARTESIAN_POINT ( 'NONE',  ( -21.05000000000000426, 65.63239632895212594, -242.1325452132893759 ) ) ;
#91675 = CARTESIAN_POINT ( 'NONE',  ( -21.64999999999999858, 10.05000000001113847, -180.2499999999999716 ) ) ;
#91674 = AXIS2_PLACEMENT_3D ( 'NONE', #223397, #61773, #42220 ) ;
#91676 = AXIS2_PLACEMENT_3D ( 'NONE', #116431, #197237, #215511 ) ;
#91679 = DIRECTION ( 'NONE',  ( 1.000000000000000000, -0.000000000000000000, 0.000000000000000000 ) ) ;
#91678 = TOROIDAL_SURFACE ( 'NONE', #20979, 11.70000000000000639, 0.1000000000000000056 ) ;
#91677 = DIRECTION ( 'NONE',  ( 0.000000000000000000, -1.000000000000000000, 0.000000000000000000 ) ) ;
#91680 = FACE_OUTER_BOUND ( 'NONE', #216612, .T. ) ;
#91681 = DIRECTION ( 'NONE',  ( 0.000000000000000000, 0.2617529984165152257, 0.9651348961777124202 ) ) ;
#91682 = DIRECTION ( 'NONE',  ( -1.000000000000000000, 0.000000000000000000, 0.000000000000000000 ) ) ;
#91683 = EDGE_LOOP ( 'NONE', ( #148200, #138754, #216053, #165967 ) ) ;
#91684 = LINE ( 'NONE', #135927, #39731 ) ;
#91685 = EDGE_CURVE ( 'NONE', #49235, #185953, #59996, .T. ) ;
#91687 = ORIENTED_EDGE ( 'NONE', *, *, #55570, .F. ) ;
#91686 = CARTESIAN_POINT ( 'NONE',  ( -18.59999999999999787, 77.25000000001209344, -128.5231074845242745 ) ) ;
#91688 = AXIS2_PLACEMENT_3D ( 'NONE', #85868, #205848, #187594 ) ;
#91689 = FACE_OUTER_BOUND ( 'NONE', #85201, .T. ) ;
#91690 = CARTESIAN_POINT ( 'NONE',  ( 20.85000000000000142, -1.835859311432481045, -112.1044391687985780 ) ) ;
#91691 = CARTESIAN_POINT ( 'NONE',  ( -16.77431908686106610, 66.05419424549407381, -123.8589467021746060 ) ) ;
#91692 = DIRECTION ( 'NONE',  ( 0.000000000000000000, 2.891205793294679805E-16, -1.000000000000000000 ) ) ;
#91694 = EDGE_LOOP ( 'NONE', ( #73902, #129315, #96217, #221451 ) ) ;
#91693 = CARTESIAN_POINT ( 'NONE',  ( 21.93340585972002543, 68.67585297715832837, -136.5231074845243597 ) ) ;
#91695 = DIRECTION ( 'NONE',  ( 1.000000000000000000, -6.938893903907222067E-15, -4.845403715540888588E-29 ) ) ;
#91696 = DIRECTION ( 'NONE',  ( -3.469446951953635015E-14, 1.000000000000000000, 0.000000000000000000 ) ) ;
#91697 = PLANE ( 'NONE',  #121901 ) ;
#91698 = DIRECTION ( 'NONE',  ( 0.000000000000000000, -0.9126074666063545004, -0.4088369013363783999 ) ) ;
#91700 = EDGE_CURVE ( 'NONE', #16660, #198941, #137953, .T. ) ;
#91699 =( BOUNDED_SURFACE ( )  B_SPLINE_SURFACE ( 3, 2, ( 
 ( #133852, #93431, #36054 ),
 ( #56848, #215942, #213381 ),
 ( #32212, #174320, #33519 ),
 ( #196388, #114289, #95994 ) ),
 .UNSPECIFIED., .F., .F., .F. ) 
 B_SPLINE_SURFACE_WITH_KNOTS ( ( 4, 4 ),
 ( 3, 3 ),
 ( 1.040834085586084257E-17, 0.001979672783031562362 ),
 ( 0.000000000000000000, 1.000000000000000000 ),
 .UNSPECIFIED. ) 
 GEOMETRIC_REPRESENTATION_ITEM ( )  RATIONAL_B_SPLINE_SURFACE ( (
 ( 1.000000000000000000, 0.7103081912008197829, 1.000000000000000000),
 ( 1.000000000000000000, 0.7104998333558716350, 1.000000000000000000),
 ( 1.000000000000000000, 0.7107238315755427527, 1.000000000000000000),
 ( 1.000000000000000000, 0.7110073749539292942, 1.000000000000000000) ) ) 
 REPRESENTATION_ITEM ( '' )  SURFACE ( )  );
#91701 = EDGE_LOOP ( 'NONE', ( #88545, #207375, #153710, #206318 ) ) ;
#91702 = DIRECTION ( 'NONE',  ( 2.715809747126116015E-16, -0.9770955615653309501, -0.2128009952263628102 ) ) ;
#91704 = ORIENTED_EDGE ( 'NONE', *, *, #110517, .T. ) ;
#91703 = VECTOR ( 'NONE', #125961, 1000.000000000000000 ) ;
#91705 = AXIS2_PLACEMENT_3D ( 'NONE', #92421, #136450, #252560 ) ;
#91706 = EDGE_CURVE ( 'NONE', #197810, #92572, #38889, .T. ) ;
#91707 = ADVANCED_FACE ( 'NONE', ( #118423 ), #197934, .F. ) ;
#91708 = CARTESIAN_POINT ( 'NONE',  ( -16.97092634996626970, 65.99911103366400766, -90.39296471822643753 ) ) ;
#91709 = ORIENTED_EDGE ( 'NONE', *, *, #211141, .T. ) ;
#91710 = CARTESIAN_POINT ( 'NONE',  ( 0.9000000000000546452, 67.75000000001118394, -14.06452884076210630 ) ) ;
#91711 = ORIENTED_EDGE ( 'NONE', *, *, #107365, .F. ) ;
#91712 = DIRECTION ( 'NONE',  ( 0.000000000000000000, 0.000000000000000000, -1.000000000000000000 ) ) ;
#91713 = PLANE ( 'NONE',  #158303 ) ;
#91714 = ADVANCED_FACE ( 'NONE', ( #16763 ), #168272, .F. ) ;
#91715 = CARTESIAN_POINT ( 'NONE',  ( -20.54999999999999716, -8.730841121484170131, -191.4019252810156217 ) ) ;
#91716 = ORIENTED_EDGE ( 'NONE', *, *, #257669, .T. ) ;
#91717 = EDGE_CURVE ( 'NONE', #69974, #128036, #84356, .T. ) ;
#91718 = EDGE_CURVE ( 'NONE', #161528, #80243, #123544, .T. ) ;
#91719 = CARTESIAN_POINT ( 'NONE',  ( -16.83233564386404879, 9.930221796584600469, -12.77547933652440726 ) ) ;
#91720 = FACE_OUTER_BOUND ( 'NONE', #247741, .T. ) ;
#91721 = CYLINDRICAL_SURFACE ( 'NONE', #224751, 0.1000000000000010741 ) ;
#91722 = CARTESIAN_POINT ( 'NONE',  ( 12.84435279558019793, 9.410708747047079825, -18.06920840584410115 ) ) ;
#91724 = CARTESIAN_POINT ( 'NONE',  ( -20.00857864376270001, 9.250000000011157297, -146.3500000000000227 ) ) ;
#91723 = AXIS2_PLACEMENT_3D ( 'NONE', #179049, #39537, #177756 ) ;
#91725 = EDGE_LOOP ( 'NONE', ( #143440, #255681, #156977, #248105, #13138 ) ) ;
#91726 = CARTESIAN_POINT ( 'NONE',  ( -23.15000000000000213, 4.150000000011156764, -188.6499999999999488 ) ) ;
#91727 = ORIENTED_EDGE ( 'NONE', *, *, #123909, .F. ) ;
#91729 = EDGE_LOOP ( 'NONE', ( #90219, #104199, #206577, #67033 ) ) ;
#91728 = CARTESIAN_POINT ( 'NONE',  ( 21.12802099929860944, 67.21944740978965172, -90.77491749959274614 ) ) ;
#91730 = ADVANCED_FACE ( 'NONE', ( #102663 ), #200513, .F. ) ;
#91731 = ORIENTED_EDGE ( 'NONE', *, *, #110604, .F. ) ;
#91732 = CARTESIAN_POINT ( 'NONE',  ( 21.05000000000000071, 65.26666169030359299, -222.4689051838086300 ) ) ;
#91733 = VERTEX_POINT ( 'NONE', #83089 ) ;
#91734 = DIRECTION ( 'NONE',  ( 0.000000000000000000, 0.000000000000000000, 1.000000000000000000 ) ) ;
#91735 = CARTESIAN_POINT ( 'NONE',  ( 22.00356870068866755, 5.513940439853673043E-12, -26.24575763824345387 ) ) ;
#91736 = ADVANCED_FACE ( 'NONE', ( #184793 ), #121009, .F. ) ;
#91737 = FACE_OUTER_BOUND ( 'NONE', #86281, .T. ) ;
#91738 = VECTOR ( 'NONE', #240109, 1000.000000000000114 ) ;
#91739 = ORIENTED_EDGE ( 'NONE', *, *, #109981, .T. ) ;
#91740 = EDGE_CURVE ( 'NONE', #51901, #90864, #4843, .T. ) ;
#91741 = ADVANCED_FACE ( 'NONE', ( #101355 ), #3587, .F. ) ;
#91742 = CARTESIAN_POINT ( 'NONE',  ( -16.88460203013675098, 66.04524099677580296, -48.65721567498616906 ) ) ;
#91743 = DIRECTION ( 'NONE',  ( -1.000000000000000000, -1.794895427898102820E-16, -3.909090864890033875E-17 ) ) ;
#91744 = ORIENTED_EDGE ( 'NONE', *, *, #164723, .F. ) ;
#91745 = B_SPLINE_CURVE_WITH_KNOTS ( 'NONE', 3,
 ( #223662, #5897, #22942, #140268, #183276, #184541, #25494, #200271, #84110, #120761, #122015, #102412, #124595, #144121, #65891, #159879, #4617, #101107, #221100 ),
 .UNSPECIFIED., .F., .F.,
 ( 4, 3, 3, 3, 3, 3, 4 ),
 ( 0.0001624081864585828479, 0.0001685232196531679001, 0.0001764526673566893435, 0.0001916878551483146103, 0.0002009890782182573881, 0.0002238845907555200366, 0.0002283406619926344556 ),
 .UNSPECIFIED. ) ;
#91747 = VERTEX_POINT ( 'NONE', #141812 ) ;
#91746 = CARTESIAN_POINT ( 'NONE',  ( 21.05000000000000071, 5.850000000000001421, -23.36750277572207679 ) ) ;
#91748 = LINE ( 'NONE', #189574, #6847 ) ;
#91749 = AXIS2_PLACEMENT_3D ( 'NONE', #123797, #224161, #6402 ) ;
#91750 = AXIS2_PLACEMENT_3D ( 'NONE', #223863, #21840, #45247 ) ;
#91751 = ORIENTED_EDGE ( 'NONE', *, *, #14430, .T. ) ;
#91752 = CARTESIAN_POINT ( 'NONE',  ( 20.99999999999999645, 66.25000000001188027, -90.37310748452436826 ) ) ;
#91753 = CARTESIAN_POINT ( 'NONE',  ( -12.84409460144753723, 66.58931770574410791, -121.0919640425761088 ) ) ;
#91754 = CARTESIAN_POINT ( 'NONE',  ( -20.87600722750343252, 18.41291479239798079, -236.9963116028434058 ) ) ;
#91755 = ORIENTED_EDGE ( 'NONE', *, *, #39142, .F. ) ;
#91756 = DIRECTION ( 'NONE',  ( -1.000000000000000000, 0.000000000000000000, 0.000000000000000000 ) ) ;
#91757 = EDGE_CURVE ( 'NONE', #107478, #231520, #23011, .T. ) ;
#91758 = EDGE_CURVE ( 'NONE', #192701, #204834, #81807, .T. ) ;
#91759 = CYLINDRICAL_SURFACE ( 'NONE', #93280, 2.000000000000001776 ) ;
#91760 = CIRCLE ( 'NONE', #179264, 11.90000000000000746 ) ;
#91761 = CIRCLE ( 'NONE', #145910, 0.1000000000000096922 ) ;
#91762 = CARTESIAN_POINT ( 'NONE',  ( -23.25000000000000000, 76.00000000001267608, -203.5231074845243597 ) ) ;
#91763 = EDGE_CURVE ( 'NONE', #51917, #192876, #214688, .T. ) ;
#91764 = CIRCLE ( 'NONE', #191571, 11.65000000000000746 ) ;
#91765 = CIRCLE ( 'NONE', #83541, 0.8750000000000007772 ) ;
#91766 = ORIENTED_EDGE ( 'NONE', *, *, #18418, .F. ) ;
#91768 = CARTESIAN_POINT ( 'NONE',  ( -20.85000000000000142, 0.1610488207298751417, -200.7158101556397582 ) ) ;
#91767 = VECTOR ( 'NONE', #192304, 1000.000000000000227 ) ;
#91769 = AXIS2_PLACEMENT_3D ( 'NONE', #77180, #220556, #117598 ) ;
#91770 = VERTEX_POINT ( 'NONE', #63556 ) ;
#91771 = CARTESIAN_POINT ( 'NONE',  ( -20.64999999999999858, 18.56623428888383387, -239.8594038951179073 ) ) ;
#91772 = FACE_OUTER_BOUND ( 'NONE', #140127, .T. ) ;
#91774 = VERTEX_POINT ( 'NONE', #20614 ) ;
#91773 = DIRECTION ( 'NONE',  ( 1.000000000000000000, 0.000000000000000000, -0.000000000000000000 ) ) ;
#91775 = CARTESIAN_POINT ( 'NONE',  ( 20.94999999999999929, 12.10919762232931163, -206.2073353557311748 ) ) ;
#91776 = CARTESIAN_POINT ( 'NONE',  ( 21.14261333020286671, 65.28430735075666291, -57.27310748452418920 ) ) ;
#91777 = DIRECTION ( 'NONE',  ( 0.000000000000000000, -0.7049548389604960441, 0.7092521942343085195 ) ) ;
#91778 = CARTESIAN_POINT ( 'NONE',  ( -16.90138253750127006, 9.949999999999983302, -20.71156270790459075 ) ) ;
#91779 = DIRECTION ( 'NONE',  ( 1.000000000000000000, 0.000000000000000000, 0.000000000000000000 ) ) ;
#91780 = ADVANCED_FACE ( 'NONE', ( #221334 ), #139226, .F. ) ;
#91781 = CARTESIAN_POINT ( 'NONE',  ( -18.59999999999999787, -1.164121893230052995, -108.4148480855716485 ) ) ;
#91782 = CARTESIAN_POINT ( 'NONE',  ( 21.11101077988997332, 6.423684734737198809, -66.98471473108573093 ) ) ;
#91783 = CIRCLE ( 'NONE', #71141, 0.1000000000000013933 ) ;
#91785 = ORIENTED_EDGE ( 'NONE', *, *, #94182, .F. ) ;
#91784 = CARTESIAN_POINT ( 'NONE',  ( -21.07928932188134041, 69.67148334361884565, -136.6220026301787414 ) ) ;
#91786 = EDGE_CURVE ( 'NONE', #31422, #89321, #14824, .T. ) ;
#91788 = EDGE_CURVE ( 'NONE', #117140, #297, #102235, .T. ) ;
#91787 = LINE ( 'NONE', #93060, #55865 ) ;
#91789 = DIRECTION ( 'NONE',  ( 0.000000000000000000, 0.9998779222360096863, -0.01562500000001061998 ) ) ;
#91790 = ADVANCED_FACE ( 'NONE', ( #24472 ), #987, .T. ) ;
#91791 = DIRECTION ( 'NONE',  ( -2.952720810173289112E-16, -1.000000000000000000, -6.982962677686266711E-15 ) ) ;
#91792 = CARTESIAN_POINT ( 'NONE',  ( -20.54999999999999716, 66.65000000001222702, -148.7731074845244166 ) ) ;
#91793 = ADVANCED_FACE ( 'NONE', ( #100099 ), #110390, .T. ) ;
#91794 = EDGE_LOOP ( 'NONE', ( #230324, #112825, #132702, #199917 ) ) ;
#91795 = AXIS2_PLACEMENT_3D ( 'NONE', #171077, #194472, #73252 ) ;
#91796 = DIRECTION ( 'NONE',  ( 1.000000000000000000, -0.000000000000000000, 0.000000000000000000 ) ) ;
#91797 = AXIS2_PLACEMENT_3D ( 'NONE', #42775, #2345, #23242 ) ;
#91798 = LINE ( 'NONE', #90499, #103300 ) ;
#91799 = ORIENTED_EDGE ( 'NONE', *, *, #96181, .F. ) ;
#91800 = AXIS2_PLACEMENT_3D ( 'NONE', #246237, #104130, #106701 ) ;
#91802 = EDGE_CURVE ( 'NONE', #160911, #234077, #209490, .T. ) ;
#91801 = DIRECTION ( 'NONE',  ( 0.000000000000000000, 0.000000000000000000, 1.000000000000000000 ) ) ;
#91803 = EDGE_CURVE ( 'NONE', #158463, #58200, #210779, .T. ) ;
#91804 = PLANE ( 'NONE',  #22297 ) ;
#91805 = ORIENTED_EDGE ( 'NONE', *, *, #24774, .T. ) ;
#91806 = CARTESIAN_POINT ( 'NONE',  ( -17.29838795458828571, 65.62845014206074268, -47.41836620190301943 ) ) ;
#91807 = VERTEX_POINT ( 'NONE', #90816 ) ;
#91808 = EDGE_CURVE ( 'NONE', #111477, #101051, #66135, .T. ) ;
#91809 = FACE_OUTER_BOUND ( 'NONE', #101801, .T. ) ;
#91811 = ORIENTED_EDGE ( 'NONE', *, *, #47315, .T. ) ;
#91810 = CARTESIAN_POINT ( 'NONE',  ( 22.00356870072048920, 76.00000000002594902, -143.7773498462486259 ) ) ;
#91812 = VERTEX_POINT ( 'NONE', #226468 ) ;
#91813 = AXIS2_PLACEMENT_3D ( 'NONE', #67485, #186162, #143160 ) ;
#91814 = CARTESIAN_POINT ( 'NONE',  ( -20.85000000000000142, 78.48087866980282001, -232.8271061603568910 ) ) ;
#91815 = ORIENTED_EDGE ( 'NONE', *, *, #41500, .T. ) ;
#91817 = ORIENTED_EDGE ( 'NONE', *, *, #209568, .T. ) ;
#91816 = ORIENTED_EDGE ( 'NONE', *, *, #35266, .T. ) ;
#91818 = LINE ( 'NONE', #12306, #132042 ) ;
#91820 = ORIENTED_EDGE ( 'NONE', *, *, #155403, .F. ) ;
#91819 = DIRECTION ( 'NONE',  ( 0.000000000000000000, 0.000000000000000000, -1.000000000000000000 ) ) ;
#91821 = ADVANCED_FACE ( 'NONE', ( #126091 ), #107828, .F. ) ;
#91822 = CARTESIAN_POINT ( 'NONE',  ( 20.94999999999999574, 1.736257131597397585, -11.56865232901749962 ) ) ;
#91823 = VECTOR ( 'NONE', #93859, 1000.000000000000000 ) ;
#91824 = ORIENTED_EDGE ( 'NONE', *, *, #49874, .F. ) ;
#91825 = AXIS2_PLACEMENT_3D ( 'NONE', #101399, #141853, #179722 ) ;
#91826 = CIRCLE ( 'NONE', #237581, 11.90000000000000746 ) ;
#91827 = EDGE_CURVE ( 'NONE', #159137, #197206, #18209, .T. ) ;
#91828 = ORIENTED_EDGE ( 'NONE', *, *, #173945, .T. ) ;
#91830 = EDGE_CURVE ( 'NONE', #148964, #8048, #246067, .T. ) ;
#91829 = DIRECTION ( 'NONE',  ( 0.000000000000000000, 0.9126074666063769270, 0.4088369013363280513 ) ) ;
#91831 = EDGE_LOOP ( 'NONE', ( #96308, #124167, #3959, #69893, #40642 ) ) ;
#91832 = DIRECTION ( 'NONE',  ( -1.000000000000000000, 0.000000000000000000, 0.000000000000000000 ) ) ;
#91833 = CARTESIAN_POINT ( 'NONE',  ( 21.13461538461538680, 65.38541703798603066, -57.17310748452440095 ) ) ;
#91834 = EDGE_CURVE ( 'NONE', #195967, #19319, #27303, .T. ) ;
#91835 = DIRECTION ( 'NONE',  ( -1.000000000000000000, 1.772924042024179943E-16, -4.808324575169860901E-17 ) ) ;
#91836 = ORIENTED_EDGE ( 'NONE', *, *, #25759, .F. ) ;
#91837 = CYLINDRICAL_SURFACE ( 'NONE', #183572, 0.1000000000000002554 ) ;
#91838 = FACE_OUTER_BOUND ( 'NONE', #53189, .T. ) ;
#91839 = AXIS2_PLACEMENT_3D ( 'NONE', #59458, #101139, #22972 ) ;
#91840 = DIRECTION ( 'NONE',  ( 0.000000000000000000, -0.07847809223012357227, -0.9969158384938622275 ) ) ;
#91841 = CIRCLE ( 'NONE', #237597, 0.09999999999999939493 ) ;
#91842 = ORIENTED_EDGE ( 'NONE', *, *, #30635, .T. ) ;
#91843 = CARTESIAN_POINT ( 'NONE',  ( 18.56579813702275317, 10.33025634372637924, -106.0870929282639281 ) ) ;
#91844 = ORIENTED_EDGE ( 'NONE', *, *, #206678, .T. ) ;
#91845 = CARTESIAN_POINT ( 'NONE',  ( -18.59999996769639097, -7.620584189787890317, -210.0095198070081324 ) ) ;
#91846 = ORIENTED_EDGE ( 'NONE', *, *, #39743, .T. ) ;
#91847 = CARTESIAN_POINT ( 'NONE',  ( -23.25000000000000000, 87.75000000001216449, -139.6231074845242688 ) ) ;
#91848 = DIRECTION ( 'NONE',  ( 0.000000000000000000, 0.6728971962616792091, -0.7397360091702790408 ) ) ;
#91849 = ORIENTED_EDGE ( 'NONE', *, *, #149888, .F. ) ;
#91850 = ORIENTED_EDGE ( 'NONE', *, *, #109079, .T. ) ;
#91851 = DIRECTION ( 'NONE',  ( 2.694716079187273439E-16, 1.000000000000000000, 6.467318590049456648E-15 ) ) ;
#91852 = ADVANCED_FACE ( 'NONE', ( #230333 ), #51675, .F. ) ;
#91853 = DIRECTION ( 'NONE',  ( 1.000000000000000000, 0.000000000000000000, 0.000000000000000000 ) ) ;
#91854 = EDGE_LOOP ( 'NONE', ( #23297, #242582, #184399, #33558 ) ) ;
#91855 = CARTESIAN_POINT ( 'NONE',  ( -21.04999999999994387, 85.92654454508293327, -48.30233646433089234 ) ) ;
#91856 = ORIENTED_EDGE ( 'NONE', *, *, #235456, .T. ) ;
#91857 = TOROIDAL_SURFACE ( 'NONE', #50149, 12.97499999999999609, 0.1000000000000000056 ) ;
#91858 = AXIS2_PLACEMENT_3D ( 'NONE', #57603, #194594, #216691 ) ;
#91859 = TOROIDAL_SURFACE ( 'NONE', #245991, 0.2000000000000000111, 0.1000000000000000056 ) ;
#91860 = VERTEX_POINT ( 'NONE', #131239 ) ;
#91861 = AXIS2_PLACEMENT_3D ( 'NONE', #130814, #112552, #9577 ) ;
#91862 = CARTESIAN_POINT ( 'NONE',  ( -23.15000000000000213, 3.558777552609279304, -231.8203201594644725 ) ) ;
#91863 = EDGE_CURVE ( 'NONE', #13761, #185096, #44008, .T. ) ;
#91864 = CARTESIAN_POINT ( 'NONE',  ( 18.59999999999999076, 1.835341550235567887, -145.5551512925629822 ) ) ;
#91865 = CARTESIAN_POINT ( 'NONE',  ( -16.88219499860498019, 9.950206425438743452, -46.14930969010730166 ) ) ;
#91867 = ORIENTED_EDGE ( 'NONE', *, *, #121153, .T. ) ;
#91866 = FACE_OUTER_BOUND ( 'NONE', #200327, .T. ) ;
#91868 = CYLINDRICAL_SURFACE ( 'NONE', #216007, 0.09999999999999939493 ) ;
#91869 = VECTOR ( 'NONE', #122799, 1000.000000000000000 ) ;
#91870 = DIRECTION ( 'NONE',  ( 2.952720810173289112E-16, 0.4088369013363282733, -0.9126074666063769270 ) ) ;
#91871 = DIRECTION ( 'NONE',  ( 0.000000000000000000, -0.2044060691543873876, 0.9788861828082220384 ) ) ;
#91873 = CARTESIAN_POINT ( 'NONE',  ( -12.25000000000000178, 9.850000000011133849, -184.2499999999999716 ) ) ;
#91872 = DIRECTION ( 'NONE',  ( 0.000000000000000000, -0.2128009952263603677, 0.9770955615653313941 ) ) ;
#91874 = DIRECTION ( 'NONE',  ( -0.000000000000000000, 1.000000000000000000, 6.352154140967427193E-15 ) ) ;
#91875 = CARTESIAN_POINT ( 'NONE',  ( 18.44364597020195262, -9.490487317151105273, -107.5579778896838974 ) ) ;
#91876 = DIRECTION ( 'NONE',  ( 1.000000000000000000, 0.000000000000000000, 0.000000000000000000 ) ) ;
#91877 = EDGE_CURVE ( 'NONE', #238989, #160578, #248015, .T. ) ;
#91878 = LINE ( 'NONE', #74917, #163493 ) ;
#91879 = EDGE_LOOP ( 'NONE', ( #90916, #124282, #51962, #52076 ) ) ;
#91880 = EDGE_LOOP ( 'NONE', ( #111379, #143650, #65885, #24496 ) ) ;
#91881 = VECTOR ( 'NONE', #94559, 1000.000000000000000 ) ;
#91882 = DIRECTION ( 'NONE',  ( 0.000000000000000000, 0.9915357197604972583, -0.1298341882519109536 ) ) ;
#91883 = FACE_OUTER_BOUND ( 'NONE', #121413, .T. ) ;
#91884 = ORIENTED_EDGE ( 'NONE', *, *, #228711, .F. ) ;
#91885 = AXIS2_PLACEMENT_3D ( 'NONE', #56671, #32044, #214490 ) ;
#91886 = FILL_AREA_STYLE_COLOUR ( '', #189328 ) ;
#91887 = CARTESIAN_POINT ( 'NONE',  ( -20.54999999999999716, 1.115600667400684642E-11, -167.4999999999999716 ) ) ;
#91888 = CARTESIAN_POINT ( 'NONE',  ( -16.87331047859651179, 22.97806745954242302, -230.9350634111226270 ) ) ;
#91889 = VECTOR ( 'NONE', #224847, 1000.000000000000000 ) ;
#91890 = CARTESIAN_POINT ( 'NONE',  ( 21.14999999999999503, -0.09999999998884338825, -21.85042919245520210 ) ) ;
#91891 = EDGE_LOOP ( 'NONE', ( #123116, #110558, #1377, #54231 ) ) ;
#91892 = EDGE_LOOP ( 'NONE', ( #188164, #53210, #198344, #58415 ) ) ;
#91893 = CARTESIAN_POINT ( 'NONE',  ( 21.13507111622890022, 60.09352091567126308, -221.2276406919921214 ) ) ;
#91894 = CARTESIAN_POINT ( 'NONE',  ( 21.05000000000000071, -7.079251802663310222, -212.6676826711374417 ) ) ;
#91895 = ORIENTED_EDGE ( 'NONE', *, *, #115109, .T. ) ;
#91896 = CIRCLE ( 'NONE', #212555, 0.1000000000000028644 ) ;
#91897 = CARTESIAN_POINT ( 'NONE',  ( -20.94999999999999929, -1.360870587180885716, -142.0729979270909951 ) ) ;
#91899 = ORIENTED_EDGE ( 'NONE', *, *, #249628, .F. ) ;
#91898 = DIRECTION ( 'NONE',  ( 0.000000000000000000, 0.000000000000000000, 1.000000000000000000 ) ) ;
#91900 = CARTESIAN_POINT ( 'NONE',  ( 18.52928932188133615, 33.76313540251413770, -236.3387713816553060 ) ) ;
#91902 = ORIENTED_EDGE ( 'NONE', *, *, #209470, .T. ) ;
#91901 = CARTESIAN_POINT ( 'NONE',  ( 18.49999999999999645, 76.00000000001142553, -36.02310748452432421 ) ) ;
#91903 = CARTESIAN_POINT ( 'NONE',  ( -18.50000972452446035, 10.29326151435326508, -72.45928225104148623 ) ) ;
#91904 = LINE ( 'NONE', #90611, #66563 ) ;
#91905 = EDGE_CURVE ( 'NONE', #193140, #22968, #7436, .T. ) ;
#91906 = DIRECTION ( 'NONE',  ( -1.000000000000000000, -0.000000000000000000, -0.000000000000000000 ) ) ;
#91908 = CARTESIAN_POINT ( 'NONE',  ( 21.04105312098506531, 8.875332623054768888, -179.8285067472120033 ) ) ;
#91907 = CARTESIAN_POINT ( 'NONE',  ( -21.55000000000000071, 7.350000000011155166, -45.75000000000000000 ) ) ;
#91909 = CARTESIAN_POINT ( 'NONE',  ( -18.69999999999999929, 10.31653824539118069, -11.82383137372478110 ) ) ;
#91910 = CIRCLE ( 'NONE', #4423, 11.80000000000000426 ) ;
#91911 = DIRECTION ( 'NONE',  ( -1.000000000000000000, -0.000000000000000000, -0.000000000000000000 ) ) ;
#91912 = CYLINDRICAL_SURFACE ( 'NONE', #159972, 0.1000000000000002554 ) ;
#91913 = CYLINDRICAL_SURFACE ( 'NONE', #76124, 0.5000000000000014433 ) ;
#91914 = CIRCLE ( 'NONE', #179425, 11.79999999999999716 ) ;
#91915 = ORIENTED_EDGE ( 'NONE', *, *, #126993, .F. ) ;
#91917 = CARTESIAN_POINT ( 'NONE',  ( -20.00857864376270001, 66.75000000001253397, -182.2731074845244166 ) ) ;
#91916 = AXIS2_PLACEMENT_3D ( 'NONE', #197271, #346, #142427 ) ;
#91918 = VERTEX_POINT ( 'NONE', #67416 ) ;
#91920 = DIRECTION ( 'NONE',  ( 0.000000000000000000, -1.000000000000000000, -0.000000000000000000 ) ) ;
#91919 = AXIS2_PLACEMENT_3D ( 'NONE', #100599, #58912, #181480 ) ;
#91921 = ORIENTED_EDGE ( 'NONE', *, *, #57895, .T. ) ;
#91922 = ADVANCED_FACE ( 'NONE', ( #92112 ), #189755, .F. ) ;
#91923 = LINE ( 'NONE', #68527, #198357 ) ;
#91924 = CARTESIAN_POINT ( 'NONE',  ( -20.05000000000000426, 66.75000000001179501, -81.87310748452438247 ) ) ;
#91925 = VECTOR ( 'NONE', #184854, 1000.000000000000000 ) ;
#91926 = AXIS2_PLACEMENT_3D ( 'NONE', #223861, #50351, #148193 ) ;
#91927 = ADVANCED_FACE ( 'NONE', ( #166551 ), #8734, .F. ) ;
#91928 = B_SPLINE_CURVE_WITH_KNOTS ( 'NONE', 3,
 ( #183442, #106432, #85570, #244674 ),
 .UNSPECIFIED., .F., .F.,
 ( 4, 4 ),
 ( 0.000000000000000000, 7.713889350927385870E-05 ),
 .UNSPECIFIED. ) ;
#91929 = EDGE_LOOP ( 'NONE', ( #3636, #68394, #189510, #82215, #131640, #38693, #121905, #98479, #8181, #242012, #183395 ) ) ;
#91930 = LINE ( 'NONE', #30711, #7001 ) ;
#91931 = EDGE_CURVE ( 'NONE', #143848, #17316, #152854, .T. ) ;
#91933 = EDGE_LOOP ( 'NONE', ( #74466, #34348, #25252, #137761 ) ) ;
#91932 = VECTOR ( 'NONE', #174462, 1000.000000000000000 ) ;
#91934 = CIRCLE ( 'NONE', #216832, 0.09999999999999950595 ) ;
#91935 = AXIS2_PLACEMENT_3D ( 'NONE', #109272, #31076, #207118 ) ;
#91936 = EDGE_LOOP ( 'NONE', ( #173928, #84402, #159061, #146205, #61895, #194784, #140335, #202772, #13483, #256124 ) ) ;
#91937 = AXIS2_PLACEMENT_3D ( 'NONE', #41620, #199407, #97685 ) ;
#91938 = AXIS2_PLACEMENT_3D ( 'NONE', #195570, #235946, #157759 ) ;
#91939 = EDGE_CURVE ( 'NONE', #59375, #215604, #135577, .T. ) ;
#91940 = CARTESIAN_POINT ( 'NONE',  ( -23.15000000000000213, 64.35000000001156195, -57.37310748452440379 ) ) ;
#91941 = CARTESIAN_POINT ( 'NONE',  ( -16.77977881697927032, 66.05339806647866396, -56.86172891140933672 ) ) ;
#91942 = CARTESIAN_POINT ( 'NONE',  ( -21.64999999999999858, 9.349999999999978328, -9.250000000000001776 ) ) ;
#91943 = CARTESIAN_POINT ( 'NONE',  ( 12.25000000000000000, 26.30888228346803004, -233.3999513616626587 ) ) ;
#91944 = CARTESIAN_POINT ( 'NONE',  ( 18.49999999999999289, 23.29878867550048938, -248.4686781323362084 ) ) ;
#91946 = CARTESIAN_POINT ( 'NONE',  ( -18.36973785203556275, 11.47550320049537476, -57.75000000000000000 ) ) ;
#91945 = DIRECTION ( 'NONE',  ( 0.000000000000000000, 0.2128009952263568427, -0.9770955615653322823 ) ) ;
#91947 = CARTESIAN_POINT ( 'NONE',  ( -15.75000000000000711, 9.350000000011140955, -83.52151937182513564 ) ) ;
#91949 = VERTEX_POINT ( 'NONE', #36011 ) ;
#91948 = LINE ( 'NONE', #134898, #13372 ) ;
#91951 = LINE ( 'NONE', #129793, #4362 ) ;
#91950 = CARTESIAN_POINT ( 'NONE',  ( 20.54374330479337374, 10.50501031423420351, -74.72568363488957743 ) ) ;
#91952 = ADVANCED_FACE ( 'NONE', ( #33471 ), #192504, .T. ) ;
#91953 = CYLINDRICAL_SURFACE ( 'NONE', #185944, 0.09999999999999939493 ) ;
#91954 = ORIENTED_EDGE ( 'NONE', *, *, #234133, .T. ) ;
#91955 = DIRECTION ( 'NONE',  ( 0.000000000000000000, 0.000000000000000000, 1.000000000000000000 ) ) ;
#91956 = DIRECTION ( 'NONE',  ( 0.000000000000000000, 0.000000000000000000, -1.000000000000000000 ) ) ;
#91957 = DIRECTION ( 'NONE',  ( -1.000000000000000000, 0.000000000000000000, -0.000000000000000000 ) ) ;
#91958 = ORIENTED_EDGE ( 'NONE', *, *, #66943, .T. ) ;
#91959 = ADVANCED_FACE ( 'NONE', ( #73874 ), #23189, .T. ) ;
#91960 = DIRECTION ( 'NONE',  ( 0.000000000000000000, -1.000000000000000000, -6.982962677686266711E-15 ) ) ;
#91961 = DIRECTION ( 'NONE',  ( 0.000000000000000000, 0.008583690987124100932, -0.9999631594459055250 ) ) ;
#91962 = FACE_OUTER_BOUND ( 'NONE', #239763, .T. ) ;
#91963 = VERTEX_POINT ( 'NONE', #72573 ) ;
#91964 = ORIENTED_EDGE ( 'NONE', *, *, #142693, .F. ) ;
#91965 = SPHERICAL_SURFACE ( 'NONE', #57566, 0.1000000000000000056 ) ;
#91966 = FACE_OUTER_BOUND ( 'NONE', #190821, .T. ) ;
#91967 = CYLINDRICAL_SURFACE ( 'NONE', #111533, 0.5000000000000004441 ) ;
#91968 = CARTESIAN_POINT ( 'NONE',  ( -20.88420186297724612, 10.33025634372637391, -206.5870929282638429 ) ) ;
#91969 = EDGE_LOOP ( 'NONE', ( #139632, #146054, #119094, #69744 ) ) ;
#91970 = CIRCLE ( 'NONE', #129395, 11.65000000000000746 ) ;
#91971 = ADVANCED_FACE ( 'NONE', ( #231643 ), #193861, .F. ) ;
#91972 = DIRECTION ( 'NONE',  ( 0.000000000000000000, -0.9165223833629894123, 0.3999834006488590110 ) ) ;
#91973 = CARTESIAN_POINT ( 'NONE',  ( 20.94999999999999929, 5.000000000011153745, -155.0947339810869323 ) ) ;
#91974 = CARTESIAN_POINT ( 'NONE',  ( 21.59780538579342490, 0.09897866960914131207, -127.1529094700567839 ) ) ;
#91975 = CARTESIAN_POINT ( 'NONE',  ( 18.49999999999999645, 1.866714910068465239, -179.2526752462819672 ) ) ;
#91976 = CIRCLE ( 'NONE', #16995, 0.1000000000000010186 ) ;
#91977 = ORIENTED_EDGE ( 'NONE', *, *, #194600, .T. ) ;
#91978 = CARTESIAN_POINT ( 'NONE',  ( 20.94999999999999929, 67.23127455305835554, -235.8551265064784559 ) ) ;
#91979 = ADVANCED_FACE ( 'NONE', ( #155970 ), #52979, .F. ) ;
#91981 = ORIENTED_EDGE ( 'NONE', *, *, #116819, .T. ) ;
#91980 = CARTESIAN_POINT ( 'NONE',  ( -1.820710678118657944, 85.92928932189354896, -145.2731074845243029 ) ) ;
#91982 = CARTESIAN_POINT ( 'NONE',  ( -20.85000000000000142, -1.263275465206102233, -108.4018646667464481 ) ) ;
#91983 = CARTESIAN_POINT ( 'NONE',  ( 22.49806830649814060, 31.82532512087596288, -238.9510566881495777 ) ) ;
#91984 = DIRECTION ( 'NONE',  ( 1.000000000000000000, 3.265361837132813093E-16, -0.000000000000000000 ) ) ;
#91985 = DIRECTION ( 'NONE',  ( 1.000000000000000000, 0.000000000000000000, 0.000000000000000000 ) ) ;
#91986 = DIRECTION ( 'NONE',  ( 0.000000000000000000, -0.8814952561688430555, 0.4721928772777346239 ) ) ;
#91987 = ORIENTED_EDGE ( 'NONE', *, *, #236392, .T. ) ;
#91988 = CARTESIAN_POINT ( 'NONE',  ( 21.13461538461538325, 8.885417037974457699, -12.25000000000000178 ) ) ;
#91989 = DIRECTION ( 'NONE',  ( -1.000000000000000000, 0.000000000000000000, 0.000000000000000000 ) ) ;
#91990 = DIRECTION ( 'NONE',  ( 0.000000000000000000, 0.1350103645451807832, 0.9908441862701610203 ) ) ;
#91991 = EDGE_CURVE ( 'NONE', #132612, #206343, #6598, .T. ) ;
#91992 = EDGE_LOOP ( 'NONE', ( #6599, #138042, #174573, #135172, #171979, #98972, #234221, #190244, #114367 ) ) ;
#91993 = DIRECTION ( 'NONE',  ( 0.000000000000000000, 0.9651348961777157509, -0.2617529984165031243 ) ) ;
#91994 = CIRCLE ( 'NONE', #71175, 0.09999999999999939493 ) ;
#91995 = DIRECTION ( 'NONE',  ( 1.000000000000000000, 0.000000000000000000, 0.000000000000000000 ) ) ;
#91996 = CARTESIAN_POINT ( 'NONE',  ( -18.50000000000000000, 71.84303044094815505, -225.1053209871248271 ) ) ;
#91997 = EDGE_CURVE ( 'NONE', #248551, #145935, #148068, .T. ) ;
#91999 = AXIS2_PLACEMENT_3D ( 'NONE', #59525, #236909, #139057 ) ;
#91998 = CARTESIAN_POINT ( 'NONE',  ( 21.05000000000034177, 6.300183336278641022, -167.4486725676592869 ) ) ;
#92000 = ADVANCED_FACE ( 'NONE', ( #95953 ), #93894, .T. ) ;
#92002 = CARTESIAN_POINT ( 'NONE',  ( 12.30626653967340900, 9.356790025057033944, -184.7048265086138201 ) ) ;
#92001 = CIRCLE ( 'NONE', #150287, 0.09999999999999609201 ) ;
#92003 = ORIENTED_EDGE ( 'NONE', *, *, #151325, .T. ) ;
#92004 = ORIENTED_EDGE ( 'NONE', *, *, #72104, .F. ) ;
#92005 = AXIS2_PLACEMENT_3D ( 'NONE', #115877, #197964, #195433 ) ;
#92006 = CARTESIAN_POINT ( 'NONE',  ( -18.42554971533678199, -9.497159669426588735, -141.0398269135486942 ) ) ;
#92007 = CARTESIAN_POINT ( 'NONE',  ( -18.50000000000000000, 11.65000000001115232, -179.6499999999999773 ) ) ;
#92009 = ADVANCED_FACE ( 'NONE', ( #153422, #235464 ), #256249, .T. ) ;
#92008 =( BOUNDED_CURVE ( )  B_SPLINE_CURVE ( 3, ( #86568, #166174, #67040, #141430 ),
 .UNSPECIFIED., .F., .F. ) 
 B_SPLINE_CURVE_WITH_KNOTS ( ( 4, 4 ),
 ( 0.000000000000000000, 1.570796326794916320 ),
 .UNSPECIFIED. ) 
 CURVE ( )  GEOMETRIC_REPRESENTATION_ITEM ( )  RATIONAL_B_SPLINE_CURVE ( ( 1.000000000000000000, 0.8047378541243603856, 0.8047378541243603856, 1.000000000000000000 ) ) 
 REPRESENTATION_ITEM ( '' )  );
#92010 = CARTESIAN_POINT ( 'NONE',  ( -21.03922262424680056, 38.16640938004818651, -236.1388068296846541 ) ) ;
#92011 = DIRECTION ( 'NONE',  ( -0.000000000000000000, -0.8660254037844468122, -0.4999999999999860112 ) ) ;
#92012 = DIRECTION ( 'NONE',  ( 1.836970198721029934E-16, 1.000000000000000000, 6.982962677686266711E-15 ) ) ;
#92013 = ADVANCED_FACE ( 'NONE', ( #175531 ), #106339, .T. ) ;
#92015 = EDGE_CURVE ( 'NONE', #198523, #18345, #217177, .T. ) ;
#92014 = CARTESIAN_POINT ( 'NONE',  ( 21.14999999999999503, 1.115600667400684642E-11, -100.5000000000000284 ) ) ;
#92016 = CIRCLE ( 'NONE', #237771, 0.1000000000000028644 ) ;
#92017 = CARTESIAN_POINT ( 'NONE',  ( -21.05000000000000071, 70.10000000001197407, -113.2422072491807086 ) ) ;
#92018 = DIRECTION ( 'NONE',  ( -1.000000000000000000, 0.000000000000000000, 0.000000000000000000 ) ) ;
#92019 = ORIENTED_EDGE ( 'NONE', *, *, #33803, .F. ) ;
#92020 = CYLINDRICAL_SURFACE ( 'NONE', #239996, 0.1000000000000024342 ) ;
#92021 = EDGE_CURVE ( 'NONE', #176927, #163980, #202241, .T. ) ;
#92022 = ORIENTED_EDGE ( 'NONE', *, *, #35358, .F. ) ;
#92023 = DIRECTION ( 'NONE',  ( -1.000000000000000000, -0.000000000000000000, -0.000000000000000000 ) ) ;
#92024 = DIRECTION ( 'NONE',  ( 0.000000000000000000, -0.4721928772777346794, -0.8814952561688431665 ) ) ;
#92025 = CYLINDRICAL_SURFACE ( 'NONE', #116135, 0.1000000000000028644 ) ;
#92026 = EDGE_CURVE ( 'NONE', #47890, #226308, #174272, .T. ) ;
#92027 = CARTESIAN_POINT ( 'NONE',  ( -22.39999999999999858, 11.65000000001115588, -66.90000000000004832 ) ) ;
#92028 = FACE_OUTER_BOUND ( 'NONE', #16994, .T. ) ;
#92029 = CYLINDRICAL_SURFACE ( 'NONE', #218420, 0.09999999999999108213 ) ;
#92030 = VERTEX_POINT ( 'NONE', #75152 ) ;
#92031 = DIRECTION ( 'NONE',  ( -0.000000000000000000, 0.4088369013363283844, -0.9126074666063769270 ) ) ;
#92032 = AXIS2_PLACEMENT_3D ( 'NONE', #230285, #193740, #131184 ) ;
#92033 = DIRECTION ( 'NONE',  ( 1.000000000000000000, -0.000000000000000000, 0.000000000000000000 ) ) ;
#92034 = AXIS2_PLACEMENT_3D ( 'NONE', #76007, #180250, #175156 ) ;
#92035 = DIRECTION ( 'NONE',  ( 1.000000000000000000, 1.476360405086644309E-16, -0.000000000000000000 ) ) ;
#92036 = CARTESIAN_POINT ( 'NONE',  ( -20.64999999999999858, 71.65000000001207070, -124.2731074845243313 ) ) ;
#92037 = AXIS2_PLACEMENT_3D ( 'NONE', #224427, #233128, #65357 ) ;
#92038 = CARTESIAN_POINT ( 'NONE',  ( -17.29158576265543346, 10.36474766602906961, -156.0827582447921884 ) ) ;
#92039 = CIRCLE ( 'NONE', #125380, 0.1000000000000028644 ) ;
#92040 = VERTEX_POINT ( 'NONE', #154689 ) ;
#92041 = LINE ( 'NONE', #13797, #227109 ) ;
#92042 = CARTESIAN_POINT ( 'NONE',  ( -18.50000000000000000, -1.164121893230052995, -208.9148480855715775 ) ) ;
#92043 = ORIENTED_EDGE ( 'NONE', *, *, #92982, .F. ) ;
#92044 = ADVANCED_FACE ( 'NONE', ( #56804 ), #173052, .T. ) ;
#92045 = EDGE_CURVE ( 'NONE', #85754, #75088, #206337, .T. ) ;
#92046 = ORIENTED_EDGE ( 'NONE', *, *, #163245, .T. ) ;
#92047 = LINE ( 'NONE', #172923, #226405 ) ;
#92048 = CARTESIAN_POINT ( 'NONE',  ( 18.46905048506370406, -9.473744257371240707, -174.1759862922554873 ) ) ;
#92049 = CIRCLE ( 'NONE', #167115, 0.2000000000000048683 ) ;
#92050 = ORIENTED_EDGE ( 'NONE', *, *, #162197, .T. ) ;
#92051 = CARTESIAN_POINT ( 'NONE',  ( -22.50000000000000000, 1.115600667400684642E-11, -88.85042919245522341 ) ) ;
#92052 = CARTESIAN_POINT ( 'NONE',  ( 21.04999999999999716, 8.871279686006802834, -42.05862899514095687 ) ) ;
#92053 = ADVANCED_FACE ( 'NONE', ( #223592 ), #162378, .F. ) ;
#92054 = ORIENTED_EDGE ( 'NONE', *, *, #209295, .F. ) ;
#92055 = CARTESIAN_POINT ( 'NONE',  ( 23.04999999999999716, 8.822561741677553471, -158.2500000000000284 ) ) ;
#92056 = ORIENTED_EDGE ( 'NONE', *, *, #135755, .F. ) ;
#92057 = CARTESIAN_POINT ( 'NONE',  ( -23.15000000000000213, 1.115600667400684642E-11, -104.4000000000000483 ) ) ;
#92058 = LINE ( 'NONE', #54213, #46237 ) ;
#92059 = VECTOR ( 'NONE', #207180, 1000.000000000000000 ) ;
#92061 = ORIENTED_EDGE ( 'NONE', *, *, #180184, .T. ) ;
#92060 = DIRECTION ( 'NONE',  ( -0.000000000000000000, 1.000000000000000000, -0.000000000000000000 ) ) ;
#92062 = DIRECTION ( 'NONE',  ( 0.000000000000000000, 0.9999631594459056361, -0.008583690987128059571 ) ) ;
#92064 = UNCERTAINTY_MEASURE_WITH_UNIT (LENGTH_MEASURE( 1.000000000000000082E-05 ), #241416, 'distance_accuracy_value', 'NONE');
#92063 = CARTESIAN_POINT ( 'NONE',  ( 21.05000000000000071, -4.871452838297987142, -233.3782557782877518 ) ) ;
#92065 = PLANE ( 'NONE',  #37799 ) ;
#92066 = CARTESIAN_POINT ( 'NONE',  ( -18.45140287520617761, 85.48607773954122990, -62.88258435783815514 ) ) ;
#92067 = CARTESIAN_POINT ( 'NONE',  ( -11.59999999999994458, 64.25000000001119815, -21.02310748452479316 ) ) ;
#92068 = CIRCLE ( 'NONE', #163028, 0.09999999999999939493 ) ;
#92069 = EDGE_CURVE ( 'NONE', #136504, #50994, #123235, .T. ) ;
#92070 = CARTESIAN_POINT ( 'NONE',  ( 18.59999999999996945, 67.85909929089923764, -227.8797997985275856 ) ) ;
#92071 = DIRECTION ( 'NONE',  ( -1.073024830501117725E-15, 0.000000000000000000, 1.000000000000000000 ) ) ;
#92073 = ORIENTED_EDGE ( 'NONE', *, *, #73375, .F. ) ;
#92072 = CYLINDRICAL_SURFACE ( 'NONE', #111281, 0.09999999999998898659 ) ;
#92074 = ORIENTED_EDGE ( 'NONE', *, *, #177987, .F. ) ;
#92076 = DIRECTION ( 'NONE',  ( 1.000000000000000000, -0.000000000000000000, -0.000000000000000000 ) ) ;
#92075 = CARTESIAN_POINT ( 'NONE',  ( -18.59999999999999787, 11.60000000001115872, -40.42820323027555673 ) ) ;
#92078 = EDGE_LOOP ( 'NONE', ( #195817, #151855, #154691, #167944 ) ) ;
#92077 = DIRECTION ( 'NONE',  ( 0.000000000000000000, 0.000000000000000000, -1.000000000000000000 ) ) ;
#92079 = CIRCLE ( 'NONE', #171250, 4.099999999999992539 ) ;
#92080 = ADVANCED_FACE ( 'NONE', ( #243171 ), #114753, .T. ) ;
#92081 = ORIENTED_EDGE ( 'NONE', *, *, #181465, .F. ) ;
#92082 = B_SPLINE_CURVE_WITH_KNOTS ( 'NONE', 3,
 ( #234279, #175619, #235562, #136447, #176913, #215993, #38662, #195196, #178196, #219853, #36108, #16545, #37395, #55616, #58198, #41257, #256354, #56900, #97309, #193897, #214722, #196438, #17794, #137737, #77762, #118197 ),
 .UNSPECIFIED., .F., .F.,
 ( 4, 2, 2, 2, 2, 2, 2, 2, 2, 2, 2, 2, 4 ),
 ( 0.005476422646581346511, 0.006160811967703526230, 0.006845201288825705950, 0.007187395949386825300, 0.007529590609947943783, 0.007871785270509062266, 0.008213979931070182483, 0.008556174591631300966, 0.008898369252192419449, 0.009240563912753537931, 0.009582758573314656414, 0.01026714789443684134, 0.01095153721555902279 ),
 .UNSPECIFIED. ) ;
#92083 = DIRECTION ( 'NONE',  ( 0.000000000000000000, -0.9770955615653313941, -0.2128009952263606730 ) ) ;
#92084 = CARTESIAN_POINT ( 'NONE',  ( 5.900000000000059863, 64.75000000001119815, -25.92310748452479174 ) ) ;
#92085 = VECTOR ( 'NONE', #31710, 1000.000000000000000 ) ;
#92086 = DIRECTION ( 'NONE',  ( 0.000000000000000000, -6.938893903907234689E-15, 1.000000000000000000 ) ) ;
#92087 = CIRCLE ( 'NONE', #29585, 2.599999999999998312 ) ;
#92088 = CARTESIAN_POINT ( 'NONE',  ( -18.59999999999999787, 64.35000000001157616, -57.27310748452440237 ) ) ;
#92089 = EDGE_CURVE ( 'NONE', #208732, #143962, #35674, .T. ) ;
#92090 = LINE ( 'NONE', #155949, #172186 ) ;
#92091 = CARTESIAN_POINT ( 'NONE',  ( -21.05000000000000071, -1.835341550224411922, -11.55515129256297868 ) ) ;
#92092 = EDGE_CURVE ( 'NONE', #136044, #22095, #152570, .T. ) ;
#92093 = CARTESIAN_POINT ( 'NONE',  ( -18.59999999999999787, 70.29876110920605470, -198.0544810472949564 ) ) ;
#92094 = VERTEX_POINT ( 'NONE', #99787 ) ;
#92095 = ORIENTED_EDGE ( 'NONE', *, *, #93268, .F. ) ;
#92096 = EDGE_CURVE ( 'NONE', #53042, #109261, #202767, .T. ) ;
#92097 = AXIS2_PLACEMENT_3D ( 'NONE', #174201, #197560, #97138 ) ;
#92098 = ORIENTED_EDGE ( 'NONE', *, *, #204543, .T. ) ;
#92099 = DIRECTION ( 'NONE',  ( 1.000000000000000000, 0.000000000000000000, 0.000000000000000000 ) ) ;
#92100 = ORIENTED_EDGE ( 'NONE', *, *, #191424, .F. ) ;
#92101 = CYLINDRICAL_SURFACE ( 'NONE', #214100, 0.1000000000000000472 ) ;
#92102 = EDGE_CURVE ( 'NONE', #144164, #39469, #201473, .T. ) ;
#92104 = EDGE_CURVE ( 'NONE', #50994, #249547, #89980, .T. ) ;
#92103 = EDGE_CURVE ( 'NONE', #76616, #8107, #156662, .T. ) ;
#92106 =( BOUNDED_SURFACE ( )  B_SPLINE_SURFACE ( 3, 2, ( 
 ( #219379, #43333, #39511 ),
 ( #40789, #142417, #21224 ),
 ( #100691, #180275, #221930 ),
 ( #45887, #50991, #6761 ),
 ( #208819, #187978, #30198 ),
 ( #189262, #150145, #227081 ),
 ( #107137, #186701, #128002 ),
 ( #9326, #86272, #10622 ) ),
 .UNSPECIFIED., .F., .F., .T. ) 
 B_SPLINE_SURFACE_WITH_KNOTS ( ( 4, 2, 2, 4 ),
 ( 3, 3 ),
 ( 0.0001704874539069911317, 0.0003809798300636659538, 0.0004862260181420033920, 0.0005914722062203408301 ),
 ( 0.000000000000000000, 1.000000000000000000 ),
 .UNSPECIFIED. ) 
 GEOMETRIC_REPRESENTATION_ITEM ( )  RATIONAL_B_SPLINE_SURFACE ( (
 ( 1.000000000000000000, 0.7071067811864942820, 1.000000000000000000),
 ( 1.000000000000000000, 0.7670648383579508067, 1.000000000000000000),
 ( 1.000000000000000000, 0.8204820770248304473, 1.000000000000000000),
 ( 1.000000000000000000, 0.8877218296116144991, 1.000000000000000000),
 ( 1.000000000000000000, 0.9080815932663784951, 1.000000000000000000),
 ( 1.000000000000000000, 0.9395541505863417298, 1.000000000000000000),
 ( 1.000000000000000000, 0.9506520335377867115, 1.000000000000000000),
 ( 1.000000000000000000, 0.9504532311154454405, 1.000000000000000000) ) ) 
 REPRESENTATION_ITEM ( '' )  SURFACE ( )  );
#92105 = PRESENTATION_LAYER_ASSIGNMENT (  '', '', ( #62894 ) ) ;
#92107 = CARTESIAN_POINT ( 'NONE',  ( -23.25000000000000000, 1.115600667400684642E-11, -167.5000000000000284 ) ) ;
#92108 = FACE_OUTER_BOUND ( 'NONE', #222910, .T. ) ;
#92109 = VERTEX_POINT ( 'NONE', #84052 ) ;
#92110 = VECTOR ( 'NONE', #175217, 1000.000000000000000 ) ;
#92111 = ORIENTED_EDGE ( 'NONE', *, *, #231915, .F. ) ;
#92112 = FACE_OUTER_BOUND ( 'NONE', #134932, .T. ) ;
#92113 = ORIENTED_EDGE ( 'NONE', *, *, #29611, .T. ) ;
#92114 = DIRECTION ( 'NONE',  ( -1.000000000000000000, -0.000000000000000000, -0.000000000000000000 ) ) ;
#92115 = ORIENTED_EDGE ( 'NONE', *, *, #210037, .T. ) ;
#92118 = EDGE_LOOP ( 'NONE', ( #24073, #84343, #197844, #122600 ) ) ;
#92117 = CARTESIAN_POINT ( 'NONE',  ( -20.94999999999999929, -11.48912529306490349, -103.6000000000000369 ) ) ;
#92116 = CARTESIAN_POINT ( 'NONE',  ( 18.49999999999999645, 4.064367954407507533, -211.9684786640956418 ) ) ;
#92119 = CIRCLE ( 'NONE', #254414, 0.09999999999999939493 ) ;
#92120 = EDGE_CURVE ( 'NONE', #137421, #169584, #185839, .T. ) ;
#92121 = LINE ( 'NONE', #189950, #160567 ) ;
#92123 = EDGE_CURVE ( 'NONE', #185054, #34317, #240613, .T. ) ;
#92122 = AXIS2_PLACEMENT_3D ( 'NONE', #136684, #173315, #132866 ) ;
#92125 = ORIENTED_EDGE ( 'NONE', *, *, #8391, .T. ) ;
#92124 = AXIS2_PLACEMENT_3D ( 'NONE', #185946, #248487, #247189 ) ;
#92126 = VECTOR ( 'NONE', #82802, 1000.000000000000000 ) ;
#92127 = EDGE_LOOP ( 'NONE', ( #256093, #229934, #47993, #179668 ) ) ;
#92128 = EDGE_CURVE ( 'NONE', #53354, #212431, #120694, .T. ) ;
#92129 = CARTESIAN_POINT ( 'NONE',  ( 23.14999999999999503, 11.65000000001116298, -93.48519422934610645 ) ) ;
#92130 = ORIENTED_EDGE ( 'NONE', *, *, #195787, .F. ) ;
#92131 = FACE_OUTER_BOUND ( 'NONE', #58316, .T. ) ;
#92132 = PLANE ( 'NONE',  #22107 ) ;
#92133 = CYLINDRICAL_SURFACE ( 'NONE', #82591, 0.1000000000000028644 ) ;
#92134 = CARTESIAN_POINT ( 'NONE',  ( 18.50000324121758055, 67.49461024981972912, -195.5605382655040216 ) ) ;
#92135 = DIRECTION ( 'NONE',  ( -1.000000000000000000, -0.000000000000000000, -0.000000000000000000 ) ) ;
#92136 = ADVANCED_FACE ( 'NONE', ( #144058 ), #180644, .F. ) ;
#92137 = ORIENTED_EDGE ( 'NONE', *, *, #156087, .T. ) ;
#92139 = ADVANCED_FACE ( 'NONE', ( #178092 ), #25432, .F. ) ;
#92138 = CARTESIAN_POINT ( 'NONE',  ( -16.93772744219066340, 44.07028146185461281, -235.2804298480971568 ) ) ;
#92140 = CARTESIAN_POINT ( 'NONE',  ( -21.02374657821566828, 64.39999999919209017, -109.9513107143265387 ) ) ;
#92141 = CARTESIAN_POINT ( 'NONE',  ( 21.12757541349815682, 6.473380571262609351, -33.49483878419025018 ) ) ;
#92142 = VERTEX_POINT ( 'NONE', #140203 ) ;
#92143 = DIRECTION ( 'NONE',  ( 0.000000000000000000, 0.000000000000000000, 1.000000000000000000 ) ) ;
#92144 = ORIENTED_EDGE ( 'NONE', *, *, #169622, .T. ) ;
#92145 = CARTESIAN_POINT ( 'NONE',  ( 23.15000000000000213, 49.36776662947724503, -253.7196102226803021 ) ) ;
#92146 = ORIENTED_EDGE ( 'NONE', *, *, #102982, .T. ) ;
#92147 = CARTESIAN_POINT ( 'NONE',  ( -18.59999999999999787, 0.4810385098657082859, -209.0827657365571213 ) ) ;
#92148 = CARTESIAN_POINT ( 'NONE',  ( -22.50000000000094147, 75.90000000001255387, -181.6726782920691790 ) ) ;
#92150 = ORIENTED_EDGE ( 'NONE', *, *, #142003, .T. ) ;
#92149 = DIRECTION ( 'NONE',  ( -1.000000000000000000, -0.000000000000000000, -0.000000000000000000 ) ) ;
#92151 = EDGE_CURVE ( 'NONE', #221229, #256826, #20300, .T. ) ;
#92152 = DIRECTION ( 'NONE',  ( -3.265361837132813093E-16, 1.000000000000000000, 0.000000000000000000 ) ) ;
#92153 = VERTEX_POINT ( 'NONE', #81503 ) ;
#92154 = AXIS2_PLACEMENT_3D ( 'NONE', #106561, #7478, #86990 ) ;
#92155 = DIRECTION ( 'NONE',  ( -1.000000000000000000, 0.000000000000000000, 0.000000000000000000 ) ) ;
#92156 = DIRECTION ( 'NONE',  ( 1.000000000000000000, 0.000000000000000000, 0.000000000000000000 ) ) ;
#92157 = ORIENTED_EDGE ( 'NONE', *, *, #98698, .F. ) ;
#92158 = EDGE_CURVE ( 'NONE', #118767, #174500, #48826, .T. ) ;
#92159 = FACE_OUTER_BOUND ( 'NONE', #112362, .T. ) ;
#92160 = CARTESIAN_POINT ( 'NONE',  ( -23.15000000000000213, 1.115600667400684642E-11, -100.5000000000000426 ) ) ;
#92161 = ORIENTED_EDGE ( 'NONE', *, *, #107824, .T. ) ;
#92162 = DIRECTION ( 'NONE',  ( 0.000000000000000000, -0.9229812358756199764, 0.3848449534832346086 ) ) ;
#92163 = ORIENTED_EDGE ( 'NONE', *, *, #187841, .T. ) ;
#92165 = CARTESIAN_POINT ( 'NONE',  ( 19.99999999999998934, 64.35000000001180354, -81.77310748452438816 ) ) ;
#92164 = CIRCLE ( 'NONE', #246305, 0.09999999999999213685 ) ;
#92166 = CARTESIAN_POINT ( 'NONE',  ( -22.59080734064478335, 64.25000000001237765, -170.0538571926214786 ) ) ;
#92167 = ADVANCED_FACE ( 'NONE', ( #89231, #188344 ), #149240, .T. ) ;
#92170 = ORIENTED_EDGE ( 'NONE', *, *, #51095, .T. ) ;
#92169 = ORIENTED_EDGE ( 'NONE', *, *, #208165, .F. ) ;
#92168 = CARTESIAN_POINT ( 'NONE',  ( 20.73486653747088937, 7.750000000011182166, -188.3499999999999659 ) ) ;
#92171 = DIRECTION ( 'NONE',  ( 1.000000000000000000, -3.265361837132813093E-16, -2.280189983783949500E-30 ) ) ;
#92172 = CARTESIAN_POINT ( 'NONE',  ( -20.94999999999999929, -11.48912529306490349, -70.10000000000005116 ) ) ;
#92173 = DIRECTION ( 'NONE',  ( -7.304098846218134667E-16, -1.000000000000000000, 0.000000000000000000 ) ) ;
#92175 = CARTESIAN_POINT ( 'NONE',  ( -15.73854595235691889, 66.64858632091015522, -52.54276391697543147 ) ) ;
#92174 = CARTESIAN_POINT ( 'NONE',  ( -20.90000000000000213, 1.212568896937007645, -7.800000000000000711 ) ) ;
#92176 = CARTESIAN_POINT ( 'NONE',  ( -20.64999999999999858, 84.73084112150763758, -160.4250327655399531 ) ) ;
#92177 = CARTESIAN_POINT ( 'NONE',  ( -20.94999999999999929, 70.15000000001235492, -159.8906102602464330 ) ) ;
#92178 = DIRECTION ( 'NONE',  ( -1.000000000000000000, 0.000000000000000000, 0.000000000000000000 ) ) ;
#92180 = VERTEX_POINT ( 'NONE', #67112 ) ;
#92179 = TOROIDAL_SURFACE ( 'NONE', #183960, 11.89999999999999858, 0.1000000000000000056 ) ;
#92181 = ORIENTED_EDGE ( 'NONE', *, *, #156734, .T. ) ;
#92182 = CYLINDRICAL_SURFACE ( 'NONE', #12543, 1.749999999999999778 ) ;
#92184 = ORIENTED_EDGE ( 'NONE', *, *, #55941, .T. ) ;
#92183 = DIRECTION ( 'NONE',  ( 0.000000000000000000, 0.9915357197604971473, -0.1298341882519111479 ) ) ;
#92185 = VERTEX_POINT ( 'NONE', #90511 ) ;
#92186 = CARTESIAN_POINT ( 'NONE',  ( -16.77732147278574715, 12.41296741182544849, -211.2569465384485170 ) ) ;
#92187 = VERTEX_POINT ( 'NONE', #108796 ) ;
#92188 = FACE_OUTER_BOUND ( 'NONE', #60492, .T. ) ;
#92189 = VERTEX_POINT ( 'NONE', #206621 ) ;
#92190 = AXIS2_PLACEMENT_3D ( 'NONE', #173669, #73259, #148925 ) ;
#92191 = CARTESIAN_POINT ( 'NONE',  ( -18.59999999999999787, 64.35000000001198828, -115.1731074845243796 ) ) ;
#92192 = FACE_OUTER_BOUND ( 'NONE', #50137, .T. ) ;
#92194 = ORIENTED_EDGE ( 'NONE', *, *, #121818, .T. ) ;
#92193 = ORIENTED_EDGE ( 'NONE', *, *, #162954, .F. ) ;
#92195 = ORIENTED_EDGE ( 'NONE', *, *, #133849, .T. ) ;
#92196 = ORIENTED_EDGE ( 'NONE', *, *, #94937, .T. ) ;
#92197 = EDGE_LOOP ( 'NONE', ( #168211, #106328, #61294, #199834 ) ) ;
#92198 = CARTESIAN_POINT ( 'NONE',  ( 19.75857864376268935, 64.25000000001176659, -78.17310748452439384 ) ) ;
#92199 = DIRECTION ( 'NONE',  ( 0.000000000000000000, 0.1350103645451876666, -0.9908441862701600211 ) ) ;
#92200 = CARTESIAN_POINT ( 'NONE',  ( -15.15564720441980029, 9.410708747058235346, -185.5692084058440798 ) ) ;
#92202 = ORIENTED_EDGE ( 'NONE', *, *, #134222, .T. ) ;
#92201 = DIRECTION ( 'NONE',  ( -0.000000000000000000, 6.982962677686266711E-15, -1.000000000000000000 ) ) ;
#92203 = CYLINDRICAL_SURFACE ( 'NONE', #136617, 0.1000000000000098310 ) ;
#92204 = CARTESIAN_POINT ( 'NONE',  ( 21.07094088545303734, 6.320167221927647461, -167.4011062974477682 ) ) ;
#92206 = ORIENTED_EDGE ( 'NONE', *, *, #101421, .T. ) ;
#92205 = PLANE ( 'NONE',  #72532 ) ;
#92207 = LINE ( 'NONE', #250009, #42904 ) ;
#92208 = EDGE_LOOP ( 'NONE', ( #239490, #198725, #174218, #244110, #79681, #203323, #103142, #130398, #75267, #120888, #60380, #6197 ) ) ;
#92209 = DIRECTION ( 'NONE',  ( 1.000000000000000000, 0.000000000000000000, 0.000000000000000000 ) ) ;
#92210 = EDGE_LOOP ( 'NONE', ( #252974, #180352, #83193, #241918 ) ) ;
#92211 = CARTESIAN_POINT ( 'NONE',  ( -21.05000000000000071, 87.65000000001215597, -139.4231074845242802 ) ) ;
#92212 = DIRECTION ( 'NONE',  ( 1.000000000000000000, -0.000000000000000000, -0.000000000000000000 ) ) ;
#92213 = AXIS2_PLACEMENT_3D ( 'NONE', #8449, #145374, #164945 ) ;
#92215 = EDGE_CURVE ( 'NONE', #24871, #62504, #127085, .T. ) ;
#92214 = AXIS2_PLACEMENT_3D ( 'NONE', #154942, #234434, #92363 ) ;
#92216 = AXIS2_PLACEMENT_3D ( 'NONE', #248503, #12480, #211960 ) ;
#92217 = ORIENTED_EDGE ( 'NONE', *, *, #247251, .F. ) ;
#92219 = CARTESIAN_POINT ( 'NONE',  ( 20.73486653747088582, 9.775875410973629442, -211.8174516384118533 ) ) ;
#92218 = PLANE ( 'NONE',  #240478 ) ;
#92220 = DIRECTION ( 'NONE',  ( 1.000000000000000000, -0.000000000000000000, 0.000000000000000000 ) ) ;
#92221 = DIRECTION ( 'NONE',  ( -0.000000000000000000, 0.9910465087640860649, 0.1335171055202901413 ) ) ;
#92222 = CARTESIAN_POINT ( 'NONE',  ( -20.94999999999999929, 1.115600667400684642E-11, -167.5000000000000284 ) ) ;
#92223 = ORIENTED_EDGE ( 'NONE', *, *, #147949, .T. ) ;
#92224 = EDGE_LOOP ( 'NONE', ( #27771, #9343, #82576, #140669 ) ) ;
#92225 = FACE_OUTER_BOUND ( 'NONE', #55678, .T. ) ;
#92226 = DIRECTION ( 'NONE',  ( 1.000000000000000000, 0.000000000000000000, -0.000000000000000000 ) ) ;
#92227 = ORIENTED_EDGE ( 'NONE', *, *, #110518, .T. ) ;
#92228 = CARTESIAN_POINT ( 'NONE',  ( 23.14999999999998437, 1.115600667400684642E-11, -134.0000000000000000 ) ) ;
#92229 = ORIENTED_EDGE ( 'NONE', *, *, #51095, .F. ) ;
#92230 = EDGE_CURVE ( 'NONE', #90102, #21472, #173247, .T. ) ;
#92231 = CYLINDRICAL_SURFACE ( 'NONE', #169171, 0.1000000000000124678 ) ;
#92232 = DIRECTION ( 'NONE',  ( -1.000000000000000000, 0.000000000000000000, 0.000000000000000000 ) ) ;
#92233 = EDGE_CURVE ( 'NONE', #154466, #126916, #160756, .T. ) ;
#92234 = FACE_OUTER_BOUND ( 'NONE', #245103, .T. ) ;
#92235 = ORIENTED_EDGE ( 'NONE', *, *, #185181, .F. ) ;
#92236 = CARTESIAN_POINT ( 'NONE',  ( -11.60000000000000320, -11.75000000000000000, 17.70000000000000639 ) ) ;
#92237 = ORIENTED_EDGE ( 'NONE', *, *, #227436, .T. ) ;
#92238 = EDGE_LOOP ( 'NONE', ( #87596, #114809, #218846, #79519 ) ) ;
#92239 = ORIENTED_EDGE ( 'NONE', *, *, #241559, .F. ) ;
#92240 = EDGE_CURVE ( 'NONE', #176580, #90236, #123310, .T. ) ;
#92241 = LINE ( 'NONE', #252599, #100146 ) ;
#92242 = CARTESIAN_POINT ( 'NONE',  ( 15.06592377766032342, 66.58221053305935300, -54.16572294054753200 ) ) ;
#92243 = SPHERICAL_SURFACE ( 'NONE', #188148, 0.1000000000000000056 ) ;
#92245 = ADVANCED_FACE ( 'NONE', ( #8429 ), #86639, .T. ) ;
#92244 = CARTESIAN_POINT ( 'NONE',  ( 23.15000000000000213, 87.75000000001156764, -57.27310748452423894 ) ) ;
#92246 = DIRECTION ( 'NONE',  ( 0.000000000000000000, 0.1298341882520022694, 0.9915357197604852679 ) ) ;
#92247 = AXIS2_PLACEMENT_3D ( 'NONE', #191946, #130648, #210207 ) ;
#92249 = CARTESIAN_POINT ( 'NONE',  ( -16.81744102076748959, 9.949999999999983302, -20.85000000000000142 ) ) ;
#92248 = CARTESIAN_POINT ( 'NONE',  ( 22.47809213839789066, -3.122838153047792442, -228.1985781362319017 ) ) ;
#92251 = EDGE_LOOP ( 'NONE', ( #13310, #203766, #122942, #237332 ) ) ;
#92250 = CARTESIAN_POINT ( 'NONE',  ( -16.87683809663752399, 9.950000000011142376, -79.65000000000004832 ) ) ;
#92252 = ORIENTED_EDGE ( 'NONE', *, *, #129217, .T. ) ;
#92253 = EDGE_CURVE ( 'NONE', #174189, #91651, #256513, .T. ) ;
#92254 = CARTESIAN_POINT ( 'NONE',  ( -14.87779219673429054, 9.430633469083952392, -149.2317657948240992 ) ) ;
#92255 = EDGE_LOOP ( 'NONE', ( #126527, #24866, #52336 ) ) ;
#92256 = ORIENTED_EDGE ( 'NONE', *, *, #134389, .T. ) ;
#92257 = DIRECTION ( 'NONE',  ( 1.000000000000000000, 0.000000000000000000, 0.000000000000000000 ) ) ;
#92258 = AXIS2_PLACEMENT_3D ( 'NONE', #135558, #230848, #14373 ) ;
#92259 = CARTESIAN_POINT ( 'NONE',  ( -16.93658211146646408, 9.994108662352344297, -46.09570493004432734 ) ) ;
#92260 = CARTESIAN_POINT ( 'NONE',  ( -21.05000000000000071, 76.08579911628717696, -209.9370863660123518 ) ) ;
#92261 = DIRECTION ( 'NONE',  ( 4.026293107431335996E-15, -0.8700118002898359348, 0.4930308989875165082 ) ) ;
#92262 = EDGE_CURVE ( 'NONE', #6238, #122696, #210783, .T. ) ;
#92263 = CIRCLE ( 'NONE', #117215, 0.5000000000000004441 ) ;
#92264 = CARTESIAN_POINT ( 'NONE',  ( 20.94983749550516450, 18.35558276679135048, -236.8903279188150464 ) ) ;
#92265 = VECTOR ( 'NONE', #101890, 1000.000000000000000 ) ;
#92266 = ORIENTED_EDGE ( 'NONE', *, *, #256768, .T. ) ;
#92268 = ORIENTED_EDGE ( 'NONE', *, *, #243027, .T. ) ;
#92267 = EDGE_CURVE ( 'NONE', #86511, #206624, #50105, .T. ) ;
#92269 = CIRCLE ( 'NONE', #221248, 0.1000000000000028644 ) ;
#92270 = DIRECTION ( 'NONE',  ( -1.000000000000000000, -0.000000000000000000, -0.000000000000000000 ) ) ;
#92271 = VERTEX_POINT ( 'NONE', #147939 ) ;
#92272 = FACE_OUTER_BOUND ( 'NONE', #12587, .T. ) ;
#92273 = CARTESIAN_POINT ( 'NONE',  ( -18.59999999999999787, 14.80545736607782814, -235.9842437978701639 ) ) ;
#92274 = EDGE_LOOP ( 'NONE', ( #97315, #192155, #150446, #157930, #157352 ) ) ;
#92275 = SPHERICAL_SURFACE ( 'NONE', #11493, 0.1000000000000000056 ) ;
#92276 = DIRECTION ( 'NONE',  ( 0.000000000000000000, -0.4930308989875170078, -0.8700118002898356018 ) ) ;
#92277 = DIRECTION ( 'NONE',  ( 0.000000000000000000, -7.086529944415886769E-15, 1.000000000000000000 ) ) ;
#92278 = CARTESIAN_POINT ( 'NONE',  ( 21.12400247839515899, 65.27851195598189804, -157.7731074845244166 ) ) ;
#92279 = ORIENTED_EDGE ( 'NONE', *, *, #128039, .F. ) ;
#92280 = DIRECTION ( 'NONE',  ( 0.000000000000000000, -0.9274965247785323941, -0.3738317757009769760 ) ) ;
#92281 = CYLINDRICAL_SURFACE ( 'NONE', #12481, 0.09999999999999939493 ) ;
#92282 = CARTESIAN_POINT ( 'NONE',  ( 20.94999999999999929, 1.360870587192041681, -8.072997927090961312 ) ) ;
#92283 = EDGE_CURVE ( 'NONE', #156526, #76578, #35837, .T. ) ;
#92284 = DIRECTION ( 'NONE',  ( 0.000000000000000000, 1.000000000000000000, 6.982962677686266711E-15 ) ) ;
#92285 = CARTESIAN_POINT ( 'NONE',  ( 20.84999999999998721, 65.66751761918668251, -97.42826094061121012 ) ) ;
#92286 = AXIS2_PLACEMENT_3D ( 'NONE', #183802, #27340, #44306 ) ;
#92287 = CARTESIAN_POINT ( 'NONE',  ( -21.05000000000000071, 57.78573798790818472, -226.2252221607603246 ) ) ;
#92288 = AXIS2_PLACEMENT_3D ( 'NONE', #233255, #211097, #74193 ) ;
#92289 = ORIENTED_EDGE ( 'NONE', *, *, #168579, .F. ) ;
#92290 = AXIS2_PLACEMENT_3D ( 'NONE', #129399, #31616, #133251 ) ;
#92291 = DIRECTION ( 'NONE',  ( 0.000000000000000000, 0.9126074666063844765, 0.4088369013363114535 ) ) ;
#92292 = ORIENTED_EDGE ( 'NONE', *, *, #60502, .T. ) ;
#92293 = FACE_OUTER_BOUND ( 'NONE', #153220, .T. ) ;
#92294 = AXIS2_PLACEMENT_3D ( 'NONE', #135388, #96261, #10658 ) ;
#92295 = DIRECTION ( 'NONE',  ( 0.000000000000000000, -0.1298341882520022694, -0.9915357197604853789 ) ) ;
#92296 = DIRECTION ( 'NONE',  ( 0.000000000000000000, -1.000000000000000000, -6.982962677686267499E-15 ) ) ;
#92297 = DIRECTION ( 'NONE',  ( -1.000000000000000000, 0.000000000000000000, 0.000000000000000000 ) ) ;
#92298 = CARTESIAN_POINT ( 'NONE',  ( -18.59999999999999787, 77.85102823015316176, -158.3691942151018566 ) ) ;
#92299 = CARTESIAN_POINT ( 'NONE',  ( 18.49999999999999645, 74.27191306321758191, -116.1386724793565577 ) ) ;
#92300 = ORIENTED_EDGE ( 'NONE', *, *, #171082, .F. ) ;
#92301 = CYLINDRICAL_SURFACE ( 'NONE', #184302, 0.09999999999998898659 ) ;
#92302 = CARTESIAN_POINT ( 'NONE',  ( -16.87331047859649757, 66.05000000001182059, -82.17310748452439384 ) ) ;
#92303 = DIRECTION ( 'NONE',  ( 1.000000000000000000, -0.000000000000000000, 0.000000000000000000 ) ) ;
#92304 = DIRECTION ( 'NONE',  ( -0.9880948137434723000, 0.1538461538461483591, -0.000000000000000000 ) ) ;
#92305 = VECTOR ( 'NONE', #3857, 1000.000000000000000 ) ;
#92306 = DIRECTION ( 'NONE',  ( 0.000000000000000000, 0.2617529984165030688, 0.9651348961777157509 ) ) ;
#92307 = VECTOR ( 'NONE', #71212, 1000.000000000000000 ) ;
#92308 = EDGE_CURVE ( 'NONE', #208145, #226146, #219148, .T. ) ;
#92309 = VECTOR ( 'NONE', #76862, 1000.000000000000000 ) ;
#92310 = ORIENTED_EDGE ( 'NONE', *, *, #170043, .T. ) ;
#92311 = EDGE_LOOP ( 'NONE', ( #207379, #55857, #16815, #254562 ) ) ;
#92312 = CARTESIAN_POINT ( 'NONE',  ( -20.54999999999999716, 4.350000000011156054, -54.65000000000000568 ) ) ;
#92313 = DIRECTION ( 'NONE',  ( -1.000000000000000000, -3.469446951953635015E-14, -2.422701857770461054E-28 ) ) ;
#92314 = FACE_OUTER_BOUND ( 'NONE', #15566, .T. ) ;
#92315 =( NAMED_UNIT ( * ) SI_UNIT ( $, .STERADIAN. ) SOLID_ANGLE_UNIT ( ) );
#92316 = DIRECTION ( 'NONE',  ( 1.000000000000000000, -0.000000000000000000, -0.000000000000000000 ) ) ;
#92317 = EDGE_CURVE ( 'NONE', #36910, #14565, #26724, .T. ) ;
#92318 = ADVANCED_FACE ( 'NONE', ( #130937 ), #248216, .T. ) ;
#92319 = ORIENTED_EDGE ( 'NONE', *, *, #23772, .F. ) ;
#92320 = FACE_OUTER_BOUND ( 'NONE', #84549, .T. ) ;
#92321 = CONTEXT_DEPENDENT_SHAPE_REPRESENTATION ( #59182, #216118 ) ;
#92322 = DIRECTION ( 'NONE',  ( 0.000000000000000000, -0.1350103645451557199, -0.9908441862701644620 ) ) ;
#92323 = EDGE_CURVE ( 'NONE', #73682, #212264, #140029, .T. ) ;
#92324 = ORIENTED_EDGE ( 'NONE', *, *, #256990, .F. ) ;
#92326 = ADVANCED_FACE ( 'NONE', ( #189638 ), #70994, .T. ) ;
#92325 = CARTESIAN_POINT ( 'NONE',  ( 20.94999999999999574, 43.39316802731212874, -245.2602608822587342 ) ) ;
#92327 = EDGE_CURVE ( 'NONE', #105990, #201752, #244099, .T. ) ;
#92328 = VECTOR ( 'NONE', #65930, 1000.000000000000000 ) ;
#92329 = ADVANCED_FACE ( 'NONE', ( #96905 ), #10894, .T. ) ;
#92330 = ORIENTED_EDGE ( 'NONE', *, *, #167121, .T. ) ;
#92332 = VERTEX_POINT ( 'NONE', #155672 ) ;
#92331 = DIRECTION ( 'NONE',  ( 0.000000000000000000, 2.602085213965226419E-14, -1.000000000000000000 ) ) ;
#92333 = EDGE_CURVE ( 'NONE', #74587, #39052, #164994, .T. ) ;
#92334 = EDGE_LOOP ( 'NONE', ( #158483, #6973, #237357, #248587 ) ) ;
#92335 = DIRECTION ( 'NONE',  ( -1.000000000000000000, -0.000000000000000000, -0.000000000000000000 ) ) ;
#92336 = PLANE ( 'NONE',  #179706 ) ;
#92337 = CARTESIAN_POINT ( 'NONE',  ( 20.95512820512820440, 10.62384868372303259, -112.6500000000000341 ) ) ;
#92338 = FACE_OUTER_BOUND ( 'NONE', #153370, .T. ) ;
#92339 = DIRECTION ( 'NONE',  ( 1.000000000000000000, -0.000000000000000000, -0.000000000000000000 ) ) ;
#92340 = CARTESIAN_POINT ( 'NONE',  ( -18.59999999999999787, 72.08710075277916474, -192.0412845115134246 ) ) ;
#92341 = CARTESIAN_POINT ( 'NONE',  ( 23.15000000000000213, -11.48912529306489816, -130.9000000000000341 ) ) ;
#92343 = FACE_OUTER_BOUND ( 'NONE', #9469, .T. ) ;
#92342 = FACE_OUTER_BOUND ( 'NONE', #73483, .T. ) ;
#92344 = DIRECTION ( 'NONE',  ( 0.000000000000000000, -0.4721928772777346239, -0.8814952561688430555 ) ) ;
#92345 = CARTESIAN_POINT ( 'NONE',  ( 21.05000000000000071, 87.65000000001144542, -38.92310748452424463 ) ) ;
#92346 = CARTESIAN_POINT ( 'NONE',  ( -18.40000000000000213, 11.47316190337310893, -91.20017075153431563 ) ) ;
#92347 = CARTESIAN_POINT ( 'NONE',  ( 20.95378194480896639, 18.77190308950016018, -228.0183910527138380 ) ) ;
#92348 = VERTEX_POINT ( 'NONE', #255964 ) ;
#92349 = CARTESIAN_POINT ( 'NONE',  ( -20.85000000106584750, 11.75000000001115197, -93.65550465647375233 ) ) ;
#92350 = LINE ( 'NONE', #71536, #178779 ) ;
#92351 = LINE ( 'NONE', #96192, #95405 ) ;
#92352 = EDGE_CURVE ( 'NONE', #189474, #18191, #137337, .T. ) ;
#92353 = AXIS2_PLACEMENT_3D ( 'NONE', #208755, #9250, #88766 ) ;
#92354 = CARTESIAN_POINT ( 'NONE',  ( 23.15000000000000213, 87.48912529308749697, -39.12310748452424747 ) ) ;
#92355 = DIRECTION ( 'NONE',  ( 0.000000000000000000, -0.9916376685811618685, 0.1290532225514649800 ) ) ;
#92356 = FACE_OUTER_BOUND ( 'NONE', #109567, .T. ) ;
#92357 = ADVANCED_FACE ( 'NONE', ( #57797 ), #254687, .F. ) ;
#92358 = EDGE_CURVE ( 'NONE', #63643, #229783, #14989, .T. ) ;
#92359 = ORIENTED_EDGE ( 'NONE', *, *, #156478, .F. ) ;
#92360 = ORIENTED_EDGE ( 'NONE', *, *, #254760, .F. ) ;
#92361 = DIRECTION ( 'NONE',  ( 2.940209281316624467E-16, -0.4721928772777302941, -0.8814952561688453869 ) ) ;
#92362 = ORIENTED_EDGE ( 'NONE', *, *, #195168, .F. ) ;
#92363 = DIRECTION ( 'NONE',  ( 1.000000000000000000, 0.000000000000000000, 0.000000000000000000 ) ) ;
#92364 = CARTESIAN_POINT ( 'NONE',  ( 21.14999999999999858, 42.98415524044398950, -233.9519173640447889 ) ) ;
#92365 = TOROIDAL_SURFACE ( 'NONE', #213162, 11.90000000000000391, 0.1000000000000000056 ) ;
#92366 = AXIS2_PLACEMENT_3D ( 'NONE', #96397, #175981, #93845 ) ;
#92367 = AXIS2_PLACEMENT_3D ( 'NONE', #111303, #228694, #172606 ) ;
#92368 = ORIENTED_EDGE ( 'NONE', *, *, #2874, .F. ) ;
#92369 = CARTESIAN_POINT ( 'NONE',  ( 20.94999999999999929, 87.48912529308798014, -106.0231074845242176 ) ) ;
#92370 = VERTEX_POINT ( 'NONE', #31866 ) ;
#92371 = DIRECTION ( 'NONE',  ( 1.000000000000000000, 0.000000000000000000, 0.000000000000000000 ) ) ;
#92372 = CARTESIAN_POINT ( 'NONE',  ( -18.40000000000000213, 41.49355468354239207, -237.7178856438439141 ) ) ;
#92373 = LINE ( 'NONE', #35019, #157796 ) ;
#92374 = CARTESIAN_POINT ( 'NONE',  ( 18.49999999999999645, 76.00000000001170974, -69.52310748452431710 ) ) ;
#92375 = CARTESIAN_POINT ( 'NONE',  ( -20.95000000000000284, 64.35000000001251408, -177.0379132551784096 ) ) ;
#92376 = CARTESIAN_POINT ( 'NONE',  ( 22.50000000000000000, 7.128833340093095217, -233.7327013124392749 ) ) ;
#92377 = AXIS2_PLACEMENT_3D ( 'NONE', #58318, #77898, #76620 ) ;
#92378 = DIRECTION ( 'NONE',  ( -1.000000000000000000, 7.166229603267617241E-16, 4.447280054184918885E-16 ) ) ;
#92379 = CARTESIAN_POINT ( 'NONE',  ( -21.05000000000000071, 5.900000000011162093, -90.28090023534366537 ) ) ;
#92381 = ORIENTED_EDGE ( 'NONE', *, *, #137489, .T. ) ;
#92380 = FACE_OUTER_BOUND ( 'NONE', #147261, .T. ) ;
#92383 = DIRECTION ( 'NONE',  ( 0.000000000000000000, -6.467318590049456648E-15, 1.000000000000000000 ) ) ;
#92382 = DIRECTION ( 'NONE',  ( -7.304098846218134667E-16, -1.000000000000000000, 0.000000000000000000 ) ) ;
#92384 = VERTEX_POINT ( 'NONE', #34440 ) ;
#92386 = ORIENTED_EDGE ( 'NONE', *, *, #9708, .T. ) ;
#92385 = DIRECTION ( 'NONE',  ( 0.000000000000000000, 0.2128009952263403282, -0.9770955615653358350 ) ) ;
#92387 = ORIENTED_EDGE ( 'NONE', *, *, #156478, .T. ) ;
#92388 = DIRECTION ( 'NONE',  ( 1.000000000000000000, -0.000000000000000000, -0.000000000000000000 ) ) ;
#92389 = DIRECTION ( 'NONE',  ( 1.224646799147353207E-16, 1.000000000000000000, 0.000000000000000000 ) ) ;
#92390 = DIRECTION ( 'NONE',  ( -1.000000000000000000, -2.952720810173289112E-16, 0.000000000000000000 ) ) ;
#92391 = CARTESIAN_POINT ( 'NONE',  ( 18.45036689428341603, -9.490184143328932009, -7.012695827486270517 ) ) ;
#92392 = DIRECTION ( 'NONE',  ( -0.000000000000000000, 1.000000000000000000, 6.982962677686267499E-15 ) ) ;
#92393 = CARTESIAN_POINT ( 'NONE',  ( 0.8999999999999992450, -8.279289321881350361, 22.02928932188134326 ) ) ;
#92394 = CARTESIAN_POINT ( 'NONE',  ( 13.40000000000005898, 63.75000000001119815, -21.02310748452479316 ) ) ;
#92395 = EDGE_CURVE ( 'NONE', #8515, #218249, #81569, .T. ) ;
#92396 = CIRCLE ( 'NONE', #104841, 0.1000000000000106498 ) ;
#92397 = AXIS2_PLACEMENT_3D ( 'NONE', #209000, #66919, #149050 ) ;
#92399 = CIRCLE ( 'NONE', #134090, 0.09999999999999939493 ) ;
#92398 = DIRECTION ( 'NONE',  ( 0.000000000000000000, 0.9126074666063660468, 0.4088369013363524762 ) ) ;
#92400 = ORIENTED_EDGE ( 'NONE', *, *, #132380, .F. ) ;
#92401 = EDGE_LOOP ( 'NONE', ( #104397, #37670, #104993 ) ) ;
#92402 = ADVANCED_FACE ( 'NONE', ( #134762 ), #169129, .F. ) ;
#92403 = CARTESIAN_POINT ( 'NONE',  ( -23.25000000000000000, 4.350000000011156054, -112.6500000000000483 ) ) ;
#92404 = ORIENTED_EDGE ( 'NONE', *, *, #230383, .T. ) ;
#92405 = DIRECTION ( 'NONE',  ( 0.000000000000000000, 0.8814952561688430555, -0.4721928772777346239 ) ) ;
#92406 = ORIENTED_EDGE ( 'NONE', *, *, #196241, .T. ) ;
#92407 = DIRECTION ( 'NONE',  ( -0.000000000000000000, 1.000000000000000000, -0.000000000000000000 ) ) ;
#92408 = ADVANCED_FACE ( 'NONE', ( #52669 ), #23385, .T. ) ;
#92409 = ADVANCED_FACE ( 'NONE', ( #215596 ), #116520, .F. ) ;
#92410 = DIRECTION ( 'NONE',  ( 0.000000000000000000, -6.938893903907222067E-15, 1.000000000000000000 ) ) ;
#92411 = CARTESIAN_POINT ( 'NONE',  ( 21.05000000000000071, 70.41157348381892689, -224.1287375179191201 ) ) ;
#92412 = DIRECTION ( 'NONE',  ( -1.000000000000000000, -0.000000000000000000, -0.000000000000000000 ) ) ;
#92413 = LINE ( 'NONE', #250217, #3946 ) ;
#92414 = ORIENTED_EDGE ( 'NONE', *, *, #165874, .T. ) ;
#92415 = DIRECTION ( 'NONE',  ( 0.000000000000000000, -1.000000000000000000, -6.982962677686265922E-15 ) ) ;
#92416 = CIRCLE ( 'NONE', #138195, 4.300000000000035350 ) ;
#92417 = CARTESIAN_POINT ( 'NONE',  ( -18.59999999999999787, 1.835341550235567887, -112.0551512925630249 ) ) ;
#92418 = DIRECTION ( 'NONE',  ( 0.000000000000000000, 0.000000000000000000, 1.000000000000000000 ) ) ;
#92419 = DIRECTION ( 'NONE',  ( -1.000000000000000000, 0.000000000000000000, 0.000000000000000000 ) ) ;
#92420 = ORIENTED_EDGE ( 'NONE', *, *, #38254, .F. ) ;
#92422 = CARTESIAN_POINT ( 'NONE',  ( 21.05000000000000071, 13.54362637910787370, -238.4879411198429580 ) ) ;
#92421 = CARTESIAN_POINT ( 'NONE',  ( 18.59999999999999076, 11.65000000001115943, -91.85000000000003695 ) ) ;
#92423 = ORIENTED_EDGE ( 'NONE', *, *, #151917, .T. ) ;
#92426 = ORIENTED_EDGE ( 'NONE', *, *, #37688, .F. ) ;
#92425 = DIRECTION ( 'NONE',  ( 3.469446951953635015E-14, -0.2128009952263604232, 0.9770955615653316162 ) ) ;
#92424 = DIRECTION ( 'NONE',  ( 0.000000000000000000, 0.000000000000000000, 1.000000000000000000 ) ) ;
#92427 = EDGE_CURVE ( 'NONE', #190621, #154962, #231647, .T. ) ;
#92428 = ADVANCED_FACE ( 'NONE', ( #111376 ), #202413, .T. ) ;
#92429 = EDGE_LOOP ( 'NONE', ( #202353, #227618, #196359, #93110 ) ) ;
#92430 = CARTESIAN_POINT ( 'NONE',  ( 20.94999999999999574, -1.736257131586239844, -145.5686523290175387 ) ) ;
#92431 = VECTOR ( 'NONE', #74263, 1000.000000000000000 ) ;
#92432 = FACE_OUTER_BOUND ( 'NONE', #143662, .T. ) ;
#92433 = DIRECTION ( 'NONE',  ( 0.000000000000000000, 0.000000000000000000, -1.000000000000000000 ) ) ;
#92435 = ORIENTED_EDGE ( 'NONE', *, *, #197179, .F. ) ;
#92434 = DIRECTION ( 'NONE',  ( 0.000000000000000000, 0.9126074666063844765, 0.4088369013363114535 ) ) ;
#92436 = VECTOR ( 'NONE', #157758, 1000.000000000000000 ) ;
#92437 = EDGE_CURVE ( 'NONE', #234056, #209722, #202596, .T. ) ;
#92438 = AXIS2_PLACEMENT_3D ( 'NONE', #123888, #1340, #125172 ) ;
#92439 = ORIENTED_EDGE ( 'NONE', *, *, #239413, .T. ) ;
#92440 = AXIS2_PLACEMENT_3D ( 'NONE', #233468, #134322, #148785 ) ;
#92441 = AXIS2_PLACEMENT_3D ( 'NONE', #182961, #121709, #97260 ) ;
#92443 = EDGE_CURVE ( 'NONE', #27329, #203889, #123489, .T. ) ;
#92442 = LINE ( 'NONE', #29945, #182664 ) ;
#92444 = CARTESIAN_POINT ( 'NONE',  ( 18.50000000000000000, -9.399999999988823518, -74.29725975966330509 ) ) ;
#92445 = DIRECTION ( 'NONE',  ( -1.476360405086644309E-16, -1.000000000000000000, -1.445602896647339410E-16 ) ) ;
#92446 = CARTESIAN_POINT ( 'NONE',  ( 22.39999999999999503, 12.58895012248959766, -223.3279127647276141 ) ) ;
#92448 = VERTEX_POINT ( 'NONE', #154393 ) ;
#92447 = AXIS2_PLACEMENT_3D ( 'NONE', #241148, #62500, #136888 ) ;
#92449 = DIRECTION ( 'NONE',  ( 0.000000000000000000, -0.008583690987162452199, 0.9999631594459053030 ) ) ;
#92450 = AXIS2_PLACEMENT_3D ( 'NONE', #29812, #109290, #188845 ) ;
#92451 = DIRECTION ( 'NONE',  ( 9.044546369203339308E-15, -0.7397360091702694929, -0.6728971962616898672 ) ) ;
#92452 = DIRECTION ( 'NONE',  ( 0.000000000000000000, 0.8660254037844411501, 0.4999999999999956701 ) ) ;
#92453 = ORIENTED_EDGE ( 'NONE', *, *, #78306, .F. ) ;
#92454 = EDGE_CURVE ( 'NONE', #39964, #211866, #173439, .T. ) ;
#92455 = FACE_OUTER_BOUND ( 'NONE', #246143, .T. ) ;
#92456 = VECTOR ( 'NONE', #140675, 1000.000000000000000 ) ;
#92457 = EDGE_CURVE ( 'NONE', #177863, #194806, #94362, .T. ) ;
#92458 = DIRECTION ( 'NONE',  ( 1.000000000000000000, -0.000000000000000000, -0.000000000000000000 ) ) ;
#92459 = CIRCLE ( 'NONE', #213082, 2.000000000000004885 ) ;
#92460 = VERTEX_POINT ( 'NONE', #35721 ) ;
#92462 = EDGE_CURVE ( 'NONE', #135981, #63725, #244273, .T. ) ;
#92461 = AXIS2_PLACEMENT_3D ( 'NONE', #160101, #234467, #100070 ) ;
#92463 = DIRECTION ( 'NONE',  ( 0.000000000000000000, -0.000000000000000000, 1.000000000000000000 ) ) ;
#92464 = DIRECTION ( 'NONE',  ( 1.000000000000000000, 0.000000000000000000, 0.000000000000000000 ) ) ;
#92465 = CIRCLE ( 'NONE', #154866, 0.1000000000000065004 ) ;
#92466 = ORIENTED_EDGE ( 'NONE', *, *, #245899, .F. ) ;
#92467 = ORIENTED_EDGE ( 'NONE', *, *, #197398, .T. ) ;
#92468 = AXIS2_PLACEMENT_3D ( 'NONE', #6024, #82972, #205513 ) ;
#92469 = CARTESIAN_POINT ( 'NONE',  ( -21.00000000000000000, 0.000000000000000000, 0.000000000000000000 ) ) ;
#92470 = ORIENTED_EDGE ( 'NONE', *, *, #182763, .T. ) ;
#92472 = ORIENTED_EDGE ( 'NONE', *, *, #231304, .T. ) ;
#92471 = CARTESIAN_POINT ( 'NONE',  ( -23.15000000000000213, 70.05000000001251692, -180.3288097895592159 ) ) ;
#92473 = EDGE_CURVE ( 'NONE', #87303, #221570, #31933, .T. ) ;
#92474 = AXIS2_PLACEMENT_3D ( 'NONE', #160957, #5689, #43567 ) ;
#92475 = ORIENTED_EDGE ( 'NONE', *, *, #58441, .F. ) ;
#92478 = EDGE_LOOP ( 'NONE', ( #130816, #175934, #210640, #230036 ) ) ;
#92477 = ORIENTED_EDGE ( 'NONE', *, *, #133935, .T. ) ;
#92476 = CARTESIAN_POINT ( 'NONE',  ( -18.79999999999999716, 7.900000000000000355, 1.212568896937007867 ) ) ;
#92479 = EDGE_CURVE ( 'NONE', #100605, #98906, #78649, .T. ) ;
#92480 = DIRECTION ( 'NONE',  ( -0.000000000000000000, 0.000000000000000000, 1.000000000000000000 ) ) ;
#92481 = ORIENTED_EDGE ( 'NONE', *, *, #4383, .F. ) ;
#92482 = FACE_OUTER_BOUND ( 'NONE', #152895, .T. ) ;
#92483 = DIRECTION ( 'NONE',  ( -0.000000000000000000, -0.000000000000000000, -1.000000000000000000 ) ) ;
#92484 = VECTOR ( 'NONE', #29258, 1000.000000000000000 ) ;
#92485 = CIRCLE ( 'NONE', #21778, 0.09999999999999939493 ) ;
#92486 = DIRECTION ( 'NONE',  ( -0.000000000000000000, -0.4721928772777346239, -0.8814952561688430555 ) ) ;
#92487 = CARTESIAN_POINT ( 'NONE',  ( -20.85000000000000142, 0.000000000000000000, -33.50000000000000000 ) ) ;
#92489 = FACE_OUTER_BOUND ( 'NONE', #26186, .T. ) ;
#92488 = CIRCLE ( 'NONE', #234132, 0.1999999999999996503 ) ;
#92490 = ORIENTED_EDGE ( 'NONE', *, *, #217240, .T. ) ;
#92491 = EDGE_LOOP ( 'NONE', ( #188216, #60776, #253179, #48726 ) ) ;
#92492 = VERTEX_POINT ( 'NONE', #202474 ) ;
#92493 = DIRECTION ( 'NONE',  ( 0.000000000000000000, 8.673617379884042375E-16, 1.000000000000000000 ) ) ;
#92495 = EDGE_LOOP ( 'NONE', ( #107912, #33440, #44825, #166369 ) ) ;
#92494 = CARTESIAN_POINT ( 'NONE',  ( 20.94999999999999574, 1.835341550235567887, -112.1551512925630192 ) ) ;
#92496 = CARTESIAN_POINT ( 'NONE',  ( -23.25000000000000000, 71.65000000001187175, -90.67310748452433700 ) ) ;
#92498 = VERTEX_POINT ( 'NONE', #2969 ) ;
#92497 = DIRECTION ( 'NONE',  ( 0.000000000000000000, 0.9126074666063769270, 0.4088369013363280513 ) ) ;
#92499 = ORIENTED_EDGE ( 'NONE', *, *, #230025, .T. ) ;
#92500 = CARTESIAN_POINT ( 'NONE',  ( 18.79999999999999005, 8.000000000000000000, -1.212568896937008089 ) ) ;
#92501 = ORIENTED_EDGE ( 'NONE', *, *, #37644, .F. ) ;
#92502 = CARTESIAN_POINT ( 'NONE',  ( -16.82542659449978117, 9.934499891438612451, -180.2446356000259868 ) ) ;
#92503 = AXIS2_PLACEMENT_3D ( 'NONE', #27197, #186242, #187542 ) ;
#92505 = ORIENTED_EDGE ( 'NONE', *, *, #21887, .T. ) ;
#92504 = ORIENTED_EDGE ( 'NONE', *, *, #176462, .T. ) ;
#92506 = ORIENTED_EDGE ( 'NONE', *, *, #255543, .F. ) ;
#92507 = DIRECTION ( 'NONE',  ( -1.000000000000000000, 0.000000000000000000, 0.000000000000000000 ) ) ;
#92508 = ORIENTED_EDGE ( 'NONE', *, *, #132789, .F. ) ;
#92509 = VERTEX_POINT ( 'NONE', #180343 ) ;
#92510 = DIRECTION ( 'NONE',  ( -0.8191520442889919096, -0.5735764363510460484, 0.000000000000000000 ) ) ;
#92512 = ORIENTED_EDGE ( 'NONE', *, *, #115998, .T. ) ;
#92511 = DIRECTION ( 'NONE',  ( 0.000000000000000000, -1.000000000000000000, -6.982962677686266711E-15 ) ) ;
#92513 = DIRECTION ( 'NONE',  ( 0.000000000000000000, -0.9651348961777158619, 0.2617529984165032353 ) ) ;
#92515 = DIRECTION ( 'NONE',  ( 0.000000000000000000, 0.000000000000000000, 1.000000000000000000 ) ) ;
#92514 = CARTESIAN_POINT ( 'NONE',  ( -2.995603634470829482E-16, -6.958851699820998604, -224.2636923771745501 ) ) ;
#92516 = CARTESIAN_POINT ( 'NONE',  ( 23.24999999999999645, 5.600000000011153389, -155.7499999999999716 ) ) ;
#92517 = FACE_OUTER_BOUND ( 'NONE', #129434, .T. ) ;
#92518 = EDGE_LOOP ( 'NONE', ( #164328, #246462, #153172, #161027, #30462, #207478, #78236 ) ) ;
#92519 = ORIENTED_EDGE ( 'NONE', *, *, #157772, .F. ) ;
#92520 = CARTESIAN_POINT ( 'NONE',  ( 18.47135592147649774, 85.47108861327761531, -96.33951254468077252 ) ) ;
#92521 = CARTESIAN_POINT ( 'NONE',  ( -20.64999999999999858, -9.499999999988846255, -191.1060308773475356 ) ) ;
#92522 = DIRECTION ( 'NONE',  ( 0.000000000000000000, -0.3999834006488773852, -0.9165223833629813077 ) ) ;
#92523 = EDGE_CURVE ( 'NONE', #189014, #69020, #240322, .T. ) ;
#92524 = ORIENTED_EDGE ( 'NONE', *, *, #122440, .T. ) ;
#92525 = CARTESIAN_POINT ( 'NONE',  ( -20.54999999999999716, 4.250000000011156409, -146.2500000000000284 ) ) ;
#92526 = VECTOR ( 'NONE', #79479, 1000.000000000000000 ) ;
#92527 = CARTESIAN_POINT ( 'NONE',  ( -0.8999999999999993561, -11.65000000000000036, 28.70000000000000284 ) ) ;
#92528 = CARTESIAN_POINT ( 'NONE',  ( -21.65000000000000213, 66.05000000001201954, -115.7731074845243597 ) ) ;
#92529 = ORIENTED_EDGE ( 'NONE', *, *, #2264, .F. ) ;
#92530 = ORIENTED_EDGE ( 'NONE', *, *, #230793, .F. ) ;
#92531 = PLANE ( 'NONE',  #34425 ) ;
#92532 = EDGE_CURVE ( 'NONE', #11679, #88959, #181636, .T. ) ;
#92533 = DIRECTION ( 'NONE',  ( -0.000000000000000000, 1.000000000000000000, 0.000000000000000000 ) ) ;
#92534 = ORIENTED_EDGE ( 'NONE', *, *, #40818, .F. ) ;
#92535 = DIRECTION ( 'NONE',  ( 0.000000000000000000, 0.1455152366551500653, 0.9893560106964507384 ) ) ;
#92536 = EDGE_LOOP ( 'NONE', ( #218826, #104879, #106956, #178064 ) ) ;
#92537 = CARTESIAN_POINT ( 'NONE',  ( 18.39999999999999858, -9.499999999988844479, -140.9221498493304239 ) ) ;
#92538 = CARTESIAN_POINT ( 'NONE',  ( 23.14999999999999858, 71.00000000001223555, -148.9283735034374843 ) ) ;
#92540 = FACE_OUTER_BOUND ( 'NONE', #62553, .T. ) ;
#92539 = CARTESIAN_POINT ( 'NONE',  ( 23.14999999999999503, 64.35000000001176090, -76.43791325517833002 ) ) ;
#92541 = ADVANCED_FACE ( 'NONE', ( #197315 ), #177794, .F. ) ;
#92543 = ADVANCED_FACE ( 'NONE', ( #18691 ), #103346, .F. ) ;
#92542 = FACE_OUTER_BOUND ( 'NONE', #154980, .T. ) ;
#92544 = CARTESIAN_POINT ( 'NONE',  ( -18.59999999999999787, 42.98415524044398950, -233.9519173640448173 ) ) ;
#92545 = CARTESIAN_POINT ( 'NONE',  ( 21.05000000000000071, -6.438379425586758131, -212.1495692908769684 ) ) ;
#92546 = AXIS2_PLACEMENT_3D ( 'NONE', #145851, #29810, #71490 ) ;
#92548 = ORIENTED_EDGE ( 'NONE', *, *, #77455, .F. ) ;
#92547 = CYLINDRICAL_SURFACE ( 'NONE', #148295, 0.09999999999998898659 ) ;
#92549 = AXIS2_PLACEMENT_3D ( 'NONE', #121601, #202390, #104536 ) ;
#92551 = ORIENTED_EDGE ( 'NONE', *, *, #162699, .F. ) ;
#92550 = ORIENTED_EDGE ( 'NONE', *, *, #122202, .T. ) ;
#92552 = VERTEX_POINT ( 'NONE', #199920 ) ;
#92553 = CIRCLE ( 'NONE', #13469, 0.09999999999999939493 ) ;
#92554 = ADVANCED_FACE ( 'NONE', ( #23863 ), #61674, .F. ) ;
#92555 = CARTESIAN_POINT ( 'NONE',  ( 22.45301702632625762, 0.01521087971018478258, 11.64979222426039129 ) ) ;
#92556 = DIRECTION ( 'NONE',  ( 1.000000000000000000, 0.000000000000000000, -0.000000000000000000 ) ) ;
#92557 = CARTESIAN_POINT ( 'NONE',  ( 21.14999999999999858, 21.15538238767524604, -233.7023398932965108 ) ) ;
#92558 = CYLINDRICAL_SURFACE ( 'NONE', #28999, 0.09999999999999939493 ) ;
#92559 = ORIENTED_EDGE ( 'NONE', *, *, #43659, .F. ) ;
#92560 = CARTESIAN_POINT ( 'NONE',  ( 22.60000000000000142, 11.45898712536580177, -198.4011321578509808 ) ) ;
#92561 = VERTEX_POINT ( 'NONE', #119087 ) ;
#92562 = EDGE_LOOP ( 'NONE', ( #95950, #99432, #159743, #137371 ) ) ;
#92563 = CARTESIAN_POINT ( 'NONE',  ( -21.04999999999999716, 69.70076908991939035, -69.62154498452471785 ) ) ;
#92565 = AXIS2_PLACEMENT_3D ( 'NONE', #53053, #90898, #36080 ) ;
#92564 = CARTESIAN_POINT ( 'NONE',  ( -23.24999999999999645, -9.599999999988845900, -107.1001893912220879 ) ) ;
#92566 = VECTOR ( 'NONE', #93741, 1000.000000000000227 ) ;
#92567 = CARTESIAN_POINT ( 'NONE',  ( -21.09096482362058822, 1.538026365827115383, -230.6931075182510256 ) ) ;
#92568 = DIRECTION ( 'NONE',  ( 1.000000000000000000, 0.000000000000000000, -0.000000000000000000 ) ) ;
#92569 = DIRECTION ( 'NONE',  ( 0.000000000000000000, 0.000000000000000000, 1.000000000000000000 ) ) ;
#92570 = ORIENTED_EDGE ( 'NONE', *, *, #216561, .F. ) ;
#92572 = VERTEX_POINT ( 'NONE', #201180 ) ;
#92571 = EDGE_CURVE ( 'NONE', #236445, #156311, #127593, .T. ) ;
#92573 = CARTESIAN_POINT ( 'NONE',  ( 20.95512820512820440, 22.85550638026973047, -230.1049725544161220 ) ) ;
#92574 = CARTESIAN_POINT ( 'NONE',  ( 22.50497660315937054, -0.07871793021434785043, -88.75020449510458320 ) ) ;
#92575 = CARTESIAN_POINT ( 'NONE',  ( 21.05000000000000071, -5.011722593499792211, -233.2041167654973322 ) ) ;
#92576 = CARTESIAN_POINT ( 'NONE',  ( 20.94999999999999574, 6.400000000011158541, -43.43042463006157305 ) ) ;
#92577 = CYLINDRICAL_SURFACE ( 'NONE', #177748, 4.000000000000003553 ) ;
#92578 = CARTESIAN_POINT ( 'NONE',  ( -16.89021194854739605, 9.950000000011137047, -188.2425681316042585 ) ) ;
#92579 = CARTESIAN_POINT ( 'NONE',  ( -18.39999999999999858, 64.52683809664941350, -93.69716141771641560 ) ) ;
#92580 = CARTESIAN_POINT ( 'NONE',  ( -22.39999999999999858, 7.790779598384559357, -33.50000000000000711 ) ) ;
#92583 = CARTESIAN_POINT ( 'NONE',  ( -18.59999999999999787, 47.07326788871598211, -255.0992659944397190 ) ) ;
#92582 = TOROIDAL_SURFACE ( 'NONE', #246529, 0.9750000000000019762, 0.1000000000000000056 ) ;
#92581 = CARTESIAN_POINT ( 'NONE',  ( -18.52328366898032641, 85.64232108905335394, -129.8082881469542258 ) ) ;
#92585 = LINE ( 'NONE', #213831, #33396 ) ;
#92584 = AXIS2_PLACEMENT_3D ( 'NONE', #26615, #220920, #185673 ) ;
#92586 = EDGE_CURVE ( 'NONE', #14612, #134542, #158246, .T. ) ;
#92587 = VECTOR ( 'NONE', #198493, 1000.000000000000000 ) ;
#92588 = DIRECTION ( 'NONE',  ( 1.000000000000000000, 0.000000000000000000, 0.000000000000000000 ) ) ;
#92589 = CARTESIAN_POINT ( 'NONE',  ( 13.40000000000005898, 67.72071067812984779, -17.05239680640613997 ) ) ;
#92591 = LINE ( 'NONE', #150033, #235782 ) ;
#92590 = B_SPLINE_CURVE_WITH_KNOTS ( 'NONE', 3,
 ( #215964, #255038, #218521, #99853, #195169, #79008, #197688, #116883, #34811, #157323 ),
 .UNSPECIFIED., .F., .F.,
 ( 4, 2, 2, 2, 4 ),
 ( 0.000000000000000000, 0.0001660831991682299249, 0.0002491247987523412147, 0.0002906455985444013454, 0.0003321663983364614762 ),
 .UNSPECIFIED. ) ;
#92593 = ORIENTED_EDGE ( 'NONE', *, *, #218992, .F. ) ;
#92592 = DIRECTION ( 'NONE',  ( 1.000000000000000000, -0.000000000000000000, -0.000000000000000000 ) ) ;
#92594 = DIRECTION ( 'NONE',  ( 0.000000000000000000, -0.2128009952263734406, 0.9770955615653287296 ) ) ;
#92595 = AXIS2_PLACEMENT_3D ( 'NONE', #8343, #167429, #227370 ) ;
#92596 = DIRECTION ( 'NONE',  ( -1.000000000000000000, -2.952720810173289112E-16, 0.000000000000000000 ) ) ;
#92597 = EDGE_CURVE ( 'NONE', #6661, #232107, #223425, .T. ) ;
#92598 = FACE_BOUND ( 'NONE', #87558, .T. ) ;
#92599 = CARTESIAN_POINT ( 'NONE',  ( 12.48201962039796520, 9.376659938544690931, -84.62819254821734205 ) ) ;
#92600 = DIRECTION ( 'NONE',  ( 0.000000000000000000, 0.4930308989875230585, 0.8700118002898322711 ) ) ;
#92601 = CIRCLE ( 'NONE', #213402, 0.1999999999999998446 ) ;
#92602 = CARTESIAN_POINT ( 'NONE',  ( 23.24999999999999289, 2.272311100394802885, -217.9150152700588592 ) ) ;
#92603 = FACE_OUTER_BOUND ( 'NONE', #79420, .T. ) ;
#92604 = CARTESIAN_POINT ( 'NONE',  ( -16.90137573187934095, 66.05000000001156479, -56.73469006042749641 ) ) ;
#92605 = ADVANCED_FACE ( 'NONE', ( #219443 ), #56808, .F. ) ;
#92606 = EDGE_CURVE ( 'NONE', #9648, #112737, #11059, .T. ) ;
#92607 = ORIENTED_EDGE ( 'NONE', *, *, #77069, .F. ) ;
#92608 = DIRECTION ( 'NONE',  ( 0.000000000000000000, -0.000000000000000000, 1.000000000000000000 ) ) ;
#92610 = EDGE_LOOP ( 'NONE', ( #30899, #138761, #19364, #227638 ) ) ;
#92609 = CARTESIAN_POINT ( 'NONE',  ( 21.05000000000000071, 1.115600667400684642E-11, -100.5000000000000284 ) ) ;
#92611 = CARTESIAN_POINT ( 'NONE',  ( -20.85000000000000142, 72.03510814376021187, -246.5782642391033903 ) ) ;
#92612 = CIRCLE ( 'NONE', #84372, 11.74999999999999645 ) ;
#92614 = ADVANCED_FACE ( 'NONE', ( #59066 ), #39577, .F. ) ;
#92613 = FACE_OUTER_BOUND ( 'NONE', #104174, .T. ) ;
#92615 = EDGE_CURVE ( 'NONE', #72387, #61667, #19449, .T. ) ;
#92616 = VERTEX_POINT ( 'NONE', #139902 ) ;
#92617 = DIRECTION ( 'NONE',  ( -1.000000000000000000, 0.000000000000000000, 0.000000000000000000 ) ) ;
#92618 = AXIS2_PLACEMENT_3D ( 'NONE', #21748, #41328, #97382 ) ;
#92619 = APPLICATION_PROTOCOL_DEFINITION ( 'draft international standard', 'automotive_design', 1998, #145654 ) ;
#92620 = CARTESIAN_POINT ( 'NONE',  ( 20.95000000000000284, 62.99095723518624368, -207.1734234082435080 ) ) ;
#92622 = AXIS2_PLACEMENT_3D ( 'NONE', #201807, #123565, #144376 ) ;
#92621 = CYLINDRICAL_SURFACE ( 'NONE', #79821, 0.09999999999998657185 ) ;
#92623 = ADVANCED_FACE ( 'NONE', ( #40859 ), #69340, .F. ) ;
#92624 = ORIENTED_EDGE ( 'NONE', *, *, #107684, .F. ) ;
#92625 = CIRCLE ( 'NONE', #134133, 0.5000000000000004441 ) ;
#92626 = CARTESIAN_POINT ( 'NONE',  ( 23.14999999999999858, 5.600000000011153389, -45.90526601891310321 ) ) ;
#92627 = DIRECTION ( 'NONE',  ( 0.000000000000000000, 0.9126074666063545004, 0.4088369013363783999 ) ) ;
#92628 = CIRCLE ( 'NONE', #217699, 11.80000000000001315 ) ;
#92629 = EDGE_CURVE ( 'NONE', #148934, #204227, #231844, .T. ) ;
#92632 = EDGE_CURVE ( 'NONE', #179904, #75051, #44393, .T. ) ;
#92631 = EDGE_CURVE ( 'NONE', #2690, #206918, #164634, .T. ) ;
#92630 = VECTOR ( 'NONE', #197207, 1000.000000000000000 ) ;
#92633 = AXIS2_PLACEMENT_3D ( 'NONE', #21873, #101347, #2279 ) ;
#92634 = CARTESIAN_POINT ( 'NONE',  ( -33.72168855820451938, 51.61886293219128419, -231.9464690156495124 ) ) ;
#92635 = ORIENTED_EDGE ( 'NONE', *, *, #23480, .T. ) ;
#92636 = ORIENTED_EDGE ( 'NONE', *, *, #105928, .T. ) ;
#92638 = CIRCLE ( 'NONE', #100971, 0.1000000000000054040 ) ;
#92637 = DIRECTION ( 'NONE',  ( -1.000000000000000000, -0.000000000000000000, -0.000000000000000000 ) ) ;
#92639 = CARTESIAN_POINT ( 'NONE',  ( 20.95000000000005258, 66.15000000001120384, -6.023107484524794941 ) ) ;
#92640 = CARTESIAN_POINT ( 'NONE',  ( 22.39999999999999503, 64.35000000001237197, -170.0231074845244166 ) ) ;
#92641 = EDGE_CURVE ( 'NONE', #91489, #23345, #25138, .T. ) ;
#92642 = CYLINDRICAL_SURFACE ( 'NONE', #186718, 0.09999999999999986677 ) ;
#92644 = CARTESIAN_POINT ( 'NONE',  ( -20.64999999999999858, 68.85000000001180354, -81.77310748452435973 ) ) ;
#92643 = CYLINDRICAL_SURFACE ( 'NONE', #215881, 0.09999999999999961697 ) ;
#92645 = AXIS2_PLACEMENT_3D ( 'NONE', #128664, #218434, #55491 ) ;
#92646 = AXIS2_PLACEMENT_3D ( 'NONE', #20730, #2409, #138072 ) ;
#92647 = CARTESIAN_POINT ( 'NONE',  ( -21.08621493067320429, 75.94380516053638530, -176.3724017756962894 ) ) ;
#92649 = EDGE_CURVE ( 'NONE', #243903, #168786, #106907, .T. ) ;
#92648 = FACE_OUTER_BOUND ( 'NONE', #108129, .T. ) ;
#92650 = DIRECTION ( 'NONE',  ( -7.304098846218134667E-16, -0.9651348961777158619, 0.2617529984165031243 ) ) ;
#92653 = ADVANCED_FACE ( 'NONE', ( #6835 ), #36015, .F. ) ;
#92652 = CARTESIAN_POINT ( 'NONE',  ( 20.94999999999999574, 10.62357026049396680, -74.49194520323059976 ) ) ;
#92651 = VECTOR ( 'NONE', #252027, 1000.000000000000000 ) ;
#92654 = ORIENTED_EDGE ( 'NONE', *, *, #245113, .F. ) ;
#92656 = ORIENTED_EDGE ( 'NONE', *, *, #171619, .F. ) ;
#92655 = PLANE ( 'NONE',  #36561 ) ;
#92657 = DIRECTION ( 'NONE',  ( 0.000000000000000000, 0.000000000000000000, 1.000000000000000000 ) ) ;
#92658 = TOROIDAL_SURFACE ( 'NONE', #5717, 11.65000000000000036, 0.1000000000000000056 ) ;
#92659 = DIRECTION ( 'NONE',  ( 0.000000000000000000, 0.9651348961777157509, -0.2617529984165031243 ) ) ;
#92660 = DIRECTION ( 'NONE',  ( 0.000000000000000000, 0.9126074666063660468, 0.4088369013363524762 ) ) ;
#92661 = AXIS2_PLACEMENT_3D ( 'NONE', #194973, #175417, #155845 ) ;
#92662 = EDGE_CURVE ( 'NONE', #152757, #228728, #145052, .T. ) ;
#92663 = ORIENTED_EDGE ( 'NONE', *, *, #186911, .T. ) ;
#92664 = CYLINDRICAL_SURFACE ( 'NONE', #2055, 0.09999999999999939493 ) ;
#92665 = DIRECTION ( 'NONE',  ( 1.000000000000000000, 0.000000000000000000, 0.000000000000000000 ) ) ;
#92666 = FACE_OUTER_BOUND ( 'NONE', #171876, .T. ) ;
#92668 = CARTESIAN_POINT ( 'NONE',  ( 15.51872946208856696, 12.91284736048184634, -216.2278651779593304 ) ) ;
#92667 = AXIS2_PLACEMENT_3D ( 'NONE', #144148, #244544, #65922 ) ;
#92669 = VERTEX_POINT ( 'NONE', #244145 ) ;
#92670 = EDGE_CURVE ( 'NONE', #176398, #207698, #111016, .T. ) ;
#92671 = ORIENTED_EDGE ( 'NONE', *, *, #104644, .T. ) ;
#92672 = CARTESIAN_POINT ( 'NONE',  ( 21.05000000000000071, 45.65843669757526158, -240.2045374387683410 ) ) ;
#92673 = ORIENTED_EDGE ( 'NONE', *, *, #215551, .T. ) ;
#92674 = DIRECTION ( 'NONE',  ( 1.000000000000000000, -0.000000000000000000, -0.000000000000000000 ) ) ;
#92675 = AXIS2_PLACEMENT_3D ( 'NONE', #152022, #92012, #251077 ) ;
#92676 = AXIS2_PLACEMENT_3D ( 'NONE', #74788, #154334, #254637 ) ;
#92677 = FACE_OUTER_BOUND ( 'NONE', #104656, .T. ) ;
#92678 = AXIS2_PLACEMENT_3D ( 'NONE', #78796, #236596, #256106 ) ;
#92679 = CARTESIAN_POINT ( 'NONE',  ( 21.05000000000000071, 8.926614585098249677, -142.4716830192231214 ) ) ;
#92680 = ORIENTED_EDGE ( 'NONE', *, *, #74636, .F. ) ;
#92681 = DIRECTION ( 'NONE',  ( 0.000000000000000000, 0.000000000000000000, 1.000000000000000000 ) ) ;
#92682 = CARTESIAN_POINT ( 'NONE',  ( -21.37071067811865532, 8.070710678118656389, -12.25000000000000000 ) ) ;
#92683 = DIRECTION ( 'NONE',  ( 1.000000000000000000, 0.000000000000000000, 0.000000000000000000 ) ) ;
#92684 = CARTESIAN_POINT ( 'NONE',  ( 18.59999999999999076, 6.450000000011156587, -155.2500000000000284 ) ) ;
#92685 = DIRECTION ( 'NONE',  ( 0.000000000000000000, -0.9770955615653259541, -0.2128009952263860971 ) ) ;
#92687 = DIRECTION ( 'NONE',  ( -1.000000000000000000, -0.000000000000000000, -0.000000000000000000 ) ) ;
#92686 = DIRECTION ( 'NONE',  ( -0.000000000000000000, -0.000000000000000000, 1.000000000000000000 ) ) ;
#92688 = CARTESIAN_POINT ( 'NONE',  ( -16.87401514999228169, 66.05000000001224691, -149.2430894919923219 ) ) ;
#92689 = ORIENTED_EDGE ( 'NONE', *, *, #93137, .T. ) ;
#92690 = AXIS2_PLACEMENT_3D ( 'NONE', #68517, #148052, #81009 ) ;
#92692 = CARTESIAN_POINT ( 'NONE',  ( -20.85000000000000142, 77.83585931145546510, -91.41866831572575336 ) ) ;
#92691 = SPHERICAL_SURFACE ( 'NONE', #124295, 0.1000000000000000056 ) ;
#92693 = ORIENTED_EDGE ( 'NONE', *, *, #173421, .T. ) ;
#92695 = ORIENTED_EDGE ( 'NONE', *, *, #157097, .T. ) ;
#92694 = DIRECTION ( 'NONE',  ( 1.000000000000000000, 0.000000000000000000, 0.000000000000000000 ) ) ;
#92696 = ORIENTED_EDGE ( 'NONE', *, *, #164989, .F. ) ;
#92697 = DIRECTION ( 'NONE',  ( 0.000000000000000000, 0.000000000000000000, 1.000000000000000000 ) ) ;
#92698 = CARTESIAN_POINT ( 'NONE',  ( 21.05000000000000071, 1.162701749938009677, -7.900000000000000355 ) ) ;
#92699 = CYLINDRICAL_SURFACE ( 'NONE', #47499, 0.1000000000000028644 ) ;
#92700 = CARTESIAN_POINT ( 'NONE',  ( 18.59999999999997655, 67.23127455305835554, -235.8551265064784559 ) ) ;
#92701 = AXIS2_PLACEMENT_3D ( 'NONE', #147506, #130500, #9276 ) ;
#92702 = EDGE_LOOP ( 'NONE', ( #74803, #24628, #140882, #6234 ) ) ;
#92703 = DIRECTION ( 'NONE',  ( 0.000000000000000000, -0.2128009952263678062, 0.9770955615653298398 ) ) ;
#92704 = VERTEX_POINT ( 'NONE', #224588 ) ;
#92705 = CARTESIAN_POINT ( 'NONE',  ( 13.40000000000005898, 67.72071067812984779, -24.99381816264344636 ) ) ;
#92706 = ADVANCED_FACE ( 'NONE', ( #68093 ), #123294, .T. ) ;
#92707 = DIRECTION ( 'NONE',  ( 0.000000000000000000, -0.1905202255954249191, -0.9816832705303010220 ) ) ;
#92708 = EDGE_LOOP ( 'NONE', ( #216522, #71145, #56302, #227456 ) ) ;
#92709 = EDGE_CURVE ( 'NONE', #143764, #127078, #140207, .T. ) ;
#92710 = DIRECTION ( 'NONE',  ( 0.000000000000000000, 1.000000000000000000, 6.982962677686266711E-15 ) ) ;
#92711 = AXIS2_PLACEMENT_3D ( 'NONE', #105796, #22465, #240220 ) ;
#92712 = ORIENTED_EDGE ( 'NONE', *, *, #140603, .F. ) ;
#92713 = DIRECTION ( 'NONE',  ( 1.000000000000000000, -0.000000000000000000, -0.000000000000000000 ) ) ;
#92714 = ORIENTED_EDGE ( 'NONE', *, *, #158180, .F. ) ;
#92715 = CARTESIAN_POINT ( 'NONE',  ( -22.50485643085238863, 76.07878633908967458, -181.7729024236968485 ) ) ;
#92716 = EDGE_CURVE ( 'NONE', #6281, #84436, #15163, .T. ) ;
#92717 = EDGE_CURVE ( 'NONE', #188088, #144636, #238494, .T. ) ;
#92718 = CARTESIAN_POINT ( 'NONE',  ( 18.49999999999999289, 34.58225676390223668, -235.1091250528070589 ) ) ;
#92719 = DIRECTION ( 'NONE',  ( 0.000000000000000000, 0.000000000000000000, -1.000000000000000000 ) ) ;
#92720 = CARTESIAN_POINT ( 'NONE',  ( -18.59999999999999787, 74.83729825007360148, -61.42310748452432989 ) ) ;
#92722 = CIRCLE ( 'NONE', #163653, 0.09999999999999609201 ) ;
#92721 = SPHERICAL_SURFACE ( 'NONE', #4601, 0.1000000000000000056 ) ;
#92723 = CARTESIAN_POINT ( 'NONE',  ( 18.59999996954842771, -9.523204137847617545, -73.88304171191651903 ) ) ;
#92724 = LINE ( 'NONE', #109717, #97212 ) ;
#92725 = ORIENTED_EDGE ( 'NONE', *, *, #15246, .T. ) ;
#92726 = DIRECTION ( 'NONE',  ( -1.000000000000000000, -0.000000000000000000, 0.000000000000000000 ) ) ;
#92728 = ORIENTED_EDGE ( 'NONE', *, *, #256443, .T. ) ;
#92727 = AXIS2_PLACEMENT_3D ( 'NONE', #154970, #237046, #59658 ) ;
#92731 = ORIENTED_EDGE ( 'NONE', *, *, #108872, .T. ) ;
#92730 = DIRECTION ( 'NONE',  ( 5.603264701231745086E-32, -1.897661533703520636E-16, 1.000000000000000000 ) ) ;
#92729 = CARTESIAN_POINT ( 'NONE',  ( -21.05000000000000071, 64.40000000001219860, -143.4513107147999449 ) ) ;
#92732 = EDGE_CURVE ( 'NONE', #106161, #155283, #144299, .T. ) ;
#92733 = ORIENTED_EDGE ( 'NONE', *, *, #156511, .T. ) ;
#92734 = CARTESIAN_POINT ( 'NONE',  ( -22.94999999999999929, 11.49641995933507843, -1.885425182446134107 ) ) ;
#92735 = EDGE_CURVE ( 'NONE', #33939, #215029, #177696, .T. ) ;
#92736 = CARTESIAN_POINT ( 'NONE',  ( -21.07928932188134041, 6.328516656393293083, 0.09889514565439641580 ) ) ;
#92737 = FACE_OUTER_BOUND ( 'NONE', #233258, .T. ) ;
#92738 = CARTESIAN_POINT ( 'NONE',  ( 20.95545211741311320, 58.99965432765223028, -225.7624460179877417 ) ) ;
#92740 = VERTEX_POINT ( 'NONE', #2434 ) ;
#92739 =( BOUNDED_SURFACE ( )  B_SPLINE_SURFACE ( 3, 2, ( 
 ( #151930, #209299, #54078 ),
 ( #31980, #232741, #230152 ),
 ( #189745, #51484, #153221 ),
 ( #52784, #93202, #172796 ) ),
 .UNSPECIFIED., .F., .F., .F. ) 
 B_SPLINE_SURFACE_WITH_KNOTS ( ( 4, 4 ),
 ( 3, 3 ),
 ( 5.727910411845712702, 5.983100554402349225 ),
 ( 0.000000000000000000, 1.000000000000000000 ),
 .UNSPECIFIED. ) 
 GEOMETRIC_REPRESENTATION_ITEM ( )  RATIONAL_B_SPLINE_SURFACE ( (
 ( 1.000000000000000000, 0.8946697475932183785, 1.000000000000000000),
 ( 1.000000000000000000, 0.9035312726220551260, 1.000000000000000000),
 ( 1.000000000000000000, 0.9104333467450264061, 1.000000000000000000),
 ( 1.000000000000000000, 0.9152888060719349683, 1.000000000000000000) ) ) 
 REPRESENTATION_ITEM ( '' )  SURFACE ( )  );
#92742 = ORIENTED_EDGE ( 'NONE', *, *, #216837, .T. ) ;
#92741 = CYLINDRICAL_SURFACE ( 'NONE', #76280, 0.09999999999998898659 ) ;
#92744 = CARTESIAN_POINT ( 'NONE',  ( 18.49999999999999289, 15.51794587355511723, -222.9505302427970719 ) ) ;
#92743 = DIRECTION ( 'NONE',  ( 0.000000000000000000, -0.4721928772777346239, -0.8814952561688430555 ) ) ;
#92746 = ORIENTED_EDGE ( 'NONE', *, *, #143887, .T. ) ;
#92745 = CARTESIAN_POINT ( 'NONE',  ( 23.14999999999999858, 76.00000000001192291, -105.0231074845243029 ) ) ;
#92747 = CIRCLE ( 'NONE', #180252, 4.099999999999996980 ) ;
#92748 = VECTOR ( 'NONE', #244788, 1000.000000000000000 ) ;
#92749 = EDGE_CURVE ( 'NONE', #193752, #241011, #215071, .T. ) ;
#92750 = ORIENTED_EDGE ( 'NONE', *, *, #75017, .F. ) ;
#92751 = EDGE_CURVE ( 'NONE', #214401, #154034, #248388, .T. ) ;
#92752 = CARTESIAN_POINT ( 'NONE',  ( 22.48660254037843842, 11.75000000001115730, -167.4499999999999318 ) ) ;
#92753 = CARTESIAN_POINT ( 'NONE',  ( 23.14999999999999858, 71.00000000001253397, -181.9283735034374843 ) ) ;
#92754 = ORIENTED_EDGE ( 'NONE', *, *, #75555, .T. ) ;
#92755 = CARTESIAN_POINT ( 'NONE',  ( 20.73486653747088937, 9.540899807986670922, -208.3889262314765460 ) ) ;
#92756 = ORIENTED_EDGE ( 'NONE', *, *, #162043, .T. ) ;
#92757 = CIRCLE ( 'NONE', #255007, 0.1000000000000002554 ) ;
#92758 = DIRECTION ( 'NONE',  ( 1.000000000000000000, -1.335000415235278971E-16, 2.979993593738921214E-16 ) ) ;
#92759 = DIRECTION ( 'NONE',  ( 1.000000000000000000, 0.000000000000000000, 0.000000000000000000 ) ) ;
#92760 = ORIENTED_EDGE ( 'NONE', *, *, #57080, .F. ) ;
#92761 = ADVANCED_FACE ( 'NONE', ( #141955 ), #6957, .T. ) ;
#92762 = CARTESIAN_POINT ( 'NONE',  ( 20.94999999999999929, 28.08470566095357057, -239.2860081655328770 ) ) ;
#92763 = VECTOR ( 'NONE', #94740, 1000.000000000000000 ) ;
#92764 = VECTOR ( 'NONE', #135376, 1000.000000000000000 ) ;
#92765 = AXIS2_PLACEMENT_3D ( 'NONE', #112262, #152686, #50958 ) ;
#92766 = EDGE_CURVE ( 'NONE', #102756, #195402, #152745, .T. ) ;
#92767 = AXIS2_PLACEMENT_3D ( 'NONE', #71167, #230218, #169008 ) ;
#92768 = EDGE_CURVE ( 'NONE', #11889, #171420, #7125, .T. ) ;
#92769 = DIRECTION ( 'NONE',  ( -0.000000000000000000, -0.000000000000000000, 1.000000000000000000 ) ) ;
#92770 = EDGE_CURVE ( 'NONE', #37719, #45489, #140676, .T. ) ;
#92771 = ORIENTED_EDGE ( 'NONE', *, *, #173940, .F. ) ;
#92772 = ORIENTED_EDGE ( 'NONE', *, *, #53225, .F. ) ;
#92773 = CARTESIAN_POINT ( 'NONE',  ( 20.74897398619101807, 18.90132073407816904, -228.0187643500604793 ) ) ;
#92774 = EDGE_LOOP ( 'NONE', ( #211514, #33596, #177494, #99226 ) ) ;
#92775 = CARTESIAN_POINT ( 'NONE',  ( 23.24999999999999289, 64.35000000001245724, -181.7731074845244450 ) ) ;
#92776 = ORIENTED_EDGE ( 'NONE', *, *, #237721, .T. ) ;
#92778 = VERTEX_POINT ( 'NONE', #216359 ) ;
#92777 = CARTESIAN_POINT ( 'NONE',  ( 21.05000000000000071, 1.115600667400684642E-11, -100.5000000000000284 ) ) ;
#92779 = EDGE_CURVE ( 'NONE', #75515, #171571, #101512, .T. ) ;
#92780 = VERTEX_POINT ( 'NONE', #78123 ) ;
#92781 = DIRECTION ( 'NONE',  ( 0.000000000000000000, 0.000000000000000000, 1.000000000000000000 ) ) ;
#92782 = ORIENTED_EDGE ( 'NONE', *, *, #82966, .F. ) ;
#92785 = VERTEX_POINT ( 'NONE', #117274 ) ;
#92784 = VERTEX_POINT ( 'NONE', #237221 ) ;
#92783 = CARTESIAN_POINT ( 'NONE',  ( -16.93440969289731157, 66.00481482419762358, -56.93187329951360454 ) ) ;
#92786 = EDGE_CURVE ( 'NONE', #228810, #67500, #15363, .T. ) ;
#92787 = AXIS2_PLACEMENT_3D ( 'NONE', #1627, #238984, #40805 ) ;
#92788 = ORIENTED_EDGE ( 'NONE', *, *, #208856, .F. ) ;
#92789 = CARTESIAN_POINT ( 'NONE',  ( 21.09706851349341861, 8.775842513484549912, -45.73556621639964703 ) ) ;
#92790 = ORIENTED_EDGE ( 'NONE', *, *, #138136, .F. ) ;
#92791 = FACE_OUTER_BOUND ( 'NONE', #94293, .T. ) ;
#92792 = EDGE_CURVE ( 'NONE', #97347, #187076, #244460, .T. ) ;
#92793 = CIRCLE ( 'NONE', #134478, 0.09999999999999939493 ) ;
#92795 = ORIENTED_EDGE ( 'NONE', *, *, #82361, .T. ) ;
#92794 = PLANE ( 'NONE',  #207532 ) ;
#92796 = DIRECTION ( 'NONE',  ( 0.000000000000000000, -6.417474130781252121E-15, 1.000000000000000000 ) ) ;
#92797 = ORIENTED_EDGE ( 'NONE', *, *, #245146, .T. ) ;
#92798 =( BOUNDED_CURVE ( )  B_SPLINE_CURVE ( 3, ( #71646, #192870, #151176, #230715 ),
 .UNSPECIFIED., .F., .F. ) 
 B_SPLINE_CURVE_WITH_KNOTS ( ( 4, 4 ),
 ( 5.731445031868798168, 5.983100554402349225 ),
 .UNSPECIFIED. ) 
 CURVE ( )  GEOMETRIC_REPRESENTATION_ITEM ( )  RATIONAL_B_SPLINE_CURVE ( ( 1.000000000000000000, 0.9947294176030464508, 0.9947294176030464508, 1.000000000000000000 ) ) 
 REPRESENTATION_ITEM ( '' )  );
#92799 = VECTOR ( 'NONE', #87481, 1000.000000000000000 ) ;
#92800 = ORIENTED_EDGE ( 'NONE', *, *, #33865, .F. ) ;
#92801 = DIRECTION ( 'NONE',  ( -0.000000000000000000, -0.000000000000000000, 1.000000000000000000 ) ) ;
#92802 = CARTESIAN_POINT ( 'NONE',  ( 18.58222699835054570, 18.41441690808118992, -236.9991004306322964 ) ) ;
#92803 = AXIS2_PLACEMENT_3D ( 'NONE', #240628, #162392, #183231 ) ;
#92804 = VECTOR ( 'NONE', #169512, 1000.000000000000114 ) ;
#92806 = ORIENTED_EDGE ( 'NONE', *, *, #40552, .F. ) ;
#92805 = AXIS2_PLACEMENT_3D ( 'NONE', #200609, #201892, #237176 ) ;
#92808 = ORIENTED_EDGE ( 'NONE', *, *, #233453, .T. ) ;
#92807 = CARTESIAN_POINT ( 'NONE',  ( -22.45354308602430748, 75.99999978013465807, -148.2735403749860836 ) ) ;
#92809 = LINE ( 'NONE', #32894, #152574 ) ;
#92810 = CIRCLE ( 'NONE', #71989, 0.2000000000000057288 ) ;
#92812 = VERTEX_POINT ( 'NONE', #18165 ) ;
#92811 = ORIENTED_EDGE ( 'NONE', *, *, #166741, .F. ) ;
#92813 = ORIENTED_EDGE ( 'NONE', *, *, #132410, .F. ) ;
#92814 = DIRECTION ( 'NONE',  ( 0.000000000000000000, -0.2617529984165032908, -0.9651348961777156399 ) ) ;
#92815 = ORIENTED_EDGE ( 'NONE', *, *, #215549, .F. ) ;
#92816 = EDGE_LOOP ( 'NONE', ( #221059, #129050, #137602, #3846 ) ) ;
#92817 = CARTESIAN_POINT ( 'NONE',  ( 20.95346350065193519, 18.82834646935051026, -229.9178759252477278 ) ) ;
#92818 = VERTEX_POINT ( 'NONE', #19458 ) ;
#92819 = DIRECTION ( 'NONE',  ( 0.000000000000000000, 0.8814952561688438326, -0.4721928772777331806 ) ) ;
#92820 = AXIS2_PLACEMENT_3D ( 'NONE', #34559, #154527, #119225 ) ;
#92821 = CARTESIAN_POINT ( 'NONE',  ( 23.14999999999999858, 71.00000000001223555, -148.4283735034374843 ) ) ;
#92823 = ORIENTED_EDGE ( 'NONE', *, *, #242690, .F. ) ;
#92822 = TOROIDAL_SURFACE ( 'NONE', #63604, 7.800000000000000711, 0.1000000000000000056 ) ;
#92824 = ORIENTED_EDGE ( 'NONE', *, *, #76075, .T. ) ;
#92825 = VECTOR ( 'NONE', #238060, 1000.000000000000000 ) ;
#92826 = CARTESIAN_POINT ( 'NONE',  ( -18.59999999999999787, 76.00000000001165290, -61.62310748452430431 ) ) ;
#92827 = EDGE_LOOP ( 'NONE', ( #64072, #118136, #139787, #35117 ) ) ;
#92828 = VECTOR ( 'NONE', #230721, 1000.000000000000000 ) ;
#92830 =( BOUNDED_CURVE ( )  B_SPLINE_CURVE ( 3, ( #91436, #229659, #9321, #50985 ),
 .UNSPECIFIED., .F., .F. ) 
 B_SPLINE_CURVE_WITH_KNOTS ( ( 4, 4 ),
 ( 0.3000847527772381729, 0.5497968875596822569 ),
 .UNSPECIFIED. ) 
 CURVE ( )  GEOMETRIC_REPRESENTATION_ITEM ( )  RATIONAL_B_SPLINE_CURVE ( ( 1.000000000000000000, 0.9948104011409419911, 0.9948104011409419911, 1.000000000000000000 ) ) 
 REPRESENTATION_ITEM ( '' )  );
#92829 = VECTOR ( 'NONE', #123127, 1000.000000000000114 ) ;
#92831 = AXIS2_PLACEMENT_3D ( 'NONE', #251828, #194453, #94030 ) ;
#92832 = AXIS2_PLACEMENT_3D ( 'NONE', #171253, #68255, #66962 ) ;
#92833 = DIRECTION ( 'NONE',  ( 0.000000000000000000, 0.000000000000000000, -1.000000000000000000 ) ) ;
#92834 = VERTEX_POINT ( 'NONE', #97674 ) ;
#92835 = ORIENTED_EDGE ( 'NONE', *, *, #111619, .T. ) ;
#92836 = DIRECTION ( 'NONE',  ( 0.000000000000000000, 0.000000000000000000, -1.000000000000000000 ) ) ;
#92837 = EDGE_CURVE ( 'NONE', #64487, #249408, #86232, .T. ) ;
#92839 = ORIENTED_EDGE ( 'NONE', *, *, #171940, .T. ) ;
#92838 = CARTESIAN_POINT ( 'NONE',  ( -16.94226253665224746, 9.950000000011137047, -121.0532654043842768 ) ) ;
#92840 = DIRECTION ( 'NONE',  ( 1.000000000000000000, 0.000000000000000000, 0.000000000000000000 ) ) ;
#92841 = CARTESIAN_POINT ( 'NONE',  ( -20.94999999999999929, 1.115600667400684642E-11, -134.0000000000000284 ) ) ;
#92842 = CARTESIAN_POINT ( 'NONE',  ( 20.95568717954149562, 65.39800594612027851, -128.9205991162557154 ) ) ;
#92843 = CARTESIAN_POINT ( 'NONE',  ( 18.59999999999999076, 33.89981536720674171, -236.1713368690715527 ) ) ;
#92844 = CARTESIAN_POINT ( 'NONE',  ( 21.05000000000000071, 5.400000000011154988, -155.0947339810869323 ) ) ;
#92845 = CARTESIAN_POINT ( 'NONE',  ( 19.90000000000000568, 1.250000000000000000, 16.50000000000000000 ) ) ;
#92846 = EDGE_CURVE ( 'NONE', #41514, #176240, #241087, .T. ) ;
#92847 = DIRECTION ( 'NONE',  ( 1.000000000000000000, 0.000000000000000000, 0.000000000000000000 ) ) ;
#92849 = ADVANCED_FACE ( 'NONE', ( #157727 ), #98952, .T. ) ;
#92848 = FACE_OUTER_BOUND ( 'NONE', #79653, .T. ) ;
#92850 = CARTESIAN_POINT ( 'NONE',  ( 18.59999996954842771, 38.22950387605726519, -261.1959452426659141 ) ) ;
#92851 = CARTESIAN_POINT ( 'NONE',  ( 18.39999999999999858, -9.519327731081283162, -73.97297637655937308 ) ) ;
#92852 = FACE_OUTER_BOUND ( 'NONE', #163448, .T. ) ;
#92853 = AXIS2_PLACEMENT_3D ( 'NONE', #112027, #96276, #74209 ) ;
#92855 = VERTEX_POINT ( 'NONE', #119861 ) ;
#92854 = CIRCLE ( 'NONE', #80353, 0.09999999999999982514 ) ;
#92856 = CIRCLE ( 'NONE', #201194, 0.3999999999999975797 ) ;
#92858 = ORIENTED_EDGE ( 'NONE', *, *, #253602, .F. ) ;
#92857 = ORIENTED_EDGE ( 'NONE', *, *, #201979, .F. ) ;
#92859 = VERTEX_POINT ( 'NONE', #20753 ) ;
#92860 = EDGE_CURVE ( 'NONE', #165636, #224344, #152931, .T. ) ;
#92861 = CARTESIAN_POINT ( 'NONE',  ( -21.44999999999999929, 68.65000000001199965, -115.2731074845243455 ) ) ;
#92862 = DIRECTION ( 'NONE',  ( -2.602085213965226419E-14, -6.982962677686266711E-15, 1.000000000000000000 ) ) ;
#92864 = DIRECTION ( 'NONE',  ( 0.000000000000000000, 0.000000000000000000, -1.000000000000000000 ) ) ;
#92863 = CARTESIAN_POINT ( 'NONE',  ( 21.14999999999999858, 8.786607556611267356, -79.25000000000004263 ) ) ;
#92865 = ORIENTED_EDGE ( 'NONE', *, *, #134649, .F. ) ;
#92866 = ORIENTED_EDGE ( 'NONE', *, *, #50047, .T. ) ;
#92867 = FACE_OUTER_BOUND ( 'NONE', #72266, .T. ) ;
#92868 = CARTESIAN_POINT ( 'NONE',  ( 19.97071067811864609, 11.72071067812981404, -58.25000000000000000 ) ) ;
#92869 = DIRECTION ( 'NONE',  ( 0.000000000000000000, 0.2617529984165033463, 0.9651348961777156399 ) ) ;
#92870 = ORIENTED_EDGE ( 'NONE', *, *, #132173, .T. ) ;
#92871 = VERTEX_POINT ( 'NONE', #84505 ) ;
#92872 = CARTESIAN_POINT ( 'NONE',  ( -18.79999999999999716, 5.488301202077016328, 16.39999999999999858 ) ) ;
#92873 = CARTESIAN_POINT ( 'NONE',  ( -23.15000000000000213, 64.25000000001186606, -90.87310748452438247 ) ) ;
#92874 = AXIS2_PLACEMENT_3D ( 'NONE', #9626, #212969, #70924 ) ;
#92875 = EDGE_CURVE ( 'NONE', #121457, #143803, #52926, .T. ) ;
#92876 = CARTESIAN_POINT ( 'NONE',  ( -18.59999999999999787, 77.13501884592258762, -162.3061306010920362 ) ) ;
#92878 = EDGE_LOOP ( 'NONE', ( #183151, #64604, #202340 ) ) ;
#92877 = DIRECTION ( 'NONE',  ( 1.000000000000000000, 0.000000000000000000, 0.000000000000000000 ) ) ;
#92879 = EDGE_CURVE ( 'NONE', #74786, #78774, #69525, .T. ) ;
#92880 = CARTESIAN_POINT ( 'NONE',  ( -21.05000000000000071, 12.71802988599559114, -223.5105008658000543 ) ) ;
#92881 = DIRECTION ( 'NONE',  ( 0.000000000000000000, -6.982962677686266711E-15, 1.000000000000000000 ) ) ;
#92882 = DIRECTION ( 'NONE',  ( 0.000000000000000000, 6.982962677686267499E-15, -1.000000000000000000 ) ) ;
#92883 = VERTEX_POINT ( 'NONE', #144511 ) ;
#92884 = CARTESIAN_POINT ( 'NONE',  ( -20.64999999999999858, 68.85000000001259934, -191.1731074845243938 ) ) ;
#92885 = SPHERICAL_SURFACE ( 'NONE', #110084, 0.1000000000000000056 ) ;
#92886 = CARTESIAN_POINT ( 'NONE',  ( -20.64999999999999858, 7.250000000011155521, -45.75000000000000000 ) ) ;
#92888 = DIRECTION ( 'NONE',  ( 1.000000000000000000, -2.849773892568378313E-16, 7.728835255496647986E-17 ) ) ;
#92887 = CARTESIAN_POINT ( 'NONE',  ( -20.54999999999999716, -9.499999999988846255, -57.10603087734755690 ) ) ;
#92889 = DIRECTION ( 'NONE',  ( 0.000000000000000000, 0.000000000000000000, 1.000000000000000000 ) ) ;
#92890 = DIRECTION ( 'NONE',  ( 0.000000000000000000, -0.9910827722268036322, 0.1332476588733685074 ) ) ;
#92891 = EDGE_CURVE ( 'NONE', #49571, #36105, #202770, .T. ) ;
#92892 = DIRECTION ( 'NONE',  ( -0.7071067811865474617, 0.7071067811865474617, 5.142139384388980375E-15 ) ) ;
#92893 = DIRECTION ( 'NONE',  ( -0.7071067811865475727, 0.7071067811865475727, 4.937700262164531476E-15 ) ) ;
#92894 = DIRECTION ( 'NONE',  ( 1.000000000000000000, 0.000000000000000000, 0.000000000000000000 ) ) ;
#92895 = ORIENTED_EDGE ( 'NONE', *, *, #67308, .T. ) ;
#92896 = AXIS2_PLACEMENT_3D ( 'NONE', #221895, #244040, #100655 ) ;
#92897 = ORIENTED_EDGE ( 'NONE', *, *, #243016, .F. ) ;
#92898 = ORIENTED_EDGE ( 'NONE', *, *, #181862, .F. ) ;
#92899 = FACE_OUTER_BOUND ( 'NONE', #205357, .T. ) ;
#92900 = DIRECTION ( 'NONE',  ( 0.000000000000000000, 0.000000000000000000, 1.000000000000000000 ) ) ;
#92901 = ORIENTED_EDGE ( 'NONE', *, *, #4202, .F. ) ;
#92902 = DIRECTION ( 'NONE',  ( 1.000000000000000000, -0.000000000000000000, 0.000000000000000000 ) ) ;
#92904 = EDGE_CURVE ( 'NONE', #235552, #157226, #184939, .T. ) ;
#92903 = EDGE_LOOP ( 'NONE', ( #38274, #164760, #222308, #139540, #194782 ) ) ;
#92905 = VECTOR ( 'NONE', #231234, 1000.000000000000000 ) ;
#92906 = VERTEX_POINT ( 'NONE', #225325 ) ;
#92907 = CARTESIAN_POINT ( 'NONE',  ( 21.05000000000000071, 76.01454569058293487, -109.5201252709567541 ) ) ;
#92908 = ORIENTED_EDGE ( 'NONE', *, *, #118778, .T. ) ;
#92909 = AXIS2_PLACEMENT_3D ( 'NONE', #80189, #239308, #138874 ) ;
#92910 = CARTESIAN_POINT ( 'NONE',  ( 18.60000000000001208, -7.621788160715480487, -210.0085134484000946 ) ) ;
#92911 = CARTESIAN_POINT ( 'NONE',  ( -16.78493211734302903, 30.19206623356038222, -234.8041291499450836 ) ) ;
#92912 = DIRECTION ( 'NONE',  ( -2.978066053179067751E-16, 1.000000000000000000, 0.000000000000000000 ) ) ;
#92913 = VECTOR ( 'NONE', #114601, 1000.000000000000114 ) ;
#92914 = EDGE_CURVE ( 'NONE', #31301, #173746, #123695, .T. ) ;
#92915 = CARTESIAN_POINT ( 'NONE',  ( -22.39999999999999858, 7.790779598384560245, -67.00000000000004263 ) ) ;
#92916 = DIRECTION ( 'NONE',  ( 0.000000000000000000, -0.1298341882520124002, -0.9915357197604841577 ) ) ;
#92918 = ORIENTED_EDGE ( 'NONE', *, *, #194473, .T. ) ;
#92917 = DIRECTION ( 'NONE',  ( 0.000000000000000000, 0.4999999999999608646, 0.8660254037844612451 ) ) ;
#92920 = DIRECTION ( 'NONE',  ( 1.000000000000000000, 0.000000000000000000, 0.000000000000000000 ) ) ;
#92919 = CARTESIAN_POINT ( 'NONE',  ( 21.05000000000000071, 6.390846877240204726, -199.6081416912452653 ) ) ;
#92921 = CARTESIAN_POINT ( 'NONE',  ( 20.95512820512820440, 10.62384868371188062, -7.664913569087605794 ) ) ;
#92922 = DIRECTION ( 'NONE',  ( -1.000000000000000000, 0.000000000000000000, -0.000000000000000000 ) ) ;
#92923 = DIRECTION ( 'NONE',  ( 1.000000000000000000, 0.000000000000000000, 0.000000000000000000 ) ) ;
#92925 = ADVANCED_FACE ( 'NONE', ( #204488 ), #85799, .F. ) ;
#92924 = DIRECTION ( 'NONE',  ( 1.000000000000000000, 0.000000000000000000, 0.000000000000000000 ) ) ;
#92926 = ADVANCED_FACE ( 'NONE', ( #207079 ), #144496, .T. ) ;
#92927 = VERTEX_POINT ( 'NONE', #222768 ) ;
#92928 = VECTOR ( 'NONE', #203188, 1000.000000000000000 ) ;
#92930 = CYLINDRICAL_SURFACE ( 'NONE', #150215, 0.1000000000000028644 ) ;
#92929 = AXIS2_PLACEMENT_3D ( 'NONE', #245489, #48554, #188075 ) ;
#92931 = VECTOR ( 'NONE', #140125, 1000.000000000000000 ) ;
#92932 = ORIENTED_EDGE ( 'NONE', *, *, #126776, .F. ) ;
#92933 = DIRECTION ( 'NONE',  ( 0.000000000000000000, 0.4721928772776164407, 0.8814952561689062271 ) ) ;
#92934 = ORIENTED_EDGE ( 'NONE', *, *, #180379, .T. ) ;
#92935 = ADVANCED_FACE ( 'NONE', ( #27189 ), #198679, .T. ) ;
#92936 = DIRECTION ( 'NONE',  ( -0.000000000000000000, 6.982962677686266711E-15, -1.000000000000000000 ) ) ;
#92937 = EDGE_CURVE ( 'NONE', #62775, #76541, #187533, .T. ) ;
#92938 = CIRCLE ( 'NONE', #176183, 0.9750000000000036415 ) ;
#92939 = CARTESIAN_POINT ( 'NONE',  ( 23.14999999999999858, 78.10000000001190301, -103.0231074845242887 ) ) ;
#92940 = DIRECTION ( 'NONE',  ( 0.000000000000000000, 0.2617529984165152257, 0.9651348961777124202 ) ) ;
#92941 = ORIENTED_EDGE ( 'NONE', *, *, #125791, .F. ) ;
#92942 = EDGE_CURVE ( 'NONE', #123636, #136369, #240217, .T. ) ;
#92943 = VERTEX_POINT ( 'NONE', #44159 ) ;
#92944 = CIRCLE ( 'NONE', #97002, 0.1000000000000028644 ) ;
#92945 = AXIS2_PLACEMENT_3D ( 'NONE', #101031, #219743, #188025 ) ;
#92946 = CIRCLE ( 'NONE', #72125, 7.900000000000003908 ) ;
#92947 = TOROIDAL_SURFACE ( 'NONE', #63742, 3.899999999999999467, 0.1000000000000000056 ) ;
#92948 = FACE_OUTER_BOUND ( 'NONE', #164277, .T. ) ;
#92949 = CARTESIAN_POINT ( 'NONE',  ( 18.59999999999999076, 4.273531877263399892, -211.9976340888692050 ) ) ;
#92950 = EDGE_CURVE ( 'NONE', #23326, #167954, #107101, .T. ) ;
#92951 = CARTESIAN_POINT ( 'NONE',  ( 20.89878130938411616, 65.67252876774583115, -164.4457041994994881 ) ) ;
#92952 = LINE ( 'NONE', #154267, #2913 ) ;
#92954 = CARTESIAN_POINT ( 'NONE',  ( -20.85000000000000142, 67.23127455305835554, -235.8551265064784559 ) ) ;
#92953 = DIRECTION ( 'NONE',  ( -1.000000000000000000, 0.000000000000000000, 1.073024830501117725E-15 ) ) ;
#92955 = LINE ( 'NONE', #192083, #28466 ) ;
#92957 = ADVANCED_FACE ( 'NONE', ( #4992 ), #68864, .T. ) ;
#92956 = CARTESIAN_POINT ( 'NONE',  ( 21.09551895715278746, 65.37856267284385581, -90.78598281862467445 ) ) ;
#92959 = EDGE_CURVE ( 'NONE', #26113, #83024, #128830, .T. ) ;
#92958 = FACE_OUTER_BOUND ( 'NONE', #23153, .T. ) ;
#92960 = ORIENTED_EDGE ( 'NONE', *, *, #31554, .F. ) ;
#92961 = PLANE ( 'NONE',  #185454 ) ;
#92963 = ORIENTED_EDGE ( 'NONE', *, *, #120412, .F. ) ;
#92962 = DIRECTION ( 'NONE',  ( 0.000000000000000000, 0.8814952561688429444, -0.4721928772777349570 ) ) ;
#92964 = CARTESIAN_POINT ( 'NONE',  ( 17.23472005113826810, 10.30788195451192202, -189.5465768600686545 ) ) ;
#92965 = CARTESIAN_POINT ( 'NONE',  ( -21.64999999999999858, 11.68239342655420110, -220.1014838121945161 ) ) ;
#92967 = CARTESIAN_POINT ( 'NONE',  ( 18.59999999999999432, 74.83729825007462466, -195.4231074845243654 ) ) ;
#92966 = CARTESIAN_POINT ( 'NONE',  ( -21.65000000000000213, 7.708578643773852157, -121.6500000000000341 ) ) ;
#92968 = ADVANCED_FACE ( 'NONE', ( #165386 ), #46699, .T. ) ;
#92969 = CARTESIAN_POINT ( 'NONE',  ( 20.05000000000002913, 7.250000000011171508, -176.7499999999999716 ) ) ;
#92971 = ORIENTED_EDGE ( 'NONE', *, *, #170808, .T. ) ;
#92970 = DIRECTION ( 'NONE',  ( 0.000000000000000000, -1.000000000000000000, 0.000000000000000000 ) ) ;
#92972 = CARTESIAN_POINT ( 'NONE',  ( 18.49999999999999645, 1.736257131608553550, -45.06865232901750318 ) ) ;
#92973 = FACE_OUTER_BOUND ( 'NONE', #185524, .T. ) ;
#92974 = CARTESIAN_POINT ( 'NONE',  ( 20.94999999999999574, 87.65000000001163016, -66.62310748452424036 ) ) ;
#92975 = CARTESIAN_POINT ( 'NONE',  ( 21.05000000000000426, 65.27628289530478867, -162.4286900929113528 ) ) ;
#92976 = VERTEX_POINT ( 'NONE', #29754 ) ;
#92977 = DIRECTION ( 'NONE',  ( 0.000000000000000000, -0.4930308989875170078, -0.8700118002898356018 ) ) ;
#92978 = ADVANCED_FACE ( 'NONE', ( #145800 ), #252835, .T. ) ;
#92979 = VERTEX_POINT ( 'NONE', #164103 ) ;
#92980 = EDGE_CURVE ( 'NONE', #156438, #194512, #32112, .T. ) ;
#92981 = AXIS2_PLACEMENT_3D ( 'NONE', #147529, #144940, #146229 ) ;
#92982 = EDGE_CURVE ( 'NONE', #127120, #188642, #74018, .T. ) ;
#92983 = AXIS2_PLACEMENT_3D ( 'NONE', #39665, #61763, #119178 ) ;
#92984 = PLANE ( 'NONE',  #38425 ) ;
#92985 = ORIENTED_EDGE ( 'NONE', *, *, #133294, .F. ) ;
#92986 = CARTESIAN_POINT ( 'NONE',  ( -18.59999999999999787, 78.57213941646344324, -232.7862224702232652 ) ) ;
#92987 = ORIENTED_EDGE ( 'NONE', *, *, #227098, .T. ) ;
#92988 = CARTESIAN_POINT ( 'NONE',  ( 20.85000000000000142, 76.32388570108224712, -103.0655178952103199 ) ) ;
#92989 = FACE_OUTER_BOUND ( 'NONE', #39701, .T. ) ;
#92990 = AXIS2_PLACEMENT_3D ( 'NONE', #205352, #128408, #65857 ) ;
#92991 = AXIS2_PLACEMENT_3D ( 'NONE', #138370, #220515, #221755 ) ;
#92992 = DIRECTION ( 'NONE',  ( -1.000000000000000000, -0.000000000000000000, 0.000000000000000000 ) ) ;
#92993 = ORIENTED_EDGE ( 'NONE', *, *, #99944, .T. ) ;
#92994 = EDGE_CURVE ( 'NONE', #1028, #199629, #115290, .T. ) ;
#92995 = VECTOR ( 'NONE', #76607, 1000.000000000000000 ) ;
#92996 = CARTESIAN_POINT ( 'NONE',  ( -21.14999999999999858, 38.08698097766499302, -236.1457910985472779 ) ) ;
#92998 = AXIS2_PLACEMENT_3D ( 'NONE', #188664, #150824, #10030 ) ;
#92997 = DIRECTION ( 'NONE',  ( 0.000000000000000000, 0.9770955615653316162, 0.2128009952263597848 ) ) ;
#92999 = DIRECTION ( 'NONE',  ( 0.000000000000000000, 0.000000000000000000, 1.000000000000000000 ) ) ;
#93000 = AXIS2_PLACEMENT_3D ( 'NONE', #203798, #138658, #81262 ) ;
#93001 = CIRCLE ( 'NONE', #176417, 0.09999999999998898659 ) ;
#93002 = CARTESIAN_POINT ( 'NONE',  ( 13.43663047529819821, 9.446645344695243196, -18.41080645610018607 ) ) ;
#93003 = AXIS2_PLACEMENT_3D ( 'NONE', #37074, #175304, #194860 ) ;
#93004 = CARTESIAN_POINT ( 'NONE',  ( -16.90987985657661241, 66.04219248183227364, -115.6538203956407358 ) ) ;
#93005 = VERTEX_POINT ( 'NONE', #54411 ) ;
#93006 = CARTESIAN_POINT ( 'NONE',  ( -18.33981767444321065, 85.56957578981628387, -129.7039456407995033 ) ) ;
#93007 = ORIENTED_EDGE ( 'NONE', *, *, #119588, .F. ) ;
#93009 = ORIENTED_EDGE ( 'NONE', *, *, #41199, .T. ) ;
#93008 = DIRECTION ( 'NONE',  ( -5.603264701231743991E-32, -7.172728831056617961E-15, 1.000000000000000000 ) ) ;
#93010 = VECTOR ( 'NONE', #241580, 1000.000000000000000 ) ;
#93011 = EDGE_LOOP ( 'NONE', ( #238371, #134220, #108056, #38164 ) ) ;
#93012 = CARTESIAN_POINT ( 'NONE',  ( -23.25000000000000000, 7.783179459866048866, -245.3643104511423019 ) ) ;
#93013 = DIRECTION ( 'NONE',  ( 7.304098846218134667E-16, -1.000000000000000000, 0.000000000000000000 ) ) ;
#93014 = CARTESIAN_POINT ( 'NONE',  ( -20.94999999999999929, 5.850000000011160495, -190.8675027757220448 ) ) ;
#93015 = VERTEX_POINT ( 'NONE', #234326 ) ;
#93016 = PLANE ( 'NONE',  #84459 ) ;
#93018 = CARTESIAN_POINT ( 'NONE',  ( -20.64999999999999858, -8.663551401869156621, -23.97589888193269658 ) ) ;
#93017 = AXIS2_PLACEMENT_3D ( 'NONE', #94195, #156779, #18527 ) ;
#93019 = ORIENTED_EDGE ( 'NONE', *, *, #24298, .T. ) ;
#93020 = TOROIDAL_SURFACE ( 'NONE', #38866, 0.2000000000000000111, 0.1000000000000000056 ) ;
#93022 = ORIENTED_EDGE ( 'NONE', *, *, #245743, .F. ) ;
#93021 = CARTESIAN_POINT ( 'NONE',  ( 22.50000000000000000, 68.20922040163875977, -136.6231074845243540 ) ) ;
#93023 = DIRECTION ( 'NONE',  ( 0.000000000000000000, -0.8814952561688430555, 0.4721928772777346239 ) ) ;
#93024 = FACE_OUTER_BOUND ( 'NONE', #65900, .T. ) ;
#93025 = VECTOR ( 'NONE', #230737, 1000.000000000000000 ) ;
#93026 = ADVANCED_FACE ( 'NONE', ( #115677 ), #93535, .T. ) ;
#93027 = CARTESIAN_POINT ( 'NONE',  ( 20.95512820512820795, 44.16399506693049659, -236.4628398677790813 ) ) ;
#93028 = ORIENTED_EDGE ( 'NONE', *, *, #174750, .F. ) ;
#93029 = EDGE_CURVE ( 'NONE', #155038, #205048, #229214, .T. ) ;
#93030 = CIRCLE ( 'NONE', #105463, 0.1000000000000000888 ) ;
#93031 = VERTEX_POINT ( 'NONE', #212226 ) ;
#93032 = AXIS2_PLACEMENT_3D ( 'NONE', #216130, #60906, #196571 ) ;
#93033 = CARTESIAN_POINT ( 'NONE',  ( 21.05000000000000071, 87.65000000001212754, -133.6231074845242119 ) ) ;
#93034 = VECTOR ( 'NONE', #15374, 1000.000000000000000 ) ;
#93035 = CARTESIAN_POINT ( 'NONE',  ( -21.05000000000000071, 1.115600667400684642E-11, -63.00000000000000000 ) ) ;
#93036 = ORIENTED_EDGE ( 'NONE', *, *, #169192, .T. ) ;
#93037 = DIRECTION ( 'NONE',  ( 0.000000000000000000, 6.938893903907222067E-15, -1.000000000000000000 ) ) ;
#93038 = DIRECTION ( 'NONE',  ( 1.000000000000000000, 0.000000000000000000, 0.000000000000000000 ) ) ;
#93039 = CARTESIAN_POINT ( 'NONE',  ( 15.48841904831874849, 8.561580951692381092, -188.3499999999999659 ) ) ;
#93040 = ADVANCED_FACE ( 'NONE', ( #233079 ), #213482, .T. ) ;
#93041 = TOROIDAL_SURFACE ( 'NONE', #1455, 7.800000000000000711, 0.1000000000000000056 ) ;
#93042 = CIRCLE ( 'NONE', #30525, 0.09999999999998898659 ) ;
#93043 = VECTOR ( 'NONE', #167842, 999.9999999999998863 ) ;
#93044 = AXIS2_PLACEMENT_3D ( 'NONE', #85712, #2349, #183578 ) ;
#93045 = ORIENTED_EDGE ( 'NONE', *, *, #105249, .T. ) ;
#93046 = CARTESIAN_POINT ( 'NONE',  ( 20.95512820512820085, 67.12384868372348024, -60.96447848938343839 ) ) ;
#93047 = ORIENTED_EDGE ( 'NONE', *, *, #201177, .F. ) ;
#93048 = CARTESIAN_POINT ( 'NONE',  ( 23.14999999999999503, 64.35000000001228670, -157.8731074845244393 ) ) ;
#93050 = ORIENTED_EDGE ( 'NONE', *, *, #105230, .F. ) ;
#93049 = CARTESIAN_POINT ( 'NONE',  ( -20.85000000000000142, -11.64999999998884483, -164.6000000000000227 ) ) ;
#93051 = LINE ( 'NONE', #172649, #224094 ) ;
#93052 = DIRECTION ( 'NONE',  ( 0.000000000000000000, 0.000000000000000000, 1.000000000000000000 ) ) ;
#93053 = DIRECTION ( 'NONE',  ( -2.915501640297154283E-16, -0.9651348961777159730, 0.2617529984165023471 ) ) ;
#93054 = LINE ( 'NONE', #228739, #87987 ) ;
#93055 = CARTESIAN_POINT ( 'NONE',  ( 18.59999999999999787, 77.83534155023670564, -158.4679561919613491 ) ) ;
#93056 = CARTESIAN_POINT ( 'NONE',  ( 18.59999999999997655, 11.75000000001115552, -100.5000000000000426 ) ) ;
#93057 = CARTESIAN_POINT ( 'NONE',  ( -23.15000000000000213, -8.999999999988846255, -43.39396912265245021 ) ) ;
#93059 = EDGE_LOOP ( 'NONE', ( #120938, #182381 ) ) ;
#93058 = CARTESIAN_POINT ( 'NONE',  ( 18.49999999999998934, 65.75000000001176659, -78.27310748452438816 ) ) ;
#93060 = CARTESIAN_POINT ( 'NONE',  ( -16.87683809663752399, 44.17636539615257618, -235.3901923532681053 ) ) ;
#93061 = VECTOR ( 'NONE', #126706, 1000.000000000000000 ) ;
#93062 = CARTESIAN_POINT ( 'NONE',  ( -18.35668295345803713, 16.37079970714665933, -222.2530670965321349 ) ) ;
#93063 = DIRECTION ( 'NONE',  ( -0.7071067811865388020, 0.6233112732207695128, -0.3338907855510773737 ) ) ;
#93064 = EDGE_LOOP ( 'NONE', ( #12605, #107184, #152121, #60493 ) ) ;
#93065 = ADVANCED_FACE ( 'NONE', ( #110530 ), #140409, .F. ) ;
#93066 = DIRECTION ( 'NONE',  ( 0.000000000000000000, 0.9126074666063844765, 0.4088369013363113980 ) ) ;
#93067 = CARTESIAN_POINT ( 'NONE',  ( 23.14999999999999858, 5.500000000011153745, -188.5947339810868755 ) ) ;
#93068 = EDGE_CURVE ( 'NONE', #105943, #149376, #11455, .T. ) ;
#93069 = DIRECTION ( 'NONE',  ( 0.000000000000000000, 0.000000000000000000, 1.000000000000000000 ) ) ;
#93070 = ORIENTED_EDGE ( 'NONE', *, *, #235378, .F. ) ;
#93071 = VECTOR ( 'NONE', #16132, 1000.000000000000000 ) ;
#93072 = DIRECTION ( 'NONE',  ( -1.000000000000000000, 0.000000000000000000, 0.000000000000000000 ) ) ;
#93073 = CIRCLE ( 'NONE', #226136, 0.1000000000000055844 ) ;
#93074 = AXIS2_PLACEMENT_3D ( 'NONE', #116922, #196446, #17803 ) ;
#93075 = CARTESIAN_POINT ( 'NONE',  ( -21.93340585971669654, 60.16248467656274102, -233.9380090624021591 ) ) ;
#93076 = EDGE_CURVE ( 'NONE', #195729, #216103, #55656, .T. ) ;
#93077 = ORIENTED_EDGE ( 'NONE', *, *, #194644, .T. ) ;
#93078 = FACE_OUTER_BOUND ( 'NONE', #135353, .T. ) ;
#93079 = ORIENTED_EDGE ( 'NONE', *, *, #63052, .T. ) ;
#93080 = LINE ( 'NONE', #249610, #150717 ) ;
#93082 = EDGE_LOOP ( 'NONE', ( #224657, #26165, #247006 ) ) ;
#93081 = CARTESIAN_POINT ( 'NONE',  ( 21.05000000000000071, 6.304516329275452691, -134.0211033080591960 ) ) ;
#93083 = EDGE_CURVE ( 'NONE', #157859, #85747, #248562, .T. ) ;
#93084 = DIRECTION ( 'NONE',  ( 1.000000000000000000, 0.000000000000000000, 0.000000000000000000 ) ) ;
#93085 = ORIENTED_EDGE ( 'NONE', *, *, #257400, .T. ) ;
#93086 = CARTESIAN_POINT ( 'NONE',  ( 21.05000000000000071, -4.735542975717121905, -233.2463119243910796 ) ) ;
#93087 = VERTEX_POINT ( 'NONE', #171836 ) ;
#93089 = ORIENTED_EDGE ( 'NONE', *, *, #52617, .T. ) ;
#93088 = ORIENTED_EDGE ( 'NONE', *, *, #175225, .F. ) ;
#93091 = FACE_OUTER_BOUND ( 'NONE', #115643, .T. ) ;
#93090 = CIRCLE ( 'NONE', #59946, 0.1000000000000028644 ) ;
#93092 = EDGE_CURVE ( 'NONE', #196564, #7658, #33621, .T. ) ;
#93094 = ORIENTED_EDGE ( 'NONE', *, *, #201940, .F. ) ;
#93093 = CARTESIAN_POINT ( 'NONE',  ( -14.00000000000000178, 62.10905854918435409, -217.1108499610990918 ) ) ;
#93095 = CARTESIAN_POINT ( 'NONE',  ( -21.05000000000000071, 7.128833340094563376, -233.7327013124401276 ) ) ;
#93096 = ORIENTED_EDGE ( 'NONE', *, *, #36691, .F. ) ;
#93097 = VECTOR ( 'NONE', #73842, 1000.000000000000000 ) ;
#93098 = CONICAL_SURFACE ( 'NONE', #251886, 7.750000000000034639, 0.7853981633974531640 ) ;
#93099 = AXIS2_PLACEMENT_3D ( 'NONE', #239685, #101398, #23228 ) ;
#93100 = ORIENTED_EDGE ( 'NONE', *, *, #86341, .T. ) ;
#93101 = DIRECTION ( 'NONE',  ( 0.000000000000000000, 0.000000000000000000, -1.000000000000000000 ) ) ;
#93102 = EDGE_CURVE ( 'NONE', #253555, #3812, #157012, .T. ) ;
#93103 = DIRECTION ( 'NONE',  ( 0.000000000000000000, 0.000000000000000000, -1.000000000000000000 ) ) ;
#93104 = CARTESIAN_POINT ( 'NONE',  ( -23.25000000000000000, 74.00000000001199396, -116.2477294072864140 ) ) ;
#93105 = ORIENTED_EDGE ( 'NONE', *, *, #193679, .F. ) ;
#93106 = DIRECTION ( 'NONE',  ( -1.000000000000000000, 0.000000000000000000, 0.000000000000000000 ) ) ;
#93107 = CARTESIAN_POINT ( 'NONE',  ( 20.94999999999999929, -11.29603075032412995, -103.5478991596638991 ) ) ;
#93108 = DIRECTION ( 'NONE',  ( 1.000000000000000000, -0.000000000000000000, -0.000000000000000000 ) ) ;
#93109 = CIRCLE ( 'NONE', #80621, 0.09999999999999978351 ) ;
#93110 = ORIENTED_EDGE ( 'NONE', *, *, #70088, .F. ) ;
#93111 = CIRCLE ( 'NONE', #201257, 0.9000000000000014655 ) ;
#93112 = DIRECTION ( 'NONE',  ( 1.000000000000000000, 0.000000000000000000, 0.000000000000000000 ) ) ;
#93113 = CARTESIAN_POINT ( 'NONE',  ( -18.50000000000000000, 57.82359945636609666, -226.0354702357591350 ) ) ;
#93114 =( NAMED_UNIT ( * ) SI_UNIT ( $, .STERADIAN. ) SOLID_ANGLE_UNIT ( ) );
#93115 = AXIS2_PLACEMENT_3D ( 'NONE', #202392, #4177, #40782 ) ;
#93116 = ORIENTED_EDGE ( 'NONE', *, *, #201049, .T. ) ;
#93117 = CARTESIAN_POINT ( 'NONE',  ( -18.59999999999999787, 1.250000000011155299, -142.0000000000000284 ) ) ;
#93118 = VERTEX_POINT ( 'NONE', #170572 ) ;
#93119 = CARTESIAN_POINT ( 'NONE',  ( -18.43599941264911024, -7.817436179055779810, -209.8389870226308744 ) ) ;
#93120 = ORIENTED_EDGE ( 'NONE', *, *, #246804, .T. ) ;
#93121 = CARTESIAN_POINT ( 'NONE',  ( -12.25000000000000178, 9.849999999999978328, -16.75000000000000355 ) ) ;
#93123 = EDGE_LOOP ( 'NONE', ( #35347, #52848, #232047, #11435 ) ) ;
#93122 = AXIS2_PLACEMENT_3D ( 'NONE', #180455, #254795, #197436 ) ;
#93124 = EDGE_LOOP ( 'NONE', ( #191097, #162591, #79688, #11309 ) ) ;
#93125 = CARTESIAN_POINT ( 'NONE',  ( -21.05000000000000071, 0.000000000000000000, 0.000000000000000000 ) ) ;
#93126 = CARTESIAN_POINT ( 'NONE',  ( -20.85000000000000142, -11.64999999998884483, -198.0999999999999659 ) ) ;
#93127 = ORIENTED_EDGE ( 'NONE', *, *, #147802, .T. ) ;
#93128 = ORIENTED_EDGE ( 'NONE', *, *, #40302, .T. ) ;
#93129 = DIRECTION ( 'NONE',  ( 0.000000000000000000, 0.000000000000000000, -1.000000000000000000 ) ) ;
#93130 = CIRCLE ( 'NONE', #109696, 11.80000000000000426 ) ;
#93131 = B_SPLINE_CURVE_WITH_KNOTS ( 'NONE', 3,
 ( #110674, #151093, #230634, #191526 ),
 .UNSPECIFIED., .F., .F.,
 ( 4, 4 ),
 ( 0.000000000000000000, 7.713889350929220882E-05 ),
 .UNSPECIFIED. ) ;
#93132 = CIRCLE ( 'NONE', #138882, 11.70000000000001528 ) ;
#93133 = CARTESIAN_POINT ( 'NONE',  ( -18.53317502108577486, 65.67736539654923433, -63.96251168765718376 ) ) ;
#93134 = AXIS2_PLACEMENT_3D ( 'NONE', #25958, #84587, #8952 ) ;
#93135 = ORIENTED_EDGE ( 'NONE', *, *, #13020, .F. ) ;
#93136 = ORIENTED_EDGE ( 'NONE', *, *, #18802, .T. ) ;
#93137 = EDGE_CURVE ( 'NONE', #205773, #249247, #250050, .T. ) ;
#93138 = CARTESIAN_POINT ( 'NONE',  ( 23.25000000000000000, 87.48912529308779540, -72.62310748452422615 ) ) ;
#93139 = DIRECTION ( 'NONE',  ( 0.000000000000000000, -1.000000000000000000, -6.982962677686266711E-15 ) ) ;
#93140 = EDGE_CURVE ( 'NONE', #182294, #256518, #190324, .T. ) ;
#93141 = DIRECTION ( 'NONE',  ( 0.000000000000000000, 0.4930308989875230585, 0.8700118002898322711 ) ) ;
#93143 = ORIENTED_EDGE ( 'NONE', *, *, #217507, .T. ) ;
#93142 = CARTESIAN_POINT ( 'NONE',  ( 21.05000000000000071, 76.00000000001170974, -69.52310748452431710 ) ) ;
#93144 = CARTESIAN_POINT ( 'NONE',  ( -17.78043020864320312, 10.85359211201683394, -110.8369508342798326 ) ) ;
#93145 = CARTESIAN_POINT ( 'NONE',  ( -22.50014994444009275, 12.60373254347260641, -223.3361492492173852 ) ) ;
#93146 = CARTESIAN_POINT ( 'NONE',  ( 23.14999999999999858, 76.00000000001213607, -136.5231074845243313 ) ) ;
#93147 = VECTOR ( 'NONE', #118036, 1000.000000000000000 ) ;
#93148 = EDGE_CURVE ( 'NONE', #161835, #197578, #211153, .T. ) ;
#93150 = DIRECTION ( 'NONE',  ( -0.000000000000000000, -6.982962677686266711E-15, 1.000000000000000000 ) ) ;
#93149 = DIRECTION ( 'NONE',  ( -0.000000000000000000, -0.000000000000000000, -1.000000000000000000 ) ) ;
#93152 = EDGE_CURVE ( 'NONE', #253265, #146973, #94805, .T. ) ;
#93151 = DIRECTION ( 'NONE',  ( -1.000000000000000000, -0.000000000000000000, -0.000000000000000000 ) ) ;
#93153 = DIRECTION ( 'NONE',  ( -1.000000000000000000, -0.000000000000000000, -0.000000000000000000 ) ) ;
#93154 = AXIS2_PLACEMENT_3D ( 'NONE', #7926, #187855, #168317 ) ;
#93155 = CYLINDRICAL_SURFACE ( 'NONE', #185153, 0.09999999999998898659 ) ;
#93157 = CARTESIAN_POINT ( 'NONE',  ( -21.04999999999999716, 76.00000000001243450, -176.5637644362255969 ) ) ;
#93156 = AXIS2_PLACEMENT_3D ( 'NONE', #228052, #32450, #130211 ) ;
#93158 = ORIENTED_EDGE ( 'NONE', *, *, #225082, .T. ) ;
#93159 = CIRCLE ( 'NONE', #47360, 0.1000000000000008799 ) ;
#93160 = AXIS2_PLACEMENT_3D ( 'NONE', #196769, #80662, #220208 ) ;
#93161 = ORIENTED_EDGE ( 'NONE', *, *, #85305, .T. ) ;
#93162 = EDGE_CURVE ( 'NONE', #221285, #160725, #12750, .T. ) ;
#93163 = DIRECTION ( 'NONE',  ( 0.000000000000000000, 0.000000000000000000, -1.000000000000000000 ) ) ;
#93164 = VECTOR ( 'NONE', #81705, 1000.000000000000000 ) ;
#93165 = EDGE_CURVE ( 'NONE', #175353, #220350, #72728, .T. ) ;
#93166 = CARTESIAN_POINT ( 'NONE',  ( -23.15000000000000213, 4.250000000000000000, -21.25000000000000000 ) ) ;
#93167 = VERTEX_POINT ( 'NONE', #2124 ) ;
#93168 = AXIS2_PLACEMENT_3D ( 'NONE', #253456, #236470, #190955 ) ;
#93169 =( LENGTH_UNIT ( ) NAMED_UNIT ( * ) SI_UNIT ( .MILLI., .METRE. ) );
#93170 = AXIS2_PLACEMENT_3D ( 'NONE', #220316, #241166, #179913 ) ;
#93171 = CARTESIAN_POINT ( 'NONE',  ( -18.79999999999999716, 7.799999999999999822, 1.212568896937007867 ) ) ;
#93172 = AXIS2_PLACEMENT_3D ( 'NONE', #198381, #22341, #8848 ) ;
#93173 = FACE_OUTER_BOUND ( 'NONE', #230455, .T. ) ;
#93174 = ORIENTED_EDGE ( 'NONE', *, *, #126356, .F. ) ;
#93175 = VERTEX_POINT ( 'NONE', #239479 ) ;
#93176 = FACE_OUTER_BOUND ( 'NONE', #238772, .T. ) ;
#93177 = DIRECTION ( 'NONE',  ( 1.000000000000000000, 0.000000000000000000, 0.000000000000000000 ) ) ;
#93178 = ADVANCED_FACE ( 'NONE', ( #19136 ), #94618, .T. ) ;
#93179 = EDGE_CURVE ( 'NONE', #21614, #38211, #153118, .T. ) ;
#93180 = PLANE ( 'NONE',  #124482 ) ;
#93182 = EDGE_LOOP ( 'NONE', ( #192264, #254101, #2796, #104072 ) ) ;
#93181 = CARTESIAN_POINT ( 'NONE',  ( -20.07928932188135107, 9.220710678129810489, -155.2500000000000284 ) ) ;
#93183 = DIRECTION ( 'NONE',  ( -1.646408749285562691E-14, -1.000000000000000000, -6.982962677686266711E-15 ) ) ;
#93184 = EDGE_CURVE ( 'NONE', #202185, #181381, #177314, .T. ) ;
#93185 = AXIS2_PLACEMENT_3D ( 'NONE', #216415, #75650, #135580 ) ;
#93187 = ORIENTED_EDGE ( 'NONE', *, *, #79021, .T. ) ;
#93186 = DIRECTION ( 'NONE',  ( -0.000000000000000000, -0.000000000000000000, -1.000000000000000000 ) ) ;
#93188 = DIRECTION ( 'NONE',  ( 0.000000000000000000, -0.4088369013363280513, 0.9126074666063769270 ) ) ;
#93189 = DIRECTION ( 'NONE',  ( -5.790381434762883172E-16, 0.9910465087640865089, 0.1335171055202867274 ) ) ;
#93190 = DIRECTION ( 'NONE',  ( -1.000000000000000000, 2.849773892568378313E-16, -7.728835255496647986E-17 ) ) ;
#93191 = DIRECTION ( 'NONE',  ( 1.000000000000000000, -0.000000000000000000, 0.000000000000000000 ) ) ;
#93192 = CIRCLE ( 'NONE', #230590, 0.3999999999999952482 ) ;
#93193 = CARTESIAN_POINT ( 'NONE',  ( 21.14999999999999858, 11.65000000001115943, -100.6000000000000369 ) ) ;
#93194 = DIRECTION ( 'NONE',  ( 0.000000000000000000, 3.552713678800509607E-15, 1.000000000000000000 ) ) ;
#93195 = CARTESIAN_POINT ( 'NONE',  ( -18.59999999999999787, 85.48068669529064323, -62.58199231576639932 ) ) ;
#93196 = CARTESIAN_POINT ( 'NONE',  ( -18.44204374631836174, 85.49103638961074125, -163.3969062143033000 ) ) ;
#93197 = CARTESIAN_POINT ( 'NONE',  ( 21.04999999999988702, 1.599564567716171615, -230.7124193606981351 ) ) ;
#93198 = DIRECTION ( 'NONE',  ( -1.000000000000000000, -1.186688945009010077E-16, -0.000000000000000000 ) ) ;
#93199 = VECTOR ( 'NONE', #38622, 1000.000000000000000 ) ;
#93201 = ORIENTED_EDGE ( 'NONE', *, *, #55452, .T. ) ;
#93200 = AXIS2_PLACEMENT_3D ( 'NONE', #168830, #245757, #67113 ) ;
#93202 = CARTESIAN_POINT ( 'NONE',  ( -16.91256925476570672, 9.985731158139332209, -79.53235751099475692 ) ) ;
#93203 = AXIS2_PLACEMENT_3D ( 'NONE', #64449, #12201, #111282 ) ;
#93204 = ORIENTED_EDGE ( 'NONE', *, *, #58381, .T. ) ;
#93205 = EDGE_LOOP ( 'NONE', ( #96036, #144737, #185555, #213300 ) ) ;
#93206 = FACE_OUTER_BOUND ( 'NONE', #54395, .T. ) ;
#93207 =( NAMED_UNIT ( * ) PLANE_ANGLE_UNIT ( ) SI_UNIT ( $, .RADIAN. ) );
#93208 =( BOUNDED_CURVE ( )  B_SPLINE_CURVE ( 3, ( #163260, #6735, #23766, #164542 ),
 .UNSPECIFIED., .F., .F. ) 
 B_SPLINE_CURVE_WITH_KNOTS ( ( 4, 4 ),
 ( 1.570796326794908992, 2.617993877991481533 ),
 .UNSPECIFIED. ) 
 CURVE ( )  GEOMETRIC_REPRESENTATION_ITEM ( )  RATIONAL_B_SPLINE_CURVE ( ( 1.000000000000000000, 0.9106836025229633202, 0.9106836025229633202, 1.000000000000000000 ) ) 
 REPRESENTATION_ITEM ( '' )  );
#93210 = EDGE_CURVE ( 'NONE', #184016, #39881, #15548, .T. ) ;
#93209 = ORIENTED_EDGE ( 'NONE', *, *, #58735, .T. ) ;
#93211 = CYLINDRICAL_SURFACE ( 'NONE', #36261, 0.09999999999999939493 ) ;
#93212 =( LENGTH_UNIT ( ) NAMED_UNIT ( * ) SI_UNIT ( .MILLI., .METRE. ) );
#93213 = AXIS2_PLACEMENT_3D ( 'NONE', #185472, #107208, #66809 ) ;
#93214 = AXIS2_PLACEMENT_3D ( 'NONE', #233862, #77336, #216851 ) ;
#93215 = ORIENTED_EDGE ( 'NONE', *, *, #232856, .F. ) ;
#93216 = AXIS2_PLACEMENT_3D ( 'NONE', #48885, #206682, #71046 ) ;
#93217 = ORIENTED_EDGE ( 'NONE', *, *, #16764, .T. ) ;
#93218 = DIRECTION ( 'NONE',  ( 0.000000000000000000, -0.9651348961777157509, 0.2617529984165031243 ) ) ;
#93219 = DIRECTION ( 'NONE',  ( 0.000000000000000000, -6.982962677686266711E-15, 1.000000000000000000 ) ) ;
#93220 = DIRECTION ( 'NONE',  ( 0.000000000000000000, 0.000000000000000000, 1.000000000000000000 ) ) ;
#93221 = DIRECTION ( 'NONE',  ( 0.000000000000000000, 1.000000000000000000, 0.000000000000000000 ) ) ;
#93222 = CARTESIAN_POINT ( 'NONE',  ( 17.23472005113827166, 10.30788195451192379, -122.5465768600687113 ) ) ;
#93223 = EDGE_CURVE ( 'NONE', #36642, #207248, #139044, .T. ) ;
#93225 = CARTESIAN_POINT ( 'NONE',  ( -1.739115166359751801E-14, 11.64999999999998970, -21.35000000000000142 ) ) ;
#93224 = DIRECTION ( 'NONE',  ( 1.000000000000000000, 0.000000000000000000, 0.000000000000000000 ) ) ;
#93226 = CARTESIAN_POINT ( 'NONE',  ( -12.47155713865592475, 9.375669526436929857, -82.86779000938599893 ) ) ;
#93228 = ORIENTED_EDGE ( 'NONE', *, *, #19328, .T. ) ;
#93227 = CARTESIAN_POINT ( 'NONE',  ( -21.05000000000000071, 74.16465844978745281, -91.46795619196133487 ) ) ;
#93230 = DIRECTION ( 'NONE',  ( 0.000000000000000000, 0.2617529984165152257, 0.9651348961777124202 ) ) ;
#93229 = DIRECTION ( 'NONE',  ( -1.000000000000000000, 3.265361837132813093E-16, 2.280189983783949500E-30 ) ) ;
#93231 = DIRECTION ( 'NONE',  ( 0.000000000000000000, 0.6728971962617388280, 0.7397360091702248619 ) ) ;
#93232 = ORIENTED_EDGE ( 'NONE', *, *, #2031, .F. ) ;
#93233 = CARTESIAN_POINT ( 'NONE',  ( -18.42609945526400139, -9.499999710479540838, -174.4993624902488136 ) ) ;
#93234 = FACE_OUTER_BOUND ( 'NONE', #60528, .T. ) ;
#93236 = EDGE_CURVE ( 'NONE', #46226, #23758, #194621, .T. ) ;
#93235 = LINE ( 'NONE', #74994, #58225 ) ;
#93237 = ORIENTED_EDGE ( 'NONE', *, *, #140649, .T. ) ;
#93238 = CARTESIAN_POINT ( 'NONE',  ( -18.59999999999999787, 74.16465844978745281, -91.46795619196133487 ) ) ;
#93239 = EDGE_CURVE ( 'NONE', #156566, #12588, #182126, .T. ) ;
#93240 = DIRECTION ( 'NONE',  ( 0.000000000000000000, -0.9999631594459056361, -0.008583690987124413183 ) ) ;
#93241 = CARTESIAN_POINT ( 'NONE',  ( -18.50000000000001066, 78.21920613375266385, -231.3255402381754493 ) ) ;
#93242 = VERTEX_POINT ( 'NONE', #240764 ) ;
#93243 = ORIENTED_EDGE ( 'NONE', *, *, #177048, .F. ) ;
#93244 = ADVANCED_FACE ( 'NONE', ( #58248 ), #159957, .F. ) ;
#93245 = VECTOR ( 'NONE', #57097, 1000.000000000000000 ) ;
#93247 = EDGE_CURVE ( 'NONE', #35062, #198003, #57186, .T. ) ;
#93246 = CARTESIAN_POINT ( 'NONE',  ( -23.25000000000000000, 74.00000000001259082, -190.2984855617622770 ) ) ;
#93248 = FACE_OUTER_BOUND ( 'NONE', #82419, .T. ) ;
#93249 = CARTESIAN_POINT ( 'NONE',  ( -21.14999999999994174, 64.25000000001119815, -3.123107484524795474 ) ) ;
#93250 = LINE ( 'NONE', #194946, #221782 ) ;
#93251 = ORIENTED_EDGE ( 'NONE', *, *, #220287, .T. ) ;
#93252 = CARTESIAN_POINT ( 'NONE',  ( 12.25000000000000000, 48.12247445990688277, -234.1702647910923361 ) ) ;
#93253 = CARTESIAN_POINT ( 'NONE',  ( 20.94999999999999574, 77.83534155023700407, -191.9679561919613491 ) ) ;
#93254 = DIRECTION ( 'NONE',  ( 0.000000000000000000, -0.2128009952263601456, 0.9770955615653316162 ) ) ;
#93255 = DIRECTION ( 'NONE',  ( -1.000000000000000000, -0.000000000000000000, -0.000000000000000000 ) ) ;
#93256 = AXIS2_PLACEMENT_3D ( 'NONE', #191907, #109753, #48504 ) ;
#93257 = EDGE_CURVE ( 'NONE', #53620, #192398, #232214, .T. ) ;
#93258 = TOROIDAL_SURFACE ( 'NONE', #34855, 0.2000000000000000111, 0.1000000000000000056 ) ;
#93260 = EDGE_CURVE ( 'NONE', #163802, #54193, #11445, .T. ) ;
#93259 = CARTESIAN_POINT ( 'NONE',  ( 21.05000000000000071, 70.60000000001205933, -124.1178414656112352 ) ) ;
#93261 = AXIS2_PLACEMENT_3D ( 'NONE', #113428, #55992, #151289 ) ;
#93263 = ORIENTED_EDGE ( 'NONE', *, *, #35791, .F. ) ;
#93262 = LINE ( 'NONE', #91980, #204304 ) ;
#93264 = DIRECTION ( 'NONE',  ( -1.000000000000000000, 1.207181226542539700E-16, -2.694675058168174199E-16 ) ) ;
#93265 = PLANE ( 'NONE',  #70273 ) ;
#93266 = DIRECTION ( 'NONE',  ( 0.000000000000000000, 0.9126074666063774821, 0.4088369013363270521 ) ) ;
#93267 = CARTESIAN_POINT ( 'NONE',  ( 21.05000000000000426, 0.06570161033324353750, -94.24168394266798998 ) ) ;
#93268 = EDGE_CURVE ( 'NONE', #46365, #136655, #196479, .T. ) ;
#93269 = CARTESIAN_POINT ( 'NONE',  ( 19.75857864376268935, 62.39550153362034735, -208.7959266050682459 ) ) ;
#93271 = ORIENTED_EDGE ( 'NONE', *, *, #108341, .F. ) ;
#93270 = DIRECTION ( 'NONE',  ( 0.000000000000000000, -7.272083257015735086E-15, 1.000000000000000000 ) ) ;
#93272 = FACE_OUTER_BOUND ( 'NONE', #32180, .T. ) ;
#93273 = FACE_OUTER_BOUND ( 'NONE', #49137, .T. ) ;
#93274 = DIRECTION ( 'NONE',  ( 1.000000000000000000, 0.000000000000000000, 0.000000000000000000 ) ) ;
#93275 = ORIENTED_EDGE ( 'NONE', *, *, #98388, .T. ) ;
#93276 = DIRECTION ( 'NONE',  ( 1.000000000000000000, 0.000000000000000000, 0.000000000000000000 ) ) ;
#93277 = DIRECTION ( 'NONE',  ( 0.000000000000000000, 0.000000000000000000, 1.000000000000000000 ) ) ;
#93278 = EDGE_CURVE ( 'NONE', #88045, #26647, #115468, .T. ) ;
#93279 = CARTESIAN_POINT ( 'NONE',  ( 18.39999999999999858, 85.60000000001186038, -96.42291809330220076 ) ) ;
#93280 = AXIS2_PLACEMENT_3D ( 'NONE', #168781, #68351, #231285 ) ;
#93281 = EDGE_CURVE ( 'NONE', #180046, #19038, #96089, .T. ) ;
#93282 = CARTESIAN_POINT ( 'NONE',  ( -20.64999999999999858, 2.000000000011154189, -120.7753780772379315 ) ) ;
#93283 = CIRCLE ( 'NONE', #247219, 0.09999999999999939493 ) ;
#93284 = DIRECTION ( 'NONE',  ( -1.000000000000000000, 0.000000000000000000, -0.000000000000000000 ) ) ;
#93286 = ORIENTED_EDGE ( 'NONE', *, *, #71539, .F. ) ;
#93285 = AXIS2_PLACEMENT_3D ( 'NONE', #157571, #21872, #137941 ) ;
#93287 = ORIENTED_EDGE ( 'NONE', *, *, #167746, .F. ) ;
#93288 = CIRCLE ( 'NONE', #239042, 0.09999999999999939493 ) ;
#93289 = ADVANCED_FACE ( 'NONE', ( #137783 ), #16595, .F. ) ;
#93290 = CARTESIAN_POINT ( 'NONE',  ( -18.41353343127311604, -9.499999999988851584, -141.0320693966997396 ) ) ;
#93291 = DIRECTION ( 'NONE',  ( -1.000000000000000000, 0.000000000000000000, 0.000000000000000000 ) ) ;
#93292 = CARTESIAN_POINT ( 'NONE',  ( 18.47688499308726051, -0.6931819285577012213, -242.2946892244310959 ) ) ;
#93293 = DIRECTION ( 'NONE',  ( 0.000000000000000000, 0.8814952561688442767, -0.4721928772777321814 ) ) ;
#93294 = EDGE_CURVE ( 'NONE', #248313, #243146, #236898, .T. ) ;
#93295 = DIRECTION ( 'NONE',  ( -0.000000000000000000, -0.000000000000000000, -1.000000000000000000 ) ) ;
#93296 = AXIS2_PLACEMENT_3D ( 'NONE', #31975, #232737, #134869 ) ;
#93297 = CIRCLE ( 'NONE', #14226, 0.1000000000000072220 ) ;
#93298 = LINE ( 'NONE', #69916, #229792 ) ;
#93299 = AXIS2_PLACEMENT_3D ( 'NONE', #173590, #253058, #193106 ) ;
#93300 = DIRECTION ( 'NONE',  ( -1.000000000000000000, -0.000000000000000000, -0.000000000000000000 ) ) ;
#93301 = AXIS2_PLACEMENT_3D ( 'NONE', #112638, #129630, #245730 ) ;
#93302 = CARTESIAN_POINT ( 'NONE',  ( -23.25000000000000000, 46.46967969402478360, -243.0849751855955674 ) ) ;
#93303 = ORIENTED_EDGE ( 'NONE', *, *, #63228, .T. ) ;
#93304 = CARTESIAN_POINT ( 'NONE',  ( -18.50000000000000000, 78.52025535392039046, -230.5241873323956554 ) ) ;
#93305 = AXIS2_PLACEMENT_3D ( 'NONE', #202584, #82595, #241709 ) ;
#93306 = ORIENTED_EDGE ( 'NONE', *, *, #115668, .F. ) ;
#93307 = CARTESIAN_POINT ( 'NONE',  ( 18.54999999999999716, 12.41403342719998548, -211.2428889513006425 ) ) ;
#93308 = DIRECTION ( 'NONE',  ( -0.7071067811865474617, -0.6909108974501236844, -0.1504730267678055788 ) ) ;
#93310 = VERTEX_POINT ( 'NONE', #197770 ) ;
#93309 = CARTESIAN_POINT ( 'NONE',  ( 18.39999999999997371, 54.09900352584866567, -229.1663746252470446 ) ) ;
#93311 = AXIS2_PLACEMENT_3D ( 'NONE', #15507, #74213, #78008 ) ;
#93312 = DIRECTION ( 'NONE',  ( 0.000000000000000000, 0.000000000000000000, -1.000000000000000000 ) ) ;
#93313 = CARTESIAN_POINT ( 'NONE',  ( 21.00000000000000000, 66.25000000001260503, -191.1731074845244223 ) ) ;
#93314 = AXIS2_PLACEMENT_3D ( 'NONE', #223231, #185403, #62885 ) ;
#93315 = CARTESIAN_POINT ( 'NONE',  ( -23.15000000000000213, 68.56901367119438362, -214.3038979092079046 ) ) ;
#93316 = ORIENTED_EDGE ( 'NONE', *, *, #153227, .T. ) ;
#93318 = DIRECTION ( 'NONE',  ( 0.000000000000000000, 0.2128009952263607008, -0.9770955615653315052 ) ) ;
#93317 = TOROIDAL_SURFACE ( 'NONE', #68388, 0.2000000000000000111, 0.1000000000000000056 ) ;
#93319 = DIRECTION ( 'NONE',  ( -2.978066053179067751E-16, 1.000000000000000000, 0.000000000000000000 ) ) ;
#93320 = CARTESIAN_POINT ( 'NONE',  ( -21.05000000000000071, 76.00000000001165290, -69.52310748452431710 ) ) ;
#93321 = CARTESIAN_POINT ( 'NONE',  ( 21.05000000000000071, 64.25000000001175238, -76.53791325517833855 ) ) ;
#93322 = CARTESIAN_POINT ( 'NONE',  ( 18.59999999999999076, 69.60000000001261355, -193.5926828544628222 ) ) ;
#93323 = ORIENTED_EDGE ( 'NONE', *, *, #47039, .T. ) ;
#93324 = CARTESIAN_POINT ( 'NONE',  ( -20.64999999999999858, 19.25956423861613231, -238.0467473098318010 ) ) ;
#93325 = DIRECTION ( 'NONE',  ( 1.000000000000000000, 0.000000000000000000, 0.000000000000000000 ) ) ;
#93326 = EDGE_CURVE ( 'NONE', #154564, #148964, #78049, .T. ) ;
#93327 = EDGE_LOOP ( 'NONE', ( #161000, #40491, #116373, #75820 ) ) ;
#93328 = ORIENTED_EDGE ( 'NONE', *, *, #124898, .T. ) ;
#93329 = DIRECTION ( 'NONE',  ( 0.000000000000000000, -1.000000000000000000, 0.000000000000000000 ) ) ;
#93330 = DIRECTION ( 'NONE',  ( 0.000000000000000000, 0.000000000000000000, -1.000000000000000000 ) ) ;
#93331 = CIRCLE ( 'NONE', #239095, 0.09999999999999317768 ) ;
#93332 = ORIENTED_EDGE ( 'NONE', *, *, #105332, .F. ) ;
#93333 = DIRECTION ( 'NONE',  ( -1.000000000000000000, -0.000000000000000000, -0.000000000000000000 ) ) ;
#93334 = CARTESIAN_POINT ( 'NONE',  ( 21.05000000000000071, 8.872080675389078408, -42.02104741883048433 ) ) ;
#93335 = AXIS2_PLACEMENT_3D ( 'NONE', #217143, #58071, #136316 ) ;
#93336 = EDGE_CURVE ( 'NONE', #58353, #133225, #86791, .T. ) ;
#93338 = ORIENTED_EDGE ( 'NONE', *, *, #19244, .F. ) ;
#93337 = AXIS2_PLACEMENT_3D ( 'NONE', #206889, #227723, #68669 ) ;
#93339 = VECTOR ( 'NONE', #102991, 1000.000000000000000 ) ;
#93340 = B_SPLINE_CURVE_WITH_KNOTS ( 'NONE', 3,
 ( #29760, #186238, #6292, #130096, #207084, #49279, #205786, #67563 ),
 .UNSPECIFIED., .F., .F.,
 ( 4, 2, 2, 4 ),
 ( 0.000000000000000000, 9.550056980124080818E-05, 0.0001910011396024816164, 0.0003820022792049778152 ),
 .UNSPECIFIED. ) ;
#93341 = VECTOR ( 'NONE', #34865, 1000.000000000000000 ) ;
#93342 = EDGE_LOOP ( 'NONE', ( #72805, #222599, #89325, #41236 ) ) ;
#93343 = DIRECTION ( 'NONE',  ( 1.836970198721030427E-16, 0.4088369013363281623, -0.9126074666063771490 ) ) ;
#93344 = DIRECTION ( 'NONE',  ( 0.000000000000000000, 0.000000000000000000, -1.000000000000000000 ) ) ;
#93346 = ORIENTED_EDGE ( 'NONE', *, *, #246677, .F. ) ;
#93345 = DIRECTION ( 'NONE',  ( 4.408576920032447355E-17, -0.1350103645451876666, 0.9908441862701600211 ) ) ;
#93348 = AXIS2_PLACEMENT_3D ( 'NONE', #222206, #186990, #246922 ) ;
#93347 = DIRECTION ( 'NONE',  ( 0.000000000000000000, -1.000000000000000000, 0.000000000000000000 ) ) ;
#93349 = CARTESIAN_POINT ( 'NONE',  ( -18.49513951962168434, 85.43772502668934976, -62.74503490949511075 ) ) ;
#93350 = DIRECTION ( 'NONE',  ( 0.000000000000000000, 0.000000000000000000, -1.000000000000000000 ) ) ;
#93351 = AXIS2_PLACEMENT_3D ( 'NONE', #200763, #241191, #2545 ) ;
#93352 = DIRECTION ( 'NONE',  ( 0.000000000000000000, 0.000000000000000000, 1.000000000000000000 ) ) ;
#93353 = CARTESIAN_POINT ( 'NONE',  ( -16.77977881697926321, 66.05339806647938872, -157.3617289114093865 ) ) ;
#93354 = AXIS2_PLACEMENT_3D ( 'NONE', #235699, #15396, #191481 ) ;
#93356 = ORIENTED_EDGE ( 'NONE', *, *, #75462, .F. ) ;
#93355 = DIRECTION ( 'NONE',  ( 0.000000000000000000, 0.8700118002898393765, -0.4930308989875104575 ) ) ;
#93357 = VERTEX_POINT ( 'NONE', #245896 ) ;
#93359 = CARTESIAN_POINT ( 'NONE',  ( -16.92280123533709002, 51.43576438431487219, -232.0284949092479962 ) ) ;
#93358 = CARTESIAN_POINT ( 'NONE',  ( -21.70464131381649509, 68.90464198104380955, -69.52310748452435973 ) ) ;
#93360 = AXIS2_PLACEMENT_3D ( 'NONE', #98601, #256370, #37410 ) ;
#93362 = ORIENTED_EDGE ( 'NONE', *, *, #33124, .T. ) ;
#93361 = DIRECTION ( 'NONE',  ( 0.000000000000000000, 0.8490545835447252943, 0.5283051335749947564 ) ) ;
#93363 = ORIENTED_EDGE ( 'NONE', *, *, #188462, .F. ) ;
#93364 = CARTESIAN_POINT ( 'NONE',  ( -22.47071067811865319, 0.3704148268516942455, -229.9999874772930752 ) ) ;
#93365 = CARTESIAN_POINT ( 'NONE',  ( -20.54999999999999716, 63.56320957583155717, -222.0641766000055668 ) ) ;
#93366 = AXIS2_PLACEMENT_3D ( 'NONE', #234214, #195132, #132569 ) ;
#93367 = FACE_OUTER_BOUND ( 'NONE', #80216, .T. ) ;
#93368 = CARTESIAN_POINT ( 'NONE',  ( 19.99999999738042789, 11.75000000001116440, -58.18717194963263495 ) ) ;
#93369 = FACE_OUTER_BOUND ( 'NONE', #69672, .T. ) ;
#93370 = TOROIDAL_SURFACE ( 'NONE', #105834, 0.2000000000000000111, 0.1000000000000000056 ) ;
#93371 = DIRECTION ( 'NONE',  ( 0.000000000000000000, -0.2617529984165031243, -0.9651348961777157509 ) ) ;
#93372 = EDGE_CURVE ( 'NONE', #60849, #246816, #256499, .T. ) ;
#93373 = ORIENTED_EDGE ( 'NONE', *, *, #75201, .F. ) ;
#93374 = EDGE_LOOP ( 'NONE', ( #70478, #152201, #55147, #195593 ) ) ;
#93375 = DIRECTION ( 'NONE',  ( 0.000000000000000000, -0.4721928772777285732, -0.8814952561688463861 ) ) ;
#93376 = EDGE_CURVE ( 'NONE', #975, #129212, #111382, .T. ) ;
#93377 = ORIENTED_EDGE ( 'NONE', *, *, #113794, .F. ) ;
#93378 = DIRECTION ( 'NONE',  ( 0.000000000000000000, 0.000000000000000000, -1.000000000000000000 ) ) ;
#93379 = ORIENTED_EDGE ( 'NONE', *, *, #126277, .T. ) ;
#93381 = AXIS2_PLACEMENT_3D ( 'NONE', #132271, #151869, #231389 ) ;
#93380 = CARTESIAN_POINT ( 'NONE',  ( -20.85000000000000142, -1.835859311432481045, -112.0044391687985694 ) ) ;
#93382 = CIRCLE ( 'NONE', #168469, 0.1000000000000028644 ) ;
#93383 = AXIS2_PLACEMENT_3D ( 'NONE', #108710, #188244, #9592 ) ;
#93384 = CARTESIAN_POINT ( 'NONE',  ( -16.91247567987037925, 9.959082683680399839, -79.62872445853739123 ) ) ;
#93385 = ADVANCED_FACE ( 'NONE', ( #244592 ), #185910, .F. ) ;
#93386 = CARTESIAN_POINT ( 'NONE',  ( -12.68215100488890101, 66.60336962369433422, -118.6160500917060858 ) ) ;
#93387 = EDGE_LOOP ( 'NONE', ( #189744, #177213, #186456, #74576 ) ) ;
#93388 = DIRECTION ( 'NONE',  ( -1.000000000000000000, 0.000000000000000000, 0.000000000000000000 ) ) ;
#93389 = ORIENTED_EDGE ( 'NONE', *, *, #63189, .F. ) ;
#93390 = EDGE_CURVE ( 'NONE', #176836, #89559, #227145, .T. ) ;
#93391 = CARTESIAN_POINT ( 'NONE',  ( 20.94999999999999929, 71.00000000001253397, -182.4283735034374843 ) ) ;
#93392 = CARTESIAN_POINT ( 'NONE',  ( 18.51997666896936678, 8.990719673716817795, -245.3850630519680465 ) ) ;
#93393 = EDGE_LOOP ( 'NONE', ( #242023, #33322, #188515 ) ) ;
#93394 = DIRECTION ( 'NONE',  ( -0.000000000000000000, 0.9651348961777157509, -0.2617529984165031243 ) ) ;
#93395 = EDGE_CURVE ( 'NONE', #19871, #51212, #146753, .T. ) ;
#93396 = VERTEX_POINT ( 'NONE', #26870 ) ;
#93399 = ORIENTED_EDGE ( 'NONE', *, *, #78924, .F. ) ;
#93398 = DIRECTION ( 'NONE',  ( 0.000000000000000000, 0.000000000000000000, 1.000000000000000000 ) ) ;
#93397 = DIRECTION ( 'NONE',  ( 0.000000000000000000, -6.982962677686266711E-15, 1.000000000000000000 ) ) ;
#93400 = DIRECTION ( 'NONE',  ( 0.000000000000000000, -0.2617529984164506107, -0.9651348961777299618 ) ) ;
#93401 = VECTOR ( 'NONE', #166000, 999.9999999999998863 ) ;
#93402 = ORIENTED_EDGE ( 'NONE', *, *, #44572, .T. ) ;
#93403 = ORIENTED_EDGE ( 'NONE', *, *, #115364, .F. ) ;
#93404 = CARTESIAN_POINT ( 'NONE',  ( 22.00411653889210584, 0.09903810578593504055, 7.253442867640402802 ) ) ;
#93405 = ORIENTED_EDGE ( 'NONE', *, *, #53704, .T. ) ;
#93406 = CYLINDRICAL_SURFACE ( 'NONE', #55871, 14.30833333333333890 ) ;
#93407 = EDGE_CURVE ( 'NONE', #18374, #19709, #132226, .T. ) ;
#93408 = DIRECTION ( 'NONE',  ( -1.000000000000000000, 0.000000000000000000, 0.000000000000000000 ) ) ;
#93409 = DIRECTION ( 'NONE',  ( 0.000000000000000000, -0.9126074666063545004, -0.4088369013363783999 ) ) ;
#93410 = CARTESIAN_POINT ( 'NONE',  ( 21.97500000000000497, 66.25000000001151079, -48.37310748452438958 ) ) ;
#93411 = CARTESIAN_POINT ( 'NONE',  ( 21.00000000000000000, 66.25000000001151079, -48.37310748452438958 ) ) ;
#93412 = ORIENTED_EDGE ( 'NONE', *, *, #51340, .T. ) ;
#93413 = CARTESIAN_POINT ( 'NONE',  ( -16.94107738177415712, 44.01795756907898749, -235.2811900454759666 ) ) ;
#93414 = CARTESIAN_POINT ( 'NONE',  ( 18.45139536634708932, 86.89352232322976022, -199.5971283272099015 ) ) ;
#93415 = CARTESIAN_POINT ( 'NONE',  ( -21.44999999999999929, 65.67360898266123570, -213.5186389139583980 ) ) ;
#93416 = ORIENTED_EDGE ( 'NONE', *, *, #218696, .F. ) ;
#93417 = PLANE ( 'NONE',  #234396 ) ;
#93418 = ORIENTED_EDGE ( 'NONE', *, *, #7946, .T. ) ;
#93419 = DIRECTION ( 'NONE',  ( -0.000000000000000000, 1.000000000000000000, 6.982962677686266711E-15 ) ) ;
#93420 = EDGE_LOOP ( 'NONE', ( #9048, #232682, #63696, #103771 ) ) ;
#93421 = CARTESIAN_POINT ( 'NONE',  ( -23.15000000000000213, 85.00000000001232081, -160.1291383618718385 ) ) ;
#93422 = DIRECTION ( 'NONE',  ( -1.000000000000000000, 0.000000000000000000, 0.000000000000000000 ) ) ;
#93424 = VERTEX_POINT ( 'NONE', #23020 ) ;
#93423 = CARTESIAN_POINT ( 'NONE',  ( 20.94999999999999574, -10.82118976317943115, -206.5294079347637819 ) ) ;
#93425 = DIRECTION ( 'NONE',  ( 1.000000000000000000, -0.000000000000000000, -0.000000000000000000 ) ) ;
#93426 = EDGE_LOOP ( 'NONE', ( #76317, #213866, #158811, #91846 ) ) ;
#93427 = EDGE_CURVE ( 'NONE', #165639, #183570, #43843, .T. ) ;
#93428 = DIRECTION ( 'NONE',  ( 0.000000000000000000, 0.000000000000000000, 1.000000000000000000 ) ) ;
#93429 = CARTESIAN_POINT ( 'NONE',  ( -16.87683809663752754, 9.865889849343227880, -113.7674268070702936 ) ) ;
#93430 = ORIENTED_EDGE ( 'NONE', *, *, #47518, .T. ) ;
#93431 = CARTESIAN_POINT ( 'NONE',  ( -22.47007471830799119, 1.115783626517291571E-11, -126.2792893480735330 ) ) ;
#93432 = CARTESIAN_POINT ( 'NONE',  ( 20.95346350065193519, 67.11282275083739535, -94.51137553748898767 ) ) ;
#93433 = ORIENTED_EDGE ( 'NONE', *, *, #5027, .T. ) ;
#93434 = DIRECTION ( 'NONE',  ( 0.000000000000000000, 0.1350103645451807555, 0.9908441862701609093 ) ) ;
#93435 = AXIS2_PLACEMENT_3D ( 'NONE', #46496, #68655, #229014 ) ;
#93436 = ORIENTED_EDGE ( 'NONE', *, *, #17685, .T. ) ;
#93437 = AXIS2_PLACEMENT_3D ( 'NONE', #246217, #130105, #109253 ) ;
#93438 = VECTOR ( 'NONE', #226590, 1000.000000000000000 ) ;
#93439 = EDGE_CURVE ( 'NONE', #87660, #17664, #253026, .T. ) ;
#93440 = CARTESIAN_POINT ( 'NONE',  ( 12.84435279558019261, 9.410708747058235346, -118.5692084058441793 ) ) ;
#93441 = LINE ( 'NONE', #156022, #114040 ) ;
#93442 = ADVANCED_FACE ( 'NONE', ( #167656, #247157 ), #46384, .T. ) ;
#93444 = EDGE_LOOP ( 'NONE', ( #11407, #131800, #222728, #161763 ) ) ;
#93443 = CARTESIAN_POINT ( 'NONE',  ( 5.900000000000059863, 64.35000000001120668, -25.92310748452479174 ) ) ;
#93445 = DIRECTION ( 'NONE',  ( 2.915501640297155269E-16, -1.000000000000000000, 0.000000000000000000 ) ) ;
#93446 = FACE_OUTER_BOUND ( 'NONE', #186397, .T. ) ;
#93447 = CARTESIAN_POINT ( 'NONE',  ( -16.93589915522259304, 10.00862525869585617, -20.94056010196031181 ) ) ;
#93448 = VECTOR ( 'NONE', #212691, 1000.000000000000000 ) ;
#93450 = CARTESIAN_POINT ( 'NONE',  ( -14.45422546970483957, 66.54939790392302257, -51.07921152142773025 ) ) ;
#93449 = CARTESIAN_POINT ( 'NONE',  ( 21.05000000000000071, -9.500000000000000000, -23.60603087734755690 ) ) ;
#93452 = EDGE_CURVE ( 'NONE', #201338, #257922, #202904, .T. ) ;
#93451 = DIRECTION ( 'NONE',  ( 0.000000000000000000, -1.000000000000000000, -6.982962677686266711E-15 ) ) ;
#93453 = CARTESIAN_POINT ( 'NONE',  ( -18.59999999999999787, 77.16412189325360771, -162.2082593989527197 ) ) ;
#93454 = SPHERICAL_SURFACE ( 'NONE', #251424, 0.1000000000000000056 ) ;
#93455 = AXIS2_PLACEMENT_3D ( 'NONE', #200390, #81680, #239521 ) ;
#93456 = CARTESIAN_POINT ( 'NONE',  ( 21.04999999999998650, 69.35000000001259934, -191.2731074845243882 ) ) ;
#93457 = CIRCLE ( 'NONE', #126794, 4.049999999999997158 ) ;
#93458 = ORIENTED_EDGE ( 'NONE', *, *, #34965, .F. ) ;
#93459 = ORIENTED_EDGE ( 'NONE', *, *, #204015, .T. ) ;
#93460 = CIRCLE ( 'NONE', #130883, 0.09999999999999939493 ) ;
#93461 = DIRECTION ( 'NONE',  ( 0.000000000000000000, 0.2965989261549202283, 0.9550021345545507412 ) ) ;
#93462 = AXIS2_PLACEMENT_3D ( 'NONE', #34023, #52240, #93948 ) ;
#93464 = ORIENTED_EDGE ( 'NONE', *, *, #169887, .T. ) ;
#93463 = DIRECTION ( 'NONE',  ( 0.000000000000000000, 0.000000000000000000, 1.000000000000000000 ) ) ;
#93465 = ORIENTED_EDGE ( 'NONE', *, *, #132373, .F. ) ;
#93466 = DIRECTION ( 'NONE',  ( 0.000000000000000000, 0.4721928772777346239, 0.8814952561688430555 ) ) ;
#93467 = EDGE_CURVE ( 'NONE', #239014, #63872, #182071, .T. ) ;
#93468 = ORIENTED_EDGE ( 'NONE', *, *, #38787, .F. ) ;
#93469 = CARTESIAN_POINT ( 'NONE',  ( -20.54999999999999716, 7.150000000011155876, -155.1500000000000057 ) ) ;
#93470 = AXIS2_PLACEMENT_3D ( 'NONE', #46066, #166052, #124336 ) ;
#93471 = EDGE_CURVE ( 'NONE', #42653, #128551, #198962, .T. ) ;
#93472 = EDGE_CURVE ( 'NONE', #197260, #18671, #69703, .T. ) ;
#93473 = ORIENTED_EDGE ( 'NONE', *, *, #169563, .T. ) ;
#93474 = CIRCLE ( 'NONE', #64272, 4.299999999999945643 ) ;
#93475 = DIRECTION ( 'NONE',  ( -1.000000000000000000, 2.952720810173289112E-16, 2.061873921506763405E-30 ) ) ;
#93476 = AXIS2_PLACEMENT_3D ( 'NONE', #166764, #8940, #168053 ) ;
#93478 = VERTEX_POINT ( 'NONE', #154528 ) ;
#93477 = ORIENTED_EDGE ( 'NONE', *, *, #217152, .F. ) ;
#93479 = ORIENTED_EDGE ( 'NONE', *, *, #20822, .T. ) ;
#93480 = EDGE_LOOP ( 'NONE', ( #108759, #133168, #49322, #117268, #139207, #238149, #204515, #170428, #66880, #232323, #124237, #55016, #69852, #136793 ) ) ;
#93481 = EDGE_LOOP ( 'NONE', ( #79605, #182996, #48087 ) ) ;
#93482 = ADVANCED_FACE ( 'NONE', ( #171518 ), #149381, .T. ) ;
#93484 = DIRECTION ( 'NONE',  ( 0.000000000000000000, 0.8814952561688440547, -0.4721928772777327921 ) ) ;
#93483 = CIRCLE ( 'NONE', #160166, 0.2000000000000057288 ) ;
#93485 = DIRECTION ( 'NONE',  ( 0.000000000000000000, -6.982962677686266711E-15, 1.000000000000000000 ) ) ;
#93486 = CARTESIAN_POINT ( 'NONE',  ( -13.77083647240106679, 9.457410930301319851, -185.9999159087463170 ) ) ;
#93488 = EDGE_LOOP ( 'NONE', ( #128630, #139031, #144850, #12036 ) ) ;
#93487 = CARTESIAN_POINT ( 'NONE',  ( 20.94999999999999929, 76.00000000001190870, -103.0231074845243029 ) ) ;
#93489 = DIRECTION ( 'NONE',  ( 0.000000000000000000, 1.000000000000000000, 6.608470384673536824E-15 ) ) ;
#93490 = EDGE_CURVE ( 'NONE', #248313, #43405, #215432, .T. ) ;
#93491 = FACE_OUTER_BOUND ( 'NONE', #154633, .T. ) ;
#93493 = VERTEX_POINT ( 'NONE', #252286 ) ;
#93492 = CARTESIAN_POINT ( 'NONE',  ( -21.56666275994539816, 0.000000000000000000, 6.957368406893326807 ) ) ;
#93494 = DIRECTION ( 'NONE',  ( 0.000000000000000000, -0.000000000000000000, 1.000000000000000000 ) ) ;
#93496 = EDGE_CURVE ( 'NONE', #10380, #241874, #19823, .T. ) ;
#93495 = ORIENTED_EDGE ( 'NONE', *, *, #230259, .T. ) ;
#93497 = CIRCLE ( 'NONE', #118465, 11.74999999999999645 ) ;
#93498 = LINE ( 'NONE', #212185, #136774 ) ;
#93499 = AXIS2_PLACEMENT_3D ( 'NONE', #190237, #188948, #67712 ) ;
#93501 = EDGE_LOOP ( 'NONE', ( #212336, #231076, #192294, #54613 ) ) ;
#93500 = DIRECTION ( 'NONE',  ( 0.000000000000000000, 0.2617529984165030132, 0.9651348961777157509 ) ) ;
#93502 = DIRECTION ( 'NONE',  ( -1.000000000000000000, -0.000000000000000000, 0.000000000000000000 ) ) ;
#93503 = DIRECTION ( 'NONE',  ( 0.000000000000000000, -0.01562499999999307672, 0.9998779222360100194 ) ) ;
#93504 = ORIENTED_EDGE ( 'NONE', *, *, #25035, .F. ) ;
#93506 = DIRECTION ( 'NONE',  ( -0.000000000000000000, -6.982962677686266711E-15, 1.000000000000000000 ) ) ;
#93505 = LINE ( 'NONE', #12721, #3128 ) ;
#93507 = DIRECTION ( 'NONE',  ( 0.000000000000000000, 0.000000000000000000, 1.000000000000000000 ) ) ;
#93508 = DIRECTION ( 'NONE',  ( 0.000000000000000000, 0.2617529984165026247, 0.9651348961777158619 ) ) ;
#93509 = CARTESIAN_POINT ( 'NONE',  ( 18.59999999999999076, 34.53503747617446606, -235.1972745784239578 ) ) ;
#93510 = ORIENTED_EDGE ( 'NONE', *, *, #248400, .F. ) ;
#93511 = ORIENTED_EDGE ( 'NONE', *, *, #66504, .T. ) ;
#93512 = FACE_OUTER_BOUND ( 'NONE', #79385, .T. ) ;
#93513 = DIRECTION ( 'NONE',  ( 1.000000000000000000, 0.000000000000000000, 0.000000000000000000 ) ) ;
#93515 = ORIENTED_EDGE ( 'NONE', *, *, #216977, .T. ) ;
#93514 = ADVANCED_FACE ( 'NONE', ( #189765 ), #153242, .T. ) ;
#93516 = CARTESIAN_POINT ( 'NONE',  ( -22.50000000000000000, -2.381330705637465961, -189.5959759702857923 ) ) ;
#93517 = ORIENTED_EDGE ( 'NONE', *, *, #201421, .F. ) ;
#93518 = EDGE_CURVE ( 'NONE', #4036, #248809, #188474, .T. ) ;
#93519 = LINE ( 'NONE', #148369, #256372 ) ;
#93520 = DIRECTION ( 'NONE',  ( 1.000000000000000000, 0.000000000000000000, 0.000000000000000000 ) ) ;
#93521 = DIRECTION ( 'NONE',  ( -0.7070776581709311559, 0.000000000000000000, 0.7071359030027479786 ) ) ;
#93522 = CIRCLE ( 'NONE', #6028, 0.2000000000000057288 ) ;
#93523 = AXIS2_PLACEMENT_3D ( 'NONE', #222953, #44343, #88571 ) ;
#93525 = EDGE_CURVE ( 'NONE', #26083, #245346, #7329, .T. ) ;
#93524 = ORIENTED_EDGE ( 'NONE', *, *, #84935, .T. ) ;
#93526 = CARTESIAN_POINT ( 'NONE',  ( 20.94999999999999929, 71.00000000001223555, -148.9283735034374843 ) ) ;
#93527 = AXIS2_PLACEMENT_3D ( 'NONE', #215568, #232602, #34399 ) ;
#93528 = ORIENTED_EDGE ( 'NONE', *, *, #30916, .F. ) ;
#93529 = VERTEX_POINT ( 'NONE', #193620 ) ;
#93530 = ORIENTED_EDGE ( 'NONE', *, *, #94608, .T. ) ;
#93531 = TOROIDAL_SURFACE ( 'NONE', #122785, 0.2000000000000000111, 0.1000000000000000056 ) ;
#93532 = PLANE ( 'NONE',  #250213 ) ;
#93533 = CARTESIAN_POINT ( 'NONE',  ( -23.15000000000000213, 66.23941198528750363, -222.8935984851895853 ) ) ;
#93534 = VECTOR ( 'NONE', #140336, 1000.000000000000000 ) ;
#93535 = SPHERICAL_SURFACE ( 'NONE', #90337, 0.1000000000000000056 ) ;
#93536 = CARTESIAN_POINT ( 'NONE',  ( 13.12229106158773639, 66.56936289831530473, -118.2548468664634385 ) ) ;
#93537 =( BOUNDED_CURVE ( )  B_SPLINE_CURVE ( 3, ( #170072, #31830, #69657, #112623 ),
 .UNSPECIFIED., .F., .T. ) 
 B_SPLINE_CURVE_WITH_KNOTS ( ( 4, 4 ),
 ( 0.06456096931748307732, 3.077031684272310219 ),
 .UNSPECIFIED. ) 
 CURVE ( )  GEOMETRIC_REPRESENTATION_ITEM ( )  RATIONAL_B_SPLINE_CURVE ( ( 1.000000000000000000, 0.3763440860215093164, 0.3763440860215093164, 1.000000000000000000 ) ) 
 REPRESENTATION_ITEM ( '' )  );
#93539 = CARTESIAN_POINT ( 'NONE',  ( -21.04999999999994387, 64.35000000001120668, -36.02310748452479316 ) ) ;
#93538 = CARTESIAN_POINT ( 'NONE',  ( 22.43288208788031568, -3.137965819587316574, -228.2274994902323328 ) ) ;
#93541 = EDGE_LOOP ( 'NONE', ( #218965, #166793, #143360, #142214 ) ) ;
#93540 = FACE_OUTER_BOUND ( 'NONE', #225039, .T. ) ;
#93542 = CARTESIAN_POINT ( 'NONE',  ( 21.05000000000000071, 76.00000000001156764, -57.37310748452432563 ) ) ;
#93543 = ORIENTED_EDGE ( 'NONE', *, *, #47757, .T. ) ;
#93544 = CARTESIAN_POINT ( 'NONE',  ( -20.90000000000000213, 6.258114003436813455, 11.90000000000000036 ) ) ;
#93545 = ORIENTED_EDGE ( 'NONE', *, *, #178063, .F. ) ;
#93546 = ORIENTED_EDGE ( 'NONE', *, *, #233760, .T. ) ;
#93547 = DIRECTION ( 'NONE',  ( -1.000000000000000000, -0.000000000000000000, -0.000000000000000000 ) ) ;
#93548 = VECTOR ( 'NONE', #140305, 1000.000000000000227 ) ;
#93549 = CARTESIAN_POINT ( 'NONE',  ( -21.05000000000000071, 6.540656951712400691, -134.1000000000000227 ) ) ;
#93551 = EDGE_CURVE ( 'NONE', #3656, #242144, #213150, .T. ) ;
#93550 = DIRECTION ( 'NONE',  ( 0.000000000000000000, -1.000000000000000000, -1.734723475976807292E-15 ) ) ;
#93552 = CIRCLE ( 'NONE', #126871, 0.09999999999998898659 ) ;
#93553 = CARTESIAN_POINT ( 'NONE',  ( 20.95483826173899899, 8.876166204781142710, -75.54627555289955865 ) ) ;
#93554 = AXIS2_PLACEMENT_3D ( 'NONE', #80023, #95753, #39682 ) ;
#93555 = ADVANCED_FACE ( 'NONE', ( #208065, #54096 ), #13688, .F. ) ;
#93556 = CARTESIAN_POINT ( 'NONE',  ( -21.65000000000000213, 7.708578643773852157, -112.7500000000000284 ) ) ;
#93557 = VERTEX_POINT ( 'NONE', #50234 ) ;
#93558 = ORIENTED_EDGE ( 'NONE', *, *, #218623, .T. ) ;
#93560 = EDGE_CURVE ( 'NONE', #11577, #166612, #23927, .T. ) ;
#93559 = DIRECTION ( 'NONE',  ( -1.000000000000000000, 0.000000000000000000, 0.000000000000000000 ) ) ;
#93561 = ORIENTED_EDGE ( 'NONE', *, *, #173958, .T. ) ;
#93562 = DIRECTION ( 'NONE',  ( -0.000000000000000000, -0.000000000000000000, 1.000000000000000000 ) ) ;
#93563 = CYLINDRICAL_SURFACE ( 'NONE', #156530, 0.09999999999998898659 ) ;
#93564 = ORIENTED_EDGE ( 'NONE', *, *, #67140, .T. ) ;
#93565 = FACE_OUTER_BOUND ( 'NONE', #178822, .T. ) ;
#93567 = AXIS2_PLACEMENT_3D ( 'NONE', #21462, #100922, #180523 ) ;
#93566 = FACE_OUTER_BOUND ( 'NONE', #22967, .T. ) ;
#93568 = CARTESIAN_POINT ( 'NONE',  ( -23.25000000000000000, 76.00000000001244871, -170.0231074845243597 ) ) ;
#93569 = FACE_OUTER_BOUND ( 'NONE', #220339, .T. ) ;
#93570 = ORIENTED_EDGE ( 'NONE', *, *, #200873, .T. ) ;
#93571 = ADVANCED_FACE ( 'NONE', ( #131069 ), #111514, .F. ) ;
#93572 = FACE_OUTER_BOUND ( 'NONE', #165942, .T. ) ;
#93573 = AXIS2_PLACEMENT_3D ( 'NONE', #112731, #192280, #12370 ) ;
#93575 = EDGE_CURVE ( 'NONE', #94400, #365, #31999, .T. ) ;
#93574 = LINE ( 'NONE', #94848, #116468 ) ;
#93576 = DIRECTION ( 'NONE',  ( -0.7070776581709311559, 0.000000000000000000, 0.7071359030027479786 ) ) ;
#93577 = B_SPLINE_CURVE_WITH_KNOTS ( 'NONE', 3,
 ( #230420, #70092, #229145, #51754, #132611, #50468 ),
 .UNSPECIFIED., .F., .F.,
 ( 4, 2, 4 ),
 ( 0.000000000000000000, 0.0002113392456166048581, 0.0004226784912332097162 ),
 .UNSPECIFIED. ) ;
#93578 = AXIS2_PLACEMENT_3D ( 'NONE', #227873, #229167, #226568 ) ;
#93579 = VECTOR ( 'NONE', #138985, 999.9999999999998863 ) ;
#93580 = EDGE_CURVE ( 'NONE', #11331, #76756, #219700, .T. ) ;
#93581 = ORIENTED_EDGE ( 'NONE', *, *, #99034, .F. ) ;
#93582 = TOROIDAL_SURFACE ( 'NONE', #97827, 0.2000000000000000111, 0.1000000000000000056 ) ;
#93584 = EDGE_CURVE ( 'NONE', #158172, #97122, #223973, .T. ) ;
#93583 = EDGE_CURVE ( 'NONE', #186109, #231870, #165756, .T. ) ;
#93585 = CARTESIAN_POINT ( 'NONE',  ( 23.24999999999999645, 7.128833340094563376, -233.7327013124401276 ) ) ;
#93586 = EDGE_LOOP ( 'NONE', ( #137115, #228232, #115293, #47580 ) ) ;
#93587 = FACE_OUTER_BOUND ( 'NONE', #24893, .T. ) ;
#93588 = CARTESIAN_POINT ( 'NONE',  ( -18.40000000000000213, 40.40436687347765599, -235.2865959907995546 ) ) ;
#93589 = DIRECTION ( 'NONE',  ( 0.000000000000000000, 0.2617529984165152257, 0.9651348961777124202 ) ) ;
#93590 = DIRECTION ( 'NONE',  ( -0.000000000000000000, 0.9770955615653313941, 0.2128009952263603677 ) ) ;
#93591 = DIRECTION ( 'NONE',  ( 0.000000000000000000, 0.9908441862701420355, 0.1350103645453197554 ) ) ;
#93592 = FACE_OUTER_BOUND ( 'NONE', #130257, .T. ) ;
#93593 = ORIENTED_EDGE ( 'NONE', *, *, #187633, .F. ) ;
#93594 = CARTESIAN_POINT ( 'NONE',  ( -16.93906926870270624, 65.98785312906551326, -123.9696551772975539 ) ) ;
#93595 = FACE_OUTER_BOUND ( 'NONE', #140760, .T. ) ;
#93596 = DIRECTION ( 'NONE',  ( 0.000000000000000000, 0.000000000000000000, -1.000000000000000000 ) ) ;
#93597 = CARTESIAN_POINT ( 'NONE',  ( -23.25000000000000355, 70.35000000001159037, -56.87310748452436115 ) ) ;
#93598 = ADVANCED_FACE ( 'NONE', ( #40991 ), #28395, .T. ) ;
#93599 = VECTOR ( 'NONE', #73977, 1000.000000000000227 ) ;
#93600 = EDGE_CURVE ( 'NONE', #46556, #30259, #248950, .T. ) ;
#93601 = DIRECTION ( 'NONE',  ( -0.5735764363510466035, -0.8191520442889914655, -0.000000000000000000 ) ) ;
#93602 = ORIENTED_EDGE ( 'NONE', *, *, #149311, .F. ) ;
#93603 = EDGE_LOOP ( 'NONE', ( #219851, #61000, #116128, #186312 ) ) ;
#93604 = CARTESIAN_POINT ( 'NONE',  ( -21.06715728752538652, 64.25000000001161027, -62.50830171387038803 ) ) ;
#93605 = CARTESIAN_POINT ( 'NONE',  ( 18.49999999999999645, 74.13328508995425636, -57.77043223824233564 ) ) ;
#93607 = EDGE_CURVE ( 'NONE', #33906, #226219, #76218, .T. ) ;
#93606 = DIRECTION ( 'NONE',  ( -1.000000000000000000, -1.794895427898103559E-16, -3.909090864890002444E-17 ) ) ;
#93608 = AXIS2_PLACEMENT_3D ( 'NONE', #181507, #180220, #43268 ) ;
#93609 = DIRECTION ( 'NONE',  ( -1.000000000000000000, -0.000000000000000000, -0.000000000000000000 ) ) ;
#93610 = EDGE_LOOP ( 'NONE', ( #158612, #249843, #109008, #145923, #157248 ) ) ;
#93612 = ADVANCED_FACE ( 'NONE', ( #39707 ), #99067, .F. ) ;
#93611 = CARTESIAN_POINT ( 'NONE',  ( -18.59999999999999787, 13.63658454968486389, -219.6758818217417968 ) ) ;
#93613 = ADVANCED_FACE ( 'NONE', ( #194921 ), #16289, .F. ) ;
#93614 = DIRECTION ( 'NONE',  ( 0.000000000000000000, 0.000000000000000000, -1.000000000000000000 ) ) ;
#93615 = ORIENTED_EDGE ( 'NONE', *, *, #145586, .T. ) ;
#93616 = DIRECTION ( 'NONE',  ( 0.000000000000000000, 0.000000000000000000, 1.000000000000000000 ) ) ;
#93617 = CARTESIAN_POINT ( 'NONE',  ( -23.25000000000000355, 70.35000000001201670, -115.6731074845243370 ) ) ;
#93618 = AXIS2_PLACEMENT_3D ( 'NONE', #59409, #239376, #257587 ) ;
#93619 = CIRCLE ( 'NONE', #251834, 11.65000000000000036 ) ;
#93620 = ORIENTED_EDGE ( 'NONE', *, *, #104260, .F. ) ;
#93621 = CARTESIAN_POINT ( 'NONE',  ( -20.94999999999999929, 60.99662849158838895, -205.1669373764474642 ) ) ;
#93622 = ORIENTED_EDGE ( 'NONE', *, *, #82563, .F. ) ;
#93623 = EDGE_CURVE ( 'NONE', #236193, #74533, #534, .T. ) ;
#93624 = CARTESIAN_POINT ( 'NONE',  ( -16.84419801905645997, 9.950000000011140600, -154.8305101537780502 ) ) ;
#93626 = EDGE_CURVE ( 'NONE', #233528, #47237, #90709, .T. ) ;
#93625 = CARTESIAN_POINT ( 'NONE',  ( -21.14999999999999858, 1.115600667400684642E-11, -122.3504291924552234 ) ) ;
#93627 = LINE ( 'NONE', #190172, #65854 ) ;
#93628 = FACE_OUTER_BOUND ( 'NONE', #219481, .T. ) ;
#93629 = CARTESIAN_POINT ( 'NONE',  ( -20.64999999999999858, 19.96675702282871256, -237.7735354486364088 ) ) ;
#93630 = CARTESIAN_POINT ( 'NONE',  ( -5.999999999999938716, 64.65000000001120384, -25.92310748452479174 ) ) ;
#93632 = DIRECTION ( 'NONE',  ( 0.000000000000000000, 0.000000000000000000, 1.000000000000000000 ) ) ;
#93631 = FACE_OUTER_BOUND ( 'NONE', #187948, .T. ) ;
#93633 = EDGE_CURVE ( 'NONE', #253865, #137271, #207442, .T. ) ;
#93634 = CARTESIAN_POINT ( 'NONE',  ( -21.05000000000000071, 1.115600667400684642E-11, -67.00000000000000000 ) ) ;
#93635 = FACE_OUTER_BOUND ( 'NONE', #108467, .T. ) ;
#93637 = DIRECTION ( 'NONE',  ( 0.000000000000000000, 2.664535259100315349E-15, 1.000000000000000000 ) ) ;
#93636 = CIRCLE ( 'NONE', #231209, 0.09999999999999939493 ) ;
#93638 = ORIENTED_EDGE ( 'NONE', *, *, #115804, .T. ) ;
#93639 = AXIS2_PLACEMENT_3D ( 'NONE', #75097, #234128, #230275 ) ;
#93640 = CARTESIAN_POINT ( 'NONE',  ( -20.94999999999999929, 11.65000000001115055, -93.71613433702194129 ) ) ;
#93641 = DIRECTION ( 'NONE',  ( 1.186688945009010077E-16, -1.000000000000000000, -0.000000000000000000 ) ) ;
#93643 = DIRECTION ( 'NONE',  ( 0.000000000000000000, 0.6728971962616783209, 0.7397360091702797069 ) ) ;
#93642 = AXIS2_PLACEMENT_3D ( 'NONE', #41314, #98645, #120855 ) ;
#93644 = CIRCLE ( 'NONE', #126959, 0.1000000000000028644 ) ;
#93645 = VERTEX_POINT ( 'NONE', #180478 ) ;
#93646 = DIRECTION ( 'NONE',  ( 0.000000000000000000, -0.4999999999999478195, 0.8660254037844686836 ) ) ;
#93647 = DIRECTION ( 'NONE',  ( 0.000000000000000000, -7.116814260417668513E-15, 1.000000000000000000 ) ) ;
#93648 = ADVANCED_FACE ( 'NONE', ( #157073 ), #132422, .T. ) ;
#93649 = DIRECTION ( 'NONE',  ( 0.000000000000000000, 0.000000000000000000, -1.000000000000000000 ) ) ;
#93650 = EDGE_LOOP ( 'NONE', ( #129561, #94447, #256867, #32971 ) ) ;
#93651 = DIRECTION ( 'NONE',  ( 1.000000000000000000, -0.000000000000000000, 0.000000000000000000 ) ) ;
#93652 = ORIENTED_EDGE ( 'NONE', *, *, #252956, .T. ) ;
#93653 = CARTESIAN_POINT ( 'NONE',  ( 21.05000000000000071, 1.115600667400684642E-11, -167.5000000000000284 ) ) ;
#93654 = CARTESIAN_POINT ( 'NONE',  ( 18.39999999999997371, 11.75000000001113953, -76.25000000000004263 ) ) ;
#93655 = CIRCLE ( 'NONE', #6149, 0.09999999999999939493 ) ;
#93656 = ADVANCED_FACE ( 'NONE', ( #155802 ), #81333, .F. ) ;
#93657 = CIRCLE ( 'NONE', #176883, 0.09999999999999520384 ) ;
#93658 = AXIS2_PLACEMENT_3D ( 'NONE', #30629, #110134, #166298 ) ;
#93659 = EDGE_LOOP ( 'NONE', ( #112637, #143491, #111792, #99471 ) ) ;
#93660 = CARTESIAN_POINT ( 'NONE',  ( 18.52928932188133970, 65.72071067813062939, -111.8731074845243683 ) ) ;
#93661 = ORIENTED_EDGE ( 'NONE', *, *, #184577, .F. ) ;
#93662 = DIRECTION ( 'NONE',  ( 0.000000000000000000, -1.000000000000000000, -7.272083257015735086E-15 ) ) ;
#93663 = CARTESIAN_POINT ( 'NONE',  ( 21.09787244211741708, 67.22462929267473442, -124.2838541002068240 ) ) ;
#93665 = TOROIDAL_SURFACE ( 'NONE', #143555, 0.2000000000000000111, 0.1000000000000000056 ) ;
#93664 = CARTESIAN_POINT ( 'NONE',  ( -18.39999999999999858, -0.8467571797981087167, -242.2246066262668194 ) ) ;
#93667 = FACE_OUTER_BOUND ( 'NONE', #116317, .T. ) ;
#93666 = CIRCLE ( 'NONE', #22782, 0.1000000000000024342 ) ;
#93668 = CARTESIAN_POINT ( 'NONE',  ( 20.94999999999999929, 67.54115598404673904, -214.0823964242964053 ) ) ;
#93669 = DIRECTION ( 'NONE',  ( -0.7071067811865475727, -0.7071067811865475727, 0.000000000000000000 ) ) ;
#93670 = DIRECTION ( 'NONE',  ( 0.000000000000000000, 0.000000000000000000, 1.000000000000000000 ) ) ;
#93671 = LINE ( 'NONE', #12881, #162236 ) ;
#93673 = ORIENTED_EDGE ( 'NONE', *, *, #236449, .F. ) ;
#93672 = DIRECTION ( 'NONE',  ( 0.000000000000000000, 0.000000000000000000, 1.000000000000000000 ) ) ;
#93675 = FACE_OUTER_BOUND ( 'NONE', #149456, .T. ) ;
#93674 = DIRECTION ( 'NONE',  ( -0.000000000000000000, -0.9126074666063770380, -0.4088369013363281068 ) ) ;
#93676 = AXIS2_PLACEMENT_3D ( 'NONE', #226980, #49624, #127887 ) ;
#93677 = ORIENTED_EDGE ( 'NONE', *, *, #131899, .F. ) ;
#93679 = ORIENTED_EDGE ( 'NONE', *, *, #9599, .T. ) ;
#93678 = DIRECTION ( 'NONE',  ( -1.000000000000000000, -0.000000000000000000, -0.000000000000000000 ) ) ;
#93680 = ORIENTED_EDGE ( 'NONE', *, *, #15541, .T. ) ;
#93681 = FACE_OUTER_BOUND ( 'NONE', #163646, .T. ) ;
#93682 = DIRECTION ( 'NONE',  ( 1.000000000000000000, 0.000000000000000000, 0.000000000000000000 ) ) ;
#93683 = CIRCLE ( 'NONE', #239428, 0.09999999999999939493 ) ;
#93684 = AXIS2_PLACEMENT_3D ( 'NONE', #204262, #166469, #6065 ) ;
#93685 = CARTESIAN_POINT ( 'NONE',  ( 20.94999999999999929, 5.850000000011156942, -56.86750277572208034 ) ) ;
#93686 = DIRECTION ( 'NONE',  ( -4.336808689942017736E-16, 0.000000000000000000, -1.000000000000000000 ) ) ;
#93687 = DIRECTION ( 'NONE',  ( 0.000000000000000000, 0.9651348961776677893, -0.2617529984166795387 ) ) ;
#93688 = CIRCLE ( 'NONE', #197730, 14.30833333333333890 ) ;
#93689 = DIRECTION ( 'NONE',  ( 1.000000000000000000, 0.000000000000000000, 0.000000000000000000 ) ) ;
#93690 = VECTOR ( 'NONE', #29589, 1000.000000000000000 ) ;
#93691 = LINE ( 'NONE', #173283, #198774 ) ;
#93692 = ADVANCED_FACE ( 'NONE', ( #196183 ), #237876, .T. ) ;
#93693 = LINE ( 'NONE', #173285, #106144 ) ;
#93694 = ORIENTED_EDGE ( 'NONE', *, *, #20771, .F. ) ;
#93695 = ORIENTED_EDGE ( 'NONE', *, *, #186367, .F. ) ;
#93696 = DIRECTION ( 'NONE',  ( 0.000000000000000000, 0.000000000000000000, -1.000000000000000000 ) ) ;
#93697 = EDGE_LOOP ( 'NONE', ( #159594, #77472, #217876 ) ) ;
#93698 = CARTESIAN_POINT ( 'NONE',  ( -22.39999999999999858, 64.25000000001269029, -203.6231074845244393 ) ) ;
#93699 = ORIENTED_EDGE ( 'NONE', *, *, #81319, .T. ) ;
#93700 = CARTESIAN_POINT ( 'NONE',  ( 18.43630871534870508, -9.679800874802955590, -40.16063206798408913 ) ) ;
#93701 = DIRECTION ( 'NONE',  ( 0.000000000000000000, -1.156482317317873105E-15, -1.000000000000000000 ) ) ;
#93702 = DIRECTION ( 'NONE',  ( 1.000000000000000000, 0.000000000000000000, 0.000000000000000000 ) ) ;
#93703 = ADVANCED_FACE ( 'NONE', ( #98321 ), #177920, .F. ) ;
#93704 = DIRECTION ( 'NONE',  ( 1.186688945009009831E-16, -0.9770955615653316162, -0.2128009952263604232 ) ) ;
#93705 = LINE ( 'NONE', #148558, #137042 ) ;
#93706 = ORIENTED_EDGE ( 'NONE', *, *, #38643, .T. ) ;
#93707 = CARTESIAN_POINT ( 'NONE',  ( -20.94999999999999929, 35.94660524813657076, -234.4748257877825495 ) ) ;
#93708 = EDGE_CURVE ( 'NONE', #170273, #43771, #11630, .T. ) ;
#93709 = AXIS2_PLACEMENT_3D ( 'NONE', #208198, #49094, #205595 ) ;
#93710 = CARTESIAN_POINT ( 'NONE',  ( 18.59999999999999076, 10.20857864377385127, -192.1499999999999488 ) ) ;
#93711 = AXIS2_PLACEMENT_3D ( 'NONE', #114576, #35077, #234510 ) ;
#93712 = DIRECTION ( 'NONE',  ( 0.000000000000000000, 0.000000000000000000, -1.000000000000000000 ) ) ;
#93713 = DIRECTION ( 'NONE',  ( 0.000000000000000000, 0.000000000000000000, 1.000000000000000000 ) ) ;
#93714 = VECTOR ( 'NONE', #25729, 1000.000000000000000 ) ;
#93715 = ORIENTED_EDGE ( 'NONE', *, *, #145570, .F. ) ;
#93717 = DIRECTION ( 'NONE',  ( 0.000000000000000000, 0.8814952561688476074, -0.4721928772777262417 ) ) ;
#93716 = LINE ( 'NONE', #174603, #133407 ) ;
#93718 = ADVANCED_FACE ( 'NONE', ( #63081 ), #236456, .T. ) ;
#93719 = ORIENTED_EDGE ( 'NONE', *, *, #68262, .F. ) ;
#93722 = ORIENTED_EDGE ( 'NONE', *, *, #6954, .F. ) ;
#93721 = FACE_OUTER_BOUND ( 'NONE', #96809, .T. ) ;
#93720 = CARTESIAN_POINT ( 'NONE',  ( 22.60000000000000142, 1.115600667400684642E-11, -33.50000000000000000 ) ) ;
#93723 = CARTESIAN_POINT ( 'NONE',  ( -2.995603634470829482E-16, -11.74999999998884448, -91.75000000000005684 ) ) ;
#93724 = TOROIDAL_SURFACE ( 'NONE', #122953, 11.65000000000000036, 0.1000000000000000056 ) ;
#93725 = EDGE_CURVE ( 'NONE', #135298, #94156, #7503, .T. ) ;
#93726 = CARTESIAN_POINT ( 'NONE',  ( -22.49999999999999645, 64.25043287652226809, -69.62396585362311896 ) ) ;
#93727 = ORIENTED_EDGE ( 'NONE', *, *, #52025, .T. ) ;
#93728 = FACE_OUTER_BOUND ( 'NONE', #247619, .T. ) ;
#93729 = EDGE_CURVE ( 'NONE', #73041, #48943, #232396, .T. ) ;
#93730 = CARTESIAN_POINT ( 'NONE',  ( -23.15000000000000213, 78.50726470275243685, -228.6618886302502176 ) ) ;
#93731 = EDGE_CURVE ( 'NONE', #43405, #7066, #119980, .T. ) ;
#93733 = ORIENTED_EDGE ( 'NONE', *, *, #191823, .T. ) ;
#93732 = DIRECTION ( 'NONE',  ( 0.000000000000000000, 0.000000000000000000, 1.000000000000000000 ) ) ;
#93734 = VECTOR ( 'NONE', #82575, 1000.000000000000000 ) ;
#93735 = EDGE_CURVE ( 'NONE', #125917, #44661, #161469, .T. ) ;
#93736 = CIRCLE ( 'NONE', #239497, 0.09999999999999939493 ) ;
#93737 = ORIENTED_EDGE ( 'NONE', *, *, #118401, .F. ) ;
#93738 = CYLINDRICAL_SURFACE ( 'NONE', #95348, 0.09999999999999939493 ) ;
#93739 = CARTESIAN_POINT ( 'NONE',  ( -23.25000000000000355, 11.75000000001113953, -46.15000000000000568 ) ) ;
#93740 = CARTESIAN_POINT ( 'NONE',  ( 21.05000000000000071, 9.307299318941717914, -220.9418877738490039 ) ) ;
#93741 = DIRECTION ( 'NONE',  ( -0.5932847527679309119, -0.7769265190100942409, 0.2107092456252278867 ) ) ;
#93742 = VERTEX_POINT ( 'NONE', #202604 ) ;
#93743 = DIRECTION ( 'NONE',  ( 0.000000000000000000, -0.1350103645451557199, -0.9908441862701644620 ) ) ;
#93744 = DIRECTION ( 'NONE',  ( 0.000000000000000000, 0.000000000000000000, 1.000000000000000000 ) ) ;
#93745 = CIRCLE ( 'NONE', #23044, 0.09999999999999954758 ) ;
#93746 = ORIENTED_EDGE ( 'NONE', *, *, #162870, .T. ) ;
#93747 = CARTESIAN_POINT ( 'NONE',  ( 20.22483756094572271, 60.19120353999515771, -225.5122212141894522 ) ) ;
#93748 = EDGE_CURVE ( 'NONE', #50255, #99797, #153302, .T. ) ;
#93749 = CARTESIAN_POINT ( 'NONE',  ( -22.39999999999999858, 1.115600667400684642E-11, -167.4999999999999716 ) ) ;
#93750 = ORIENTED_EDGE ( 'NONE', *, *, #29048, .F. ) ;
#93751 = DIRECTION ( 'NONE',  ( -0.000000000000000000, 0.4088369013363282733, -0.9126074666063769270 ) ) ;
#93752 = ORIENTED_EDGE ( 'NONE', *, *, #71245, .T. ) ;
#93753 = CIRCLE ( 'NONE', #202102, 2.000000000000002665 ) ;
#93754 = ORIENTED_EDGE ( 'NONE', *, *, #221006, .F. ) ;
#93755 = EDGE_CURVE ( 'NONE', #154754, #159944, #82616, .T. ) ;
#93756 = CARTESIAN_POINT ( 'NONE',  ( 20.94999999999999574, 67.07338541492521244, -161.5514244653012952 ) ) ;
#93757 = ORIENTED_EDGE ( 'NONE', *, *, #160543, .T. ) ;
#93759 = ORIENTED_EDGE ( 'NONE', *, *, #181674, .F. ) ;
#93758 = CARTESIAN_POINT ( 'NONE',  ( 18.49999999999999289, 7.120270961708750512, -70.65956304183931991 ) ) ;
#93762 = ORIENTED_EDGE ( 'NONE', *, *, #115998, .F. ) ;
#93761 = VERTEX_POINT ( 'NONE', #224716 ) ;
#93760 = DIRECTION ( 'NONE',  ( 0.000000000000000000, 0.000000000000000000, -1.000000000000000000 ) ) ;
#93763 = CARTESIAN_POINT ( 'NONE',  ( -21.05000000000000071, 87.75000000001247713, -172.9231074845242802 ) ) ;
#93764 = DIRECTION ( 'NONE',  ( -0.000000000000000000, -6.982962677686266711E-15, 1.000000000000000000 ) ) ;
#93765 = CARTESIAN_POINT ( 'NONE',  ( 21.07888907270776002, 10.72506921352637654, -112.7211935868332375 ) ) ;
#93766 = VECTOR ( 'NONE', #12396, 1000.000000000000000 ) ;
#93767 = DIRECTION ( 'NONE',  ( 1.000000000000000000, 0.000000000000000000, 0.000000000000000000 ) ) ;
#93768 = EDGE_CURVE ( 'NONE', #185160, #33839, #15924, .T. ) ;
#93769 = DIRECTION ( 'NONE',  ( 0.000000000000000000, 1.000000000000000000, 0.000000000000000000 ) ) ;
#93770 = FACE_OUTER_BOUND ( 'NONE', #82884, .T. ) ;
#93771 = ORIENTED_EDGE ( 'NONE', *, *, #117380, .T. ) ;
#93772 = ORIENTED_EDGE ( 'NONE', *, *, #178854, .F. ) ;
#93773 = ORIENTED_EDGE ( 'NONE', *, *, #184687, .F. ) ;
#93774 = CIRCLE ( 'NONE', #177026, 0.3999999999999975797 ) ;
#93776 = VERTEX_POINT ( 'NONE', #163478 ) ;
#93775 = CARTESIAN_POINT ( 'NONE',  ( -16.93234230245722216, 66.00189262946545909, -182.6054172028581775 ) ) ;
#93777 = VERTEX_POINT ( 'NONE', #206454 ) ;
#93778 = EDGE_CURVE ( 'NONE', #110538, #153266, #203878, .T. ) ;
#93779 = ORIENTED_EDGE ( 'NONE', *, *, #86643, .T. ) ;
#93780 = CARTESIAN_POINT ( 'NONE',  ( 23.14999999999999858, 7.128833340094563376, -233.7327013124401276 ) ) ;
#93781 = ADVANCED_FACE ( 'NONE', ( #106041 ), #184311, .T. ) ;
#93782 = ADVANCED_FACE ( 'NONE', ( #160925 ), #169879, .F. ) ;
#93783 = VERTEX_POINT ( 'NONE', #186920 ) ;
#93784 = LINE ( 'NONE', #155088, #239593 ) ;
#93785 = CARTESIAN_POINT ( 'NONE',  ( -20.54999999999999716, -8.663551401869156621, -23.97589888193269658 ) ) ;
#93786 = EDGE_CURVE ( 'NONE', #24784, #137793, #201314, .T. ) ;
#93789 = ORIENTED_EDGE ( 'NONE', *, *, #158900, .T. ) ;
#93788 = ORIENTED_EDGE ( 'NONE', *, *, #150414, .F. ) ;
#93787 = CIRCLE ( 'NONE', #18959, 0.1000000000000000472 ) ;
#93790 = AXIS2_PLACEMENT_3D ( 'NONE', #45476, #42916, #67602 ) ;
#93791 = ORIENTED_EDGE ( 'NONE', *, *, #220100, .F. ) ;
#93792 = DIRECTION ( 'NONE',  ( 0.000000000000000000, -1.000000000000000000, 0.000000000000000000 ) ) ;
#93793 = ORIENTED_EDGE ( 'NONE', *, *, #96264, .T. ) ;
#93794 = ORIENTED_EDGE ( 'NONE', *, *, #34464, .F. ) ;
#93795 = EDGE_CURVE ( 'NONE', #144818, #9346, #157392, .T. ) ;
#93796 = DIRECTION ( 'NONE',  ( 1.875376730785737719E-16, 1.000000000000000000, 6.982962677686266711E-15 ) ) ;
#93798 = ORIENTED_EDGE ( 'NONE', *, *, #252388, .F. ) ;
#93797 = CARTESIAN_POINT ( 'NONE',  ( 18.41832399655374175, -9.682403266662738872, -107.1568436200277006 ) ) ;
#93799 = DIRECTION ( 'NONE',  ( 1.000000000000000000, 0.000000000000000000, 0.000000000000000000 ) ) ;
#93801 = DIRECTION ( 'NONE',  ( 1.000000000000000000, 0.000000000000000000, 0.000000000000000000 ) ) ;
#93800 = CARTESIAN_POINT ( 'NONE',  ( -23.15000000000000213, 85.00000000001232081, -160.1291383618718385 ) ) ;
#93802 = CARTESIAN_POINT ( 'NONE',  ( 20.94999999999999929, -11.39257802169451317, -130.9260504201681101 ) ) ;
#93803 = CARTESIAN_POINT ( 'NONE',  ( -22.39999999999999858, 76.10085836911147794, -215.2726746080137445 ) ) ;
#93804 = CARTESIAN_POINT ( 'NONE',  ( 21.07928932188134397, 30.84304088367083097, -252.0482413927653340 ) ) ;
#93805 = ORIENTED_EDGE ( 'NONE', *, *, #197196, .T. ) ;
#93806 = ORIENTED_EDGE ( 'NONE', *, *, #17941, .F. ) ;
#93807 = DIRECTION ( 'NONE',  ( -0.000000000000000000, -6.982962677686266711E-15, 1.000000000000000000 ) ) ;
#93808 = CARTESIAN_POINT ( 'NONE',  ( -22.39999999999999858, -0.1008583690875579364, -122.2504328765106294 ) ) ;
#93809 = FACE_OUTER_BOUND ( 'NONE', #14352, .T. ) ;
#93810 = CIRCLE ( 'NONE', #218695, 0.09999999999999864553 ) ;
#93811 = VERTEX_POINT ( 'NONE', #220869 ) ;
#93812 = DIRECTION ( 'NONE',  ( 1.000000000000000000, 0.000000000000000000, 0.000000000000000000 ) ) ;
#93813 = VECTOR ( 'NONE', #247638, 1000.000000000000000 ) ;
#93814 = VECTOR ( 'NONE', #192062, 1000.000000000000000 ) ;
#93815 = CIRCLE ( 'NONE', #60485, 0.1000000000000028644 ) ;
#93816 = EDGE_CURVE ( 'NONE', #228990, #46891, #42254, .T. ) ;
#93817 = CARTESIAN_POINT ( 'NONE',  ( 23.24999999999999645, 0.000000000000000000, 0.000000000000000000 ) ) ;
#93818 = DIRECTION ( 'NONE',  ( 0.000000000000000000, -2.771150684185008344E-14, -1.000000000000000000 ) ) ;
#93819 = ORIENTED_EDGE ( 'NONE', *, *, #90860, .F. ) ;
#93820 = VERTEX_POINT ( 'NONE', #222131 ) ;
#93821 =( GEOMETRIC_REPRESENTATION_CONTEXT ( 3 ) GLOBAL_UNCERTAINTY_ASSIGNED_CONTEXT ( ( #256526 ) ) GLOBAL_UNIT_ASSIGNED_CONTEXT ( ( #102480, #40013, #25561 ) ) REPRESENTATION_CONTEXT ( 'NONE', 'WORKASPACE' ) );
#93822 = FACE_OUTER_BOUND ( 'NONE', #667, .T. ) ;
#93823 = DIRECTION ( 'NONE',  ( -1.000000000000000000, -0.000000000000000000, -0.000000000000000000 ) ) ;
#93825 = EDGE_CURVE ( 'NONE', #13346, #74153, #85139, .T. ) ;
#93824 = ORIENTED_EDGE ( 'NONE', *, *, #72631, .F. ) ;
#93826 = DIRECTION ( 'NONE',  ( 0.000000000000000000, 0.000000000000000000, 1.000000000000000000 ) ) ;
#93827 = VERTEX_POINT ( 'NONE', #33005 ) ;
#93828 = EDGE_CURVE ( 'NONE', #253877, #68201, #133345, .T. ) ;
#93829 = DIRECTION ( 'NONE',  ( -0.000000000000000000, 1.000000000000000000, -1.224646799147352961E-16 ) ) ;
#93830 = DIRECTION ( 'NONE',  ( 0.000000000000000000, 1.000000000000000000, 0.000000000000000000 ) ) ;
#93832 = DIRECTION ( 'NONE',  ( -1.000000000000000000, 0.000000000000000000, -0.000000000000000000 ) ) ;
#93831 = DIRECTION ( 'NONE',  ( 0.000000000000000000, 1.000000000000000000, 6.982962677686266711E-15 ) ) ;
#93833 = CARTESIAN_POINT ( 'NONE',  ( -21.05000000000000071, 74.83729825007388570, -94.92310748452432279 ) ) ;
#93834 = CARTESIAN_POINT ( 'NONE',  ( 18.59117750673696534, 65.66751761918722252, -164.4282609406112670 ) ) ;
#93835 = DIRECTION ( 'NONE',  ( 1.000000000000000000, -0.000000000000000000, 0.000000000000000000 ) ) ;
#93836 = ADVANCED_FACE ( 'NONE', ( #212882 ), #89060, .F. ) ;
#93838 = ORIENTED_EDGE ( 'NONE', *, *, #99018, .F. ) ;
#93837 = CARTESIAN_POINT ( 'NONE',  ( -20.85000000000000142, 68.97833521811131163, -32.18954208262707795 ) ) ;
#93839 = AXIS2_PLACEMENT_3D ( 'NONE', #161440, #221367, #141844 ) ;
#93840 = AXIS2_PLACEMENT_3D ( 'NONE', #202194, #1405, #143492 ) ;
#93842 = ORIENTED_EDGE ( 'NONE', *, *, #10989, .F. ) ;
#93841 = ORIENTED_EDGE ( 'NONE', *, *, #195029, .T. ) ;
#93843 = ORIENTED_EDGE ( 'NONE', *, *, #40839, .F. ) ;
#93844 = CIRCLE ( 'NONE', #122899, 0.1000000000000028644 ) ;
#93845 = DIRECTION ( 'NONE',  ( 0.000000000000000000, 0.000000000000000000, 1.000000000000000000 ) ) ;
#93846 = DIRECTION ( 'NONE',  ( 0.000000000000000000, 0.4088369013363229998, -0.9126074666063793694 ) ) ;
#93847 = FACE_OUTER_BOUND ( 'NONE', #60520, .T. ) ;
#93849 = CARTESIAN_POINT ( 'NONE',  ( -22.57320508075687115, 11.75000000001115552, -33.50000000000002842 ) ) ;
#93848 = CARTESIAN_POINT ( 'NONE',  ( 18.59999999999999076, 69.55000000001253113, -182.3731074845244109 ) ) ;
#93850 = DIRECTION ( 'NONE',  ( 0.000000000000000000, 0.8814952561688476074, -0.4721928772777262417 ) ) ;
#93851 = EDGE_LOOP ( 'NONE', ( #23173, #91358, #118953, #55254 ) ) ;
#93852 = CIRCLE ( 'NONE', #43776, 0.1000000000000028644 ) ;
#93853 = DIRECTION ( 'NONE',  ( -0.000000000000000000, 0.7397360091702694929, 0.6728971962616898672 ) ) ;
#93854 = AXIS2_PLACEMENT_3D ( 'NONE', #92055, #38218, #29556 ) ;
#93855 = VECTOR ( 'NONE', #218195, 1000.000000000000000 ) ;
#93856 = ORIENTED_EDGE ( 'NONE', *, *, #227888, .F. ) ;
#93858 = ADVANCED_FACE ( 'NONE', ( #189467 ), #57382, .T. ) ;
#93857 = ORIENTED_EDGE ( 'NONE', *, *, #87543, .F. ) ;
#93859 = DIRECTION ( 'NONE',  ( 0.000000000000000000, 0.000000000000000000, -1.000000000000000000 ) ) ;
#93860 = DIRECTION ( 'NONE',  ( 1.186688945009009831E-16, 0.9651348961777157509, -0.2617529984165031243 ) ) ;
#93861 = CARTESIAN_POINT ( 'NONE',  ( 22.00356870071856363, 76.00000000003105072, -210.7773498462513260 ) ) ;
#93862 = DIRECTION ( 'NONE',  ( 0.000000000000000000, -0.9342891509276819439, -0.3565161741896589742 ) ) ;
#93863 = CIRCLE ( 'NONE', #239620, 0.1000000000000001860 ) ;
#93864 = DIRECTION ( 'NONE',  ( -1.000000000000000000, 0.000000000000000000, 0.000000000000000000 ) ) ;
#93865 = VERTEX_POINT ( 'NONE', #229875 ) ;
#93866 = EDGE_LOOP ( 'NONE', ( #165686, #185521, #235543, #13205 ) ) ;
#93867 = AXIS2_PLACEMENT_3D ( 'NONE', #20019, #77384, #156966 ) ;
#93868 = FACE_OUTER_BOUND ( 'NONE', #85314, .T. ) ;
#93869 = CARTESIAN_POINT ( 'NONE',  ( 18.49999999999999289, 69.15387683765909799, -65.78538121767449809 ) ) ;
#93870 = PLANE ( 'NONE',  #218789 ) ;
#93871 = FACE_OUTER_BOUND ( 'NONE', #97854, .T. ) ;
#93872 = AXIS2_PLACEMENT_3D ( 'NONE', #108394, #250459, #86226 ) ;
#93873 = CARTESIAN_POINT ( 'NONE',  ( -20.94999999999999929, 76.00000000001267608, -203.5231074845243597 ) ) ;
#93874 = AXIS2_PLACEMENT_3D ( 'NONE', #20277, #222280, #238016 ) ;
#93875 = FACE_OUTER_BOUND ( 'NONE', #38910, .T. ) ;
#93876 = CARTESIAN_POINT ( 'NONE',  ( 23.14999999999999858, 71.18691588786276725, -158.0815897280005800 ) ) ;
#93877 = EDGE_CURVE ( 'NONE', #73136, #154872, #124051, .T. ) ;
#93879 = DIRECTION ( 'NONE',  ( 0.000000000000000000, 0.000000000000000000, 1.000000000000000000 ) ) ;
#93878 = LINE ( 'NONE', #113443, #182789 ) ;
#93880 = DIRECTION ( 'NONE',  ( 0.000000000000000000, 0.000000000000000000, 1.000000000000000000 ) ) ;
#93881 = CYLINDRICAL_SURFACE ( 'NONE', #162516, 11.74999999999999645 ) ;
#93883 = ADVANCED_FACE ( 'NONE', ( #10829 ), #78238, .T. ) ;
#93882 = DIRECTION ( 'NONE',  ( 1.000000000000000000, 1.394253735153569469E-16, 2.602809386958778209E-16 ) ) ;
#93884 = FACE_OUTER_BOUND ( 'NONE', #136415, .T. ) ;
#93886 = ORIENTED_EDGE ( 'NONE', *, *, #92233, .F. ) ;
#93885 = DIRECTION ( 'NONE',  ( -1.000000000000000000, 0.000000000000000000, -0.000000000000000000 ) ) ;
#93887 = EDGE_CURVE ( 'NONE', #62504, #29706, #32499, .T. ) ;
#93888 = EDGE_CURVE ( 'NONE', #78587, #253474, #65774, .T. ) ;
#93889 = SPHERICAL_SURFACE ( 'NONE', #220056, 0.1000000000000000056 ) ;
#93891 = CIRCLE ( 'NONE', #164824, 0.1000000000000028644 ) ;
#93890 = CARTESIAN_POINT ( 'NONE',  ( -22.48660254037843487, 64.35000000001194564, -103.0731074845243711 ) ) ;
#93892 = CIRCLE ( 'NONE', #135574, 0.5000000000000004441 ) ;
#93893 = DIRECTION ( 'NONE',  ( -1.000000000000000000, -0.000000000000000000, 0.000000000000000000 ) ) ;
#93894 = TOROIDAL_SURFACE ( 'NONE', #106523, 11.65000000000000036, 0.1000000000000000056 ) ;
#93895 = CARTESIAN_POINT ( 'NONE',  ( 15.31784899511109899, 9.396630376328872103, -84.90705739281834497 ) ) ;
#93896 = DIRECTION ( 'NONE',  ( 0.000000000000000000, 0.000000000000000000, 1.000000000000000000 ) ) ;
#93897 = ADVANCED_FACE ( 'NONE', ( #52497 ), #7714, .T. ) ;
#93898 = CARTESIAN_POINT ( 'NONE',  ( 18.59999999999999787, 77.83534155023700407, -191.9679561919613491 ) ) ;
#93899 = ADVANCED_FACE ( 'NONE', ( #167357 ), #246851, .T. ) ;
#93900 = LINE ( 'NONE', #173504, #19811 ) ;
#93901 = CARTESIAN_POINT ( 'NONE',  ( 23.14999999999999503, 57.93055674131822741, -245.5071546967800771 ) ) ;
#93902 = AXIS2_PLACEMENT_3D ( 'NONE', #217532, #195451, #78034 ) ;
#93903 = AXIS2_PLACEMENT_3D ( 'NONE', #81977, #221503, #161575 ) ;
#93904 = ORIENTED_EDGE ( 'NONE', *, *, #80925, .F. ) ;
#93905 = CARTESIAN_POINT ( 'NONE',  ( -20.94999999999999929, -1.835341550213257733, -45.05515129256298223 ) ) ;
#93907 = ORIENTED_EDGE ( 'NONE', *, *, #131151, .T. ) ;
#93906 = DIRECTION ( 'NONE',  ( -1.000000000000000000, -0.000000000000000000, 0.000000000000000000 ) ) ;
#93908 = CARTESIAN_POINT ( 'NONE',  ( -23.25000000000000000, 1.115600667400684642E-11, -167.5000000000000284 ) ) ;
#93909 = CARTESIAN_POINT ( 'NONE',  ( 20.94999999999999574, 1.851028230152016674, -112.1539132694225316 ) ) ;
#93910 = DIRECTION ( 'NONE',  ( 0.000000000000000000, 0.000000000000000000, 1.000000000000000000 ) ) ;
#93911 = VECTOR ( 'NONE', #162141, 1000.000000000000000 ) ;
#93912 = ORIENTED_EDGE ( 'NONE', *, *, #148686, .T. ) ;
#93913 = CARTESIAN_POINT ( 'NONE',  ( -16.82055514392402173, 66.05000000001263061, -190.8463094099826378 ) ) ;
#93914 = AXIS2_PLACEMENT_3D ( 'NONE', #10167, #11459, #208382 ) ;
#93915 = PRODUCT_CONTEXT ( 'NONE', #198973, 'mechanical' ) ;
#93916 = EDGE_CURVE ( 'NONE', #102952, #58722, #174335, .T. ) ;
#93917 = CARTESIAN_POINT ( 'NONE',  ( 22.49533356619853564, 11.36930514850300611, -198.4572374200820093 ) ) ;
#93918 = CARTESIAN_POINT ( 'NONE',  ( 22.40000000000010516, -2.500503813845274870, -189.5187041743088230 ) ) ;
#93919 = AXIS2_PLACEMENT_3D ( 'NONE', #11658, #109437, #151163 ) ;
#93920 = VERTEX_POINT ( 'NONE', #111210 ) ;
#93921 = CARTESIAN_POINT ( 'NONE',  ( 21.14999999999999858, 11.65000000001116298, -45.65000000000000568 ) ) ;
#93922 = DIRECTION ( 'NONE',  ( 0.000000000000000000, 0.2617529984164506107, 0.9651348961777299618 ) ) ;
#93923 = EDGE_CURVE ( 'NONE', #206022, #231849, #165940, .T. ) ;
#93924 = CARTESIAN_POINT ( 'NONE',  ( 20.95483826173900255, 8.876166204781142710, -176.0462755528994876 ) ) ;
#93925 = ORIENTED_EDGE ( 'NONE', *, *, #149064, .F. ) ;
#93926 = AXIS2_PLACEMENT_3D ( 'NONE', #38289, #175265, #235203 ) ;
#93927 = EDGE_LOOP ( 'NONE', ( #23012, #49955, #227460, #213618 ) ) ;
#93928 = ADVANCED_FACE ( 'NONE', ( #68230 ), #171230, .T. ) ;
#93929 = CARTESIAN_POINT ( 'NONE',  ( -20.64999999999999858, 68.75000000001151079, -48.27310748452437394 ) ) ;
#93930 = DIRECTION ( 'NONE',  ( 0.000000000000000000, -7.429790795770644761E-15, 1.000000000000000000 ) ) ;
#93931 = CARTESIAN_POINT ( 'NONE',  ( -16.87036670365548474, 14.22508806334145959, -219.3732768077300932 ) ) ;
#93932 = CARTESIAN_POINT ( 'NONE',  ( -22.39999999999999858, 68.20922040163854660, -103.0231074845243739 ) ) ;
#93934 = CARTESIAN_POINT ( 'NONE',  ( 22.50000000000000000, -2.381330705637465961, -189.5959759702857923 ) ) ;
#93933 = DIRECTION ( 'NONE',  ( 0.000000000000000000, -1.000000000000000000, -6.982962677686265922E-15 ) ) ;
#93935 = EDGE_CURVE ( 'NONE', #131400, #159106, #128499, .T. ) ;
#93936 = CYLINDRICAL_SURFACE ( 'NONE', #40229, 0.5000000000000007772 ) ;
#93937 = DIRECTION ( 'NONE',  ( 1.000000000000000000, 0.000000000000000000, 0.000000000000000000 ) ) ;
#93938 = CARTESIAN_POINT ( 'NONE',  ( -18.47140463609785499, 87.08089277388562266, -199.6145310103756003 ) ) ;
#93939 = LINE ( 'NONE', #169678, #76365 ) ;
#93940 = EDGE_LOOP ( 'NONE', ( #206748, #79394, #127450, #186183 ) ) ;
#93941 = CIRCLE ( 'NONE', #218822, 0.1999999999999987899 ) ;
#93942 = ORIENTED_EDGE ( 'NONE', *, *, #79782, .F. ) ;
#93943 = DIRECTION ( 'NONE',  ( 1.000000000000000000, -0.000000000000000000, 0.000000000000000000 ) ) ;
#93944 = DIRECTION ( 'NONE',  ( 0.000000000000000000, -6.652207440891554563E-15, 1.000000000000000000 ) ) ;
#93946 = CARTESIAN_POINT ( 'NONE',  ( 5.900000000000060751, 64.35000000001120668, -21.92310748452479174 ) ) ;
#93945 = DIRECTION ( 'NONE',  ( 1.000000000000000000, -1.207181226542539700E-16, 2.694675058168174199E-16 ) ) ;
#93947 = ORIENTED_EDGE ( 'NONE', *, *, #108553, .F. ) ;
#93948 = DIRECTION ( 'NONE',  ( 0.000000000000000000, 0.9994937237965558774, 0.03181660087586650476 ) ) ;
#93949 = DIRECTION ( 'NONE',  ( 0.000000000000000000, 0.9126074666063804797, 0.4088369013363203908 ) ) ;
#93950 = EDGE_CURVE ( 'NONE', #245468, #18434, #49197, .T. ) ;
#93951 = LINE ( 'NONE', #251747, #161936 ) ;
#93952 = CARTESIAN_POINT ( 'NONE',  ( 13.54577453029515510, 13.15902077901803402, -217.0103513519799776 ) ) ;
#93953 = ORIENTED_EDGE ( 'NONE', *, *, #241839, .T. ) ;
#93954 = ORIENTED_EDGE ( 'NONE', *, *, #121323, .T. ) ;
#93955 = DIRECTION ( 'NONE',  ( 0.000000000000000000, 0.9893560106964510714, -0.1455152366551481502 ) ) ;
#93956 = ORIENTED_EDGE ( 'NONE', *, *, #40616, .F. ) ;
#93957 = CARTESIAN_POINT ( 'NONE',  ( 20.85000000000000142, 77.83585931145546510, -91.51866831572576189 ) ) ;
#93958 = CIRCLE ( 'NONE', #135645, 0.1000000000000007550 ) ;
#93959 = CARTESIAN_POINT ( 'NONE',  ( 20.94999999999999574, 87.39257802171731271, -66.44915790469229933 ) ) ;
#93960 = CARTESIAN_POINT ( 'NONE',  ( 21.72449340488910252, 20.13867536412185189, -229.0352267540020819 ) ) ;
#93961 = VECTOR ( 'NONE', #228995, 1000.000000000000000 ) ;
#93962 = EDGE_LOOP ( 'NONE', ( #141843, #7832, #133189, #193627 ) ) ;
#93963 = CARTESIAN_POINT ( 'NONE',  ( -16.92507428761701505, 9.949999999999983302, -12.71339745962155909 ) ) ;
#93964 = FACE_OUTER_BOUND ( 'NONE', #168672, .T. ) ;
#93965 = CARTESIAN_POINT ( 'NONE',  ( -20.94999999999999929, 1.750000000011155743, -145.6695115579016715 ) ) ;
#93966 = DIRECTION ( 'NONE',  ( 0.7071067811865486830, -0.1850873201762207598, -0.6824534298470361637 ) ) ;
#93967 = CARTESIAN_POINT ( 'NONE',  ( 21.13435531349745844, 65.53152359378273673, -242.1224433109954930 ) ) ;
#93969 = CARTESIAN_POINT ( 'NONE',  ( -23.15000000000000213, 76.00000000001216449, -140.5731074845242858 ) ) ;
#93968 = CARTESIAN_POINT ( 'NONE',  ( 23.14999999999999503, 6.650000000011155876, -179.7499999999999716 ) ) ;
#93970 = CARTESIAN_POINT ( 'NONE',  ( -20.54999999999999361, 11.65000000001115232, -155.3500000000000227 ) ) ;
#93971 = ORIENTED_EDGE ( 'NONE', *, *, #199661, .T. ) ;
#93973 = CYLINDRICAL_SURFACE ( 'NONE', #114183, 0.09999999999999939493 ) ;
#93972 = CYLINDRICAL_SURFACE ( 'NONE', #3470, 0.1000000000000028644 ) ;
#93974 = EDGE_LOOP ( 'NONE', ( #68323, #51784, #136272, #8608 ) ) ;
#93975 = ORIENTED_EDGE ( 'NONE', *, *, #73659, .T. ) ;
#93976 = CIRCLE ( 'NONE', #173149, 11.65000000000000036 ) ;
#93977 = EDGE_LOOP ( 'NONE', ( #197702, #110081 ) ) ;
#93978 = AXIS2_PLACEMENT_3D ( 'NONE', #99978, #239531, #41352 ) ;
#93979 = CARTESIAN_POINT ( 'NONE',  ( -18.38204789744325396, 11.47950103717623982, -91.25000000000005684 ) ) ;
#93980 = CARTESIAN_POINT ( 'NONE',  ( 15.66039659514496130, 66.63925083009715422, -152.7085373439171860 ) ) ;
#93981 = CARTESIAN_POINT ( 'NONE',  ( -18.40000000000000213, 11.47316190337364183, -188.4499999999999886 ) ) ;
#93982 = DIRECTION ( 'NONE',  ( 0.000000000000000000, -4.163336342344333240E-14, -1.000000000000000000 ) ) ;
#93983 = ORIENTED_EDGE ( 'NONE', *, *, #50924, .T. ) ;
#93984 = CYLINDRICAL_SURFACE ( 'NONE', #155819, 0.09999999999999976963 ) ;
#93985 = DIRECTION ( 'NONE',  ( 0.000000000000000000, 0.1335171055202867274, 0.9910465087640866200 ) ) ;
#93986 = VERTEX_POINT ( 'NONE', #55058 ) ;
#93987 = CARTESIAN_POINT ( 'NONE',  ( 20.94999999999999574, 76.00000000001213607, -136.5231074845242745 ) ) ;
#93988 = EDGE_CURVE ( 'NONE', #44800, #75249, #49399, .T. ) ;
#93990 = VECTOR ( 'NONE', #184721, 1000.000000000000227 ) ;
#93989 = DIRECTION ( 'NONE',  ( 1.000000000000000000, 0.000000000000000000, 0.000000000000000000 ) ) ;
#93991 = VERTEX_POINT ( 'NONE', #134595 ) ;
#93993 = DIRECTION ( 'NONE',  ( 0.000000000000000000, -0.9126074666063769270, -0.4088369013363280513 ) ) ;
#93992 = CIRCLE ( 'NONE', #10627, 0.1000000000000028644 ) ;
#93994 = TOROIDAL_SURFACE ( 'NONE', #27409, 4.149999999999999467, 0.1000000000000000056 ) ;
#93995 = CIRCLE ( 'NONE', #248127, 4.049999999999995381 ) ;
#93996 = ORIENTED_EDGE ( 'NONE', *, *, #112672, .F. ) ;
#93997 = CARTESIAN_POINT ( 'NONE',  ( 18.51697539158856642, 65.68434038414355314, -97.48668807260654035 ) ) ;
#93998 = EDGE_LOOP ( 'NONE', ( #103911, #89122, #68648, #108336 ) ) ;
#93999 = CARTESIAN_POINT ( 'NONE',  ( -22.57848426163147693, 76.00426432929559439, -181.7731657914146979 ) ) ;
#94000 =( GEOMETRIC_REPRESENTATION_CONTEXT ( 3 ) GLOBAL_UNCERTAINTY_ASSIGNED_CONTEXT ( ( #37559 ) ) GLOBAL_UNIT_ASSIGNED_CONTEXT ( ( #240756, #162510, #122088 ) ) REPRESENTATION_CONTEXT ( 'NONE', 'WORKASPACE' ) );
#94001 = CARTESIAN_POINT ( 'NONE',  ( 21.05000000000000071, 85.00000000001179501, -79.01707660717669057 ) ) ;
#94002 = CARTESIAN_POINT ( 'NONE',  ( 18.79999999999999716, 10.88519226655716565, -15.14794223642649840 ) ) ;
#94003 = CYLINDRICAL_SURFACE ( 'NONE', #220269, 0.5000000000000004441 ) ;
#94004 = ADVANCED_FACE ( 'NONE', ( #195898 ), #14706, .F. ) ;
#94005 = CARTESIAN_POINT ( 'NONE',  ( 20.94999999999999929, 76.00000000001244871, -170.0231074845243597 ) ) ;
#94006 = CARTESIAN_POINT ( 'NONE',  ( 18.46932045258646937, -9.670685200254602876, -73.67386037299664281 ) ) ;
#94007 = DIRECTION ( 'NONE',  ( 0.000000000000000000, -0.8660254037844411501, -0.4999999999999956146 ) ) ;
#94008 = VERTEX_POINT ( 'NONE', #98027 ) ;
#94010 = CARTESIAN_POINT ( 'NONE',  ( 23.14999999999999503, 69.35000000001200249, -115.2731074845243455 ) ) ;
#94009 = CARTESIAN_POINT ( 'NONE',  ( -18.39999999999999858, 11.75000000001113953, -76.25000000000004263 ) ) ;
#94011 = AXIS2_PLACEMENT_3D ( 'NONE', #240641, #101075, #120724 ) ;
#94012 = ORIENTED_EDGE ( 'NONE', *, *, #58408, .T. ) ;
#94015 = ORIENTED_EDGE ( 'NONE', *, *, #46866, .F. ) ;
#94014 = LINE ( 'NONE', #78300, #162895 ) ;
#94013 = DIRECTION ( 'NONE',  ( -1.000000000000000000, 7.510212038922846022E-17, -1.676432719286211941E-16 ) ) ;
#94016 = ORIENTED_EDGE ( 'NONE', *, *, #111284, .F. ) ;
#94017 = DIRECTION ( 'NONE',  ( -1.000000000000000000, -0.000000000000000000, -0.000000000000000000 ) ) ;
#94018 = AXIS2_PLACEMENT_3D ( 'NONE', #207257, #108142, #72894 ) ;
#94019 = FACE_OUTER_BOUND ( 'NONE', #208924, .T. ) ;
#94020 = DIRECTION ( 'NONE',  ( 1.000000000000000000, 0.000000000000000000, 0.000000000000000000 ) ) ;
#94021 = ADVANCED_FACE ( 'NONE', ( #253270 ), #173808, .T. ) ;
#94022 = CARTESIAN_POINT ( 'NONE',  ( 21.00000000000000000, 11.49641995933507843, 1.885425182446133885 ) ) ;
#94023 = EDGE_LOOP ( 'NONE', ( #87002, #78131, #61414, #153086 ) ) ;
#94025 = ORIENTED_EDGE ( 'NONE', *, *, #45943, .F. ) ;
#94024 = CARTESIAN_POINT ( 'NONE',  ( -16.87786941232800686, 66.04184528586702640, -115.6459216847303537 ) ) ;
#94026 = EDGE_CURVE ( 'NONE', #186401, #240710, #237580, .T. ) ;
#94027 = AXIS2_PLACEMENT_3D ( 'NONE', #141136, #242780, #143684 ) ;
#94028 = AXIS2_PLACEMENT_3D ( 'NONE', #10320, #225472, #230644 ) ;
#94029 = ADVANCED_FACE ( 'NONE', ( #215438 ), #95183, .T. ) ;
#94031 = DIRECTION ( 'NONE',  ( -0.000000000000000000, 0.9942466578594195692, -0.1071148137998398919 ) ) ;
#94030 = DIRECTION ( 'NONE',  ( 0.000000000000000000, 0.2128009952263603677, -0.9770955615653313941 ) ) ;
#94032 = AXIS2_PLACEMENT_3D ( 'NONE', #84997, #47160, #28959 ) ;
#94033 = AXIS2_PLACEMENT_3D ( 'NONE', #22609, #104653, #45995 ) ;
#94035 = ORIENTED_EDGE ( 'NONE', *, *, #20499, .F. ) ;
#94034 = CARTESIAN_POINT ( 'NONE',  ( 18.49999999999998934, 10.25000000001115552, -125.1500000000000341 ) ) ;
#94036 = EDGE_CURVE ( 'NONE', #256256, #223322, #57567, .T. ) ;
#94037 = ORIENTED_EDGE ( 'NONE', *, *, #196042, .T. ) ;
#94038 = DIRECTION ( 'NONE',  ( 0.000000000000000000, 0.000000000000000000, 1.000000000000000000 ) ) ;
#94039 = VECTOR ( 'NONE', #61053, 1000.000000000000114 ) ;
#94040 = DIRECTION ( 'NONE',  ( 0.000000000000000000, 0.000000000000000000, -1.000000000000000000 ) ) ;
#94041 = ORIENTED_EDGE ( 'NONE', *, *, #153169, .T. ) ;
#94042 = DIRECTION ( 'NONE',  ( 0.000000000000000000, -0.2128009952263403282, 0.9770955615653358350 ) ) ;
#94043 = ADVANCED_FACE ( 'NONE', ( #214161 ), #99259, .T. ) ;
#94044 = ORIENTED_EDGE ( 'NONE', *, *, #37868, .F. ) ;
#94045 = AXIS2_PLACEMENT_3D ( 'NONE', #178966, #18573, #42003 ) ;
#94046 = CARTESIAN_POINT ( 'NONE',  ( -18.38817693311004575, 11.48149151591092476, -158.2500000000000284 ) ) ;
#94047 = DIRECTION ( 'NONE',  ( 0.000000000000000000, 0.000000000000000000, -1.000000000000000000 ) ) ;
#94048 = VECTOR ( 'NONE', #10277, 1000.000000000000000 ) ;
#94050 = ORIENTED_EDGE ( 'NONE', *, *, #78955, .F. ) ;
#94049 = VECTOR ( 'NONE', #46236, 1000.000000000000114 ) ;
#94051 = DIRECTION ( 'NONE',  ( 0.000000000000000000, 0.1298341882520022694, 0.9915357197604852679 ) ) ;
#94052 = EDGE_CURVE ( 'NONE', #9728, #197944, #178503, .T. ) ;
#94053 = CARTESIAN_POINT ( 'NONE',  ( -18.40000000000000213, 11.47316190337364183, -124.6740539331920843 ) ) ;
#94054 = ORIENTED_EDGE ( 'NONE', *, *, #22074, .F. ) ;
#94055 = ORIENTED_EDGE ( 'NONE', *, *, #74095, .F. ) ;
#94056 = CARTESIAN_POINT ( 'NONE',  ( 20.22516295850462598, 18.77592805117411601, -228.7415353349608438 ) ) ;
#94057 = VERTEX_POINT ( 'NONE', #86171 ) ;
#94058 = DIRECTION ( 'NONE',  ( 1.000000000000000000, 0.000000000000000000, 0.000000000000000000 ) ) ;
#94059 = ORIENTED_EDGE ( 'NONE', *, *, #82288, .F. ) ;
#94061 = VERTEX_POINT ( 'NONE', #221829 ) ;
#94060 = DIRECTION ( 'NONE',  ( 0.000000000000000000, 1.000000000000000000, 0.000000000000000000 ) ) ;
#94062 = EDGE_LOOP ( 'NONE', ( #87257, #116175, #39298, #109397 ) ) ;
#94063 = AXIS2_PLACEMENT_3D ( 'NONE', #117139, #196657, #135396 ) ;
#94064 = CARTESIAN_POINT ( 'NONE',  ( -20.85000000000000142, 7.021664781900089913, -37.33356540189728889 ) ) ;
#94065 = ORIENTED_EDGE ( 'NONE', *, *, #21700, .F. ) ;
#94066 = CIRCLE ( 'NONE', #194057, 0.1000000000000028644 ) ;
#94069 = ORIENTED_EDGE ( 'NONE', *, *, #12500, .F. ) ;
#94068 = ORIENTED_EDGE ( 'NONE', *, *, #119171, .T. ) ;
#94067 = DIRECTION ( 'NONE',  ( 1.073024830501117725E-15, -0.2617529984165031243, -0.9651348961777157509 ) ) ;
#94070 = AXIS2_PLACEMENT_3D ( 'NONE', #226919, #246480, #147385 ) ;
#94071 = AXIS2_PLACEMENT_3D ( 'NONE', #142771, #63247, #22876 ) ;
#94072 = EDGE_LOOP ( 'NONE', ( #255170, #54357, #28903, #194833 ) ) ;
#94073 = AXIS2_PLACEMENT_3D ( 'NONE', #189983, #109142, #110438 ) ;
#94074 = EDGE_CURVE ( 'NONE', #55596, #115794, #88399, .T. ) ;
#94075 = CARTESIAN_POINT ( 'NONE',  ( 21.08832698747859169, 8.775364393428372267, -45.72871746646415403 ) ) ;
#94076 = EDGE_CURVE ( 'NONE', #217215, #162824, #82490, .T. ) ;
#94077 = ORIENTED_EDGE ( 'NONE', *, *, #12279, .F. ) ;
#94078 = CARTESIAN_POINT ( 'NONE',  ( -23.15000000000000213, 1.115600667400684642E-11, -79.87500000000004263 ) ) ;
#94080 = ORIENTED_EDGE ( 'NONE', *, *, #56151, .T. ) ;
#94079 = DIRECTION ( 'NONE',  ( -1.000000000000000000, 0.000000000000000000, 0.000000000000000000 ) ) ;
#94081 = CARTESIAN_POINT ( 'NONE',  ( 20.94999999999999929, 76.00000000001165290, -69.52310748452431710 ) ) ;
#94082 = ORIENTED_EDGE ( 'NONE', *, *, #34362, .F. ) ;
#94083 = ADVANCED_FACE ( 'NONE', ( #163184 ), #257434, .T. ) ;
#94085 = EDGE_CURVE ( 'NONE', #11913, #50748, #3393, .T. ) ;
#94084 = AXIS2_PLACEMENT_3D ( 'NONE', #161, #57562, #139661 ) ;
#94086 = EDGE_LOOP ( 'NONE', ( #242637, #76509, #16813, #184835 ) ) ;
#94087 = DIRECTION ( 'NONE',  ( 1.073024830501117725E-15, 0.2128009952263604232, -0.9770955615653316162 ) ) ;
#94088 = DIRECTION ( 'NONE',  ( 0.000000000000000000, 0.000000000000000000, 1.000000000000000000 ) ) ;
#94089 = VECTOR ( 'NONE', #177010, 1000.000000000000227 ) ;
#94090 = EDGE_CURVE ( 'NONE', #203870, #223079, #70077, .T. ) ;
#94091 = EDGE_LOOP ( 'NONE', ( #51030, #174605, #116153, #157750 ) ) ;
#94092 = ORIENTED_EDGE ( 'NONE', *, *, #203929, .T. ) ;
#94094 = EDGE_CURVE ( 'NONE', #211746, #228703, #215782, .T. ) ;
#94093 = DIRECTION ( 'NONE',  ( 0.000000000000000000, 1.000000000000000000, 0.000000000000000000 ) ) ;
#94096 = EDGE_CURVE ( 'NONE', #251548, #73136, #66644, .T. ) ;
#94095 = EDGE_CURVE ( 'NONE', #124703, #219174, #103350, .T. ) ;
#94098 = ORIENTED_EDGE ( 'NONE', *, *, #83795, .F. ) ;
#94097 = VERTEX_POINT ( 'NONE', #121505 ) ;
#94099 = VERTEX_POINT ( 'NONE', #45788 ) ;
#94100 = DIRECTION ( 'NONE',  ( 0.000000000000000000, 4.440892098500631684E-15, -1.000000000000000000 ) ) ;
#94101 = ORIENTED_EDGE ( 'NONE', *, *, #55442, .T. ) ;
#94102 = ORIENTED_EDGE ( 'NONE', *, *, #231951, .F. ) ;
#94103 = ADVANCED_FACE ( 'NONE', ( #199756 ), #124059, .T. ) ;
#94104 = DIRECTION ( 'NONE',  ( 0.000000000000000000, -1.000000000000000000, 0.000000000000000000 ) ) ;
#94105 = TOROIDAL_SURFACE ( 'NONE', #69203, 14.20833333333334103, 0.1000000000000000056 ) ;
#94106 = ORIENTED_EDGE ( 'NONE', *, *, #88429, .T. ) ;
#94107 = DIRECTION ( 'NONE',  ( 0.000000000000000000, -0.4721928772776973204, -0.8814952561688629284 ) ) ;
#94108 = DIRECTION ( 'NONE',  ( 1.000000000000000000, -0.000000000000000000, -0.000000000000000000 ) ) ;
#94109 = EDGE_LOOP ( 'NONE', ( #192686, #229773, #114418, #168366 ) ) ;
#94110 = EDGE_CURVE ( 'NONE', #14805, #48836, #21121, .T. ) ;
#94111 = ORIENTED_EDGE ( 'NONE', *, *, #26784, .T. ) ;
#94112 = CARTESIAN_POINT ( 'NONE',  ( 21.00000000000000000, 66.25000000001199396, -115.2731074845243597 ) ) ;
#94113 = ADVANCED_FACE ( 'NONE', ( #203581 ), #103177, .T. ) ;
#94114 = EDGE_CURVE ( 'NONE', #131327, #62762, #157584, .T. ) ;
#94115 = VERTEX_POINT ( 'NONE', #1515 ) ;
#94116 = AXIS2_PLACEMENT_3D ( 'NONE', #168965, #247158, #248461 ) ;
#94117 = AXIS2_PLACEMENT_3D ( 'NONE', #77795, #158666, #118226 ) ;
#94118 = VECTOR ( 'NONE', #230809, 1000.000000000000000 ) ;
#94119 = EDGE_CURVE ( 'NONE', #128423, #239176, #81041, .T. ) ;
#94120 = LINE ( 'NONE', #190692, #234075 ) ;
#94121 = ORIENTED_EDGE ( 'NONE', *, *, #107306, .F. ) ;
#94122 = VERTEX_POINT ( 'NONE', #240150 ) ;
#94123 = DIRECTION ( 'NONE',  ( -1.000000000000000000, -0.000000000000000000, 0.000000000000000000 ) ) ;
#94126 = ADVANCED_FACE ( 'NONE', ( #141051 ), #62789, .T. ) ;
#94125 = VERTEX_POINT ( 'NONE', #61511 ) ;
#94124 = CARTESIAN_POINT ( 'NONE',  ( -16.92989507731676468, 9.950000000011137047, -121.1174989306102390 ) ) ;
#94127 = CARTESIAN_POINT ( 'NONE',  ( 21.08479644141221954, 0.05855444257531394053, -127.6549613422681375 ) ) ;
#94128 = FACE_BOUND ( 'NONE', #121378, .T. ) ;
#94129 = EDGE_CURVE ( 'NONE', #144177, #169497, #236637, .T. ) ;
#94130 = CARTESIAN_POINT ( 'NONE',  ( 22.88900146558018989, 67.29609520889924568, -123.8731074845243683 ) ) ;
#94131 = CARTESIAN_POINT ( 'NONE',  ( 18.52928932304239495, 33.73464088294735319, -236.3235076462605377 ) ) ;
#94132 = DIRECTION ( 'NONE',  ( 0.000000000000000000, 1.000000000000000000, 2.891205793294679805E-16 ) ) ;
#94133 = CARTESIAN_POINT ( 'NONE',  ( -20.00857864376270001, 66.85000000001222986, -148.7731074845244166 ) ) ;
#94134 = LINE ( 'NONE', #95426, #203824 ) ;
#94135 = CARTESIAN_POINT ( 'NONE',  ( 21.33487959338958362, 33.90926806716007746, -243.4133681147159223 ) ) ;
#94136 = CARTESIAN_POINT ( 'NONE',  ( 20.94999999999999929, 69.55000000001159322, -59.50608031408435039 ) ) ;
#94137 = FACE_OUTER_BOUND ( 'NONE', #162806, .T. ) ;
#94138 = DIRECTION ( 'NONE',  ( 0.000000000000000000, 0.000000000000000000, -1.000000000000000000 ) ) ;
#94139 = CIRCLE ( 'NONE', #69227, 11.65000000000000036 ) ;
#94140 = VECTOR ( 'NONE', #124027, 1000.000000000000000 ) ;
#94141 = EDGE_LOOP ( 'NONE', ( #165232, #71144, #244504 ) ) ;
#94143 = EDGE_LOOP ( 'NONE', ( #247764, #165284, #121384, #233540, #154437 ) ) ;
#94142 = ORIENTED_EDGE ( 'NONE', *, *, #195762, .F. ) ;
#94144 = AXIS2_PLACEMENT_3D ( 'NONE', #93320, #209413, #15081 ) ;
#94145 = ORIENTED_EDGE ( 'NONE', *, *, #229525, .F. ) ;
#94146 = CARTESIAN_POINT ( 'NONE',  ( -21.14999999999994174, 64.35000000001120668, -3.123107484524795474 ) ) ;
#94147 = DIRECTION ( 'NONE',  ( 0.000000000000000000, 0.9553114395363172529, -0.2956011730204217702 ) ) ;
#94149 = CARTESIAN_POINT ( 'NONE',  ( -20.54999999999999716, 68.75000000001253397, -182.2731074845244166 ) ) ;
#94148 = FACE_OUTER_BOUND ( 'NONE', #221951, .T. ) ;
#94150 = VERTEX_POINT ( 'NONE', #126612 ) ;
#94151 = EDGE_LOOP ( 'NONE', ( #243469, #12014, #125379 ) ) ;
#94152 = CARTESIAN_POINT ( 'NONE',  ( -23.15000000000000213, -8.999999999988844479, -57.70603087734755832 ) ) ;
#94153 = DIRECTION ( 'NONE',  ( -0.000000000000000000, -0.2128009952263604787, 0.9770955615653313941 ) ) ;
#94154 = CARTESIAN_POINT ( 'NONE',  ( 18.49505816908823874, -9.437872553199980530, -73.77765720167090535 ) ) ;
#94155 = ORIENTED_EDGE ( 'NONE', *, *, #66500, .F. ) ;
#94156 = VERTEX_POINT ( 'NONE', #130461 ) ;
#94157 = AXIS2_PLACEMENT_3D ( 'NONE', #4001, #6568, #100501 ) ;
#94158 = CARTESIAN_POINT ( 'NONE',  ( -23.25000000000000000, 65.66751761918668251, -97.42826094061121012 ) ) ;
#94159 = EDGE_LOOP ( 'NONE', ( #134548, #178181, #88683, #33626 ) ) ;
#94160 = DIRECTION ( 'NONE',  ( 1.000000000000000000, 0.000000000000000000, 0.000000000000000000 ) ) ;
#94162 = EDGE_LOOP ( 'NONE', ( #19406, #15370, #181615 ) ) ;
#94161 = CARTESIAN_POINT ( 'NONE',  ( 20.95512820512820440, 67.12384868372393498, -124.3731074845243683 ) ) ;
#94163 = DIRECTION ( 'NONE',  ( 0.000000000000000000, 0.000000000000000000, -1.000000000000000000 ) ) ;
#94164 = DIRECTION ( 'NONE',  ( -0.000000000000000000, 0.8814952561688430555, -0.4721928772777346239 ) ) ;
#94165 = CARTESIAN_POINT ( 'NONE',  ( -20.94999999999999929, 69.09936979046463534, -247.6075824278584889 ) ) ;
#94166 = ORIENTED_EDGE ( 'NONE', *, *, #196340, .T. ) ;
#94167 = CARTESIAN_POINT ( 'NONE',  ( -18.50000000000000000, 13.71992543034163958, -238.5823796952984992 ) ) ;
#94168 = CARTESIAN_POINT ( 'NONE',  ( -18.40000000000000213, 11.47316190337362940, -180.1085786437626552 ) ) ;
#94169 = DIRECTION ( 'NONE',  ( 1.000000000000000000, 0.000000000000000000, 0.000000000000000000 ) ) ;
#94170 = EDGE_CURVE ( 'NONE', #79169, #161112, #13102, .T. ) ;
#94172 = FACE_OUTER_BOUND ( 'NONE', #176983, .T. ) ;
#94171 = CARTESIAN_POINT ( 'NONE',  ( -33.72168855820451938, 60.93935776605888321, -221.0417277355861359 ) ) ;
#94173 = CYLINDRICAL_SURFACE ( 'NONE', #74733, 0.1000000000000089567 ) ;
#94174 = CIRCLE ( 'NONE', #148350, 0.1000000000000124678 ) ;
#94175 = CARTESIAN_POINT ( 'NONE',  ( -23.15000000000000213, 1.115600667400684642E-11, -134.0000000000000000 ) ) ;
#94177 = EDGE_CURVE ( 'NONE', #102509, #75871, #32699, .T. ) ;
#94176 = PLANE ( 'NONE',  #1514 ) ;
#94178 = CARTESIAN_POINT ( 'NONE',  ( 22.39999999999999503, 7.790779598384535376, -33.50000000000000000 ) ) ;
#94179 = AXIS2_PLACEMENT_3D ( 'NONE', #171573, #153299, #91995 ) ;
#94180 = VERTEX_POINT ( 'NONE', #210015 ) ;
#94181 = VERTEX_POINT ( 'NONE', #228294 ) ;
#94182 = EDGE_CURVE ( 'NONE', #236296, #236185, #178414, .T. ) ;
#94183 = DIRECTION ( 'NONE',  ( 0.000000000000000000, 0.1350103645451876666, 0.9908441862701600211 ) ) ;
#94184 = EDGE_CURVE ( 'NONE', #19166, #125075, #190894, .T. ) ;
#94185 = CARTESIAN_POINT ( 'NONE',  ( -21.05000000000000071, 1.115600667400684642E-11, -67.00000000000004263 ) ) ;
#94186 = VERTEX_POINT ( 'NONE', #70527 ) ;
#94187 = DIRECTION ( 'NONE',  ( 0.000000000000000000, -7.429790795770644761E-15, 1.000000000000000000 ) ) ;
#94188 = EDGE_LOOP ( 'NONE', ( #105197, #137526, #163664, #202098, #91836 ) ) ;
#94189 =( NAMED_UNIT ( * ) PLANE_ANGLE_UNIT ( ) SI_UNIT ( $, .RADIAN. ) );
#94190 = ORIENTED_EDGE ( 'NONE', *, *, #2633, .F. ) ;
#94191 = CARTESIAN_POINT ( 'NONE',  ( 21.05000000000000071, 75.96798630682398823, -109.2819502080621277 ) ) ;
#94192 = TOROIDAL_SURFACE ( 'NONE', #40074, 7.791421356237316687, 0.1000000000000000056 ) ;
#94193 = EDGE_LOOP ( 'NONE', ( #189645, #243392, #254590, #137062 ) ) ;
#94194 = EDGE_CURVE ( 'NONE', #78387, #203718, #240930, .T. ) ;
#94195 = CARTESIAN_POINT ( 'NONE',  ( -22.39999999999999858, 7.790779598384560245, -66.90000000000004832 ) ) ;
#94197 = EDGE_CURVE ( 'NONE', #11614, #61629, #28851, .T. ) ;
#94196 = AXIS2_PLACEMENT_3D ( 'NONE', #2281, #222608, #80524 ) ;
#94198 = CARTESIAN_POINT ( 'NONE',  ( -12.25000000000000000, 9.350000000011133849, -50.36574316727391221 ) ) ;
#94199 = CARTESIAN_POINT ( 'NONE',  ( -20.64999999999999858, 73.50000000001151079, -49.24772940728643533 ) ) ;
#94200 = DIRECTION ( 'NONE',  ( -0.000000000000000000, 6.982962677686266711E-15, -1.000000000000000000 ) ) ;
#94201 = FACE_BOUND ( 'NONE', #254676, .T. ) ;
#94204 = ORIENTED_EDGE ( 'NONE', *, *, #77880, .F. ) ;
#94203 = FACE_OUTER_BOUND ( 'NONE', #82032, .T. ) ;
#94202 = AXIS2_PLACEMENT_3D ( 'NONE', #110985, #35340, #32772 ) ;
#94206 = CARTESIAN_POINT ( 'NONE',  ( 19.75857864376268935, 11.75000000001118927, -192.2499999999999432 ) ) ;
#94205 = CARTESIAN_POINT ( 'NONE',  ( 21.07928932188134397, 6.162520550847358614, -199.5566553493351307 ) ) ;
#94207 = CARTESIAN_POINT ( 'NONE',  ( -21.64999999999999858, 68.65000000001180069, -81.77310748452435973 ) ) ;
#94208 = FACE_OUTER_BOUND ( 'NONE', #229328, .T. ) ;
#94209 = VECTOR ( 'NONE', #38862, 999.9999999999998863 ) ;
#94210 = FACE_OUTER_BOUND ( 'NONE', #229189, .T. ) ;
#94211 = DIRECTION ( 'NONE',  ( 0.000000000000000000, -1.000000000000000000, -6.982962677686265922E-15 ) ) ;
#94213 = ORIENTED_EDGE ( 'NONE', *, *, #75513, .F. ) ;
#94212 = VECTOR ( 'NONE', #168259, 1000.000000000000000 ) ;
#94214 = LINE ( 'NONE', #198458, #237509 ) ;
#94215 = ADVANCED_FACE ( 'NONE', ( #92603 ), #167058, .T. ) ;
#94216 = EDGE_LOOP ( 'NONE', ( #9497, #239364, #191847, #154519 ) ) ;
#94217 = CARTESIAN_POINT ( 'NONE',  ( -18.59999999999999787, 77.16412189325286874, -61.80825939895269272 ) ) ;
#94218 = ADVANCED_FACE ( 'NONE', ( #172215 ), #28603, .F. ) ;
#94219 = ORIENTED_EDGE ( 'NONE', *, *, #208760, .F. ) ;
#94220 = AXIS2_PLACEMENT_3D ( 'NONE', #29375, #108865, #250926 ) ;
#94221 = CARTESIAN_POINT ( 'NONE',  ( 21.72449340488909897, 62.76341949586993252, -213.0402075299554951 ) ) ;
#94222 = VECTOR ( 'NONE', #11119, 1000.000000000000000 ) ;
#94223 = AXIS2_PLACEMENT_3D ( 'NONE', #29520, #127303, #71199 ) ;
#94224 = CARTESIAN_POINT ( 'NONE',  ( 21.00000000000000000, 9.750000000011153745, -179.8499999999999943 ) ) ;
#94225 = CARTESIAN_POINT ( 'NONE',  ( -21.05000000000000071, 76.00000000001213607, -136.5231074845243313 ) ) ;
#94226 = VERTEX_POINT ( 'NONE', #250404 ) ;
#94227 = VECTOR ( 'NONE', #205670, 1000.000000000000000 ) ;
#94228 = ORIENTED_EDGE ( 'NONE', *, *, #148751, .T. ) ;
#94229 = ADVANCED_FACE ( 'NONE', ( #73098 ), #69232, .F. ) ;
#94230 = EDGE_CURVE ( 'NONE', #149519, #26230, #90040, .T. ) ;
#94231 = DIRECTION ( 'NONE',  ( -1.000000000000000000, 1.646408749285563322E-14, -1.073024830501002749E-15 ) ) ;
#94232 = FACE_OUTER_BOUND ( 'NONE', #139655, .T. ) ;
#94233 = CARTESIAN_POINT ( 'NONE',  ( -21.05000000000000071, 65.49889199258218753, -241.8691648588935266 ) ) ;
#94234 = CARTESIAN_POINT ( 'NONE',  ( -16.91256925476571382, 66.01426884188369115, -90.49074997352965966 ) ) ;
#94235 = CIRCLE ( 'NONE', #223791, 0.09999999999999939493 ) ;
#94237 = CARTESIAN_POINT ( 'NONE',  ( 22.39999999999999858, 36.65892442174472876, -249.5511627012454596 ) ) ;
#94236 = CARTESIAN_POINT ( 'NONE',  ( -23.15000000000000213, 27.73205844876672899, -240.0613753537626565 ) ) ;
#94238 = EDGE_CURVE ( 'NONE', #31259, #51418, #122628, .T. ) ;
#94239 = DIRECTION ( 'NONE',  ( 3.265361837132813093E-16, -1.000000000000000000, -0.000000000000000000 ) ) ;
#94240 = CARTESIAN_POINT ( 'NONE',  ( 13.54577453029516221, 9.450602096099677496, -51.94389596309667922 ) ) ;
#94241 = DIRECTION ( 'NONE',  ( -1.836970198721029934E-16, 1.000000000000000000, 0.000000000000000000 ) ) ;
#94242 = VERTEX_POINT ( 'NONE', #148759 ) ;
#94243 = FACE_OUTER_BOUND ( 'NONE', #152888, .T. ) ;
#94245 = ORIENTED_EDGE ( 'NONE', *, *, #222824, .F. ) ;
#94244 = FACE_OUTER_BOUND ( 'NONE', #126359, .T. ) ;
#94246 = CARTESIAN_POINT ( 'NONE',  ( -20.94999999999999929, 11.75000000001115552, -74.01480577065404987 ) ) ;
#94247 = DIRECTION ( 'NONE',  ( 0.000000000000000000, 0.000000000000000000, -1.000000000000000000 ) ) ;
#94249 = DIRECTION ( 'NONE',  ( -1.000000000000000000, -2.952720810173289112E-16, 0.000000000000000000 ) ) ;
#94248 = DIRECTION ( 'NONE',  ( -1.000000000000000000, 0.000000000000000000, 0.000000000000000000 ) ) ;
#94251 = VERTEX_POINT ( 'NONE', #48355 ) ;
#94250 = LINE ( 'NONE', #134643, #86055 ) ;
#94252 = CARTESIAN_POINT ( 'NONE',  ( -23.25000000000000355, 64.25000000001161027, -60.27310748452440947 ) ) ;
#94253 = CARTESIAN_POINT ( 'NONE',  ( 22.39999999999999503, 0.1000000000111554016, -27.25000000000000355 ) ) ;
#94254 = EDGE_CURVE ( 'NONE', #160204, #77606, #99438, .T. ) ;
#94255 = CARTESIAN_POINT ( 'NONE',  ( 18.59999999999999432, 0.5876173420563349792, -209.1618981382189588 ) ) ;
#94256 = CARTESIAN_POINT ( 'NONE',  ( -20.85000000000000142, 77.16412189325360771, -162.1082593989527254 ) ) ;
#94257 = CARTESIAN_POINT ( 'NONE',  ( -20.64999999999999858, 76.00000000001195133, -103.0231074845243171 ) ) ;
#94258 = ORIENTED_EDGE ( 'NONE', *, *, #201994, .T. ) ;
#94259 = CARTESIAN_POINT ( 'NONE',  ( 18.59999999999999076, 11.65000000001115943, -167.5000000000000284 ) ) ;
#94260 = CIRCLE ( 'NONE', #240016, 0.1000000000000016431 ) ;
#94261 = ORIENTED_EDGE ( 'NONE', *, *, #142629, .F. ) ;
#94262 = AXIS2_PLACEMENT_3D ( 'NONE', #162932, #183760, #42968 ) ;
#94263 = ADVANCED_FACE ( 'NONE', ( #226993 ), #186605, .T. ) ;
#94264 = AXIS2_PLACEMENT_3D ( 'NONE', #121671, #237740, #98188 ) ;
#94265 = CARTESIAN_POINT ( 'NONE',  ( 20.94999999999999929, 85.00000000001251976, -179.9170766071767389 ) ) ;
#94266 = ORIENTED_EDGE ( 'NONE', *, *, #212262, .F. ) ;
#94267 = CARTESIAN_POINT ( 'NONE',  ( 22.10000000000000142, -11.65000000000000036, 32.89999999999999858 ) ) ;
#94268 = ORIENTED_EDGE ( 'NONE', *, *, #231318, .T. ) ;
#94269 = CIRCLE ( 'NONE', #240026, 0.09999999999999939493 ) ;
#94270 = DIRECTION ( 'NONE',  ( 0.000000000000000000, 0.000000000000000000, 1.000000000000000000 ) ) ;
#94271 =( BOUNDED_SURFACE ( )  B_SPLINE_SURFACE ( 3, 2, ( 
 ( #101514, #98954, #16900 ),
 ( #97677, #37757, #57270 ),
 ( #58557, #39034, #121156 ),
 ( #156435, #76849, #96402 ),
 ( #136824, #177276, #237223 ),
 ( #36479, #216361, #238496 ),
 ( #198085, #181114, #78126 ),
 ( #217624, #2438, #116004 ),
 ( #118573, #81953, #258009 ),
 ( #59834, #139376, #218920 ),
 ( #40343, #20756, #100241 ),
 ( #179829, #1147, #160279 ) ),
 .UNSPECIFIED., .F., .F., .T. ) 
 B_SPLINE_SURFACE_WITH_KNOTS ( ( 4, 2, 2, 2, 2, 4 ),
 ( 3, 3 ),
 ( 3.174653483277205090, 3.943930578431714018, 4.713207673586222946, 5.482484768740731873, 5.867123316317986337, 6.251761863895240801 ),
 ( 0.000000000000000000, 1.000000000000000000 ),
 .UNSPECIFIED. ) 
 GEOMETRIC_REPRESENTATION_ITEM ( )  RATIONAL_B_SPLINE_SURFACE ( (
 ( 1.000000000000000000, 0.8659465255642357917, 1.000000000000000000),
 ( 1.000000000000000000, 0.8648614068488756912, 1.000000000000000000),
 ( 1.000000000000000000, 0.8489031841323320116, 1.000000000000000000),
 ( 1.000000000000000000, 0.7927507630162191621, 1.000000000000000000),
 ( 1.000000000000000000, 0.7523013859014273663, 1.000000000000000000),
 ( 1.000000000000000000, 0.6616226951191639394, 1.000000000000000000),
 ( 1.000000000000000000, 0.6112214368730266578, 1.000000000000000000),
 ( 1.000000000000000000, 0.5507684314495190359, 1.000000000000000000),
 ( 1.000000000000000000, 0.5333267243157234772, 1.000000000000000000),
 ( 1.000000000000000000, 0.5084565446475229900, 1.000000000000000000),
 ( 1.000000000000000000, 0.5010722703454241200, 1.000000000000000000),
 ( 1.000000000000000000, 0.5001234037138393429, 1.000000000000000000) ) ) 
 REPRESENTATION_ITEM ( '' )  SURFACE ( )  );
#94272 = CARTESIAN_POINT ( 'NONE',  ( 23.24999999999999289, 11.65000000000000746, 11.75000000000000000 ) ) ;
#94273 = ORIENTED_EDGE ( 'NONE', *, *, #74453, .T. ) ;
#94274 = CIRCLE ( 'NONE', #244114, 0.1000000000000052097 ) ;
#94276 = VECTOR ( 'NONE', #181804, 1000.000000000000000 ) ;
#94275 = FACE_OUTER_BOUND ( 'NONE', #214397, .T. ) ;
#94277 = CARTESIAN_POINT ( 'NONE',  ( 20.85000000000000142, 28.55432187084631934, -258.5393726171218418 ) ) ;
#94278 = AXIS2_PLACEMENT_3D ( 'NONE', #126643, #165793, #83619 ) ;
#94279 = CARTESIAN_POINT ( 'NONE',  ( -18.39999999999999858, -9.599999999988845900, -207.7001893912220112 ) ) ;
#94280 = FACE_OUTER_BOUND ( 'NONE', #154392, .T. ) ;
#94281 = CARTESIAN_POINT ( 'NONE',  ( -16.92563707711778775, 66.03100930561521409, -115.6423491850004126 ) ) ;
#94282 = ORIENTED_EDGE ( 'NONE', *, *, #58408, .F. ) ;
#94283 = CARTESIAN_POINT ( 'NONE',  ( -18.43634282235119670, 85.67978719994012238, -129.8624555990704721 ) ) ;
#94284 = ORIENTED_EDGE ( 'NONE', *, *, #11419, .T. ) ;
#94286 = ORIENTED_EDGE ( 'NONE', *, *, #229133, .T. ) ;
#94285 = DIRECTION ( 'NONE',  ( -0.000000000000000000, 0.8814952561688430555, -0.4721928772777346239 ) ) ;
#94287 = ORIENTED_EDGE ( 'NONE', *, *, #174064, .F. ) ;
#94288 = CARTESIAN_POINT ( 'NONE',  ( 18.47654891039378455, 85.46527494839494921, -196.3971315793296526 ) ) ;
#94289 = DIRECTION ( 'NONE',  ( -1.000000000000000000, -4.624352451196580357E-15, 3.439547145395922042E-14 ) ) ;
#94290 = CARTESIAN_POINT ( 'NONE',  ( 23.14999999999999858, 5.600000000011153389, -88.09473398108696074 ) ) ;
#94291 = LINE ( 'NONE', #190870, #137440 ) ;
#94293 = EDGE_LOOP ( 'NONE', ( #140823, #165662, #181390, #32775 ) ) ;
#94292 = VECTOR ( 'NONE', #37359, 1000.000000000000000 ) ;
#94294 = CARTESIAN_POINT ( 'NONE',  ( -20.94999999999999929, 46.32970330538243786, -243.0551226933711746 ) ) ;
#94295 = DIRECTION ( 'NONE',  ( 0.000000000000000000, 1.000000000000000000, 6.938893903907222067E-15 ) ) ;
#94296 = ORIENTED_EDGE ( 'NONE', *, *, #81322, .F. ) ;
#94298 = ORIENTED_EDGE ( 'NONE', *, *, #90309, .T. ) ;
#94297 = CARTESIAN_POINT ( 'NONE',  ( -20.85000000000000142, 74.83412143252222393, -233.7087995678629966 ) ) ;
#94299 = CARTESIAN_POINT ( 'NONE',  ( 21.05000000000000071, 10.72371710471867701, -146.1500000000000341 ) ) ;
#94300 = CYLINDRICAL_SURFACE ( 'NONE', #123174, 0.5000000000000004441 ) ;
#94301 = CARTESIAN_POINT ( 'NONE',  ( 21.08489247129320887, 44.30010541822777981, -236.4001943044475809 ) ) ;
#94302 = CIRCLE ( 'NONE', #135987, 0.2000000000000010658 ) ;
#94303 = ORIENTED_EDGE ( 'NONE', *, *, #2745, .T. ) ;
#94304 = AXIS2_PLACEMENT_3D ( 'NONE', #198731, #119209, #20111 ) ;
#94305 = CIRCLE ( 'NONE', #90029, 4.149999999999993250 ) ;
#94306 = AXIS2_PLACEMENT_3D ( 'NONE', #41293, #19125, #119530 ) ;
#94307 = ORIENTED_EDGE ( 'NONE', *, *, #144050, .F. ) ;
#94308 = CARTESIAN_POINT ( 'NONE',  ( -22.39999999999999503, 33.38250548509083160, -242.4821227592188961 ) ) ;
#94309 = ORIENTED_EDGE ( 'NONE', *, *, #249799, .T. ) ;
#94310 = FACE_OUTER_BOUND ( 'NONE', #167639, .T. ) ;
#94311 = EDGE_CURVE ( 'NONE', #158894, #37076, #124419, .T. ) ;
#94312 = DIRECTION ( 'NONE',  ( -1.000000000000000000, -1.836970198721029934E-16, 0.000000000000000000 ) ) ;
#94313 = CARTESIAN_POINT ( 'NONE',  ( 18.59999999999999076, 64.35000000001177511, -78.17310748452437963 ) ) ;
#94314 = EDGE_CURVE ( 'NONE', #137749, #20778, #36962, .T. ) ;
#94315 = EDGE_CURVE ( 'NONE', #88353, #252254, #217675, .T. ) ;
#94316 = CIRCLE ( 'NONE', #198382, 11.64999999999999325 ) ;
#94317 = CIRCLE ( 'NONE', #235969, 7.900000000000003908 ) ;
#94318 = TOROIDAL_SURFACE ( 'NONE', #219221, 0.4000000000000009104, 0.1000000000000000056 ) ;
#94319 = VERTEX_POINT ( 'NONE', #174779 ) ;
#94320 = CARTESIAN_POINT ( 'NONE',  ( 18.60000000000000497, 1.115600667400684642E-11, -100.5000000000000284 ) ) ;
#94321 = AXIS2_PLACEMENT_3D ( 'NONE', #117095, #17976, #97489 ) ;
#94322 = ORIENTED_EDGE ( 'NONE', *, *, #184423, .F. ) ;
#94323 = CARTESIAN_POINT ( 'NONE',  ( -18.39999999999999858, 85.50000000001263345, -196.4910380878246201 ) ) ;
#94324 = EDGE_CURVE ( 'NONE', #166820, #29646, #66134, .T. ) ;
#94325 = CARTESIAN_POINT ( 'NONE',  ( -16.94107738177415712, 10.01423928514777550, -79.55000000000005400 ) ) ;
#94327 = ORIENTED_EDGE ( 'NONE', *, *, #209234, .T. ) ;
#94326 = DIRECTION ( 'NONE',  ( 0.000000000000000000, -5.551115123125777653E-14, 1.000000000000000000 ) ) ;
#94328 = DIRECTION ( 'NONE',  ( -1.000000000000000000, 0.000000000000000000, 0.000000000000000000 ) ) ;
#94329 = CARTESIAN_POINT ( 'NONE',  ( -23.15000000000000213, -8.999999999988844479, -124.1060308773475924 ) ) ;
#94330 = DIRECTION ( 'NONE',  ( 0.000000000000000000, 0.000000000000000000, -1.000000000000000000 ) ) ;
#94331 = CARTESIAN_POINT ( 'NONE',  ( 20.84999999999999432, 74.93036000061670165, -233.6816308724374949 ) ) ;
#94332 = CARTESIAN_POINT ( 'NONE',  ( -19.89999999999999858, 1.350000000000000089, 21.90000000000000213 ) ) ;
#94333 = CARTESIAN_POINT ( 'NONE',  ( 23.14999999999999858, 69.35000000001228670, -157.6731074845243938 ) ) ;
#94334 = FACE_OUTER_BOUND ( 'NONE', #169371, .T. ) ;
#94336 = VERTEX_POINT ( 'NONE', #198137 ) ;
#94335 = CARTESIAN_POINT ( 'NONE',  ( -22.47071067811865319, 68.27992525551407255, -136.6221999392269595 ) ) ;
#94337 = AXIS2_PLACEMENT_3D ( 'NONE', #215041, #35164, #235876 ) ;
#94338 = DIRECTION ( 'NONE',  ( 0.000000000000000000, 0.000000000000000000, -1.000000000000000000 ) ) ;
#94339 = EDGE_CURVE ( 'NONE', #254433, #233882, #112875, .T. ) ;
#94340 = EDGE_CURVE ( 'NONE', #118551, #181442, #134296, .T. ) ;
#94341 = DIRECTION ( 'NONE',  ( -1.000000000000000000, -0.000000000000000000, -0.000000000000000000 ) ) ;
#94342 = LINE ( 'NONE', #13547, #84669 ) ;
#94343 = CIRCLE ( 'NONE', #253134, 0.09999999999999700795 ) ;
#94344 = ORIENTED_EDGE ( 'NONE', *, *, #116202, .T. ) ;
#94345 = CARTESIAN_POINT ( 'NONE',  ( -22.10000000000000142, -1.467286812112899463, 33.00000000000000000 ) ) ;
#94346 = CARTESIAN_POINT ( 'NONE',  ( -18.40000000000000213, 23.82801463864234037, -229.3483719500187306 ) ) ;
#94348 = EDGE_CURVE ( 'NONE', #230038, #195218, #136882, .T. ) ;
#94347 = DIRECTION ( 'NONE',  ( 1.000000000000000000, 0.000000000000000000, 0.000000000000000000 ) ) ;
#94349 = CIRCLE ( 'NONE', #77775, 0.09999999999998898659 ) ;
#94350 = EDGE_LOOP ( 'NONE', ( #242849, #170073, #74272, #99444 ) ) ;
#94351 = VECTOR ( 'NONE', #165676, 1000.000000000000114 ) ;
#94352 = CIRCLE ( 'NONE', #106829, 0.09999999999999939493 ) ;
#94353 = CARTESIAN_POINT ( 'NONE',  ( -21.44999999999999929, 9.809744668562228043, -211.5030428704195913 ) ) ;
#94354 =( BOUNDED_SURFACE ( )  B_SPLINE_SURFACE ( 3, 2, ( 
 ( #4712, #23043, #146790 ),
 ( #123403, #222472, #86818 ),
 ( #84210, #205491, #244620 ),
 ( #163821, #166412, #25594 ),
 ( #202932, #3436, #201649 ),
 ( #102513, #182100, #45144 ),
 ( #85516, #162548, #105075 ),
 ( #81665, #206789, #184647 ),
 ( #65991, #225042, #46415 ),
 ( #242054, #47696, #125953 ) ),
 .UNSPECIFIED., .F., .F., .F. ) 
 B_SPLINE_SURFACE_WITH_KNOTS ( ( 4, 2, 2, 2, 4 ),
 ( 3, 3 ),
 ( 0.0001836757140119304782, 0.0004000170051583701661, 0.0005081876507315899287, 0.0005622729735181998100, 0.0006163582963048097997 ),
 ( 0.000000000000000000, 1.000000000000000000 ),
 .UNSPECIFIED. ) 
 GEOMETRIC_REPRESENTATION_ITEM ( )  RATIONAL_B_SPLINE_SURFACE ( (
 ( 1.000000000000000000, 0.7071067811866005304, 1.000000000000000000),
 ( 1.000000000000000000, 0.6461995200062370381, 1.000000000000000000),
 ( 1.000000000000000000, 0.5776453529505152229, 1.000000000000000000),
 ( 1.000000000000000000, 0.4585233068373967824, 1.000000000000000000),
 ( 1.000000000000000000, 0.4154092989939170422, 1.000000000000000000),
 ( 1.000000000000000000, 0.3550093145836495379, 1.000000000000000000),
 ( 1.000000000000000000, 0.3354498651689102329, 1.000000000000000000),
 ( 1.000000000000000000, 0.3060347992252177574, 1.000000000000000000),
 ( 1.000000000000000000, 0.2963555829630397653, 1.000000000000000000),
 ( 1.000000000000000000, 0.2966190024560962923, 1.000000000000000000) ) ) 
 REPRESENTATION_ITEM ( '' )  SURFACE ( )  );
#94355 = DIRECTION ( 'NONE',  ( 0.000000000000000000, 0.8814952561688428334, -0.4721928772777349570 ) ) ;
#94356 = AXIS2_PLACEMENT_3D ( 'NONE', #146179, #225690, #126623 ) ;
#94357 = ORIENTED_EDGE ( 'NONE', *, *, #157521, .T. ) ;
#94358 = CARTESIAN_POINT ( 'NONE',  ( 20.85000000000000142, 43.21392023178792385, -245.1418509714632421 ) ) ;
#94359 = EDGE_LOOP ( 'NONE', ( #203643, #150915 ) ) ;
#94361 = VERTEX_POINT ( 'NONE', #95191 ) ;
#94360 = LINE ( 'NONE', #74849, #205633 ) ;
#94362 = LINE ( 'NONE', #173969, #115123 ) ;
#94363 = EDGE_CURVE ( 'NONE', #247150, #244468, #141166, .T. ) ;
#94364 = ORIENTED_EDGE ( 'NONE', *, *, #109479, .T. ) ;
#94365 = DIRECTION ( 'NONE',  ( 1.000000000000000000, 0.000000000000000000, 0.000000000000000000 ) ) ;
#94366 = VERTEX_POINT ( 'NONE', #216416 ) ;
#94368 = ORIENTED_EDGE ( 'NONE', *, *, #76909, .F. ) ;
#94367 = ORIENTED_EDGE ( 'NONE', *, *, #246951, .T. ) ;
#94369 = DIRECTION ( 'NONE',  ( 0.7071067811865487940, 4.851104656540973741E-15, -0.7071067811865463515 ) ) ;
#94371 = ORIENTED_EDGE ( 'NONE', *, *, #129588, .T. ) ;
#94370 = DIRECTION ( 'NONE',  ( -1.000000000000000000, -0.000000000000000000, -0.000000000000000000 ) ) ;
#94372 = DIRECTION ( 'NONE',  ( 0.000000000000000000, -7.109473446599835262E-15, 1.000000000000000000 ) ) ;
#94374 = VERTEX_POINT ( 'NONE', #194322 ) ;
#94373 = AXIS2_PLACEMENT_3D ( 'NONE', #31736, #69558, #246885 ) ;
#94375 = AXIS2_PLACEMENT_3D ( 'NONE', #78934, #222292, #61979 ) ;
#94376 = CIRCLE ( 'NONE', #33933, 0.1000000000000028644 ) ;
#94377 = ADVANCED_FACE ( 'NONE', ( #33980 ), #124826, .T. ) ;
#94378 = AXIS2_PLACEMENT_3D ( 'NONE', #185573, #4353, #106009 ) ;
#94379 = ADVANCED_FACE ( 'NONE', ( #57324 ), #97723, .F. ) ;
#94380 = ORIENTED_EDGE ( 'NONE', *, *, #158983, .T. ) ;
#94381 = CIRCLE ( 'NONE', #90280, 0.2000000000000057288 ) ;
#94382 = PLANE ( 'NONE',  #186982 ) ;
#94383 = CARTESIAN_POINT ( 'NONE',  ( 21.59780538579342135, 75.90102133041372667, -76.37019801446757583 ) ) ;
#94384 = CARTESIAN_POINT ( 'NONE',  ( 20.73486653747088582, 7.250000000000026645, -20.85000000000000142 ) ) ;
#94385 = ORIENTED_EDGE ( 'NONE', *, *, #208756, .T. ) ;
#94386 = CIRCLE ( 'NONE', #131812, 0.1000000000000008937 ) ;
#94387 = ADVANCED_FACE ( 'NONE', ( #117324 ), #156487, .F. ) ;
#94389 = EDGE_CURVE ( 'NONE', #22402, #107433, #93900, .T. ) ;
#94388 = CARTESIAN_POINT ( 'NONE',  ( 23.14999999999999858, 75.47649400317826007, -205.4533772768803317 ) ) ;
#94390 = VECTOR ( 'NONE', #236523, 1000.000000000000000 ) ;
#94391 = FACE_OUTER_BOUND ( 'NONE', #176538, .T. ) ;
#94392 = DIRECTION ( 'NONE',  ( 0.000000000000000000, 0.000000000000000000, -1.000000000000000000 ) ) ;
#94393 = VERTEX_POINT ( 'NONE', #15686 ) ;
#94394 = CARTESIAN_POINT ( 'NONE',  ( 23.24999999999999645, 76.00000000001244871, -170.0231074845243597 ) ) ;
#94395 = DIRECTION ( 'NONE',  ( 0.000000000000000000, 3.552713678800500535E-15, -1.000000000000000000 ) ) ;
#94396 = CARTESIAN_POINT ( 'NONE',  ( -23.25000000000000355, 9.950000000011138823, -143.2500000000000284 ) ) ;
#94397 = VERTEX_POINT ( 'NONE', #155200 ) ;
#94398 = CARTESIAN_POINT ( 'NONE',  ( 23.14999999999999858, 9.374458193048763377, -220.5475659691911119 ) ) ;
#94399 = ORIENTED_EDGE ( 'NONE', *, *, #32412, .T. ) ;
#94400 = VERTEX_POINT ( 'NONE', #234707 ) ;
#94401 = EDGE_CURVE ( 'NONE', #47453, #91812, #253565, .T. ) ;
#94402 = AXIS2_PLACEMENT_3D ( 'NONE', #55276, #174024, #38332 ) ;
#94403 = EDGE_CURVE ( 'NONE', #131118, #52856, #215956, .T. ) ;
#94404 = AXIS2_PLACEMENT_3D ( 'NONE', #244265, #123063, #3080 ) ;
#94405 = AXIS2_PLACEMENT_3D ( 'NONE', #83966, #223512, #141419 ) ;
#94406 = CARTESIAN_POINT ( 'NONE',  ( 11.60000000000006182, 63.75000000001119815, -21.02310748452479316 ) ) ;
#94407 = ORIENTED_EDGE ( 'NONE', *, *, #147678, .F. ) ;
#94408 = VERTEX_POINT ( 'NONE', #181163 ) ;
#94409 = FACE_OUTER_BOUND ( 'NONE', #254930, .T. ) ;
#94410 = DIRECTION ( 'NONE',  ( -1.000000000000000000, -0.000000000000000000, -0.000000000000000000 ) ) ;
#94411 = ORIENTED_EDGE ( 'NONE', *, *, #117445, .T. ) ;
#94412 = EDGE_CURVE ( 'NONE', #225270, #133820, #28785, .T. ) ;
#94413 = ORIENTED_EDGE ( 'NONE', *, *, #92267, .T. ) ;
#94414 = DIRECTION ( 'NONE',  ( 0.5932847527679310229, -0.8049926720990042694, -6.366092712777067056E-16 ) ) ;
#94415 = CARTESIAN_POINT ( 'NONE',  ( -18.50000324121759121, 65.70692517833214197, -64.06446533783034170 ) ) ;
#94416 = ORIENTED_EDGE ( 'NONE', *, *, #70326, .T. ) ;
#94417 = EDGE_CURVE ( 'NONE', #65247, #206663, #170245, .T. ) ;
#94418 = EDGE_CURVE ( 'NONE', #113685, #11797, #101573, .T. ) ;
#94419 = EDGE_CURVE ( 'NONE', #123398, #170736, #116048, .T. ) ;
#94420 = VERTEX_POINT ( 'NONE', #9881 ) ;
#94421 = CARTESIAN_POINT ( 'NONE',  ( -21.05000000000000071, 76.00000000001165290, -69.52310748452431710 ) ) ;
#94422 = ADVANCED_FACE ( 'NONE', ( #206808 ), #28202, .F. ) ;
#94423 = CARTESIAN_POINT ( 'NONE',  ( -20.94999999999999929, 1.162701749949165642, -175.4999999999999716 ) ) ;
#94424 = CARTESIAN_POINT ( 'NONE',  ( -16.87487986503753845, 9.950007555096753720, -46.14997473968674058 ) ) ;
#94425 = CARTESIAN_POINT ( 'NONE',  ( -33.72168855820451938, 66.05000000001186322, -90.37310748452443931 ) ) ;
#94426 = EDGE_CURVE ( 'NONE', #40045, #38363, #193702, .T. ) ;
#94427 = VECTOR ( 'NONE', #106217, 1000.000000000000000 ) ;
#94428 = DIRECTION ( 'NONE',  ( 0.000000000000000000, 0.2617529984165027912, 0.9651348961777157509 ) ) ;
#94429 = CARTESIAN_POINT ( 'NONE',  ( 20.85000000000000142, 0.000000000000000000, -33.50000000000000000 ) ) ;
#94430 = EDGE_CURVE ( 'NONE', #106895, #18436, #62052, .T. ) ;
#94432 = B_SPLINE_CURVE_WITH_KNOTS ( 'NONE', 3,
 ( #134633, #113810, #56386, #253313, #175122, #150389, #152980, #194670 ),
 .UNSPECIFIED., .F., .F.,
 ( 4, 2, 2, 4 ),
 ( 0.000000000000000000, 0.0001881495939909944156, 0.0002822243909864270727, 0.0003762991879818597570 ),
 .UNSPECIFIED. ) ;
#94431 = VECTOR ( 'NONE', #209208, 1000.000000000000000 ) ;
#94433 = FACE_OUTER_BOUND ( 'NONE', #179409, .T. ) ;
#94435 = DIRECTION ( 'NONE',  ( 1.000000000000000000, 0.000000000000000000, 0.000000000000000000 ) ) ;
#94434 = CARTESIAN_POINT ( 'NONE',  ( 21.05000000000000071, 76.10000000001170406, -76.06376443622556849 ) ) ;
#94437 = CIRCLE ( 'NONE', #69338, 4.000000000000003553 ) ;
#94436 = CARTESIAN_POINT ( 'NONE',  ( -21.05000000000000071, 1.835341550235567887, -179.0551512925629538 ) ) ;
#94438 = AXIS2_PLACEMENT_3D ( 'NONE', #63702, #6287, #143235 ) ;
#94440 = EDGE_CURVE ( 'NONE', #140362, #61948, #195160, .T. ) ;
#94439 = DIRECTION ( 'NONE',  ( 1.000000000000000000, 3.265361837132813093E-16, -0.000000000000000000 ) ) ;
#94441 = DIRECTION ( 'NONE',  ( 0.000000000000000000, 6.982962677686266711E-15, -1.000000000000000000 ) ) ;
#94442 = CARTESIAN_POINT ( 'NONE',  ( -21.05000000000000071, 76.02110330807200000, -176.3276238137887901 ) ) ;
#94444 = ORIENTED_EDGE ( 'NONE', *, *, #232009, .F. ) ;
#94443 = CIRCLE ( 'NONE', #219350, 0.3999999999999994671 ) ;
#94445 = B_SPLINE_CURVE_WITH_KNOTS ( 'NONE', 3,
 ( #252867, #153831, #74275, #36425 ),
 .UNSPECIFIED., .F., .F.,
 ( 4, 4 ),
 ( 0.000000000000000000, 0.0002118541922231894411 ),
 .UNSPECIFIED. ) ;
#94447 = ORIENTED_EDGE ( 'NONE', *, *, #109274, .F. ) ;
#94446 = FACE_OUTER_BOUND ( 'NONE', #148993, .T. ) ;
#94448 = ADVANCED_FACE ( 'NONE', ( #128553 ), #161611, .F. ) ;
#94449 = CIRCLE ( 'NONE', #219354, 0.09999999999999939493 ) ;
#94450 = CYLINDRICAL_SURFACE ( 'NONE', #210935, 0.1000000000000028644 ) ;
#94451 = AXIS2_PLACEMENT_3D ( 'NONE', #11733, #225592, #50809 ) ;
#94452 = CYLINDRICAL_SURFACE ( 'NONE', #235996, 0.09999999999999939493 ) ;
#94453 = ORIENTED_EDGE ( 'NONE', *, *, #60606, .T. ) ;
#94454 = VECTOR ( 'NONE', #149777, 1000.000000000000000 ) ;
#94455 = DIRECTION ( 'NONE',  ( -0.8049926720990042694, -0.5796958986739304542, -0.1262515858416409231 ) ) ;
#94456 = DIRECTION ( 'NONE',  ( 0.000000000000000000, -7.147358527629766941E-15, 1.000000000000000000 ) ) ;
#94457 = VERTEX_POINT ( 'NONE', #89412 ) ;
#94458 = FACE_OUTER_BOUND ( 'NONE', #199576, .T. ) ;
#94459 = FACE_OUTER_BOUND ( 'NONE', #42028, .T. ) ;
#94460 = CARTESIAN_POINT ( 'NONE',  ( -21.13614978966381841, 10.19766428898124211, -228.0037713484281880 ) ) ;
#94462 = ORIENTED_EDGE ( 'NONE', *, *, #181868, .T. ) ;
#94461 = DIRECTION ( 'NONE',  ( -3.469446951953515108E-14, 0.000000000000000000, 1.000000000000000000 ) ) ;
#94463 = PLANE ( 'NONE',  #45527 ) ;
#94465 = EDGE_LOOP ( 'NONE', ( #121836, #211704, #212792, #119812 ) ) ;
#94464 = CARTESIAN_POINT ( 'NONE',  ( -18.40904629823847216, 85.50000000001186606, -96.42291792204295575 ) ) ;
#94466 = CARTESIAN_POINT ( 'NONE',  ( -21.05000000000000426, 10.02604994829658125, -228.1850015638761136 ) ) ;
#94467 = CARTESIAN_POINT ( 'NONE',  ( 18.59999999999997655, 11.75000000001115552, -67.00000000000000000 ) ) ;
#94468 = CARTESIAN_POINT ( 'NONE',  ( 21.05000000000005400, 67.65000000001118963, -14.06452884076210630 ) ) ;
#94469 = CARTESIAN_POINT ( 'NONE',  ( -16.87683809663752399, 12.47642768288813286, -211.9993005936843815 ) ) ;
#94470 = EDGE_CURVE ( 'NONE', #231732, #215045, #68586, .T. ) ;
#94472 = CARTESIAN_POINT ( 'NONE',  ( -20.00857864376270001, 66.65000000001259650, -191.1731074845244223 ) ) ;
#94471 = DIRECTION ( 'NONE',  ( 0.000000000000000000, 0.000000000000000000, 1.000000000000000000 ) ) ;
#94473 = CARTESIAN_POINT ( 'NONE',  ( -18.59999999999999787, 1.115600667400684642E-11, -67.00000000000004263 ) ) ;
#94474 = DIRECTION ( 'NONE',  ( -0.000000000000000000, -1.000000000000000000, -7.272083257015735086E-15 ) ) ;
#94475 = DIRECTION ( 'NONE',  ( 0.000000000000000000, 0.000000000000000000, -1.000000000000000000 ) ) ;
#94476 = AXIS2_PLACEMENT_3D ( 'NONE', #108344, #129191, #169642 ) ;
#94477 = AXIS2_PLACEMENT_3D ( 'NONE', #168654, #166060, #72083 ) ;
#94478 = EDGE_CURVE ( 'NONE', #147074, #92855, #224359, .T. ) ;
#94479 = CARTESIAN_POINT ( 'NONE',  ( 21.04999999999436966, 1.394874610627388156, -230.6776777473732807 ) ) ;
#94480 = AXIS2_PLACEMENT_3D ( 'NONE', #218424, #651, #166217 ) ;
#94482 = DIRECTION ( 'NONE',  ( 1.000000000000000000, -0.000000000000000000, -0.000000000000000000 ) ) ;
#94481 = VECTOR ( 'NONE', #42532, 1000.000000000000000 ) ;
#94483 = ORIENTED_EDGE ( 'NONE', *, *, #112133, .T. ) ;
#94484 = DIRECTION ( 'NONE',  ( 1.000000000000000000, 7.136802563874199107E-16, 1.554319503706929991E-16 ) ) ;
#94485 = ORIENTED_EDGE ( 'NONE', *, *, #234019, .T. ) ;
#94486 = ORIENTED_EDGE ( 'NONE', *, *, #112350, .F. ) ;
#94487 = EDGE_CURVE ( 'NONE', #99741, #235390, #49008, .T. ) ;
#94488 = DIRECTION ( 'NONE',  ( 0.000000000000000000, 0.000000000000000000, -1.000000000000000000 ) ) ;
#94489 = ADVANCED_FACE ( 'NONE', ( #100300 ), #111953, .T. ) ;
#94490 = DIRECTION ( 'NONE',  ( 0.000000000000000000, -0.5868805631290126001, -0.8096735173027292953 ) ) ;
#94491 = ORIENTED_EDGE ( 'NONE', *, *, #121761, .F. ) ;
#94492 = EDGE_LOOP ( 'NONE', ( #51643, #228128, #138372, #35339, #898, #242282 ) ) ;
#94493 = TOROIDAL_SURFACE ( 'NONE', #161149, 14.20833333333334103, 0.1000000000000000056 ) ;
#94494 = CARTESIAN_POINT ( 'NONE',  ( 18.59999999999997655, 11.75000000001115552, -134.0000000000000284 ) ) ;
#94495 = CIRCLE ( 'NONE', #48715, 2.100000000000004530 ) ;
#94496 = AXIS2_PLACEMENT_3D ( 'NONE', #115092, #55084, #254568 ) ;
#94497 = ORIENTED_EDGE ( 'NONE', *, *, #175654, .T. ) ;
#94498 = ORIENTED_EDGE ( 'NONE', *, *, #88848, .T. ) ;
#94499 = SPHERICAL_SURFACE ( 'NONE', #46364, 0.1000000000000000056 ) ;
#94500 = LINE ( 'NONE', #115353, #11981 ) ;
#94501 = CIRCLE ( 'NONE', #240278, 4.049999999999998046 ) ;
#94502 = DIRECTION ( 'NONE',  ( -1.000000000000000000, 0.000000000000000000, 0.000000000000000000 ) ) ;
#94503 = DIRECTION ( 'NONE',  ( 0.000000000000000000, 0.8814952561688426114, -0.4721928772777353456 ) ) ;
#94504 = CARTESIAN_POINT ( 'NONE',  ( -23.15000000000000213, 61.47936603916259202, -212.1738987416902376 ) ) ;
#94506 = CARTESIAN_POINT ( 'NONE',  ( 19.75857864376268935, 64.25000000001196554, -111.6731074845243796 ) ) ;
#94505 = LINE ( 'NONE', #257377, #83356 ) ;
#94507 = CARTESIAN_POINT ( 'NONE',  ( 21.05000000000000071, 76.00000000001217870, -143.0637644362255401 ) ) ;
#94509 = VERTEX_POINT ( 'NONE', #192377 ) ;
#94508 = CARTESIAN_POINT ( 'NONE',  ( -18.50000000000000000, 76.00000000001237765, -170.0231074845243597 ) ) ;
#94511 = DIRECTION ( 'NONE',  ( 0.000000000000000000, 1.000000000000000000, 0.000000000000000000 ) ) ;
#94510 = CARTESIAN_POINT ( 'NONE',  ( -17.29158576265542990, 22.08723780851632412, -229.9873656484244862 ) ) ;
#94512 = EDGE_LOOP ( 'NONE', ( #39185, #28891, #155075, #215590 ) ) ;
#94513 = CARTESIAN_POINT ( 'NONE',  ( 21.12802099929860944, 8.780552590233368093, -146.2481899849316278 ) ) ;
#94514 = SPHERICAL_SURFACE ( 'NONE', #154523, 0.1000000000000000056 ) ;
#94515 = VERTEX_POINT ( 'NONE', #90695 ) ;
#94516 = CARTESIAN_POINT ( 'NONE',  ( 18.59999999999999076, 77.14957036958755054, -95.20719500002232394 ) ) ;
#94517 = CIRCLE ( 'NONE', #165262, 0.09999999999999939493 ) ;
#94518 = CARTESIAN_POINT ( 'NONE',  ( 21.05000000000000071, -11.48912529306489994, -97.40000000000004832 ) ) ;
#94519 = EDGE_CURVE ( 'NONE', #223652, #10686, #207832, .T. ) ;
#94520 = CARTESIAN_POINT ( 'NONE',  ( 14.45204356427541548, 66.54933111084433506, -87.96756099431701159 ) ) ;
#94521 = EDGE_LOOP ( 'NONE', ( #14207, #147631, #198752, #180560 ) ) ;
#94522 = ORIENTED_EDGE ( 'NONE', *, *, #176278, .F. ) ;
#94523 = DIRECTION ( 'NONE',  ( 0.000000000000000000, 0.4088369013363783999, -0.9126074666063545004 ) ) ;
#94524 = CARTESIAN_POINT ( 'NONE',  ( 23.14999999999999858, 71.18691588786226987, -81.46462524104816794 ) ) ;
#94525 = CYLINDRICAL_SURFACE ( 'NONE', #178188, 0.1000000000000033362 ) ;
#94526 = CARTESIAN_POINT ( 'NONE',  ( 18.59999999999999787, 74.13328508995498112, -158.2704322382423641 ) ) ;
#94527 = ORIENTED_EDGE ( 'NONE', *, *, #237235, .F. ) ;
#94528 = AXIS2_PLACEMENT_3D ( 'NONE', #14715, #91655, #250717 ) ;
#94529 = ADVANCED_FACE ( 'NONE', ( #252331 ), #35890, .T. ) ;
#94530 = CARTESIAN_POINT ( 'NONE',  ( 12.29592348164039528, 47.70130725485972789, -234.3525798712488495 ) ) ;
#94531 = DIRECTION ( 'NONE',  ( 0.000000000000000000, 0.000000000000000000, 1.000000000000000000 ) ) ;
#94532 = ADVANCED_FACE ( 'NONE', ( #71164 ), #169006, .F. ) ;
#94533 = CARTESIAN_POINT ( 'NONE',  ( -16.91256925476569251, 9.985731158139328656, -121.4676424890052999 ) ) ;
#94534 = FACE_OUTER_BOUND ( 'NONE', #231407, .T. ) ;
#94535 = AXIS2_PLACEMENT_3D ( 'NONE', #146909, #127377, #128668 ) ;
#94536 = AXIS2_PLACEMENT_3D ( 'NONE', #198046, #178524, #158961 ) ;
#94537 = CARTESIAN_POINT ( 'NONE',  ( -18.50000000000000000, -9.419084502802133940, -207.8299078070253927 ) ) ;
#94538 = AXIS2_PLACEMENT_3D ( 'NONE', #78496, #120247, #180194 ) ;
#94539 = EDGE_CURVE ( 'NONE', #11973, #181359, #194963, .T. ) ;
#94541 = ORIENTED_EDGE ( 'NONE', *, *, #58578, .T. ) ;
#94540 = CARTESIAN_POINT ( 'NONE',  ( -20.94999999999999929, 18.86061765788380740, -226.6874733728449485 ) ) ;
#94542 = DIRECTION ( 'NONE',  ( -1.000000000000000000, -0.000000000000000000, -0.000000000000000000 ) ) ;
#94543 = CIRCLE ( 'NONE', #207571, 4.000000000000000000 ) ;
#94544 = LINE ( 'NONE', #210654, #145240 ) ;
#94545 = CARTESIAN_POINT ( 'NONE',  ( -18.39999999999999858, 11.47316190337362762, -76.29982924846605385 ) ) ;
#94546 = DIRECTION ( 'NONE',  ( -1.073024830501117725E-15, 6.982962677686266711E-15, -1.000000000000000000 ) ) ;
#94547 = TOROIDAL_SURFACE ( 'NONE', #15474, 2.100000000000002309, 0.1000000000000000056 ) ;
#94548 = EDGE_CURVE ( 'NONE', #190980, #124703, #253612, .T. ) ;
#94550 = ORIENTED_EDGE ( 'NONE', *, *, #25256, .T. ) ;
#94549 = DIRECTION ( 'NONE',  ( 0.000000000000000000, -6.853228547068871147E-15, 1.000000000000000000 ) ) ;
#94551 = CARTESIAN_POINT ( 'NONE',  ( -15.55912972643740488, 8.490870273573721150, -87.95000000000004547 ) ) ;
#94552 = ADVANCED_FACE ( 'NONE', ( #129823 ), #211955, .F. ) ;
#94553 = CYLINDRICAL_SURFACE ( 'NONE', #59299, 0.09999999999999990841 ) ;
#94554 = CARTESIAN_POINT ( 'NONE',  ( -18.34804628011471195, 11.47316190336237796, -9.250000000000001776 ) ) ;
#94555 = ORIENTED_EDGE ( 'NONE', *, *, #94810, .T. ) ;
#94556 = FACE_OUTER_BOUND ( 'NONE', #69516, .T. ) ;
#94557 = CARTESIAN_POINT ( 'NONE',  ( -23.25000000000000000, -5.011722593499800205, -233.2041167654973322 ) ) ;
#94558 = CARTESIAN_POINT ( 'NONE',  ( 21.87500000000000355, 66.25000000001199396, -115.2731074845243597 ) ) ;
#94559 = DIRECTION ( 'NONE',  ( 0.000000000000000000, 0.000000000000000000, -1.000000000000000000 ) ) ;
#94560 = EDGE_CURVE ( 'NONE', #109819, #93920, #28870, .T. ) ;
#94561 = FACE_OUTER_BOUND ( 'NONE', #43736, .T. ) ;
#94562 = AXIS2_PLACEMENT_3D ( 'NONE', #150081, #250434, #28876 ) ;
#94563 = CARTESIAN_POINT ( 'NONE',  ( 21.05000000000000071, 1.349084418638171412, -41.48649896354548616 ) ) ;
#94564 = CIRCLE ( 'NONE', #244405, 0.1000000000000016154 ) ;
#94565 = ORIENTED_EDGE ( 'NONE', *, *, #62797, .F. ) ;
#94566 = ORIENTED_EDGE ( 'NONE', *, *, #27732, .F. ) ;
#94567 = VECTOR ( 'NONE', #197122, 1000.000000000000000 ) ;
#94568 = CARTESIAN_POINT ( 'NONE',  ( -18.40000000000000213, 64.51332499825466016, -160.7731074845244450 ) ) ;
#94569 = DIRECTION ( 'NONE',  ( 1.000000000000000000, -0.000000000000000000, 0.000000000000000000 ) ) ;
#94570 = AXIS2_PLACEMENT_3D ( 'NONE', #86599, #189595, #226108 ) ;
#94571 = ADVANCED_FACE ( 'NONE', ( #189815 ), #15039, .F. ) ;
#94572 = CARTESIAN_POINT ( 'NONE',  ( 22.60000000000000142, 1.115600667400684642E-11, -33.50000000000000000 ) ) ;
#94573 = CARTESIAN_POINT ( 'NONE',  ( -21.12642695952773764, 6.375659922046319927, -133.9010967168106276 ) ) ;
#94574 = AXIS2_PLACEMENT_3D ( 'NONE', #90492, #170089, #249590 ) ;
#94575 = VECTOR ( 'NONE', #40937, 1000.000000000000114 ) ;
#94576 = DIRECTION ( 'NONE',  ( 0.000000000000000000, 0.4999999999999863998, -0.8660254037844464792 ) ) ;
#94577 = DIRECTION ( 'NONE',  ( 0.000000000000000000, 0.2617529984165031243, 0.9651348961777157509 ) ) ;
#94578 = FACE_OUTER_BOUND ( 'NONE', #191624, .T. ) ;
#94579 = CYLINDRICAL_SURFACE ( 'NONE', #181860, 0.09999999999998898659 ) ;
#94580 = VECTOR ( 'NONE', #75861, 1000.000000000000000 ) ;
#94581 = VECTOR ( 'NONE', #250081, 1000.000000000000114 ) ;
#94582 = ORIENTED_EDGE ( 'NONE', *, *, #172204, .T. ) ;
#94583 = DIRECTION ( 'NONE',  ( 1.000000000000000000, 0.000000000000000000, 0.000000000000000000 ) ) ;
#94584 = ORIENTED_EDGE ( 'NONE', *, *, #26694, .F. ) ;
#94585 = ORIENTED_EDGE ( 'NONE', *, *, #210392, .T. ) ;
#94586 = FACE_OUTER_BOUND ( 'NONE', #5244, .T. ) ;
#94587 = CARTESIAN_POINT ( 'NONE',  ( -21.05000000000000071, 6.540656951712399803, -100.5000000000000142 ) ) ;
#94588 = CARTESIAN_POINT ( 'NONE',  ( -20.00857864376270001, 9.250000000011157297, -88.15000000000004832 ) ) ;
#94590 = ORIENTED_EDGE ( 'NONE', *, *, #156715, .T. ) ;
#94589 = DIRECTION ( 'NONE',  ( 1.000000000000000000, 0.000000000000000000, 0.000000000000000000 ) ) ;
#94591 = DIRECTION ( 'NONE',  ( 1.000000000000000000, 0.000000000000000000, 0.000000000000000000 ) ) ;
#94592 = DIRECTION ( 'NONE',  ( 0.000000000000000000, -0.4721928772777358452, -0.8814952561688423893 ) ) ;
#94593 = CARTESIAN_POINT ( 'NONE',  ( 18.44208962362758442, 85.55234049692009535, -62.68093442906086210 ) ) ;
#94594 = ORIENTED_EDGE ( 'NONE', *, *, #135287, .F. ) ;
#94595 = DIRECTION ( 'NONE',  ( 0.000000000000000000, -1.000000000000000000, 0.000000000000000000 ) ) ;
#94596 = CARTESIAN_POINT ( 'NONE',  ( 18.49999999999999289, 65.75000000001220712, -145.3731074845244393 ) ) ;
#94597 = LINE ( 'NONE', #34660, #218848 ) ;
#94598 = VECTOR ( 'NONE', #223366, 1000.000000000000000 ) ;
#94599 = DIRECTION ( 'NONE',  ( 0.000000000000000000, -0.9770955615653318382, -0.2128009952263588411 ) ) ;
#94600 = DIRECTION ( 'NONE',  ( 0.000000000000000000, 1.000000000000000000, 0.000000000000000000 ) ) ;
#94601 = ADVANCED_FACE ( 'NONE', ( #30761 ), #93265, .F. ) ;
#94602 = ORIENTED_EDGE ( 'NONE', *, *, #208067, .T. ) ;
#94603 = VECTOR ( 'NONE', #54324, 1000.000000000000000 ) ;
#94604 = CARTESIAN_POINT ( 'NONE',  ( -22.59999999999999787, 75.89914163091351895, -148.2726746080136877 ) ) ;
#94605 = CARTESIAN_POINT ( 'NONE',  ( -16.87372386987899020, 66.11939976637512473, -89.87383761265797943 ) ) ;
#94606 = ORIENTED_EDGE ( 'NONE', *, *, #237461, .T. ) ;
#94607 = DIRECTION ( 'NONE',  ( -0.000000000000000000, 0.2617529984165031243, 0.9651348961777157509 ) ) ;
#94608 = EDGE_CURVE ( 'NONE', #59064, #88196, #86385, .T. ) ;
#94609 = DIRECTION ( 'NONE',  ( -1.000000000000000000, 4.625929269271478222E-14, 0.000000000000000000 ) ) ;
#94610 = AXIS2_PLACEMENT_3D ( 'NONE', #246725, #125504, #189341 ) ;
#94611 = VECTOR ( 'NONE', #240352, 1000.000000000000000 ) ;
#94612 = ADVANCED_FACE ( 'NONE', ( #214493 ), #157779, .T. ) ;
#94613 = ORIENTED_EDGE ( 'NONE', *, *, #128000, .F. ) ;
#94616 = EDGE_CURVE ( 'NONE', #46280, #233154, #191064, .T. ) ;
#94615 = AXIS2_PLACEMENT_3D ( 'NONE', #146136, #24937, #180149 ) ;
#94614 = CARTESIAN_POINT ( 'NONE',  ( 18.33996824403499915, -9.569639859420224326, -174.3190656375171841 ) ) ;
#94617 = DIRECTION ( 'NONE',  ( 2.952720810173289112E-16, -0.9770955615653316162, -0.2128009952263604232 ) ) ;
#94618 = TOROIDAL_SURFACE ( 'NONE', #127962, 0.2000000000000000111, 0.1000000000000000056 ) ;
#94619 = VERTEX_POINT ( 'NONE', #153287 ) ;
#94620 = AXIS2_PLACEMENT_3D ( 'NONE', #161493, #105305, #241017 ) ;
#94621 = EDGE_LOOP ( 'NONE', ( #213126, #206738, #129773, #166919 ) ) ;
#94622 = CARTESIAN_POINT ( 'NONE',  ( -20.54999999999999716, 7.150000000011155876, -188.6499999999999488 ) ) ;
#94623 = EDGE_CURVE ( 'NONE', #133438, #129974, #94544, .T. ) ;
#94624 = CARTESIAN_POINT ( 'NONE',  ( 18.59999999999999787, -10.35479209691423996, -194.7565409830737337 ) ) ;
#94626 = ORIENTED_EDGE ( 'NONE', *, *, #83849, .F. ) ;
#94625 = CARTESIAN_POINT ( 'NONE',  ( -20.64999999999999858, 1.115600667400684642E-11, -165.5000000000000284 ) ) ;
#94627 = DIRECTION ( 'NONE',  ( 1.000000000000000000, 0.000000000000000000, 0.000000000000000000 ) ) ;
#94629 = CARTESIAN_POINT ( 'NONE',  ( -16.87331047859651179, 9.950000000011142376, -113.1500000000000341 ) ) ;
#94628 = UNCERTAINTY_MEASURE_WITH_UNIT (LENGTH_MEASURE( 1.000000000000000082E-05 ), #172462, 'distance_accuracy_value', 'NONE');
#94630 = EDGE_CURVE ( 'NONE', #55457, #87660, #20368, .T. ) ;
#94631 = CARTESIAN_POINT ( 'NONE',  ( -20.89192007715127986, 65.67101464000523947, -130.9404391622479977 ) ) ;
#94632 = CARTESIAN_POINT ( 'NONE',  ( -18.59999999999999787, 80.78317333349157536, -192.9003134612048882 ) ) ;
#94633 = DIRECTION ( 'NONE',  ( 1.000000000000000000, -0.000000000000000000, 0.000000000000000000 ) ) ;
#94634 = AXIS2_PLACEMENT_3D ( 'NONE', #33704, #235696, #256486 ) ;
#94635 = DIRECTION ( 'NONE',  ( -3.265361837132813093E-16, -1.000000000000000000, -6.982962677686266711E-15 ) ) ;
#94636 = CARTESIAN_POINT ( 'NONE',  ( 18.49999999999999289, 10.99842653345846699, -220.2504445088529792 ) ) ;
#94638 = ORIENTED_EDGE ( 'NONE', *, *, #153350, .F. ) ;
#94637 = LINE ( 'NONE', #191210, #44639 ) ;
#94640 = EDGE_LOOP ( 'NONE', ( #101247, #200532, #65848, #101775 ) ) ;
#94639 = PRODUCT_DEFINITION ( 'UNKNOWN', '', #219622, #115799 ) ;
#94642 = CARTESIAN_POINT ( 'NONE',  ( -16.84793658983461029, 51.54252634946470835, -231.9806668642130774 ) ) ;
#94641 = CARTESIAN_POINT ( 'NONE',  ( 20.85000000000000142, 1.115600667400684642E-11, -67.00000000000000000 ) ) ;
#94644 = ORIENTED_EDGE ( 'NONE', *, *, #12959, .F. ) ;
#94643 = DIRECTION ( 'NONE',  ( -1.073024830501117725E-15, 0.000000000000000000, 1.000000000000000000 ) ) ;
#94645 = ORIENTED_EDGE ( 'NONE', *, *, #154936, .F. ) ;
#94646 = CARTESIAN_POINT ( 'NONE',  ( 21.00000000000000000, 66.25000000001151079, -48.27310748452438816 ) ) ;
#94647 = DIRECTION ( 'NONE',  ( 0.000000000000000000, 0.9908441862701605762, 0.1350103645451835310 ) ) ;
#94648 = AXIS2_PLACEMENT_3D ( 'NONE', #238886, #64095, #139755 ) ;
#94650 = ADVANCED_FACE ( 'NONE', ( #59231 ), #81374, .T. ) ;
#94649 = FACE_OUTER_BOUND ( 'NONE', #99513, .T. ) ;
#94651 = CARTESIAN_POINT ( 'NONE',  ( -23.25000000000000000, 85.00000000001197975, -112.9170766071766820 ) ) ;
#94652 = ADVANCED_FACE ( 'NONE', ( #160967 ), #69877, .F. ) ;
#94653 = EDGE_CURVE ( 'NONE', #29202, #93167, #121838, .T. ) ;
#94654 = DIRECTION ( 'NONE',  ( 0.000000000000000000, 0.5859227990963362664, 0.8103668758649469339 ) ) ;
#94655 = CARTESIAN_POINT ( 'NONE',  ( -18.50000000000000000, 9.250000000000001776, -21.25000000000000000 ) ) ;
#94656 = DIRECTION ( 'NONE',  ( 0.000000000000000000, 0.000000000000000000, 1.000000000000000000 ) ) ;
#94657 = ORIENTED_EDGE ( 'NONE', *, *, #256990, .T. ) ;
#94658 = EDGE_LOOP ( 'NONE', ( #21084, #107553, #45058, #252702 ) ) ;
#94659 = EDGE_CURVE ( 'NONE', #216916, #201029, #227867, .T. ) ;
#94660 = AXIS2_PLACEMENT_3D ( 'NONE', #208405, #29784, #190111 ) ;
#94661 = ORIENTED_EDGE ( 'NONE', *, *, #193878, .T. ) ;
#94662 = AXIS2_PLACEMENT_3D ( 'NONE', #66780, #146305, #8099 ) ;
#94664 = CARTESIAN_POINT ( 'NONE',  ( -21.04999999999994387, 76.00000000001119815, -36.02310748452479316 ) ) ;
#94663 = AXIS2_PLACEMENT_3D ( 'NONE', #166737, #105405, #24656 ) ;
#94665 = ORIENTED_EDGE ( 'NONE', *, *, #58551, .F. ) ;
#94666 = DIRECTION ( 'NONE',  ( 0.000000000000000000, -3.339342691255258236E-13, 1.000000000000000000 ) ) ;
#94667 = DIRECTION ( 'NONE',  ( 0.000000000000000000, 0.000000000000000000, 1.000000000000000000 ) ) ;
#94668 = EDGE_LOOP ( 'NONE', ( #131928, #140639, #19559, #103270 ) ) ;
#94669 = CARTESIAN_POINT ( 'NONE',  ( -12.48127053791144903, 66.62341902196808974, -118.8961612375124446 ) ) ;
#94670 = EDGE_LOOP ( 'NONE', ( #22697, #173194, #25890, #92019 ) ) ;
#94671 = DIRECTION ( 'NONE',  ( 0.000000000000000000, 0.2128009952263601179, -0.9770955615653315052 ) ) ;
#94672 = ORIENTED_EDGE ( 'NONE', *, *, #252209, .F. ) ;
#94673 = EDGE_CURVE ( 'NONE', #133332, #114106, #140082, .T. ) ;
#94674 = CARTESIAN_POINT ( 'NONE',  ( 17.74533788810830259, 65.18150020854109528, -92.70948480957680715 ) ) ;
#94675 = VECTOR ( 'NONE', #68036, 1000.000000000000000 ) ;
#94676 = ORIENTED_EDGE ( 'NONE', *, *, #67546, .F. ) ;
#94678 = SPHERICAL_SURFACE ( 'NONE', #206684, 0.1000000000000000056 ) ;
#94677 = CIRCLE ( 'NONE', #128024, 0.09999999999999939493 ) ;
#94679 = ORIENTED_EDGE ( 'NONE', *, *, #131526, .F. ) ;
#94682 = EDGE_LOOP ( 'NONE', ( #238609, #234167, #217563, #35153 ) ) ;
#94681 = CARTESIAN_POINT ( 'NONE',  ( -20.00857864376270001, 63.96254146938299101, -212.9509700271909196 ) ) ;
#94680 = FACE_OUTER_BOUND ( 'NONE', #199228, .T. ) ;
#94683 = CARTESIAN_POINT ( 'NONE',  ( -21.05000000000000071, -0.09999999998884338825, -26.95934304829875927 ) ) ;
#94684 = ORIENTED_EDGE ( 'NONE', *, *, #239023, .T. ) ;
#94685 =( BOUNDED_SURFACE ( )  B_SPLINE_SURFACE ( 3, 2, ( 
 ( #154735, #19043, #218503 ),
 ( #234232, #236798, #76441 ),
 ( #115574, #214670, #255024 ),
 ( #156016, #55567, #98534 ),
 ( #217225, #235516, #116863 ),
 ( #196391, #17742, #197673 ) ),
 .UNSPECIFIED., .F., .F., .T. ) 
 B_SPLINE_SURFACE_WITH_KNOTS ( ( 4, 2, 4 ),
 ( 3, 3 ),
 ( 0.0001792624049599491926, 0.0003686986002124538345, 0.0005581347954649585035 ),
 ( 0.000000000000000000, 1.000000000000000000 ),
 .UNSPECIFIED. ) 
 GEOMETRIC_REPRESENTATION_ITEM ( )  RATIONAL_B_SPLINE_SURFACE ( (
 ( 1.000000000000000000, 0.9238795325112717505, 1.000000000000000000),
 ( 1.000000000000000000, 0.9229318695244472792, 1.000000000000000000),
 ( 1.000000000000000000, 0.8926288119222632877, 1.000000000000000000),
 ( 1.000000000000000000, 0.8123777807279800589, 1.000000000000000000),
 ( 1.000000000000000000, 0.7629087100925328047, 1.000000000000000000),
 ( 1.000000000000000000, 0.7071067811865475727, 1.000000000000000000) ) ) 
 REPRESENTATION_ITEM ( '' )  SURFACE ( )  );
#94686 = CIRCLE ( 'NONE', #173869, 0.09999999999998898659 ) ;
#94687 = ORIENTED_EDGE ( 'NONE', *, *, #21363, .T. ) ;
#94688 = ADVANCED_FACE ( 'NONE', ( #159677 ), #39751, .T. ) ;
#94689 = CARTESIAN_POINT ( 'NONE',  ( -18.50000000000000000, 77.13501884592258762, -162.3061306010920362 ) ) ;
#94690 = ORIENTED_EDGE ( 'NONE', *, *, #228510, .F. ) ;
#94691 = CARTESIAN_POINT ( 'NONE',  ( -20.94999999999999929, 5.850000000011105428, -177.6324972242779268 ) ) ;
#94692 = CARTESIAN_POINT ( 'NONE',  ( 20.95000000000005613, 67.75000000001118394, -25.52310748452478606 ) ) ;
#94693 = DIRECTION ( 'NONE',  ( 0.000000000000000000, 0.000000000000000000, -1.000000000000000000 ) ) ;
#94694 = CARTESIAN_POINT ( 'NONE',  ( -23.49999999999994316, 74.83745509109094485, -43.82310748452479743 ) ) ;
#94695 = EDGE_CURVE ( 'NONE', #67500, #176291, #165746, .T. ) ;
#94696 = DIRECTION ( 'NONE',  ( -1.000000000000000000, 0.000000000000000000, 0.000000000000000000 ) ) ;
#94697 = ORIENTED_EDGE ( 'NONE', *, *, #18930, .T. ) ;
#94698 = DIRECTION ( 'NONE',  ( -1.000000000000000000, 0.000000000000000000, 0.000000000000000000 ) ) ;
#94699 = CARTESIAN_POINT ( 'NONE',  ( 18.47688499308725341, 86.88896063274113146, -199.5328573411169941 ) ) ;
#94700 = DIRECTION ( 'NONE',  ( -1.000000000000000000, 0.000000000000000000, 0.000000000000000000 ) ) ;
#94701 = AXIS2_PLACEMENT_3D ( 'NONE', #69481, #193269, #92864 ) ;
#94702 = ORIENTED_EDGE ( 'NONE', *, *, #78337, .T. ) ;
#94703 = CARTESIAN_POINT ( 'NONE',  ( 22.47071067811866030, 7.522163794833009121, -199.2603376134759117 ) ) ;
#94704 = VERTEX_POINT ( 'NONE', #41027 ) ;
#94705 = CARTESIAN_POINT ( 'NONE',  ( -22.24259225415828212, 33.50553549281345056, -242.7544660500353757 ) ) ;
#94706 = VERTEX_POINT ( 'NONE', #77531 ) ;
#94707 = EDGE_CURVE ( 'NONE', #84436, #48144, #141378, .T. ) ;
#94708 = ADVANCED_FACE ( 'NONE', ( #218330 ), #82299, .F. ) ;
#94709 = DIRECTION ( 'NONE',  ( 0.000000000000000000, 0.000000000000000000, -1.000000000000000000 ) ) ;
#94710 = DIRECTION ( 'NONE',  ( 0.000000000000000000, 1.999342311295302429E-14, -1.000000000000000000 ) ) ;
#94712 = EDGE_LOOP ( 'NONE', ( #190591, #141544, #109589, #75230 ) ) ;
#94711 = DIRECTION ( 'NONE',  ( 1.000000000000000000, 0.000000000000000000, 0.000000000000000000 ) ) ;
#94713 = DIRECTION ( 'NONE',  ( 1.000000000000000000, 0.000000000000000000, 0.000000000000000000 ) ) ;
#94714 = ORIENTED_EDGE ( 'NONE', *, *, #190461, .T. ) ;
#94715 = AXIS2_PLACEMENT_3D ( 'NONE', #182119, #157453, #43888 ) ;
#94716 = CARTESIAN_POINT ( 'NONE',  ( 18.54999999999999716, 10.51799536955200232, -208.1761252362501864 ) ) ;
#94717 = CARTESIAN_POINT ( 'NONE',  ( -16.82542659449987354, 9.934499891438514751, -113.2446356000265268 ) ) ;
#94718 = EDGE_LOOP ( 'NONE', ( #227038, #240743, #180892, #243925 ) ) ;
#94719 = AXIS2_PLACEMENT_3D ( 'NONE', #237351, #160405, #80814 ) ;
#94720 = CARTESIAN_POINT ( 'NONE',  ( 23.24999999999999645, 11.75000000001113953, -42.75000000000000000 ) ) ;
#94721 = DIRECTION ( 'NONE',  ( -0.000000000000000000, -6.982962677686266711E-15, 1.000000000000000000 ) ) ;
#94722 = ORIENTED_EDGE ( 'NONE', *, *, #153278, .F. ) ;
#94723 = FACE_OUTER_BOUND ( 'NONE', #242349, .T. ) ;
#94724 = AXIS2_PLACEMENT_3D ( 'NONE', #51656, #210758, #12584 ) ;
#94725 = TOROIDAL_SURFACE ( 'NONE', #32217, 0.2000000000000000111, 0.1000000000000000056 ) ;
#94726 = ADVANCED_FACE ( 'NONE', ( #1849 ), #194899, .F. ) ;
#94727 = ORIENTED_EDGE ( 'NONE', *, *, #53208, .F. ) ;
#94728 = AXIS2_PLACEMENT_3D ( 'NONE', #142706, #21510, #180571 ) ;
#94729 = CARTESIAN_POINT ( 'NONE',  ( 12.42718393586866732, 9.370655051134638924, -118.0258232559809528 ) ) ;
#94731 = CARTESIAN_POINT ( 'NONE',  ( -20.94999999999999929, 18.82290990851282331, -233.3604470821920529 ) ) ;
#94730 = CIRCLE ( 'NONE', #98796, 0.1000000000000028644 ) ;
#94732 = EDGE_CURVE ( 'NONE', #66589, #18615, #7307, .T. ) ;
#94733 = CIRCLE ( 'NONE', #240491, 11.80000000000000426 ) ;
#94735 = ORIENTED_EDGE ( 'NONE', *, *, #224421, .T. ) ;
#94734 = DIRECTION ( 'NONE',  ( 0.7071067811865388020, -0.7071067811865561215, 0.000000000000000000 ) ) ;
#94736 = CARTESIAN_POINT ( 'NONE',  ( -23.25000000000000000, 40.44624540816119662, -247.8544895606997329 ) ) ;
#94737 = CARTESIAN_POINT ( 'NONE',  ( 21.05000000000000071, 84.66355140188147743, -160.4990063664569959 ) ) ;
#94738 = ADVANCED_FACE ( 'NONE', ( #63117 ), #219686, .F. ) ;
#94739 = CARTESIAN_POINT ( 'NONE',  ( 21.05000000000000071, -11.74999999998883560, -63.89999999999999858 ) ) ;
#94740 = DIRECTION ( 'NONE',  ( -0.5932847527679310229, -0.8049926720990042694, -4.984624513800578906E-15 ) ) ;
#94741 = CARTESIAN_POINT ( 'NONE',  ( -20.85000000000000142, 74.95904887477786360, -233.7774272632847783 ) ) ;
#94742 = EDGE_CURVE ( 'NONE', #144670, #55413, #173956, .T. ) ;
#94743 = VECTOR ( 'NONE', #79488, 1000.000000000000000 ) ;
#94744 = CARTESIAN_POINT ( 'NONE',  ( 18.42555734704283665, -9.497158361925555070, -40.53983049773493974 ) ) ;
#94745 = CARTESIAN_POINT ( 'NONE',  ( 23.14999999999999858, 71.00000000001151079, -47.92837350343745584 ) ) ;
#94746 = VERTEX_POINT ( 'NONE', #107389 ) ;
#94747 = EDGE_LOOP ( 'NONE', ( #74524, #76286, #222974, #2399, #193531, #171626, #70428, #43836, #163605 ) ) ;
#94749 = CARTESIAN_POINT ( 'NONE',  ( -20.94999999999999929, 64.35000000001214460, -136.5231074845244166 ) ) ;
#94748 = AXIS2_PLACEMENT_3D ( 'NONE', #113376, #132954, #129092 ) ;
#94750 = CIRCLE ( 'NONE', #78181, 11.80000000000000426 ) ;
#94752 = ORIENTED_EDGE ( 'NONE', *, *, #81937, .T. ) ;
#94751 = DIRECTION ( 'NONE',  ( 0.000000000000000000, 0.000000000000000000, 1.000000000000000000 ) ) ;
#94753 = AXIS2_PLACEMENT_3D ( 'NONE', #14521, #253088, #57452 ) ;
#94754 = VERTEX_POINT ( 'NONE', #102217 ) ;
#94755 = CARTESIAN_POINT ( 'NONE',  ( -21.05000000000000071, 11.65000000001115588, -67.10000000000005116 ) ) ;
#94756 = ORIENTED_EDGE ( 'NONE', *, *, #58044, .F. ) ;
#94757 = CARTESIAN_POINT ( 'NONE',  ( -22.39999999999999858, 11.75000000001115552, -167.4999999999999716 ) ) ;
#94758 = ADVANCED_FACE ( 'NONE', ( #181800 ), #227339, .F. ) ;
#94759 = EDGE_CURVE ( 'NONE', #116058, #23751, #132396, .T. ) ;
#94760 = VERTEX_POINT ( 'NONE', #5700 ) ;
#94761 = CARTESIAN_POINT ( 'NONE',  ( 22.60000000000000142, 0.1008583691098682150, -21.75043287651061164 ) ) ;
#94764 = ORIENTED_EDGE ( 'NONE', *, *, #171039, .F. ) ;
#94763 = EDGE_LOOP ( 'NONE', ( #244144, #172518, #140064 ) ) ;
#94762 = VECTOR ( 'NONE', #228224, 1000.000000000000000 ) ;
#94765 = VERTEX_POINT ( 'NONE', #147822 ) ;
#94766 = CONICAL_SURFACE ( 'NONE', #40664, 4.299999999999953637, 0.7853981633974466137 ) ;
#94767 = AXIS2_PLACEMENT_3D ( 'NONE', #208094, #242055, #243339 ) ;
#94768 = ORIENTED_EDGE ( 'NONE', *, *, #47847, .T. ) ;
#94769 = ORIENTED_EDGE ( 'NONE', *, *, #140464, .F. ) ;
#94770 = FACE_OUTER_BOUND ( 'NONE', #110403, .T. ) ;
#94771 = CARTESIAN_POINT ( 'NONE',  ( -20.94999999999999929, 0.2561057920922211739, 0.03489644167229202787 ) ) ;
#94772 = DIRECTION ( 'NONE',  ( 0.000000000000000000, 0.000000000000000000, -1.000000000000000000 ) ) ;
#94773 = ORIENTED_EDGE ( 'NONE', *, *, #18221, .F. ) ;
#94774 = CARTESIAN_POINT ( 'NONE',  ( 20.53930447208009014, 40.69342982378280738, -237.9069413209054744 ) ) ;
#94775 = DIRECTION ( 'NONE',  ( 1.000000000000000000, -0.000000000000000000, 0.000000000000000000 ) ) ;
#94777 = ORIENTED_EDGE ( 'NONE', *, *, #79073, .T. ) ;
#94776 = FACE_OUTER_BOUND ( 'NONE', #93851, .T. ) ;
#94778 = DIRECTION ( 'NONE',  ( 1.000000000000000000, 0.000000000000000000, 0.000000000000000000 ) ) ;
#94779 = EDGE_LOOP ( 'NONE', ( #157616, #103823 ) ) ;
#94780 = DIRECTION ( 'NONE',  ( 0.000000000000000000, 6.982962677686266711E-15, -1.000000000000000000 ) ) ;
#94782 = ORIENTED_EDGE ( 'NONE', *, *, #218, .T. ) ;
#94781 = CARTESIAN_POINT ( 'NONE',  ( 23.24999999999999289, 6.550000000011156231, -88.35000000000003695 ) ) ;
#94783 = TOROIDAL_SURFACE ( 'NONE', #240543, 0.2000000000000000111, 0.1000000000000000056 ) ;
#94784 = DIRECTION ( 'NONE',  ( 1.000000000000000000, 0.000000000000000000, 0.000000000000000000 ) ) ;
#94785 = CARTESIAN_POINT ( 'NONE',  ( -20.54999999999999716, 19.73066058418984170, -238.2142830767208466 ) ) ;
#94786 = AXIS2_PLACEMENT_3D ( 'NONE', #31340, #249084, #109536 ) ;
#94787 = VERTEX_POINT ( 'NONE', #145225 ) ;
#94789 = DIRECTION ( 'NONE',  ( 0.000000000000000000, 0.000000000000000000, -1.000000000000000000 ) ) ;
#94788 = CARTESIAN_POINT ( 'NONE',  ( -16.92209698673556417, 9.950000000011138823, -121.2893644329473659 ) ) ;
#94790 = AXIS2_PLACEMENT_3D ( 'NONE', #190826, #53852, #228654 ) ;
#94791 = ADVANCED_FACE ( 'NONE', ( #146502 ), #205195, .T. ) ;
#94792 = CARTESIAN_POINT ( 'NONE',  ( 21.05000000000000071, 10.72371710471867701, -134.0000000000000000 ) ) ;
#94793 = CARTESIAN_POINT ( 'NONE',  ( -18.59999999999999787, 1.750000000011155743, -145.6695115579016715 ) ) ;
#94794 = ORIENTED_EDGE ( 'NONE', *, *, #7077, .T. ) ;
#94795 = ORIENTED_EDGE ( 'NONE', *, *, #81319, .F. ) ;
#94796 = CIRCLE ( 'NONE', #69880, 0.09999999999999939493 ) ;
#94797 = CARTESIAN_POINT ( 'NONE',  ( -23.25000000000000000, 85.00000000001179501, -78.81707660717668773 ) ) ;
#94798 = ORIENTED_EDGE ( 'NONE', *, *, #164141, .T. ) ;
#94799 = DIRECTION ( 'NONE',  ( 0.000000000000000000, 0.2128009952264106608, -0.9770955615653206250 ) ) ;
#94800 = ORIENTED_EDGE ( 'NONE', *, *, #205266, .T. ) ;
#94801 = CARTESIAN_POINT ( 'NONE',  ( -20.54999999999999716, 74.00000000001254818, -183.2477294072864709 ) ) ;
#94802 = CARTESIAN_POINT ( 'NONE',  ( -14.00000000000000178, 66.15000000001155911, -52.77310748452439526 ) ) ;
#94803 = AXIS2_PLACEMENT_3D ( 'NONE', #71341, #167881, #49184 ) ;
#94804 = AXIS2_PLACEMENT_3D ( 'NONE', #238515, #247505, #109260 ) ;
#94805 = CIRCLE ( 'NONE', #190524, 12.97499999999998721 ) ;
#94806 = VERTEX_POINT ( 'NONE', #26599 ) ;
#94807 = VECTOR ( 'NONE', #256205, 1000.000000000000000 ) ;
#94808 = DIRECTION ( 'NONE',  ( 0.000000000000000000, 0.2617529984164915779, 0.9651348961777189706 ) ) ;
#94809 =( NAMED_UNIT ( * ) SI_UNIT ( $, .STERADIAN. ) SOLID_ANGLE_UNIT ( ) );
#94810 = EDGE_CURVE ( 'NONE', #55017, #152124, #103523, .T. ) ;
#94811 = TOROIDAL_SURFACE ( 'NONE', #240565, 0.2000000000000000111, 0.1000000000000000056 ) ;
#94812 = ORIENTED_EDGE ( 'NONE', *, *, #202823, .F. ) ;
#94813 = ORIENTED_EDGE ( 'NONE', *, *, #224870, .F. ) ;
#94814 = ORIENTED_EDGE ( 'NONE', *, *, #217932, .F. ) ;
#94815 = CARTESIAN_POINT ( 'NONE',  ( -16.77683809663752257, 66.05416425680742520, -56.85915846542017960 ) ) ;
#94816 = CARTESIAN_POINT ( 'NONE',  ( 21.05000000000000071, 70.97296516614450468, -234.1788952109995137 ) ) ;
#94817 = DIRECTION ( 'NONE',  ( 0.000000000000000000, -0.4721928772777346239, -0.8814952561688430555 ) ) ;
#94818 = CARTESIAN_POINT ( 'NONE',  ( -21.05000000000000071, 75.74389420792016381, -170.0580039261966476 ) ) ;
#94819 = CARTESIAN_POINT ( 'NONE',  ( 15.74999999999999645, 66.65000000001204228, -119.7731074845243739 ) ) ;
#94821 = DIRECTION ( 'NONE',  ( -0.000000000000000000, 1.000000000000000000, 6.982962677686266711E-15 ) ) ;
#94820 = DIRECTION ( 'NONE',  ( 0.000000000000000000, 0.000000000000000000, 1.000000000000000000 ) ) ;
#94823 = ORIENTED_EDGE ( 'NONE', *, *, #194355, .T. ) ;
#94822 = DIRECTION ( 'NONE',  ( -2.827886303505249259E-16, 0.8660254037844412611, 0.4999999999999956701 ) ) ;
#94824 = CARTESIAN_POINT ( 'NONE',  ( -16.86578989773641979, 9.984809801269951990, -79.53533511337781192 ) ) ;
#94825 = ORIENTED_EDGE ( 'NONE', *, *, #143594, .F. ) ;
#94826 = CARTESIAN_POINT ( 'NONE',  ( 20.85000000000000142, 7.021664781911246322, -204.8335654018972605 ) ) ;
#94827 = ORIENTED_EDGE ( 'NONE', *, *, #5739, .T. ) ;
#94828 = ORIENTED_EDGE ( 'NONE', *, *, #177329, .F. ) ;
#94829 = DIRECTION ( 'NONE',  ( -1.000000000000000000, 0.000000000000000000, 0.000000000000000000 ) ) ;
#94830 = VECTOR ( 'NONE', #237955, 1000.000000000000227 ) ;
#94831 = DIRECTION ( 'NONE',  ( 0.7071359030028288029, 0.000000000000000000, -0.7070776581708504427 ) ) ;
#94832 = PLANE ( 'NONE',  #133634 ) ;
#94833 = FACE_OUTER_BOUND ( 'NONE', #147938, .T. ) ;
#94834 = DIRECTION ( 'NONE',  ( 1.000000000000000000, 0.000000000000000000, 0.000000000000000000 ) ) ;
#94835 = VERTEX_POINT ( 'NONE', #3137 ) ;
#94836 = ORIENTED_EDGE ( 'NONE', *, *, #56662, .F. ) ;
#94837 = DIRECTION ( 'NONE',  ( 1.000000000000000000, 0.000000000000000000, 0.000000000000000000 ) ) ;
#94838 = EDGE_LOOP ( 'NONE', ( #212837, #138, #257970, #144992, #185778, #181367, #168227, #58549, #61680, #62268, #88638 ) ) ;
#94839 = CARTESIAN_POINT ( 'NONE',  ( -18.50000000000000000, 52.32046880629621199, -232.2896150449452364 ) ) ;
#94840 = DIRECTION ( 'NONE',  ( -1.000000000000000000, 7.304098846218134667E-16, 4.217023435051625732E-16 ) ) ;
#94841 = EDGE_LOOP ( 'NONE', ( #162156, #63985, #121656, #91202 ) ) ;
#94842 = DIRECTION ( 'NONE',  ( 0.000000000000000000, 0.000000000000000000, -1.000000000000000000 ) ) ;
#94843 = CARTESIAN_POINT ( 'NONE',  ( -18.59999999999999787, 1.115600667400684642E-11, -134.0000000000000284 ) ) ;
#94844 = CARTESIAN_POINT ( 'NONE',  ( -21.05000000000000426, 6.195222845121298505, -199.6891624788988224 ) ) ;
#94845 = CARTESIAN_POINT ( 'NONE',  ( 18.39999999999999503, 23.69729366125098835, -229.5924034189314682 ) ) ;
#94846 = ORIENTED_EDGE ( 'NONE', *, *, #215318, .T. ) ;
#94847 = CYLINDRICAL_SURFACE ( 'NONE', #171108, 0.09999999999999781286 ) ;
#94848 = CARTESIAN_POINT ( 'NONE',  ( -5.999999999999938716, 64.35000000001120668, -26.02310748452479316 ) ) ;
#94849 = ADVANCED_FACE ( 'NONE', ( #43577 ), #99049, .T. ) ;
#94850 = AXIS2_PLACEMENT_3D ( 'NONE', #201680, #206820, #145549 ) ;
#94852 = CIRCLE ( 'NONE', #90742, 0.09999999999999062417 ) ;
#94851 = PLANE ( 'NONE',  #28255 ) ;
#94853 = TOROIDAL_SURFACE ( 'NONE', #15791, 0.2000000000000000111, 0.1000000000000000056 ) ;
#94854 = VERTEX_POINT ( 'NONE', #185654 ) ;
#94855 = EDGE_CURVE ( 'NONE', #112788, #221278, #57362, .T. ) ;
#94856 = DIRECTION ( 'NONE',  ( 0.000000000000000000, -0.9876197685951263461, 0.1568667991644794590 ) ) ;
#94857 = VERTEX_POINT ( 'NONE', #246897 ) ;
#94858 = DIRECTION ( 'NONE',  ( -1.000000000000000000, -0.000000000000000000, -0.000000000000000000 ) ) ;
#94859 = CYLINDRICAL_SURFACE ( 'NONE', #216831, 0.09999999999999939493 ) ;
#94860 = EDGE_CURVE ( 'NONE', #7235, #140173, #124041, .T. ) ;
#94861 = DIRECTION ( 'NONE',  ( -0.7071067811865474617, -0.3338907855510734324, -0.6233112732207618523 ) ) ;
#94862 = CYLINDRICAL_SURFACE ( 'NONE', #218996, 0.09999999999999939493 ) ;
#94863 = CARTESIAN_POINT ( 'NONE',  ( 22.39999999999999503, 64.35000000001237197, -170.1231074845244393 ) ) ;
#94864 = FACE_OUTER_BOUND ( 'NONE', #134437, .T. ) ;
#94865 = ORIENTED_EDGE ( 'NONE', *, *, #236139, .T. ) ;
#94866 = DIRECTION ( 'NONE',  ( 9.044546369203337730E-15, 0.8900778951570211817, 0.4558084472153261513 ) ) ;
#94867 = CARTESIAN_POINT ( 'NONE',  ( 21.06600267594171783, 67.22483393081216718, -124.3188447021496188 ) ) ;
#94868 = VECTOR ( 'NONE', #177132, 1000.000000000000000 ) ;
#94869 = DIRECTION ( 'NONE',  ( -1.000000000000000000, -0.000000000000000000, 0.000000000000000000 ) ) ;
#94870 = CARTESIAN_POINT ( 'NONE',  ( -21.14999999999999858, 11.65000000001115588, -40.28386566297815108 ) ) ;
#94871 = CONICAL_SURFACE ( 'NONE', #194859, 7.750000000000013323, 0.7853981633974531640 ) ;
#94872 = EDGE_CURVE ( 'NONE', #133775, #193922, #68283, .T. ) ;
#94873 = CARTESIAN_POINT ( 'NONE',  ( 21.05000000000000071, -9.000000000000001776, -9.893969122652443104 ) ) ;
#94874 = AXIS2_PLACEMENT_3D ( 'NONE', #252877, #74285, #134207 ) ;
#94875 = EDGE_LOOP ( 'NONE', ( #183144, #75996, #14493, #198352 ) ) ;
#94876 = ORIENTED_EDGE ( 'NONE', *, *, #139948, .F. ) ;
#94877 = CARTESIAN_POINT ( 'NONE',  ( -20.94999999999999929, 64.25000000001161027, -62.50830171387040934 ) ) ;
#94878 = CARTESIAN_POINT ( 'NONE',  ( 18.59999999999996945, 14.80545736607782814, -235.9842437978701639 ) ) ;
#94879 = CARTESIAN_POINT ( 'NONE',  ( 18.60000000000000497, -9.523946312317709939, -40.38202799533822684 ) ) ;
#94880 = DIRECTION ( 'NONE',  ( 0.000000000000000000, 0.2605042016806672911, -0.9654727137038716656 ) ) ;
#94881 = DIRECTION ( 'NONE',  ( -0.000000000000000000, -6.982962677686266711E-15, 1.000000000000000000 ) ) ;
#94882 = ADVANCED_FACE ( 'NONE', ( #142648 ), #123118, .T. ) ;
#94883 = ORIENTED_EDGE ( 'NONE', *, *, #100332, .T. ) ;
#94884 = FACE_OUTER_BOUND ( 'NONE', #94188, .T. ) ;
#94885 = DIRECTION ( 'NONE',  ( 0.000000000000000000, -6.467318590049456648E-15, 1.000000000000000000 ) ) ;
#94886 = ORIENTED_EDGE ( 'NONE', *, *, #181788, .F. ) ;
#94887 = CARTESIAN_POINT ( 'NONE',  ( -16.97683809663752186, 12.47642768288816661, -211.9993005936845805 ) ) ;
#94888 = DIRECTION ( 'NONE',  ( 0.000000000000000000, -0.9651348961776677893, 0.2617529984166795387 ) ) ;
#94889 = TOROIDAL_SURFACE ( 'NONE', #190600, 3.899999999999999467, 0.1000000000000000056 ) ;
#94890 = VERTEX_POINT ( 'NONE', #143944 ) ;
#94891 = CARTESIAN_POINT ( 'NONE',  ( -21.03922262424674017, 12.81730801556627952, -205.2285241112374194 ) ) ;
#94892 = ORIENTED_EDGE ( 'NONE', *, *, #154429, .T. ) ;
#94893 = DIRECTION ( 'NONE',  ( 0.000000000000000000, -1.186135710069611419E-15, 1.000000000000000000 ) ) ;
#94894 = DIRECTION ( 'NONE',  ( 1.000000000000000000, 0.000000000000000000, 0.000000000000000000 ) ) ;
#94895 = AXIS2_PLACEMENT_3D ( 'NONE', #69584, #149123, #43586 ) ;
#94896 = DIRECTION ( 'NONE',  ( 0.000000000000000000, -0.2617529984165152257, -0.9651348961777124202 ) ) ;
#94897 = CARTESIAN_POINT ( 'NONE',  ( -18.50000000000000000, 64.35000000001191722, -103.0231074845243882 ) ) ;
#94898 = DIRECTION ( 'NONE',  ( 0.000000000000000000, 6.982962677686266711E-15, -1.000000000000000000 ) ) ;
#94899 = DIRECTION ( 'NONE',  ( 1.000000000000000000, 0.000000000000000000, 0.000000000000000000 ) ) ;
#94900 = CARTESIAN_POINT ( 'NONE',  ( -18.59999999999999787, 68.97833521811233481, -166.1895420826271277 ) ) ;
#94901 = CARTESIAN_POINT ( 'NONE',  ( -20.64999999999999858, 76.00000000001141132, -34.02310748452431710 ) ) ;
#94903 = LINE ( 'NONE', #253973, #41534 ) ;
#94902 = CARTESIAN_POINT ( 'NONE',  ( 20.95566103547454517, 10.61824765095822087, -108.1318401929806186 ) ) ;
#94904 = DIRECTION ( 'NONE',  ( 1.000000000000000000, 0.000000000000000000, 0.000000000000000000 ) ) ;
#94905 = CARTESIAN_POINT ( 'NONE',  ( -18.59999999999999787, 68.97833521811159585, -65.68954208262705663 ) ) ;
#94906 = FACE_OUTER_BOUND ( 'NONE', #81250, .T. ) ;
#94907 = CARTESIAN_POINT ( 'NONE',  ( 20.95539060131842746, 18.89207542883556101, -227.9818558096623065 ) ) ;
#94908 = AXIS2_PLACEMENT_3D ( 'NONE', #257524, #238014, #663 ) ;
#94909 = ORIENTED_EDGE ( 'NONE', *, *, #120150, .F. ) ;
#94910 = TOROIDAL_SURFACE ( 'NONE', #128249, 0.2000000000000000111, 0.1000000000000000056 ) ;
#94911 = CYLINDRICAL_SURFACE ( 'NONE', #8063, 0.09999999999999939493 ) ;
#94912 = PLANE ( 'NONE',  #107865 ) ;
#94913 = ADVANCED_FACE ( 'NONE', ( #44859 ), #252042, .T. ) ;
#94914 = CIRCLE ( 'NONE', #219811, 0.9000000000000014655 ) ;
#94915 = ORIENTED_EDGE ( 'NONE', *, *, #243718, .F. ) ;
#94916 = CARTESIAN_POINT ( 'NONE',  ( -17.04761207306817283, 65.97354912661374726, -48.67310748452440805 ) ) ;
#94917 = CARTESIAN_POINT ( 'NONE',  ( -23.25000000000000000, -1.835859311432481045, -112.1044391687985780 ) ) ;
#94918 = EDGE_CURVE ( 'NONE', #50852, #44809, #11613, .T. ) ;
#94919 = ORIENTED_EDGE ( 'NONE', *, *, #145765, .T. ) ;
#94920 = CARTESIAN_POINT ( 'NONE',  ( 23.15000000000000213, 84.59626168225560150, -194.0729799673740104 ) ) ;
#94921 = ORIENTED_EDGE ( 'NONE', *, *, #136026, .F. ) ;
#94922 = EDGE_CURVE ( 'NONE', #60388, #30618, #169859, .T. ) ;
#94923 = DIRECTION ( 'NONE',  ( 0.000000000000000000, 0.8814952561688430555, -0.4721928772777346239 ) ) ;
#94924 = AXIS2_PLACEMENT_3D ( 'NONE', #209095, #111289, #145575 ) ;
#94925 = AXIS2_PLACEMENT_3D ( 'NONE', #164670, #248046, #66848 ) ;
#94926 = AXIS2_PLACEMENT_3D ( 'NONE', #105318, #85755, #87056 ) ;
#94927 = AXIS2_PLACEMENT_3D ( 'NONE', #176534, #218180, #42155 ) ;
#94929 = EDGE_LOOP ( 'NONE', ( #5636, #242334, #58725, #71960 ) ) ;
#94928 = VECTOR ( 'NONE', #79265, 1000.000000000000000 ) ;
#94930 = CARTESIAN_POINT ( 'NONE',  ( 18.52928932188134326, 65.72071067813062939, -111.8145288407616960 ) ) ;
#94931 = EDGE_CURVE ( 'NONE', #43099, #153815, #119759, .T. ) ;
#94932 = EDGE_LOOP ( 'NONE', ( #233902, #224193, #172161, #58181 ) ) ;
#94933 = CIRCLE ( 'NONE', #161622, 4.049999999999998934 ) ;
#94934 = DIRECTION ( 'NONE',  ( -1.000000000000000000, -0.000000000000000000, -0.000000000000000000 ) ) ;
#94936 = CARTESIAN_POINT ( 'NONE',  ( 18.59999999999997655, 1.115600667400684642E-11, -100.5000000000000426 ) ) ;
#94935 = PRODUCT_DEFINITION_CONTEXT ( 'detailed design', #165871, 'design' ) ;
#94937 = EDGE_CURVE ( 'NONE', #74571, #147215, #244807, .T. ) ;
#94938 = CARTESIAN_POINT ( 'NONE',  ( 23.15000000000000213, -11.64999999998883595, -97.40000000000004832 ) ) ;
#94939 = EDGE_CURVE ( 'NONE', #40931, #113219, #3197, .T. ) ;
#94940 = CARTESIAN_POINT ( 'NONE',  ( -16.83199030136657726, 9.930648033113465445, -12.77240102265748156 ) ) ;
#94941 = CARTESIAN_POINT ( 'NONE',  ( -15.75000000000000000, 47.91396133265956792, -234.2636761031307913 ) ) ;
#94942 = DIRECTION ( 'NONE',  ( 0.000000000000000000, -0.000000000000000000, 1.000000000000000000 ) ) ;
#94943 = CARTESIAN_POINT ( 'NONE',  ( -20.54999999999999716, 0.000000000000000000, -31.50000000000000000 ) ) ;
#94945 = ORIENTED_EDGE ( 'NONE', *, *, #62336, .T. ) ;
#94944 = CARTESIAN_POINT ( 'NONE',  ( 21.05000000000000071, 69.58602111852350447, -102.9373083682503562 ) ) ;
#94946 = ORIENTED_EDGE ( 'NONE', *, *, #35618, .F. ) ;
#94948 = DIRECTION ( 'NONE',  ( 0.000000000000000000, -0.4999999999999929501, -0.8660254037844427044 ) ) ;
#94947 = CARTESIAN_POINT ( 'NONE',  ( -21.05000000000000426, 6.270085863689140560, 0.03486800301310564315 ) ) ;
#94949 = ORIENTED_EDGE ( 'NONE', *, *, #191369, .T. ) ;
#94951 = ORIENTED_EDGE ( 'NONE', *, *, #252223, .T. ) ;
#94950 = SURFACE_STYLE_USAGE ( .BOTH. , #171978 ) ;
#94952 = VECTOR ( 'NONE', #64351, 1000.000000000000000 ) ;
#94953 = ORIENTED_EDGE ( 'NONE', *, *, #132307, .F. ) ;
#94954 = LINE ( 'NONE', #254027, #48762 ) ;
#94955 = STYLED_ITEM ( 'NONE', ( #179071 ), #20540 ) ;
#94956 = AXIS2_PLACEMENT_3D ( 'NONE', #48678, #152966, #232487 ) ;
#94957 = PLANE ( 'NONE',  #221897 ) ;
#94958 = EDGE_CURVE ( 'NONE', #216037, #92030, #240550, .T. ) ;
#94959 = CLOSED_SHELL ( 'NONE', ( #61817, #203578, #167434, #59164, #246017, #114096, #124125, #232802, #162605, #191597, #85392, #103413, #85349, #71844, #231006, #35411, #211705, #244319, #68528, #128771, #107199, #83728, #48466, #120602, #237972, #94913, #198184, #121850, #6194, #111797, #229272, #54755, #188330, #91793, #228322, #438, #31503, #59019, #134815, #150870, #4604, #236946, #72942, #61663, #215669, #82706, #75321, #77343, #186495, #170325, #191731, #49682, #122838 ) ) ;
#94960 = CARTESIAN_POINT ( 'NONE',  ( -18.59999999999999787, -9.399999999988787991, -107.7972597596633193 ) ) ;
#94961 = CYLINDRICAL_SURFACE ( 'NONE', #151736, 0.5000000000000008882 ) ;
#94962 = DIRECTION ( 'NONE',  ( 0.000000000000000000, 0.000000000000000000, -1.000000000000000000 ) ) ;
#94963 = EDGE_CURVE ( 'NONE', #92943, #202854, #153101, .T. ) ;
#94964 = ADVANCED_FACE ( 'NONE', ( #55095 ), #248199, .T. ) ;
#94965 = CARTESIAN_POINT ( 'NONE',  ( -18.39999999999999858, 20.76715588789282307, -228.0228088279911560 ) ) ;
#94966 = FACE_OUTER_BOUND ( 'NONE', #44546, .T. ) ;
#94967 = AXIS2_PLACEMENT_3D ( 'NONE', #137781, #58246, #201619 ) ;
#94968 = AXIS2_PLACEMENT_3D ( 'NONE', #11442, #247462, #128817 ) ;
#94969 = DIRECTION ( 'NONE',  ( 0.000000000000000000, 0.2617529984165035684, 0.9651348961777156399 ) ) ;
#94970 = ORIENTED_EDGE ( 'NONE', *, *, #126454, .F. ) ;
#94971 = ORIENTED_EDGE ( 'NONE', *, *, #160181, .T. ) ;
#94972 = FACE_OUTER_BOUND ( 'NONE', #16244, .T. ) ;
#94973 = CONICAL_SURFACE ( 'NONE', #240731, 4.049999999999998046, 0.7853981633974604915 ) ;
#94974 = ORIENTED_EDGE ( 'NONE', *, *, #29329, .T. ) ;
#94975 = CARTESIAN_POINT ( 'NONE',  ( -20.64999999999999858, 76.00000000001190870, -103.0231074845243029 ) ) ;
#94976 = ORIENTED_EDGE ( 'NONE', *, *, #200971, .T. ) ;
#94977 = CARTESIAN_POINT ( 'NONE',  ( -18.40000000000000213, 5.649999999999983480, -20.85000000000000142 ) ) ;
#94978 = VECTOR ( 'NONE', #118861, 1000.000000000000000 ) ;
#94979 = EDGE_CURVE ( 'NONE', #221570, #213669, #207815, .T. ) ;
#94980 = DIRECTION ( 'NONE',  ( 0.000000000000000000, 0.000000000000000000, -1.000000000000000000 ) ) ;
#94981 = LINE ( 'NONE', #194112, #101225 ) ;
#94982 = ADVANCED_FACE ( 'NONE', ( #152986 ), #232509, .T. ) ;
#94984 = EDGE_LOOP ( 'NONE', ( #110227, #17090, #87982, #26162 ) ) ;
#94983 = DIRECTION ( 'NONE',  ( -3.265361837132813093E-16, -1.000000000000000000, -7.086529944415894657E-15 ) ) ;
#94985 = VERTEX_POINT ( 'NONE', #154284 ) ;
#94986 = AXIS2_PLACEMENT_3D ( 'NONE', #90875, #93434, #34793 ) ;
#94987 = DIRECTION ( 'NONE',  ( -0.000000000000000000, 0.8103668758649578141, -0.5859227990963212784 ) ) ;
#94988 = DIRECTION ( 'NONE',  ( 0.000000000000000000, -0.8700118002898357128, 0.4930308989875171188 ) ) ;
#94989 = AXIS2_PLACEMENT_3D ( 'NONE', #132703, #33642, #234348 ) ;
#94991 = CARTESIAN_POINT ( 'NONE',  ( 23.14999999999999503, 64.35000000001228670, -157.7731074845244450 ) ) ;
#94990 = AXIS2_PLACEMENT_3D ( 'NONE', #120527, #235299, #215727 ) ;
#94992 = EDGE_CURVE ( 'NONE', #101907, #112448, #29195, .T. ) ;
#94993 = CARTESIAN_POINT ( 'NONE',  ( 18.49999999999999289, 29.08883969319483498, -237.9520757887960940 ) ) ;
#94994 = TOROIDAL_SURFACE ( 'NONE', #182510, 11.90000000000000391, 0.1000000000000000056 ) ;
#94995 = CARTESIAN_POINT ( 'NONE',  ( -21.44999999999999929, 63.34400729675436281, -222.1083394899400503 ) ) ;
#94996 = EDGE_LOOP ( 'NONE', ( #194273, #45039, #240607, #33809 ) ) ;
#94998 = DIRECTION ( 'NONE',  ( -1.000000000000000000, 0.000000000000000000, 0.000000000000000000 ) ) ;
#94997 = CARTESIAN_POINT ( 'NONE',  ( -21.37071067811865532, 67.92928932189285263, -48.27310748452438105 ) ) ;
#94999 = VERTEX_POINT ( 'NONE', #168712 ) ;
#95002 = EDGE_LOOP ( 'NONE', ( #211396, #123372, #234252, #80690 ) ) ;
#95001 = CARTESIAN_POINT ( 'NONE',  ( -18.39999999999999858, -9.399999999988850163, -122.2500000000000284 ) ) ;
#95000 = DIRECTION ( 'NONE',  ( 0.000000000000000000, 0.000000000000000000, 1.000000000000000000 ) ) ;
#95003 = CIRCLE ( 'NONE', #65960, 0.09999999999999982514 ) ;
#95004 = DIRECTION ( 'NONE',  ( -1.000000000000000000, -3.427148797533456523E-14, -5.467925025959484217E-15 ) ) ;
#95005 = ORIENTED_EDGE ( 'NONE', *, *, #61637, .F. ) ;
#95006 = DIRECTION ( 'NONE',  ( 0.000000000000000000, 0.4088369013363283844, -0.9126074666063769270 ) ) ;
#95007 = LINE ( 'NONE', #173323, #244604 ) ;
#95008 = CARTESIAN_POINT ( 'NONE',  ( -21.14999999999999858, -11.64999999998884483, -167.4999999999999432 ) ) ;
#95010 = ORIENTED_EDGE ( 'NONE', *, *, #29971, .F. ) ;
#95009 = CARTESIAN_POINT ( 'NONE',  ( 21.14999999999999858, 64.35000000001228670, -157.8731074845244393 ) ) ;
#95011 = AXIS2_PLACEMENT_3D ( 'NONE', #20890, #3863, #139508 ) ;
#95012 = ADVANCED_FACE ( 'NONE', ( #233779 ), #51246, .F. ) ;
#95013 = ORIENTED_EDGE ( 'NONE', *, *, #114926, .T. ) ;
#95014 = ADVANCED_FACE ( 'NONE', ( #210364 ), #129538, .T. ) ;
#95015 = DIRECTION ( 'NONE',  ( 1.000000000000000000, 0.000000000000000000, 0.000000000000000000 ) ) ;
#95016 = LINE ( 'NONE', #252799, #199208 ) ;
#95017 = CARTESIAN_POINT ( 'NONE',  ( -16.77902162784673834, 44.14788894467815084, -235.2972969561471075 ) ) ;
#95018 = CIRCLE ( 'NONE', #174174, 12.77500000000000036 ) ;
#95019 = DIRECTION ( 'NONE',  ( -3.440080580676165868E-14, -0.1298341882520124002, -0.9915357197604841577 ) ) ;
#95020 = ORIENTED_EDGE ( 'NONE', *, *, #24391, .T. ) ;
#95021 = DIRECTION ( 'NONE',  ( -3.265361837132813093E-16, 1.000000000000000000, 0.000000000000000000 ) ) ;
#95022 = ADVANCED_FACE ( 'NONE', ( #130810 ), #30448, .F. ) ;
#95023 = EDGE_CURVE ( 'NONE', #180003, #234900, #148985, .T. ) ;
#95024 = DIRECTION ( 'NONE',  ( -0.000000000000000000, 0.000000000000000000, 1.000000000000000000 ) ) ;
#95025 = DIRECTION ( 'NONE',  ( 0.000000000000000000, 0.1298341882519953583, 0.9915357197604862671 ) ) ;
#95026 = ORIENTED_EDGE ( 'NONE', *, *, #223798, .F. ) ;
#95027 = CARTESIAN_POINT ( 'NONE',  ( 20.53930447207968157, 60.77696664501686996, -225.3571726667190376 ) ) ;
#95028 = ADVANCED_FACE ( 'NONE', ( #91689 ), #211655, .F. ) ;
#95029 = DIRECTION ( 'NONE',  ( 1.000000000000000000, -1.541976423090492636E-14, 0.000000000000000000 ) ) ;
#95030 = ORIENTED_EDGE ( 'NONE', *, *, #22922, .F. ) ;
#95031 = TOROIDAL_SURFACE ( 'NONE', #240794, 0.2000000000000000111, 0.1000000000000000056 ) ;
#95032 = AXIS2_PLACEMENT_3D ( 'NONE', #172543, #252017, #226003 ) ;
#95034 = AXIS2_PLACEMENT_3D ( 'NONE', #47591, #170175, #147999 ) ;
#95033 = DIRECTION ( 'NONE',  ( -0.000000000000000000, -0.000000000000000000, -1.000000000000000000 ) ) ;
#95035 = DIRECTION ( 'NONE',  ( 1.000000000000000000, 0.000000000000000000, 0.000000000000000000 ) ) ;
#95036 = CIRCLE ( 'NONE', #107503, 0.5000000000000004441 ) ;
#95037 = FACE_OUTER_BOUND ( 'NONE', #100538, .T. ) ;
#95038 = EDGE_CURVE ( 'NONE', #70123, #208162, #153281, .T. ) ;
#95039 = ORIENTED_EDGE ( 'NONE', *, *, #189400, .F. ) ;
#95040 = ORIENTED_EDGE ( 'NONE', *, *, #38117, .T. ) ;
#95041 = EDGE_CURVE ( 'NONE', #194903, #86704, #7695, .T. ) ;
#95042 = DIRECTION ( 'NONE',  ( 0.000000000000000000, -0.2558827019434133376, 0.9667078373770113808 ) ) ;
#95043 = ORIENTED_EDGE ( 'NONE', *, *, #119453, .F. ) ;
#95045 = ORIENTED_EDGE ( 'NONE', *, *, #109894, .F. ) ;
#95044 = DIRECTION ( 'NONE',  ( -1.000000000000000000, -0.000000000000000000, -0.000000000000000000 ) ) ;
#95046 = EDGE_CURVE ( 'NONE', #250368, #198727, #195946, .T. ) ;
#95049 = EDGE_LOOP ( 'NONE', ( #244137, #199588, #51304, #196452 ) ) ;
#95048 = VERTEX_POINT ( 'NONE', #134640 ) ;
#95047 = CARTESIAN_POINT ( 'NONE',  ( 20.94999999999999929, 71.14953271029243353, -124.4888400755226598 ) ) ;
#95050 = AXIS2_PLACEMENT_3D ( 'NONE', #89103, #226016, #207804 ) ;
#95051 = DIRECTION ( 'NONE',  ( 1.000000000000000000, 0.000000000000000000, -0.000000000000000000 ) ) ;
#95052 = CARTESIAN_POINT ( 'NONE',  ( -16.97683809663752186, 12.57413723904469904, -211.9780204941619388 ) ) ;
#95053 = CARTESIAN_POINT ( 'NONE',  ( 21.05563370358598263, 10.72423035585766549, -112.6830908159630980 ) ) ;
#95054 = ADVANCED_FACE ( 'NONE', ( #75979 ), #39457, .T. ) ;
#95055 = CARTESIAN_POINT ( 'NONE',  ( 21.05000000000000071, 65.31570632562542755, -195.9964335458869300 ) ) ;
#95056 = PLANE ( 'NONE',  #226233 ) ;
#95057 = CIRCLE ( 'NONE', #219962, 0.5999999999999872102 ) ;
#95058 = CARTESIAN_POINT ( 'NONE',  ( -18.39999999999999858, 87.08727414655710675, -199.6327537731849873 ) ) ;
#95059 = ORIENTED_EDGE ( 'NONE', *, *, #57290, .T. ) ;
#95060 = VERTEX_POINT ( 'NONE', #57679 ) ;
#95061 = VERTEX_POINT ( 'NONE', #36890 ) ;
#95062 = EDGE_CURVE ( 'NONE', #93478, #180230, #145034, .T. ) ;
#95063 = DIRECTION ( 'NONE',  ( 0.000000000000000000, -0.1350103645451945777, 0.9908441862701590219 ) ) ;
#95065 = ORIENTED_EDGE ( 'NONE', *, *, #133658, .F. ) ;
#95064 = CARTESIAN_POINT ( 'NONE',  ( 23.24999999999999645, 4.775700934590584090, -45.34876810404598046 ) ) ;
#95066 = DIRECTION ( 'NONE',  ( 1.000000000000000000, 0.000000000000000000, 0.000000000000000000 ) ) ;
#95067 = VERTEX_POINT ( 'NONE', #1559 ) ;
#95068 = CARTESIAN_POINT ( 'NONE',  ( 21.46681500593265213, 6.857511159395767386, -100.5000000000000426 ) ) ;
#95069 =( BOUNDED_CURVE ( )  B_SPLINE_CURVE ( 3, ( #7630, #208419, #6328, #183705 ),
 .UNSPECIFIED., .F., .F. ) 
 B_SPLINE_CURVE_WITH_KNOTS ( ( 4, 4 ),
 ( 0.000000000000000000, 1.570796326794908992 ),
 .UNSPECIFIED. ) 
 CURVE ( )  GEOMETRIC_REPRESENTATION_ITEM ( )  RATIONAL_B_SPLINE_CURVE ( ( 1.000000000000000000, 0.8047378541243619399, 0.8047378541243619399, 1.000000000000000000 ) ) 
 REPRESENTATION_ITEM ( '' )  );
#95070 = ORIENTED_EDGE ( 'NONE', *, *, #247552, .F. ) ;
#95071 = EDGE_CURVE ( 'NONE', #91918, #96525, #107455, .T. ) ;
#95072 = CARTESIAN_POINT ( 'NONE',  ( 21.05000000000000071, 40.27305497204160645, -251.4871534980821082 ) ) ;
#95073 = ADVANCED_FACE ( 'NONE', ( #176385 ), #77247, .F. ) ;
#95074 = EDGE_LOOP ( 'NONE', ( #78979, #37020, #150036, #222321 ) ) ;
#95075 = DIRECTION ( 'NONE',  ( -1.000000000000000000, 0.000000000000000000, 0.000000000000000000 ) ) ;
#95076 = CARTESIAN_POINT ( 'NONE',  ( 20.94999999999999929, -8.663551401858002876, -143.5241011180673070 ) ) ;
#95077 = VECTOR ( 'NONE', #8878, 1000.000000000000000 ) ;
#95078 = AXIS2_PLACEMENT_3D ( 'NONE', #242577, #82195, #200892 ) ;
#95079 = AXIS2_PLACEMENT_3D ( 'NONE', #8954, #134024, #108062 ) ;
#95081 = ORIENTED_EDGE ( 'NONE', *, *, #14692, .F. ) ;
#95080 = ORIENTED_EDGE ( 'NONE', *, *, #121500, .F. ) ;
#95082 = ORIENTED_EDGE ( 'NONE', *, *, #15366, .F. ) ;
#95083 = CARTESIAN_POINT ( 'NONE',  ( -21.05000000000000071, 0.000000000000000000, -33.50000000000000000 ) ) ;
#95084 = ORIENTED_EDGE ( 'NONE', *, *, #23486, .F. ) ;
#95085 =( BOUNDED_SURFACE ( )  B_SPLINE_SURFACE ( 3, 2, ( 
 ( #16799, #192861, #177169 ),
 ( #254088, #96292, #155036 ),
 ( #213691, #75496, #196686 ),
 ( #234537, #217525, #38922 ) ),
 .UNSPECIFIED., .F., .F., .F. ) 
 B_SPLINE_SURFACE_WITH_KNOTS ( ( 4, 4 ),
 ( 3, 3 ),
 ( 4.712388980384689674, 5.765869716888459173 ),
 ( 0.000000000000000000, 1.000000000000000000 ),
 .UNSPECIFIED. ) 
 GEOMETRIC_REPRESENTATION_ITEM ( )  RATIONAL_B_SPLINE_SURFACE ( (
 ( 1.000000000000000000, 0.7071067811865229258, 1.000000000000000000),
 ( 1.000000000000000000, 0.7953136715913396992, 1.000000000000000000),
 ( 1.000000000000000000, 0.8646876308615339957, 1.000000000000000000),
 ( 1.000000000000000000, 0.8984936768950558816, 1.000000000000000000) ) ) 
 REPRESENTATION_ITEM ( '' )  SURFACE ( )  );
#95086 = ORIENTED_EDGE ( 'NONE', *, *, #165004, .F. ) ;
#95087 = DIRECTION ( 'NONE',  ( 1.000000000000000000, 0.000000000000000000, 0.000000000000000000 ) ) ;
#95089 = EDGE_LOOP ( 'NONE', ( #42778, #12995, #95203, #147593 ) ) ;
#95088 = CARTESIAN_POINT ( 'NONE',  ( -20.94999999999999929, 7.980037321000004624, -237.6410835587014390 ) ) ;
#95090 = ADVANCED_FACE ( 'NONE', ( #120280 ), #190880, .F. ) ;
#95091 = CARTESIAN_POINT ( 'NONE',  ( 18.59999999999997655, 1.115600667400684642E-11, -167.5000000000000284 ) ) ;
#95092 = TOROIDAL_SURFACE ( 'NONE', #11728, 2.100000000000002309, 0.1000000000000000056 ) ;
#95094 = CARTESIAN_POINT ( 'NONE',  ( -18.59999999999999787, 13.71992543034163958, -238.5823796952984992 ) ) ;
#95093 = PLANE ( 'NONE',  #207207 ) ;
#95095 = CARTESIAN_POINT ( 'NONE',  ( 23.24999999999999645, 72.10000000001141984, -36.02310748452435263 ) ) ;
#95096 = CARTESIAN_POINT ( 'NONE',  ( 18.39999999999999858, -9.499999999988842703, -74.03206939669971121 ) ) ;
#95097 = CARTESIAN_POINT ( 'NONE',  ( 21.59780538579342490, 30.36975234701187176, -252.2601773037668806 ) ) ;
#95098 = ORIENTED_EDGE ( 'NONE', *, *, #143649, .T. ) ;
#95099 = EDGE_LOOP ( 'NONE', ( #80251, #9383, #135327, #142365 ) ) ;
#95100 = DIRECTION ( 'NONE',  ( 1.020425574104004196E-15, 1.210927747993693964E-31, 1.000000000000000000 ) ) ;
#95101 = EDGE_CURVE ( 'NONE', #30385, #176240, #117668, .T. ) ;
#95102 = CARTESIAN_POINT ( 'NONE',  ( -21.05000000000000071, 75.96636726467852441, -142.7819246792058152 ) ) ;
#95103 = DIRECTION ( 'NONE',  ( 0.000000000000000000, 0.9915357197604982575, -0.1298341882519033486 ) ) ;
#95104 = ORIENTED_EDGE ( 'NONE', *, *, #212973, .T. ) ;
#95105 = CIRCLE ( 'NONE', #115767, 0.1000000000000028644 ) ;
#95107 = CARTESIAN_POINT ( 'NONE',  ( -21.05000000000000071, 1.115600667400684642E-11, -67.00000000000004263 ) ) ;
#95106 = AXIS2_PLACEMENT_3D ( 'NONE', #5325, #79731, #142292 ) ;
#95108 = CARTESIAN_POINT ( 'NONE',  ( 23.14999999999999858, 80.00000000001170974, -69.52310748452428868 ) ) ;
#95109 = DIRECTION ( 'NONE',  ( 0.000000000000000000, 0.000000000000000000, -1.000000000000000000 ) ) ;
#95110 = CIRCLE ( 'NONE', #149295, 0.09999999999999693856 ) ;
#95111 = ORIENTED_EDGE ( 'NONE', *, *, #150744, .T. ) ;
#95112 = ORIENTED_EDGE ( 'NONE', *, *, #85953, .T. ) ;
#95113 = DIRECTION ( 'NONE',  ( 2.952720810173289112E-16, -1.000000000000000000, 0.000000000000000000 ) ) ;
#95114 = ADVANCED_FACE ( 'NONE', ( #254585 ), #160682, .T. ) ;
#95115 = CARTESIAN_POINT ( 'NONE',  ( -23.15000000000000213, 11.75000000001115552, -112.6500000000000341 ) ) ;
#95116 = ORIENTED_EDGE ( 'NONE', *, *, #153700, .F. ) ;
#95117 = CARTESIAN_POINT ( 'NONE',  ( -18.42554971533677133, -9.497159669426594064, -174.5398269135486089 ) ) ;
#95118 = ORIENTED_EDGE ( 'NONE', *, *, #69830, .F. ) ;
#95119 = CARTESIAN_POINT ( 'NONE',  ( 18.44206774312976904, -9.491027357528897923, -140.6262275046982779 ) ) ;
#95120 = CARTESIAN_POINT ( 'NONE',  ( -16.80117486205003630, 9.949657268323468529, -154.8488548729255285 ) ) ;
#95122 = DIRECTION ( 'NONE',  ( -0.000000000000000000, -0.000000000000000000, -1.000000000000000000 ) ) ;
#95121 = DIRECTION ( 'NONE',  ( 0.000000000000000000, -0.1350103645451807555, -0.9908441862701609093 ) ) ;
#95123 = CIRCLE ( 'NONE', #190999, 0.5000000000000001110 ) ;
#95124 = CARTESIAN_POINT ( 'NONE',  ( 18.55121869061587958, 65.67252876774583115, -164.4457041994994881 ) ) ;
#95125 = CARTESIAN_POINT ( 'NONE',  ( 21.07189867249812210, 65.27501972991871071, -90.81065604224765764 ) ) ;
#95126 = AXIS2_PLACEMENT_3D ( 'NONE', #26311, #44590, #105808 ) ;
#95127 = DIRECTION ( 'NONE',  ( -1.000000000000000000, 0.000000000000000000, -0.000000000000000000 ) ) ;
#95128 = EDGE_CURVE ( 'NONE', #126771, #87224, #252806, .T. ) ;
#95131 = EDGE_LOOP ( 'NONE', ( #177907, #186179, #247453, #145048 ) ) ;
#95130 = EDGE_LOOP ( 'NONE', ( #135751, #153072, #58171, #191968 ) ) ;
#95129 = TOROIDAL_SURFACE ( 'NONE', #240876, 0.6000000000000009770, 0.1000000000000000056 ) ;
#95132 = ORIENTED_EDGE ( 'NONE', *, *, #180997, .T. ) ;
#95133 = AXIS2_PLACEMENT_3D ( 'NONE', #97969, #257020, #177576 ) ;
#95134 = AXIS2_PLACEMENT_3D ( 'NONE', #52986, #193796, #210787 ) ;
#95135 = FACE_OUTER_BOUND ( 'NONE', #101786, .T. ) ;
#95136 = DIRECTION ( 'NONE',  ( 0.000000000000000000, 0.000000000000000000, -1.000000000000000000 ) ) ;
#95137 = CARTESIAN_POINT ( 'NONE',  ( -18.59999999999999787, -9.480686695267820596, -140.9411151687578752 ) ) ;
#95138 = CARTESIAN_POINT ( 'NONE',  ( -18.49499033040907037, -9.438148771733516185, -107.6981532259234484 ) ) ;
#95139 = CIRCLE ( 'NONE', #86727, 12.87499999999999822 ) ;
#95141 = CARTESIAN_POINT ( 'NONE',  ( -12.25000000000000711, 66.65000000001188596, -86.50453852712175262 ) ) ;
#95140 = DIRECTION ( 'NONE',  ( 0.000000000000000000, 0.8814952561688476074, -0.4721928772777262417 ) ) ;
#95142 = CARTESIAN_POINT ( 'NONE',  ( -22.48660254037843487, 11.65000000001115588, -100.4500000000000597 ) ) ;
#95143 = VERTEX_POINT ( 'NONE', #194676 ) ;
#95144 = DIRECTION ( 'NONE',  ( 0.000000000000000000, 0.000000000000000000, -1.000000000000000000 ) ) ;
#95145 = ORIENTED_EDGE ( 'NONE', *, *, #5219, .F. ) ;
#95146 = EDGE_LOOP ( 'NONE', ( #257548, #254061, #224955, #86126 ) ) ;
#95147 = FACE_OUTER_BOUND ( 'NONE', #76135, .T. ) ;
#95148 = CYLINDRICAL_SURFACE ( 'NONE', #205683, 0.1000000000000028644 ) ;
#95149 = DIRECTION ( 'NONE',  ( 1.000000000000000000, 2.952720810173289112E-16, -0.000000000000000000 ) ) ;
#95150 = B_SPLINE_CURVE_WITH_KNOTS ( 'NONE', 3,
 ( #32860, #232327, #112367, #114922, #13265, #137053, #156653, #256946, #237438, #133204 ),
 .UNSPECIFIED., .F., .F.,
 ( 4, 3, 3, 4 ),
 ( 0.000000000000000000, 0.0002000000000008536833, 0.001000000000082972495, 0.001967863649483305062 ),
 .UNSPECIFIED. ) ;
#95151 = AXIS2_PLACEMENT_3D ( 'NONE', #234526, #231990, #196678 ) ;
#95152 = VECTOR ( 'NONE', #159363, 1000.000000000000000 ) ;
#95153 = CARTESIAN_POINT ( 'NONE',  ( 28.12018973533754362, 11.62642356364896123, -347.0000000000001137 ) ) ;
#95154 = CARTESIAN_POINT ( 'NONE',  ( 22.49999999999999645, 0.1000000000111554016, -155.8504291924551808 ) ) ;
#95155 = EDGE_LOOP ( 'NONE', ( #124192, #198363, #70096, #44464 ) ) ;
#95156 = VERTEX_POINT ( 'NONE', #16032 ) ;
#95157 = DIRECTION ( 'NONE',  ( 0.000000000000000000, 6.938893903907222067E-15, -1.000000000000000000 ) ) ;
#95158 = CARTESIAN_POINT ( 'NONE',  ( 18.59999999999997655, 11.75000000001115552, -200.9999999999999432 ) ) ;
#95159 = CARTESIAN_POINT ( 'NONE',  ( 21.05000000000000071, 86.27712145182582049, -209.5223386573213702 ) ) ;
#95160 = CARTESIAN_POINT ( 'NONE',  ( -23.15000000000000213, 85.00000000001179501, -78.91707660717668205 ) ) ;
#95161 = CYLINDRICAL_SURFACE ( 'NONE', #204457, 0.5000000000000004441 ) ;
#95162 = PLANE ( 'NONE',  #167304 ) ;
#95163 = CARTESIAN_POINT ( 'NONE',  ( -23.25000000000000000, 6.982009704856444898, -37.19615211825629331 ) ) ;
#95164 = AXIS2_PLACEMENT_3D ( 'NONE', #241726, #123074, #71788 ) ;
#95166 = CARTESIAN_POINT ( 'NONE',  ( 18.49999999999999289, 54.57427006634497957, -228.7596887170734306 ) ) ;
#95165 = CARTESIAN_POINT ( 'NONE',  ( 18.39999999999999147, 67.17743825834622839, -194.2731074845244166 ) ) ;
#95168 = EDGE_CURVE ( 'NONE', #121571, #69398, #56394, .T. ) ;
#95167 = DIRECTION ( 'NONE',  ( 2.840903330521633255E-16, 0.8700118002898357128, -0.4930308989875171188 ) ) ;
#95169 = AXIS2_PLACEMENT_3D ( 'NONE', #210909, #117893, #191380 ) ;
#95170 = DIRECTION ( 'NONE',  ( 0.000000000000000000, 0.000000000000000000, -1.000000000000000000 ) ) ;
#95171 = DIRECTION ( 'NONE',  ( 0.000000000000000000, 1.000000000000000000, 6.982962677686266711E-15 ) ) ;
#95173 = CARTESIAN_POINT ( 'NONE',  ( 18.50000000000000000, 85.40000000001263913, -196.2258477248609836 ) ) ;
#95172 = AXIS2_PLACEMENT_3D ( 'NONE', #82053, #142053, #161653 ) ;
#95175 = ORIENTED_EDGE ( 'NONE', *, *, #87441, .F. ) ;
#95174 = DIRECTION ( 'NONE',  ( 0.000000000000000000, 0.000000000000000000, -1.000000000000000000 ) ) ;
#95176 = EDGE_CURVE ( 'NONE', #60871, #57597, #158130, .T. ) ;
#95177 = DIRECTION ( 'NONE',  ( 0.000000000000000000, 1.000000000000000000, 6.982962677686266711E-15 ) ) ;
#95178 = ORIENTED_EDGE ( 'NONE', *, *, #244581, .F. ) ;
#95179 = CIRCLE ( 'NONE', #36773, 0.1000000000000028644 ) ;
#95180 = EDGE_CURVE ( 'NONE', #188655, #140955, #170050, .T. ) ;
#95181 = CARTESIAN_POINT ( 'NONE',  ( -20.85000000000000142, 76.00000000001213607, -136.5231074845243313 ) ) ;
#95182 = AXIS2_PLACEMENT_3D ( 'NONE', #232786, #193646, #196203 ) ;
#95183 = TOROIDAL_SURFACE ( 'NONE', #153490, 11.65000000000000036, 0.1000000000000000056 ) ;
#95184 = ORIENTED_EDGE ( 'NONE', *, *, #82500, .T. ) ;
#95185 = CARTESIAN_POINT ( 'NONE',  ( -20.94999999999999929, 70.10000000001193143, -92.80400771986793984 ) ) ;
#95186 = CIRCLE ( 'NONE', #236640, 0.09999999999999600875 ) ;
#95187 = CARTESIAN_POINT ( 'NONE',  ( 12.60873083341396850, 9.389571634557563939, -84.81764071236919733 ) ) ;
#95188 = CARTESIAN_POINT ( 'NONE',  ( 20.85000000000000142, 77.83585931145526615, -57.91866831572577468 ) ) ;
#95189 = ADVANCED_FACE ( 'NONE', ( #40740 ), #253189, .T. ) ;
#95190 = FACE_OUTER_BOUND ( 'NONE', #137395, .T. ) ;
#95191 = CARTESIAN_POINT ( 'NONE',  ( 23.15000000000000213, 81.86853375790846599, -214.9828603846715964 ) ) ;
#95192 = PLANE ( 'NONE',  #73856 ) ;
#95193 = EDGE_CURVE ( 'NONE', #129423, #88113, #140774, .T. ) ;
#95195 = ORIENTED_EDGE ( 'NONE', *, *, #75829, .F. ) ;
#95194 = EDGE_CURVE ( 'NONE', #86723, #239491, #44562, .T. ) ;
#95196 = CARTESIAN_POINT ( 'NONE',  ( -21.59142135623730852, 7.850000000011158718, -179.7499999999999716 ) ) ;
#95198 = ORIENTED_EDGE ( 'NONE', *, *, #188829, .T. ) ;
#95197 = PLANE ( 'NONE',  #105259 ) ;
#95199 = LINE ( 'NONE', #13109, #71454 ) ;
#95200 = CARTESIAN_POINT ( 'NONE',  ( 20.95512820512820440, 22.85550638026973047, -230.1049725544161220 ) ) ;
#95201 = EDGE_CURVE ( 'NONE', #246321, #221635, #62832, .T. ) ;
#95202 = DIRECTION ( 'NONE',  ( -0.7071067811865475727, 0.7071067811865475727, 4.937700262164531476E-15 ) ) ;
#95203 = ORIENTED_EDGE ( 'NONE', *, *, #213092, .F. ) ;
#95204 = CARTESIAN_POINT ( 'NONE',  ( -21.00857864376268935, 11.59999999999999787, -6.928203230275555846 ) ) ;
#95205 = AXIS2_PLACEMENT_3D ( 'NONE', #94936, #72853, #254011 ) ;
#95206 = PRODUCT_CONTEXT ( 'NONE', #243908, 'mechanical' ) ;
#95207 = CARTESIAN_POINT ( 'NONE',  ( 23.15000000000000213, 49.57218508014540959, -254.1759139559835035 ) ) ;
#95209 = EDGE_CURVE ( 'NONE', #244686, #142904, #28380, .T. ) ;
#95208 = DIRECTION ( 'NONE',  ( 0.000000000000000000, 0.000000000000000000, -1.000000000000000000 ) ) ;
#95210 = VERTEX_POINT ( 'NONE', #101929 ) ;
#95211 = DIRECTION ( 'NONE',  ( -1.000000000000000000, -0.000000000000000000, 0.000000000000000000 ) ) ;
#95212 = CARTESIAN_POINT ( 'NONE',  ( -16.77732147262506146, 9.945966932629787038, -121.3364912432759013 ) ) ;
#95213 = ORIENTED_EDGE ( 'NONE', *, *, #73614, .F. ) ;
#95214 = ORIENTED_EDGE ( 'NONE', *, *, #169593, .F. ) ;
#95215 = CARTESIAN_POINT ( 'NONE',  ( -23.39999999999994529, 64.25000000001119815, -51.02310748452479316 ) ) ;
#95216 = ADVANCED_FACE ( 'NONE', ( #5393 ), #128317, .T. ) ;
#95217 = DIRECTION ( 'NONE',  ( -1.000000000000000000, 0.000000000000000000, 0.000000000000000000 ) ) ;
#95218 = DIRECTION ( 'NONE',  ( -1.000000000000000000, -0.000000000000000000, -0.000000000000000000 ) ) ;
#95219 = CARTESIAN_POINT ( 'NONE',  ( -21.51976009735018991, 69.08954155835274946, -103.0231074845243739 ) ) ;
#95221 = DIRECTION ( 'NONE',  ( 1.000000000000000000, 0.000000000000000000, 0.000000000000000000 ) ) ;
#95220 = CARTESIAN_POINT ( 'NONE',  ( -15.75000000000000355, 9.850000000011133849, -184.2499999999999716 ) ) ;
#95222 = TOROIDAL_SURFACE ( 'NONE', #236862, 11.70000000000000107, 0.1000000000000000056 ) ;
#95224 = CARTESIAN_POINT ( 'NONE',  ( 23.25000000000000000, 11.75000000000000711, -21.35000000000000142 ) ) ;
#95223 = AXIS2_PLACEMENT_3D ( 'NONE', #54024, #18749, #115281 ) ;
#95225 = DIRECTION ( 'NONE',  ( 0.000000000000000000, 0.8660254037844385966, -0.5000000000000003331 ) ) ;
#95226 = FACE_OUTER_BOUND ( 'NONE', #194900, .T. ) ;
#95227 = CARTESIAN_POINT ( 'NONE',  ( -0.8999999999999437339, 64.35000000001120668, -10.02310748452479139 ) ) ;
#95228 = ORIENTED_EDGE ( 'NONE', *, *, #33116, .T. ) ;
#95229 = ORIENTED_EDGE ( 'NONE', *, *, #236920, .T. ) ;
#95230 = FACE_OUTER_BOUND ( 'NONE', #102359, .T. ) ;
#95231 = DIRECTION ( 'NONE',  ( -1.000000000000000000, -0.000000000000000000, -0.000000000000000000 ) ) ;
#95233 = CARTESIAN_POINT ( 'NONE',  ( 21.05000000000000071, 71.18691588786271041, -148.4646252410481964 ) ) ;
#95232 = CARTESIAN_POINT ( 'NONE',  ( 21.09813707148777340, 69.61493789427515821, -69.55445898405388050 ) ) ;
#95234 = EDGE_CURVE ( 'NONE', #206482, #94125, #120151, .T. ) ;
#95235 = CIRCLE ( 'NONE', #161902, 0.1000000000000028644 ) ;
#95236 = DIRECTION ( 'NONE',  ( -1.836970198721029934E-16, 1.000000000000000000, 0.000000000000000000 ) ) ;
#95237 = CARTESIAN_POINT ( 'NONE',  ( 20.94999999999999929, 77.16412189325330928, -128.6082593989527254 ) ) ;
#95238 = CARTESIAN_POINT ( 'NONE',  ( 15.31784899511109721, 12.99204546914880254, -216.4972940033653401 ) ) ;
#95239 = ORIENTED_EDGE ( 'NONE', *, *, #57176, .T. ) ;
#95240 = ORIENTED_EDGE ( 'NONE', *, *, #173448, .F. ) ;
#95241 = AXIS2_PLACEMENT_3D ( 'NONE', #165959, #248027, #129372 ) ;
#95242 = CIRCLE ( 'NONE', #157833, 0.1000000000000028644 ) ;
#95244 = AXIS2_PLACEMENT_3D ( 'NONE', #252733, #132818, #89810 ) ;
#95243 = DIRECTION ( 'NONE',  ( 0.000000000000000000, 0.000000000000000000, 1.000000000000000000 ) ) ;
#95245 = ORIENTED_EDGE ( 'NONE', *, *, #174964, .F. ) ;
#95246 = EDGE_CURVE ( 'NONE', #145844, #186227, #174134, .T. ) ;
#95247 = CARTESIAN_POINT ( 'NONE',  ( 20.85000000000000142, 1.115600667400684642E-11, -134.0000000000000284 ) ) ;
#95248 = EDGE_CURVE ( 'NONE', #131374, #104540, #181516, .T. ) ;
#95250 = CARTESIAN_POINT ( 'NONE',  ( -18.39999999999999858, -7.817436562502981801, -209.8389866834999111 ) ) ;
#95249 = AXIS2_PLACEMENT_3D ( 'NONE', #115311, #198706, #117877 ) ;
#95251 = DIRECTION ( 'NONE',  ( 0.000000000000000000, 0.000000000000000000, 1.000000000000000000 ) ) ;
#95252 = EDGE_LOOP ( 'NONE', ( #225272, #218665, #77820, #125919 ) ) ;
#95253 = CARTESIAN_POINT ( 'NONE',  ( -18.79999999999999716, -11.65000000000000036, 0.000000000000000000 ) ) ;
#95254 = ADVANCED_FACE ( 'NONE', ( #185349 ), #125383, .T. ) ;
#95255 = B_SPLINE_CURVE_WITH_KNOTS ( 'NONE', 3,
 ( #184370, #143961, #83944, #146518 ),
 .UNSPECIFIED., .F., .F.,
 ( 4, 4 ),
 ( 3.469446951953614189E-18, 0.0001058379652594853209 ),
 .UNSPECIFIED. ) ;
#95256 = CARTESIAN_POINT ( 'NONE',  ( -23.15000000000000213, 4.768403829798271154, -213.4961173936592331 ) ) ;
#95257 = DIRECTION ( 'NONE',  ( 1.000000000000000000, 0.000000000000000000, 0.000000000000000000 ) ) ;
#95258 = ADVANCED_FACE ( 'NONE', ( #143645 ), #122825, .T. ) ;
#95259 = CARTESIAN_POINT ( 'NONE',  ( -20.90000000000000213, 8.000000000000000000, -1.212568896937008089 ) ) ;
#95260 = ADVANCED_FACE ( 'NONE', ( #124106 ), #82362, .T. ) ;
#95261 = CYLINDRICAL_SURFACE ( 'NONE', #9770, 0.09999999999999724387 ) ;
#95263 = CARTESIAN_POINT ( 'NONE',  ( 23.14999999999999503, 45.29262862071417572, -238.6157088101306556 ) ) ;
#95262 = FACE_OUTER_BOUND ( 'NONE', #139197, .T. ) ;
#95264 = CARTESIAN_POINT ( 'NONE',  ( -16.93710578446435377, 66.05000000001224691, -149.4419114683242640 ) ) ;
#95265 = AXIS2_PLACEMENT_3D ( 'NONE', #149385, #50237, #46388 ) ;
#95266 = ORIENTED_EDGE ( 'NONE', *, *, #74020, .F. ) ;
#95268 = CARTESIAN_POINT ( 'NONE',  ( -17.11825945287482753, 10.05000000001113847, -180.1499999999999773 ) ) ;
#95267 = CARTESIAN_POINT ( 'NONE',  ( 20.94999999999999929, 1.835341550235569663, -78.55515129256303908 ) ) ;
#95269 = ORIENTED_EDGE ( 'NONE', *, *, #160356, .T. ) ;
#95271 = EDGE_LOOP ( 'NONE', ( #125046, #216839, #170551, #61665 ) ) ;
#95270 = DIRECTION ( 'NONE',  ( 1.000000000000000000, -2.952720810173289112E-16, -2.061873921506763405E-30 ) ) ;
#95272 = CIRCLE ( 'NONE', #241020, 0.1000000000000028644 ) ;
#95273 = ORIENTED_EDGE ( 'NONE', *, *, #34415, .T. ) ;
#95274 = DIRECTION ( 'NONE',  ( -1.000000000000000000, 0.000000000000000000, 0.000000000000000000 ) ) ;
#95275 = CARTESIAN_POINT ( 'NONE',  ( -18.59999999999999787, 74.16465844978765176, -124.9679561919613207 ) ) ;
#95276 = CARTESIAN_POINT ( 'NONE',  ( -21.05000000000000426, 30.91403104479204345, -252.1478540170565736 ) ) ;
#95277 = ADVANCED_FACE ( 'NONE', ( #87510 ), #141095, .T. ) ;
#95278 = FACE_OUTER_BOUND ( 'NONE', #134541, .T. ) ;
#95279 = ORIENTED_EDGE ( 'NONE', *, *, #77540, .T. ) ;
#95280 = CARTESIAN_POINT ( 'NONE',  ( 21.13461538461539035, 8.885417037985600786, -112.7500000000000142 ) ) ;
#95281 = CIRCLE ( 'NONE', #174443, 12.87499999999999822 ) ;
#95282 = CARTESIAN_POINT ( 'NONE',  ( 22.50014994444005367, 64.25028026812066173, -203.6061876412436504 ) ) ;
#95283 = ORIENTED_EDGE ( 'NONE', *, *, #151468, .F. ) ;
#95284 = DIRECTION ( 'NONE',  ( 0.000000000000000000, 0.4088369013363279403, -0.9126074666063771490 ) ) ;
#95285 = CARTESIAN_POINT ( 'NONE',  ( 21.08078803292165659, 6.333012964437116921, 0.07918598715778434050 ) ) ;
#95286 = ORIENTED_EDGE ( 'NONE', *, *, #110077, .T. ) ;
#95287 = ORIENTED_EDGE ( 'NONE', *, *, #173587, .F. ) ;
#95288 = VECTOR ( 'NONE', #170270, 1000.000000000000000 ) ;
#95289 = FACE_OUTER_BOUND ( 'NONE', #248900, .T. ) ;
#95290 = TOROIDAL_SURFACE ( 'NONE', #157697, 0.2000000000000000111, 0.1000000000000000056 ) ;
#95291 = ORIENTED_EDGE ( 'NONE', *, *, #47966, .F. ) ;
#95292 = CARTESIAN_POINT ( 'NONE',  ( -13.39999999999994351, 66.35000000001119247, -23.62310748452479103 ) ) ;
#95294 = VERTEX_POINT ( 'NONE', #121558 ) ;
#95293 = CIRCLE ( 'NONE', #241054, 0.1000000000000072220 ) ;
#95295 = CARTESIAN_POINT ( 'NONE',  ( 20.94999999999999929, 87.65000000001172964, -72.42310748452422331 ) ) ;
#95296 = ADVANCED_FACE ( 'NONE', ( #4134 ), #94973, .F. ) ;
#95297 = DIRECTION ( 'NONE',  ( -1.000000000000000000, -0.000000000000000000, -0.000000000000000000 ) ) ;
#95298 = DIRECTION ( 'NONE',  ( 1.000000000000000000, 0.000000000000000000, 0.000000000000000000 ) ) ;
#95299 = EDGE_CURVE ( 'NONE', #115264, #81578, #78401, .T. ) ;
#95300 = DIRECTION ( 'NONE',  ( 1.000000000000000000, 0.000000000000000000, 0.000000000000000000 ) ) ;
#95301 = CIRCLE ( 'NONE', #141651, 2.599999999999998312 ) ;
#95302 = CIRCLE ( 'NONE', #145354, 0.09999999999999520384 ) ;
#95303 = EDGE_CURVE ( 'NONE', #6721, #147377, #83637, .T. ) ;
#95304 = DIRECTION ( 'NONE',  ( -1.000000000000000000, -0.000000000000000000, -0.000000000000000000 ) ) ;
#95305 = AXIS2_PLACEMENT_3D ( 'NONE', #16710, #14156, #214891 ) ;
#95306 = CARTESIAN_POINT ( 'NONE',  ( 18.40916198585730967, -9.499999999988844479, -73.60018963182341167 ) ) ;
#95307 = DIRECTION ( 'NONE',  ( 1.000000000000000000, 0.000000000000000000, 0.000000000000000000 ) ) ;
#95308 = VERTEX_POINT ( 'NONE', #90081 ) ;
#95310 = CYLINDRICAL_SURFACE ( 'NONE', #185476, 0.09999999999999986677 ) ;
#95309 = CARTESIAN_POINT ( 'NONE',  ( 21.14999999999999858, 22.98593783141596703, -230.0732594427593938 ) ) ;
#95311 = ORIENTED_EDGE ( 'NONE', *, *, #93496, .T. ) ;
#95314 = VERTEX_POINT ( 'NONE', #14442 ) ;
#95313 = CARTESIAN_POINT ( 'NONE',  ( -20.54999999999999716, 2.000000000011154189, -120.7753780772379315 ) ) ;
#95312 = DIRECTION ( 'NONE',  ( 0.000000000000000000, 0.2128009952263603677, -0.9770955615653313941 ) ) ;
#95315 = AXIS2_PLACEMENT_3D ( 'NONE', #104402, #183967, #5295 ) ;
#95316 = VERTEX_POINT ( 'NONE', #150097 ) ;
#95317 = CARTESIAN_POINT ( 'NONE',  ( -18.59999999999999787, 11.65000000001115232, -45.65000000000000568 ) ) ;
#95318 = AXIS2_PLACEMENT_3D ( 'NONE', #218905, #40326, #161534 ) ;
#95319 = CARTESIAN_POINT ( 'NONE',  ( 21.07954640115360334, 0.06600770715084654239, -60.67071230397558423 ) ) ;
#95320 = AXIS2_PLACEMENT_3D ( 'NONE', #164377, #147376, #144783 ) ;
#95321 = CARTESIAN_POINT ( 'NONE',  ( -20.64999999999999858, 74.00000000001254818, -183.2477294072864709 ) ) ;
#95322 = CARTESIAN_POINT ( 'NONE',  ( -16.85312841634287651, 9.913606177331356406, -113.3971731332925685 ) ) ;
#95323 = VERTEX_POINT ( 'NONE', #151378 ) ;
#95325 = ORIENTED_EDGE ( 'NONE', *, *, #3023, .F. ) ;
#95324 = DIRECTION ( 'NONE',  ( 0.000000000000000000, 0.000000000000000000, -1.000000000000000000 ) ) ;
#95326 = CIRCLE ( 'NONE', #249458, 0.09999999999998898659 ) ;
#95328 = CARTESIAN_POINT ( 'NONE',  ( -22.94999999999999929, 11.49641995933507843, 1.885425182446134107 ) ) ;
#95327 = SPHERICAL_SURFACE ( 'NONE', #230810, 0.1000000000000000056 ) ;
#95330 = ORIENTED_EDGE ( 'NONE', *, *, #109112, .F. ) ;
#95329 = DIRECTION ( 'NONE',  ( -1.000000000000000000, -0.000000000000000000, 0.000000000000000000 ) ) ;
#95331 = PRODUCT_DEFINITION_SHAPE ( 'NONE', 'NONE',  #258107 ) ;
#95332 = ORIENTED_EDGE ( 'NONE', *, *, #132319, .T. ) ;
#95333 = EDGE_CURVE ( 'NONE', #691, #173524, #152674, .T. ) ;
#95334 = VECTOR ( 'NONE', #147963, 1000.000000000000000 ) ;
#95335 = AXIS2_PLACEMENT_3D ( 'NONE', #122492, #181188, #185017 ) ;
#95336 = CARTESIAN_POINT ( 'NONE',  ( 20.95420533658165141, 11.91469018375357436, -206.1500060891886505 ) ) ;
#95338 = AXIS2_PLACEMENT_3D ( 'NONE', #247629, #10322, #209795 ) ;
#95337 = CARTESIAN_POINT ( 'NONE',  ( 20.95263205890650582, 67.10425989211782394, -94.53359907758274971 ) ) ;
#95339 = VERTEX_POINT ( 'NONE', #73139 ) ;
#95340 = VERTEX_POINT ( 'NONE', #129230 ) ;
#95341 = EDGE_CURVE ( 'NONE', #44088, #174960, #82470, .T. ) ;
#95342 = FACE_OUTER_BOUND ( 'NONE', #247896, .T. ) ;
#95343 = DIRECTION ( 'NONE',  ( -1.000000000000000000, 0.000000000000000000, 0.000000000000000000 ) ) ;
#95344 = VERTEX_POINT ( 'NONE', #88788 ) ;
#95345 = DIRECTION ( 'NONE',  ( 1.000000000000000000, 0.000000000000000000, 0.000000000000000000 ) ) ;
#95346 = CIRCLE ( 'NONE', #12160, 0.09999999999999939493 ) ;
#95347 = ADVANCED_FACE ( 'NONE', ( #32737 ), #191798, .T. ) ;
#95348 = AXIS2_PLACEMENT_3D ( 'NONE', #151162, #251522, #95015 ) ;
#95349 = EDGE_CURVE ( 'NONE', #37909, #69101, #38072, .T. ) ;
#95350 = VECTOR ( 'NONE', #152363, 1000.000000000000000 ) ;
#95351 = CIRCLE ( 'NONE', #170416, 0.6000000000000015321 ) ;
#95352 = EDGE_CURVE ( 'NONE', #40566, #132925, #127947, .T. ) ;
#95353 = ORIENTED_EDGE ( 'NONE', *, *, #215703, .F. ) ;
#95354 = EDGE_LOOP ( 'NONE', ( #214465, #256853, #50569 ) ) ;
#95357 = ADVANCED_FACE ( 'NONE', ( #232199 ), #131789, .F. ) ;
#95356 = ADVANCED_FACE ( 'NONE', ( #227034 ), #245004, .T. ) ;
#95355 = CARTESIAN_POINT ( 'NONE',  ( 18.54116936837188589, -9.463564198361288149, -107.5485424908882948 ) ) ;
#95358 = ORIENTED_EDGE ( 'NONE', *, *, #59944, .T. ) ;
#95359 = ORIENTED_EDGE ( 'NONE', *, *, #140541, .T. ) ;
#95361 = EDGE_LOOP ( 'NONE', ( #147760, #57430, #229502 ) ) ;
#95360 = CARTESIAN_POINT ( 'NONE',  ( 20.94999999999999929, 70.15000000001192859, -92.89061026024637613 ) ) ;
#95362 = ORIENTED_EDGE ( 'NONE', *, *, #2935, .F. ) ;
#95363 = FACE_OUTER_BOUND ( 'NONE', #254980, .T. ) ;
#95364 = CIRCLE ( 'NONE', #141165, 0.1000000000000124678 ) ;
#95365 = AXIS2_PLACEMENT_3D ( 'NONE', #91353, #151338, #127905 ) ;
#95366 = ORIENTED_EDGE ( 'NONE', *, *, #15675, .T. ) ;
#95369 = ORIENTED_EDGE ( 'NONE', *, *, #132898, .F. ) ;
#95368 = ORIENTED_EDGE ( 'NONE', *, *, #124275, .T. ) ;
#95367 = CARTESIAN_POINT ( 'NONE',  ( 18.49999999999999645, 1.148907358139439339E-11, -201.0000000000015064 ) ) ;
#95370 = ORIENTED_EDGE ( 'NONE', *, *, #199673, .F. ) ;
#95371 = DIRECTION ( 'NONE',  ( 0.000000000000000000, 1.000000000000000000, 0.000000000000000000 ) ) ;
#95372 = EDGE_CURVE ( 'NONE', #196598, #59275, #178397, .T. ) ;
#95373 = EDGE_CURVE ( 'NONE', #182399, #191682, #70061, .T. ) ;
#95374 = FACE_OUTER_BOUND ( 'NONE', #118519, .T. ) ;
#95375 = ORIENTED_EDGE ( 'NONE', *, *, #190809, .T. ) ;
#95376 = EDGE_CURVE ( 'NONE', #27558, #150130, #31447, .T. ) ;
#95377 = CARTESIAN_POINT ( 'NONE',  ( 23.15000000000000213, -11.74999999998883560, -45.65000000000000568 ) ) ;
#95379 = ORIENTED_EDGE ( 'NONE', *, *, #216170, .F. ) ;
#95378 = CARTESIAN_POINT ( 'NONE',  ( 20.94999999999999929, 87.65000000001190017, -103.0231074845242176 ) ) ;
#95380 = DIRECTION ( 'NONE',  ( 0.000000000000000000, -6.982962677686266711E-15, 1.000000000000000000 ) ) ;
#95381 = ORIENTED_EDGE ( 'NONE', *, *, #212572, .T. ) ;
#95382 = ORIENTED_EDGE ( 'NONE', *, *, #84, .F. ) ;
#95384 = EDGE_CURVE ( 'NONE', #235467, #56908, #245203, .T. ) ;
#95383 = CARTESIAN_POINT ( 'NONE',  ( 22.00411653889210584, 0.09903810579733299257, -160.2465571323595555 ) ) ;
#95385 = CARTESIAN_POINT ( 'NONE',  ( 20.94999999999999574, -1.835341550224411922, -11.55515129256297868 ) ) ;
#95386 = ORIENTED_EDGE ( 'NONE', *, *, #144169, .F. ) ;
#95387 = EDGE_CURVE ( 'NONE', #241424, #35186, #70570, .T. ) ;
#95388 = ORIENTED_EDGE ( 'NONE', *, *, #139706, .T. ) ;
#95389 = CARTESIAN_POINT ( 'NONE',  ( -16.93772744219066340, 9.993541108763512426, -180.0980619719696847 ) ) ;
#95390 = CARTESIAN_POINT ( 'NONE',  ( 18.59999999999999076, 6.450000000011156587, -77.01702717044007329 ) ) ;
#95392 = ORIENTED_EDGE ( 'NONE', *, *, #142129, .T. ) ;
#95391 = ORIENTED_EDGE ( 'NONE', *, *, #257687, .F. ) ;
#95393 = VERTEX_POINT ( 'NONE', #159085 ) ;
#95394 = CARTESIAN_POINT ( 'NONE',  ( 21.05000000000000071, 36.65892442174935439, -249.5511627012433848 ) ) ;
#95395 = ORIENTED_EDGE ( 'NONE', *, *, #63875, .T. ) ;
#95396 = ORIENTED_EDGE ( 'NONE', *, *, #155086, .F. ) ;
#95397 = PLANE ( 'NONE',  #5114 ) ;
#95398 = VERTEX_POINT ( 'NONE', #213895 ) ;
#95399 = EDGE_CURVE ( 'NONE', #106067, #169023, #249300, .T. ) ;
#95400 = CARTESIAN_POINT ( 'NONE',  ( 20.94999999999999929, 6.724511449164476851, -231.8762197454659884 ) ) ;
#95401 = DIRECTION ( 'NONE',  ( 0.000000000000000000, 0.000000000000000000, 1.000000000000000000 ) ) ;
#95402 = ORIENTED_EDGE ( 'NONE', *, *, #84486, .F. ) ;
#95403 = ORIENTED_EDGE ( 'NONE', *, *, #236335, .T. ) ;
#95404 = EDGE_CURVE ( 'NONE', #235019, #92906, #217725, .T. ) ;
#95405 = VECTOR ( 'NONE', #171939, 1000.000000000000000 ) ;
#95406 = CYLINDRICAL_SURFACE ( 'NONE', #107774, 0.09999999999999939493 ) ;
#95407 = AXIS2_PLACEMENT_3D ( 'NONE', #168394, #72802, #147494 ) ;
#95408 = CIRCLE ( 'NONE', #162063, 4.049999999999998046 ) ;
#95409 = VERTEX_POINT ( 'NONE', #16998 ) ;
#95410 = AXIS2_PLACEMENT_3D ( 'NONE', #95492, #56348, #78484 ) ;
#95411 = CARTESIAN_POINT ( 'NONE',  ( -18.59999999999999787, 76.00000000001213607, -136.5231074845242745 ) ) ;
#95412 = EDGE_LOOP ( 'NONE', ( #78076, #84617, #22082, #109064, #242212, #20108, #50506, #54662, #193037, #26433, #166500 ) ) ;
#95413 = ORIENTED_EDGE ( 'NONE', *, *, #154904, .F. ) ;
#95414 = FACE_OUTER_BOUND ( 'NONE', #205300, .T. ) ;
#95415 = ADVANCED_FACE ( 'NONE', ( #178659 ), #199430, .T. ) ;
#95417 = EDGE_LOOP ( 'NONE', ( #98083, #73065, #79290, #170062, #223448, #134111, #56178, #251590, #65961, #73271 ) ) ;
#95416 = CYLINDRICAL_SURFACE ( 'NONE', #216894, 0.09999999999999939493 ) ;
#95418 = CARTESIAN_POINT ( 'NONE',  ( -23.15000000000000213, -9.600000000000001421, -23.60603087734756045 ) ) ;
#95419 = DIRECTION ( 'NONE',  ( 0.000000000000000000, 6.467318590049456648E-15, -1.000000000000000000 ) ) ;
#95420 = VERTEX_POINT ( 'NONE', #36584 ) ;
#95421 = PLANE ( 'NONE',  #56329 ) ;
#95422 = CARTESIAN_POINT ( 'NONE',  ( 18.49999999999999289, 33.67810952736942198, -236.3734420906320679 ) ) ;
#95423 = FACE_OUTER_BOUND ( 'NONE', #25159, .T. ) ;
#95424 = CARTESIAN_POINT ( 'NONE',  ( -23.15000000000000213, -9.599999999988844124, -88.75000000000004263 ) ) ;
#95426 = CARTESIAN_POINT ( 'NONE',  ( 20.09999999999999787, 11.49509093111729108, -207.9633242410238552 ) ) ;
#95425 = AXIS2_PLACEMENT_3D ( 'NONE', #20673, #169828, #178471 ) ;
#95428 = DIRECTION ( 'NONE',  ( 1.000000000000000000, 0.000000000000000000, 0.000000000000000000 ) ) ;
#95427 = AXIS2_PLACEMENT_3D ( 'NONE', #87452, #187874, #30094 ) ;
#95429 = CYLINDRICAL_SURFACE ( 'NONE', #36192, 0.09999999999999939493 ) ;
#95430 = VECTOR ( 'NONE', #180614, 1000.000000000000000 ) ;
#95431 = CARTESIAN_POINT ( 'NONE',  ( -23.15000000000000213, 4.350000000011156054, -121.7500000000000426 ) ) ;
#95432 = DIRECTION ( 'NONE',  ( -1.000000000000000000, 0.000000000000000000, -0.000000000000000000 ) ) ;
#95433 = ORIENTED_EDGE ( 'NONE', *, *, #235614, .T. ) ;
#95435 = ORIENTED_EDGE ( 'NONE', *, *, #93575, .T. ) ;
#95434 = VERTEX_POINT ( 'NONE', #177376 ) ;
#95436 = ORIENTED_EDGE ( 'NONE', *, *, #107954, .T. ) ;
#95437 = LINE ( 'NONE', #253219, #78028 ) ;
#95438 = DIRECTION ( 'NONE',  ( 1.000000000000000000, -0.000000000000000000, -0.000000000000000000 ) ) ;
#95440 = LINE ( 'NONE', #175036, #248847 ) ;
#95439 = LINE ( 'NONE', #150296, #228421 ) ;
#95441 = EDGE_LOOP ( 'NONE', ( #2667, #127763, #3941, #241634 ) ) ;
#95442 = ORIENTED_EDGE ( 'NONE', *, *, #153683, .T. ) ;
#95443 = DIRECTION ( 'NONE',  ( 0.000000000000000000, 0.000000000000000000, 1.000000000000000000 ) ) ;
#95444 = DIRECTION ( 'NONE',  ( 0.000000000000000000, -2.775557561562888827E-14, 1.000000000000000000 ) ) ;
#95445 = CARTESIAN_POINT ( 'NONE',  ( -18.39999999999999858, 78.33723480602354527, -231.5810597241785729 ) ) ;
#95446 = CARTESIAN_POINT ( 'NONE',  ( -20.94999999999999929, 57.84918772656043728, -226.1321410194968280 ) ) ;
#95447 = ORIENTED_EDGE ( 'NONE', *, *, #87919, .T. ) ;
#95448 = ORIENTED_EDGE ( 'NONE', *, *, #64134, .T. ) ;
#95449 = TOROIDAL_SURFACE ( 'NONE', #128774, 0.4000000000000005773, 0.1000000000000000056 ) ;
#95450 = CARTESIAN_POINT ( 'NONE',  ( -15.55912972643741199, 8.490870273562562076, -12.55000000000000249 ) ) ;
#95451 = CARTESIAN_POINT ( 'NONE',  ( 21.07928932188134397, 1.115600667400684642E-11, -167.4999999999999716 ) ) ;
#95452 = ORIENTED_EDGE ( 'NONE', *, *, #142097, .T. ) ;
#95453 = CYLINDRICAL_SURFACE ( 'NONE', #82921, 0.09999999999999950595 ) ;
#95454 = FACE_OUTER_BOUND ( 'NONE', #187787, .T. ) ;
#95455 = AXIS2_PLACEMENT_3D ( 'NONE', #180428, #177873, #139985 ) ;
#95456 = DIRECTION ( 'NONE',  ( 1.000000000000000000, 1.836970198721029934E-16, 3.186635328391151676E-31 ) ) ;
#95457 = CARTESIAN_POINT ( 'NONE',  ( 23.14999999999999503, 11.65000000001116298, -126.9851942293460922 ) ) ;
#95458 = DIRECTION ( 'NONE',  ( 0.000000000000000000, -0.2617529984165033463, -0.9651348961777157509 ) ) ;
#95459 = ORIENTED_EDGE ( 'NONE', *, *, #142470, .T. ) ;
#95460 = LINE ( 'NONE', #117597, #156960 ) ;
#95461 = FACE_OUTER_BOUND ( 'NONE', #122963, .T. ) ;
#95462 = CARTESIAN_POINT ( 'NONE',  ( -18.59999999999999787, 1.835341550235567887, -78.65515129256301918 ) ) ;
#95464 = DIRECTION ( 'NONE',  ( 1.000000000000000000, 0.000000000000000000, 0.000000000000000000 ) ) ;
#95463 = CARTESIAN_POINT ( 'NONE',  ( -23.25000000000000000, 77.83585931145546510, -91.51866831572576189 ) ) ;
#95466 = EDGE_CURVE ( 'NONE', #10380, #185627, #211887, .T. ) ;
#95465 = DIRECTION ( 'NONE',  ( 0.000000000000000000, -1.000000000000000000, -6.982962677686266711E-15 ) ) ;
#95467 = DIRECTION ( 'NONE',  ( -1.000000000000000000, 0.000000000000000000, -0.000000000000000000 ) ) ;
#95468 = DIRECTION ( 'NONE',  ( -1.000000000000000000, -0.000000000000000000, 0.000000000000000000 ) ) ;
#95469 = FACE_OUTER_BOUND ( 'NONE', #53255, .T. ) ;
#95470 = CIRCLE ( 'NONE', #228758, 0.09999999999998898659 ) ;
#95471 = ORIENTED_EDGE ( 'NONE', *, *, #32888, .T. ) ;
#95472 = AXIS2_PLACEMENT_3D ( 'NONE', #209098, #70905, #150433 ) ;
#95473 = ORIENTED_EDGE ( 'NONE', *, *, #135493, .T. ) ;
#95474 = CARTESIAN_POINT ( 'NONE',  ( 18.69999999999999929, -10.84999999999999076, 31.59999999999999787 ) ) ;
#95475 = ORIENTED_EDGE ( 'NONE', *, *, #29012, .T. ) ;
#95476 = CARTESIAN_POINT ( 'NONE',  ( -20.64999999999999858, -9.399999999988846611, -57.10603087734755690 ) ) ;
#95477 = CIRCLE ( 'NONE', #228767, 11.74999999999999112 ) ;
#95478 = VECTOR ( 'NONE', #66046, 1000.000000000000000 ) ;
#95479 = EDGE_CURVE ( 'NONE', #148838, #84065, #16093, .T. ) ;
#95480 = EDGE_LOOP ( 'NONE', ( #95459, #191124, #243578, #177164 ) ) ;
#95481 = CARTESIAN_POINT ( 'NONE',  ( -20.64999999999999858, 68.75000000001179501, -81.87310748452436826 ) ) ;
#95482 = VERTEX_POINT ( 'NONE', #136925 ) ;
#95483 = AXIS2_PLACEMENT_3D ( 'NONE', #207082, #144513, #27191 ) ;
#95484 = DIRECTION ( 'NONE',  ( -1.000000000000000000, 0.000000000000000000, 0.000000000000000000 ) ) ;
#95485 = VECTOR ( 'NONE', #22128, 1000.000000000000114 ) ;
#95486 = AXIS2_PLACEMENT_3D ( 'NONE', #81308, #184289, #146434 ) ;
#95487 = DIRECTION ( 'NONE',  ( 0.000000000000000000, 0.000000000000000000, 1.000000000000000000 ) ) ;
#95488 = DIRECTION ( 'NONE',  ( 1.000000000000000000, 0.000000000000000000, 1.073024830501117725E-15 ) ) ;
#95489 = AXIS2_PLACEMENT_3D ( 'NONE', #210887, #169232, #132642 ) ;
#95490 = EDGE_CURVE ( 'NONE', #248044, #151819, #232734, .T. ) ;
#95491 = EDGE_CURVE ( 'NONE', #18113, #118231, #153672, .T. ) ;
#95492 = CARTESIAN_POINT ( 'NONE',  ( 23.14999999999999503, 69.55000000001246008, -181.7731074845244166 ) ) ;
#95494 = ORIENTED_EDGE ( 'NONE', *, *, #198613, .T. ) ;
#95493 = CARTESIAN_POINT ( 'NONE',  ( -16.77431908686106610, 30.19186540481982206, -234.8040555917334302 ) ) ;
#95496 = CARTESIAN_POINT ( 'NONE',  ( 20.04142135391667168, 11.75000000001116263, -192.2025068656294309 ) ) ;
#95495 = CARTESIAN_POINT ( 'NONE',  ( 21.04999999999999716, 6.297325973826397139, -199.6466443475954122 ) ) ;
#95497 = CIRCLE ( 'NONE', #166262, 0.09999999999998898659 ) ;
#95498 = DIRECTION ( 'NONE',  ( -0.000000000000000000, 0.000000000000000000, 1.000000000000000000 ) ) ;
#95499 = DIRECTION ( 'NONE',  ( 0.000000000000000000, 0.9910465087640860649, -0.1335171055202901413 ) ) ;
#95501 = EDGE_CURVE ( 'NONE', #103887, #237621, #19560, .T. ) ;
#95500 = CARTESIAN_POINT ( 'NONE',  ( -21.14999999999994174, 79.88763423575340994, -7.282924647898262549 ) ) ;
#95502 = CARTESIAN_POINT ( 'NONE',  ( 20.94999999999999929, 1.115650877919449575E-11, -129.9000000000000341 ) ) ;
#95503 = ORIENTED_EDGE ( 'NONE', *, *, #76418, .F. ) ;
#95504 = FILL_AREA_STYLE_COLOUR ( '', #119518 ) ;
#95505 = CARTESIAN_POINT ( 'NONE',  ( -16.87331047859651179, 9.950000000011142376, -113.1500000000000341 ) ) ;
#95506 = EDGE_CURVE ( 'NONE', #228856, #243788, #195643, .T. ) ;
#95507 = ORIENTED_EDGE ( 'NONE', *, *, #105555, .F. ) ;
#95508 = CYLINDRICAL_SURFACE ( 'NONE', #69022, 0.09999999999999939493 ) ;
#95510 = ORIENTED_EDGE ( 'NONE', *, *, #43528, .F. ) ;
#95509 = AXIS2_PLACEMENT_3D ( 'NONE', #21486, #17595, #136245 ) ;
#95511 = LINE ( 'NONE', #96765, #26235 ) ;
#95512 = EDGE_CURVE ( 'NONE', #17744, #57945, #136860, .T. ) ;
#95513 = CARTESIAN_POINT ( 'NONE',  ( -16.91776028072577631, 9.963400393629743945, -20.87502401470212732 ) ) ;
#95514 = DIRECTION ( 'NONE',  ( 1.000000000000000000, 0.000000000000000000, 0.000000000000000000 ) ) ;
#95515 = EDGE_LOOP ( 'NONE', ( #73657, #86900, #14825, #235566, #141504, #47026, #184571, #201343, #157544, #155360, #185359, #80456 ) ) ;
#95516 = ORIENTED_EDGE ( 'NONE', *, *, #161459, .F. ) ;
#95517 = AXIS2_PLACEMENT_3D ( 'NONE', #42, #57440, #239960 ) ;
#95518 = EDGE_CURVE ( 'NONE', #185762, #28751, #195145, .T. ) ;
#95519 = CARTESIAN_POINT ( 'NONE',  ( -21.05000000000000071, 76.00000000001216449, -140.8231074845242574 ) ) ;
#95520 = CARTESIAN_POINT ( 'NONE',  ( 20.95083306685154056, 10.51659053420942413, -207.3856434995966538 ) ) ;
#95521 = CARTESIAN_POINT ( 'NONE',  ( -20.94999999999999929, -11.64999999999999858, -30.39999999999999503 ) ) ;
#95522 = CARTESIAN_POINT ( 'NONE',  ( -23.15000000000000213, 1.115651490242849210E-11, -29.35000000000000142 ) ) ;
#95523 = AXIS2_PLACEMENT_3D ( 'NONE', #139830, #120327, #58991 ) ;
#95525 = DIRECTION ( 'NONE',  ( 0.000000000000000000, 0.000000000000000000, -1.000000000000000000 ) ) ;
#95524 = DIRECTION ( 'NONE',  ( 0.000000000000000000, 0.000000000000000000, -1.000000000000000000 ) ) ;
#95526 = CARTESIAN_POINT ( 'NONE',  ( -14.00000000000000178, 9.849999999999978328, -16.75000000000000355 ) ) ;
#95527 = CARTESIAN_POINT ( 'NONE',  ( 12.68104795156994768, 9.396533993965078935, -51.40593977917330193 ) ) ;
#95528 = CARTESIAN_POINT ( 'NONE',  ( -18.59999999999999787, 18.81339837015603322, -226.7756228984618190 ) ) ;
#95529 = ORIENTED_EDGE ( 'NONE', *, *, #180165, .T. ) ;
#95530 = CARTESIAN_POINT ( 'NONE',  ( -20.64999999999999858, 36.65892442174935439, -249.5511627012433848 ) ) ;
#95531 = AXIS2_PLACEMENT_3D ( 'NONE', #251972, #70800, #73372 ) ;
#95533 = EDGE_LOOP ( 'NONE', ( #50688, #95596, #184320, #186378 ) ) ;
#95532 = CARTESIAN_POINT ( 'NONE',  ( -23.15000000000000213, 86.52890073500824997, -209.5906233940697234 ) ) ;
#95534 = FACE_OUTER_BOUND ( 'NONE', #106637, .T. ) ;
#95535 = DIRECTION ( 'NONE',  ( 0.000000000000000000, -0.9126074666063660468, -0.4088369013363524762 ) ) ;
#95537 = DIRECTION ( 'NONE',  ( 0.000000000000000000, 0.9126074666063660468, 0.4088369013363524762 ) ) ;
#95536 = CARTESIAN_POINT ( 'NONE',  ( -16.97683809663752186, 23.64127277249475156, -231.2903243416350847 ) ) ;
#95539 = ORIENTED_EDGE ( 'NONE', *, *, #80907, .F. ) ;
#95538 = CARTESIAN_POINT ( 'NONE',  ( -18.50000000000000000, -1.164121893230052995, -208.7148480855715604 ) ) ;
#95541 = DIRECTION ( 'NONE',  ( 0.000000000000000000, -0.9651348961777157509, 0.2617529984165031243 ) ) ;
#95540 = DIRECTION ( 'NONE',  ( -1.000000000000000000, 0.000000000000000000, -0.000000000000000000 ) ) ;
#95542 = CARTESIAN_POINT ( 'NONE',  ( -16.89021194854739605, 51.52081980694187990, -231.9903911278292981 ) ) ;
#95543 = DIRECTION ( 'NONE',  ( -0.000000000000000000, 0.9651348961777157509, -0.2617529984165031243 ) ) ;
#95544 = DIRECTION ( 'NONE',  ( -0.000000000000000000, 0.7397360091702694929, 0.6728971962616898672 ) ) ;
#95545 = DIRECTION ( 'NONE',  ( 1.000000000000000000, 0.000000000000000000, 0.000000000000000000 ) ) ;
#95546 = ORIENTED_EDGE ( 'NONE', *, *, #225571, .F. ) ;
#95547 = CYLINDRICAL_SURFACE ( 'NONE', #222063, 0.1000000000000054040 ) ;
#95549 = ORIENTED_EDGE ( 'NONE', *, *, #240711, .F. ) ;
#95548 = CIRCLE ( 'NONE', #195536, 0.09999999999998898659 ) ;
#95550 = AXIS2_PLACEMENT_3D ( 'NONE', #246442, #126490, #185184 ) ;
#95551 = LINE ( 'NONE', #198505, #67645 ) ;
#95552 = VERTEX_POINT ( 'NONE', #114800 ) ;
#95553 = CARTESIAN_POINT ( 'NONE',  ( -20.90851465518106167, 46.44433919924416898, -243.0795225066946159 ) ) ;
#95554 = AXIS2_PLACEMENT_3D ( 'NONE', #27687, #6794, #147592 ) ;
#95555 = ORIENTED_EDGE ( 'NONE', *, *, #256196, .F. ) ;
#95556 = EDGE_CURVE ( 'NONE', #15852, #51812, #24456, .T. ) ;
#95557 = DIRECTION ( 'NONE',  ( 0.000000000000000000, 0.6046243595031880469, 0.7965107556683460599 ) ) ;
#95558 = DIRECTION ( 'NONE',  ( 0.7071067811865475727, -0.7071067811865475727, 0.000000000000000000 ) ) ;
#95559 = DIRECTION ( 'NONE',  ( 0.000000000000000000, -0.9915357197604971473, 0.1298341882519111479 ) ) ;
#95560 = EDGE_LOOP ( 'NONE', ( #11616, #90523, #122381, #56456 ) ) ;
#95561 = EDGE_CURVE ( 'NONE', #57819, #59493, #128482, .T. ) ;
#95562 = EDGE_CURVE ( 'NONE', #64056, #194835, #28584, .T. ) ;
#95563 = CARTESIAN_POINT ( 'NONE',  ( -22.14074124539699895, -1.475831776601470802, -193.7581091773087110 ) ) ;
#95564 = ADVANCED_FACE ( 'NONE', ( #58648 ), #25080, .T. ) ;
#95565 = CARTESIAN_POINT ( 'NONE',  ( 16.87683809663750267, 66.05000000001207638, -123.8731074845243683 ) ) ;
#95567 = AXIS2_PLACEMENT_3D ( 'NONE', #60952, #158808, #16718 ) ;
#95566 = CARTESIAN_POINT ( 'NONE',  ( 21.15000000000005187, 87.50449464844290048, -37.85861909827351468 ) ) ;
#95568 = DIRECTION ( 'NONE',  ( 0.000000000000000000, 0.000000000000000000, -1.000000000000000000 ) ) ;
#95569 = EDGE_CURVE ( 'NONE', #28934, #153892, #91070, .T. ) ;
#95570 = VERTEX_POINT ( 'NONE', #66381 ) ;
#95572 = EDGE_CURVE ( 'NONE', #21323, #13609, #126345, .T. ) ;
#95571 = DIRECTION ( 'NONE',  ( -1.000000000000000000, 0.000000000000000000, 0.000000000000000000 ) ) ;
#95573 = ORIENTED_EDGE ( 'NONE', *, *, #18514, .T. ) ;
#95575 = ORIENTED_EDGE ( 'NONE', *, *, #249854, .T. ) ;
#95574 = CARTESIAN_POINT ( 'NONE',  ( -21.14999999999999858, 76.10000000001245724, -181.6726782920691505 ) ) ;
#95576 = ORIENTED_EDGE ( 'NONE', *, *, #39151, .F. ) ;
#95577 = CARTESIAN_POINT ( 'NONE',  ( 21.46681500597990677, 1.115539681028482333E-11, -60.14248884057332134 ) ) ;
#95578 = DIRECTION ( 'NONE',  ( -1.000000000000000000, 2.952720810173289112E-16, 2.061873921506763405E-30 ) ) ;
#95579 = DIRECTION ( 'NONE',  ( 0.000000000000000000, -0.8814952561688476074, 0.4721928772777262417 ) ) ;
#95580 = ADVANCED_FACE ( 'NONE', ( #181208 ), #243731, .T. ) ;
#95581 = DIRECTION ( 'NONE',  ( 1.000000000000000000, 0.000000000000000000, 0.000000000000000000 ) ) ;
#95582 = EDGE_LOOP ( 'NONE', ( #224705, #240071, #84832 ) ) ;
#95583 = CARTESIAN_POINT ( 'NONE',  ( -16.97048326478264713, 9.950000000011137047, -147.1411068801272108 ) ) ;
#95584 = DIRECTION ( 'NONE',  ( 1.000000000000000000, 0.000000000000000000, 0.000000000000000000 ) ) ;
#95585 = ORIENTED_EDGE ( 'NONE', *, *, #35431, .T. ) ;
#95587 = ORIENTED_EDGE ( 'NONE', *, *, #171932, .T. ) ;
#95586 = CARTESIAN_POINT ( 'NONE',  ( -16.90202395485833264, 66.03405545546138455, -115.6200937632638954 ) ) ;
#95588 = CARTESIAN_POINT ( 'NONE',  ( 20.12481660106788439, 66.47365600773714789, -128.2969658154281660 ) ) ;
#95589 = DIRECTION ( 'NONE',  ( -0.000000000000000000, -0.000000000000000000, 1.000000000000000000 ) ) ;
#95590 = AXIS2_PLACEMENT_3D ( 'NONE', #73782, #34650, #253655 ) ;
#95591 = AXIS2_PLACEMENT_3D ( 'NONE', #229505, #234629, #190391 ) ;
#95592 = EDGE_CURVE ( 'NONE', #207603, #15847, #178593, .T. ) ;
#95593 = VECTOR ( 'NONE', #133419, 1000.000000000000000 ) ;
#95595 = AXIS2_PLACEMENT_3D ( 'NONE', #200667, #203224, #22040 ) ;
#95594 = LINE ( 'NONE', #21226, #201279 ) ;
#95596 = ORIENTED_EDGE ( 'NONE', *, *, #83341, .T. ) ;
#95597 = EDGE_CURVE ( 'NONE', #233373, #221772, #57739, .T. ) ;
#95598 = AXIS2_PLACEMENT_3D ( 'NONE', #176042, #195605, #233448 ) ;
#95599 = CARTESIAN_POINT ( 'NONE',  ( -20.90000000000000213, 7.973296578895943121, 1.410778198689825347 ) ) ;
#95600 = VERTEX_POINT ( 'NONE', #100339 ) ;
#95601 = CARTESIAN_POINT ( 'NONE',  ( -23.15000000000000213, 64.35000000001150511, -48.17310748452440805 ) ) ;
#95602 = B_SPLINE_CURVE_WITH_KNOTS ( 'NONE', 3,
 ( #139555, #116177, #96570, #176159, #40518, #155322, #138267, #234825, #255618, #19639 ),
 .UNSPECIFIED., .F., .F.,
 ( 4, 2, 2, 2, 4 ),
 ( 0.000000000000000000, 3.990160268012894350E-05, 7.980320536025788699E-05, 0.0001596064107205239868, 0.0003192128214410228202 ),
 .UNSPECIFIED. ) ;
#95603 = EDGE_CURVE ( 'NONE', #238064, #222495, #61850, .T. ) ;
#95604 = DIRECTION ( 'NONE',  ( 0.000000000000000000, 0.000000000000000000, 1.000000000000000000 ) ) ;
#95605 = ADVANCED_FACE ( 'NONE', ( #144611 ), #224155, .F. ) ;
#95606 = SPHERICAL_SURFACE ( 'NONE', #96856, 0.1000000000000000056 ) ;
#95607 = AXIS2_PLACEMENT_3D ( 'NONE', #122131, #221207, #158717 ) ;
#95608 = AXIS2_PLACEMENT_3D ( 'NONE', #99137, #242518, #118743 ) ;
#95609 = ORIENTED_EDGE ( 'NONE', *, *, #65694, .F. ) ;
#95610 = CARTESIAN_POINT ( 'NONE',  ( 20.95429402530582408, 67.12380584890942714, -61.00002078658653204 ) ) ;
#95611 = ORIENTED_EDGE ( 'NONE', *, *, #151543, .T. ) ;
#95612 = CARTESIAN_POINT ( 'NONE',  ( -21.05000000000000071, 44.00266445878927613, -258.8505972146074896 ) ) ;
#95613 = CARTESIAN_POINT ( 'NONE',  ( -23.25000000000000000, 1.910280373842930812, -121.3686321448010972 ) ) ;
#95615 = ORIENTED_EDGE ( 'NONE', *, *, #141912, .T. ) ;
#95614 = CARTESIAN_POINT ( 'NONE',  ( 20.95512840106819752, 10.62384869378447583, -146.2024792207988924 ) ) ;
#95616 = LINE ( 'NONE', #210453, #161768 ) ;
#95617 = DIRECTION ( 'NONE',  ( 0.000000000000000000, -0.2617529984165036239, -0.9651348961777156399 ) ) ;
#95618 = CARTESIAN_POINT ( 'NONE',  ( -15.75000000000000355, 66.15000000001185754, -86.27310748452437394 ) ) ;
#95619 = DIRECTION ( 'NONE',  ( -1.652117596168391897E-15, 0.4088369013363280513, -0.9126074666063769270 ) ) ;
#95620 = CARTESIAN_POINT ( 'NONE',  ( 21.11833042828137508, 6.445644693866518615, -33.49289949094065122 ) ) ;
#95621 = DIRECTION ( 'NONE',  ( 0.000000000000000000, 7.056502275159890832E-15, -1.000000000000000000 ) ) ;
#95622 = CARTESIAN_POINT ( 'NONE',  ( 21.08621493067296626, 6.349294291182826733, -66.94380516052393659 ) ) ;
#95624 = VERTEX_POINT ( 'NONE', #183761 ) ;
#95623 = LINE ( 'NONE', #57774, #161137 ) ;
#95625 = CONICAL_SURFACE ( 'NONE', #212164, 4.049999999999998046, 0.7853981633974604915 ) ;
#95626 = CARTESIAN_POINT ( 'NONE',  ( 18.59999999999999076, 28.81810206650552075, -238.0339362645743222 ) ) ;
#95627 = TOROIDAL_SURFACE ( 'NONE', #83124, 0.2000000000000000111, 0.1000000000000000056 ) ;
#95628 = DIRECTION ( 'NONE',  ( 1.836970198721029934E-16, 1.000000000000000000, 6.982962677686266711E-15 ) ) ;
#95629 = CARTESIAN_POINT ( 'NONE',  ( -18.60000000000000142, 85.32100840337393777, -196.2871692354464130 ) ) ;
#95630 = VERTEX_POINT ( 'NONE', #2536 ) ;
#95631 = DIRECTION ( 'NONE',  ( 1.000000000000000000, -0.000000000000000000, -0.000000000000000000 ) ) ;
#95632 = EDGE_CURVE ( 'NONE', #145626, #196062, #111936, .T. ) ;
#95633 = CARTESIAN_POINT ( 'NONE',  ( -1.820710678118658388, -4.456319993567025683, -227.1983682421737569 ) ) ;
#95634 = DIRECTION ( 'NONE',  ( -1.000000000000000000, 0.000000000000000000, 0.000000000000000000 ) ) ;
#95635 = EDGE_CURVE ( 'NONE', #53354, #111912, #105464, .T. ) ;
#95636 = ORIENTED_EDGE ( 'NONE', *, *, #45079, .T. ) ;
#95637 = AXIS2_PLACEMENT_3D ( 'NONE', #59938, #136930, #238602 ) ;
#95638 = FACE_OUTER_BOUND ( 'NONE', #69141, .T. ) ;
#95639 = AXIS2_PLACEMENT_3D ( 'NONE', #186679, #86251, #6739 ) ;
#95640 = CARTESIAN_POINT ( 'NONE',  ( -16.94062896051973865, 66.00728089491192918, -190.9205909424056244 ) ) ;
#95641 = ADVANCED_FACE ( 'NONE', ( #220329 ), #161831, .T. ) ;
#95642 = VERTEX_POINT ( 'NONE', #121261 ) ;
#95644 = ADVANCED_FACE ( 'NONE', ( #6397 ), #66120, .T. ) ;
#95643 = CARTESIAN_POINT ( 'NONE',  ( 18.49999999999999289, 21.17283678855157802, -243.7231193059830332 ) ) ;
#95645 = AXIS2_PLACEMENT_3D ( 'NONE', #34575, #172833, #78790 ) ;
#95646 = EDGE_LOOP ( 'NONE', ( #81696, #21699, #246152, #79672 ) ) ;
#95647 = CARTESIAN_POINT ( 'NONE',  ( 21.05000000000000071, 77.04701199367727327, -199.6625678998140359 ) ) ;
#95649 = ORIENTED_EDGE ( 'NONE', *, *, #169480, .F. ) ;
#95648 = CARTESIAN_POINT ( 'NONE',  ( 21.09096482362069835, 6.363544365415761739, -133.9605517212259542 ) ) ;
#95650 = AXIS2_PLACEMENT_3D ( 'NONE', #243660, #181139, #80715 ) ;
#95651 = VECTOR ( 'NONE', #76306, 1000.000000000000114 ) ;
#95652 = CARTESIAN_POINT ( 'NONE',  ( 23.24999999999999645, 67.23127455305841238, -235.8551265064783991 ) ) ;
#95653 = ORIENTED_EDGE ( 'NONE', *, *, #200460, .T. ) ;
#95654 = FACE_OUTER_BOUND ( 'NONE', #204358, .T. ) ;
#95655 = EDGE_LOOP ( 'NONE', ( #69923, #64132, #72807, #103899 ) ) ;
#95657 = EDGE_LOOP ( 'NONE', ( #106826, #133801, #227536, #236165 ) ) ;
#95656 = ORIENTED_EDGE ( 'NONE', *, *, #100332, .F. ) ;
#95658 = CARTESIAN_POINT ( 'NONE',  ( 23.25000000000000355, 52.04006110304540300, -267.2673759609633635 ) ) ;
#95659 = ORIENTED_EDGE ( 'NONE', *, *, #255330, .T. ) ;
#95660 = FACE_OUTER_BOUND ( 'NONE', #49891, .T. ) ;
#95661 = ORIENTED_EDGE ( 'NONE', *, *, #233639, .T. ) ;
#95662 = AXIS2_PLACEMENT_3D ( 'NONE', #103783, #102493, #165070 ) ;
#95664 = EDGE_CURVE ( 'NONE', #19166, #225834, #78591, .T. ) ;
#95663 = VECTOR ( 'NONE', #200436, 1000.000000000000000 ) ;
#95665 = VECTOR ( 'NONE', #130744, 999.9999999999998863 ) ;
#95666 = AXIS2_PLACEMENT_3D ( 'NONE', #217456, #137922, #135359 ) ;
#95667 = ORIENTED_EDGE ( 'NONE', *, *, #254894, .T. ) ;
#95669 = CIRCLE ( 'NONE', #99743, 0.1000000000000028644 ) ;
#95668 = CARTESIAN_POINT ( 'NONE',  ( 18.39999999999999858, -7.817436562502981801, -209.8389866834999395 ) ) ;
#95670 = CARTESIAN_POINT ( 'NONE',  ( 21.05000000000000071, 76.00000000001205080, -123.5481074845242802 ) ) ;
#95671 = DIRECTION ( 'NONE',  ( 0.000000000000000000, -0.8660254037844411501, -0.4999999999999956701 ) ) ;
#95672 = ORIENTED_EDGE ( 'NONE', *, *, #164694, .T. ) ;
#95673 = DIRECTION ( 'NONE',  ( 0.000000000000000000, 0.000000000000000000, 1.000000000000000000 ) ) ;
#95674 = PLANE ( 'NONE',  #123099 ) ;
#95675 = CARTESIAN_POINT ( 'NONE',  ( 20.94999999999999574, -1.835341550224411922, -11.55515129256297868 ) ) ;
#95676 = VERTEX_POINT ( 'NONE', #44260 ) ;
#95677 = CARTESIAN_POINT ( 'NONE',  ( -20.64999999999999858, 44.91518204311810081, -238.0177672736398620 ) ) ;
#95679 = EDGE_CURVE ( 'NONE', #121929, #209214, #45274, .T. ) ;
#95678 = PLANE ( 'NONE',  #161285 ) ;
#95680 = LINE ( 'NONE', #51390, #124004 ) ;
#95681 = VERTEX_POINT ( 'NONE', #123790 ) ;
#95682 = ADVANCED_FACE ( 'NONE', ( #203326 ), #221572, .T. ) ;
#95683 = LINE ( 'NONE', #93117, #13829 ) ;
#95684 = VERTEX_POINT ( 'NONE', #62531 ) ;
#95685 = ORIENTED_EDGE ( 'NONE', *, *, #8475, .T. ) ;
#95686 = CARTESIAN_POINT ( 'NONE',  ( -20.94999999999999929, 76.00000000001244871, -170.0231074845243597 ) ) ;
#95687 = ORIENTED_EDGE ( 'NONE', *, *, #11040, .F. ) ;
#95688 = VERTEX_POINT ( 'NONE', #202041 ) ;
#95689 = CARTESIAN_POINT ( 'NONE',  ( -18.59999999999999787, 7.783179459866048866, -245.3643104511423019 ) ) ;
#95690 = CARTESIAN_POINT ( 'NONE',  ( 22.50000000000000000, 76.00000000001195133, -103.0231074845243171 ) ) ;
#95691 = ORIENTED_EDGE ( 'NONE', *, *, #57052, .F. ) ;
#95692 = ORIENTED_EDGE ( 'NONE', *, *, #19191, .T. ) ;
#95693 = EDGE_CURVE ( 'NONE', #150597, #135871, #209745, .T. ) ;
#95694 = DIRECTION ( 'NONE',  ( 0.000000000000000000, -1.000000000000000000, 0.000000000000000000 ) ) ;
#95695 = DIRECTION ( 'NONE',  ( 1.000000000000000000, 0.000000000000000000, -0.000000000000000000 ) ) ;
#95696 = ADVANCED_FACE ( 'NONE', ( #108081 ), #27289, .T. ) ;
#95697 = CIRCLE ( 'NONE', #120673, 0.09999999999999939493 ) ;
#95698 = ORIENTED_EDGE ( 'NONE', *, *, #175806, .T. ) ;
#95699 = CIRCLE ( 'NONE', #12529, 11.65000000000000036 ) ;
#95700 = EDGE_CURVE ( 'NONE', #127870, #80656, #53654, .T. ) ;
#95701 = ORIENTED_EDGE ( 'NONE', *, *, #55422, .T. ) ;
#95702 = CIRCLE ( 'NONE', #29133, 0.09999999999998898659 ) ;
#95703 = CARTESIAN_POINT ( 'NONE',  ( -20.64999999999999858, 7.250000000011155521, -188.6499999999999488 ) ) ;
#95704 = CARTESIAN_POINT ( 'NONE',  ( 18.39999999999999503, 11.47316190337363828, -188.3499999999999659 ) ) ;
#95705 = EDGE_CURVE ( 'NONE', #213950, #119397, #228455, .T. ) ;
#95706 = CARTESIAN_POINT ( 'NONE',  ( -16.89060415895971090, 9.951220762813354881, -46.14592022427046203 ) ) ;
#95707 = DIRECTION ( 'NONE',  ( 1.000000000000000000, 0.000000000000000000, 0.000000000000000000 ) ) ;
#95708 = FACE_OUTER_BOUND ( 'NONE', #197230, .T. ) ;
#95709 = AXIS2_PLACEMENT_3D ( 'NONE', #108994, #169027, #69910 ) ;
#95710 = DIRECTION ( 'NONE',  ( 0.000000000000000000, 0.2128009952263630322, -0.9770955615653309501 ) ) ;
#95711 = ADVANCED_FACE ( 'NONE', ( #151059 ), #3568, .T. ) ;
#95712 = AXIS2_PLACEMENT_3D ( 'NONE', #204728, #207332, #206032 ) ;
#95714 = CARTESIAN_POINT ( 'NONE',  ( -21.05000000000000071, 87.65000000001246860, -173.1231074845242688 ) ) ;
#95713 = CARTESIAN_POINT ( 'NONE',  ( 21.05000000000000071, 75.96798630682366138, -75.78195020806214188 ) ) ;
#95715 = DIRECTION ( 'NONE',  ( 0.000000000000000000, -1.000000000000000000, 0.000000000000000000 ) ) ;
#95716 = DIRECTION ( 'NONE',  ( 1.186688945009010077E-16, 1.000000000000000000, 6.982962677686266711E-15 ) ) ;
#95717 = CARTESIAN_POINT ( 'NONE',  ( -21.05000000000000071, 87.75000000001192291, -106.0231074845242176 ) ) ;
#95718 = DIRECTION ( 'NONE',  ( -1.000000000000000000, -0.000000000000000000, -0.000000000000000000 ) ) ;
#95719 = CIRCLE ( 'NONE', #70646, 4.099999999999999645 ) ;
#95720 = ORIENTED_EDGE ( 'NONE', *, *, #50581, .F. ) ;
#95722 = ORIENTED_EDGE ( 'NONE', *, *, #95798, .T. ) ;
#95721 = CYLINDRICAL_SURFACE ( 'NONE', #78164, 0.1000000000000000472 ) ;
#95723 = DIRECTION ( 'NONE',  ( 0.000000000000000000, 0.000000000000000000, 1.000000000000000000 ) ) ;
#95724 = CARTESIAN_POINT ( 'NONE',  ( 19.90000000000000568, 5.586869315528661062, 16.41686199900910736 ) ) ;
#95725 = ORIENTED_EDGE ( 'NONE', *, *, #255199, .T. ) ;
#95726 =( NAMED_UNIT ( * ) PLANE_ANGLE_UNIT ( ) SI_UNIT ( $, .RADIAN. ) );
#95727 = B_SPLINE_CURVE_WITH_KNOTS ( 'NONE', 3,
 ( #205375, #142825, #81560, #101101, #146675, #41217, #43755, #185828, #7176, #86703, #120754, #2041, #240668, #30637 ),
 .UNSPECIFIED., .F., .F.,
 ( 4, 2, 2, 2, 2, 2, 4 ),
 ( 0.000000000000000000, 2.389617747644075618E-05, 4.779235495288151236E-05, 9.558470990574922824E-05, 0.0001911694198114619731, 0.0003823388396229078457, 0.0007646776792457995369 ),
 .UNSPECIFIED. ) ;
#95729 = DIRECTION ( 'NONE',  ( 0.000000000000000000, 6.982962677686266711E-15, -1.000000000000000000 ) ) ;
#95728 = CIRCLE ( 'NONE', #20770, 0.09999999999999939493 ) ;
#95730 = VECTOR ( 'NONE', #220706, 1000.000000000000000 ) ;
#95731 = CARTESIAN_POINT ( 'NONE',  ( -17.05016517656233432, 9.950000000010200907, -54.32730200400028053 ) ) ;
#95732 = ORIENTED_EDGE ( 'NONE', *, *, #111877, .F. ) ;
#95733 = CARTESIAN_POINT ( 'NONE',  ( 20.94999999999999929, 1.115600667400684642E-11, -134.0000000000000284 ) ) ;
#95734 = DIRECTION ( 'NONE',  ( 0.000000000000000000, -0.3634403228828347321, 0.9316174814283063599 ) ) ;
#95735 = DIRECTION ( 'NONE',  ( -1.000000000000000000, 0.000000000000000000, 0.000000000000000000 ) ) ;
#95737 = ORIENTED_EDGE ( 'NONE', *, *, #70450, .F. ) ;
#95736 = DIRECTION ( 'NONE',  ( 0.000000000000000000, -0.9770955615653315052, -0.2128009952263603954 ) ) ;
#95739 = ORIENTED_EDGE ( 'NONE', *, *, #49973, .F. ) ;
#95738 = CARTESIAN_POINT ( 'NONE',  ( -18.31572283045166216, 85.54843783089741294, -96.17248183346565327 ) ) ;
#95740 = FACE_OUTER_BOUND ( 'NONE', #146631, .T. ) ;
#95741 = DIRECTION ( 'NONE',  ( 1.000000000000000000, -0.000000000000000000, -0.000000000000000000 ) ) ;
#95742 = CYLINDRICAL_SURFACE ( 'NONE', #74152, 0.1000000000000028644 ) ;
#95743 = DIRECTION ( 'NONE',  ( -0.000000000000000000, 0.9770955615653316162, 0.2128009952263603122 ) ) ;
#95744 = AXIS2_PLACEMENT_3D ( 'NONE', #9623, #130856, #89154 ) ;
#95747 = LINE ( 'NONE', #159605, #162335 ) ;
#95746 = AXIS2_PLACEMENT_3D ( 'NONE', #123040, #242968, #162182 ) ;
#95745 = CARTESIAN_POINT ( 'NONE',  ( 18.49999999999999289, 9.070023979453765151, -245.4580351522096748 ) ) ;
#95749 = EDGE_CURVE ( 'NONE', #166926, #183834, #190192, .T. ) ;
#95748 = FACE_OUTER_BOUND ( 'NONE', #132616, .T. ) ;
#95750 = AXIS2_PLACEMENT_3D ( 'NONE', #163752, #86750, #45078 ) ;
#95751 = AXIS2_PLACEMENT_3D ( 'NONE', #80369, #63391, #142918 ) ;
#95752 = DIRECTION ( 'NONE',  ( 0.000000000000000000, 0.2617529984165045120, 0.9651348961777153068 ) ) ;
#95753 = DIRECTION ( 'NONE',  ( -1.000000000000000000, 7.304098846218133681E-16, -4.217023435051677994E-16 ) ) ;
#95754 = CARTESIAN_POINT ( 'NONE',  ( 20.04142135623730070, 11.75000000001115907, -155.3500000000000227 ) ) ;
#95755 = ORIENTED_EDGE ( 'NONE', *, *, #65652, .T. ) ;
#95756 = FACE_OUTER_BOUND ( 'NONE', #210243, .T. ) ;
#95757 = CIRCLE ( 'NONE', #37534, 0.1000000000000028644 ) ;
#95758 = ORIENTED_EDGE ( 'NONE', *, *, #5808, .F. ) ;
#95759 = VERTEX_POINT ( 'NONE', #7702 ) ;
#95760 = FACE_OUTER_BOUND ( 'NONE', #72808, .T. ) ;
#95761 = EDGE_CURVE ( 'NONE', #211306, #187198, #111942, .T. ) ;
#95762 = CARTESIAN_POINT ( 'NONE',  ( 18.59999999999999076, 7.120270961697594103, -37.15956304183931991 ) ) ;
#95763 = ORIENTED_EDGE ( 'NONE', *, *, #115932, .F. ) ;
#95764 = APPLICATION_CONTEXT ( 'automotive_design' ) ;
#95765 = EDGE_CURVE ( 'NONE', #136260, #97145, #74550, .T. ) ;
#95767 = EDGE_CURVE ( 'NONE', #232714, #13799, #137044, .T. ) ;
#95766 = AXIS2_PLACEMENT_3D ( 'NONE', #217351, #17877, #861 ) ;
#95768 = VERTEX_POINT ( 'NONE', #207187 ) ;
#95769 = CIRCLE ( 'NONE', #91705, 0.1000000000000028644 ) ;
#95770 = DIRECTION ( 'NONE',  ( 0.000000000000000000, 0.8814952561688428334, -0.4721928772777350125 ) ) ;
#95771 = ORIENTED_EDGE ( 'NONE', *, *, #147447, .T. ) ;
#95772 = ORIENTED_EDGE ( 'NONE', *, *, #214510, .F. ) ;
#95773 = DIRECTION ( 'NONE',  ( 0.000000000000000000, -0.4999999999999689138, -0.8660254037844565822 ) ) ;
#95774 = FACE_OUTER_BOUND ( 'NONE', #226102, .T. ) ;
#95775 = DIRECTION ( 'NONE',  ( -1.000000000000000000, 0.000000000000000000, -0.000000000000000000 ) ) ;
#95776 = DIRECTION ( 'NONE',  ( 0.000000000000000000, 0.4721928772777346239, 0.8814952561688430555 ) ) ;
#95777 = CARTESIAN_POINT ( 'NONE',  ( -16.87036670365548474, 51.72098459467785858, -231.8575261499355236 ) ) ;
#95778 = EDGE_CURVE ( 'NONE', #191015, #54157, #82833, .T. ) ;
#95779 =( BOUNDED_CURVE ( )  B_SPLINE_CURVE ( 3, ( #42008, #165810, #225732, #2838 ),
 .UNSPECIFIED., .F., .F. ) 
 B_SPLINE_CURVE_WITH_KNOTS ( ( 4, 4 ),
 ( 3.752122642744651682, 4.712388980384675463 ),
 .UNSPECIFIED. ) 
 CURVE ( )  GEOMETRIC_REPRESENTATION_ITEM ( )  RATIONAL_B_SPLINE_CURVE ( ( 1.000000000000000000, 0.9246222802177319622, 0.9246222802177319622, 1.000000000000000000 ) ) 
 REPRESENTATION_ITEM ( '' )  );
#95781 = CYLINDRICAL_SURFACE ( 'NONE', #25209, 12.87499999999999822 ) ;
#95780 = CARTESIAN_POINT ( 'NONE',  ( 23.24999999999999645, 3.900000000011155432, -100.5000000000000426 ) ) ;
#95782 = DIRECTION ( 'NONE',  ( 0.000000000000000000, 0.000000000000000000, 1.000000000000000000 ) ) ;
#95784 = ORIENTED_EDGE ( 'NONE', *, *, #6965, .T. ) ;
#95783 = CARTESIAN_POINT ( 'NONE',  ( -18.50000000000000000, 70.65875701002080689, -179.8297576910124178 ) ) ;
#95785 = CARTESIAN_POINT ( 'NONE',  ( 22.57856590037848576, 76.00412833007658264, -148.2731659471997148 ) ) ;
#95786 = DIRECTION ( 'NONE',  ( 0.000000000000000000, 0.7397360091702755991, -0.6728971962616832059 ) ) ;
#95787 = ORIENTED_EDGE ( 'NONE', *, *, #204280, .T. ) ;
#95788 = CARTESIAN_POINT ( 'NONE',  ( 21.06600267594171783, 8.775166069211060460, -146.2042627823747409 ) ) ;
#95789 = DIRECTION ( 'NONE',  ( 2.259780016855445309E-14, -0.9875055080513764905, 0.1575844902526679359 ) ) ;
#95790 = VERTEX_POINT ( 'NONE', #106775 ) ;
#95791 = CARTESIAN_POINT ( 'NONE',  ( -18.79999999999999716, 11.59510167572422112, -1.901609089591594470 ) ) ;
#95792 = DIRECTION ( 'NONE',  ( 1.000000000000000000, -0.000000000000000000, -0.000000000000000000 ) ) ;
#95793 = B_SPLINE_CURVE_WITH_KNOTS ( 'NONE', 3,
 ( #152624, #191754, #112207, #215134, #13098, #230867, #114754, #135578, #93895, #57320, #155195, #56027, #35247, #194315, #234700, #254238, #131742, #74380, #15681, #195595, #170927, #75645, #95187, #92599, #172208, #153932, #174775, #173498, #232145, #116052 ),
 .UNSPECIFIED., .F., .F.,
 ( 4, 2, 2, 2, 2, 2, 2, 2, 2, 2, 2, 2, 2, 2, 4 ),
 ( 0.000000000000000000, 0.0003422764154113348617, 0.0006845528308226697233, 0.001026829246234006428, 0.001369105661645343350, 0.002053658492468013290, 0.002738211323290683664, 0.003080487738702016465, 0.003422764154113348400, 0.003765040569524680768, 0.004107316984936013569, 0.004449593400347345504, 0.004791869815758678305, 0.005134146231170010240, 0.005476422646581343041 ),
 .UNSPECIFIED. ) ;
#95794 = FACE_OUTER_BOUND ( 'NONE', #152361, .T. ) ;
#95795 = ORIENTED_EDGE ( 'NONE', *, *, #154765, .T. ) ;
#95796 = ORIENTED_EDGE ( 'NONE', *, *, #33740, .F. ) ;
#95797 = DIRECTION ( 'NONE',  ( -1.000000000000000000, -2.952720810173289112E-16, 0.000000000000000000 ) ) ;
#95798 = EDGE_CURVE ( 'NONE', #173295, #1463, #92350, .T. ) ;
#95800 = CARTESIAN_POINT ( 'NONE',  ( -18.58744394320964943, -0.7665302784960944527, -242.4350121447238280 ) ) ;
#95799 = VECTOR ( 'NONE', #204506, 1000.000000000000000 ) ;
#95801 = DIRECTION ( 'NONE',  ( -0.000000000000000000, 0.9916376685811522096, -0.1290532225515392817 ) ) ;
#95802 = DIRECTION ( 'NONE',  ( 0.000000000000000000, -0.000000000000000000, -1.000000000000000000 ) ) ;
#95803 = ORIENTED_EDGE ( 'NONE', *, *, #126515, .T. ) ;
#95804 = CARTESIAN_POINT ( 'NONE',  ( 13.43443725621853879, 46.56801681390926007, -234.7608386620030387 ) ) ;
#95805 = CARTESIAN_POINT ( 'NONE',  ( 22.39999999999999858, 68.20922040163929978, -203.6231074845244109 ) ) ;
#95806 = EDGE_CURVE ( 'NONE', #29061, #26218, #99590, .T. ) ;
#95807 = CARTESIAN_POINT ( 'NONE',  ( 21.05000000000000071, 70.41157348381892689, -224.1287375179191201 ) ) ;
#95808 = LINE ( 'NONE', #562, #128368 ) ;
#95809 = AXIS2_PLACEMENT_3D ( 'NONE', #173234, #170672, #110640 ) ;
#95811 = FACE_OUTER_BOUND ( 'NONE', #23651, .T. ) ;
#95810 = CIRCLE ( 'NONE', #16747, 0.09999999999998898659 ) ;
#95813 = EDGE_LOOP ( 'NONE', ( #2992, #105060, #127861, #199701, #86499, #116264, #191353, #191942 ) ) ;
#95812 = FACE_OUTER_BOUND ( 'NONE', #168622, .T. ) ;
#95814 = CYLINDRICAL_SURFACE ( 'NONE', #239125, 0.09999999999998898659 ) ;
#95815 = CARTESIAN_POINT ( 'NONE',  ( -16.97683809663752186, 66.05000000001187743, -89.62074346632789457 ) ) ;
#95816 = FACE_OUTER_BOUND ( 'NONE', #76992, .T. ) ;
#95817 = VECTOR ( 'NONE', #211612, 1000.000000000000000 ) ;
#95818 = CARTESIAN_POINT ( 'NONE',  ( -22.57848426163147693, -0.004264329271961140103, -122.2499416931096619 ) ) ;
#95819 = DIRECTION ( 'NONE',  ( 0.000000000000000000, 0.000000000000000000, 1.000000000000000000 ) ) ;
#95821 = ORIENTED_EDGE ( 'NONE', *, *, #133045, .F. ) ;
#95820 = DIRECTION ( 'NONE',  ( -1.000000000000000000, 0.000000000000000000, 0.000000000000000000 ) ) ;
#95822 = CARTESIAN_POINT ( 'NONE',  ( -22.50000000000000000, 11.75000000001115552, -33.50000000000000000 ) ) ;
#95823 = AXIS2_PLACEMENT_3D ( 'NONE', #186269, #50573, #247517 ) ;
#95824 = CARTESIAN_POINT ( 'NONE',  ( 20.94999999999999929, 85.50000000001188027, -93.12913836187179584 ) ) ;
#95825 = DIRECTION ( 'NONE',  ( 0.000000000000000000, -1.000000000000000000, 0.000000000000000000 ) ) ;
#95826 = CONICAL_SURFACE ( 'NONE', #166806, 4.299999999999970512, 0.7853981633974466137 ) ;
#95827 = ORIENTED_EDGE ( 'NONE', *, *, #242514, .F. ) ;
#95828 = DIRECTION ( 'NONE',  ( 0.000000000000000000, 6.982962677686266711E-15, -1.000000000000000000 ) ) ;
#95829 = CARTESIAN_POINT ( 'NONE',  ( -21.65000000000000213, 18.70606281991846842, -231.7096448200342138 ) ) ;
#95830 = DIRECTION ( 'NONE',  ( -1.000000000000000000, 0.000000000000000000, 6.938893903907270030E-14 ) ) ;
#95831 = FACE_OUTER_BOUND ( 'NONE', #78495, .T. ) ;
#95832 = CARTESIAN_POINT ( 'NONE',  ( -22.59999999999999787, 11.64957080755595520, -167.3999999999999773 ) ) ;
#95834 = CARTESIAN_POINT ( 'NONE',  ( -22.39999999999999858, -0.02128009951114784304, -200.9022904438449757 ) ) ;
#95833 = AXIS2_PLACEMENT_3D ( 'NONE', #160319, #101562, #39081 ) ;
#95835 = AXIS2_PLACEMENT_3D ( 'NONE', #95263, #166177, #35333 ) ;
#95837 = ORIENTED_EDGE ( 'NONE', *, *, #123579, .T. ) ;
#95836 = AXIS2_PLACEMENT_3D ( 'NONE', #157765, #36509, #57302 ) ;
#95838 = ORIENTED_EDGE ( 'NONE', *, *, #7888, .F. ) ;
#95839 = CIRCLE ( 'NONE', #241607, 0.09999999999999971412 ) ;
#95840 = AXIS2_PLACEMENT_3D ( 'NONE', #195875, #120208, #81019 ) ;
#95841 = EDGE_CURVE ( 'NONE', #155156, #38568, #70263, .T. ) ;
#95842 = CARTESIAN_POINT ( 'NONE',  ( -18.35235881385853318, 64.52658099229942934, -160.7731074845244450 ) ) ;
#95844 = EDGE_CURVE ( 'NONE', #95048, #132728, #12845, .T. ) ;
#95843 = CARTESIAN_POINT ( 'NONE',  ( -18.59999999999999787, 0.6656436123793491033, -212.6810495496487476 ) ) ;
#95845 = CARTESIAN_POINT ( 'NONE',  ( 18.49999999999999645, -0.6210911348947316668, -242.4105802476707936 ) ) ;
#95846 = FACE_OUTER_BOUND ( 'NONE', #172979, .T. ) ;
#95847 = EDGE_CURVE ( 'NONE', #28569, #235019, #247582, .T. ) ;
#95848 = EDGE_CURVE ( 'NONE', #19933, #11153, #127642, .T. ) ;
#95849 = PLANE ( 'NONE',  #209193 ) ;
#95850 = CYLINDRICAL_SURFACE ( 'NONE', #42530, 0.09999999999999939493 ) ;
#95851 = VECTOR ( 'NONE', #73909, 1000.000000000000000 ) ;
#95852 = ADVANCED_FACE ( 'NONE', ( #128928 ), #70448, .T. ) ;
#95853 = DIRECTION ( 'NONE',  ( -1.000000000000000000, 0.000000000000000000, 0.000000000000000000 ) ) ;
#95854 = LINE ( 'NONE', #175438, #136028 ) ;
#95855 = ADVANCED_FACE ( 'NONE', ( #147195 ), #226722, .T. ) ;
#95857 = EDGE_CURVE ( 'NONE', #189424, #72122, #28766, .T. ) ;
#95856 = ADVANCED_FACE ( 'NONE', ( #75392 ), #173230, .F. ) ;
#95858 = ORIENTED_EDGE ( 'NONE', *, *, #168853, .F. ) ;
#95859 = DIRECTION ( 'NONE',  ( 0.000000000000000000, 0.8814952561688428334, -0.4721928772777349015 ) ) ;
#95860 = ORIENTED_EDGE ( 'NONE', *, *, #162181, .T. ) ;
#95861 = ORIENTED_EDGE ( 'NONE', *, *, #152964, .F. ) ;
#95862 = CARTESIAN_POINT ( 'NONE',  ( 20.85000000000000142, 7.576017155224048061, -241.7224044826512284 ) ) ;
#95863 = CARTESIAN_POINT ( 'NONE',  ( 21.87500000000000355, 9.750000000011153745, -179.8499999999999943 ) ) ;
#95864 = DIRECTION ( 'NONE',  ( 0.000000000000000000, 1.000000000000000000, 0.000000000000000000 ) ) ;
#95867 = ADVANCED_FACE ( 'NONE', ( #113203 ), #221515, .F. ) ;
#95866 = ORIENTED_EDGE ( 'NONE', *, *, #239231, .T. ) ;
#95865 = LINE ( 'NONE', #124132, #70175 ) ;
#95868 = DIRECTION ( 'NONE',  ( 0.000000000000000000, 0.9770955615653316162, 0.2128009952263597848 ) ) ;
#95869 = FACE_OUTER_BOUND ( 'NONE', #722, .T. ) ;
#95870 = B_SPLINE_CURVE_WITH_KNOTS ( 'NONE', 3,
 ( #239968, #195724, #75759, #179997, #41784, #200836, #121335 ),
 .UNSPECIFIED., .F., .F.,
 ( 4, 3, 4 ),
 ( 0.000000000000000000, 3.357501770814687536E-05, 5.199112466349470742E-05 ),
 .UNSPECIFIED. ) ;
#95871 = CARTESIAN_POINT ( 'NONE',  ( -21.37071067811865532, 67.92928932189394686, -191.2731074845244166 ) ) ;
#95873 = ORIENTED_EDGE ( 'NONE', *, *, #157746, .F. ) ;
#95872 = AXIS2_PLACEMENT_3D ( 'NONE', #102038, #220729, #180323 ) ;
#95874 = DIRECTION ( 'NONE',  ( 1.000000000000000000, 2.952720810173289112E-16, -0.000000000000000000 ) ) ;
#95875 = EDGE_CURVE ( 'NONE', #163200, #56536, #24655, .T. ) ;
#95876 = DIRECTION ( 'NONE',  ( 0.000000000000000000, -1.000000000000000000, 0.000000000000000000 ) ) ;
#95877 = AXIS2_PLACEMENT_3D ( 'NONE', #195150, #131292, #251226 ) ;
#95878 = LINE ( 'NONE', #73792, #243984 ) ;
#95879 = DIRECTION ( 'NONE',  ( 0.000000000000000000, 0.000000000000000000, 1.000000000000000000 ) ) ;
#95880 = EDGE_CURVE ( 'NONE', #129556, #241225, #232925, .T. ) ;
#95881 = EDGE_CURVE ( 'NONE', #80895, #46326, #112124, .T. ) ;
#95882 = AXIS2_PLACEMENT_3D ( 'NONE', #208412, #230531, #171871 ) ;
#95883 = ORIENTED_EDGE ( 'NONE', *, *, #240182, .T. ) ;
#95884 =( BOUNDED_SURFACE ( )  B_SPLINE_SURFACE ( 3, 2, ( 
 ( #30044, #56911, #169573 ),
 ( #136460, #70466, #37405 ),
 ( #149988, #17805, #91282 ),
 ( #196450, #97319, #246490 ) ),
 .UNSPECIFIED., .F., .F., .F. ) 
 B_SPLINE_SURFACE_WITH_KNOTS ( ( 4, 4 ),
 ( 3, 3 ),
 ( 3.658908243880847788, 4.712388980384689674 ),
 ( 0.000000000000000000, 1.000000000000000000 ),
 .UNSPECIFIED. ) 
 GEOMETRIC_REPRESENTATION_ITEM ( )  RATIONAL_B_SPLINE_SURFACE ( (
 ( 1.000000000000000000, 0.8984936768950610997, 1.000000000000000000),
 ( 1.000000000000000000, 0.8646876308615627504, 1.000000000000000000),
 ( 1.000000000000000000, 0.7953136715913320387, 1.000000000000000000),
 ( 1.000000000000000000, 0.7071067811865475727, 1.000000000000000000) ) ) 
 REPRESENTATION_ITEM ( '' )  SURFACE ( )  );
#95885 = LINE ( 'NONE', #622, #118611 ) ;
#95887 = EDGE_CURVE ( 'NONE', #12940, #99065, #74725, .T. ) ;
#95886 = CARTESIAN_POINT ( 'NONE',  ( -23.15000000000000213, 64.35000000001180354, -81.67310748452439384 ) ) ;
#95888 = ORIENTED_EDGE ( 'NONE', *, *, #199134, .F. ) ;
#95889 = CARTESIAN_POINT ( 'NONE',  ( -23.25000000000000000, 2.000000000011154189, -53.77537807723790309 ) ) ;
#95890 = DIRECTION ( 'NONE',  ( -0.000000000000000000, -6.982962677686266711E-15, 1.000000000000000000 ) ) ;
#95891 = FACE_OUTER_BOUND ( 'NONE', #129627, .T. ) ;
#95892 = ADVANCED_FACE ( 'NONE', ( #196581 ), #94911, .T. ) ;
#95893 = CIRCLE ( 'NONE', #162570, 0.09999999999999939493 ) ;
#95894 = VECTOR ( 'NONE', #17765, 1000.000000000000000 ) ;
#95895 = ORIENTED_EDGE ( 'NONE', *, *, #217400, .T. ) ;
#95896 = CARTESIAN_POINT ( 'NONE',  ( 21.05000000000000071, 2.739812813550880577, -213.5801053551551547 ) ) ;
#95897 = EDGE_CURVE ( 'NONE', #226140, #222619, #97458, .T. ) ;
#95898 = ORIENTED_EDGE ( 'NONE', *, *, #135117, .T. ) ;
#95899 = AXIS2_PLACEMENT_3D ( 'NONE', #86422, #203829, #160877 ) ;
#95900 = AXIS2_PLACEMENT_3D ( 'NONE', #182287, #21928, #181006 ) ;
#95901 = ORIENTED_EDGE ( 'NONE', *, *, #94324, .T. ) ;
#95902 = CARTESIAN_POINT ( 'NONE',  ( 18.59999999999999432, 74.73821383144657204, -61.43660852097884373 ) ) ;
#95903 = EDGE_CURVE ( 'NONE', #9700, #18932, #57907, .T. ) ;
#95904 = CARTESIAN_POINT ( 'NONE',  ( 20.94999999999999929, -11.48912529307605546, -30.50000000000000000 ) ) ;
#95906 = ORIENTED_EDGE ( 'NONE', *, *, #9721, .F. ) ;
#95905 = CARTESIAN_POINT ( 'NONE',  ( -22.50000000000000000, 1.148907358139439339E-11, -201.0000000000015064 ) ) ;
#95907 = DIRECTION ( 'NONE',  ( 0.000000000000000000, 0.000000000000000000, -1.000000000000000000 ) ) ;
#95908 = DIRECTION ( 'NONE',  ( 1.000000000000000000, 0.000000000000000000, -0.000000000000000000 ) ) ;
#95909 = DIRECTION ( 'NONE',  ( 0.000000000000000000, 0.9875102702516471709, 0.1575546449569757979 ) ) ;
#95910 = CARTESIAN_POINT ( 'NONE',  ( -18.59999999999999787, 11.64999999999999680, -7.014805770654001016 ) ) ;
#95911 = CARTESIAN_POINT ( 'NONE',  ( -18.59999999999999787, 77.16270174994961906, -61.42310748452431568 ) ) ;
#95913 = VERTEX_POINT ( 'NONE', #36262 ) ;
#95912 = DIRECTION ( 'NONE',  ( -0.000000000000000000, 1.000000000000000000, -0.000000000000000000 ) ) ;
#95915 = VERTEX_POINT ( 'NONE', #96191 ) ;
#95914 = DIRECTION ( 'NONE',  ( 0.000000000000000000, 0.9126074666063844765, 0.4088369013363113980 ) ) ;
#95918 = CARTESIAN_POINT ( 'NONE',  ( 20.86777300164945004, 10.33200063080771969, -72.59316749566428939 ) ) ;
#95917 = CARTESIAN_POINT ( 'NONE',  ( -18.59999999999999787, 76.00000000001126921, -203.5231074845248997 ) ) ;
#95916 = AXIS2_PLACEMENT_3D ( 'NONE', #47938, #126193, #167933 ) ;
#95919 = AXIS2_PLACEMENT_3D ( 'NONE', #6479, #22222, #80870 ) ;
#95921 = VERTEX_POINT ( 'NONE', #174524 ) ;
#95920 = CARTESIAN_POINT ( 'NONE',  ( 21.05000000000000071, 8.926614585098253229, -75.47168301922316402 ) ) ;
#95922 = ORIENTED_EDGE ( 'NONE', *, *, #220141, .F. ) ;
#95923 = CARTESIAN_POINT ( 'NONE',  ( 23.14999999999999858, 71.18691588786246882, -114.9646252410481537 ) ) ;
#95924 = DIRECTION ( 'NONE',  ( 0.000000000000000000, -7.086529944415886769E-15, 1.000000000000000000 ) ) ;
#95925 = DIRECTION ( 'NONE',  ( 1.000000000000000000, 0.000000000000000000, 0.000000000000000000 ) ) ;
#95926 = DIRECTION ( 'NONE',  ( 1.000000000000000000, 0.000000000000000000, 0.000000000000000000 ) ) ;
#95927 = CARTESIAN_POINT ( 'NONE',  ( -18.50016250449483479, 67.49429988484524756, -195.5441618131978316 ) ) ;
#95928 = DIRECTION ( 'NONE',  ( 0.000000000000000000, -1.000000000000000000, -0.000000000000000000 ) ) ;
#95929 = CARTESIAN_POINT ( 'NONE',  ( -16.86133551771148475, 66.05000000001201954, -115.7217640499777360 ) ) ;
#95930 = AXIS2_PLACEMENT_3D ( 'NONE', #96535, #74472, #34060 ) ;
#95932 = ORIENTED_EDGE ( 'NONE', *, *, #188464, .F. ) ;
#95931 = EDGE_CURVE ( 'NONE', #166220, #57378, #203686, .T. ) ;
#95933 = ORIENTED_EDGE ( 'NONE', *, *, #10347, .T. ) ;
#95934 = AXIS2_PLACEMENT_3D ( 'NONE', #189128, #224387, #164441 ) ;
#95935 = CARTESIAN_POINT ( 'NONE',  ( 21.05000000000000071, 30.73075574124490572, -252.3164853687435709 ) ) ;
#95936 = AXIS2_PLACEMENT_3D ( 'NONE', #29456, #248468, #69849 ) ;
#95937 = ADVANCED_FACE ( 'NONE', ( #54508 ), #197863, .F. ) ;
#95938 = ORIENTED_EDGE ( 'NONE', *, *, #20834, .T. ) ;
#95939 = LINE ( 'NONE', #234169, #151238 ) ;
#95940 = CARTESIAN_POINT ( 'NONE',  ( 18.58222699835054570, 68.11153784908182729, -224.1393723182492579 ) ) ;
#95941 = DIRECTION ( 'NONE',  ( -1.000000000000000000, 0.000000000000000000, 0.000000000000000000 ) ) ;
#95942 = CIRCLE ( 'NONE', #87572, 0.1000000000000028644 ) ;
#95943 = DIRECTION ( 'NONE',  ( 1.000000000000000000, -0.000000000000000000, -0.000000000000000000 ) ) ;
#95944 = EDGE_CURVE ( 'NONE', #129705, #117379, #253547, .T. ) ;
#95945 = ORIENTED_EDGE ( 'NONE', *, *, #188941, .T. ) ;
#95947 = ADVANCED_FACE ( 'NONE', ( #219998 ), #183454, .F. ) ;
#95946 = CARTESIAN_POINT ( 'NONE',  ( 21.14999999999999858, 6.650000000011155876, -79.35000000000005116 ) ) ;
#95948 = VERTEX_POINT ( 'NONE', #102587 ) ;
#95949 = DIRECTION ( 'NONE',  ( 0.000000000000000000, -0.9893560106964500722, 0.1455152366551550613 ) ) ;
#95950 = ORIENTED_EDGE ( 'NONE', *, *, #195585, .T. ) ;
#95951 = EDGE_CURVE ( 'NONE', #186480, #156438, #6074, .T. ) ;
#95952 = AXIS2_PLACEMENT_3D ( 'NONE', #81063, #40715, #160653 ) ;
#95953 = FACE_OUTER_BOUND ( 'NONE', #170843, .T. ) ;
#95954 = CARTESIAN_POINT ( 'NONE',  ( 18.39999999999998082, 64.52683809664941350, -93.77310748452438816 ) ) ;
#95955 = CARTESIAN_POINT ( 'NONE',  ( 20.94999999999999929, 65.27628289530427708, -81.77310748452438816 ) ) ;
#95956 = EDGE_LOOP ( 'NONE', ( #71846, #96029, #134370 ) ) ;
#95957 = CARTESIAN_POINT ( 'NONE',  ( -23.25000000000000355, 9.949999999999983302, -9.250000000000001776 ) ) ;
#95959 = EDGE_LOOP ( 'NONE', ( #84514, #42572, #118102, #232402 ) ) ;
#95958 = CARTESIAN_POINT ( 'NONE',  ( 20.85000000000000142, 7.476371755685457643, -241.7308184205399471 ) ) ;
#95960 = CARTESIAN_POINT ( 'NONE',  ( -18.39999999999999858, -9.499999999988849808, -73.99928567783889832 ) ) ;
#95961 = VERTEX_POINT ( 'NONE', #123471 ) ;
#95962 = EDGE_CURVE ( 'NONE', #201469, #43558, #218698, .T. ) ;
#95963 = ORIENTED_EDGE ( 'NONE', *, *, #87734, .T. ) ;
#95964 = DIRECTION ( 'NONE',  ( 0.7071067811865475727, -0.7071067811865475727, 0.000000000000000000 ) ) ;
#95965 = ORIENTED_EDGE ( 'NONE', *, *, #57099, .F. ) ;
#95966 = CARTESIAN_POINT ( 'NONE',  ( -20.85000000000000142, -1.835859311443637010, -45.00443916879852679 ) ) ;
#95967 = FACE_OUTER_BOUND ( 'NONE', #93426, .T. ) ;
#95968 = FACE_OUTER_BOUND ( 'NONE', #25469, .T. ) ;
#95969 = DIRECTION ( 'NONE',  ( 1.000000000000000000, 0.000000000000000000, 0.000000000000000000 ) ) ;
#95970 = CARTESIAN_POINT ( 'NONE',  ( -21.08376601933334271, 0.06377601094103593771, -60.65805272872431431 ) ) ;
#95971 = ORIENTED_EDGE ( 'NONE', *, *, #93326, .T. ) ;
#95972 = DIRECTION ( 'NONE',  ( -0.000000000000000000, 0.000000000000000000, -1.000000000000000000 ) ) ;
#95973 = CARTESIAN_POINT ( 'NONE',  ( 18.39999999999999858, 86.89640087696871262, -199.6396878666313341 ) ) ;
#95974 = CARTESIAN_POINT ( 'NONE',  ( -20.99551997958390714, 11.75000000001129052, -160.6516591376896201 ) ) ;
#95975 = AXIS2_PLACEMENT_3D ( 'NONE', #215561, #59023, #257210 ) ;
#95976 = ORIENTED_EDGE ( 'NONE', *, *, #71892, .T. ) ;
#95977 = EDGE_CURVE ( 'NONE', #106612, #210954, #132965, .T. ) ;
#95978 = DIRECTION ( 'NONE',  ( 0.000000000000000000, -0.2617529984165045120, -0.9651348961777153068 ) ) ;
#95979 = ORIENTED_EDGE ( 'NONE', *, *, #225434, .F. ) ;
#95980 = DIRECTION ( 'NONE',  ( 1.000000000000000000, 0.000000000000000000, 0.000000000000000000 ) ) ;
#95981 = VERTEX_POINT ( 'NONE', #179612 ) ;
#95982 = DIRECTION ( 'NONE',  ( 0.000000000000000000, 0.000000000000000000, -1.000000000000000000 ) ) ;
#95983 = CARTESIAN_POINT ( 'NONE',  ( -20.54999999999999716, 0.000000000000000000, -33.50000000000000000 ) ) ;
#95984 = CIRCLE ( 'NONE', #145878, 0.09999999999998898659 ) ;
#95986 = ORIENTED_EDGE ( 'NONE', *, *, #148288, .F. ) ;
#95985 = CARTESIAN_POINT ( 'NONE',  ( -20.94999999999999929, 76.00000000001192291, -100.1231074845243256 ) ) ;
#95987 = CARTESIAN_POINT ( 'NONE',  ( -18.40000000000000213, 8.812905490826906885, -245.4119551738195071 ) ) ;
#95988 = VERTEX_POINT ( 'NONE', #161333 ) ;
#95989 = EDGE_CURVE ( 'NONE', #80321, #176854, #53837, .T. ) ;
#95990 = CARTESIAN_POINT ( 'NONE',  ( -21.04999999999999716, 36.17635217701701578, -235.9630383263116187 ) ) ;
#95991 = CARTESIAN_POINT ( 'NONE',  ( -18.50000000000000000, 9.150000000011157653, -188.6499999999999488 ) ) ;
#95992 = ADVANCED_FACE ( 'NONE', ( #141740 ), #120502, .T. ) ;
#95993 = VERTEX_POINT ( 'NONE', #45213 ) ;
#95994 = CARTESIAN_POINT ( 'NONE',  ( -21.00023020733502577, 1.115539681028482333E-11, -127.6091307547316518 ) ) ;
#95995 = CARTESIAN_POINT ( 'NONE',  ( -22.60000000000094289, -3.180729737798059009, -228.0957332317256885 ) ) ;
#95996 = EDGE_LOOP ( 'NONE', ( #194029, #105298, #55335 ) ) ;
#95997 = CARTESIAN_POINT ( 'NONE',  ( -16.89268316805466341, 66.04827818676987761, -123.8788599630699281 ) ) ;
#95998 = CIRCLE ( 'NONE', #16932, 0.1000000000000028644 ) ;
#95999 = VECTOR ( 'NONE', #46512, 1000.000000000000000 ) ;
#96000 = ORIENTED_EDGE ( 'NONE', *, *, #111258, .F. ) ;
#96001 = ADVANCED_FACE ( 'NONE', ( #165165 ), #2218, .T. ) ;
#96002 = FACE_OUTER_BOUND ( 'NONE', #255714, .T. ) ;
#96003 = CARTESIAN_POINT ( 'NONE',  ( -18.46907102845853998, -9.473727364752948077, -73.67603473873651865 ) ) ;
#96004 = TOROIDAL_SURFACE ( 'NONE', #158591, 4.041421356237312246, 0.1000000000000000056 ) ;
#96005 = ADVANCED_FACE ( 'NONE', ( #244684 ), #62218, .T. ) ;
#96006 = VECTOR ( 'NONE', #246870, 1000.000000000000000 ) ;
#96007 = ADVANCED_FACE ( 'NONE', ( #199159 ), #220443, .T. ) ;
#96008 = CIRCLE ( 'NONE', #25327, 11.80000000000000426 ) ;
#96010 = ORIENTED_EDGE ( 'NONE', *, *, #216186, .F. ) ;
#96009 = CARTESIAN_POINT ( 'NONE',  ( 20.94999999999999929, 1.115649653272650466E-11, -96.50000000000004263 ) ) ;
#96011 = CARTESIAN_POINT ( 'NONE',  ( 21.30000000000002558, 4.959819536546777642E-16, 4.049999999999998934 ) ) ;
#96012 = CARTESIAN_POINT ( 'NONE',  ( -23.25000000000000355, 64.25000000001182343, -82.17310748452439384 ) ) ;
#96013 = CARTESIAN_POINT ( 'NONE',  ( -16.93415306273742260, 9.995622260012515525, -20.91005694236041634 ) ) ;
#96014 = ADVANCED_FACE ( 'NONE', ( #144283 ), #62038, .T. ) ;
#96016 = CARTESIAN_POINT ( 'NONE',  ( -0.8999999999999993561, -8.250000000000005329, 28.60000000000000142 ) ) ;
#96015 = DIRECTION ( 'NONE',  ( 0.000000000000000000, 0.8700118002898393765, -0.4930308989875104575 ) ) ;
#96017 = DIRECTION ( 'NONE',  ( 0.000000000000000000, -0.8740096314914906905, 0.4859085964048265316 ) ) ;
#96018 = FACE_OUTER_BOUND ( 'NONE', #5659, .T. ) ;
#96019 = CARTESIAN_POINT ( 'NONE',  ( 18.39999999999999858, -9.499999999988842703, -40.53206939669966857 ) ) ;
#96020 = AXIS2_PLACEMENT_3D ( 'NONE', #34935, #114438, #50590 ) ;
#96021 = CARTESIAN_POINT ( 'NONE',  ( -22.16821283564876666, 68.44102665923136897, -136.5231074845243313 ) ) ;
#96022 = AXIS2_PLACEMENT_3D ( 'NONE', #192081, #241547, #25098 ) ;
#96023 = VECTOR ( 'NONE', #102517, 1000.000000000000000 ) ;
#96024 = ORIENTED_EDGE ( 'NONE', *, *, #12127, .F. ) ;
#96026 = ORIENTED_EDGE ( 'NONE', *, *, #8183, .F. ) ;
#96025 = CIRCLE ( 'NONE', #154358, 0.1000000000000000888 ) ;
#96027 = CARTESIAN_POINT ( 'NONE',  ( -21.05000000000000071, -11.64999999998884306, -197.8999999999999773 ) ) ;
#96029 = ORIENTED_EDGE ( 'NONE', *, *, #149124, .T. ) ;
#96028 = DIRECTION ( 'NONE',  ( 0.000000000000000000, -0.8814952561685467369, 0.4721928772782874595 ) ) ;
#96030 = ORIENTED_EDGE ( 'NONE', *, *, #211457, .F. ) ;
#96031 = EDGE_CURVE ( 'NONE', #80057, #248144, #208456, .T. ) ;
#96032 = CARTESIAN_POINT ( 'NONE',  ( -23.25000000000000000, 2.600000000011156054, -180.7246219227620543 ) ) ;
#96033 = ORIENTED_EDGE ( 'NONE', *, *, #4055, .F. ) ;
#96034 = CARTESIAN_POINT ( 'NONE',  ( 22.39999999999999503, 76.00000000001200817, -110.7731074845243171 ) ) ;
#96035 = AXIS2_PLACEMENT_3D ( 'NONE', #37042, #179127, #237784 ) ;
#96036 = ORIENTED_EDGE ( 'NONE', *, *, #5419, .T. ) ;
#96037 = SURFACE_STYLE_FILL_AREA ( #217258 ) ;
#96038 = DIRECTION ( 'NONE',  ( 1.000000000000000000, -0.000000000000000000, 0.000000000000000000 ) ) ;
#96040 = ORIENTED_EDGE ( 'NONE', *, *, #242088, .T. ) ;
#96039 = ORIENTED_EDGE ( 'NONE', *, *, #209227, .T. ) ;
#96041 = EDGE_LOOP ( 'NONE', ( #67495, #113979, #71500, #23014 ) ) ;
#96042 = EDGE_LOOP ( 'NONE', ( #77025, #151784, #232653, #73293 ) ) ;
#96043 = VERTEX_POINT ( 'NONE', #60916 ) ;
#96044 = DIRECTION ( 'NONE',  ( -1.000000000000000000, 0.000000000000000000, -0.000000000000000000 ) ) ;
#96046 = ORIENTED_EDGE ( 'NONE', *, *, #173663, .F. ) ;
#96045 = LINE ( 'NONE', #111785, #124995 ) ;
#96047 = CARTESIAN_POINT ( 'NONE',  ( -22.39999999999999858, 33.47376623175147614, -242.4412390690852703 ) ) ;
#96048 = CARTESIAN_POINT ( 'NONE',  ( 21.14999999999999503, -2.576749817950531707, -189.6385361693310756 ) ) ;
#96050 = ORIENTED_EDGE ( 'NONE', *, *, #30530, .F. ) ;
#96049 = CARTESIAN_POINT ( 'NONE',  ( 20.95052659398289308, 10.47982436779105875, -141.5752387558655983 ) ) ;
#96051 = FACE_OUTER_BOUND ( 'NONE', #51258, .T. ) ;
#96052 = ORIENTED_EDGE ( 'NONE', *, *, #133360, .T. ) ;
#96053 = CARTESIAN_POINT ( 'NONE',  ( -20.64999999999999858, 6.878457983866232972, -212.1414458560986986 ) ) ;
#96054 = AXIS2_PLACEMENT_3D ( 'NONE', #127756, #6504, #7810 ) ;
#96056 = ORIENTED_EDGE ( 'NONE', *, *, #15655, .T. ) ;
#96055 = CARTESIAN_POINT ( 'NONE',  ( 21.14999999999999858, 1.363275264940682741, -230.6442496871288483 ) ) ;
#96057 = FACE_OUTER_BOUND ( 'NONE', #46170, .T. ) ;
#96058 = CARTESIAN_POINT ( 'NONE',  ( -16.92570016628984320, 9.958788957751014692, -113.1206506700390406 ) ) ;
#96059 = CARTESIAN_POINT ( 'NONE',  ( 19.81427058490564264, 11.66856398039202070, -91.75000000000005684 ) ) ;
#96060 = ORIENTED_EDGE ( 'NONE', *, *, #182661, .T. ) ;
#96062 = CARTESIAN_POINT ( 'NONE',  ( 20.95000000000005258, 66.15000000001120384, -4.523107484524794053 ) ) ;
#96061 = CARTESIAN_POINT ( 'NONE',  ( -16.80621392010913340, 9.942202577518862938, -46.18959196541719336 ) ) ;
#96063 = CARTESIAN_POINT ( 'NONE',  ( 18.33683296300426235, 85.51114997114527227, -163.1174000718142452 ) ) ;
#96064 = CARTESIAN_POINT ( 'NONE',  ( 17.74533788810830970, 15.50479229951815263, -221.3531188506081548 ) ) ;
#96065 = ORIENTED_EDGE ( 'NONE', *, *, #77036, .T. ) ;
#96066 = ORIENTED_EDGE ( 'NONE', *, *, #43936, .T. ) ;
#96068 = AXIS2_PLACEMENT_3D ( 'NONE', #87104, #106658, #105359 ) ;
#96067 = CARTESIAN_POINT ( 'NONE',  ( 21.05000000000000071, 8.776282895292473185, -8.558628995140949769 ) ) ;
#96069 = CARTESIAN_POINT ( 'NONE',  ( 20.94999999999999929, -1.135018845899022466, -108.2169768834323662 ) ) ;
#96070 = ORIENTED_EDGE ( 'NONE', *, *, #124211, .T. ) ;
#96071 = DIRECTION ( 'NONE',  ( 0.000000000000000000, -0.8636236514130390951, 0.5041370733441546959 ) ) ;
#96072 = ORIENTED_EDGE ( 'NONE', *, *, #119989, .F. ) ;
#96073 = CARTESIAN_POINT ( 'NONE',  ( 20.84999999999999432, -1.164121893230052995, -208.9148480855715775 ) ) ;
#96074 = ADVANCED_FACE ( 'NONE', ( #140454 ), #242123, .F. ) ;
#96075 = DIRECTION ( 'NONE',  ( 1.000000000000000000, -0.000000000000000000, 0.000000000000000000 ) ) ;
#96076 = TOROIDAL_SURFACE ( 'NONE', #154396, 0.2000000000000000111, 0.1000000000000000056 ) ;
#96077 = EDGE_CURVE ( 'NONE', #109277, #227367, #143007, .T. ) ;
#96078 = EDGE_CURVE ( 'NONE', #40625, #116437, #49562, .T. ) ;
#96079 = ORIENTED_EDGE ( 'NONE', *, *, #148192, .T. ) ;
#96080 = CARTESIAN_POINT ( 'NONE',  ( -23.15000000000000213, 4.350000000011156054, -179.6499999999999773 ) ) ;
#96081 = TOROIDAL_SURFACE ( 'NONE', #250040, 11.65000000000000036, 0.1000000000000000056 ) ;
#96083 = ORIENTED_EDGE ( 'NONE', *, *, #254215, .F. ) ;
#96082 = AXIS2_PLACEMENT_3D ( 'NONE', #178226, #40007, #179505 ) ;
#96084 = VERTEX_POINT ( 'NONE', #26967 ) ;
#96085 = ORIENTED_EDGE ( 'NONE', *, *, #228913, .T. ) ;
#96086 = VECTOR ( 'NONE', #176889, 1000.000000000000000 ) ;
#96087 = DIRECTION ( 'NONE',  ( 1.000000000000000000, 0.000000000000000000, 0.000000000000000000 ) ) ;
#96088 = DIRECTION ( 'NONE',  ( 0.000000000000000000, -0.9908441862701596881, 0.1350103645451899148 ) ) ;
#96089 = LINE ( 'NONE', #158683, #202959 ) ;
#96090 = CARTESIAN_POINT ( 'NONE',  ( 13.22461703343585526, 66.56333706821293106, -118.2000707522294647 ) ) ;
#96091 = EDGE_CURVE ( 'NONE', #4416, #141605, #170350, .T. ) ;
#96093 = CARTESIAN_POINT ( 'NONE',  ( 18.59999999999998366, 67.23127455305835554, -235.8551265064784559 ) ) ;
#96092 = CARTESIAN_POINT ( 'NONE',  ( 23.14999999999999858, 71.22429906543206357, -47.87187558857031888 ) ) ;
#96095 = EDGE_LOOP ( 'NONE', ( #46191, #150879, #64447, #175491, #162470 ) ) ;
#96094 = CARTESIAN_POINT ( 'NONE',  ( -18.50000000000000000, 7.021664781911246322, -70.83356540189728889 ) ) ;
#96096 = LINE ( 'NONE', #255131, #62475 ) ;
#96097 = ORIENTED_EDGE ( 'NONE', *, *, #220287, .F. ) ;
#96098 = CARTESIAN_POINT ( 'NONE',  ( -15.75000000000000355, 9.350000000011140955, -150.7500000000000284 ) ) ;
#96099 = EDGE_LOOP ( 'NONE', ( #41877, #22102, #82681, #26266 ) ) ;
#96100 = ORIENTED_EDGE ( 'NONE', *, *, #62140, .F. ) ;
#96101 = CARTESIAN_POINT ( 'NONE',  ( -16.93589915522259304, 65.99137474131565284, -48.58254738256407990 ) ) ;
#96102 = CARTESIAN_POINT ( 'NONE',  ( -21.04999999999999361, 6.300179817925542380, -133.9485171181182466 ) ) ;
#96103 = CARTESIAN_POINT ( 'NONE',  ( -22.39999999999999858, 33.38250548509083160, -242.4821227592188961 ) ) ;
#96104 = VERTEX_POINT ( 'NONE', #30816 ) ;
#96105 = CARTESIAN_POINT ( 'NONE',  ( -15.75000000000000355, 9.350000000011140955, -117.2500000000000284 ) ) ;
#96106 = AXIS2_PLACEMENT_3D ( 'NONE', #21895, #161420, #183539 ) ;
#96107 = CARTESIAN_POINT ( 'NONE',  ( 20.94788355080264353, 18.36312997293286031, -236.9042258689303821 ) ) ;
#96108 = VERTEX_POINT ( 'NONE', #131164 ) ;
#96109 = ORIENTED_EDGE ( 'NONE', *, *, #167386, .T. ) ;
#96110 = DIRECTION ( 'NONE',  ( 0.000000000000000000, 0.4930308989875230585, 0.8700118002898322711 ) ) ;
#96112 = EDGE_LOOP ( 'NONE', ( #7135, #67828, #188950, #37122 ) ) ;
#96111 = EDGE_CURVE ( 'NONE', #136679, #166383, #51667, .T. ) ;
#96113 = DIRECTION ( 'NONE',  ( 0.000000000000000000, 0.8814952561688476074, -0.4721928772777262417 ) ) ;
#96114 = CARTESIAN_POINT ( 'NONE',  ( -18.50000000000000000, 68.97833521811179480, -99.38954208262707368 ) ) ;
#96115 = ORIENTED_EDGE ( 'NONE', *, *, #223309, .T. ) ;
#96116 = EDGE_CURVE ( 'NONE', #59470, #93820, #8241, .T. ) ;
#96117 = CARTESIAN_POINT ( 'NONE',  ( -23.25000000000000000, 4.360421613930902218, -245.4659189663672691 ) ) ;
#96118 = CARTESIAN_POINT ( 'NONE',  ( -21.04999999999999361, 6.349973371233773811, -199.7193876399858254 ) ) ;
#96119 = DIRECTION ( 'NONE',  ( 0.000000000000000000, 0.000000000000000000, -1.000000000000000000 ) ) ;
#96120 = ORIENTED_EDGE ( 'NONE', *, *, #238319, .T. ) ;
#96121 = CARTESIAN_POINT ( 'NONE',  ( -18.40000000000000213, 70.35000000001159037, -56.87310748452436115 ) ) ;
#96122 = VECTOR ( 'NONE', #126041, 1000.000000000000000 ) ;
#96123 = CIRCLE ( 'NONE', #104481, 0.1999999999999987899 ) ;
#96124 = DIRECTION ( 'NONE',  ( 1.000000000000000000, 0.000000000000000000, 0.000000000000000000 ) ) ;
#96125 = ADVANCED_FACE ( 'NONE', ( #107751 ), #166475, .F. ) ;
#96126 = AXIS2_PLACEMENT_3D ( 'NONE', #111883, #170617, #124068 ) ;
#96127 = DIRECTION ( 'NONE',  ( 0.000000000000000000, -7.147358527629766941E-15, 1.000000000000000000 ) ) ;
#96128 = ORIENTED_EDGE ( 'NONE', *, *, #131526, .T. ) ;
#96129 = CIRCLE ( 'NONE', #129475, 0.1000000000000028644 ) ;
#96130 = CARTESIAN_POINT ( 'NONE',  ( -18.59999999999999787, 74.14897176987174987, -191.8691942151018850 ) ) ;
#96131 = ORIENTED_EDGE ( 'NONE', *, *, #67848, .T. ) ;
#96132 = CARTESIAN_POINT ( 'NONE',  ( 15.52844286134409124, 66.62433047358648253, -154.1553174751384461 ) ) ;
#96133 = DIRECTION ( 'NONE',  ( 1.000000000000000000, 0.000000000000000000, -0.000000000000000000 ) ) ;
#96134 = DIRECTION ( 'NONE',  ( 0.000000000000000000, 0.8814952561688476074, -0.4721928772777262417 ) ) ;
#96135 = DIRECTION ( 'NONE',  ( -0.7071067811865456854, -0.6824534298470390503, 0.1850873201762214815 ) ) ;
#96136 = CARTESIAN_POINT ( 'NONE',  ( -23.15000000000000213, -11.39257802169451139, -63.92605042016806749 ) ) ;
#96137 = CARTESIAN_POINT ( 'NONE',  ( 21.05000000000000071, 87.48912529308769592, -66.62310748452424036 ) ) ;
#96138 = VECTOR ( 'NONE', #254261, 1000.000000000000000 ) ;
#96139 = ORIENTED_EDGE ( 'NONE', *, *, #251975, .F. ) ;
#96140 = EDGE_CURVE ( 'NONE', #241350, #12190, #109128, .T. ) ;
#96141 = CARTESIAN_POINT ( 'NONE',  ( 23.14999999999999503, 11.65000000001116298, -54.85000000000000142 ) ) ;
#96142 = CARTESIAN_POINT ( 'NONE',  ( 21.07964655665547582, 67.22511038503350278, -124.3011909015603038 ) ) ;
#96143 = CARTESIAN_POINT ( 'NONE',  ( 21.05000000000000071, 18.71355990949045633, -229.9253020726244188 ) ) ;
#96144 = CARTESIAN_POINT ( 'NONE',  ( 21.07928932188134397, 76.00000000001267608, -203.5231074845243597 ) ) ;
#96145 = CYLINDRICAL_SURFACE ( 'NONE', #40730, 0.09999999999999939493 ) ;
#96146 = ORIENTED_EDGE ( 'NONE', *, *, #38010, .F. ) ;
#96147 = VERTEX_POINT ( 'NONE', #205554 ) ;
#96148 = DIRECTION ( 'NONE',  ( 0.000000000000000000, 1.000000000000000000, 0.000000000000000000 ) ) ;
#96149 = CYLINDRICAL_SURFACE ( 'NONE', #200977, 4.049999999999998046 ) ;
#96151 = ADVANCED_FACE ( 'NONE', ( #66055 ), #103875, .T. ) ;
#96150 = CARTESIAN_POINT ( 'NONE',  ( 19.97071067811864609, 11.72071067812981404, -125.2500000000000284 ) ) ;
#96152 = CARTESIAN_POINT ( 'NONE',  ( -18.59999999999999787, 68.97833521811203639, -132.8895420826271163 ) ) ;
#96153 = DIRECTION ( 'NONE',  ( -0.000000000000000000, -1.000000000000000000, 6.308085367188393199E-16 ) ) ;
#96154 = AXIS2_PLACEMENT_3D ( 'NONE', #235352, #56689, #136232 ) ;
#96155 = ORIENTED_EDGE ( 'NONE', *, *, #140851, .T. ) ;
#96156 = CARTESIAN_POINT ( 'NONE',  ( -20.94999999999999929, 16.50669723772569952, -240.7258389668962479 ) ) ;
#96157 = EDGE_CURVE ( 'NONE', #210270, #96826, #230262, .T. ) ;
#96158 = EDGE_CURVE ( 'NONE', #167205, #244509, #46481, .T. ) ;
#96159 = CARTESIAN_POINT ( 'NONE',  ( 20.85000000000000142, -1.263275465206102233, -108.4018646667464481 ) ) ;
#96160 = AXIS2_PLACEMENT_3D ( 'NONE', #188519, #68583, #47710 ) ;
#96161 = EDGE_LOOP ( 'NONE', ( #36241, #196926, #22254, #182017 ) ) ;
#96162 = SPHERICAL_SURFACE ( 'NONE', #54817, 0.1000000000000000056 ) ;
#96163 = PLANE ( 'NONE',  #95407 ) ;
#96164 = CONICAL_SURFACE ( 'NONE', #58744, 7.750000000000034639, 0.7853981633974531640 ) ;
#96165 = ADVANCED_FACE ( 'NONE', ( #126023 ), #220616, .F. ) ;
#96166 = ADVANCED_FACE ( 'NONE', ( #127321 ), #204767, .T. ) ;
#96167 = VERTEX_POINT ( 'NONE', #149475 ) ;
#96168 = CARTESIAN_POINT ( 'NONE',  ( -21.04999999999999361, 12.92448621296781930, -205.1280733356431938 ) ) ;
#96169 = CIRCLE ( 'NONE', #221071, 0.09999999999999939493 ) ;
#96170 = ORIENTED_EDGE ( 'NONE', *, *, #65339, .T. ) ;
#96171 = CARTESIAN_POINT ( 'NONE',  ( -21.14999999999994174, 77.73640333653723644, -47.54092689884382850 ) ) ;
#96172 = LINE ( 'NONE', #160041, #13289 ) ;
#96174 = ADVANCED_FACE ( 'NONE', ( #219370 ), #213264, .F. ) ;
#96173 = DIRECTION ( 'NONE',  ( -1.000000000000000000, 0.000000000000000000, 0.000000000000000000 ) ) ;
#96175 = DIRECTION ( 'NONE',  ( 1.000000000000000000, 0.000000000000000000, 0.000000000000000000 ) ) ;
#96176 = FACE_OUTER_BOUND ( 'NONE', #40443, .T. ) ;
#96177 = CYLINDRICAL_SURFACE ( 'NONE', #243518, 0.09999999999999939493 ) ;
#96178 = CARTESIAN_POINT ( 'NONE',  ( 20.27550659511088682, 9.216043722520002035, -42.75000000000000000 ) ) ;
#96179 = DIRECTION ( 'NONE',  ( -4.801466763864313332E-15, -0.2605042016806672911, -0.9654727137038716656 ) ) ;
#96180 = DIRECTION ( 'NONE',  ( 0.000000000000000000, -0.2128009952263485993, 0.9770955615653341697 ) ) ;
#96181 = EDGE_CURVE ( 'NONE', #242362, #60954, #232863, .T. ) ;
#96182 = CARTESIAN_POINT ( 'NONE',  ( -21.05000000000000071, 77.83534155023670564, -158.4679561919613491 ) ) ;
#96183 = DIRECTION ( 'NONE',  ( 7.589415207398576792E-15, -1.000000000000000000, -0.000000000000000000 ) ) ;
#96184 = LINE ( 'NONE', #253979, #102207 ) ;
#96185 = DIRECTION ( 'NONE',  ( -0.000000000000000000, 0.1298341882519735979, 0.9915357197604890427 ) ) ;
#96186 = VECTOR ( 'NONE', #8663, 1000.000000000000000 ) ;
#96187 = VERTEX_POINT ( 'NONE', #112897 ) ;
#96188 = EDGE_CURVE ( 'NONE', #198131, #158463, #66494, .T. ) ;
#96190 = ADVANCED_FACE ( 'NONE', ( #79843 ), #108015, .F. ) ;
#96189 = AXIS2_PLACEMENT_3D ( 'NONE', #67080, #113584, #13216 ) ;
#96191 = CARTESIAN_POINT ( 'NONE',  ( -23.25000000000000000, 11.39998237908105416, -245.7725481090871540 ) ) ;
#96192 = CARTESIAN_POINT ( 'NONE',  ( 21.05000000000000071, 70.50000000001151079, -48.42837350343745584 ) ) ;
#96193 = CIRCLE ( 'NONE', #137691, 0.1000000000000008799 ) ;
#96194 = EDGE_LOOP ( 'NONE', ( #111454, #64475, #139569, #128714 ) ) ;
#96195 = TOROIDAL_SURFACE ( 'NONE', #154507, 11.70000000000000462, 0.1000000000000000056 ) ;
#96196 = CARTESIAN_POINT ( 'NONE',  ( -18.34374000495059676, 62.50563584222673796, -209.4474707446456421 ) ) ;
#96198 = EDGE_CURVE ( 'NONE', #146024, #152762, #19915, .T. ) ;
#96197 = CARTESIAN_POINT ( 'NONE',  ( 21.10000000000000142, 6.342459739679072506, 12.00000000000000000 ) ) ;
#96199 = LINE ( 'NONE', #211035, #180980 ) ;
#96200 = TOROIDAL_SURFACE ( 'NONE', #12851, 11.65000000000000036, 0.1000000000000000056 ) ;
#96201 = TOROIDAL_SURFACE ( 'NONE', #254403, 11.65000000000000036, 0.1000000000000000056 ) ;
#96202 = ORIENTED_EDGE ( 'NONE', *, *, #24321, .F. ) ;
#96203 = CARTESIAN_POINT ( 'NONE',  ( 20.90000000326035590, 6.338045365888074656, 12.02580456186802671 ) ) ;
#96204 = EDGE_CURVE ( 'NONE', #231632, #59304, #120679, .T. ) ;
#96205 = EDGE_CURVE ( 'NONE', #194152, #14603, #195518, .T. ) ;
#96206 = CARTESIAN_POINT ( 'NONE',  ( -18.59999999999999787, 9.150000000011157653, -88.75000000000004263 ) ) ;
#96207 = ORIENTED_EDGE ( 'NONE', *, *, #158030, .T. ) ;
#96208 = DIRECTION ( 'NONE',  ( -1.000000000000000000, -0.000000000000000000, -0.000000000000000000 ) ) ;
#96209 = CARTESIAN_POINT ( 'NONE',  ( 20.85000000000000142, 78.48087866980282001, -232.8271061603568910 ) ) ;
#96210 = EDGE_CURVE ( 'NONE', #190865, #52387, #237666, .T. ) ;
#96211 = VECTOR ( 'NONE', #213983, 1000.000000000000000 ) ;
#96212 = TOROIDAL_SURFACE ( 'NONE', #221109, 0.2000000000000000111, 0.1000000000000000056 ) ;
#96213 = AXIS2_PLACEMENT_3D ( 'NONE', #161245, #221188, #24311 ) ;
#96214 = CIRCLE ( 'NONE', #137899, 0.5000000000000004441 ) ;
#96215 = ORIENTED_EDGE ( 'NONE', *, *, #252515, .F. ) ;
#96216 = CARTESIAN_POINT ( 'NONE',  ( -20.64999999999999858, 9.614325556249161409, -211.5456030694648746 ) ) ;
#96217 = ORIENTED_EDGE ( 'NONE', *, *, #85001, .T. ) ;
#96218 = EDGE_CURVE ( 'NONE', #203210, #28455, #12350, .T. ) ;
#96219 = CARTESIAN_POINT ( 'NONE',  ( 23.24999999999999289, 6.650000000011155876, -45.65000000000000568 ) ) ;
#96220 = EDGE_CURVE ( 'NONE', #239082, #77400, #152042, .T. ) ;
#96221 = DIRECTION ( 'NONE',  ( -1.000000000000000000, -0.000000000000000000, -0.000000000000000000 ) ) ;
#96222 = CARTESIAN_POINT ( 'NONE',  ( -21.05000000000000071, 1.148907358139439339E-11, -201.0000000000015064 ) ) ;
#96223 = DIRECTION ( 'NONE',  ( 0.000000000000000000, -0.4930308989874653269, -0.8700118002898649117 ) ) ;
#96224 = DIRECTION ( 'NONE',  ( 0.000000000000000000, 1.000000000000000000, 1.265107689135680095E-16 ) ) ;
#96225 = CIRCLE ( 'NONE', #133656, 0.09999999999999939493 ) ;
#96226 = CARTESIAN_POINT ( 'NONE',  ( -14.56556274378147542, 46.56801681390926007, -234.7608386620030956 ) ) ;
#96227 = DIRECTION ( 'NONE',  ( -0.7071067811865474617, -0.7071067811865474617, -0.000000000000000000 ) ) ;
#96229 = ORIENTED_EDGE ( 'NONE', *, *, #109981, .F. ) ;
#96228 = CARTESIAN_POINT ( 'NONE',  ( -18.42554971533677488, -9.497159669426592288, -40.53982691354863022 ) ) ;
#96230 = ORIENTED_EDGE ( 'NONE', *, *, #194300, .F. ) ;
#96232 = DIRECTION ( 'NONE',  ( 0.000000000000000000, 1.000000000000000000, 0.000000000000000000 ) ) ;
#96231 = CARTESIAN_POINT ( 'NONE',  ( 23.25000000000000000, 84.59626168225530307, -160.5729799673740104 ) ) ;
#96234 = ORIENTED_EDGE ( 'NONE', *, *, #172287, .F. ) ;
#96233 = DIRECTION ( 'NONE',  ( -0.000000000000000000, 0.4856429311786307768, 0.8741572761215385956 ) ) ;
#96235 = EDGE_LOOP ( 'NONE', ( #182519, #95391, #234625, #59648 ) ) ;
#96236 = CARTESIAN_POINT ( 'NONE',  ( -28.12018973533754362, 11.62642356364895413, -347.0000000000001137 ) ) ;
#96237 = DIRECTION ( 'NONE',  ( -6.938893903907222856E-15, -1.000000000000000000, -7.272083257015735086E-15 ) ) ;
#96238 = LINE ( 'NONE', #59662, #184048 ) ;
#96239 = DIRECTION ( 'NONE',  ( 0.000000000000000000, 0.3738317757009345654, 0.9274965247785492695 ) ) ;
#96240 = CARTESIAN_POINT ( 'NONE',  ( 23.15000000000000213, -12.41227409414968363, -30.50000000000000000 ) ) ;
#96241 = DIRECTION ( 'NONE',  ( -0.000000000000000000, -6.982962677686266711E-15, 1.000000000000000000 ) ) ;
#96242 = DIRECTION ( 'NONE',  ( 0.000000000000000000, 0.000000000000000000, -1.000000000000000000 ) ) ;
#96243 = AXIS2_PLACEMENT_3D ( 'NONE', #46587, #44047, #123584 ) ;
#96244 = FACE_OUTER_BOUND ( 'NONE', #114131, .T. ) ;
#96246 = ORIENTED_EDGE ( 'NONE', *, *, #22907, .F. ) ;
#96245 = EDGE_CURVE ( 'NONE', #185020, #220166, #231566, .T. ) ;
#96247 = ORIENTED_EDGE ( 'NONE', *, *, #185197, .F. ) ;
#96248 = CARTESIAN_POINT ( 'NONE',  ( -13.39999999999994529, 64.25000000001119815, -21.02310748452479316 ) ) ;
#96249 = ADVANCED_FACE ( 'NONE', ( #253671 ), #41576, .T. ) ;
#96250 = ORIENTED_EDGE ( 'NONE', *, *, #203219, .F. ) ;
#96251 = DIRECTION ( 'NONE',  ( 0.000000000000000000, -0.2558827019433787542, 0.9667078373770204847 ) ) ;
#96252 = ORIENTED_EDGE ( 'NONE', *, *, #222466, .T. ) ;
#96253 = DIRECTION ( 'NONE',  ( 2.952720810173289605E-16, -0.4721928772777354011, -0.8814952561688425003 ) ) ;
#96254 = AXIS2_PLACEMENT_3D ( 'NONE', #59509, #139041, #81635 ) ;
#96255 = CARTESIAN_POINT ( 'NONE',  ( 16.27683809663749770, 66.65000000001161595, -60.27310748452438816 ) ) ;
#96257 = VERTEX_POINT ( 'NONE', #252380 ) ;
#96256 = DIRECTION ( 'NONE',  ( 1.000000000000000000, 0.000000000000000000, 0.000000000000000000 ) ) ;
#96258 = CARTESIAN_POINT ( 'NONE',  ( -23.49999999999994316, 77.36076146337680370, -43.99645795275012006 ) ) ;
#96259 = ORIENTED_EDGE ( 'NONE', *, *, #245510, .F. ) ;
#96260 = CARTESIAN_POINT ( 'NONE',  ( 23.14999999999999858, 70.40000000001199965, -115.4283735034374274 ) ) ;
#96261 = DIRECTION ( 'NONE',  ( 0.000000000000000000, 0.9651348961777157509, -0.2617529984165031243 ) ) ;
#96262 = DIRECTION ( 'NONE',  ( 0.000000000000000000, -1.000000000000000000, 0.000000000000000000 ) ) ;
#96263 = DIRECTION ( 'NONE',  ( 0.000000000000000000, 0.2617529984164035373, 0.9651348961777428404 ) ) ;
#96264 = EDGE_CURVE ( 'NONE', #251476, #237540, #13792, .T. ) ;
#96265 = ORIENTED_EDGE ( 'NONE', *, *, #20948, .T. ) ;
#96266 = FACE_OUTER_BOUND ( 'NONE', #75236, .T. ) ;
#96267 = ORIENTED_EDGE ( 'NONE', *, *, #183752, .T. ) ;
#96270 = ORIENTED_EDGE ( 'NONE', *, *, #75031, .T. ) ;
#96269 = DIRECTION ( 'NONE',  ( -1.000000000000000000, -7.304098846218105085E-16, -4.217023435051676515E-16 ) ) ;
#96268 = PLANE ( 'NONE',  #103302 ) ;
#96271 = CIRCLE ( 'NONE', #133699, 0.09999999999999939493 ) ;
#96272 = DIRECTION ( 'NONE',  ( 1.000000000000000000, 7.304098846218135653E-16, 0.000000000000000000 ) ) ;
#96273 = CIRCLE ( 'NONE', #75477, 0.09999999999999939493 ) ;
#96274 = CARTESIAN_POINT ( 'NONE',  ( -22.39999999999999858, -2.598867842139048090, -189.5410128746472083 ) ) ;
#96275 = ORIENTED_EDGE ( 'NONE', *, *, #110851, .T. ) ;
#96276 = DIRECTION ( 'NONE',  ( -1.000000000000000000, 0.000000000000000000, -0.000000000000000000 ) ) ;
#96277 = DIRECTION ( 'NONE',  ( 0.000000000000000000, 0.8814952561688476074, -0.4721928772777262417 ) ) ;
#96278 = CARTESIAN_POINT ( 'NONE',  ( -23.25000000000000000, 77.16412189325286874, -61.60825939895269698 ) ) ;
#96280 = ORIENTED_EDGE ( 'NONE', *, *, #35863, .T. ) ;
#96279 = DIRECTION ( 'NONE',  ( 0.000000000000000000, 0.000000000000000000, 1.000000000000000000 ) ) ;
#96281 = DIRECTION ( 'NONE',  ( 0.000000000000000000, 0.1350103645451807555, 0.9908441862701609093 ) ) ;
#96282 = CIRCLE ( 'NONE', #597, 0.09999999999998898659 ) ;
#96283 = ORIENTED_EDGE ( 'NONE', *, *, #89977, .F. ) ;
#96284 = CARTESIAN_POINT ( 'NONE',  ( -16.89797118371585682, 9.976380722655704858, -180.0627066324412340 ) ) ;
#96285 = DIRECTION ( 'NONE',  ( 0.000000000000000000, 0.000000000000000000, -1.000000000000000000 ) ) ;
#96286 = CARTESIAN_POINT ( 'NONE',  ( -16.77977881697926676, 44.14725513176800575, -235.2973807268633379 ) ) ;
#96287 = VERTEX_POINT ( 'NONE', #93322 ) ;
#96288 = CARTESIAN_POINT ( 'NONE',  ( 20.85000000000000142, -1.851617760457748618, -78.60318971960367662 ) ) ;
#96289 = ORIENTED_EDGE ( 'NONE', *, *, #94177, .T. ) ;
#96290 = CARTESIAN_POINT ( 'NONE',  ( -18.50000000000000000, 9.350000000000001421, -21.15000000000000213 ) ) ;
#96291 = DIRECTION ( 'NONE',  ( 1.000000000000000000, 0.000000000000000000, 0.000000000000000000 ) ) ;
#96292 = CARTESIAN_POINT ( 'NONE',  ( -17.05016517656101627, 9.950000000012078516, -46.17269799600016000 ) ) ;
#96293 = VERTEX_POINT ( 'NONE', #132458 ) ;
#96294 = DIRECTION ( 'NONE',  ( 0.000000000000000000, 1.598721155460229520E-14, 1.000000000000000000 ) ) ;
#96295 = EDGE_CURVE ( 'NONE', #50451, #115380, #99774, .T. ) ;
#96296 = DIRECTION ( 'NONE',  ( 1.000000000000000000, 0.000000000000000000, 0.000000000000000000 ) ) ;
#96297 = TOROIDAL_SURFACE ( 'NONE', #183807, 7.800000000000000711, 0.1000000000000000056 ) ;
#96298 = AXIS2_PLACEMENT_3D ( 'NONE', #79204, #200456, #141751 ) ;
#96299 = ADVANCED_FACE ( 'NONE', ( #133732 ), #119012, .F. ) ;
#96300 = EDGE_LOOP ( 'NONE', ( #124478, #47109, #59067, #131713 ) ) ;
#96301 = AXIS2_PLACEMENT_3D ( 'NONE', #4731, #242072, #205512 ) ;
#96302 = DIRECTION ( 'NONE',  ( -1.000000000000000000, -1.652117596168391700E-15, -1.153667551319263085E-29 ) ) ;
#96303 = CARTESIAN_POINT ( 'NONE',  ( 23.14999999999999503, 69.45000000001259366, -191.1731074845243938 ) ) ;
#96304 = DIRECTION ( 'NONE',  ( 0.000000000000000000, -4.744542840278440942E-15, 1.000000000000000000 ) ) ;
#96305 = ORIENTED_EDGE ( 'NONE', *, *, #139293, .T. ) ;
#96306 = ADVANCED_FACE ( 'NONE', ( #29107 ), #48614, .F. ) ;
#96307 = SPHERICAL_SURFACE ( 'NONE', #241640, 0.1000000000000000056 ) ;
#96308 = ORIENTED_EDGE ( 'NONE', *, *, #186775, .T. ) ;
#96310 = ORIENTED_EDGE ( 'NONE', *, *, #47559, .T. ) ;
#96309 = DIRECTION ( 'NONE',  ( -1.000000000000000000, 1.207181226542539700E-16, -2.694675058168174199E-16 ) ) ;
#96311 = EDGE_CURVE ( 'NONE', #53074, #91270, #169907, .T. ) ;
#96312 = VECTOR ( 'NONE', #7675, 1000.000000000000000 ) ;
#96315 = ORIENTED_EDGE ( 'NONE', *, *, #96078, .T. ) ;
#96314 = ORIENTED_EDGE ( 'NONE', *, *, #205928, .F. ) ;
#96313 = LINE ( 'NONE', #115907, #96919 ) ;
#96316 = DIRECTION ( 'NONE',  ( 1.000000000000000000, 0.000000000000000000, 0.000000000000000000 ) ) ;
#96317 = CARTESIAN_POINT ( 'NONE',  ( -20.94999027547553894, 65.70673848566926267, -30.56382523348290547 ) ) ;
#96318 = CYLINDRICAL_SURFACE ( 'NONE', #235560, 0.09999999999999939493 ) ;
#96319 = EDGE_CURVE ( 'NONE', #198468, #183601, #133134, .T. ) ;
#96320 = CARTESIAN_POINT ( 'NONE',  ( -21.14999999999999858, 64.35000000001166143, -69.42310748452440805 ) ) ;
#96321 = CARTESIAN_POINT ( 'NONE',  ( 20.94999999999999929, 4.850467289730772791, -79.03426740900172831 ) ) ;
#96322 = CARTESIAN_POINT ( 'NONE',  ( -21.05000000000000071, -1.835341550213255957, -45.15515129256298366 ) ) ;
#96323 = LINE ( 'NONE', #135456, #26570 ) ;
#96324 = ORIENTED_EDGE ( 'NONE', *, *, #46542, .F. ) ;
#96325 = ORIENTED_EDGE ( 'NONE', *, *, #203800, .F. ) ;
#96326 = ORIENTED_EDGE ( 'NONE', *, *, #137173, .F. ) ;
#96327 = DIRECTION ( 'NONE',  ( 0.000000000000000000, -1.000000000000000000, 8.673617379884042375E-16 ) ) ;
#96329 = ORIENTED_EDGE ( 'NONE', *, *, #27656, .T. ) ;
#96328 = CARTESIAN_POINT ( 'NONE',  ( 23.15000000000000213, 87.19425987394825484, -209.6674621343692024 ) ) ;
#96330 = ORIENTED_EDGE ( 'NONE', *, *, #87905, .F. ) ;
#96331 = EDGE_CURVE ( 'NONE', #127614, #165621, #149732, .T. ) ;
#96333 = CARTESIAN_POINT ( 'NONE',  ( -23.25000000000000000, 76.00000000001207923, -128.6231074845243540 ) ) ;
#96332 = CIRCLE ( 'NONE', #17263, 0.3999999999999983569 ) ;
#96334 = ORIENTED_EDGE ( 'NONE', *, *, #193360, .F. ) ;
#96335 = CARTESIAN_POINT ( 'NONE',  ( -21.14999999999999858, 11.65000000000000036, -0.1000000000000028644 ) ) ;
#96336 = B_SPLINE_CURVE_WITH_KNOTS ( 'NONE', 3,
 ( #242966, #64348, #59161, #218254, #39672, #111179, #185570 ),
 .UNSPECIFIED., .F., .F.,
 ( 4, 3, 4 ),
 ( 0.000000000000000000, 1.860045280646151707E-05, 5.251155757305330614E-05 ),
 .UNSPECIFIED. ) ;
#96337 = CIRCLE ( 'NONE', #212895, 0.09999999999998898659 ) ;
#96338 = VERTEX_POINT ( 'NONE', #210279 ) ;
#96340 = CIRCLE ( 'NONE', #246220, 0.2000000000000000944 ) ;
#96339 = LINE ( 'NONE', #113361, #18817 ) ;
#96341 = DIRECTION ( 'NONE',  ( -2.602085213965226419E-14, -0.000000000000000000, -1.000000000000000000 ) ) ;
#96343 = ORIENTED_EDGE ( 'NONE', *, *, #174601, .F. ) ;
#96342 = ORIENTED_EDGE ( 'NONE', *, *, #25337, .F. ) ;
#96344 = VERTEX_POINT ( 'NONE', #95137 ) ;
#96346 = SPHERICAL_SURFACE ( 'NONE', #157522, 0.1000000000000000056 ) ;
#96345 = AXIS2_PLACEMENT_3D ( 'NONE', #154535, #157080, #234025 ) ;
#96347 = VERTEX_POINT ( 'NONE', #111170 ) ;
#96348 = ORIENTED_EDGE ( 'NONE', *, *, #7805, .T. ) ;
#96349 = CARTESIAN_POINT ( 'NONE',  ( -23.49999999999994316, 84.00000000001119815, -37.18565239344504647 ) ) ;
#96350 = CIRCLE ( 'NONE', #146254, 0.09999999999999939493 ) ;
#96352 = ORIENTED_EDGE ( 'NONE', *, *, #116565, .T. ) ;
#96351 = DIRECTION ( 'NONE',  ( -1.000000000000000000, -0.000000000000000000, -0.000000000000000000 ) ) ;
#96353 = DIRECTION ( 'NONE',  ( 1.000000000000000000, 0.000000000000000000, 0.000000000000000000 ) ) ;
#96355 = CARTESIAN_POINT ( 'NONE',  ( 20.95035502843362707, 65.52236167323586358, -162.4468077757880451 ) ) ;
#96354 = DIRECTION ( 'NONE',  ( -1.000000000000000000, -2.952720810173289112E-16, 0.000000000000000000 ) ) ;
#96356 = PLANE ( 'NONE',  #119855 ) ;
#96357 = CARTESIAN_POINT ( 'NONE',  ( -16.94107738177415712, 60.85118289042637940, -221.1214263997032106 ) ) ;
#96358 = CARTESIAN_POINT ( 'NONE',  ( 23.40000000000005542, 83.90000000001120384, -37.18565239344504647 ) ) ;
#96359 = ORIENTED_EDGE ( 'NONE', *, *, #160580, .F. ) ;
#96360 = ORIENTED_EDGE ( 'NONE', *, *, #124691, .T. ) ;
#96361 = DIRECTION ( 'NONE',  ( -1.836970198721029934E-16, 1.000000000000000000, 0.000000000000000000 ) ) ;
#96362 = LINE ( 'NONE', #135491, #14396 ) ;
#96363 = CARTESIAN_POINT ( 'NONE',  ( 21.30000000000002558, 76.00000000001192291, -98.97310748452431994 ) ) ;
#96365 = ORIENTED_EDGE ( 'NONE', *, *, #232777, .T. ) ;
#96364 = CIRCLE ( 'NONE', #13198, 0.1999999999999987899 ) ;
#96366 = DIRECTION ( 'NONE',  ( -1.000000000000000000, 0.000000000000000000, 0.000000000000000000 ) ) ;
#96367 = AXIS2_PLACEMENT_3D ( 'NONE', #200832, #256895, #157897 ) ;
#96368 = EDGE_CURVE ( 'NONE', #82065, #19295, #195547, .T. ) ;
#96369 = DIRECTION ( 'NONE',  ( 1.000000000000000000, 0.000000000000000000, 0.000000000000000000 ) ) ;
#96370 = DIRECTION ( 'NONE',  ( 1.000000000000000000, -0.000000000000000000, -0.000000000000000000 ) ) ;
#96371 = ORIENTED_EDGE ( 'NONE', *, *, #127030, .T. ) ;
#96372 = EDGE_LOOP ( 'NONE', ( #227101, #152063, #51059, #133278 ) ) ;
#96373 = AXIS2_PLACEMENT_3D ( 'NONE', #75043, #55405, #150263 ) ;
#96374 = CARTESIAN_POINT ( 'NONE',  ( 18.59999999999997655, 11.75000000000000000, -33.50000000000000000 ) ) ;
#96375 = CARTESIAN_POINT ( 'NONE',  ( -23.25000000000000000, 43.27008861172207332, -245.2265230569236110 ) ) ;
#96376 = EDGE_LOOP ( 'NONE', ( #34830, #190505, #81241, #237824, #248976, #219571, #257596, #169425, #17180, #78922, #206770, #185103, #149915, #9384, #207889, #93543 ) ) ;
#96377 = CARTESIAN_POINT ( 'NONE',  ( 18.59999999999997655, 1.115600667400684642E-11, -208.8999999999999488 ) ) ;
#96378 = ORIENTED_EDGE ( 'NONE', *, *, #191032, .T. ) ;
#96379 = DIRECTION ( 'NONE',  ( 1.000000000000000000, 0.000000000000000000, 0.000000000000000000 ) ) ;
#96382 = ADVANCED_FACE ( 'NONE', ( #155148 ), #150305, .T. ) ;
#96381 = CIRCLE ( 'NONE', #133989, 0.2000000000000057288 ) ;
#96380 = DIRECTION ( 'NONE',  ( 1.000000000000000000, -2.952720810173289112E-16, -2.061873921506763405E-30 ) ) ;
#96384 = CARTESIAN_POINT ( 'NONE',  ( -21.14999999999999858, -1.391858308744749140, -194.6091531227727955 ) ) ;
#96383 = LINE ( 'NONE', #194252, #19787 ) ;
#96385 = DIRECTION ( 'NONE',  ( 0.000000000000000000, -1.000000000000000000, -6.860497997771532351E-15 ) ) ;
#96386 = CARTESIAN_POINT ( 'NONE',  ( 21.05000000000000071, 65.27628289530434813, -90.86191719039695158 ) ) ;
#96387 = EDGE_CURVE ( 'NONE', #91407, #87397, #203852, .T. ) ;
#96388 = EDGE_CURVE ( 'NONE', #29926, #151185, #28948, .T. ) ;
#96389 = CARTESIAN_POINT ( 'NONE',  ( -21.05000000000000071, -11.48912529306489994, -198.0999999999999659 ) ) ;
#96390 = CIRCLE ( 'NONE', #217186, 12.77499999999999325 ) ;
#96391 = CIRCLE ( 'NONE', #108875, 0.1000000000000013933 ) ;
#96392 = CIRCLE ( 'NONE', #146451, 11.64999999999999325 ) ;
#96393 = AXIS2_PLACEMENT_3D ( 'NONE', #199153, #20536, #189857 ) ;
#96395 = EDGE_LOOP ( 'NONE', ( #171091, #218482, #62871, #129246 ) ) ;
#96394 = ORIENTED_EDGE ( 'NONE', *, *, #236152, .T. ) ;
#96396 = VERTEX_POINT ( 'NONE', #167312 ) ;
#96397 = CARTESIAN_POINT ( 'NONE',  ( -22.84999999999999787, 0.000000000000000000, 0.000000000000000000 ) ) ;
#96398 = DIRECTION ( 'NONE',  ( -1.000000000000000000, 0.000000000000000000, 0.000000000000000000 ) ) ;
#96399 = DIRECTION ( 'NONE',  ( 0.000000000000000000, 6.982962677686266711E-15, -1.000000000000000000 ) ) ;
#96400 = CARTESIAN_POINT ( 'NONE',  ( -23.25000000000000000, 11.75000000001115552, -59.98519422934606382 ) ) ;
#96401 = EDGE_CURVE ( 'NONE', #181466, #37087, #90299, .T. ) ;
#96403 = CARTESIAN_POINT ( 'NONE',  ( -15.75000000000000355, 66.65000000001185754, -86.27310748452437394 ) ) ;
#96402 = CARTESIAN_POINT ( 'NONE',  ( 20.21494484322224849, 9.303170737868777351, -8.340265191770429354 ) ) ;
#96404 = DIRECTION ( 'NONE',  ( -1.000000000000000000, -2.885090398161910739E-16, -6.283419270304611573E-17 ) ) ;
#96405 = ORIENTED_EDGE ( 'NONE', *, *, #225220, .F. ) ;
#96406 = EDGE_CURVE ( 'NONE', #238847, #118231, #107304, .T. ) ;
#96407 = PLANE ( 'NONE',  #897 ) ;
#96408 = ORIENTED_EDGE ( 'NONE', *, *, #35616, .F. ) ;
#96409 = ORIENTED_EDGE ( 'NONE', *, *, #245732, .T. ) ;
#96410 = CARTESIAN_POINT ( 'NONE',  ( 21.14999999999999858, 65.28660755661270798, -191.2731074845244166 ) ) ;
#96411 = CARTESIAN_POINT ( 'NONE',  ( -18.59999999999999787, 74.83729825007360148, -61.42310748452432989 ) ) ;
#96412 = CARTESIAN_POINT ( 'NONE',  ( -20.54999999999999716, 76.00000000001126921, -203.5231074845248997 ) ) ;
#96413 = CARTESIAN_POINT ( 'NONE',  ( 19.75857864376268935, 11.75000000001115907, -158.8500000000000227 ) ) ;
#96414 = DIRECTION ( 'NONE',  ( -1.000000000000000000, 0.000000000000000000, 0.000000000000000000 ) ) ;
#96415 = ORIENTED_EDGE ( 'NONE', *, *, #145636, .T. ) ;
#96416 = ORIENTED_EDGE ( 'NONE', *, *, #135373, .T. ) ;
#96417 = CARTESIAN_POINT ( 'NONE',  ( -20.64999999999999858, 7.250000000011155521, -88.25000000000005684 ) ) ;
#96418 = EDGE_CURVE ( 'NONE', #225759, #53074, #224692, .T. ) ;
#96419 = DIRECTION ( 'NONE',  ( 1.000000000000000000, 2.952720810173289112E-16, -0.000000000000000000 ) ) ;
#96420 = EDGE_CURVE ( 'NONE', #156184, #114049, #128870, .T. ) ;
#96421 = CARTESIAN_POINT ( 'NONE',  ( -23.15000000000000213, 64.35000000001218723, -143.5379132551784096 ) ) ;
#96422 = DIRECTION ( 'NONE',  ( 1.000000000000000000, 0.000000000000000000, 0.000000000000000000 ) ) ;
#96423 = ADVANCED_FACE ( 'NONE', ( #89018 ), #186869, .T. ) ;
#96424 = DIRECTION ( 'NONE',  ( 0.000000000000000000, 0.000000000000000000, 1.000000000000000000 ) ) ;
#96425 = TOROIDAL_SURFACE ( 'NONE', #129204, 0.2000000000000000111, 0.1000000000000000056 ) ;
#96426 = CARTESIAN_POINT ( 'NONE',  ( 5.899999999999996803, -11.65000000000000036, 14.00000000000000178 ) ) ;
#96428 = DIRECTION ( 'NONE',  ( 1.186688945009010077E-16, 1.000000000000000000, 6.982962677686266711E-15 ) ) ;
#96427 = CARTESIAN_POINT ( 'NONE',  ( -20.94999999999999929, 87.65000000001246860, -172.9231074845242802 ) ) ;
#96429 = CARTESIAN_POINT ( 'NONE',  ( -18.50000000000000000, 11.75000000001115197, -122.2500000000000284 ) ) ;
#96430 = CARTESIAN_POINT ( 'NONE',  ( -18.50000000000000000, 11.65000000001115588, -100.5000000000000426 ) ) ;
#96431 = CARTESIAN_POINT ( 'NONE',  ( -17.11825945287481332, 65.95000000001152785, -48.67310748452439384 ) ) ;
#96432 = DIRECTION ( 'NONE',  ( 1.000000000000000000, 0.000000000000000000, 0.000000000000000000 ) ) ;
#96434 = ORIENTED_EDGE ( 'NONE', *, *, #163668, .T. ) ;
#96433 = PLANE ( 'NONE',  #202999 ) ;
#96435 = CIRCLE ( 'NONE', #567, 0.1000000000000028644 ) ;
#96436 = EDGE_CURVE ( 'NONE', #227912, #94985, #162190, .T. ) ;
#96437 = FACE_OUTER_BOUND ( 'NONE', #112701, .T. ) ;
#96438 = EDGE_LOOP ( 'NONE', ( #193449, #17122, #227843, #10104 ) ) ;
#96439 = DIRECTION ( 'NONE',  ( -1.000000000000000000, 0.000000000000000000, 0.000000000000000000 ) ) ;
#96440 = CARTESIAN_POINT ( 'NONE',  ( 18.49999999999998934, 64.35000000001177511, -78.27310748452438816 ) ) ;
#96441 = ORIENTED_EDGE ( 'NONE', *, *, #128198, .F. ) ;
#96442 = EDGE_CURVE ( 'NONE', #109044, #212285, #248101, .T. ) ;
#96443 = LINE ( 'NONE', #78171, #13274 ) ;
#96444 = DIRECTION ( 'NONE',  ( 0.000000000000000000, 0.9908441862701596881, 0.1350103645451904977 ) ) ;
#96445 = CARTESIAN_POINT ( 'NONE',  ( 21.05000000000000071, -9.399999999988846611, -76.89396912265249284 ) ) ;
#96446 = AXIS2_PLACEMENT_3D ( 'NONE', #89375, #205476, #125935 ) ;
#96447 = AXIS2_PLACEMENT_3D ( 'NONE', #128164, #224674, #126877 ) ;
#96448 = CARTESIAN_POINT ( 'NONE',  ( -20.94999999999999929, 70.37092869010230345, -198.1237041667535550 ) ) ;
#96449 = DIRECTION ( 'NONE',  ( 1.000000000000000000, 0.000000000000000000, 0.000000000000000000 ) ) ;
#96451 = CARTESIAN_POINT ( 'NONE',  ( -16.97683809663752186, 9.850000000011137402, -154.0976359818037054 ) ) ;
#96450 = AXIS2_PLACEMENT_3D ( 'NONE', #245012, #23435, #164210 ) ;
#96452 = ORIENTED_EDGE ( 'NONE', *, *, #12018, .F. ) ;
#96453 = DIRECTION ( 'NONE',  ( 1.000000000000000000, 0.000000000000000000, 0.000000000000000000 ) ) ;
#96455 = EDGE_LOOP ( 'NONE', ( #179539, #46400, #198734, #85437 ) ) ;
#96454 = CARTESIAN_POINT ( 'NONE',  ( -23.15000000000000213, 87.65000000001192859, -106.1231074845242262 ) ) ;
#96456 = DIRECTION ( 'NONE',  ( -0.000000000000000000, 0.9126074666063770380, 0.4088369013363281068 ) ) ;
#96457 = EDGE_CURVE ( 'NONE', #193233, #24117, #228815, .T. ) ;
#96458 = CARTESIAN_POINT ( 'NONE',  ( -18.59999999999999787, 7.021664781911246322, -204.7335654018972662 ) ) ;
#96459 = VERTEX_POINT ( 'NONE', #255439 ) ;
#96460 = DIRECTION ( 'NONE',  ( 1.000000000000000000, -2.952720810173289112E-16, -2.061873921506763405E-30 ) ) ;
#96461 = EDGE_CURVE ( 'NONE', #209609, #176903, #43340, .T. ) ;
#96462 = PRODUCT_CONTEXT ( 'NONE', #39080, 'mechanical' ) ;
#96463 = CARTESIAN_POINT ( 'NONE',  ( 23.24999999999999645, 5.650000000011139001, -54.34999999999999432 ) ) ;
#96464 = DIRECTION ( 'NONE',  ( 0.000000000000000000, 0.000000000000000000, 1.000000000000000000 ) ) ;
#96465 = AXIS2_PLACEMENT_3D ( 'NONE', #196566, #119621, #117045 ) ;
#96466 = EDGE_LOOP ( 'NONE', ( #40028, #110743, #205847, #25988 ) ) ;
#96468 = ADVANCED_FACE ( 'NONE', ( #121381 ), #138307, .T. ) ;
#96467 = CARTESIAN_POINT ( 'NONE',  ( 23.24999999999999645, 71.22429906543278832, -148.3718755885703331 ) ) ;
#96469 = CARTESIAN_POINT ( 'NONE',  ( 18.59999999999999076, 11.65000000000000391, 11.75000000000000000 ) ) ;
#96470 = ADVANCED_FACE ( 'NONE', ( #40560 ), #22257, .F. ) ;
#96471 = EDGE_CURVE ( 'NONE', #125507, #133309, #70801, .T. ) ;
#96472 = CARTESIAN_POINT ( 'NONE',  ( 18.59999999999999787, 77.83585931145498193, -24.51866831572578675 ) ) ;
#96473 = ORIENTED_EDGE ( 'NONE', *, *, #93390, .F. ) ;
#96474 = ORIENTED_EDGE ( 'NONE', *, *, #188289, .F. ) ;
#96475 = CARTESIAN_POINT ( 'NONE',  ( -20.64999999999999858, -8.999999999988844479, -124.5060308773475839 ) ) ;
#96476 = CARTESIAN_POINT ( 'NONE',  ( -20.94999999999999929, 74.16465844978787914, -158.4679561919613775 ) ) ;
#96477 = DIRECTION ( 'NONE',  ( 0.000000000000000000, -0.2128009952263651694, 0.9770955615653305060 ) ) ;
#96478 = CARTESIAN_POINT ( 'NONE',  ( -23.15000000000000213, 64.25000000001259082, -191.3731074845244393 ) ) ;
#96480 = CARTESIAN_POINT ( 'NONE',  ( 20.94999999999999929, -8.999999999988842703, -191.1060308773475072 ) ) ;
#96479 = VECTOR ( 'NONE', #68028, 1000.000000000000000 ) ;
#96481 = AXIS2_PLACEMENT_3D ( 'NONE', #244652, #66023, #145548 ) ;
#96484 = CYLINDRICAL_SURFACE ( 'NONE', #12133, 0.09999999999999939493 ) ;
#96483 = AXIS2_PLACEMENT_3D ( 'NONE', #103530, #81380, #99668 ) ;
#96482 = DIRECTION ( 'NONE',  ( -1.000000000000000000, 0.000000000000000000, 0.000000000000000000 ) ) ;
#96485 = CARTESIAN_POINT ( 'NONE',  ( 20.94999999999999929, 65.70729864260954400, -30.56574559737246233 ) ) ;
#96486 = LINE ( 'NONE', #156522, #122845 ) ;
#96487 = CARTESIAN_POINT ( 'NONE',  ( 23.24999999999999289, 5.950000000000007283, -23.19429769496518645 ) ) ;
#96488 = DIRECTION ( 'NONE',  ( 0.000000000000000000, -6.853228547068871147E-15, 1.000000000000000000 ) ) ;
#96489 = ORIENTED_EDGE ( 'NONE', *, *, #51230, .T. ) ;
#96490 = EDGE_CURVE ( 'NONE', #4288, #210631, #108375, .T. ) ;
#96491 = EDGE_LOOP ( 'NONE', ( #236663, #113674, #69834, #30266, #128411 ) ) ;
#96492 = DIRECTION ( 'NONE',  ( 1.000000000000000000, -0.000000000000000000, -0.000000000000000000 ) ) ;
#96493 = ADVANCED_FACE ( 'NONE', ( #200871 ), #37471, .F. ) ;
#96494 = DIRECTION ( 'NONE',  ( 1.000000000000000000, 0.000000000000000000, 0.000000000000000000 ) ) ;
#96496 = DIRECTION ( 'NONE',  ( 1.000000000000000000, 0.000000000000000000, 0.000000000000000000 ) ) ;
#96495 = CARTESIAN_POINT ( 'NONE',  ( 21.05000000000000071, 71.14953271029243353, -124.4888400755226598 ) ) ;
#96497 = DIRECTION ( 'NONE',  ( -1.000000000000000000, 0.000000000000000000, 0.000000000000000000 ) ) ;
#96499 = EDGE_CURVE ( 'NONE', #144360, #16182, #183204, .T. ) ;
#96498 = CYLINDRICAL_SURFACE ( 'NONE', #254040, 0.09999999999999817368 ) ;
#96500 = CARTESIAN_POINT ( 'NONE',  ( -21.05000000000000071, 0.09779029131994770863, -94.24218538952392521 ) ) ;
#96501 = VERTEX_POINT ( 'NONE', #118784 ) ;
#96502 = ORIENTED_EDGE ( 'NONE', *, *, #75291, .F. ) ;
#96503 = EDGE_CURVE ( 'NONE', #254324, #28381, #49917, .T. ) ;
#96504 = CARTESIAN_POINT ( 'NONE',  ( -20.94999999999999929, 64.40000000001190017, -96.09490425424884563 ) ) ;
#96505 = ORIENTED_EDGE ( 'NONE', *, *, #240187, .F. ) ;
#96506 = EDGE_CURVE ( 'NONE', #87569, #154428, #242559, .T. ) ;
#96507 = CARTESIAN_POINT ( 'NONE',  ( -21.14999999999999858, 31.98723526783714988, -238.8784020251475511 ) ) ;
#96508 = DIRECTION ( 'NONE',  ( -1.000000000000000000, -0.000000000000000000, -0.000000000000000000 ) ) ;
#96509 = ADVANCED_FACE ( 'NONE', ( #62660 ), #120090, .T. ) ;
#96510 = ORIENTED_EDGE ( 'NONE', *, *, #16887, .F. ) ;
#96511 = LINE ( 'NONE', #176104, #63768 ) ;
#96512 = CIRCLE ( 'NONE', #242270, 4.049999999999998046 ) ;
#96513 = ORIENTED_EDGE ( 'NONE', *, *, #188599, .F. ) ;
#96514 = CARTESIAN_POINT ( 'NONE',  ( -18.59999999999999787, 12.97363049771892207, -205.3537238898406940 ) ) ;
#96515 = ADVANCED_FACE ( 'NONE', ( #163058 ), #199618, .F. ) ;
#96516 = FACE_OUTER_BOUND ( 'NONE', #75873, .T. ) ;
#96518 = AXIS2_PLACEMENT_3D ( 'NONE', #107008, #186578, #7936 ) ;
#96517 = DIRECTION ( 'NONE',  ( 1.000000000000000000, 0.000000000000000000, 0.000000000000000000 ) ) ;
#96519 = DIRECTION ( 'NONE',  ( -1.000000000000000000, 0.000000000000000000, 0.000000000000000000 ) ) ;
#96520 = CARTESIAN_POINT ( 'NONE',  ( -16.97683809663752186, 9.949999999999983302, -13.40236401819648648 ) ) ;
#96522 = CARTESIAN_POINT ( 'NONE',  ( -11.60000000000000320, -8.250000000000007105, 12.40000000000000391 ) ) ;
#96521 = CARTESIAN_POINT ( 'NONE',  ( -18.59999999999999787, 1.162701749949165642, -142.1000000000000227 ) ) ;
#96524 = FACE_OUTER_BOUND ( 'NONE', #48850, .T. ) ;
#96523 = AXIS2_PLACEMENT_3D ( 'NONE', #129648, #231338, #111372 ) ;
#96525 = VERTEX_POINT ( 'NONE', #160494 ) ;
#96527 = CARTESIAN_POINT ( 'NONE',  ( -23.25000000000000000, 76.10000000001245724, -181.6726782920691505 ) ) ;
#96526 = CARTESIAN_POINT ( 'NONE',  ( 23.24999999999999289, 69.35000000001222986, -148.8731074845244109 ) ) ;
#96528 = VERTEX_POINT ( 'NONE', #82178 ) ;
#96530 = VERTEX_POINT ( 'NONE', #241303 ) ;
#96529 = CARTESIAN_POINT ( 'NONE',  ( 21.05000000000000071, 71.00000000001205080, -124.1178414656112352 ) ) ;
#96531 = ORIENTED_EDGE ( 'NONE', *, *, #189791, .T. ) ;
#96532 = DIRECTION ( 'NONE',  ( -4.408576920032448588E-17, 0.1350103645451876666, -0.9908441862701600211 ) ) ;
#96533 = CARTESIAN_POINT ( 'NONE',  ( 21.05000000000000071, -7.176961358819842651, -212.6889627706600834 ) ) ;
#96534 = DIRECTION ( 'NONE',  ( 0.000000000000000000, 0.000000000000000000, -1.000000000000000000 ) ) ;
#96535 = CARTESIAN_POINT ( 'NONE',  ( 20.94999999999999574, -10.76604040606816959, -206.3127087229280789 ) ) ;
#96536 = CIRCLE ( 'NONE', #92450, 2.099999999999990763 ) ;
#96537 = ORIENTED_EDGE ( 'NONE', *, *, #215398, .F. ) ;
#96538 = DIRECTION ( 'NONE',  ( 0.000000000000000000, -0.8371762388950346745, -0.5469332180710581026 ) ) ;
#96539 =( NAMED_UNIT ( * ) SI_UNIT ( $, .STERADIAN. ) SOLID_ANGLE_UNIT ( ) );
#96540 = CARTESIAN_POINT ( 'NONE',  ( -23.15000000000000213, -11.48912529306489994, -64.00000000000000000 ) ) ;
#96541 = VERTEX_POINT ( 'NONE', #23565 ) ;
#96542 = AXIS2_PLACEMENT_3D ( 'NONE', #201944, #204487, #122407 ) ;
#96543 = CARTESIAN_POINT ( 'NONE',  ( -23.15000000000000213, 1.115600667400684642E-11, -79.77500000000003411 ) ) ;
#96544 = AXIS2_PLACEMENT_3D ( 'NONE', #128213, #223438, #69536 ) ;
#96545 = CARTESIAN_POINT ( 'NONE',  ( -18.40000000000000213, 70.35000000001261355, -190.8731074845244109 ) ) ;
#96546 = AXIS2_PLACEMENT_3D ( 'NONE', #172958, #111653, #110363 ) ;
#96547 = VERTEX_POINT ( 'NONE', #143462 ) ;
#96548 = EDGE_LOOP ( 'NONE', ( #134041, #207331, #27720, #71340 ) ) ;
#96549 = CARTESIAN_POINT ( 'NONE',  ( -16.85718274719488363, 9.976142314632912900, -188.4366536678175521 ) ) ;
#96550 = AXIS2_PLACEMENT_3D ( 'NONE', #158536, #75153, #16458 ) ;
#96551 = ORIENTED_EDGE ( 'NONE', *, *, #211986, .F. ) ;
#96552 = CARTESIAN_POINT ( 'NONE',  ( 21.14999999999999858, 0.09779029131994770863, -27.24218538952387547 ) ) ;
#96553 = ORIENTED_EDGE ( 'NONE', *, *, #111069, .F. ) ;
#96554 = CARTESIAN_POINT ( 'NONE',  ( 23.15000000000000213, -3.770473190032740174, -225.9805569534692324 ) ) ;
#96555 = AXIS2_PLACEMENT_3D ( 'NONE', #56997, #136546, #139092 ) ;
#96556 = EDGE_CURVE ( 'NONE', #183119, #40953, #238719, .T. ) ;
#96557 = CARTESIAN_POINT ( 'NONE',  ( -21.05000000000000071, -11.48912529306490349, -36.39999999999999858 ) ) ;
#96558 = CARTESIAN_POINT ( 'NONE',  ( 21.05000000000024585, 60.89892960307708591, -225.3088725716038709 ) ) ;
#96559 = CIRCLE ( 'NONE', #229862, 0.09999999999999230338 ) ;
#96560 = CARTESIAN_POINT ( 'NONE',  ( -16.86379686415369150, 63.08322136712259010, -213.0405382708815409 ) ) ;
#96561 = DIRECTION ( 'NONE',  ( 0.000000000000000000, 0.2617529984165031243, 0.9651348961777157509 ) ) ;
#96562 = CARTESIAN_POINT ( 'NONE',  ( 18.37172112093854892, -9.570961652231936512, -73.81673445348330631 ) ) ;
#96563 = EDGE_CURVE ( 'NONE', #215553, #27724, #19685, .T. ) ;
#96564 = ORIENTED_EDGE ( 'NONE', *, *, #815, .F. ) ;
#96566 = LINE ( 'NONE', #58721, #10694 ) ;
#96565 = DIRECTION ( 'NONE',  ( 0.000000000000000000, -0.9126074666063770380, -0.4088369013363281068 ) ) ;
#96567 = VECTOR ( 'NONE', #57019, 1000.000000000000000 ) ;
#96568 = ORIENTED_EDGE ( 'NONE', *, *, #140713, .T. ) ;
#96571 = ORIENTED_EDGE ( 'NONE', *, *, #98211, .T. ) ;
#96570 = CARTESIAN_POINT ( 'NONE',  ( -18.42554971533678199, 85.49715966944935985, -62.48328057097562294 ) ) ;
#96569 = CARTESIAN_POINT ( 'NONE',  ( -23.25000000000000000, 30.73962027982165779, -265.0781340245722504 ) ) ;
#96572 = VECTOR ( 'NONE', #198840, 1000.000000000000000 ) ;
#96573 = ORIENTED_EDGE ( 'NONE', *, *, #216596, .F. ) ;
#96574 = AXIS2_PLACEMENT_3D ( 'NONE', #28501, #187552, #168002 ) ;
#96575 = CARTESIAN_POINT ( 'NONE',  ( 12.60053434924909688, 66.61046543766556738, -154.3482981801344636 ) ) ;
#96576 = DIRECTION ( 'NONE',  ( -1.000000000000000000, -0.000000000000000000, -0.000000000000000000 ) ) ;
#96577 = ORIENTED_EDGE ( 'NONE', *, *, #144792, .F. ) ;
#96578 = CARTESIAN_POINT ( 'NONE',  ( 20.04142135623730070, 64.25000000001179501, -81.67310748452439384 ) ) ;
#96580 = DIRECTION ( 'NONE',  ( 1.000000000000000000, -2.952720810173289112E-16, -2.061873921506763405E-30 ) ) ;
#96579 =( BOUNDED_CURVE ( )  B_SPLINE_CURVE ( 3, ( #17755, #196406, #253807, #235529 ),
 .UNSPECIFIED., .F., .F. ) 
 B_SPLINE_CURVE_WITH_KNOTS ( ( 4, 4 ),
 ( 4.712388980384696779, 6.231880751915386263 ),
 .UNSPECIFIED. ) 
 CURVE ( )  GEOMETRIC_REPRESENTATION_ITEM ( )  RATIONAL_B_SPLINE_CURVE ( ( 1.000000000000000000, 0.8166740347213244933, 0.8166740347213244933, 1.000000000000000000 ) ) 
 REPRESENTATION_ITEM ( '' )  );
#96582 = DIRECTION ( 'NONE',  ( 0.7071067811865708874, -0.3338907855511046296, -0.6233112732207185536 ) ) ;
#96581 = SPHERICAL_SURFACE ( 'NONE', #196897, 0.1000000000000000056 ) ;
#96584 = EDGE_LOOP ( 'NONE', ( #241796, #129392, #18703, #32064, #234004, #89829, #63681, #11, #103733, #98618, #54369 ) ) ;
#96583 = CARTESIAN_POINT ( 'NONE',  ( -18.59999999999999787, -8.262584272387851314, 10.47734830970188824 ) ) ;
#96585 = ORIENTED_EDGE ( 'NONE', *, *, #154513, .T. ) ;
#96586 = AXIS2_PLACEMENT_3D ( 'NONE', #216676, #155465, #249702 ) ;
#96587 = CARTESIAN_POINT ( 'NONE',  ( 18.59999999999998366, 68.97833521811179480, -99.18954208262705663 ) ) ;
#96588 = FACE_OUTER_BOUND ( 'NONE', #11871, .T. ) ;
#96589 = ORIENTED_EDGE ( 'NONE', *, *, #35804, .F. ) ;
#96590 = FACE_BOUND ( 'NONE', #29117, .T. ) ;
#96591 = ORIENTED_EDGE ( 'NONE', *, *, #149896, .F. ) ;
#96592 =( BOUNDED_SURFACE ( )  B_SPLINE_SURFACE ( 3, 2, ( 
 ( #155778, #120505, #74957 ),
 ( #154498, #134867, #35820 ),
 ( #214423, #115326, #194892 ),
 ( #244253, #200018, #102156 ),
 ( #166046, #103452, #26526 ),
 ( #160903, #63054, #82589 ) ),
 .UNSPECIFIED., .F., .F., .F. ) 
 B_SPLINE_SURFACE_WITH_KNOTS ( ( 4, 2, 4 ),
 ( 3, 3 ),
 ( 1.570796326794895448, 2.356194490192343505, 3.141592653589791784 ),
 ( 0.000000000000000000, 1.000000000000000000 ),
 .UNSPECIFIED. ) 
 GEOMETRIC_REPRESENTATION_ITEM ( )  RATIONAL_B_SPLINE_SURFACE ( (
 ( 1.000000000000000000, 0.7071067811865475727, 1.000000000000000000),
 ( 1.000000000000000000, 0.6611148371779108635, 1.000000000000000000),
 ( 1.000000000000000000, 0.6092287576696373552, 1.000000000000000000),
 ( 1.000000000000000000, 0.5278258667057376119, 1.000000000000000000),
 ( 1.000000000000000000, 0.4993418825334632327, 1.000000000000000000),
 ( 1.000000000000000000, 0.5000000000000456302, 1.000000000000000000) ) ) 
 REPRESENTATION_ITEM ( '' )  SURFACE ( )  );
#96593 = CARTESIAN_POINT ( 'NONE',  ( 18.39999999999999858, 85.50000000001185185, -96.42291809330220076 ) ) ;
#96594 = CARTESIAN_POINT ( 'NONE',  ( -20.54999999999999716, -8.999999999988844479, -124.1060308773475924 ) ) ;
#96595 = CARTESIAN_POINT ( 'NONE',  ( 20.04142135623730070, 11.65000000001115943, -54.85000000000000142 ) ) ;
#96596 = ORIENTED_EDGE ( 'NONE', *, *, #57755, .F. ) ;
#96597 = DIRECTION ( 'NONE',  ( 1.000000000000000000, -7.304098846218134667E-16, -5.100424963727256530E-30 ) ) ;
#96598 = EDGE_CURVE ( 'NONE', #173665, #90836, #208158, .T. ) ;
#96599 = CARTESIAN_POINT ( 'NONE',  ( -5.899999999999938183, 64.25000000001119815, -25.92310748452479174 ) ) ;
#96600 =( BOUNDED_SURFACE ( )  B_SPLINE_SURFACE ( 3, 2, ( 
 ( #75713, #19590, #57399 ),
 ( #93967, #117394, #196923 ),
 ( #133113, #18291, #157849 ),
 ( #237348, #177400, #256846 ),
 ( #174854, #114823, #138215 ),
 ( #76975, #135655, #173572 ) ),
 .UNSPECIFIED., .F., .F., .F. ) 
 B_SPLINE_SURFACE_WITH_KNOTS ( ( 4, 2, 4 ),
 ( 3, 3 ),
 ( 0.0001300404313046487020, 0.0003183318589266567809, 0.0005066232865486648869 ),
 ( 0.000000000000000000, 1.000000000000000000 ),
 .UNSPECIFIED. ) 
 GEOMETRIC_REPRESENTATION_ITEM ( )  RATIONAL_B_SPLINE_SURFACE ( (
 ( 1.000000000000000000, 0.7071067811865732189, 1.000000000000000000),
 ( 1.000000000000000000, 0.7625113560535831114, 1.000000000000000000),
 ( 1.000000000000000000, 0.8126073484694227300, 1.000000000000000000),
 ( 1.000000000000000000, 0.8923049332726431526, 1.000000000000000000),
 ( 1.000000000000000000, 0.9231914937774265972, 1.000000000000000000),
 ( 1.000000000000000000, 0.9238795325112875156, 1.000000000000000000) ) ) 
 REPRESENTATION_ITEM ( '' )  SURFACE ( )  );
#96601 = VERTEX_POINT ( 'NONE', #123920 ) ;
#96602 = EDGE_LOOP ( 'NONE', ( #141548, #31315, #42776, #31561 ) ) ;
#96603 = LINE ( 'NONE', #116222, #44518 ) ;
#96604 = EDGE_LOOP ( 'NONE', ( #156699, #169413, #103036, #212685 ) ) ;
#96605 = ADVANCED_FACE ( 'NONE', ( #203449 ), #178787, .T. ) ;
#96606 = ORIENTED_EDGE ( 'NONE', *, *, #104249, .F. ) ;
#96608 = VERTEX_POINT ( 'NONE', #109458 ) ;
#96607 = CARTESIAN_POINT ( 'NONE',  ( -18.59999999999999787, 70.22889768795992893, -198.1282601183952750 ) ) ;
#96609 = EDGE_CURVE ( 'NONE', #210045, #198468, #28, .T. ) ;
#96610 = ORIENTED_EDGE ( 'NONE', *, *, #220571, .F. ) ;
#96611 = LINE ( 'NONE', #53668, #164147 ) ;
#96614 = ORIENTED_EDGE ( 'NONE', *, *, #30064, .T. ) ;
#96613 = ORIENTED_EDGE ( 'NONE', *, *, #247190, .F. ) ;
#96612 = CARTESIAN_POINT ( 'NONE',  ( 21.14999999999999858, 1.115600667400684642E-11, -79.15000000000004832 ) ) ;
#96615 = VECTOR ( 'NONE', #53494, 1000.000000000000227 ) ;
#96617 = ADVANCED_FACE ( 'NONE', ( #46911 ), #127765, .T. ) ;
#96616 = VERTEX_POINT ( 'NONE', #88602 ) ;
#96618 = DIRECTION ( 'NONE',  ( 0.000000000000000000, 0.8777080977375655291, -0.4791956752370622463 ) ) ;
#96619 = DIRECTION ( 'NONE',  ( -0.000000000000000000, -0.000000000000000000, -1.000000000000000000 ) ) ;
#96620 = VECTOR ( 'NONE', #149159, 1000.000000000000000 ) ;
#96621 = CARTESIAN_POINT ( 'NONE',  ( -20.54999999999999716, 12.46703344576493144, -249.9218526068032133 ) ) ;
#96622 = VERTEX_POINT ( 'NONE', #146025 ) ;
#96623 = CARTESIAN_POINT ( 'NONE',  ( -16.93344882324368683, 9.996588767299030565, -154.9130256948049578 ) ) ;
#96625 = ORIENTED_EDGE ( 'NONE', *, *, #181972, .F. ) ;
#96624 = CARTESIAN_POINT ( 'NONE',  ( 23.14999999999999503, 11.65000000000000746, -21.35000000000000142 ) ) ;
#96626 = DIRECTION ( 'NONE',  ( 1.000000000000000000, 0.000000000000000000, -0.000000000000000000 ) ) ;
#96628 = VERTEX_POINT ( 'NONE', #243844 ) ;
#96627 = CARTESIAN_POINT ( 'NONE',  ( 23.14999999999999503, 6.450000000011156587, -21.75000000000000355 ) ) ;
#96629 = EDGE_CURVE ( 'NONE', #173155, #252143, #207312, .T. ) ;
#96630 = ORIENTED_EDGE ( 'NONE', *, *, #50623, .T. ) ;
#96631 = CARTESIAN_POINT ( 'NONE',  ( -20.54999999999999716, 1.940186915899004161, -188.1708807889466470 ) ) ;
#96632 = PLANE ( 'NONE',  #107587 ) ;
#96633 = EDGE_CURVE ( 'NONE', #10839, #129734, #206014, .T. ) ;
#96634 = VECTOR ( 'NONE', #158605, 1000.000000000000227 ) ;
#96635 = ORIENTED_EDGE ( 'NONE', *, *, #249062, .F. ) ;
#96636 = ORIENTED_EDGE ( 'NONE', *, *, #156273, .T. ) ;
#96637 = CARTESIAN_POINT ( 'NONE',  ( -16.93970660449832977, 10.01284139164673270, -180.0522817357944234 ) ) ;
#96639 = ORIENTED_EDGE ( 'NONE', *, *, #60201, .F. ) ;
#96638 = VERTEX_POINT ( 'NONE', #249006 ) ;
#96640 = EDGE_LOOP ( 'NONE', ( #39460, #122415, #216104, #145041 ) ) ;
#96641 = DIRECTION ( 'NONE',  ( 0.000000000000000000, 0.9126074666063844765, 0.4088369013363113980 ) ) ;
#96642 = VERTEX_POINT ( 'NONE', #228150 ) ;
#96643 = ORIENTED_EDGE ( 'NONE', *, *, #194959, .F. ) ;
#96644 = CARTESIAN_POINT ( 'NONE',  ( 23.15000000000000213, -5.637547571910521249, -233.4427589080015650 ) ) ;
#96645 = EDGE_LOOP ( 'NONE', ( #227941, #83615, #125201, #36853 ) ) ;
#96646 = DIRECTION ( 'NONE',  ( 1.000000000000000000, 0.000000000000000000, 0.000000000000000000 ) ) ;
#96648 = CARTESIAN_POINT ( 'NONE',  ( -22.49436431346200038, 64.35004905235922479, -203.5900110142466986 ) ) ;
#96647 = DIRECTION ( 'NONE',  ( -0.000000000000000000, -0.000000000000000000, -1.000000000000000000 ) ) ;
#96649 = ADVANCED_FACE ( 'NONE', ( #86023 ), #186455, .F. ) ;
#96650 = EDGE_LOOP ( 'NONE', ( #50148, #214414, #112258 ) ) ;
#96651 = AXIS2_PLACEMENT_3D ( 'NONE', #216521, #237378, #15793 ) ;
#96652 = TOROIDAL_SURFACE ( 'NONE', #246531, 0.4000000000000005773, 0.1000000000000000056 ) ;
#96653 = ORIENTED_EDGE ( 'NONE', *, *, #40329, .F. ) ;
#96654 = AXIS2_PLACEMENT_3D ( 'NONE', #214219, #35609, #115112 ) ;
#96655 = VERTEX_POINT ( 'NONE', #226852 ) ;
#96656 = EDGE_CURVE ( 'NONE', #134584, #45686, #247702, .T. ) ;
#96657 = FACE_OUTER_BOUND ( 'NONE', #55556, .T. ) ;
#96658 = VERTEX_POINT ( 'NONE', #70384 ) ;
#96659 = ORIENTED_EDGE ( 'NONE', *, *, #131464, .F. ) ;
#96660 = CYLINDRICAL_SURFACE ( 'NONE', #171160, 0.09999999999999031886 ) ;
#96662 = ORIENTED_EDGE ( 'NONE', *, *, #218031, .T. ) ;
#96661 = CYLINDRICAL_SURFACE ( 'NONE', #187887, 0.1999999999999987899 ) ;
#96663 = CARTESIAN_POINT ( 'NONE',  ( -20.85000000000000142, -1.164121893230052995, -208.9148480855715775 ) ) ;
#96664 = DIRECTION ( 'NONE',  ( 0.000000000000000000, 0.9908441862701605762, 0.1350103645451835310 ) ) ;
#96665 = ORIENTED_EDGE ( 'NONE', *, *, #125377, .T. ) ;
#96666 = DIRECTION ( 'NONE',  ( 0.000000000000000000, 0.000000000000000000, -1.000000000000000000 ) ) ;
#96668 = ADVANCED_FACE ( 'NONE', ( #69085 ), #87325, .F. ) ;
#96667 = DIRECTION ( 'NONE',  ( 0.000000000000000000, 0.000000000000000000, 1.000000000000000000 ) ) ;
#96669 = AXIS2_PLACEMENT_3D ( 'NONE', #47434, #63147, #3170 ) ;
#96670 = DIRECTION ( 'NONE',  ( 1.020425574104004196E-15, 1.210927747993693964E-31, -1.000000000000000000 ) ) ;
#96671 = CARTESIAN_POINT ( 'NONE',  ( 20.94999999999999929, 69.06797323185276127, -247.4100621602722470 ) ) ;
#96672 = FACE_OUTER_BOUND ( 'NONE', #87201, .T. ) ;
#96673 = CARTESIAN_POINT ( 'NONE',  ( 21.06490991615909891, 65.27510865242517468, -157.8193961309912936 ) ) ;
#96674 = DIRECTION ( 'NONE',  ( 2.715809747126116508E-16, -1.000000000000000000, -1.629485848275670102E-15 ) ) ;
#96675 = CARTESIAN_POINT ( 'NONE',  ( -20.54999999999999716, -8.999999999988844479, -57.10603087734755690 ) ) ;
#96676 = CARTESIAN_POINT ( 'NONE',  ( -23.25000000000000000, 71.85000000001228670, -157.6731074845243654 ) ) ;
#96677 = EDGE_CURVE ( 'NONE', #22494, #126916, #148617, .T. ) ;
#96678 = ORIENTED_EDGE ( 'NONE', *, *, #80063, .F. ) ;
#96679 = B_SPLINE_CURVE_WITH_KNOTS ( 'NONE', 3,
 ( #231255, #252074, #31785, #34346, #109990, #30484, #192129, #73476, #113851, #232545 ),
 .UNSPECIFIED., .F., .F.,
 ( 4, 3, 3, 4 ),
 ( 0.000000000000000000, 0.0002000000000002894374, 0.001000000000045112372, 0.001967863649472102218 ),
 .UNSPECIFIED. ) ;
#96681 = VERTEX_POINT ( 'NONE', #5210 ) ;
#96680 = ORIENTED_EDGE ( 'NONE', *, *, #151024, .F. ) ;
#96682 = VERTEX_POINT ( 'NONE', #45655 ) ;
#96683 = DIRECTION ( 'NONE',  ( 0.000000000000000000, -1.000000000000000000, 0.000000000000000000 ) ) ;
#96684 = CIRCLE ( 'NONE', #150881, 0.5000000000000004441 ) ;
#96685 = EDGE_CURVE ( 'NONE', #114917, #53100, #225542, .T. ) ;
#96686 = CARTESIAN_POINT ( 'NONE',  ( -20.94999999999999929, 76.00000000001126921, -203.5231074845248997 ) ) ;
#96688 = DIRECTION ( 'NONE',  ( 1.000000000000000000, 0.000000000000000000, 0.000000000000000000 ) ) ;
#96687 = DIRECTION ( 'NONE',  ( -4.408576920032448588E-17, -0.9594490217226104845, -0.2818822000686205254 ) ) ;
#96689 = EDGE_LOOP ( 'NONE', ( #6905, #68141, #122862, #229592 ) ) ;
#96690 = AXIS2_PLACEMENT_3D ( 'NONE', #106697, #65016, #87137 ) ;
#96691 = EDGE_CURVE ( 'NONE', #17720, #63242, #246423, .T. ) ;
#96692 = CARTESIAN_POINT ( 'NONE',  ( -22.39999999999999858, 0.1000000000111554016, -159.7092204016265384 ) ) ;
#96693 = EDGE_CURVE ( 'NONE', #7829, #182906, #33392, .T. ) ;
#96694 = LINE ( 'NONE', #137146, #16826 ) ;
#96695 = AXIS2_PLACEMENT_3D ( 'NONE', #26075, #180017, #163024 ) ;
#96696 = CARTESIAN_POINT ( 'NONE',  ( 18.54999999999999716, 67.25000000001227818, -157.3731074845244393 ) ) ;
#96697 = CIRCLE ( 'NONE', #179950, 0.1000000000000028644 ) ;
#96698 = AXIS2_PLACEMENT_3D ( 'NONE', #51104, #227200, #30305 ) ;
#96699 = CARTESIAN_POINT ( 'NONE',  ( 18.45139536634708222, -9.486081720270041373, -73.64051161781067378 ) ) ;
#96700 = VERTEX_POINT ( 'NONE', #126469 ) ;
#96701 = ORIENTED_EDGE ( 'NONE', *, *, #235673, .F. ) ;
#96702 = CIRCLE ( 'NONE', #125765, 0.09999999999999939493 ) ;
#96703 = DIRECTION ( 'NONE',  ( 0.000000000000000000, 0.000000000000000000, 1.000000000000000000 ) ) ;
#96704 = EDGE_CURVE ( 'NONE', #47933, #221530, #67779, .T. ) ;
#96705 = VERTEX_POINT ( 'NONE', #26103 ) ;
#96706 = DIRECTION ( 'NONE',  ( 0.000000000000000000, 1.000000000000000000, 0.000000000000000000 ) ) ;
#96707 = CARTESIAN_POINT ( 'NONE',  ( 18.41815437325358573, 77.14150793766424385, -241.8237832882541625 ) ) ;
#96708 = DIRECTION ( 'NONE',  ( 0.000000000000000000, -6.982962677686266711E-15, 1.000000000000000000 ) ) ;
#96709 = EDGE_CURVE ( 'NONE', #222373, #211242, #204032, .T. ) ;
#96710 = CARTESIAN_POINT ( 'NONE',  ( -21.52071067811865746, 7.779289321892505882, -155.2500000000000284 ) ) ;
#96711 = DIRECTION ( 'NONE',  ( -0.000000000000000000, 1.000000000000000000, 6.352154140967427193E-15 ) ) ;
#96712 = EDGE_CURVE ( 'NONE', #164082, #253301, #245141, .T. ) ;
#96714 = CIRCLE ( 'NONE', #55195, 0.1000000000000013933 ) ;
#96713 = DIRECTION ( 'NONE',  ( -1.000000000000000000, -0.000000000000000000, 1.073024830501117725E-15 ) ) ;
#96715 = EDGE_LOOP ( 'NONE', ( #126908, #9691, #191567, #224014 ) ) ;
#96716 = DIRECTION ( 'NONE',  ( 0.000000000000000000, -0.3945274997758418944, 0.9188841341108372474 ) ) ;
#96717 = DIRECTION ( 'NONE',  ( -2.915501640297154776E-16, 0.4721928772777346794, 0.8814952561688429444 ) ) ;
#96718 = DIRECTION ( 'NONE',  ( 0.7071067811865475727, 0.7071067811865475727, -0.000000000000000000 ) ) ;
#96719 = TOROIDAL_SURFACE ( 'NONE', #146796, 0.2000000000000000111, 0.1000000000000000056 ) ;
#96721 = CARTESIAN_POINT ( 'NONE',  ( 21.05000000000000071, -11.48912529306490349, -136.9000000000000341 ) ) ;
#96720 = DIRECTION ( 'NONE',  ( 0.000000000000000000, -1.265107689135680095E-16, 1.000000000000000000 ) ) ;
#96722 = CARTESIAN_POINT ( 'NONE',  ( -20.64999999999999858, 73.60000000001204512, -123.2984855617622202 ) ) ;
#96724 = CARTESIAN_POINT ( 'NONE',  ( 21.13614978966381841, 1.115600741516067204E-11, -27.00089529816621337 ) ) ;
#96723 = VECTOR ( 'NONE', #115497, 1000.000000000000000 ) ;
#96725 = CIRCLE ( 'NONE', #113504, 2.000000000000000000 ) ;
#96726 = CARTESIAN_POINT ( 'NONE',  ( 18.49999999999999645, 70.30054753569086756, -182.5653814410942459 ) ) ;
#96727 = CARTESIAN_POINT ( 'NONE',  ( 13.99999999999999822, 66.15000000001204228, -119.7731074845243739 ) ) ;
#96728 = VECTOR ( 'NONE', #198104, 1000.000000000000000 ) ;
#96729 = ORIENTED_EDGE ( 'NONE', *, *, #22188, .T. ) ;
#96730 = CIRCLE ( 'NONE', #42590, 0.1999999999999945155 ) ;
#96731 = VERTEX_POINT ( 'NONE', #187748 ) ;
#96732 = DIRECTION ( 'NONE',  ( 1.000000000000000000, 0.000000000000000000, 0.000000000000000000 ) ) ;
#96733 = EDGE_CURVE ( 'NONE', #86681, #224268, #174880, .T. ) ;
#96734 = VERTEX_POINT ( 'NONE', #53353 ) ;
#96735 = EDGE_CURVE ( 'NONE', #204082, #245148, #91619, .T. ) ;
#96736 = AXIS2_PLACEMENT_3D ( 'NONE', #73966, #119486, #218549 ) ;
#96737 = DIRECTION ( 'NONE',  ( -0.000000000000000000, -1.265107689135680095E-16, 1.000000000000000000 ) ) ;
#96738 = EDGE_CURVE ( 'NONE', #146933, #122358, #151181, .T. ) ;
#96739 = DIRECTION ( 'NONE',  ( 0.000000000000000000, -1.000000000000000000, 0.000000000000000000 ) ) ;
#96740 = AXIS2_PLACEMENT_3D ( 'NONE', #142676, #98389, #162283 ) ;
#96741 = ORIENTED_EDGE ( 'NONE', *, *, #181861, .F. ) ;
#96742 = VECTOR ( 'NONE', #232565, 1000.000000000000000 ) ;
#96744 = LINE ( 'NONE', #253269, #84590 ) ;
#96743 = AXIS2_PLACEMENT_3D ( 'NONE', #176982, #219924, #221193 ) ;
#96745 = CARTESIAN_POINT ( 'NONE',  ( -14.56336952470180179, 9.446645344706404046, -51.91080645610022515 ) ) ;
#96746 = DIRECTION ( 'NONE',  ( -1.000000000000000000, -3.265361837132813093E-16, 0.000000000000000000 ) ) ;
#96747 = CARTESIAN_POINT ( 'NONE',  ( 18.49999999999999289, 10.32573593129922607, -192.3499999999999659 ) ) ;
#96749 = ORIENTED_EDGE ( 'NONE', *, *, #103639, .F. ) ;
#96748 = CARTESIAN_POINT ( 'NONE',  ( -16.87683809663752399, 9.950000000011137047, -187.5976359818036485 ) ) ;
#96751 = LINE ( 'NONE', #232469, #229424 ) ;
#96750 = DIRECTION ( 'NONE',  ( 1.000000000000000000, -2.849773892568378313E-16, 7.728835255496647986E-17 ) ) ;
#96752 = DIRECTION ( 'NONE',  ( -1.000000000000000000, -0.000000000000000000, -0.000000000000000000 ) ) ;
#96753 = DIRECTION ( 'NONE',  ( 0.000000000000000000, 0.000000000000000000, -1.000000000000000000 ) ) ;
#96754 = CARTESIAN_POINT ( 'NONE',  ( -19.99999999999999645, 5.472724050409169649, 16.54552871969761796 ) ) ;
#96755 = LINE ( 'NONE', #135892, #95817 ) ;
#96756 = ORIENTED_EDGE ( 'NONE', *, *, #170683, .T. ) ;
#96757 = ADVANCED_FACE ( 'NONE', ( #234554 ), #57172, .F. ) ;
#96758 = CARTESIAN_POINT ( 'NONE',  ( 0.000000000000000000, 0.000000000000000000, 0.000000000000000000 ) ) ;
#96759 = LINE ( 'NONE', #177650, #33533 ) ;
#96760 = ORIENTED_EDGE ( 'NONE', *, *, #142242, .T. ) ;
#96761 = EDGE_CURVE ( 'NONE', #123954, #243905, #14249, .T. ) ;
#96762 = FACE_OUTER_BOUND ( 'NONE', #228000, .T. ) ;
#96763 = CIRCLE ( 'NONE', #17672, 0.1000000000000028644 ) ;
#96764 = ORIENTED_EDGE ( 'NONE', *, *, #134117, .T. ) ;
#96765 = CARTESIAN_POINT ( 'NONE',  ( 21.05000000000000071, 36.69980811187836878, -249.6424234479061113 ) ) ;
#96766 = CARTESIAN_POINT ( 'NONE',  ( 23.24999999999999645, 76.00000000001165290, -69.52310748452431710 ) ) ;
#96767 = EDGE_CURVE ( 'NONE', #224623, #190789, #95699, .T. ) ;
#96768 = CARTESIAN_POINT ( 'NONE',  ( 21.05000000000005400, 65.36599112033563586, -30.02023607076051803 ) ) ;
#96769 = ORIENTED_EDGE ( 'NONE', *, *, #108778, .T. ) ;
#96770 = ORIENTED_EDGE ( 'NONE', *, *, #133629, .F. ) ;
#96771 = EDGE_CURVE ( 'NONE', #173885, #140050, #230719, .T. ) ;
#96772 = LINE ( 'NONE', #78512, #227654 ) ;
#96773 = DIRECTION ( 'NONE',  ( 0.000000000000000000, -0.9908441862701420355, -0.1350103645453197554 ) ) ;
#96774 = CARTESIAN_POINT ( 'NONE',  ( -16.92280123533710068, 63.03321624328317796, -213.3212588345534186 ) ) ;
#96775 = LINE ( 'NONE', #16017, #99379 ) ;
#96776 = EDGE_CURVE ( 'NONE', #30259, #46556, #199963, .T. ) ;
#96778 = CARTESIAN_POINT ( 'NONE',  ( 23.24999999999999645, 70.40000000001174385, -81.27310748452435973 ) ) ;
#96777 = CARTESIAN_POINT ( 'NONE',  ( -21.53752568622143571, 75.90102553874154978, -143.3099153590729031 ) ) ;
#96779 = CARTESIAN_POINT ( 'NONE',  ( -18.35663730107557257, 58.57862133557244988, -223.9242990443918302 ) ) ;
#96780 = CARTESIAN_POINT ( 'NONE',  ( -20.54999999999999716, 2.000000000011154189, -53.77537807723790309 ) ) ;
#96781 = DIRECTION ( 'NONE',  ( -1.836970198721029934E-16, 1.000000000000000000, 0.000000000000000000 ) ) ;
#96782 = ORIENTED_EDGE ( 'NONE', *, *, #29438, .F. ) ;
#96783 = CARTESIAN_POINT ( 'NONE',  ( 20.94999999999999929, 1.115600667400684642E-11, -67.00000000000000000 ) ) ;
#96784 = EDGE_CURVE ( 'NONE', #29239, #241214, #55889, .T. ) ;
#96785 = TOROIDAL_SURFACE ( 'NONE', #213323, 6.258578643762712446, 0.1000000000000000056 ) ;
#96787 = ORIENTED_EDGE ( 'NONE', *, *, #131899, .T. ) ;
#96786 = CARTESIAN_POINT ( 'NONE',  ( 23.14999999999999858, 71.00000000001199396, -115.4283735034374274 ) ) ;
#96788 = DIRECTION ( 'NONE',  ( 0.000000000000000000, 0.000000000000000000, -1.000000000000000000 ) ) ;
#96790 = EDGE_CURVE ( 'NONE', #256577, #102162, #224869, .T. ) ;
#96789 = ADVANCED_FACE ( 'NONE', ( #52048 ), #255344, .T. ) ;
#96791 = DIRECTION ( 'NONE',  ( -0.000000000000000000, 1.000000000000000000, -0.000000000000000000 ) ) ;
#96793 = DIRECTION ( 'NONE',  ( 0.000000000000000000, 0.8814952561688427224, -0.4721928772777352901 ) ) ;
#96792 = DIRECTION ( 'NONE',  ( -0.000000000000000000, -0.000000000000000000, -1.000000000000000000 ) ) ;
#96794 = ORIENTED_EDGE ( 'NONE', *, *, #28695, .T. ) ;
#96796 = DIRECTION ( 'NONE',  ( 1.000000000000000000, 0.000000000000000000, -0.000000000000000000 ) ) ;
#96795 = CARTESIAN_POINT ( 'NONE',  ( -21.05000000000000071, 1.736257131608553550, -145.5686523290175387 ) ) ;
#96797 = DIRECTION ( 'NONE',  ( 1.000000000000000000, -1.734723475976817507E-14, 0.000000000000000000 ) ) ;
#96798 = CARTESIAN_POINT ( 'NONE',  ( -20.07928932188135107, 66.77928932189333011, -115.2731074845243597 ) ) ;
#96799 = DIRECTION ( 'NONE',  ( 0.000000000000000000, -0.4721928772777380656, -0.8814952561688412791 ) ) ;
#96800 = ORIENTED_EDGE ( 'NONE', *, *, #67360, .F. ) ;
#96801 = DIRECTION ( 'NONE',  ( 1.000000000000000000, 0.000000000000000000, 0.000000000000000000 ) ) ;
#96802 = ORIENTED_EDGE ( 'NONE', *, *, #114094, .F. ) ;
#96804 = AXIS2_PLACEMENT_3D ( 'NONE', #154881, #191449, #132740 ) ;
#96803 = CARTESIAN_POINT ( 'NONE',  ( -18.44448725179914206, -9.490081715483329461, -40.12896029406248033 ) ) ;
#96805 = ORIENTED_EDGE ( 'NONE', *, *, #117314, .T. ) ;
#96806 = CYLINDRICAL_SURFACE ( 'NONE', #84476, 0.9000000000000014655 ) ;
#96807 = ADVANCED_FACE ( 'NONE', ( #174640 ), #113326, .T. ) ;
#96808 = EDGE_CURVE ( 'NONE', #15766, #90604, #88224, .T. ) ;
#96809 = EDGE_LOOP ( 'NONE', ( #37326, #7498, #135176, #49298 ) ) ;
#96810 = AXIS2_PLACEMENT_3D ( 'NONE', #79541, #59977, #139525 ) ;
#96811 = CARTESIAN_POINT ( 'NONE',  ( 18.59999999999999432, 16.60731133254646963, -240.9277311905271688 ) ) ;
#96812 = AXIS2_PLACEMENT_3D ( 'NONE', #230493, #90970, #170573 ) ;
#96813 = ADVANCED_FACE ( 'NONE', ( #195458 ), #213706, .F. ) ;
#96814 = LINE ( 'NONE', #176409, #84557 ) ;
#96815 = VERTEX_POINT ( 'NONE', #233298 ) ;
#96816 = EDGE_CURVE ( 'NONE', #211450, #240371, #29125, .T. ) ;
#96817 = DIRECTION ( 'NONE',  ( 2.978066053179066272E-16, 1.000000000000000000, 7.147358527629759053E-15 ) ) ;
#96818 = ADVANCED_FACE ( 'NONE', ( #134163 ), #96307, .T. ) ;
#96819 = CARTESIAN_POINT ( 'NONE',  ( -23.15000000000000213, 71.75000000001223555, -148.7731074845243882 ) ) ;
#96820 = CARTESIAN_POINT ( 'NONE',  ( -23.15000000000000213, -11.48912529307605368, -30.39999999999999503 ) ) ;
#96821 = TOROIDAL_SURFACE ( 'NONE', #117698, 2.100000000000002309, 0.1000000000000000056 ) ;
#96822 = CARTESIAN_POINT ( 'NONE',  ( -20.54999999999999716, 1.115600667400684642E-11, -167.4999999999999716 ) ) ;
#96823 = CARTESIAN_POINT ( 'NONE',  ( -20.64999999999999858, 1.115600667400684642E-11, -134.0000000000000000 ) ) ;
#96824 = ORIENTED_EDGE ( 'NONE', *, *, #79987, .F. ) ;
#96825 = CARTESIAN_POINT ( 'NONE',  ( -18.49372193242229301, 85.44248452337028255, -129.7583262244892808 ) ) ;
#96826 = VERTEX_POINT ( 'NONE', #214986 ) ;
#96828 = ORIENTED_EDGE ( 'NONE', *, *, #92904, .T. ) ;
#96827 = FACE_OUTER_BOUND ( 'NONE', #133906, .T. ) ;
#96829 = ORIENTED_EDGE ( 'NONE', *, *, #233697, .F. ) ;
#96830 = CARTESIAN_POINT ( 'NONE',  ( 23.24999999999999645, 0.000000000000000000, 0.000000000000000000 ) ) ;
#96831 = DIRECTION ( 'NONE',  ( -1.000000000000000000, -2.885090398161910739E-16, -6.283419270304611573E-17 ) ) ;
#96832 = DIRECTION ( 'NONE',  ( -1.000000000000000000, -0.000000000000000000, -0.000000000000000000 ) ) ;
#96833 = AXIS2_PLACEMENT_3D ( 'NONE', #198240, #97830, #78285 ) ;
#96834 = DIRECTION ( 'NONE',  ( -1.000000000000000000, 0.000000000000000000, 0.000000000000000000 ) ) ;
#96835 = ORIENTED_EDGE ( 'NONE', *, *, #97666, .F. ) ;
#96836 = EDGE_CURVE ( 'NONE', #251327, #234302, #91201, .T. ) ;
#96837 = DIRECTION ( 'NONE',  ( -0.000000000000000000, -0.4791956752371546724, -0.8777080977375153470 ) ) ;
#96838 = CARTESIAN_POINT ( 'NONE',  ( 20.04142135623730070, 64.35000000001150511, -48.17310748452440095 ) ) ;
#96839 = ORIENTED_EDGE ( 'NONE', *, *, #75537, .F. ) ;
#96840 = CIRCLE ( 'NONE', #105190, 0.1000000000000028644 ) ;
#96842 = ORIENTED_EDGE ( 'NONE', *, *, #181646, .T. ) ;
#96841 = CYLINDRICAL_SURFACE ( 'NONE', #92676, 0.09999999999999939493 ) ;
#96843 = AXIS2_PLACEMENT_3D ( 'NONE', #69025, #148551, #49441 ) ;
#96844 = CIRCLE ( 'NONE', #117724, 0.09999999999999939493 ) ;
#96845 = DIRECTION ( 'NONE',  ( 0.000000000000000000, 0.8700118002898321601, -0.4930308989875230030 ) ) ;
#96846 = AXIS2_PLACEMENT_3D ( 'NONE', #114661, #194228, #233353 ) ;
#96847 = EDGE_CURVE ( 'NONE', #47818, #191501, #175063, .T. ) ;
#96848 = DIRECTION ( 'NONE',  ( -1.000000000000000000, 0.000000000000000000, 0.000000000000000000 ) ) ;
#96849 = DIRECTION ( 'NONE',  ( 0.000000000000000000, -1.000000000000000000, -6.982962677686265922E-15 ) ) ;
#96850 = ORIENTED_EDGE ( 'NONE', *, *, #186174, .F. ) ;
#96851 = DIRECTION ( 'NONE',  ( -0.000000000000000000, -0.8814952561688430555, 0.4721928772777346239 ) ) ;
#96852 = ADVANCED_FACE ( 'NONE', ( #138002 ), #97577, .F. ) ;
#96853 = DIRECTION ( 'NONE',  ( 2.342056488767300981E-15, 0.8096735173027139743, -0.5868805631290339164 ) ) ;
#96854 = DIRECTION ( 'NONE',  ( 0.000000000000000000, 1.000000000000000000, 6.938893903907222067E-15 ) ) ;
#96855 = CARTESIAN_POINT ( 'NONE',  ( 23.25000000000000000, -8.999999999988842703, -90.60603087734760663 ) ) ;
#96856 = AXIS2_PLACEMENT_3D ( 'NONE', #113889, #31819, #111330 ) ;
#96857 = AXIS2_PLACEMENT_3D ( 'NONE', #126536, #27480, #186516 ) ;
#96858 = ADVANCED_FACE ( 'NONE', ( #256627 ), #129219, .T. ) ;
#96859 = ORIENTED_EDGE ( 'NONE', *, *, #139444, .F. ) ;
#96860 = DIRECTION ( 'NONE',  ( 0.000000000000000000, -7.056502275159890043E-15, 1.000000000000000000 ) ) ;
#96861 = ORIENTED_EDGE ( 'NONE', *, *, #123043, .T. ) ;
#96862 = LINE ( 'NONE', #215558, #31175 ) ;
#96863 = CARTESIAN_POINT ( 'NONE',  ( -22.57848426163147693, -0.004264329271961149644, -21.74994169310966541 ) ) ;
#96864 = AXIS2_PLACEMENT_3D ( 'NONE', #73620, #132273, #12358 ) ;
#96866 = ORIENTED_EDGE ( 'NONE', *, *, #244867, .F. ) ;
#96865 = CARTESIAN_POINT ( 'NONE',  ( 21.09793522318412684, 10.72462451022393282, -146.2392908709771575 ) ) ;
#96867 = CARTESIAN_POINT ( 'NONE',  ( -18.59999999999999787, 68.11287320386161070, -224.1382462126928488 ) ) ;
#96868 = DIRECTION ( 'NONE',  ( -0.000000000000000000, 1.000000000000000000, -0.000000000000000000 ) ) ;
#96869 = DIRECTION ( 'NONE',  ( 0.000000000000000000, 0.008583690987124100932, -0.9999631594459055250 ) ) ;
#96870 = CARTESIAN_POINT ( 'NONE',  ( -20.54999999999999716, 2.399999999999999467, -13.22462192276210224 ) ) ;
#96871 = AXIS2_PLACEMENT_3D ( 'NONE', #94526, #34589, #75010 ) ;
#96872 = CARTESIAN_POINT ( 'NONE',  ( 21.05000000000000071, 76.00000000001139711, -31.92310748452432279 ) ) ;
#96873 = CARTESIAN_POINT ( 'NONE',  ( -18.49346865148325492, 85.44307379853697171, -129.3379112292089417 ) ) ;
#96875 = ORIENTED_EDGE ( 'NONE', *, *, #164308, .T. ) ;
#96874 = CARTESIAN_POINT ( 'NONE',  ( -21.59780538579341069, 69.15290947006889155, -136.6220861541223428 ) ) ;
#96876 = AXIS2_PLACEMENT_3D ( 'NONE', #36352, #175856, #18041 ) ;
#96877 = CIRCLE ( 'NONE', #205226, 0.1000000000000028644 ) ;
#96878 = VECTOR ( 'NONE', #143503, 1000.000000000000000 ) ;
#96879 = CIRCLE ( 'NONE', #17783, 11.74999999999999645 ) ;
#96880 = AXIS2_PLACEMENT_3D ( 'NONE', #118414, #58394, #197923 ) ;
#96881 = FACE_OUTER_BOUND ( 'NONE', #221194, .T. ) ;
#96882 = DIRECTION ( 'NONE',  ( 0.000000000000000000, 0.2617529984165152257, 0.9651348961777124202 ) ) ;
#96883 = CARTESIAN_POINT ( 'NONE',  ( 21.53752568617673191, 69.21319212550805844, -103.1220819457950171 ) ) ;
#96884 = VECTOR ( 'NONE', #121797, 1000.000000000000000 ) ;
#96885 = ORIENTED_EDGE ( 'NONE', *, *, #33963, .F. ) ;
#96886 = CARTESIAN_POINT ( 'NONE',  ( 18.59999999999999076, 15.28205413790855971, -223.0019049476732675 ) ) ;
#96887 = CIRCLE ( 'NONE', #34594, 11.70000000000000284 ) ;
#96888 = ADVANCED_FACE ( 'NONE', ( #161455 ), #21102, .F. ) ;
#96889 = CARTESIAN_POINT ( 'NONE',  ( -22.57320508075687115, 64.25000000001237765, -170.0231074845244166 ) ) ;
#96890 = AXIS2_PLACEMENT_3D ( 'NONE', #234207, #217202, #58123 ) ;
#96891 = ORIENTED_EDGE ( 'NONE', *, *, #228523, .F. ) ;
#96892 = CARTESIAN_POINT ( 'NONE',  ( -23.25000000000000000, -8.596261682231835621, -176.9501275171502641 ) ) ;
#96893 = VECTOR ( 'NONE', #32546, 1000.000000000000000 ) ;
#96894 = VECTOR ( 'NONE', #95543, 1000.000000000000000 ) ;
#96896 = VECTOR ( 'NONE', #160467, 1000.000000000000000 ) ;
#96895 = CARTESIAN_POINT ( 'NONE',  ( -16.93772744219066340, 66.00645889126025168, -190.9250455125547035 ) ) ;
#96897 = VERTEX_POINT ( 'NONE', #140579 ) ;
#96898 = VECTOR ( 'NONE', #25289, 1000.000000000000000 ) ;
#96899 = LINE ( 'NONE', #94358, #52681 ) ;
#96900 = ORIENTED_EDGE ( 'NONE', *, *, #191736, .T. ) ;
#96901 = EDGE_CURVE ( 'NONE', #254691, #153829, #108551, .T. ) ;
#96902 = DIRECTION ( 'NONE',  ( 1.000000000000000000, 0.000000000000000000, 0.000000000000000000 ) ) ;
#96904 = VERTEX_POINT ( 'NONE', #196704 ) ;
#96903 = CARTESIAN_POINT ( 'NONE',  ( 22.10000000000000497, 6.223900101154161923, 12.09999999999999964 ) ) ;
#96906 = EDGE_CURVE ( 'NONE', #195729, #69727, #79302, .T. ) ;
#96905 = FACE_OUTER_BOUND ( 'NONE', #38923, .T. ) ;
#96907 = ORIENTED_EDGE ( 'NONE', *, *, #89012, .F. ) ;
#96908 = DIRECTION ( 'NONE',  ( 0.000000000000000000, -3.729655473350132098E-14, -1.000000000000000000 ) ) ;
#96909 = VERTEX_POINT ( 'NONE', #221385 ) ;
#96911 = ORIENTED_EDGE ( 'NONE', *, *, #107918, .F. ) ;
#96910 = VERTEX_POINT ( 'NONE', #121063 ) ;
#96912 = LINE ( 'NONE', #55223, #123678 ) ;
#96913 = ORIENTED_EDGE ( 'NONE', *, *, #133041, .F. ) ;
#96914 = CARTESIAN_POINT ( 'NONE',  ( -20.94999999999999929, 70.15000000001192859, -92.89061026024637613 ) ) ;
#96917 = EDGE_CURVE ( 'NONE', #69180, #218291, #37654, .T. ) ;
#96916 = EDGE_LOOP ( 'NONE', ( #220202, #246098, #83354, #220218 ) ) ;
#96915 = AXIS2_PLACEMENT_3D ( 'NONE', #126435, #5175, #48178 ) ;
#96918 = AXIS2_PLACEMENT_3D ( 'NONE', #180915, #2250, #947 ) ;
#96919 = VECTOR ( 'NONE', #101415, 1000.000000000000227 ) ;
#96920 = EDGE_CURVE ( 'NONE', #183881, #241131, #62587, .T. ) ;
#96921 = EDGE_CURVE ( 'NONE', #124804, #178010, #212614, .T. ) ;
#96922 = VERTEX_POINT ( 'NONE', #257912 ) ;
#96923 = CARTESIAN_POINT ( 'NONE',  ( -20.94999999999999929, 87.39257802171783851, -139.5970570643562212 ) ) ;
#96924 = CARTESIAN_POINT ( 'NONE',  ( 21.40925344232283223, 75.90104981139204199, -76.18162634391477184 ) ) ;
#96925 = DIRECTION ( 'NONE',  ( -0.7071067811865389130, 8.659560562355038861E-17, -0.7071067811865561215 ) ) ;
#96926 = DIRECTION ( 'NONE',  ( 1.000000000000000000, -0.000000000000000000, -0.000000000000000000 ) ) ;
#96927 = ORIENTED_EDGE ( 'NONE', *, *, #2289, .F. ) ;
#96928 = EDGE_CURVE ( 'NONE', #97342, #119120, #201843, .T. ) ;
#96929 = CARTESIAN_POINT ( 'NONE',  ( -20.94999999999999929, 1.835341550235569663, -78.55515129256303908 ) ) ;
#96930 = CARTESIAN_POINT ( 'NONE',  ( 23.14999999999999858, -1.999999999988846699, -67.00000000000000000 ) ) ;
#96931 = LINE ( 'NONE', #176526, #218812 ) ;
#96932 = ORIENTED_EDGE ( 'NONE', *, *, #93916, .F. ) ;
#96933 = CYLINDRICAL_SURFACE ( 'NONE', #54563, 0.09999999999999939493 ) ;
#96934 = DIRECTION ( 'NONE',  ( 0.000000000000000000, 0.000000000000000000, -1.000000000000000000 ) ) ;
#96935 = CARTESIAN_POINT ( 'NONE',  ( 21.05000000000000071, 65.57661458509917907, -129.0310555606542664 ) ) ;
#96936 = EDGE_CURVE ( 'NONE', #246557, #200447, #12718, .T. ) ;
#96937 = EDGE_LOOP ( 'NONE', ( #183050, #73457, #168778, #36404, #65432 ) ) ;
#96939 = CARTESIAN_POINT ( 'NONE',  ( -16.92925196614874750, 66.02766820360174904, -90.40636263680760010 ) ) ;
#96938 = AXIS2_PLACEMENT_3D ( 'NONE', #33275, #93198, #9814 ) ;
#96940 = ORIENTED_EDGE ( 'NONE', *, *, #125030, .F. ) ;
#96941 = ORIENTED_EDGE ( 'NONE', *, *, #10692, .T. ) ;
#96942 = DIRECTION ( 'NONE',  ( -0.000000000000000000, 1.000000000000000000, 6.982962677686266711E-15 ) ) ;
#96943 = ORIENTED_EDGE ( 'NONE', *, *, #190156, .F. ) ;
#96944 = CIRCLE ( 'NONE', #205104, 0.09999999999999939493 ) ;
#96945 = ORIENTED_EDGE ( 'NONE', *, *, #9068, .T. ) ;
#96946 = DIRECTION ( 'NONE',  ( 1.000000000000000000, 0.000000000000000000, 0.000000000000000000 ) ) ;
#96947 = DIRECTION ( 'NONE',  ( -1.000000000000000000, -0.000000000000000000, -0.000000000000000000 ) ) ;
#96948 = ORIENTED_EDGE ( 'NONE', *, *, #212283, .F. ) ;
#96949 = ADVANCED_FACE ( 'NONE', ( #242245 ), #177186, .F. ) ;
#96950 = ORIENTED_EDGE ( 'NONE', *, *, #216588, .T. ) ;
#96951 = DIRECTION ( 'NONE',  ( 1.000000000000000000, 0.000000000000000000, 0.000000000000000000 ) ) ;
#96952 = CARTESIAN_POINT ( 'NONE',  ( 18.59999999999999787, 5.900000000011102586, -144.2190997646564483 ) ) ;
#96953 = EDGE_CURVE ( 'NONE', #211183, #195803, #237127, .T. ) ;
#96954 = ORIENTED_EDGE ( 'NONE', *, *, #58426, .F. ) ;
#96955 = ORIENTED_EDGE ( 'NONE', *, *, #86590, .F. ) ;
#96956 = ORIENTED_EDGE ( 'NONE', *, *, #155569, .T. ) ;
#96957 = AXIS2_PLACEMENT_3D ( 'NONE', #163540, #27915, #1867 ) ;
#96958 = CARTESIAN_POINT ( 'NONE',  ( 23.14999999999999858, 70.40000000001253966, -182.4283735034374843 ) ) ;
#96959 = EDGE_CURVE ( 'NONE', #117714, #95434, #145953, .T. ) ;
#96960 = LINE ( 'NONE', #256018, #17973 ) ;
#96961 = DIRECTION ( 'NONE',  ( 0.000000000000000000, 0.8814952561688434995, -0.4721928772777335137 ) ) ;
#96962 = CARTESIAN_POINT ( 'NONE',  ( 23.25000000000000000, -11.64999999998883595, -197.8999999999999773 ) ) ;
#96963 = CARTESIAN_POINT ( 'NONE',  ( 20.94999999999999929, 6.550000000000000711, -12.15000000000000036 ) ) ;
#96964 = CARTESIAN_POINT ( 'NONE',  ( -22.49806830649814415, 11.64988965485023620, -66.92253568367453909 ) ) ;
#96965 = DIRECTION ( 'NONE',  ( -0.000000000000000000, 1.000000000000000000, 6.982962677686266711E-15 ) ) ;
#96967 = DIRECTION ( 'NONE',  ( 0.000000000000000000, 0.000000000000000000, 1.000000000000000000 ) ) ;
#96966 = CARTESIAN_POINT ( 'NONE',  ( 21.04999999999999716, 75.98528214348812071, -75.86783088861417923 ) ) ;
#96968 = CARTESIAN_POINT ( 'NONE',  ( -20.90000000000000213, -11.65000000000000036, 0.000000000000000000 ) ) ;
#96969 = CARTESIAN_POINT ( 'NONE',  ( -18.59999999999999787, 30.14024212288317628, -235.5657495473015501 ) ) ;
#96970 = VECTOR ( 'NONE', #104802, 1000.000000000000000 ) ;
#96971 = DIRECTION ( 'NONE',  ( 0.000000000000000000, 0.000000000000000000, 1.000000000000000000 ) ) ;
#96972 = DIRECTION ( 'NONE',  ( -1.000000000000000000, 0.000000000000000000, -0.000000000000000000 ) ) ;
#96973 = ORIENTED_EDGE ( 'NONE', *, *, #55824, .F. ) ;
#96974 = ADVANCED_FACE ( 'NONE', ( #59740 ), #139280, .T. ) ;
#96975 = AXIS2_PLACEMENT_3D ( 'NONE', #101196, #105046, #120842 ) ;
#96977 = EDGE_LOOP ( 'NONE', ( #203227, #19683, #158798, #45285 ) ) ;
#96976 = DIRECTION ( 'NONE',  ( 0.000000000000000000, 0.000000000000000000, -1.000000000000000000 ) ) ;
#96978 = ADVANCED_FACE ( 'NONE', ( #20663 ), #195880, .T. ) ;
#96979 = CARTESIAN_POINT ( 'NONE',  ( 21.00000000000000000, 9.749999999999998224, -21.15000000000000213 ) ) ;
#96980 = FACE_OUTER_BOUND ( 'NONE', #247701, .T. ) ;
#96981 = ORIENTED_EDGE ( 'NONE', *, *, #179744, .F. ) ;
#96982 = VECTOR ( 'NONE', #200632, 1000.000000000000114 ) ;
#96983 = ADVANCED_FACE ( 'NONE', ( #28385 ), #229181, .T. ) ;
#96985 = AXIS2_PLACEMENT_3D ( 'NONE', #162714, #25756, #223937 ) ;
#96984 = FILL_AREA_STYLE ('',( #134842 ) ) ;
#96986 = ADVANCED_FACE ( 'NONE', ( #127448 ), #124883, .F. ) ;
#96987 = B_SPLINE_CURVE_WITH_KNOTS ( 'NONE', 3,
 ( #48196, #45641, #125181, #9074, #247686, #148598, #84717, #228134, #49488, #185145, #129032, #208581, #189001, #10376 ),
 .UNSPECIFIED., .F., .F.,
 ( 4, 2, 2, 2, 2, 2, 4 ),
 ( 2.797157557069881010E-17, 0.0003823333598417795291, 0.0005735000397626551991, 0.0006690833797230931424, 0.0007168750497033133610, 0.0007407708846934235244, 0.0007646667196835337963 ),
 .UNSPECIFIED. ) ;
#96989 = VECTOR ( 'NONE', #119306, 999.9999999999998863 ) ;
#96988 = FACE_OUTER_BOUND ( 'NONE', #238972, .T. ) ;
#96990 = CARTESIAN_POINT ( 'NONE',  ( -16.90202395485727394, 66.03405545546317512, -157.4261212057837440 ) ) ;
#96991 = EDGE_CURVE ( 'NONE', #249371, #29748, #58450, .T. ) ;
#96992 = EDGE_LOOP ( 'NONE', ( #194986, #129027, #162775, #199206 ) ) ;
#96993 = CARTESIAN_POINT ( 'NONE',  ( -21.14999999893415250, 11.75000000001115197, -140.8444953435266314 ) ) ;
#96994 = CARTESIAN_POINT ( 'NONE',  ( -20.64999999999999858, 7.150000000000000355, -12.34999999999999964 ) ) ;
#96995 = EDGE_CURVE ( 'NONE', #59523, #71575, #84415, .T. ) ;
#96996 = VECTOR ( 'NONE', #804, 1000.000000000000000 ) ;
#96997 = CARTESIAN_POINT ( 'NONE',  ( -21.09610168723073542, 10.11132180231042810, -228.0938213842520383 ) ) ;
#96999 = EDGE_LOOP ( 'NONE', ( #147734, #158255, #196085, #131600, #215717, #213427, #22006, #174424, #185329, #78298, #161480, #192565, #66277, #110158, #84674, #130779, #113912, #240350 ) ) ;
#96998 = DIRECTION ( 'NONE',  ( 0.000000000000000000, 0.000000000000000000, -1.000000000000000000 ) ) ;
#97001 = EDGE_LOOP ( 'NONE', ( #199006, #172703, #241545, #204751, #79059, #155143, #55, #236151 ) ) ;
#97000 = CARTESIAN_POINT ( 'NONE',  ( -18.49372193242234275, 85.44248452336996991, -96.25832622448969289 ) ) ;
#97002 = AXIS2_PLACEMENT_3D ( 'NONE', #246890, #223472, #224754 ) ;
#97003 = FACE_OUTER_BOUND ( 'NONE', #89941, .T. ) ;
#97005 = CARTESIAN_POINT ( 'NONE',  ( -19.99999999999999645, 5.488301202077012775, 16.50000000000000000 ) ) ;
#97004 = CIRCLE ( 'NONE', #201110, 0.1999999999999987899 ) ;
#97006 = VECTOR ( 'NONE', #128940, 1000.000000000000000 ) ;
#97007 = CARTESIAN_POINT ( 'NONE',  ( 21.05000000000000071, 5.000000000011153745, -146.4052660189131245 ) ) ;
#97008 = FACE_OUTER_BOUND ( 'NONE', #192553, .T. ) ;
#97009 = VECTOR ( 'NONE', #197500, 1000.000000000000000 ) ;
#97011 = LINE ( 'NONE', #176612, #74499 ) ;
#97010 = DIRECTION ( 'NONE',  ( 0.000000000000000000, 6.769652589177795712E-15, -1.000000000000000000 ) ) ;
#97012 = CARTESIAN_POINT ( 'NONE',  ( -21.05000000000000071, 34.04033409713371583, -243.8666379817185543 ) ) ;
#97013 = SPHERICAL_SURFACE ( 'NONE', #103844, 0.1000000000000000056 ) ;
#97014 = CARTESIAN_POINT ( 'NONE',  ( -18.48408745364673678, 85.66432225867556838, -163.3400289511960466 ) ) ;
#97015 = CARTESIAN_POINT ( 'NONE',  ( 21.11101077988997332, 10.14857762567122457, -228.0630360965454315 ) ) ;
#97016 = VERTEX_POINT ( 'NONE', #243535 ) ;
#97017 = EDGE_CURVE ( 'NONE', #19526, #135831, #87003, .T. ) ;
#97018 = CARTESIAN_POINT ( 'NONE',  ( 21.04999999999999361, 0.01471785653522959120, -94.15527659591015208 ) ) ;
#97019 = ORIENTED_EDGE ( 'NONE', *, *, #56358, .T. ) ;
#97020 = ORIENTED_EDGE ( 'NONE', *, *, #130371, .F. ) ;
#97021 = LINE ( 'NONE', #74966, #44440 ) ;
#97022 = CARTESIAN_POINT ( 'NONE',  ( -22.50000000000000000, 55.89093952297024970, -232.7795287750844579 ) ) ;
#97023 = EDGE_CURVE ( 'NONE', #71184, #107478, #220965, .T. ) ;
#97024 = EDGE_LOOP ( 'NONE', ( #42130, #230465, #61570, #110086 ) ) ;
#97025 = ADVANCED_FACE ( 'NONE', ( #6200 ), #128738, .F. ) ;
#97026 = EDGE_LOOP ( 'NONE', ( #137960, #97311, #32941 ) ) ;
#97027 = CIRCLE ( 'NONE', #242815, 0.1000000000000028644 ) ;
#97028 = CIRCLE ( 'NONE', #242817, 5.000000000000000888 ) ;
#97029 = ORIENTED_EDGE ( 'NONE', *, *, #223705, .F. ) ;
#97030 = ORIENTED_EDGE ( 'NONE', *, *, #170322, .F. ) ;
#97031 = LINE ( 'NONE', #236572, #17358 ) ;
#97032 = DIRECTION ( 'NONE',  ( 0.7070776581708965169, 0.000000000000000000, 0.7071359030027827286 ) ) ;
#97033 = DIRECTION ( 'NONE',  ( 1.000000000000000000, 0.000000000000000000, 0.000000000000000000 ) ) ;
#97034 = CARTESIAN_POINT ( 'NONE',  ( 14.77516762759922031, 9.436674251842843475, -15.17686193099920722 ) ) ;
#97035 = CIRCLE ( 'NONE', #213796, 0.09999999999998898659 ) ;
#97036 = AXIS2_PLACEMENT_3D ( 'NONE', #151573, #135811, #52423 ) ;
#97037 = CARTESIAN_POINT ( 'NONE',  ( 21.05000000000000071, 76.00000000001244871, -170.0231074845243597 ) ) ;
#97038 = CARTESIAN_POINT ( 'NONE',  ( -21.05000000000000071, -1.249999999988843369, -75.00000000000004263 ) ) ;
#97040 = ORIENTED_EDGE ( 'NONE', *, *, #202684, .F. ) ;
#97039 = DIRECTION ( 'NONE',  ( 0.000000000000000000, 6.982962677686266711E-15, -1.000000000000000000 ) ) ;
#97042 = DIRECTION ( 'NONE',  ( 1.000000000000000000, 0.000000000000000000, 0.000000000000000000 ) ) ;
#97041 = DIRECTION ( 'NONE',  ( -1.000000000000000000, 0.000000000000000000, 0.000000000000000000 ) ) ;
#97043 = DIRECTION ( 'NONE',  ( 0.000000000000000000, 0.000000000000000000, -1.000000000000000000 ) ) ;
#97044 = VERTEX_POINT ( 'NONE', #29661 ) ;
#97045 = VECTOR ( 'NONE', #139442, 1000.000000000000000 ) ;
#97046 = DIRECTION ( 'NONE',  ( 0.000000000000000000, -0.9908441862701600211, -0.1350103645451876666 ) ) ;
#97047 = CARTESIAN_POINT ( 'NONE',  ( -23.25000000000000000, 36.65892442174935439, -249.5511627012433848 ) ) ;
#97048 = ORIENTED_EDGE ( 'NONE', *, *, #146914, .F. ) ;
#97049 = ADVANCED_FACE ( 'NONE', ( #222673 ), #85707, .F. ) ;
#97050 = VECTOR ( 'NONE', #107844, 1000.000000000000000 ) ;
#97052 = CARTESIAN_POINT ( 'NONE',  ( 22.60000000000000142, 75.89914163091303578, -81.27267460801371612 ) ) ;
#97051 = DIRECTION ( 'NONE',  ( 0.000000000000000000, -0.2617529984165152257, -0.9651348961777124202 ) ) ;
#97053 = AXIS2_PLACEMENT_3D ( 'NONE', #36102, #215987, #170521 ) ;
#97054 = DIRECTION ( 'NONE',  ( 1.000000000000000000, -0.000000000000000000, -0.000000000000000000 ) ) ;
#97055 = CARTESIAN_POINT ( 'NONE',  ( 21.05000000000000071, -0.09999999998884338825, -167.4999999999999716 ) ) ;
#97056 = ORIENTED_EDGE ( 'NONE', *, *, #109345, .F. ) ;
#97057 = EDGE_LOOP ( 'NONE', ( #1856, #145473, #202248, #197699 ) ) ;
#97058 = AXIS2_PLACEMENT_3D ( 'NONE', #92107, #114241, #150798 ) ;
#97059 = DIRECTION ( 'NONE',  ( 1.000000000000000000, 0.000000000000000000, 0.000000000000000000 ) ) ;
#97060 = CARTESIAN_POINT ( 'NONE',  ( -18.49372193242242446, -0.6578241932036854589, -242.3519091605612630 ) ) ;
#97061 = DIRECTION ( 'NONE',  ( 0.000000000000000000, -1.000000000000000000, -6.982962677686265922E-15 ) ) ;
#97062 = CARTESIAN_POINT ( 'NONE',  ( 20.94999999999999929, 4.813084112160680661, -78.94151775652387926 ) ) ;
#97063 = ORIENTED_EDGE ( 'NONE', *, *, #181939, .F. ) ;
#97065 = CIRCLE ( 'NONE', #167874, 0.09999999999999799327 ) ;
#97064 = CARTESIAN_POINT ( 'NONE',  ( -23.25000000000000000, -11.64999999998884483, -131.0000000000000284 ) ) ;
#97066 = EDGE_CURVE ( 'NONE', #56126, #150070, #211180, .T. ) ;
#97067 = DIRECTION ( 'NONE',  ( 0.000000000000000000, 0.9651348961777157509, -0.2617529984165031243 ) ) ;
#97068 = TOROIDAL_SURFACE ( 'NONE', #151314, 0.2000000000000000111, 0.1000000000000000056 ) ;
#97069 = CARTESIAN_POINT ( 'NONE',  ( -20.94999999999999929, 87.65000000001192859, -99.92310748452422331 ) ) ;
#97070 = EDGE_CURVE ( 'NONE', #155655, #182610, #204218, .T. ) ;
#97071 = DIRECTION ( 'NONE',  ( 0.000000000000000000, 0.9126074666063751506, 0.4088369013363322146 ) ) ;
#97072 = VECTOR ( 'NONE', #251228, 1000.000000000000000 ) ;
#97073 = TOROIDAL_SURFACE ( 'NONE', #109591, 4.149999999999999467, 0.1000000000000000056 ) ;
#97074 = AXIS2_PLACEMENT_3D ( 'NONE', #215892, #58102, #76385 ) ;
#97075 = EDGE_CURVE ( 'NONE', #118789, #122630, #8598, .T. ) ;
#97077 = ORIENTED_EDGE ( 'NONE', *, *, #4485, .F. ) ;
#97076 = LINE ( 'NONE', #181797, #133763 ) ;
#97078 = AXIS2_PLACEMENT_3D ( 'NONE', #137206, #197172, #58921 ) ;
#97079 = DIRECTION ( 'NONE',  ( 1.000000000000000000, -0.000000000000000000, -0.000000000000000000 ) ) ;
#97080 = EDGE_CURVE ( 'NONE', #2800, #197139, #47893, .T. ) ;
#97081 = CARTESIAN_POINT ( 'NONE',  ( 21.05000000000000071, 8.815452279208711772, -142.4203925526142882 ) ) ;
#97082 = DIRECTION ( 'NONE',  ( -0.000000000000000000, 0.000000000000000000, -1.000000000000000000 ) ) ;
#97083 = CARTESIAN_POINT ( 'NONE',  ( -20.94999999999994600, 64.25000000001119815, -30.12310748452479103 ) ) ;
#97084 = CARTESIAN_POINT ( 'NONE',  ( 20.95262331984772430, 10.50415726280109219, -175.0608883295932401 ) ) ;
#97086 = ORIENTED_EDGE ( 'NONE', *, *, #238737, .F. ) ;
#97085 = CARTESIAN_POINT ( 'NONE',  ( 21.72449340488910252, 10.28395627749112151, -12.65000000000000568 ) ) ;
#97087 = DIRECTION ( 'NONE',  ( -0.7071067811865456854, 0.7071067811865493491, 0.000000000000000000 ) ) ;
#97088 = CARTESIAN_POINT ( 'NONE',  ( 20.94999999999999929, 87.65000000001215597, -139.5231074845243029 ) ) ;
#97089 = CARTESIAN_POINT ( 'NONE',  ( 20.87600722750343252, 67.49230083716666684, -195.4236814984208763 ) ) ;
#97090 = ORIENTED_EDGE ( 'NONE', *, *, #205819, .T. ) ;
#97091 = DIRECTION ( 'NONE',  ( -1.020425574104004196E-15, 6.982962677686266711E-15, -1.000000000000000000 ) ) ;
#97092 = CARTESIAN_POINT ( 'NONE',  ( 21.05000000000000071, 76.09999993531950224, -176.5011857056192639 ) ) ;
#97093 = PLANE ( 'NONE',  #29800 ) ;
#97094 = DIRECTION ( 'NONE',  ( -0.8191520442889921316, -0.5735764363510457153, 0.000000000000000000 ) ) ;
#97095 = CARTESIAN_POINT ( 'NONE',  ( -18.40000000000000213, 78.24390740893980478, -231.6169762517609456 ) ) ;
#97096 = AXIS2_PLACEMENT_3D ( 'NONE', #213033, #235176, #39575 ) ;
#97097 = CIRCLE ( 'NONE', #1456, 0.09999999999999939493 ) ;
#97098 = CARTESIAN_POINT ( 'NONE',  ( -23.25000000000000000, 0.000000000000000000, -33.50000000000000000 ) ) ;
#97100 = EDGE_CURVE ( 'NONE', #83901, #179299, #33874, .T. ) ;
#97099 = TOROIDAL_SURFACE ( 'NONE', #255308, 0.2000000000000000111, 0.1000000000000000056 ) ;
#97101 = AXIS2_PLACEMENT_3D ( 'NONE', #126148, #23247, #223967 ) ;
#97102 = EDGE_CURVE ( 'NONE', #217847, #128659, #252513, .T. ) ;
#97103 = VERTEX_POINT ( 'NONE', #12657 ) ;
#97104 = VERTEX_POINT ( 'NONE', #129989 ) ;
#97105 = FACE_OUTER_BOUND ( 'NONE', #86020, .T. ) ;
#97106 = CARTESIAN_POINT ( 'NONE',  ( 21.05000000000000071, -11.74999999998883560, -197.8999999999999773 ) ) ;
#97107 = CARTESIAN_POINT ( 'NONE',  ( -21.65000000000000213, 7.708578643773852157, -146.3500000000000227 ) ) ;
#97108 = DIRECTION ( 'NONE',  ( 1.000000000000000000, 2.952720810173289112E-16, -0.000000000000000000 ) ) ;
#97109 = VERTEX_POINT ( 'NONE', #213388 ) ;
#97110 = PLANE ( 'NONE',  #150945 ) ;
#97111 = CARTESIAN_POINT ( 'NONE',  ( -18.59999999999999787, 7.661991824395936845, -241.5144583139544636 ) ) ;
#97112 = EDGE_CURVE ( 'NONE', #42158, #149408, #141854, .T. ) ;
#97113 = DIRECTION ( 'NONE',  ( 0.000000000000000000, 0.000000000000000000, -1.000000000000000000 ) ) ;
#97114 = EDGE_CURVE ( 'NONE', #218153, #28211, #29479, .T. ) ;
#97115 = CARTESIAN_POINT ( 'NONE',  ( -18.79999999999999716, 7.973296578895943121, -1.410778198689825791 ) ) ;
#97116 = ORIENTED_EDGE ( 'NONE', *, *, #156373, .T. ) ;
#97117 = CARTESIAN_POINT ( 'NONE',  ( -23.25000000000000000, 64.35000000001156195, -57.37310748452439668 ) ) ;
#97118 = EDGE_LOOP ( 'NONE', ( #54929, #180937 ) ) ;
#97119 = ORIENTED_EDGE ( 'NONE', *, *, #156256, .F. ) ;
#97120 = LINE ( 'NONE', #138821, #226170 ) ;
#97121 = CARTESIAN_POINT ( 'NONE',  ( -16.92507428761700439, 66.05000000001187743, -90.30971002490282729 ) ) ;
#97122 = VERTEX_POINT ( 'NONE', #75198 ) ;
#97123 = EDGE_CURVE ( 'NONE', #115218, #248248, #104248, .T. ) ;
#97124 = LINE ( 'NONE', #77578, #223996 ) ;
#97125 = DIRECTION ( 'NONE',  ( 0.000000000000000000, 0.8814952561688444987, -0.4721928772777320149 ) ) ;
#97126 = DIRECTION ( 'NONE',  ( -1.000000000000000000, 0.000000000000000000, -0.000000000000000000 ) ) ;
#97127 = EDGE_LOOP ( 'NONE', ( #52674, #112089, #164312, #200559 ) ) ;
#97128 = CARTESIAN_POINT ( 'NONE',  ( -20.54999999999999716, 9.690755012883057518, -211.4266134137857023 ) ) ;
#97130 = ORIENTED_EDGE ( 'NONE', *, *, #216596, .T. ) ;
#97129 = CARTESIAN_POINT ( 'NONE',  ( 18.49999999999999289, 65.74999999739320344, -145.3359355348928261 ) ) ;
#97131 = DIRECTION ( 'NONE',  ( 1.000000000000000000, 0.000000000000000000, 0.000000000000000000 ) ) ;
#97132 = DIRECTION ( 'NONE',  ( 2.840903330521633255E-16, -0.8700118002898322711, 0.4930308989875231696 ) ) ;
#97133 = ADVANCED_FACE ( 'NONE', ( #96002 ), #45999, .T. ) ;
#97134 = CIRCLE ( 'NONE', #189340, 0.09999999999998898659 ) ;
#97135 = CIRCLE ( 'NONE', #205502, 7.899999999999995914 ) ;
#97136 = ORIENTED_EDGE ( 'NONE', *, *, #245899, .T. ) ;
#97137 = CARTESIAN_POINT ( 'NONE',  ( -23.25000000000000000, 76.00000000001169553, -67.42310748452430857 ) ) ;
#97138 = DIRECTION ( 'NONE',  ( -6.938893903907209445E-14, -0.9999176327611370985, -0.01283462868040260302 ) ) ;
#97139 = CARTESIAN_POINT ( 'NONE',  ( -21.65000000000000213, 9.950000000011138823, -180.2499999999999716 ) ) ;
#97140 = ORIENTED_EDGE ( 'NONE', *, *, #52212, .T. ) ;
#97141 = CARTESIAN_POINT ( 'NONE',  ( 21.08078803292165659, 6.333012964448272442, -133.9208140128422144 ) ) ;
#97142 = EDGE_CURVE ( 'NONE', #139646, #208712, #150085, .T. ) ;
#97143 = CARTESIAN_POINT ( 'NONE',  ( 22.48660254037843842, 55.97436536266719997, -232.8539608197349935 ) ) ;
#97144 = CARTESIAN_POINT ( 'NONE',  ( -18.50000000000000711, 18.86061765788380740, -226.6874733728449485 ) ) ;
#97145 = VERTEX_POINT ( 'NONE', #133860 ) ;
#97146 = VECTOR ( 'NONE', #98427, 999.9999999999998863 ) ;
#97147 = ORIENTED_EDGE ( 'NONE', *, *, #15764, .F. ) ;
#97148 = VECTOR ( 'NONE', #59340, 1000.000000000000000 ) ;
#97149 = TOROIDAL_SURFACE ( 'NONE', #38961, 0.4000000000000003553, 0.1000000000000000056 ) ;
#97150 = ORIENTED_EDGE ( 'NONE', *, *, #167437, .F. ) ;
#97151 = CARTESIAN_POINT ( 'NONE',  ( -16.88460203013675454, 9.954759003246872240, -87.86589180953826883 ) ) ;
#97152 = DIRECTION ( 'NONE',  ( 1.000000000000000000, 0.000000000000000000, 0.000000000000000000 ) ) ;
#97154 = ORIENTED_EDGE ( 'NONE', *, *, #129430, .T. ) ;
#97153 = DIRECTION ( 'NONE',  ( 0.000000000000000000, 0.2128009952263602567, -0.9770955615653315052 ) ) ;
#97155 = DIRECTION ( 'NONE',  ( 1.000000000000000000, 0.000000000000000000, -0.000000000000000000 ) ) ;
#97156 = DIRECTION ( 'NONE',  ( 0.000000000000000000, 1.000000000000000000, 0.000000000000000000 ) ) ;
#97157 = DIRECTION ( 'NONE',  ( 0.000000000000000000, 0.000000000000000000, 1.000000000000000000 ) ) ;
#97158 = CARTESIAN_POINT ( 'NONE',  ( -18.46907102845853643, 85.47372736477574051, -62.84707274578772740 ) ) ;
#97159 = CARTESIAN_POINT ( 'NONE',  ( -21.10000000000000142, 6.223900101154156594, 12.09999999999999964 ) ) ;
#97160 = VECTOR ( 'NONE', #55632, 1000.000000000000000 ) ;
#97161 = DIRECTION ( 'NONE',  ( 1.000000000000000000, -0.000000000000000000, -0.000000000000000000 ) ) ;
#97163 = ORIENTED_EDGE ( 'NONE', *, *, #193060, .T. ) ;
#97162 = DIRECTION ( 'NONE',  ( 1.000000000000000000, 0.000000000000000000, 0.000000000000000000 ) ) ;
#97165 = ORIENTED_EDGE ( 'NONE', *, *, #230785, .F. ) ;
#97164 = FACE_OUTER_BOUND ( 'NONE', #180454, .T. ) ;
#97168 = DIRECTION ( 'NONE',  ( -0.000000000000000000, -0.4721928772777351790, -0.8814952561688427224 ) ) ;
#97167 = CARTESIAN_POINT ( 'NONE',  ( -20.94999999999999929, 74.73821383144760944, -195.4366085209788935 ) ) ;
#97166 = CIRCLE ( 'NONE', #105563, 0.1000000000000028644 ) ;
#97170 = VERTEX_POINT ( 'NONE', #209553 ) ;
#97169 = LINE ( 'NONE', #132497, #247341 ) ;
#97171 = EDGE_LOOP ( 'NONE', ( #88217, #180558 ) ) ;
#97172 = DIRECTION ( 'NONE',  ( -1.000000000000000000, 0.000000000000000000, 0.000000000000000000 ) ) ;
#97173 = DIRECTION ( 'NONE',  ( 1.000000000000000000, 0.000000000000000000, 0.000000000000000000 ) ) ;
#97174 = DIRECTION ( 'NONE',  ( 0.000000000000000000, -0.1568667991644355497, -0.9876197685951332295 ) ) ;
#97175 = AXIS2_PLACEMENT_3D ( 'NONE', #123362, #191056, #250980 ) ;
#97176 = DIRECTION ( 'NONE',  ( 1.000000000000000000, 0.000000000000000000, -0.000000000000000000 ) ) ;
#97177 = CARTESIAN_POINT ( 'NONE',  ( -23.25000000000000000, 71.85000000001259934, -191.1731074845243654 ) ) ;
#97178 = FACE_OUTER_BOUND ( 'NONE', #247088, .T. ) ;
#97179 = TOROIDAL_SURFACE ( 'NONE', #59792, 0.2000000000000000111, 0.1000000000000000056 ) ;
#97180 = AXIS2_PLACEMENT_3D ( 'NONE', #54905, #173649, #253107 ) ;
#97181 = AXIS2_PLACEMENT_3D ( 'NONE', #34373, #67361, #113877 ) ;
#97183 = CIRCLE ( 'NONE', #89218, 11.79999999999999361 ) ;
#97182 = CARTESIAN_POINT ( 'NONE',  ( -23.15000000000000213, 76.00000000001169553, -67.52310748452430289 ) ) ;
#97184 = ORIENTED_EDGE ( 'NONE', *, *, #173188, .T. ) ;
#97185 = ORIENTED_EDGE ( 'NONE', *, *, #205661, .F. ) ;
#97186 = EDGE_CURVE ( 'NONE', #105103, #173457, #30949, .T. ) ;
#97187 = FACE_OUTER_BOUND ( 'NONE', #47562, .T. ) ;
#97188 = ORIENTED_EDGE ( 'NONE', *, *, #184085, .T. ) ;
#97189 = CARTESIAN_POINT ( 'NONE',  ( 18.59999999999999076, 66.34920340998563404, -213.7018660128499334 ) ) ;
#97190 = CARTESIAN_POINT ( 'NONE',  ( 18.59999999999996945, 68.11287320386161070, -224.1382462126928488 ) ) ;
#97191 = CARTESIAN_POINT ( 'NONE',  ( -14.11697426661281263, 66.54258905524415013, -54.52302351073435460 ) ) ;
#97192 = CARTESIAN_POINT ( 'NONE',  ( -21.07016717457010557, -1.345102501103331294, -194.8238367621760858 ) ) ;
#97193 = ORIENTED_EDGE ( 'NONE', *, *, #131418, .T. ) ;
#97194 = EDGE_CURVE ( 'NONE', #215622, #164805, #111736, .T. ) ;
#97195 = CARTESIAN_POINT ( 'NONE',  ( -15.06720934482788365, 66.58230930894893618, -118.3815067877597897 ) ) ;
#97196 = ORIENTED_EDGE ( 'NONE', *, *, #249679, .F. ) ;
#97197 = CARTESIAN_POINT ( 'NONE',  ( -18.59999999999999787, -1.135018845910178431, -41.21697688343231647 ) ) ;
#97198 = VERTEX_POINT ( 'NONE', #53035 ) ;
#97199 = EDGE_CURVE ( 'NONE', #64371, #87242, #192413, .T. ) ;
#97200 = DIRECTION ( 'NONE',  ( 1.000000000000000000, -3.151514657663852580E-16, 8.547182517843351137E-17 ) ) ;
#97201 = DIRECTION ( 'NONE',  ( 0.000000000000000000, 6.982962677686266711E-15, -1.000000000000000000 ) ) ;
#97202 = AXIS2_PLACEMENT_3D ( 'NONE', #225758, #45858, #241497 ) ;
#97203 = CARTESIAN_POINT ( 'NONE',  ( 18.79999999999999716, 1.885425182446133663, -11.49641995933507843 ) ) ;
#97204 = ORIENTED_EDGE ( 'NONE', *, *, #130588, .F. ) ;
#97205 = AXIS2_PLACEMENT_3D ( 'NONE', #117587, #200980, #118888 ) ;
#97206 = DIRECTION ( 'NONE',  ( 1.000000000000000000, 0.000000000000000000, 0.000000000000000000 ) ) ;
#97208 = EDGE_LOOP ( 'NONE', ( #44724, #240881, #104456, #105859, #245766, #19622, #181755, #73446, #14292, #244970 ) ) ;
#97207 = CARTESIAN_POINT ( 'NONE',  ( 23.50000000000005684, 83.80000000001119531, -51.02310748452479316 ) ) ;
#97209 = CIRCLE ( 'NONE', #235207, 0.09999999999999939493 ) ;
#97210 = CARTESIAN_POINT ( 'NONE',  ( -21.05000000000000071, 64.40000000001147384, -42.95131071479990936 ) ) ;
#97211 = ORIENTED_EDGE ( 'NONE', *, *, #143665, .T. ) ;
#97212 = VECTOR ( 'NONE', #51008, 1000.000000000000000 ) ;
#97213 = EDGE_CURVE ( 'NONE', #181336, #4366, #254882, .T. ) ;
#97214 = CIRCLE ( 'NONE', #172342, 0.1000000000000028644 ) ;
#97215 = DIRECTION ( 'NONE',  ( 0.000000000000000000, -1.000000000000000000, 0.000000000000000000 ) ) ;
#97216 = EDGE_CURVE ( 'NONE', #138262, #1820, #121699, .T. ) ;
#97217 = VERTEX_POINT ( 'NONE', #76446 ) ;
#97218 = DIRECTION ( 'NONE',  ( 0.000000000000000000, 0.000000000000000000, 1.000000000000000000 ) ) ;
#97219 = FACE_OUTER_BOUND ( 'NONE', #177383, .T. ) ;
#97220 = FACE_OUTER_BOUND ( 'NONE', #116757, .T. ) ;
#97221 = CARTESIAN_POINT ( 'NONE',  ( 18.58222699835054570, 67.49225400653517681, -195.4205142095401584 ) ) ;
#97222 = AXIS2_PLACEMENT_3D ( 'NONE', #181177, #82020, #164174 ) ;
#97223 = EDGE_CURVE ( 'NONE', #242821, #41483, #27874, .T. ) ;
#97224 = CARTESIAN_POINT ( 'NONE',  ( -21.09813707148783379, 0.03135149954059018862, -60.61493789426336321 ) ) ;
#97225 = CIRCLE ( 'NONE', #72348, 0.1000000000000024342 ) ;
#97226 = VERTEX_POINT ( 'NONE', #164672 ) ;
#97227 = TOROIDAL_SURFACE ( 'NONE', #151477, 7.800000000000000711, 0.1000000000000000056 ) ;
#97228 = CARTESIAN_POINT ( 'NONE',  ( 20.94999999999999929, 70.60000000001259934, -191.1178414656113205 ) ) ;
#97229 = CARTESIAN_POINT ( 'NONE',  ( 21.05000000000021743, 6.344359042054673381, -100.4851443651061942 ) ) ;
#97231 = CARTESIAN_POINT ( 'NONE',  ( -5.900000000000003020, -11.75000000000000000, 10.10000000000000142 ) ) ;
#97230 = CIRCLE ( 'NONE', #255456, 0.09999999999999939493 ) ;
#97232 = EDGE_LOOP ( 'NONE', ( #146059, #33932, #197314, #48298 ) ) ;
#97233 = CARTESIAN_POINT ( 'NONE',  ( 20.94999999999999929, 9.290509600414956992, -221.0404682250134840 ) ) ;
#97234 = ORIENTED_EDGE ( 'NONE', *, *, #64242, .F. ) ;
#97235 = CARTESIAN_POINT ( 'NONE',  ( 23.15000000000000213, 11.43341603104965110, -245.8667934851861787 ) ) ;
#97237 = EDGE_LOOP ( 'NONE', ( #194961, #179820, #210403, #52714 ) ) ;
#97236 = AXIS2_PLACEMENT_3D ( 'NONE', #114596, #196685, #93744 ) ;
#97238 = ADVANCED_FACE ( 'NONE', ( #223338 ), #5564, .F. ) ;
#97239 = CARTESIAN_POINT ( 'NONE',  ( 20.94999999999999929, 70.50000000001253397, -182.4283735034374843 ) ) ;
#97240 = DIRECTION ( 'NONE',  ( 0.000000000000000000, -6.454785026890489601E-15, 1.000000000000000000 ) ) ;
#97242 = EDGE_LOOP ( 'NONE', ( #141581, #195053, #7117, #241628, #105125, #35287, #211126, #130950, #10212, #100515 ) ) ;
#97241 = DIRECTION ( 'NONE',  ( 1.000000000000000000, 0.000000000000000000, 0.000000000000000000 ) ) ;
#97243 = DIRECTION ( 'NONE',  ( 0.000000000000000000, -0.4791956752371546169, -0.8777080977375152360 ) ) ;
#97244 = ORIENTED_EDGE ( 'NONE', *, *, #251905, .T. ) ;
#97245 = CIRCLE ( 'NONE', #151490, 0.1000000000000000472 ) ;
#97246 = CARTESIAN_POINT ( 'NONE',  ( 18.39999999999999503, 11.75000000001113953, -46.15000000000000568 ) ) ;
#97247 = DIRECTION ( 'NONE',  ( -1.000000000000000000, -9.792504721693619684E-16, -4.386921467590155985E-16 ) ) ;
#97249 = ADVANCED_FACE ( 'NONE', ( #65559 ), #53236, .T. ) ;
#97248 = ORIENTED_EDGE ( 'NONE', *, *, #116006, .T. ) ;
#97250 = ORIENTED_EDGE ( 'NONE', *, *, #182493, .T. ) ;
#97251 = AXIS2_PLACEMENT_3D ( 'NONE', #109163, #71360, #230413 ) ;
#97252 = DIRECTION ( 'NONE',  ( -0.000000000000000000, -0.8814952561688430555, 0.4721928772777346239 ) ) ;
#97253 = CARTESIAN_POINT ( 'NONE',  ( 20.95159278453404639, 67.09210366206283993, -94.53838729941513463 ) ) ;
#97254 = ORIENTED_EDGE ( 'NONE', *, *, #226337, .T. ) ;
#97255 = CARTESIAN_POINT ( 'NONE',  ( -20.64999999999999858, 71.75000000001229239, -157.6731074845243654 ) ) ;
#97257 = ORIENTED_EDGE ( 'NONE', *, *, #112456, .T. ) ;
#97256 = VECTOR ( 'NONE', #163706, 1000.000000000000114 ) ;
#97258 = VERTEX_POINT ( 'NONE', #102091 ) ;
#97259 = AXIS2_PLACEMENT_3D ( 'NONE', #83761, #159508, #239030 ) ;
#97260 = DIRECTION ( 'NONE',  ( 1.000000000000000000, 0.000000000000000000, 0.000000000000000000 ) ) ;
#97261 = AXIS2_PLACEMENT_3D ( 'NONE', #210994, #67941, #34955 ) ;
#97262 = DIRECTION ( 'NONE',  ( -1.000000000000000000, -3.265361837132813093E-16, 0.000000000000000000 ) ) ;
#97263 = APPLICATION_CONTEXT ( 'automotive_design' ) ;
#97265 = ORIENTED_EDGE ( 'NONE', *, *, #77470, .T. ) ;
#97264 = CARTESIAN_POINT ( 'NONE',  ( 18.50000000000000711, 85.41920976342116489, -95.77533802176530742 ) ) ;
#97266 = DIRECTION ( 'NONE',  ( 1.000000000000000000, 0.000000000000000000, 0.000000000000000000 ) ) ;
#97267 = DIRECTION ( 'NONE',  ( 1.000000000000000000, 1.875376730785737719E-16, 0.000000000000000000 ) ) ;
#97268 = DIRECTION ( 'NONE',  ( 0.000000000000000000, -0.9126074666064696306, -0.4088369013361213278 ) ) ;
#97269 = LINE ( 'NONE', #76456, #169428 ) ;
#97270 = CARTESIAN_POINT ( 'NONE',  ( -20.54999999999999716, 74.07476635515219243, -115.7533510176504450 ) ) ;
#97271 = DIRECTION ( 'NONE',  ( 0.000000000000000000, 0.9803012954743849372, 0.1975078988072195840 ) ) ;
#97272 = AXIS2_PLACEMENT_3D ( 'NONE', #31569, #229732, #225843 ) ;
#97273 = DIRECTION ( 'NONE',  ( -2.342056488767301376E-15, -0.1350103645451904977, 0.9908441862701596881 ) ) ;
#97274 = AXIS2_PLACEMENT_3D ( 'NONE', #12266, #10964, #150483 ) ;
#97275 = CARTESIAN_POINT ( 'NONE',  ( 22.59080734064467677, 11.75000000001115552, -133.9692502919029380 ) ) ;
#97276 = CIRCLE ( 'NONE', #193015, 11.80000000000000426 ) ;
#97277 = VECTOR ( 'NONE', #150861, 1000.000000000000000 ) ;
#97278 = ORIENTED_EDGE ( 'NONE', *, *, #38315, .T. ) ;
#97279 = ORIENTED_EDGE ( 'NONE', *, *, #219735, .T. ) ;
#97280 = EDGE_CURVE ( 'NONE', #117708, #235384, #104650, .T. ) ;
#97281 = ADVANCED_FACE ( 'NONE', ( #220786 ), #200788, .F. ) ;
#97283 = ORIENTED_EDGE ( 'NONE', *, *, #184409, .T. ) ;
#97282 = DIRECTION ( 'NONE',  ( -1.000000000000000000, -0.000000000000000000, -0.000000000000000000 ) ) ;
#97284 = EDGE_LOOP ( 'NONE', ( #86934, #107995, #79410, #20449 ) ) ;
#97285 = CARTESIAN_POINT ( 'NONE',  ( -21.05000000000000071, 14.00000000001115374, -95.07290746961757577 ) ) ;
#97286 =( BOUNDED_SURFACE ( )  B_SPLINE_SURFACE ( 3, 2, ( 
 ( #134070, #153709, #213613 ),
 ( #196615, #233211, #114523 ),
 ( #256536, #75425, #16720 ),
 ( #113234, #14165, #94944 ),
 ( #15439, #174553, #135351 ),
 ( #214900, #57084, #157542 ) ),
 .UNSPECIFIED., .F., .F., .F. ) 
 B_SPLINE_SURFACE_WITH_KNOTS ( ( 4, 2, 4 ),
 ( 3, 3 ),
 ( 0.0001792624049599557520, 0.0003686986002124558403, 0.0005581347954649559014 ),
 ( 0.000000000000000000, 1.000000000000000000 ),
 .UNSPECIFIED. ) 
 GEOMETRIC_REPRESENTATION_ITEM ( )  RATIONAL_B_SPLINE_SURFACE ( (
 ( 1.000000000000000000, 0.9238795325112858503, 1.000000000000000000),
 ( 1.000000000000000000, 0.9229318695231540914, 1.000000000000000000),
 ( 1.000000000000000000, 0.8926288119239994545, 1.000000000000000000),
 ( 1.000000000000000000, 0.8123777807262057005, 1.000000000000000000),
 ( 1.000000000000000000, 0.7629087100938296562, 1.000000000000000000),
 ( 1.000000000000000000, 0.7071067811865966446, 1.000000000000000000) ) ) 
 REPRESENTATION_ITEM ( '' )  SURFACE ( )  );
#97287 = ORIENTED_EDGE ( 'NONE', *, *, #66648, .T. ) ;
#97288 = CARTESIAN_POINT ( 'NONE',  ( -33.72168855820451938, 9.950000000011156587, -188.3500000000000227 ) ) ;
#97289 = ADVANCED_FACE ( 'NONE', ( #44728 ), #42164, .T. ) ;
#97290 = ADVANCED_FACE ( 'NONE', ( #143805 ), #103380, .T. ) ;
#97291 = EDGE_LOOP ( 'NONE', ( #70762, #12854, #210408, #15862 ) ) ;
#97292 = EDGE_CURVE ( 'NONE', #113568, #60596, #179952, .T. ) ;
#97293 = SURFACE_SIDE_STYLE ('',( #96037 ) ) ;
#97294 = CARTESIAN_POINT ( 'NONE',  ( -18.59999999999999787, 77.26178616857691850, -94.93660852097882241 ) ) ;
#97295 = EDGE_CURVE ( 'NONE', #123863, #9710, #184205, .T. ) ;
#97297 = EDGE_LOOP ( 'NONE', ( #241873, #67906, #55219, #125444 ) ) ;
#97296 = ORIENTED_EDGE ( 'NONE', *, *, #50583, .F. ) ;
#97298 = EDGE_LOOP ( 'NONE', ( #101591, #129840, #152793 ) ) ;
#97300 = EDGE_CURVE ( 'NONE', #143470, #147289, #62991, .T. ) ;
#97299 = EDGE_CURVE ( 'NONE', #92030, #223374, #204869, .T. ) ;
#97301 = VERTEX_POINT ( 'NONE', #83797 ) ;
#97302 = ORIENTED_EDGE ( 'NONE', *, *, #247710, .T. ) ;
#97303 = DIRECTION ( 'NONE',  ( 0.000000000000000000, -0.1335171055202867274, -0.9910465087640866200 ) ) ;
#97304 = VECTOR ( 'NONE', #127998, 1000.000000000000000 ) ;
#97305 = CARTESIAN_POINT ( 'NONE',  ( -22.94999999999999929, -1.786320531569725478, -11.50977166988710820 ) ) ;
#97307 = ORIENTED_EDGE ( 'NONE', *, *, #162636, .F. ) ;
#97306 = CARTESIAN_POINT ( 'NONE',  ( -20.94999999999999929, 65.70729864261004138, -97.56574559737244101 ) ) ;
#97308 = CARTESIAN_POINT ( 'NONE',  ( 20.94999999999999929, 1.115600667400684642E-11, -46.37500000000000000 ) ) ;
#97309 = CARTESIAN_POINT ( 'NONE',  ( 14.87567385445976598, 12.45583213463953420, -213.8748143118951646 ) ) ;
#97311 = ORIENTED_EDGE ( 'NONE', *, *, #12578, .T. ) ;
#97310 = CARTESIAN_POINT ( 'NONE',  ( 20.95512820512820440, 10.62384868372303615, -141.6649135690876165 ) ) ;
#97312 = DIRECTION ( 'NONE',  ( 0.000000000000000000, 0.9126074666063791474, 0.4088369013363231108 ) ) ;
#97313 = EDGE_LOOP ( 'NONE', ( #160704, #105916, #127264, #153517 ) ) ;
#97315 = ORIENTED_EDGE ( 'NONE', *, *, #86325, .F. ) ;
#97314 = DIRECTION ( 'NONE',  ( -1.000000000000000000, 0.000000000000000000, 0.000000000000000000 ) ) ;
#97316 = DIRECTION ( 'NONE',  ( 1.000000000000000000, 0.000000000000000000, 0.000000000000000000 ) ) ;
#97318 = EDGE_CURVE ( 'NONE', #208842, #152772, #250842, .T. ) ;
#97317 = CARTESIAN_POINT ( 'NONE',  ( 18.49999999999999645, 36.65892442174935439, -249.5511627012433848 ) ) ;
#97319 = CARTESIAN_POINT ( 'NONE',  ( -17.11825945287481687, 9.950000000011140600, -87.85000000000005116 ) ) ;
#97320 = ORIENTED_EDGE ( 'NONE', *, *, #250917, .F. ) ;
#97322 = DIRECTION ( 'NONE',  ( 1.186688945009010077E-16, 0.9651348961777157509, -0.2617529984165031243 ) ) ;
#97321 = CARTESIAN_POINT ( 'NONE',  ( -16.92280123533723213, 9.950000000011137047, -46.35063231408512507 ) ) ;
#97323 = EDGE_CURVE ( 'NONE', #117767, #42156, #42564, .T. ) ;
#97325 = EDGE_CURVE ( 'NONE', #175273, #39343, #71815, .T. ) ;
#97324 = VECTOR ( 'NONE', #55193, 1000.000000000000000 ) ;
#97326 = CARTESIAN_POINT ( 'NONE',  ( 21.76363531954645936, 7.012936547882880234, -133.9009981257005961 ) ) ;
#97327 = VECTOR ( 'NONE', #246316, 1000.000000000000000 ) ;
#97328 = DIRECTION ( 'NONE',  ( 1.000000000000000000, 0.000000000000000000, 0.000000000000000000 ) ) ;
#97329 = DIRECTION ( 'NONE',  ( 0.7071359030027940529, 0.000000000000000000, -0.7070776581708850816 ) ) ;
#97330 = EDGE_LOOP ( 'NONE', ( #73258, #39264, #186103, #180573 ) ) ;
#97332 = ORIENTED_EDGE ( 'NONE', *, *, #130311, .F. ) ;
#97331 = CIRCLE ( 'NONE', #76510, 0.1000000000000054040 ) ;
#97333 = EDGE_CURVE ( 'NONE', #86374, #248733, #125763, .T. ) ;
#97334 = DIRECTION ( 'NONE',  ( 0.000000000000000000, -0.9594490217226103734, -0.2818822000686205254 ) ) ;
#97335 = CARTESIAN_POINT ( 'NONE',  ( 20.94999999999999929, -4.259020970815407203, -226.0869574510824123 ) ) ;
#97336 = ORIENTED_EDGE ( 'NONE', *, *, #224165, .T. ) ;
#97337 = DIRECTION ( 'NONE',  ( 0.000000000000000000, -1.000000000000000000, -0.000000000000000000 ) ) ;
#97338 = ORIENTED_EDGE ( 'NONE', *, *, #99381, .T. ) ;
#97339 = CARTESIAN_POINT ( 'NONE',  ( -20.54999999999999716, -9.399999999988846611, -57.10603087734755690 ) ) ;
#97340 = CARTESIAN_POINT ( 'NONE',  ( -21.55000000000000426, 7.708578643762696636, -21.15000000000000213 ) ) ;
#97341 = EDGE_CURVE ( 'NONE', #167581, #166958, #75888, .T. ) ;
#97342 = VERTEX_POINT ( 'NONE', #165979 ) ;
#97343 = TOROIDAL_SURFACE ( 'NONE', #55646, 11.90000000000000391, 0.1000000000000000056 ) ;
#97344 = CARTESIAN_POINT ( 'NONE',  ( -18.59999999999999787, 77.83585931145498193, -24.51866831572578675 ) ) ;
#97345 = AXIS2_PLACEMENT_3D ( 'NONE', #99146, #254365, #40523 ) ;
#97346 = EDGE_LOOP ( 'NONE', ( #148400, #244388, #27681, #164866 ) ) ;
#97347 = VERTEX_POINT ( 'NONE', #9436 ) ;
#97348 = VERTEX_POINT ( 'NONE', #250609 ) ;
#97349 = CIRCLE ( 'NONE', #72467, 0.1000000000000124678 ) ;
#97350 = CARTESIAN_POINT ( 'NONE',  ( 19.97071067811864609, 64.27928932189330169, -111.8731074845243825 ) ) ;
#97351 = CYLINDRICAL_SURFACE ( 'NONE', #3367, 0.09999999999999939493 ) ;
#97352 = DIRECTION ( 'NONE',  ( 1.000000000000000000, 7.304098846218134667E-16, -0.000000000000000000 ) ) ;
#97353 = DIRECTION ( 'NONE',  ( 0.000000000000000000, -0.1495327102803792052, -0.9887567792719320625 ) ) ;
#97354 = FACE_OUTER_BOUND ( 'NONE', #210264, .T. ) ;
#97356 = CARTESIAN_POINT ( 'NONE',  ( 23.15000000000000213, 87.75000000001247713, -173.1231074845242688 ) ) ;
#97355 = DIRECTION ( 'NONE',  ( 1.000000000000000000, 0.000000000000000000, 0.000000000000000000 ) ) ;
#97357 = CARTESIAN_POINT ( 'NONE',  ( 18.54999999999999716, 67.25000000001251976, -182.6731074845244223 ) ) ;
#97359 = ORIENTED_EDGE ( 'NONE', *, *, #255932, .T. ) ;
#97358 = DIRECTION ( 'NONE',  ( 0.000000000000000000, 1.000000000000000000, -1.387778780781444413E-14 ) ) ;
#97360 = CARTESIAN_POINT ( 'NONE',  ( -16.86379686415369861, 9.975217759264314310, -79.56661011090976388 ) ) ;
#97361 = ORIENTED_EDGE ( 'NONE', *, *, #126659, .T. ) ;
#97362 = CARTESIAN_POINT ( 'NONE',  ( 23.24999999999999289, 64.25000000001269029, -203.4231074845244507 ) ) ;
#97363 = VERTEX_POINT ( 'NONE', #69436 ) ;
#97364 = ORIENTED_EDGE ( 'NONE', *, *, #10589, .F. ) ;
#97365 = CARTESIAN_POINT ( 'NONE',  ( -16.93344882324368683, 66.00341123272364996, -48.61008178971947302 ) ) ;
#97367 = CIRCLE ( 'NONE', #239053, 0.09999999999999939493 ) ;
#97366 = CARTESIAN_POINT ( 'NONE',  ( -21.05000000000000071, 69.20602499728043711, -247.8456586332460176 ) ) ;
#97368 = DIRECTION ( 'NONE',  ( 0.000000000000000000, 0.4930308989875575865, 0.8700118002898125091 ) ) ;
#97369 = AXIS2_PLACEMENT_3D ( 'NONE', #144428, #105293, #56737 ) ;
#97370 = ORIENTED_EDGE ( 'NONE', *, *, #205141, .F. ) ;
#97371 = AXIS2_PLACEMENT_3D ( 'NONE', #95626, #193471, #16130 ) ;
#97372 = SPHERICAL_SURFACE ( 'NONE', #100998, 0.1000000000000000056 ) ;
#97373 = EDGE_LOOP ( 'NONE', ( #20133, #10870, #60979, #207704 ) ) ;
#97374 = ORIENTED_EDGE ( 'NONE', *, *, #189177, .T. ) ;
#97375 = DIRECTION ( 'NONE',  ( 0.000000000000000000, -0.8814952561688476074, 0.4721928772777262417 ) ) ;
#97376 = ORIENTED_EDGE ( 'NONE', *, *, #49259, .F. ) ;
#97377 = DIRECTION ( 'NONE',  ( 0.000000000000000000, -0.9908441862701782288, -0.1350103645450539402 ) ) ;
#97378 = CARTESIAN_POINT ( 'NONE',  ( -20.94999999999999929, 1.851028230152016674, -78.65391326942254580 ) ) ;
#97379 = ORIENTED_EDGE ( 'NONE', *, *, #146481, .F. ) ;
#97380 = DIRECTION ( 'NONE',  ( 0.000000000000000000, 0.8814952561688438326, -0.4721928772777332362 ) ) ;
#97381 = CARTESIAN_POINT ( 'NONE',  ( -0.8999999999999993561, -9.650000000000003908, 26.00000000000000355 ) ) ;
#97382 = DIRECTION ( 'NONE',  ( 0.000000000000000000, 0.1350103645451876666, -0.9908441862701600211 ) ) ;
#97383 = VERTEX_POINT ( 'NONE', #207661 ) ;
#97384 = AXIS2_PLACEMENT_3D ( 'NONE', #151158, #129025, #149883 ) ;
#97385 = AXIS2_PLACEMENT_3D ( 'NONE', #164567, #165858, #65447 ) ;
#97386 = CIRCLE ( 'NONE', #105765, 4.049999999999998046 ) ;
#97387 = DIRECTION ( 'NONE',  ( -0.000000000000000000, -0.000000000000000000, -1.000000000000000000 ) ) ;
#97388 = ADVANCED_FACE ( 'NONE', ( #225887 ), #171133, .F. ) ;
#97389 = DIRECTION ( 'NONE',  ( 0.000000000000000000, 0.000000000000000000, 1.000000000000000000 ) ) ;
#97390 = CARTESIAN_POINT ( 'NONE',  ( -22.46246831459151494, 26.01821253579841198, -254.2940600222800072 ) ) ;
#97391 = EDGE_CURVE ( 'NONE', #24660, #149548, #10733, .T. ) ;
#97392 = ORIENTED_EDGE ( 'NONE', *, *, #170186, .T. ) ;
#97393 =( BOUNDED_SURFACE ( )  B_SPLINE_SURFACE ( 3, 2, ( 
 ( #224733, #102197, #3111 ),
 ( #46102, #86488, #81352 ),
 ( #121815, #166096, #164783 ),
 ( #146477, #104766, #47378 ) ),
 .UNSPECIFIED., .F., .F., .T. ) 
 B_SPLINE_SURFACE_WITH_KNOTS ( ( 4, 4 ),
 ( 3, 3 ),
 ( 1.734723475976807094E-18, 0.001979672783031534173 ),
 ( 0.000000000000000000, 1.000000000000000000 ),
 .UNSPECIFIED. ) 
 GEOMETRIC_REPRESENTATION_ITEM ( )  RATIONAL_B_SPLINE_SURFACE ( (
 ( 1.000000000000000000, 0.7103081912008384347, 1.000000000000000000),
 ( 1.000000000000000000, 0.7104998333558379953, 1.000000000000000000),
 ( 1.000000000000000000, 0.7107238315755348701, 1.000000000000000000),
 ( 1.000000000000000000, 0.7110073749539290722, 1.000000000000000000) ) ) 
 REPRESENTATION_ITEM ( '' )  SURFACE ( )  );
#97394 = ADVANCED_FACE ( 'NONE', ( #111109 ), #169850, .T. ) ;
#97395 = CARTESIAN_POINT ( 'NONE',  ( -21.05000000000000071, -11.64999999999999858, -30.59999999999999432 ) ) ;
#97396 = ADVANCED_FACE ( 'NONE', ( #108544 ), #142506, .F. ) ;
#97397 = ORIENTED_EDGE ( 'NONE', *, *, #118195, .T. ) ;
#97398 = CYLINDRICAL_SURFACE ( 'NONE', #197327, 0.1000000000000035305 ) ;
#97399 = SPHERICAL_SURFACE ( 'NONE', #79456, 0.1000000000000000056 ) ;
#97400 = DIRECTION ( 'NONE',  ( 0.000000000000000000, 0.000000000000000000, 1.000000000000000000 ) ) ;
#97401 = CARTESIAN_POINT ( 'NONE',  ( 21.10000000000000142, -11.75000000000000000, 11.89999999999999680 ) ) ;
#97402 = LINE ( 'NONE', #235654, #146441 ) ;
#97403 = DIRECTION ( 'NONE',  ( 0.000000000000000000, -1.000000000000000000, 0.000000000000000000 ) ) ;
#97404 = VERTEX_POINT ( 'NONE', #151553 ) ;
#97405 = VECTOR ( 'NONE', #42358, 1000.000000000000000 ) ;
#97406 = CARTESIAN_POINT ( 'NONE',  ( -23.15000000000000213, 64.25000000001165290, -69.52310748452440237 ) ) ;
#97407 = CARTESIAN_POINT ( 'NONE',  ( -22.50047199487840999, 0.04490605192048083977, 11.75004741891856597 ) ) ;
#97409 = AXIS2_PLACEMENT_3D ( 'NONE', #171664, #193758, #152087 ) ;
#97408 = CARTESIAN_POINT ( 'NONE',  ( -23.49999999999994316, 84.00000000001119815, -37.18565239344504647 ) ) ;
#97410 = CIRCLE ( 'NONE', #26544, 0.09999999999999958922 ) ;
#97411 = CARTESIAN_POINT ( 'NONE',  ( 20.94999999999999929, -11.64999999998883595, -131.1000000000000227 ) ) ;
#97412 = EDGE_CURVE ( 'NONE', #145174, #56292, #113300, .T. ) ;
#97413 = ADVANCED_FACE ( 'NONE', ( #147674 ), #231083, .F. ) ;
#97414 = VERTEX_POINT ( 'NONE', #27757 ) ;
#97415 = ORIENTED_EDGE ( 'NONE', *, *, #114713, .T. ) ;
#97416 = DIRECTION ( 'NONE',  ( 1.000000000000000000, -0.000000000000000000, 0.000000000000000000 ) ) ;
#97417 = AXIS2_PLACEMENT_3D ( 'NONE', #139547, #157900, #194432 ) ;
#97418 = CARTESIAN_POINT ( 'NONE',  ( 23.14999999999999147, 1.115600667400684642E-11, -100.5000000000000284 ) ) ;
#97419 = CARTESIAN_POINT ( 'NONE',  ( 20.04142135623730070, 54.35086488289006468, -228.7501953506800305 ) ) ;
#97420 = DIRECTION ( 'NONE',  ( 1.000000000000000000, 0.000000000000000000, 0.000000000000000000 ) ) ;
#97421 = AXIS2_PLACEMENT_3D ( 'NONE', #145778, #221452, #46676 ) ;
#97422 = CARTESIAN_POINT ( 'NONE',  ( -18.50000000000000000, -9.399999999988850163, -73.88204184817267617 ) ) ;
#97423 = ORIENTED_EDGE ( 'NONE', *, *, #53452, .T. ) ;
#97424 = CARTESIAN_POINT ( 'NONE',  ( -20.54999999999999716, -9.000000000000003553, -9.893969122652444881 ) ) ;
#97425 = AXIS2_PLACEMENT_3D ( 'NONE', #200413, #118319, #197835 ) ;
#97427 = CIRCLE ( 'NONE', #64151, 0.1000000000000035305 ) ;
#97426 = DIRECTION ( 'NONE',  ( 0.000000000000000000, 0.000000000000000000, 1.000000000000000000 ) ) ;
#97428 = ORIENTED_EDGE ( 'NONE', *, *, #71125, .F. ) ;
#97429 = DIRECTION ( 'NONE',  ( -0.000000000000000000, -1.000000000000000000, -6.982962677686266711E-15 ) ) ;
#97430 = AXIS2_PLACEMENT_3D ( 'NONE', #23101, #257781, #102580 ) ;
#97431 = EDGE_CURVE ( 'NONE', #63374, #101017, #250656, .T. ) ;
#97432 = CIRCLE ( 'NONE', #18363, 1.899999999999999023 ) ;
#97433 = CARTESIAN_POINT ( 'NONE',  ( -23.25000000000000000, 69.06610602788535402, -65.73746165015079157 ) ) ;
#97434 = EDGE_CURVE ( 'NONE', #97103, #140176, #50918, .T. ) ;
#97435 = AXIS2_PLACEMENT_3D ( 'NONE', #217524, #140560, #83121 ) ;
#97436 = ORIENTED_EDGE ( 'NONE', *, *, #163355, .F. ) ;
#97437 = DIRECTION ( 'NONE',  ( -1.000000000000000000, 0.000000000000000000, 0.000000000000000000 ) ) ;
#97438 = ORIENTED_EDGE ( 'NONE', *, *, #147191, .F. ) ;
#97439 = CARTESIAN_POINT ( 'NONE',  ( -20.64999999999999858, 76.00000000001142553, -36.02310748452432421 ) ) ;
#97440 = DIRECTION ( 'NONE',  ( -1.000000000000000000, -0.000000000000000000, -0.000000000000000000 ) ) ;
#97442 = CIRCLE ( 'NONE', #72551, 0.1999999999999987899 ) ;
#97441 = DIRECTION ( 'NONE',  ( 0.000000000000000000, 0.4721928772777331251, 0.8814952561688439436 ) ) ;
#97443 = EDGE_CURVE ( 'NONE', #123629, #192047, #239831, .T. ) ;
#97444 = DIRECTION ( 'NONE',  ( 0.000000000000000000, 0.000000000000000000, -1.000000000000000000 ) ) ;
#97445 = LINE ( 'NONE', #239561, #32130 ) ;
#97446 = CARTESIAN_POINT ( 'NONE',  ( 21.04999999999999716, 18.76843759928042843, -228.0065070820658093 ) ) ;
#97447 = LINE ( 'NONE', #236998, #237132 ) ;
#97448 = LINE ( 'NONE', #256489, #214002 ) ;
#97449 = EDGE_CURVE ( 'NONE', #75576, #135228, #167497, .T. ) ;
#97450 = DIRECTION ( 'NONE',  ( -1.000000000000000000, -3.265361837132813093E-16, 0.000000000000000000 ) ) ;
#97451 = CIRCLE ( 'NONE', #101731, 12.87499999999999822 ) ;
#97452 = DIRECTION ( 'NONE',  ( 0.000000000000000000, -0.9126074666063771490, -0.4088369013363281623 ) ) ;
#97453 = DIRECTION ( 'NONE',  ( 0.000000000000000000, -7.116814260417660624E-15, 1.000000000000000000 ) ) ;
#97454 = FACE_OUTER_BOUND ( 'NONE', #192735, .T. ) ;
#97455 = CARTESIAN_POINT ( 'NONE',  ( 18.59999999999996945, 10.33248238083634440, -206.5948465439131496 ) ) ;
#97456 = ADVANCED_FACE ( 'NONE', ( #188084 ), #88960, .F. ) ;
#97457 = CIRCLE ( 'NONE', #243217, 0.1000000000000001721 ) ;
#97458 = LINE ( 'NONE', #77914, #157939 ) ;
#97459 = CARTESIAN_POINT ( 'NONE',  ( -13.40000000000000213, -8.279289321881350361, 15.00000000000000355 ) ) ;
#97460 = CIRCLE ( 'NONE', #239143, 0.1000000000000054040 ) ;
#97461 = AXIS2_PLACEMENT_3D ( 'NONE', #183420, #240826, #244658 ) ;
#97462 = ORIENTED_EDGE ( 'NONE', *, *, #57496, .T. ) ;
#97463 = LINE ( 'NONE', #233187, #254225 ) ;
#97464 = DIRECTION ( 'NONE',  ( -1.000000000000000000, 1.207181226542539700E-16, -2.694675058168174199E-16 ) ) ;
#97465 = ADVANCED_FACE ( 'NONE', ( #177543 ), #242466, .F. ) ;
#97466 = ORIENTED_EDGE ( 'NONE', *, *, #150092, .F. ) ;
#97467 = CARTESIAN_POINT ( 'NONE',  ( 21.10000000000000497, 6.342459739679071618, 12.00000000000000355 ) ) ;
#97468 = DIRECTION ( 'NONE',  ( -0.7071067811865562325, -0.7071067811865388020, 0.000000000000000000 ) ) ;
#97469 = EDGE_CURVE ( 'NONE', #122358, #225207, #135790, .T. ) ;
#97470 = ORIENTED_EDGE ( 'NONE', *, *, #152130, .T. ) ;
#97471 = CARTESIAN_POINT ( 'NONE',  ( -22.94999999999999929, 0.000000000000000000, 0.000000000000000000 ) ) ;
#97472 = CARTESIAN_POINT ( 'NONE',  ( 20.94999999999999574, -1.249999999988843369, -75.00000000000004263 ) ) ;
#97473 = AXIS2_PLACEMENT_3D ( 'NONE', #182585, #117467, #140879 ) ;
#97474 = ORIENTED_EDGE ( 'NONE', *, *, #50886, .F. ) ;
#97475 = AXIS2_PLACEMENT_3D ( 'NONE', #33223, #151874, #192271 ) ;
#97476 = VERTEX_POINT ( 'NONE', #232366 ) ;
#97477 = DIRECTION ( 'NONE',  ( 2.952720810173289112E-16, 1.000000000000000000, 6.530723674265620862E-15 ) ) ;
#97478 = VERTEX_POINT ( 'NONE', #197048 ) ;
#97479 = CARTESIAN_POINT ( 'NONE',  ( -20.85000000000000142, 7.675662554762638479, -241.7139905447625381 ) ) ;
#97480 = CARTESIAN_POINT ( 'NONE',  ( 23.14999999999999503, 64.35000000001222986, -148.6731074845244507 ) ) ;
#97482 = CARTESIAN_POINT ( 'NONE',  ( 22.50000000000000000, 29.50811709945092076, -252.6450601445781103 ) ) ;
#97481 = UNCERTAINTY_MEASURE_WITH_UNIT (LENGTH_MEASURE( 1.000000000000000082E-05 ), #129485, 'distance_accuracy_value', 'NONE');
#97483 = CARTESIAN_POINT ( 'NONE',  ( 20.94999999999999929, 76.00000000001156764, -56.64810748452432421 ) ) ;
#97484 = CARTESIAN_POINT ( 'NONE',  ( 21.05000000000000071, 87.39257802171711376, -39.09705706435617856 ) ) ;
#97485 = LINE ( 'NONE', #55786, #187430 ) ;
#97486 = FACE_OUTER_BOUND ( 'NONE', #118845, .T. ) ;
#97487 = CARTESIAN_POINT ( 'NONE',  ( 21.00023020733503643, 1.495312417593671173, -230.7149783752102508 ) ) ;
#97488 = B_SPLINE_CURVE_WITH_KNOTS ( 'NONE', 3,
 ( #150157, #90138, #70633, #124171, #74495, #36643, #194422, #171038 ),
 .UNSPECIFIED., .F., .F.,
 ( 4, 2, 2, 4 ),
 ( 0.000000000000000000, 0.0001881495939909204459, 0.0002822243909863701521, 0.0003762991879818198583 ),
 .UNSPECIFIED. ) ;
#97490 = VERTEX_POINT ( 'NONE', #212791 ) ;
#97489 = DIRECTION ( 'NONE',  ( 0.000000000000000000, 0.000000000000000000, 1.000000000000000000 ) ) ;
#97491 = EDGE_LOOP ( 'NONE', ( #104144, #197029, #32296, #172115 ) ) ;
#97493 = FACE_OUTER_BOUND ( 'NONE', #47590, .T. ) ;
#97492 = CARTESIAN_POINT ( 'NONE',  ( 25.10847955711010115, 9.068702471349586958, 33.00000000000000000 ) ) ;
#97495 = VERTEX_POINT ( 'NONE', #38020 ) ;
#97494 = CARTESIAN_POINT ( 'NONE',  ( -18.79999999999999716, -1.786320531569725478, -11.50977166988710820 ) ) ;
#97496 = ORIENTED_EDGE ( 'NONE', *, *, #172646, .T. ) ;
#97497 = CARTESIAN_POINT ( 'NONE',  ( -14.00000000000000178, 9.850000000011133849, -150.7500000000000284 ) ) ;
#97498 = DIRECTION ( 'NONE',  ( 0.000000000000000000, 0.9908441862701600211, -0.1350103645451876666 ) ) ;
#97499 = AXIS2_PLACEMENT_3D ( 'NONE', #51972, #128973, #208521 ) ;
#97500 = CYLINDRICAL_SURFACE ( 'NONE', #179791, 0.09999999999999939493 ) ;
#97501 = CARTESIAN_POINT ( 'NONE',  ( 18.49351773456751857, -9.443025695145427889, -7.185325526027306786 ) ) ;
#97502 = CARTESIAN_POINT ( 'NONE',  ( 20.94999999999999929, 76.00000000001215028, -138.5231074845243313 ) ) ;
#97503 = LINE ( 'NONE', #216184, #193701 ) ;
#97504 = DIRECTION ( 'NONE',  ( 0.000000000000000000, 0.2128009952263601456, -0.9770955615653316162 ) ) ;
#97505 = FACE_OUTER_BOUND ( 'NONE', #187029, .T. ) ;
#97506 = EDGE_LOOP ( 'NONE', ( #198689, #23660, #14096 ) ) ;
#97507 = ORIENTED_EDGE ( 'NONE', *, *, #188694, .T. ) ;
#97508 = DIRECTION ( 'NONE',  ( 0.000000000000000000, -1.000000000000000000, 0.000000000000000000 ) ) ;
#97509 = VECTOR ( 'NONE', #185149, 1000.000000000000000 ) ;
#97510 = AXIS2_PLACEMENT_3D ( 'NONE', #90757, #89475, #69951 ) ;
#97511 = EDGE_LOOP ( 'NONE', ( #44374, #25608, #93356 ) ) ;
#97512 = DIRECTION ( 'NONE',  ( 0.000000000000000000, 0.000000000000000000, 1.000000000000000000 ) ) ;
#97513 = VERTEX_POINT ( 'NONE', #156690 ) ;
#97514 = DIRECTION ( 'NONE',  ( -1.000000000000000000, -0.000000000000000000, -0.000000000000000000 ) ) ;
#97515 = CIRCLE ( 'NONE', #105895, 0.09999999999999530098 ) ;
#97516 = CARTESIAN_POINT ( 'NONE',  ( -18.59999999999999787, 64.25000000001206502, -124.3731074845243825 ) ) ;
#97517 = EDGE_CURVE ( 'NONE', #33482, #15173, #236186, .T. ) ;
#97519 = ORIENTED_EDGE ( 'NONE', *, *, #143391, .T. ) ;
#97518 = DIRECTION ( 'NONE',  ( 0.7071359030027419834, 0.000000000000000000, 0.7070776581709371511 ) ) ;
#97520 = CARTESIAN_POINT ( 'NONE',  ( -23.24999999999999645, 85.60000000001186038, -96.32291809330219223 ) ) ;
#97521 = ORIENTED_EDGE ( 'NONE', *, *, #148429, .F. ) ;
#97522 = DIRECTION ( 'NONE',  ( -1.000000000000000000, -0.000000000000000000, -0.000000000000000000 ) ) ;
#97523 = EDGE_CURVE ( 'NONE', #237457, #142313, #154134, .T. ) ;
#97524 = FACE_BOUND ( 'NONE', #190784, .T. ) ;
#97525 = ADVANCED_FACE ( 'NONE', ( #237481 ), #35464, .T. ) ;
#97526 = CARTESIAN_POINT ( 'NONE',  ( -21.05000000000000071, 75.96636726467806966, -75.78192467920580100 ) ) ;
#97528 = CIRCLE ( 'NONE', #14205, 0.1000000000000051820 ) ;
#97527 = CARTESIAN_POINT ( 'NONE',  ( -22.50000000000000000, 75.90000000001222702, -148.1726782920690937 ) ) ;
#97529 = DIRECTION ( 'NONE',  ( 3.616040088954490704E-32, 7.105427357601001859E-15, -1.000000000000000000 ) ) ;
#97530 = ORIENTED_EDGE ( 'NONE', *, *, #178631, .F. ) ;
#97531 = DIRECTION ( 'NONE',  ( 0.000000000000000000, 0.2617529984165024026, 0.9651348961777158619 ) ) ;
#97533 = ORIENTED_EDGE ( 'NONE', *, *, #45337, .F. ) ;
#97532 = CIRCLE ( 'NONE', #72646, 0.09999999999999911737 ) ;
#97536 = ORIENTED_EDGE ( 'NONE', *, *, #175999, .T. ) ;
#97535 = CARTESIAN_POINT ( 'NONE',  ( -20.94999999999999929, 77.84915357198788399, -91.41714086472724432 ) ) ;
#97534 = CARTESIAN_POINT ( 'NONE',  ( -20.90000000000000213, 6.742993295648862961, 9.658650260582458458 ) ) ;
#97537 = CARTESIAN_POINT ( 'NONE',  ( 22.10000000000000497, 6.223900101154157483, 12.09999999999999964 ) ) ;
#97538 = CIRCLE ( 'NONE', #110036, 0.9000000000000014655 ) ;
#97539 = VECTOR ( 'NONE', #8777, 1000.000000000000000 ) ;
#97540 = DIRECTION ( 'NONE',  ( 1.000000000000000000, -7.304098846218134667E-16, 0.000000000000000000 ) ) ;
#97541 = VERTEX_POINT ( 'NONE', #255708 ) ;
#97543 = CARTESIAN_POINT ( 'NONE',  ( 18.41832399655371688, 85.68240326668606599, -129.8662638644967728 ) ) ;
#97542 = AXIS2_PLACEMENT_3D ( 'NONE', #190515, #245334, #187930 ) ;
#97544 = ADVANCED_FACE ( 'NONE', ( #216623 ), #256984, .F. ) ;
#97545 = DIRECTION ( 'NONE',  ( 0.000000000000000000, 0.4999999999999689138, -0.8660254037844565822 ) ) ;
#97546 = DIRECTION ( 'NONE',  ( -1.000000000000000000, -0.000000000000000000, -0.000000000000000000 ) ) ;
#97548 = EDGE_LOOP ( 'NONE', ( #93373, #113524, #129088, #119186, #40844, #209100, #213318, #248592 ) ) ;
#97547 = FACE_OUTER_BOUND ( 'NONE', #71976, .T. ) ;
#97549 = CIRCLE ( 'NONE', #14412, 0.09999999999999363565 ) ;
#97550 = CIRCLE ( 'NONE', #51764, 0.1000000000000028644 ) ;
#97551 = DIRECTION ( 'NONE',  ( 0.000000000000000000, 0.1455152366551500653, 0.9893560106964507384 ) ) ;
#97552 = AXIS2_PLACEMENT_3D ( 'NONE', #124486, #240568, #244411 ) ;
#97553 = ORIENTED_EDGE ( 'NONE', *, *, #200758, .F. ) ;
#97554 = CARTESIAN_POINT ( 'NONE',  ( -16.90202395485789211, 9.965944544561791574, -180.0969862787400473 ) ) ;
#97555 = CARTESIAN_POINT ( 'NONE',  ( 18.59999999999999787, -9.321008403350148797, -74.23593824907790406 ) ) ;
#97556 = AXIS2_PLACEMENT_3D ( 'NONE', #231853, #208444, #212289 ) ;
#97557 = CARTESIAN_POINT ( 'NONE',  ( -16.77683809663752257, 44.14991418685006153, -235.2970290647049580 ) ) ;
#97558 = EDGE_LOOP ( 'NONE', ( #207152, #207755 ) ) ;
#97559 = DIRECTION ( 'NONE',  ( 1.000000000000000000, 0.000000000000000000, 0.000000000000000000 ) ) ;
#97560 = EDGE_LOOP ( 'NONE', ( #55075, #239630, #32648, #203166 ) ) ;
#97561 = CARTESIAN_POINT ( 'NONE',  ( 21.56666275994539816, 65.41016251146582761, -242.5699255415354685 ) ) ;
#97562 = CIRCLE ( 'NONE', #30989, 4.000000000000010658 ) ;
#97563 = ADVANCED_FACE ( 'NONE', ( #215338 ), #18427, .F. ) ;
#97564 = CARTESIAN_POINT ( 'NONE',  ( -14.00000000000000178, 9.850000000011133849, -150.7500000000000284 ) ) ;
#97565 = LINE ( 'NONE', #117169, #31138 ) ;
#97566 = EDGE_CURVE ( 'NONE', #210954, #186763, #17603, .T. ) ;
#97567 = EDGE_LOOP ( 'NONE', ( #14104, #62752, #21763, #174112, #82669, #232076, #29155, #64829, #50978, #50226, #89348, #248262, #19405, #28703, #95442, #166493 ) ) ;
#97568 = CARTESIAN_POINT ( 'NONE',  ( 18.59999999999999432, 70.30054753569118020, -216.0653814410942175 ) ) ;
#97569 = AXIS2_PLACEMENT_3D ( 'NONE', #32520, #134127, #255318 ) ;
#97570 = CARTESIAN_POINT ( 'NONE',  ( -21.14999999999994174, 67.85000000001119247, -3.023107484524792277 ) ) ;
#97571 = CARTESIAN_POINT ( 'NONE',  ( -20.94999999999999929, 11.65000000001115232, -93.71613433702194129 ) ) ;
#97573 = EDGE_CURVE ( 'NONE', #57307, #71383, #58746, .T. ) ;
#97572 = ORIENTED_EDGE ( 'NONE', *, *, #73005, .F. ) ;
#97574 = CARTESIAN_POINT ( 'NONE',  ( -21.65000000000000213, 7.708578643773852157, -54.75000000000000000 ) ) ;
#97575 = DIRECTION ( 'NONE',  ( -0.000000000000000000, -1.000000000000000000, 0.000000000000000000 ) ) ;
#97576 = ORIENTED_EDGE ( 'NONE', *, *, #31700, .T. ) ;
#97577 = CYLINDRICAL_SURFACE ( 'NONE', #179311, 0.5000000000000004441 ) ;
#97578 = ORIENTED_EDGE ( 'NONE', *, *, #46308, .T. ) ;
#97580 = ORIENTED_EDGE ( 'NONE', *, *, #173568, .F. ) ;
#97579 = CARTESIAN_POINT ( 'NONE',  ( -18.59999999999999787, 43.57568952063339651, -245.1784935019914826 ) ) ;
#97584 = EDGE_CURVE ( 'NONE', #251642, #113738, #152841, .T. ) ;
#97583 = ORIENTED_EDGE ( 'NONE', *, *, #157731, .F. ) ;
#97582 = ORIENTED_EDGE ( 'NONE', *, *, #231860, .T. ) ;
#97581 = CARTESIAN_POINT ( 'NONE',  ( 21.05000000000000071, 5.900000000011162093, -90.28090023534366537 ) ) ;
#97585 = AXIS2_PLACEMENT_3D ( 'NONE', #31479, #90113, #49723 ) ;
#97586 = DIRECTION ( 'NONE',  ( 0.000000000000000000, 0.7397890806274223241, 0.6728388485993012091 ) ) ;
#97587 = DIRECTION ( 'NONE',  ( 1.000000000000000000, 7.304098846218134667E-16, 4.639676173203993355E-30 ) ) ;
#97588 = TOROIDAL_SURFACE ( 'NONE', #6031, 0.2000000000000000111, 0.1000000000000000056 ) ;
#97589 = FACE_OUTER_BOUND ( 'NONE', #170004, .T. ) ;
#97590 = DIRECTION ( 'NONE',  ( 0.000000000000000000, 1.000000000000000000, 2.891205793294679805E-16 ) ) ;
#97591 = AXIS2_PLACEMENT_3D ( 'NONE', #13824, #12561, #16412 ) ;
#97592 = DIRECTION ( 'NONE',  ( 1.000000000000000000, 7.492892343619937423E-30, -1.073024830501117725E-15 ) ) ;
#97593 = DIRECTION ( 'NONE',  ( 0.000000000000000000, 0.000000000000000000, 1.000000000000000000 ) ) ;
#97595 = DIRECTION ( 'NONE',  ( 1.000000000000000000, 0.000000000000000000, 0.000000000000000000 ) ) ;
#97594 = CARTESIAN_POINT ( 'NONE',  ( -20.54999999999999716, 7.250000000011155521, -45.75000000000000000 ) ) ;
#97596 = ORIENTED_EDGE ( 'NONE', *, *, #63261, .T. ) ;
#97597 = ORIENTED_EDGE ( 'NONE', *, *, #115285, .T. ) ;
#97599 = EDGE_LOOP ( 'NONE', ( #92206, #87066, #70616, #49007 ) ) ;
#97598 = CIRCLE ( 'NONE', #168604, 0.09999999999999939493 ) ;
#97600 = ADVANCED_FACE ( 'NONE', ( #56252 ), #95397, .T. ) ;
#97601 = CARTESIAN_POINT ( 'NONE',  ( 23.24999999999999645, 76.00000000001213607, -136.5231074845243313 ) ) ;
#97602 = VECTOR ( 'NONE', #40004, 1000.000000000000000 ) ;
#97604 = ORIENTED_EDGE ( 'NONE', *, *, #208286, .F. ) ;
#97603 = CARTESIAN_POINT ( 'NONE',  ( -23.15000000000000213, -9.599999999988844124, -21.75000000000000711 ) ) ;
#97605 = LINE ( 'NONE', #78064, #146756 ) ;
#97606 = VERTEX_POINT ( 'NONE', #233637 ) ;
#97607 = DIRECTION ( 'NONE',  ( 0.000000000000000000, -7.116814260417668513E-15, 1.000000000000000000 ) ) ;
#97608 = VERTEX_POINT ( 'NONE', #174986 ) ;
#97609 = CARTESIAN_POINT ( 'NONE',  ( -23.25000000000000355, 65.08943781962308606, -222.1672656287770451 ) ) ;
#97610 = CIRCLE ( 'NONE', #76790, 11.64999999999999325 ) ;
#97611 = EDGE_CURVE ( 'NONE', #239382, #43357, #254442, .T. ) ;
#97612 = ADVANCED_FACE ( 'NONE', ( #183922 ), #84200, .T. ) ;
#97613 = VECTOR ( 'NONE', #257636, 1000.000000000000000 ) ;
#97614 = AXIS2_PLACEMENT_3D ( 'NONE', #30808, #146850, #66047 ) ;
#97615 = ORIENTED_EDGE ( 'NONE', *, *, #105654, .F. ) ;
#97616 = VECTOR ( 'NONE', #187192, 1000.000000000000000 ) ;
#97617 = CARTESIAN_POINT ( 'NONE',  ( 20.05000000000002913, 68.75000000001158185, -60.27310748452437394 ) ) ;
#97618 = DIRECTION ( 'NONE',  ( -1.000000000000000000, 0.000000000000000000, 0.000000000000000000 ) ) ;
#97619 = ADVANCED_FACE ( 'NONE', ( #161818 ), #241342, .T. ) ;
#97621 = ORIENTED_EDGE ( 'NONE', *, *, #210214, .T. ) ;
#97620 = EDGE_LOOP ( 'NONE', ( #162765, #22642, #19452, #148822 ) ) ;
#97622 = ORIENTED_EDGE ( 'NONE', *, *, #75840, .T. ) ;
#97624 = EDGE_CURVE ( 'NONE', #70449, #69371, #22305, .T. ) ;
#97623 = DIRECTION ( 'NONE',  ( -0.000000000000000000, -6.982962677686266711E-15, 1.000000000000000000 ) ) ;
#97625 = ORIENTED_EDGE ( 'NONE', *, *, #148095, .F. ) ;
#97626 = ORIENTED_EDGE ( 'NONE', *, *, #243931, .F. ) ;
#97627 = CARTESIAN_POINT ( 'NONE',  ( -21.37071067811865532, 8.070710678118656389, -21.15000000000000213 ) ) ;
#97628 = ORIENTED_EDGE ( 'NONE', *, *, #213063, .F. ) ;
#97630 = EDGE_CURVE ( 'NONE', #71443, #17147, #142220, .T. ) ;
#97629 = TOROIDAL_SURFACE ( 'NONE', #218437, 0.2000000000000000111, 0.1000000000000000056 ) ;
#97632 = CARTESIAN_POINT ( 'NONE',  ( 20.95203847575071521, 65.49893946073831330, -162.4560361359008596 ) ) ;
#97631 = CARTESIAN_POINT ( 'NONE',  ( 20.94999999999999574, 59.10678033798691189, -225.7992625810339575 ) ) ;
#97633 = DIRECTION ( 'NONE',  ( -1.000000000000000000, -0.000000000000000000, 0.000000000000000000 ) ) ;
#97634 = CARTESIAN_POINT ( 'NONE',  ( 20.85000000000000142, 56.23643450586807546, -227.9054833905874204 ) ) ;
#97635 = PLANE ( 'NONE',  #167816 ) ;
#97636 = EDGE_LOOP ( 'NONE', ( #71593, #149221, #184177, #80186, #73746 ) ) ;
#97637 = ORIENTED_EDGE ( 'NONE', *, *, #169861, .F. ) ;
#97638 = CARTESIAN_POINT ( 'NONE',  ( -17.01473183483380680, 66.05000000001182059, -82.27310748452441658 ) ) ;
#97639 = AXIS2_PLACEMENT_3D ( 'NONE', #254754, #172750, #216945 ) ;
#97641 = EDGE_CURVE ( 'NONE', #194138, #83796, #80948, .T. ) ;
#97640 = FACE_OUTER_BOUND ( 'NONE', #221497, .T. ) ;
#97642 = ORIENTED_EDGE ( 'NONE', *, *, #241818, .T. ) ;
#97643 = CARTESIAN_POINT ( 'NONE',  ( 23.14999999999999858, 5.500000000011153745, -121.5947339810869465 ) ) ;
#97644 = EDGE_CURVE ( 'NONE', #21871, #256969, #242656, .T. ) ;
#97645 = EDGE_CURVE ( 'NONE', #210716, #227165, #55187, .T. ) ;
#97646 = AXIS2_PLACEMENT_3D ( 'NONE', #71371, #209581, #171767 ) ;
#97647 = SPHERICAL_SURFACE ( 'NONE', #138682, 0.1000000000000000056 ) ;
#97648 = VECTOR ( 'NONE', #78555, 1000.000000000000114 ) ;
#97649 = DIRECTION ( 'NONE',  ( 0.000000000000000000, -0.8700118002898359348, 0.4930308989875165082 ) ) ;
#97650 = VERTEX_POINT ( 'NONE', #120138 ) ;
#97651 = ORIENTED_EDGE ( 'NONE', *, *, #21664, .T. ) ;
#97652 = EDGE_CURVE ( 'NONE', #90236, #239112, #160536, .T. ) ;
#97653 = DIRECTION ( 'NONE',  ( 1.000000000000000000, 0.000000000000000000, 0.000000000000000000 ) ) ;
#97654 = CARTESIAN_POINT ( 'NONE',  ( -0.8999999999999991340, -9.650000000000003908, 23.40000000000000213 ) ) ;
#97655 = VERTEX_POINT ( 'NONE', #202205 ) ;
#97656 = DIRECTION ( 'NONE',  ( -0.000000000000000000, 1.000000000000000000, 7.272083257015735086E-15 ) ) ;
#97657 = EDGE_LOOP ( 'NONE', ( #84205, #5063, #213804, #242450, #124862 ) ) ;
#97658 = DIRECTION ( 'NONE',  ( 1.000000000000000000, 0.000000000000000000, 0.000000000000000000 ) ) ;
#97659 = DIRECTION ( 'NONE',  ( -1.000000000000000000, -0.000000000000000000, 0.000000000000000000 ) ) ;
#97661 = CARTESIAN_POINT ( 'NONE',  ( -22.57320508075687826, 55.89093952297026391, -232.7795287750844579 ) ) ;
#97660 = DIRECTION ( 'NONE',  ( -1.000000000000000000, -0.000000000000000000, -0.000000000000000000 ) ) ;
#97662 = ADVANCED_FACE ( 'NONE', ( #223040 ), #79665, .F. ) ;
#97664 = EDGE_CURVE ( 'NONE', #65513, #81245, #230189, .T. ) ;
#97663 = CARTESIAN_POINT ( 'NONE',  ( 18.49999999999998934, 65.70711192142415769, -164.5651054685122858 ) ) ;
#97665 = CARTESIAN_POINT ( 'NONE',  ( -20.00857864376270001, 66.75000000001179501, -81.87310748452438247 ) ) ;
#97666 = EDGE_CURVE ( 'NONE', #120372, #14875, #80118, .T. ) ;
#97667 = DIRECTION ( 'NONE',  ( -0.000000000000000000, 0.9651348961777161950, -0.2617529984165014589 ) ) ;
#97669 = ORIENTED_EDGE ( 'NONE', *, *, #101550, .F. ) ;
#97668 = ORIENTED_EDGE ( 'NONE', *, *, #76235, .T. ) ;
#97670 = ORIENTED_EDGE ( 'NONE', *, *, #76886, .F. ) ;
#97671 = CARTESIAN_POINT ( 'NONE',  ( 18.49999999999999289, 6.450000000011156587, -43.51702717044002355 ) ) ;
#97672 = CARTESIAN_POINT ( 'NONE',  ( -18.41353343127311248, -7.785976468740646084, -209.8926132507865816 ) ) ;
#97673 = CIRCLE ( 'NONE', #243431, 0.09999999999999986677 ) ;
#97674 = CARTESIAN_POINT ( 'NONE',  ( 22.88900146558018989, 67.29609520889898988, -82.17310748452437963 ) ) ;
#97675 = CARTESIAN_POINT ( 'NONE',  ( -18.41353343127310893, -9.499999999988851584, -107.5320693966996970 ) ) ;
#97676 = EDGE_CURVE ( 'NONE', #221772, #90288, #52269, .T. ) ;
#97677 = CARTESIAN_POINT ( 'NONE',  ( 20.77526135991778133, 8.932009016622666664, -8.468568542723934556 ) ) ;
#97678 = CARTESIAN_POINT ( 'NONE',  ( 21.00000000000000000, 30.37633856152204359, -235.1250019192171408 ) ) ;
#97679 = ORIENTED_EDGE ( 'NONE', *, *, #33768, .F. ) ;
#97680 = CARTESIAN_POINT ( 'NONE',  ( -20.15000000000000568, 52.25315717083599765, -232.3839580427603835 ) ) ;
#97681 = VERTEX_POINT ( 'NONE', #224327 ) ;
#97682 = ORIENTED_EDGE ( 'NONE', *, *, #89715, .T. ) ;
#97683 = DIRECTION ( 'NONE',  ( -3.265361837132813093E-16, -1.000000000000000000, -6.938893903907229955E-15 ) ) ;
#97684 = CARTESIAN_POINT ( 'NONE',  ( -18.59999999999999787, -1.162701749926853712, -75.10000000000003695 ) ) ;
#97685 = DIRECTION ( 'NONE',  ( 0.000000000000000000, 6.938893903907030216E-14, -1.000000000000000000 ) ) ;
#97686 = DIRECTION ( 'NONE',  ( 0.000000000000000000, 0.2128009952263603954, -0.9770955615653315052 ) ) ;
#97687 = CIRCLE ( 'NONE', #31683, 0.1000000000000001860 ) ;
#97688 = VECTOR ( 'NONE', #249579, 1000.000000000000000 ) ;
#97689 = LINE ( 'NONE', #179843, #158989 ) ;
#97690 = ORIENTED_EDGE ( 'NONE', *, *, #237074, .T. ) ;
#97691 = VERTEX_POINT ( 'NONE', #100497 ) ;
#97692 = FACE_OUTER_BOUND ( 'NONE', #29687, .T. ) ;
#97693 = CARTESIAN_POINT ( 'NONE',  ( 21.14999999999999503, 11.65000000000000746, -0.1000000000000028644 ) ) ;
#97694 = VERTEX_POINT ( 'NONE', #180084 ) ;
#97695 = CARTESIAN_POINT ( 'NONE',  ( -17.05016517656152431, 22.99807563533816435, -230.9457812431605817 ) ) ;
#97696 = FACE_OUTER_BOUND ( 'NONE', #203434, .T. ) ;
#97697 = DIRECTION ( 'NONE',  ( 0.000000000000000000, 0.000000000000000000, -1.000000000000000000 ) ) ;
#97698 = DIRECTION ( 'NONE',  ( -0.000000000000000000, 0.2128009952263603677, -0.9770955615653313941 ) ) ;
#97700 = CARTESIAN_POINT ( 'NONE',  ( -23.25000000000000000, 1.115600667400684642E-11, -167.5000000000000284 ) ) ;
#97699 = CARTESIAN_POINT ( 'NONE',  ( -16.90128866880176517, 30.21929489460931961, -234.8096846487093501 ) ) ;
#97701 = DIRECTION ( 'NONE',  ( 0.000000000000000000, -0.2617529984165031243, -0.9651348961777157509 ) ) ;
#97702 = DIRECTION ( 'NONE',  ( -1.000000000000000000, 0.000000000000000000, 0.000000000000000000 ) ) ;
#97703 = EDGE_CURVE ( 'NONE', #10248, #45345, #100954, .T. ) ;
#97704 = CARTESIAN_POINT ( 'NONE',  ( -21.05000000000000071, 77.16270174995064224, -195.4231074845243370 ) ) ;
#97705 = CARTESIAN_POINT ( 'NONE',  ( -23.25000000000000000, 11.75000000001115552, -88.35000000000003695 ) ) ;
#97706 = CIRCLE ( 'NONE', #243467, 11.64999999999999325 ) ;
#97708 = ORIENTED_EDGE ( 'NONE', *, *, #17494, .T. ) ;
#97707 = DIRECTION ( 'NONE',  ( 0.000000000000000000, 0.000000000000000000, -1.000000000000000000 ) ) ;
#97709 = EDGE_CURVE ( 'NONE', #49212, #122858, #221788, .T. ) ;
#97710 = AXIS2_PLACEMENT_3D ( 'NONE', #191186, #231580, #193733 ) ;
#97711 = AXIS2_PLACEMENT_3D ( 'NONE', #37228, #58032, #201414 ) ;
#97712 = FACE_OUTER_BOUND ( 'NONE', #56230, .T. ) ;
#97713 = EDGE_CURVE ( 'NONE', #227850, #116777, #122688, .T. ) ;
#97714 = VERTEX_POINT ( 'NONE', #125236 ) ;
#97715 = CARTESIAN_POINT ( 'NONE',  ( -18.40000000000000213, 11.48667500176882328, -109.7500000000000426 ) ) ;
#97716 = DIRECTION ( 'NONE',  ( 0.000000000000000000, 0.000000000000000000, -1.000000000000000000 ) ) ;
#97717 = ORIENTED_EDGE ( 'NONE', *, *, #34693, .F. ) ;
#97718 = FACE_OUTER_BOUND ( 'NONE', #42351, .T. ) ;
#97719 = ADVANCED_FACE ( 'NONE', ( #169540 ), #86068, .T. ) ;
#97720 = CARTESIAN_POINT ( 'NONE',  ( 22.49436431346199683, 0.06690352973341695542, -21.85004905234654515 ) ) ;
#97721 = AXIS2_PLACEMENT_3D ( 'NONE', #221138, #218566, #239444 ) ;
#97722 = DIRECTION ( 'NONE',  ( -4.408576920032448588E-17, 0.1350103645451876944, 0.9908441862701601321 ) ) ;
#97723 = PLANE ( 'NONE',  #236812 ) ;
#97724 = PLANE ( 'NONE',  #115505 ) ;
#97725 = CIRCLE ( 'NONE', #60329, 0.3999999999999975797 ) ;
#97726 = TOROIDAL_SURFACE ( 'NONE', #139432, 11.70000000000000107, 0.1000000000000000056 ) ;
#97727 = EDGE_LOOP ( 'NONE', ( #161802, #86087, #206215, #138639 ) ) ;
#97728 = DIRECTION ( 'NONE',  ( 0.000000000000000000, 0.000000000000000000, 1.000000000000000000 ) ) ;
#97730 = EDGE_LOOP ( 'NONE', ( #136800, #207578, #50295, #42888 ) ) ;
#97729 = DIRECTION ( 'NONE',  ( 0.000000000000000000, 0.9126074666063660468, 0.4088369013363524762 ) ) ;
#97731 = DIRECTION ( 'NONE',  ( 0.000000000000000000, -6.938893903907222067E-15, 1.000000000000000000 ) ) ;
#97732 = CARTESIAN_POINT ( 'NONE',  ( -16.78270389226384651, 9.947372616628161524, -188.3412070369114417 ) ) ;
#97733 = DIRECTION ( 'NONE',  ( 0.000000000000000000, -6.661338147750933721E-15, 1.000000000000000000 ) ) ;
#97734 = VERTEX_POINT ( 'NONE', #130351 ) ;
#97735 = CARTESIAN_POINT ( 'NONE',  ( -18.59999999999999787, 11.65000000001115232, -67.00000000000000000 ) ) ;
#97736 = CIRCLE ( 'NONE', #106115, 0.5999999999999998668 ) ;
#97737 = APPLICATION_PROTOCOL_DEFINITION ( 'draft international standard', 'automotive_design', 1998, #212334 ) ;
#97738 = AXIS2_PLACEMENT_3D ( 'NONE', #126370, #24738, #182518 ) ;
#97739 = CIRCLE ( 'NONE', #168744, 0.1000000000000013933 ) ;
#97740 = LINE ( 'NONE', #157798, #21589 ) ;
#97741 = ORIENTED_EDGE ( 'NONE', *, *, #183393, .T. ) ;
#97742 = DIRECTION ( 'NONE',  ( 0.000000000000000000, -0.4088369013363280513, 0.9126074666063769270 ) ) ;
#97743 = CARTESIAN_POINT ( 'NONE',  ( -23.25000000000000000, 64.35000000001249987, -177.0379132551784096 ) ) ;
#97744 = CIRCLE ( 'NONE', #243511, 2.100000000000004530 ) ;
#97745 = AXIS2_PLACEMENT_3D ( 'NONE', #109117, #129960, #188668 ) ;
#97746 = DIRECTION ( 'NONE',  ( 0.000000000000000000, 0.000000000000000000, -1.000000000000000000 ) ) ;
#97748 = EDGE_LOOP ( 'NONE', ( #218369, #218680, #147091, #164044 ) ) ;
#97747 = AXIS2_PLACEMENT_3D ( 'NONE', #103868, #186000, #68628 ) ;
#97749 = VERTEX_POINT ( 'NONE', #204753 ) ;
#97750 = CARTESIAN_POINT ( 'NONE',  ( 21.04999999999998650, 6.650000000011155876, -179.7499999999999716 ) ) ;
#97751 = VECTOR ( 'NONE', #248010, 1000.000000000000000 ) ;
#97752 = LINE ( 'NONE', #19545, #188311 ) ;
#97753 = CIRCLE ( 'NONE', #18676, 0.1000000000000054040 ) ;
#97754 = EDGE_CURVE ( 'NONE', #43729, #233023, #50802, .T. ) ;
#97755 = LINE ( 'NONE', #172236, #219453 ) ;
#97756 = LINE ( 'NONE', #118660, #156862 ) ;
#97757 = ADVANCED_FACE ( 'NONE', ( #170832 ), #46824, .T. ) ;
#97759 = CARTESIAN_POINT ( 'NONE',  ( -21.14999999999999858, 76.10000000001218723, -142.7731074845243029 ) ) ;
#97758 = CARTESIAN_POINT ( 'NONE',  ( -18.50000000000000000, 31.44980407958351165, -233.5445995079518866 ) ) ;
#97760 = DIRECTION ( 'NONE',  ( -0.000000000000000000, -1.000000000000000000, -0.000000000000000000 ) ) ;
#97761 = DIRECTION ( 'NONE',  ( 0.000000000000000000, -1.000000000000000000, -6.982962677686265922E-15 ) ) ;
#97762 = CARTESIAN_POINT ( 'NONE',  ( 18.56579813702275317, 65.66974365629616273, -30.43601455626050623 ) ) ;
#97763 = CARTESIAN_POINT ( 'NONE',  ( 21.05000000000000071, 4.813084112160680661, -112.4415177565238650 ) ) ;
#97764 = ORIENTED_EDGE ( 'NONE', *, *, #137020, .F. ) ;
#97765 = EDGE_LOOP ( 'NONE', ( #237790, #131656, #188585, #16980 ) ) ;
#97766 = CARTESIAN_POINT ( 'NONE',  ( -21.65000000000000213, 68.75000000001226397, -149.1731074845244223 ) ) ;
#97768 = CARTESIAN_POINT ( 'NONE',  ( 6.000000000000061284, 64.35000000001120668, -22.12310748452479103 ) ) ;
#97767 = DIRECTION ( 'NONE',  ( 1.000000000000000000, -0.000000000000000000, 0.000000000000000000 ) ) ;
#97769 = EDGE_CURVE ( 'NONE', #113878, #140349, #249049, .T. ) ;
#97770 = DIRECTION ( 'NONE',  ( 1.000000000000000000, -0.000000000000000000, -0.000000000000000000 ) ) ;
#97771 = DIRECTION ( 'NONE',  ( -0.000000000000000000, 1.000000000000000000, -8.673617379884045333E-16 ) ) ;
#97772 = CARTESIAN_POINT ( 'NONE',  ( 13.43663047529819821, 13.14811317477304442, -216.9788617421937147 ) ) ;
#97773 = EDGE_CURVE ( 'NONE', #135192, #95630, #6561, .T. ) ;
#97774 = EDGE_LOOP ( 'NONE', ( #117255, #79039, #74075, #83469 ) ) ;
#97775 = ADVANCED_FACE ( 'NONE', ( #110796 ), #190360, .T. ) ;
#97776 = VERTEX_POINT ( 'NONE', #69130 ) ;
#97777 = CIRCLE ( 'NONE', #231108, 0.09999999999999939493 ) ;
#97778 = CIRCLE ( 'NONE', #206145, 7.800000000000001599 ) ;
#97779 = DIRECTION ( 'NONE',  ( 0.000000000000000000, 0.000000000000000000, -1.000000000000000000 ) ) ;
#97780 = EDGE_CURVE ( 'NONE', #218193, #145161, #26146, .T. ) ;
#97781 = ORIENTED_EDGE ( 'NONE', *, *, #7108, .F. ) ;
#97782 = DIRECTION ( 'NONE',  ( 1.000000000000000000, 0.000000000000000000, 0.000000000000000000 ) ) ;
#97783 = AXIS2_PLACEMENT_3D ( 'NONE', #44949, #226118, #245718 ) ;
#97784 = DIRECTION ( 'NONE',  ( 1.000000000000000000, 0.000000000000000000, 0.000000000000000000 ) ) ;
#97785 = VECTOR ( 'NONE', #163639, 1000.000000000000000 ) ;
#97786 = AXIS2_PLACEMENT_3D ( 'NONE', #122752, #64040, #118896 ) ;
#97787 = ORIENTED_EDGE ( 'NONE', *, *, #116022, .F. ) ;
#97788 = CARTESIAN_POINT ( 'NONE',  ( -17.11825945287482753, 66.05000000001263061, -190.7731074845244166 ) ) ;
#97789 = EDGE_CURVE ( 'NONE', #100153, #102227, #92628, .T. ) ;
#97790 = ORIENTED_EDGE ( 'NONE', *, *, #51428, .T. ) ;
#97791 = DIRECTION ( 'NONE',  ( -3.265361837132813093E-16, 1.000000000000000000, 0.000000000000000000 ) ) ;
#97793 = CIRCLE ( 'NONE', #114403, 0.1000000000000055844 ) ;
#97792 = CARTESIAN_POINT ( 'NONE',  ( 20.02499999999999858, 9.750000000011153745, -155.2500000000000000 ) ) ;
#97794 = CARTESIAN_POINT ( 'NONE',  ( -18.59999999999999787, 59.16775194334852728, -221.0793150863668473 ) ) ;
#97795 = CARTESIAN_POINT ( 'NONE',  ( 22.47071067811865319, 75.90090754530959316, -144.2431822290223522 ) ) ;
#97796 = CARTESIAN_POINT ( 'NONE',  ( 21.05000000000000071, 85.50000000001188027, -93.12913836187179584 ) ) ;
#97797 = B_SPLINE_CURVE_WITH_KNOTS ( 'NONE', 3,
 ( #218071, #100677, #124147, #39494, #19911, #42044, #180259, #119007, #98110, #121597 ),
 .UNSPECIFIED., .F., .F.,
 ( 4, 3, 3, 4 ),
 ( 0.000000000000000000, 4.874959354401577961E-05, 9.785140065119720494E-05, 0.0001360444631935916505 ),
 .UNSPECIFIED. ) ;
#97799 = CARTESIAN_POINT ( 'NONE',  ( 18.54148534481893407, 65.67467670974440352, -130.9531731826884879 ) ) ;
#97798 = DIRECTION ( 'NONE',  ( 0.000000000000000000, 0.000000000000000000, 1.000000000000000000 ) ) ;
#97800 = VECTOR ( 'NONE', #128183, 1000.000000000000000 ) ;
#97801 = PLANE ( 'NONE',  #94719 ) ;
#97802 = ORIENTED_EDGE ( 'NONE', *, *, #125456, .F. ) ;
#97804 = CARTESIAN_POINT ( 'NONE',  ( -16.81744102076748959, 66.05000000001201954, -115.6731074845243796 ) ) ;
#97803 = CARTESIAN_POINT ( 'NONE',  ( 13.40000000000005898, 66.35000000001119247, -23.62310748452479103 ) ) ;
#97805 = ORIENTED_EDGE ( 'NONE', *, *, #57582, .T. ) ;
#97807 = EDGE_LOOP ( 'NONE', ( #242763, #71648, #182326, #156929 ) ) ;
#97806 = DIRECTION ( 'NONE',  ( 1.000000000000000000, 7.304098846218135653E-16, 5.100424963727256530E-30 ) ) ;
#97808 = ORIENTED_EDGE ( 'NONE', *, *, #170387, .T. ) ;
#97809 = FACE_OUTER_BOUND ( 'NONE', #45077, .T. ) ;
#97810 = CYLINDRICAL_SURFACE ( 'NONE', #246669, 0.09999999999999939493 ) ;
#97811 = DIRECTION ( 'NONE',  ( 0.000000000000000000, 1.000000000000000000, 6.982962677686266711E-15 ) ) ;
#97812 = DIRECTION ( 'NONE',  ( 0.000000000000000000, 1.000000000000000000, -1.224646799147353207E-16 ) ) ;
#97813 = ORIENTED_EDGE ( 'NONE', *, *, #215601, .F. ) ;
#97814 = CARTESIAN_POINT ( 'NONE',  ( -21.65000000000000213, 68.75000000001209344, -127.2731074845243597 ) ) ;
#97815 = CARTESIAN_POINT ( 'NONE',  ( 21.08804582317318577, 8.878166167103049844, -112.8499998294053910 ) ) ;
#97817 = DIRECTION ( 'NONE',  ( -1.020425574104004196E-15, 6.982962677686266711E-15, -1.000000000000000000 ) ) ;
#97816 = AXIS2_PLACEMENT_3D ( 'NONE', #35303, #57368, #254285 ) ;
#97818 = ORIENTED_EDGE ( 'NONE', *, *, #119195, .T. ) ;
#97819 = DIRECTION ( 'NONE',  ( 0.000000000000000000, 0.000000000000000000, -1.000000000000000000 ) ) ;
#97820 = FACE_OUTER_BOUND ( 'NONE', #31750, .T. ) ;
#97821 = VERTEX_POINT ( 'NONE', #146065 ) ;
#97822 = VERTEX_POINT ( 'NONE', #108244 ) ;
#97823 = CARTESIAN_POINT ( 'NONE',  ( -20.54999999999999716, 1.115600667400684642E-11, -79.97500000000005116 ) ) ;
#97824 = CIRCLE ( 'NONE', #127074, 7.900000000000000355 ) ;
#97825 = EDGE_CURVE ( 'NONE', #189010, #137157, #142684, .T. ) ;
#97826 = ORIENTED_EDGE ( 'NONE', *, *, #98055, .F. ) ;
#97827 = AXIS2_PLACEMENT_3D ( 'NONE', #74446, #176100, #172269 ) ;
#97828 = FACE_OUTER_BOUND ( 'NONE', #244883, .T. ) ;
#97829 = ORIENTED_EDGE ( 'NONE', *, *, #195457, .T. ) ;
#97830 = DIRECTION ( 'NONE',  ( -0.7071067811865487940, 0.7071067811865463515, 0.000000000000000000 ) ) ;
#97831 = DIRECTION ( 'NONE',  ( 0.000000000000000000, 0.000000000000000000, -1.000000000000000000 ) ) ;
#97832 = LINE ( 'NONE', #213968, #51741 ) ;
#97833 = EDGE_CURVE ( 'NONE', #70783, #62010, #234266, .T. ) ;
#97834 = FACE_OUTER_BOUND ( 'NONE', #101481, .T. ) ;
#97835 = EDGE_CURVE ( 'NONE', #47640, #100678, #104962, .T. ) ;
#97836 = ADVANCED_FACE ( 'NONE', ( #106936 ), #7871, .T. ) ;
#97837 = FACE_OUTER_BOUND ( 'NONE', #11988, .T. ) ;
#97838 = CARTESIAN_POINT ( 'NONE',  ( -21.08078803292166725, 0.07918598716886203481, -27.16698703556286176 ) ) ;
#97839 = CARTESIAN_POINT ( 'NONE',  ( -22.39999999999999858, 11.75000000000000000, 0.09999999999999592548 ) ) ;
#97840 = ORIENTED_EDGE ( 'NONE', *, *, #247634, .F. ) ;
#97841 = CIRCLE ( 'NONE', #243617, 0.1000000000000016709 ) ;
#97843 = CARTESIAN_POINT ( 'NONE',  ( -21.70464131381649509, 7.095358018979010417, -33.50000000000000000 ) ) ;
#97842 = DIRECTION ( 'NONE',  ( 0.000000000000000000, 0.5000000000000004441, 0.8660254037844384856 ) ) ;
#97844 = ORIENTED_EDGE ( 'NONE', *, *, #67270, .F. ) ;
#97847 = VERTEX_POINT ( 'NONE', #187788 ) ;
#97846 = DIRECTION ( 'NONE',  ( -0.000000000000000000, 1.000000000000000000, -0.000000000000000000 ) ) ;
#97845 = DIRECTION ( 'NONE',  ( -1.000000000000000000, -2.952720810173289112E-16, 0.000000000000000000 ) ) ;
#97848 = VERTEX_POINT ( 'NONE', #246460 ) ;
#97849 = CARTESIAN_POINT ( 'NONE',  ( -18.59999999999999787, 1.115600667400684642E-11, -67.00000000000000000 ) ) ;
#97850 = CARTESIAN_POINT ( 'NONE',  ( 12.29592348164038995, 66.64419340838213657, -153.7320049529782864 ) ) ;
#97851 = DIRECTION ( 'NONE',  ( -3.265361837132813586E-16, 1.000000000000000000, 0.000000000000000000 ) ) ;
#97852 = DIRECTION ( 'NONE',  ( -1.000000000000000000, 0.000000000000000000, 0.000000000000000000 ) ) ;
#97853 = VECTOR ( 'NONE', #101278, 1000.000000000000000 ) ;
#97854 = EDGE_LOOP ( 'NONE', ( #95059, #8968, #183679, #126982 ) ) ;
#97855 = LINE ( 'NONE', #177460, #88740 ) ;
#97856 = EDGE_CURVE ( 'NONE', #19319, #186847, #225877, .T. ) ;
#97857 = DIRECTION ( 'NONE',  ( 0.000000000000000000, -2.771150684185008344E-14, -1.000000000000000000 ) ) ;
#97858 = EDGE_CURVE ( 'NONE', #92976, #33536, #9140, .T. ) ;
#97860 = CARTESIAN_POINT ( 'NONE',  ( -23.15000000000000213, 64.25000000001158185, -57.27310748452440237 ) ) ;
#97859 = CYLINDRICAL_SURFACE ( 'NONE', #209362, 0.1000000000000028644 ) ;
#97862 = ORIENTED_EDGE ( 'NONE', *, *, #166935, .F. ) ;
#97861 = CARTESIAN_POINT ( 'NONE',  ( 21.14999999999999858, 87.65000000001236913, -170.0231074845242745 ) ) ;
#97863 = PRODUCT_DEFINITION ( 'UNKNOWN', '', #61421, #212352 ) ;
#97864 = VERTEX_POINT ( 'NONE', #228193 ) ;
#97865 = VECTOR ( 'NONE', #192552, 999.9999999999998863 ) ;
#97866 = CIRCLE ( 'NONE', #2014, 0.09999999999999939493 ) ;
#97867 = CARTESIAN_POINT ( 'NONE',  ( -16.87036670365549895, 44.00112830765706917, -235.3159266546824995 ) ) ;
#97868 = ORIENTED_EDGE ( 'NONE', *, *, #198556, .F. ) ;
#97869 = DIRECTION ( 'NONE',  ( 1.000000000000000000, 0.000000000000000000, 0.000000000000000000 ) ) ;
#97870 = ORIENTED_EDGE ( 'NONE', *, *, #53434, .F. ) ;
#97871 = EDGE_CURVE ( 'NONE', #173524, #38945, #129089, .T. ) ;
#97872 = CARTESIAN_POINT ( 'NONE',  ( 20.94999999999999574, 58.93913529358839298, -225.8436373810195334 ) ) ;
#97874 = EDGE_CURVE ( 'NONE', #87157, #50799, #196867, .T. ) ;
#97873 = LINE ( 'NONE', #120073, #199156 ) ;
#97875 = DIRECTION ( 'NONE',  ( 0.000000000000000000, 0.000000000000000000, 1.000000000000000000 ) ) ;
#97876 = EDGE_CURVE ( 'NONE', #75223, #89932, #1015, .T. ) ;
#97877 = EDGE_LOOP ( 'NONE', ( #152506, #171212, #182654, #127547 ) ) ;
#97878 = CARTESIAN_POINT ( 'NONE',  ( -20.64999999999999858, 23.68770167995059595, -252.8127582590406348 ) ) ;
#97879 = VECTOR ( 'NONE', #45017, 1000.000000000000000 ) ;
#97880 = DIRECTION ( 'NONE',  ( 1.000000000000000000, 0.000000000000000000, 0.000000000000000000 ) ) ;
#97881 = AXIS2_PLACEMENT_3D ( 'NONE', #114855, #134393, #234806 ) ;
#97882 = CIRCLE ( 'NONE', #110379, 0.1000000000000002554 ) ;
#97883 = AXIS2_PLACEMENT_3D ( 'NONE', #15653, #75620, #234669 ) ;
#97884 = VERTEX_POINT ( 'NONE', #112108 ) ;
#97885 = VERTEX_POINT ( 'NONE', #232053 ) ;
#97886 = CARTESIAN_POINT ( 'NONE',  ( -21.59142135623730852, 65.21721683441403172, -213.2912489251323507 ) ) ;
#97887 = ORIENTED_EDGE ( 'NONE', *, *, #31816, .F. ) ;
#97888 = STYLED_ITEM ( 'NONE', ( #22357 ), #250584 ) ;
#97889 = ORIENTED_EDGE ( 'NONE', *, *, #213695, .T. ) ;
#97891 = ORIENTED_EDGE ( 'NONE', *, *, #230098, .F. ) ;
#97890 = CARTESIAN_POINT ( 'NONE',  ( 20.94999999999999929, 49.53130139001177668, -254.0846532093228802 ) ) ;
#97892 = EDGE_LOOP ( 'NONE', ( #104946, #13814, #112409, #199331 ) ) ;
#97896 = EDGE_CURVE ( 'NONE', #70888, #185004, #180140, .T. ) ;
#97895 = VERTEX_POINT ( 'NONE', #230768 ) ;
#97894 = ORIENTED_EDGE ( 'NONE', *, *, #72263, .F. ) ;
#97893 = CARTESIAN_POINT ( 'NONE',  ( -18.50000000000000000, 11.65000000001115232, -88.75000000000004263 ) ) ;
#97897 = VERTEX_POINT ( 'NONE', #115945 ) ;
#97898 = CARTESIAN_POINT ( 'NONE',  ( -23.15000000000000213, 24.21659883365190069, -253.0960739854072870 ) ) ;
#97899 = AXIS2_PLACEMENT_3D ( 'NONE', #96290, #16797, #218809 ) ;
#97900 = CARTESIAN_POINT ( 'NONE',  ( -23.15000000000000213, 76.00000000001210765, -132.5231074845243313 ) ) ;
#97901 = AXIS2_PLACEMENT_3D ( 'NONE', #192906, #255379, #114642 ) ;
#97902 = CARTESIAN_POINT ( 'NONE',  ( -16.87683809663752399, 13.94542889413352604, -218.6696862871272060 ) ) ;
#97903 = AXIS2_PLACEMENT_3D ( 'NONE', #51599, #90746, #54194 ) ;
#97904 = ORIENTED_EDGE ( 'NONE', *, *, #10738, .F. ) ;
#97905 = EDGE_CURVE ( 'NONE', #99065, #12940, #51088, .T. ) ;
#97906 = CARTESIAN_POINT ( 'NONE',  ( 11.60000000000006004, 67.65000000001118963, -25.06452884076210097 ) ) ;
#97908 = ORIENTED_EDGE ( 'NONE', *, *, #74505, .F. ) ;
#97907 = CARTESIAN_POINT ( 'NONE',  ( 22.14074124539698829, 7.390077851054901892, -167.4009471041559038 ) ) ;
#97909 = CARTESIAN_POINT ( 'NONE',  ( -20.54999999999999716, 6.780748427709700543, -212.1627259556213403 ) ) ;
#97911 = ORIENTED_EDGE ( 'NONE', *, *, #162620, .T. ) ;
#97910 = DIRECTION ( 'NONE',  ( 1.000000000000000000, 0.000000000000000000, 0.000000000000000000 ) ) ;
#97912 = ORIENTED_EDGE ( 'NONE', *, *, #64395, .T. ) ;
#97913 = AXIS2_PLACEMENT_3D ( 'NONE', #175178, #58998, #94295 ) ;
#97914 = ADVANCED_FACE ( 'NONE', ( #233344 ), #196747, .T. ) ;
#97915 = AXIS2_PLACEMENT_3D ( 'NONE', #191193, #128635, #98134 ) ;
#97916 = AXIS2_PLACEMENT_3D ( 'NONE', #56545, #137386, #216922 ) ;
#97917 = CARTESIAN_POINT ( 'NONE',  ( 21.07016717457012689, 1.115540062193308597E-11, -161.1790591618990618 ) ) ;
#97918 = DIRECTION ( 'NONE',  ( 0.000000000000000000, -1.000000000000000000, -1.897661533703519897E-16 ) ) ;
#97919 = EDGE_CURVE ( 'NONE', #209722, #97226, #5305, .T. ) ;
#97920 = EDGE_LOOP ( 'NONE', ( #985, #209782, #119870, #193271, #90287, #77995, #209130, #80561, #112324, #141862, #55441, #159899, #230828, #157688, #257707, #179094 ) ) ;
#97921 = ORIENTED_EDGE ( 'NONE', *, *, #214884, .F. ) ;
#97922 = CARTESIAN_POINT ( 'NONE',  ( 23.04999999999999716, 8.822561741677553471, -176.7499999999999716 ) ) ;
#97923 = DIRECTION ( 'NONE',  ( -0.000000000000000000, 0.000000000000000000, 1.000000000000000000 ) ) ;
#97924 = ADVANCED_FACE ( 'NONE', ( #55935 ), #172103, .F. ) ;
#97926 = ORIENTED_EDGE ( 'NONE', *, *, #97896, .T. ) ;
#97925 = ORIENTED_EDGE ( 'NONE', *, *, #120997, .F. ) ;
#97927 = VERTEX_POINT ( 'NONE', #131648 ) ;
#97929 = EDGE_CURVE ( 'NONE', #206700, #243903, #155220, .T. ) ;
#97928 = DIRECTION ( 'NONE',  ( 1.000000000000000000, -1.186688945009010077E-16, -8.286604613020808509E-31 ) ) ;
#97930 = ORIENTED_EDGE ( 'NONE', *, *, #134142, .T. ) ;
#97931 = TOROIDAL_SURFACE ( 'NONE', #14796, 0.9750000000000019762, 0.1000000000000000056 ) ;
#97932 = ORIENTED_EDGE ( 'NONE', *, *, #35265, .T. ) ;
#97933 = DIRECTION ( 'NONE',  ( 0.000000000000000000, 0.9126074666063769270, 0.4088369013363280513 ) ) ;
#97934 = EDGE_LOOP ( 'NONE', ( #138646, #50732, #241177, #34751 ) ) ;
#97935 = CARTESIAN_POINT ( 'NONE',  ( -16.93906926870270624, 12.45421141385810770, -211.1353277132250241 ) ) ;
#97936 = AXIS2_PLACEMENT_3D ( 'NONE', #45844, #107094, #150105 ) ;
#97937 = TOROIDAL_SURFACE ( 'NONE', #89761, 0.2000000000000000111, 0.1000000000000000056 ) ;
#97939 = CARTESIAN_POINT ( 'NONE',  ( -16.97683809663752186, 66.05000000001157900, -56.12074346632790878 ) ) ;
#97938 = DIRECTION ( 'NONE',  ( 0.000000000000000000, 0.4721928772777346239, 0.8814952561688430555 ) ) ;
#97940 = ORIENTED_EDGE ( 'NONE', *, *, #8246, .T. ) ;
#97942 = ORIENTED_EDGE ( 'NONE', *, *, #127937, .T. ) ;
#97941 = VERTEX_POINT ( 'NONE', #251596 ) ;
#97943 = DIRECTION ( 'NONE',  ( 0.000000000000000000, 0.000000000000000000, -1.000000000000000000 ) ) ;
#97944 = CYLINDRICAL_SURFACE ( 'NONE', #32636, 0.09999999999999982514 ) ;
#97945 = VERTEX_POINT ( 'NONE', #132948 ) ;
#97946 = ADVANCED_FACE ( 'NONE', ( #72996 ), #252870, .F. ) ;
#97947 = B_SPLINE_CURVE_WITH_KNOTS ( 'NONE', 3,
 ( #49602, #10485, #89999, #169600, #215094, #252926, #74341, #153894, #133007, #216371, #117285, #177287, #195557, #152591, #114712, #32651 ),
 .UNSPECIFIED., .F., .F.,
 ( 4, 3, 3, 3, 3, 4 ),
 ( 0.000000000000000000, 2.209075297430721397E-05, 5.594258369009613512E-05, 8.979524372342007066E-05, 0.0001236472815274586030, 0.0001574990747609554737 ),
 .UNSPECIFIED. ) ;
#97948 = EDGE_CURVE ( 'NONE', #133309, #176065, #89780, .T. ) ;
#97949 = CARTESIAN_POINT ( 'NONE',  ( -20.85000000000000142, 64.25000000001250555, -176.8647081744215086 ) ) ;
#97950 = ORIENTED_EDGE ( 'NONE', *, *, #172783, .F. ) ;
#97951 = ORIENTED_EDGE ( 'NONE', *, *, #171261, .F. ) ;
#97952 = EDGE_CURVE ( 'NONE', #203639, #234056, #192915, .T. ) ;
#97953 = LINE ( 'NONE', #211516, #141873 ) ;
#97954 = EDGE_LOOP ( 'NONE', ( #230332, #154508, #186553, #140619 ) ) ;
#97955 = FACE_OUTER_BOUND ( 'NONE', #42218, .T. ) ;
#97956 = DIRECTION ( 'NONE',  ( 0.000000000000000000, -0.000000000000000000, -1.000000000000000000 ) ) ;
#97957 = ORIENTED_EDGE ( 'NONE', *, *, #152458, .F. ) ;
#97958 = DIRECTION ( 'NONE',  ( 0.000000000000000000, 0.000000000000000000, -1.000000000000000000 ) ) ;
#97959 = CARTESIAN_POINT ( 'NONE',  ( -20.54999999999999716, 1.148907358139439339E-11, -201.0000000000015064 ) ) ;
#97961 = DIRECTION ( 'NONE',  ( 1.000000000000000000, 0.000000000000000000, 0.000000000000000000 ) ) ;
#97960 = DIRECTION ( 'NONE',  ( -1.836970198721030427E-16, -0.4088369013363281623, 0.9126074666063771490 ) ) ;
#97962 = DIRECTION ( 'NONE',  ( 1.000000000000000000, 0.000000000000000000, 0.000000000000000000 ) ) ;
#97963 = CIRCLE ( 'NONE', #64664, 0.09999999999999939493 ) ;
#97964 = FACE_OUTER_BOUND ( 'NONE', #110264, .T. ) ;
#97965 = CARTESIAN_POINT ( 'NONE',  ( 21.05193202509564543, 65.27606398031511503, -157.8505728811986728 ) ) ;
#97967 = ADVANCED_FACE ( 'NONE', ( #14297 ), #213750, .F. ) ;
#97966 = DIRECTION ( 'NONE',  ( 0.000000000000000000, 0.000000000000000000, -1.000000000000000000 ) ) ;
#97968 = AXIS2_PLACEMENT_3D ( 'NONE', #159817, #239341, #38573 ) ;
#97969 = CARTESIAN_POINT ( 'NONE',  ( 21.97500000000000497, 9.749999999999998224, -12.35000000000000320 ) ) ;
#97970 = CARTESIAN_POINT ( 'NONE',  ( 18.49999999999999289, 33.67810952736942198, -236.3734420906320395 ) ) ;
#97971 = CIRCLE ( 'NONE', #122950, 0.1000000000000033223 ) ;
#97972 = EDGE_CURVE ( 'NONE', #88303, #233233, #134317, .T. ) ;
#97973 = ORIENTED_EDGE ( 'NONE', *, *, #112198, .F. ) ;
#97974 = CIRCLE ( 'NONE', #56291, 0.09999999999998898659 ) ;
#97976 = ORIENTED_EDGE ( 'NONE', *, *, #194523, .T. ) ;
#97975 = ORIENTED_EDGE ( 'NONE', *, *, #256196, .T. ) ;
#97977 = CIRCLE ( 'NONE', #118871, 11.74999999999999645 ) ;
#97978 = VERTEX_POINT ( 'NONE', #114653 ) ;
#97979 = EDGE_LOOP ( 'NONE', ( #68064, #88521, #242943, #168470 ) ) ;
#97980 = CARTESIAN_POINT ( 'NONE',  ( -21.10320863425827298, 0.02502225123826237740, -94.09972261354079137 ) ) ;
#97981 = CARTESIAN_POINT ( 'NONE',  ( -20.94999999999999929, 1.115600667400684642E-11, -134.0000000000000000 ) ) ;
#97982 = EDGE_CURVE ( 'NONE', #121315, #103565, #167677, .T. ) ;
#97983 = VECTOR ( 'NONE', #143823, 1000.000000000000000 ) ;
#97985 = CARTESIAN_POINT ( 'NONE',  ( -20.94999999999999929, 74.26374286841418382, -57.95445515550683524 ) ) ;
#97984 = DIRECTION ( 'NONE',  ( 0.000000000000000000, -0.4721928772777346239, -0.8814952561688430555 ) ) ;
#97986 = EDGE_CURVE ( 'NONE', #181640, #189831, #155098, .T. ) ;
#97988 = ORIENTED_EDGE ( 'NONE', *, *, #138659, .T. ) ;
#97987 = AXIS2_PLACEMENT_3D ( 'NONE', #28484, #128835, #46703 ) ;
#97989 = CARTESIAN_POINT ( 'NONE',  ( 20.94999999999999929, 87.29603075034721371, -99.97520832486037534 ) ) ;
#97990 = CIRCLE ( 'NONE', #14845, 12.97500000000000320 ) ;
#97991 = CARTESIAN_POINT ( 'NONE',  ( -23.25000000000000000, 85.00000000001149658, -45.91707660717669626 ) ) ;
#97992 = CARTESIAN_POINT ( 'NONE',  ( -18.50000000000000000, 9.250000000011157297, -179.8499999999999943 ) ) ;
#97993 = ORIENTED_EDGE ( 'NONE', *, *, #235401, .F. ) ;
#97994 = B_SPLINE_CURVE_WITH_KNOTS ( 'NONE', 3,
 ( #68623, #128594, #208148, #102573, #182154, #162595, #242109, #142990 ),
 .UNSPECIFIED., .F., .F.,
 ( 4, 2, 2, 4 ),
 ( 0.000000000000000000, 0.0001881495939909221806, 0.0002822243909863843552, 0.0003762991879818465297 ),
 .UNSPECIFIED. ) ;
#97995 = DIRECTION ( 'NONE',  ( 1.000000000000000000, 0.000000000000000000, 0.000000000000000000 ) ) ;
#97996 = ORIENTED_EDGE ( 'NONE', *, *, #10522, .F. ) ;
#97997 = CARTESIAN_POINT ( 'NONE',  ( 23.14999999999999858, 2.000000000011158630, -167.5000000000000284 ) ) ;
#97998 = VECTOR ( 'NONE', #156972, 1000.000000000000000 ) ;
#97999 = DIRECTION ( 'NONE',  ( 0.000000000000000000, 1.000000000000000000, 0.000000000000000000 ) ) ;
#98000 = DIRECTION ( 'NONE',  ( 0.000000000000000000, -0.9915357197604971473, 0.1298341882519111479 ) ) ;
#98001 = DIRECTION ( 'NONE',  ( -1.000000000000000000, 0.000000000000000000, 0.000000000000000000 ) ) ;
#98002 = DIRECTION ( 'NONE',  ( -1.000000000000000000, -0.000000000000000000, 0.000000000000000000 ) ) ;
#98003 = VERTEX_POINT ( 'NONE', #257962 ) ;
#98004 = CARTESIAN_POINT ( 'NONE',  ( -20.94999999999999929, 76.00000000001139711, -32.02310748452432421 ) ) ;
#98005 = SPHERICAL_SURFACE ( 'NONE', #205767, 0.1000000000000000056 ) ;
#98006 = DIRECTION ( 'NONE',  ( -1.000000000000000000, 0.000000000000000000, -0.000000000000000000 ) ) ;
#98008 = FACE_OUTER_BOUND ( 'NONE', #102021, .T. ) ;
#98007 = LINE ( 'NONE', #18509, #240857 ) ;
#98009 = CARTESIAN_POINT ( 'NONE',  ( 21.05000000000000071, 1.115650877919449575E-11, -96.40000000000003411 ) ) ;
#98010 = DIRECTION ( 'NONE',  ( 1.000000000000000000, 0.000000000000000000, 0.000000000000000000 ) ) ;
#98011 = DIRECTION ( 'NONE',  ( 0.000000000000000000, 0.000000000000000000, -1.000000000000000000 ) ) ;
#98012 = CARTESIAN_POINT ( 'NONE',  ( 22.44352723754029810, 75.99072290496874871, -114.6728288298730263 ) ) ;
#98014 = ORIENTED_EDGE ( 'NONE', *, *, #12485, .T. ) ;
#98013 = AXIS2_PLACEMENT_3D ( 'NONE', #238477, #100221, #58538 ) ;
#98015 = EDGE_CURVE ( 'NONE', #92859, #236521, #72176, .T. ) ;
#98016 = AXIS2_PLACEMENT_3D ( 'NONE', #29536, #188570, #50324 ) ;
#98017 = EDGE_LOOP ( 'NONE', ( #70089, #167987, #44297, #138991 ) ) ;
#98018 = DIRECTION ( 'NONE',  ( -1.000000000000000000, -0.000000000000000000, -0.000000000000000000 ) ) ;
#98019 = ORIENTED_EDGE ( 'NONE', *, *, #57836, .F. ) ;
#98020 = CARTESIAN_POINT ( 'NONE',  ( -23.15000000000000213, 1.554534886597881638, -188.6360030214194694 ) ) ;
#98021 = CARTESIAN_POINT ( 'NONE',  ( -20.85000000000000142, 7.225717546301074989, -233.4207493275448257 ) ) ;
#98022 = ADVANCED_FACE ( 'NONE', ( #23284 ), #121105, .T. ) ;
#98023 = CARTESIAN_POINT ( 'NONE',  ( -18.59999999999999787, 77.16412189325330928, -128.8082593989527425 ) ) ;
#98024 = AXIS2_PLACEMENT_3D ( 'NONE', #168929, #210577, #30683 ) ;
#98025 = ORIENTED_EDGE ( 'NONE', *, *, #193338, .T. ) ;
#98026 = FACE_OUTER_BOUND ( 'NONE', #119674, .T. ) ;
#98027 = CARTESIAN_POINT ( 'NONE',  ( -18.59999999999999787, 64.40000000001263913, -196.5949042542488883 ) ) ;
#98028 = AXIS2_PLACEMENT_3D ( 'NONE', #177049, #157497, #38807 ) ;
#98029 = DIRECTION ( 'NONE',  ( -1.000000000000000000, 0.000000000000000000, 0.000000000000000000 ) ) ;
#98031 = ORIENTED_EDGE ( 'NONE', *, *, #56859, .F. ) ;
#98030 = CYLINDRICAL_SURFACE ( 'NONE', #75909, 0.1000000000000028644 ) ;
#98033 = CARTESIAN_POINT ( 'NONE',  ( -17.73285935862336515, 10.85798180379888223, -157.2585618097758982 ) ) ;
#98032 = DIRECTION ( 'NONE',  ( 0.000000000000000000, 0.000000000000000000, 1.000000000000000000 ) ) ;
#98034 = DIRECTION ( 'NONE',  ( 1.000000000000000000, 0.000000000000000000, 0.000000000000000000 ) ) ;
#98035 = FACE_OUTER_BOUND ( 'NONE', #71073, .T. ) ;
#98036 = CARTESIAN_POINT ( 'NONE',  ( 18.54286124688534798, 87.05290861654455625, -199.5360271546132367 ) ) ;
#98037 = CARTESIAN_POINT ( 'NONE',  ( -11.60000000000000320, -8.350000000000004974, 15.00000000000000355 ) ) ;
#98038 = ORIENTED_EDGE ( 'NONE', *, *, #197607, .F. ) ;
#98039 = CARTESIAN_POINT ( 'NONE',  ( 0.000000000000000000, 0.000000000000000000, 0.000000000000000000 ) ) ;
#98040 = CARTESIAN_POINT ( 'NONE',  ( 21.14999999999999503, 1.115600667400684642E-11, -33.50000000000000000 ) ) ;
#98041 = VERTEX_POINT ( 'NONE', #20707 ) ;
#98042 = CARTESIAN_POINT ( 'NONE',  ( 21.13736287352038445, 8.046642376383999817, -20.84999999999999787 ) ) ;
#98043 = ORIENTED_EDGE ( 'NONE', *, *, #52920, .F. ) ;
#98044 = VECTOR ( 'NONE', #187130, 1000.000000000000000 ) ;
#98046 = CARTESIAN_POINT ( 'NONE',  ( 18.50000000000000355, 54.96412023489454413, -230.1191065505895779 ) ) ;
#98045 = AXIS2_PLACEMENT_3D ( 'NONE', #23386, #83296, #159039 ) ;
#98047 = DIRECTION ( 'NONE',  ( 0.000000000000000000, -0.2128009952263604232, 0.9770955615653316162 ) ) ;
#98048 = CARTESIAN_POINT ( 'NONE',  ( 20.94999999999999929, 0.000000000000000000, -33.50000000000000000 ) ) ;
#98049 = ORIENTED_EDGE ( 'NONE', *, *, #191362, .F. ) ;
#98050 = ORIENTED_EDGE ( 'NONE', *, *, #48403, .F. ) ;
#98051 = CARTESIAN_POINT ( 'NONE',  ( 18.69999999999999929, -11.65000000000000036, 32.89999999999999858 ) ) ;
#98052 = DIRECTION ( 'NONE',  ( 0.000000000000000000, -0.000000000000000000, 1.000000000000000000 ) ) ;
#98053 = CYLINDRICAL_SURFACE ( 'NONE', #166184, 0.09999999999999939493 ) ;
#98054 = DIRECTION ( 'NONE',  ( -0.000000000000000000, 1.000000000000000000, -1.224646799147352961E-16 ) ) ;
#98055 = EDGE_CURVE ( 'NONE', #171657, #234584, #79858, .T. ) ;
#98058 = CARTESIAN_POINT ( 'NONE',  ( 20.04142135623731136, 64.25000000001250555, -178.7559501969990947 ) ) ;
#98057 = VECTOR ( 'NONE', #237459, 1000.000000000000000 ) ;
#98056 = CARTESIAN_POINT ( 'NONE',  ( 23.14999999999999858, 64.35000000001249987, -177.0379132551783812 ) ) ;
#98059 = FACE_OUTER_BOUND ( 'NONE', #241831, .T. ) ;
#98060 = AXIS2_PLACEMENT_3D ( 'NONE', #222596, #124818, #221319 ) ;
#98061 = CARTESIAN_POINT ( 'NONE',  ( 21.13461538461538680, 65.38541703798632909, -90.67310748452437963 ) ) ;
#98062 = CARTESIAN_POINT ( 'NONE',  ( -17.04761207306817283, 65.97354912661423043, -115.6731074845243938 ) ) ;
#98064 = ORIENTED_EDGE ( 'NONE', *, *, #135200, .F. ) ;
#98063 = CIRCLE ( 'NONE', #48030, 0.5000000000000014433 ) ;
#98065 = LINE ( 'NONE', #202337, #194028 ) ;
#98066 = CIRCLE ( 'NONE', #44125, 0.1000000000000028644 ) ;
#98068 = ORIENTED_EDGE ( 'NONE', *, *, #54977, .F. ) ;
#98067 = CARTESIAN_POINT ( 'NONE',  ( 23.15000000000000213, 87.65000000001172964, -81.27310748452423184 ) ) ;
#98069 = CARTESIAN_POINT ( 'NONE',  ( 20.94999999999999929, 1.115600667400684642E-11, -46.47500000000000142 ) ) ;
#98070 = DIRECTION ( 'NONE',  ( -0.7071067811865463515, 0.7071067811865487940, 4.178957128135655137E-15 ) ) ;
#98072 = FACE_OUTER_BOUND ( 'NONE', #220605, .T. ) ;
#98071 = CARTESIAN_POINT ( 'NONE',  ( -23.25000000000000000, 14.80545736607782814, -235.9842437978701639 ) ) ;
#98073 = STYLED_ITEM ( 'NONE', ( #107965 ), #48300 ) ;
#98074 = EDGE_CURVE ( 'NONE', #184776, #201448, #109560, .T. ) ;
#98075 = ORIENTED_EDGE ( 'NONE', *, *, #188336, .F. ) ;
#98077 = FACE_BOUND ( 'NONE', #238503, .T. ) ;
#98076 = CYLINDRICAL_SURFACE ( 'NONE', #255752, 4.000000000000003553 ) ;
#98078 = CARTESIAN_POINT ( 'NONE',  ( 23.25000000000000000, 87.65000000001238334, -170.0231074845242745 ) ) ;
#98079 = CARTESIAN_POINT ( 'NONE',  ( 21.15000000000005187, 77.75000000001119815, -47.64205752314703801 ) ) ;
#98080 = FACE_OUTER_BOUND ( 'NONE', #226691, .T. ) ;
#98081 = DIRECTION ( 'NONE',  ( -1.000000000000000000, -1.394253735153569469E-16, -2.602809386958778209E-16 ) ) ;
#98082 = EDGE_CURVE ( 'NONE', #217454, #176291, #167858, .T. ) ;
#98083 = ORIENTED_EDGE ( 'NONE', *, *, #119574, .F. ) ;
#98084 = FACE_OUTER_BOUND ( 'NONE', #29143, .T. ) ;
#98085 = ORIENTED_EDGE ( 'NONE', *, *, #91788, .T. ) ;
#98086 = CARTESIAN_POINT ( 'NONE',  ( 22.40000000000010516, 76.00000000001371347, -215.1726782920694632 ) ) ;
#98087 = EDGE_CURVE ( 'NONE', #65554, #145681, #105439, .T. ) ;
#98088 = EDGE_LOOP ( 'NONE', ( #175779, #196366, #172930, #130719 ) ) ;
#98089 = CARTESIAN_POINT ( 'NONE',  ( -20.85000000000000142, 46.46967969402478360, -243.0849751855955674 ) ) ;
#98090 = AXIS2_PLACEMENT_3D ( 'NONE', #229098, #129968, #189970 ) ;
#98091 = EDGE_LOOP ( 'NONE', ( #142758, #150928, #145081, #83374 ) ) ;
#98092 = CARTESIAN_POINT ( 'NONE',  ( -21.45000000000000284, 7.708578643773852157, -79.35000000000005116 ) ) ;
#98093 = CIRCLE ( 'NONE', #94018, 0.09999999999999939493 ) ;
#98094 = CARTESIAN_POINT ( 'NONE',  ( -18.50000000000000000, 8.980461154494397746, -187.0187154576991304 ) ) ;
#98096 = ORIENTED_EDGE ( 'NONE', *, *, #142096, .T. ) ;
#98095 = AXIS2_PLACEMENT_3D ( 'NONE', #83675, #1601, #81132 ) ;
#98097 = EDGE_CURVE ( 'NONE', #235554, #10681, #88702, .T. ) ;
#98098 =( BOUNDED_CURVE ( )  B_SPLINE_CURVE ( 3, ( #99323, #1521, #118933, #161918 ),
 .UNSPECIFIED., .F., .F. ) 
 B_SPLINE_CURVE_WITH_KNOTS ( ( 4, 4 ),
 ( 4.712388980384689674, 5.672655318024514060 ),
 .UNSPECIFIED. ) 
 CURVE ( )  GEOMETRIC_REPRESENTATION_ITEM ( )  RATIONAL_B_SPLINE_CURVE ( ( 1.000000000000000000, 0.9246222802177627154, 0.9246222802177627154, 1.000000000000000000 ) ) 
 REPRESENTATION_ITEM ( '' )  );
#98099 = AXIS2_PLACEMENT_3D ( 'NONE', #129278, #208816, #150143 ) ;
#98100 = AXIS2_PLACEMENT_3D ( 'NONE', #193129, #35370, #71900 ) ;
#98101 = AXIS2_PLACEMENT_3D ( 'NONE', #231085, #31611, #94107 ) ;
#98102 = FACE_OUTER_BOUND ( 'NONE', #126861, .T. ) ;
#98103 = DIRECTION ( 'NONE',  ( -1.000000000000000000, 0.000000000000000000, -0.000000000000000000 ) ) ;
#98104 = DIRECTION ( 'NONE',  ( 0.000000000000000000, 0.2617529984164955192, 0.9651348961777178603 ) ) ;
#98105 = CARTESIAN_POINT ( 'NONE',  ( 18.49999999999999645, 77.83585931145546510, -91.51866831572576189 ) ) ;
#98106 = FACE_OUTER_BOUND ( 'NONE', #50195, .T. ) ;
#98107 = ORIENTED_EDGE ( 'NONE', *, *, #198397, .F. ) ;
#98108 = CARTESIAN_POINT ( 'NONE',  ( 21.05000000000000071, 84.73084112150729652, -112.6211822035085675 ) ) ;
#98109 = ORIENTED_EDGE ( 'NONE', *, *, #173253, .F. ) ;
#98111 = ORIENTED_EDGE ( 'NONE', *, *, #231841, .T. ) ;
#98110 = CARTESIAN_POINT ( 'NONE',  ( -16.88495309932523014, 66.04537294153901428, -90.38855881071248177 ) ) ;
#98112 = VERTEX_POINT ( 'NONE', #1092 ) ;
#98113 = DIRECTION ( 'NONE',  ( 0.000000000000000000, 0.9126074666063602736, 0.4088369013363654103 ) ) ;
#98114 = CARTESIAN_POINT ( 'NONE',  ( 12.60053434924909332, 66.61046543766585160, -187.8482981801344920 ) ) ;
#98116 =( BOUNDED_SURFACE ( )  B_SPLINE_SURFACE ( 3, 2, ( 
 ( #19824, #132369, #211924 ),
 ( #58897, #93233, #170266 ),
 ( #249753, #33311, #252298 ),
 ( #73709, #51515, #131080 ),
 ( #112811, #139729, #39400 ),
 ( #191087, #219277, #177626 ),
 ( #12446, #216713, #60199 ),
 ( #192348, #232772, #217975 ) ),
 .UNSPECIFIED., .F., .F., .F. ) 
 B_SPLINE_SURFACE_WITH_KNOTS ( ( 4, 2, 2, 4 ),
 ( 3, 3 ),
 ( 0.0001723339234021422576, 0.0002782939632049988201, 0.0003842540030078554097, 0.0005961740826135685347 ),
 ( 0.000000000000000000, 1.000000000000000000 ),
 .UNSPECIFIED. ) 
 GEOMETRIC_REPRESENTATION_ITEM ( )  RATIONAL_B_SPLINE_SURFACE ( (
 ( 1.000000000000000000, 0.9504532311154454405, 1.000000000000000000),
 ( 1.000000000000000000, 0.9506023220707116028, 1.000000000000000000),
 ( 1.000000000000000000, 0.9395774818185572697, 1.000000000000000000),
 ( 1.000000000000000000, 0.9079328464643486862, 1.000000000000000000),
 ( 1.000000000000000000, 0.8875702416205991652, 1.000000000000000000),
 ( 1.000000000000000000, 0.8205919608039309310, 1.000000000000000000),
 ( 1.000000000000000000, 0.7666842783598621924, 1.000000000000000000),
 ( 1.000000000000000000, 0.7071067811865253683, 1.000000000000000000) ) ) 
 REPRESENTATION_ITEM ( '' )  SURFACE ( )  );
#98115 = AXIS2_PLACEMENT_3D ( 'NONE', #224459, #227029, #92331 ) ;
#98117 = CARTESIAN_POINT ( 'NONE',  ( -16.94445028196808778, 66.00793639031455484, -157.4157773061059800 ) ) ;
#98118 = CYLINDRICAL_SURFACE ( 'NONE', #208211, 0.09999999999999939493 ) ;
#98119 = ORIENTED_EDGE ( 'NONE', *, *, #97905, .T. ) ;
#98120 = AXIS2_PLACEMENT_3D ( 'NONE', #35310, #194372, #76951 ) ;
#98121 = DIRECTION ( 'NONE',  ( 2.952720810173289112E-16, -1.000000000000000000, 0.000000000000000000 ) ) ;
#98122 = CYLINDRICAL_SURFACE ( 'NONE', #52147, 0.09999999999999810429 ) ;
#98123 = AXIS2_PLACEMENT_3D ( 'NONE', #240167, #44535, #82332 ) ;
#98124 = EDGE_LOOP ( 'NONE', ( #93228, #11093, #234433, #9479 ) ) ;
#98125 = ADVANCED_FACE ( 'NONE', ( #241029 ), #63654, .T. ) ;
#98127 = ORIENTED_EDGE ( 'NONE', *, *, #252118, .F. ) ;
#98126 = FACE_OUTER_BOUND ( 'NONE', #99869, .T. ) ;
#98128 = CARTESIAN_POINT ( 'NONE',  ( -16.85722902420149794, 9.950000000011137047, -79.76554747377056742 ) ) ;
#98129 =( BOUNDED_CURVE ( )  B_SPLINE_CURVE ( 3, ( #167189, #246678, #121631, #165891 ),
 .UNSPECIFIED., .F., .F. ) 
 B_SPLINE_CURVE_WITH_KNOTS ( ( 4, 4 ),
 ( 4.712388980384681680, 5.672655318024688142 ),
 .UNSPECIFIED. ) 
 CURVE ( )  GEOMETRIC_REPRESENTATION_ITEM ( )  RATIONAL_B_SPLINE_CURVE ( ( 1.000000000000000000, 0.9246222802177346267, 0.9246222802177346267, 1.000000000000000000 ) ) 
 REPRESENTATION_ITEM ( '' )  );
#98130 = ADVANCED_FACE ( 'NONE', ( #140625 ), #178506, .T. ) ;
#98131 = CARTESIAN_POINT ( 'NONE',  ( -20.64999999999999858, 68.85000000001156195, -57.17310748452437252 ) ) ;
#98132 = ORIENTED_EDGE ( 'NONE', *, *, #54203, .F. ) ;
#98133 = DIRECTION ( 'NONE',  ( -1.000000000000000000, -0.000000000000000000, -0.000000000000000000 ) ) ;
#98134 = DIRECTION ( 'NONE',  ( 1.000000000000000000, 0.000000000000000000, -0.000000000000000000 ) ) ;
#98135 = CARTESIAN_POINT ( 'NONE',  ( 14.45963434102924516, 66.54845833862603399, -51.06923198569381128 ) ) ;
#98136 = EDGE_CURVE ( 'NONE', #200635, #43175, #213612, .T. ) ;
#98137 = DIRECTION ( 'NONE',  ( 0.000000000000000000, 0.8454177738465994407, 0.5341055959866553016 ) ) ;
#98138 = TOROIDAL_SURFACE ( 'NONE', #44001, 2.100000000000002309, 0.1000000000000000056 ) ;
#98139 = AXIS2_PLACEMENT_3D ( 'NONE', #128386, #171402, #33174 ) ;
#98140 = EDGE_CURVE ( 'NONE', #159384, #98991, #217874, .T. ) ;
#98141 = AXIS2_PLACEMENT_3D ( 'NONE', #85655, #222615, #218774 ) ;
#98142 = VERTEX_POINT ( 'NONE', #102762 ) ;
#98143 = DIRECTION ( 'NONE',  ( 1.000000000000000000, 0.000000000000000000, 0.000000000000000000 ) ) ;
#98144 = AXIS2_PLACEMENT_3D ( 'NONE', #189012, #109451, #212438 ) ;
#98145 = B_SPLINE_CURVE_WITH_KNOTS ( 'NONE', 3,
 ( #106604, #32253, #7530, #12693, #227858, #49218, #248712, #128772, #46633, #90911 ),
 .UNSPECIFIED., .F., .F.,
 ( 4, 3, 3, 4 ),
 ( 0.000000000000000000, 1.004626015991452777E-05, 1.831183478182391193E-05, 2.062343583995917743E-05 ),
 .UNSPECIFIED. ) ;
#98146 = ORIENTED_EDGE ( 'NONE', *, *, #209856, .T. ) ;
#98147 = CARTESIAN_POINT ( 'NONE',  ( 20.94999999999999929, 30.48950451747912993, -239.6099224343151946 ) ) ;
#98148 = CARTESIAN_POINT ( 'NONE',  ( 16.27683809663750125, 60.62847850914943137, -224.4802381816402033 ) ) ;
#98151 = EDGE_CURVE ( 'NONE', #112231, #190860, #163736, .T. ) ;
#98150 = VERTEX_POINT ( 'NONE', #122362 ) ;
#98149 = CARTESIAN_POINT ( 'NONE',  ( -20.94999999999999929, 74.16465844978765176, -124.9679561919613207 ) ) ;
#98152 = CARTESIAN_POINT ( 'NONE',  ( -20.54999999999999716, 2.000000000011154189, -187.7753780772378889 ) ) ;
#98153 = DIRECTION ( 'NONE',  ( -0.5932847527679310229, 0.8049926720990042694, -6.366092712777067056E-16 ) ) ;
#98155 = DIRECTION ( 'NONE',  ( 0.000000000000000000, -1.000000000000000000, 0.000000000000000000 ) ) ;
#98154 = TOROIDAL_SURFACE ( 'NONE', #48306, 4.099999999999999645, 0.1000000000000000056 ) ;
#98156 = CARTESIAN_POINT ( 'NONE',  ( 18.54999999999999716, 8.750000000011182166, -79.65000000000004832 ) ) ;
#98157 = CIRCLE ( 'NONE', #68995, 4.000000000000003553 ) ;
#98158 = EDGE_CURVE ( 'NONE', #16250, #19295, #234455, .T. ) ;
#98159 = FACE_OUTER_BOUND ( 'NONE', #122038, .T. ) ;
#98160 = ADVANCED_FACE ( 'NONE', ( #139326 ), #104043, .F. ) ;
#98161 = CARTESIAN_POINT ( 'NONE',  ( -18.59999999999999787, -1.261786168553869603, -75.08649896354552311 ) ) ;
#98163 = ORIENTED_EDGE ( 'NONE', *, *, #141038, .T. ) ;
#98162 = CARTESIAN_POINT ( 'NONE',  ( 20.99999999999999645, 9.750000000011137757, -113.1500000000000483 ) ) ;
#98164 = AXIS2_PLACEMENT_3D ( 'NONE', #255167, #76585, #178289 ) ;
#98166 = EDGE_CURVE ( 'NONE', #70373, #47548, #76239, .T. ) ;
#98165 = CARTESIAN_POINT ( 'NONE',  ( -20.00857864376270001, 66.85000000001180354, -81.77310748452437394 ) ) ;
#98167 = ORIENTED_EDGE ( 'NONE', *, *, #228944, .F. ) ;
#98168 = CIRCLE ( 'NONE', #27525, 0.1999999999999987899 ) ;
#98170 = ADVANCED_FACE ( 'NONE', ( #61091 ), #220177, .F. ) ;
#98169 = DIRECTION ( 'NONE',  ( -0.000000000000000000, -0.9651348961777157509, 0.2617529984165031243 ) ) ;
#98171 = CARTESIAN_POINT ( 'NONE',  ( -18.40000000000000213, 85.50000000001264766, -196.5237453873442064 ) ) ;
#98172 = ADVANCED_FACE ( 'NONE', ( #224007 ), #107919, .F. ) ;
#98173 = ORIENTED_EDGE ( 'NONE', *, *, #41436, .T. ) ;
#98174 = DIRECTION ( 'NONE',  ( -0.000000000000000000, 0.9875055080513808203, -0.1575844902526395142 ) ) ;
#98175 = ORIENTED_EDGE ( 'NONE', *, *, #171941, .T. ) ;
#98176 = AXIS2_PLACEMENT_3D ( 'NONE', #134257, #70492, #213816 ) ;
#98177 = VECTOR ( 'NONE', #153552, 1000.000000000000000 ) ;
#98178 = VECTOR ( 'NONE', #19839, 1000.000000000000000 ) ;
#98179 = CARTESIAN_POINT ( 'NONE',  ( 23.24999999999999289, 11.65000000001116298, -193.9851942293460070 ) ) ;
#98180 = VERTEX_POINT ( 'NONE', #66235 ) ;
#98181 = CARTESIAN_POINT ( 'NONE',  ( -21.05000000000000071, 60.91865828504416669, -234.1430899377568267 ) ) ;
#98182 = ADVANCED_FACE ( 'NONE', ( #45380 ), #67507, .F. ) ;
#98183 = ORIENTED_EDGE ( 'NONE', *, *, #222469, .F. ) ;
#98184 = ADVANCED_FACE ( 'NONE', ( #127488 ), #172167, .T. ) ;
#98185 = CARTESIAN_POINT ( 'NONE',  ( -16.97048326478264713, 9.950000000011137047, -46.64110688012716821 ) ) ;
#98187 = ORIENTED_EDGE ( 'NONE', *, *, #182149, .T. ) ;
#98186 = DIRECTION ( 'NONE',  ( -1.000000000000000000, -0.000000000000000000, -0.000000000000000000 ) ) ;
#98188 = DIRECTION ( 'NONE',  ( 0.000000000000000000, 0.2128009952263604510, -0.9770955615653315052 ) ) ;
#98189 = VERTEX_POINT ( 'NONE', #190030 ) ;
#98190 = CYLINDRICAL_SURFACE ( 'NONE', #76444, 0.1000000000000028644 ) ;
#98191 = ORIENTED_EDGE ( 'NONE', *, *, #24683, .F. ) ;
#98194 = EDGE_CURVE ( 'NONE', #99532, #84823, #71538, .T. ) ;
#98193 = ORIENTED_EDGE ( 'NONE', *, *, #234035, .F. ) ;
#98192 = VERTEX_POINT ( 'NONE', #166650 ) ;
#98195 = CARTESIAN_POINT ( 'NONE',  ( -23.15000000000000213, 71.65000000001199965, -115.1731074845243370 ) ) ;
#98196 = VERTEX_POINT ( 'NONE', #46644 ) ;
#98197 = CARTESIAN_POINT ( 'NONE',  ( -20.94999999999999929, 76.00000000001264766, -200.6231074845243825 ) ) ;
#98198 = CIRCLE ( 'NONE', #160631, 0.09999999999998898659 ) ;
#98199 = EDGE_LOOP ( 'NONE', ( #82401, #152026, #151236, #116605 ) ) ;
#98200 = AXIS2_PLACEMENT_3D ( 'NONE', #244383, #163583, #29247 ) ;
#98201 = ORIENTED_EDGE ( 'NONE', *, *, #83448, .T. ) ;
#98202 = DIRECTION ( 'NONE',  ( 0.000000000000000000, 1.000000000000000000, 6.853228547068871147E-15 ) ) ;
#98203 = DIRECTION ( 'NONE',  ( 1.000000000000000000, 0.000000000000000000, 0.000000000000000000 ) ) ;
#98205 = ORIENTED_EDGE ( 'NONE', *, *, #63167, .F. ) ;
#98204 = LINE ( 'NONE', #211789, #232300 ) ;
#98206 = FACE_OUTER_BOUND ( 'NONE', #30742, .T. ) ;
#98207 = ORIENTED_EDGE ( 'NONE', *, *, #138885, .F. ) ;
#98208 = FACE_OUTER_BOUND ( 'NONE', #107136, .T. ) ;
#98209 = DIRECTION ( 'NONE',  ( -0.000000000000000000, -0.9651348961777157509, 0.2617529984165031243 ) ) ;
#98210 = DIRECTION ( 'NONE',  ( 1.000000000000000000, 0.000000000000000000, 0.000000000000000000 ) ) ;
#98212 = ORIENTED_EDGE ( 'NONE', *, *, #67170, .T. ) ;
#98211 = EDGE_CURVE ( 'NONE', #241077, #92185, #146961, .T. ) ;
#98213 = CARTESIAN_POINT ( 'NONE',  ( 20.73486653747088582, 68.75000000001251976, -182.6731074845244223 ) ) ;
#98214 = CARTESIAN_POINT ( 'NONE',  ( -18.31331870001019624, 38.21057351245658396, -261.2006551925339863 ) ) ;
#98215 = CYLINDRICAL_SURFACE ( 'NONE', #223921, 4.049999999999998046 ) ;
#98216 = EDGE_CURVE ( 'NONE', #165316, #8049, #204440, .T. ) ;
#98217 = ORIENTED_EDGE ( 'NONE', *, *, #107906, .T. ) ;
#98218 = CARTESIAN_POINT ( 'NONE',  ( -23.15000000000000213, 76.00000000001213607, -136.5231074845242745 ) ) ;
#98219 = EDGE_LOOP ( 'NONE', ( #55918, #214532, #225337, #168650 ) ) ;
#98220 = ORIENTED_EDGE ( 'NONE', *, *, #250429, .F. ) ;
#98221 = VECTOR ( 'NONE', #198657, 1000.000000000000227 ) ;
#98222 = CARTESIAN_POINT ( 'NONE',  ( -21.64999999999999858, 7.350000000011155166, -45.75000000000000000 ) ) ;
#98223 = EDGE_CURVE ( 'NONE', #143764, #101718, #68810, .T. ) ;
#98224 = VERTEX_POINT ( 'NONE', #226565 ) ;
#98225 = EDGE_LOOP ( 'NONE', ( #117524, #167219, #63900, #78613, #45554, #59273, #10585, #1636, #12602 ) ) ;
#98227 = EDGE_CURVE ( 'NONE', #253747, #39190, #238570, .T. ) ;
#98226 = CARTESIAN_POINT ( 'NONE',  ( -21.05000000000000071, 28.37802281961254636, -258.4449340416662722 ) ) ;
#98228 = CARTESIAN_POINT ( 'NONE',  ( 18.39999999999999858, 85.40000000001174385, -81.27310748452426026 ) ) ;
#98229 = EDGE_LOOP ( 'NONE', ( #219412, #105593, #59524, #67784 ) ) ;
#98230 = VERTEX_POINT ( 'NONE', #205730 ) ;
#98231 = EDGE_CURVE ( 'NONE', #220609, #92818, #51276, .T. ) ;
#98232 = CARTESIAN_POINT ( 'NONE',  ( -18.50000000000000000, 79.19526988099229925, -196.1889237952725296 ) ) ;
#98233 = EDGE_LOOP ( 'NONE', ( #172728, #74613, #185942, #132864 ) ) ;
#98234 = ORIENTED_EDGE ( 'NONE', *, *, #182490, .T. ) ;
#98235 = CIRCLE ( 'NONE', #2398, 0.09999999999998898659 ) ;
#98236 = TOROIDAL_SURFACE ( 'NONE', #85770, 3.899999999999999467, 0.1000000000000000056 ) ;
#98237 = ORIENTED_EDGE ( 'NONE', *, *, #143252, .F. ) ;
#98238 = CIRCLE ( 'NONE', #252381, 0.2000000000000000944 ) ;
#98239 = AXIS2_PLACEMENT_3D ( 'NONE', #122326, #104013, #23252 ) ;
#98240 = EDGE_CURVE ( 'NONE', #190315, #200838, #154844, .T. ) ;
#98241 = EDGE_CURVE ( 'NONE', #47998, #249181, #159470, .T. ) ;
#98242 = MECHANICAL_DESIGN_GEOMETRIC_PRESENTATION_REPRESENTATION (  '', ( #239764 ), #181519 ) ;
#98243 = DIRECTION ( 'NONE',  ( -0.000000000000000000, -1.000000000000000000, -6.982962677686266711E-15 ) ) ;
#98244 = EDGE_CURVE ( 'NONE', #174189, #224643, #188672, .T. ) ;
#98245 = CARTESIAN_POINT ( 'NONE',  ( -16.78805706634180694, 14.15604990364249716, -219.2497315528685249 ) ) ;
#98246 = DIRECTION ( 'NONE',  ( -1.000000000000000000, -0.000000000000000000, -0.000000000000000000 ) ) ;
#98247 = FACE_OUTER_BOUND ( 'NONE', #139699, .T. ) ;
#98248 = CARTESIAN_POINT ( 'NONE',  ( 22.50000000000000000, 1.115600667400684642E-11, -100.5000000000000284 ) ) ;
#98249 = CARTESIAN_POINT ( 'NONE',  ( -21.55000000000000071, 7.150000000011155876, -155.2500000000000284 ) ) ;
#98251 = FACE_OUTER_BOUND ( 'NONE', #213984, .T. ) ;
#98250 = DIRECTION ( 'NONE',  ( -1.000000000000000000, -0.000000000000000000, -0.000000000000000000 ) ) ;
#98252 = CARTESIAN_POINT ( 'NONE',  ( -18.79999999999999716, 1.149999999999999911, 16.60000000000000142 ) ) ;
#98253 = CARTESIAN_POINT ( 'NONE',  ( -16.85697194749116790, 23.20972200652296280, -231.1061839156225233 ) ) ;
#98254 = CARTESIAN_POINT ( 'NONE',  ( 18.59999999999999432, 47.89822068137787170, -246.3100470504847692 ) ) ;
#98255 = LINE ( 'NONE', #20065, #67808 ) ;
#98256 = EDGE_CURVE ( 'NONE', #165093, #160597, #221968, .T. ) ;
#98257 = EDGE_CURVE ( 'NONE', #208155, #255663, #184982, .T. ) ;
#98258 = CIRCLE ( 'NONE', #198253, 4.299999999999956302 ) ;
#98259 = ORIENTED_EDGE ( 'NONE', *, *, #50790, .T. ) ;
#98260 = AXIS2_PLACEMENT_3D ( 'NONE', #129933, #110385, #8726 ) ;
#98261 = ADVANCED_FACE ( 'NONE', ( #169218 ), #111782, .F. ) ;
#98263 = ORIENTED_EDGE ( 'NONE', *, *, #42241, .T. ) ;
#98262 = PLANE ( 'NONE',  #136396 ) ;
#98264 = VECTOR ( 'NONE', #58687, 1000.000000000000000 ) ;
#98265 = ADVANCED_FACE ( 'NONE', ( #53076 ), #136441, .F. ) ;
#98266 = FACE_OUTER_BOUND ( 'NONE', #23340, .T. ) ;
#98267 = AXIS2_PLACEMENT_3D ( 'NONE', #191539, #113251, #153721 ) ;
#98268 = AXIS2_PLACEMENT_3D ( 'NONE', #203492, #43140, #240055 ) ;
#98269 = CARTESIAN_POINT ( 'NONE',  ( -22.45372860728439690, 64.16750481150683072, -247.0948467376672113 ) ) ;
#98270 = EDGE_CURVE ( 'NONE', #202658, #201029, #113059, .T. ) ;
#98271 = EDGE_LOOP ( 'NONE', ( #184505, #206213, #209964, #73319, #61950 ) ) ;
#98272 = CARTESIAN_POINT ( 'NONE',  ( -20.94999999999999929, 1.115600667400684642E-11, -74.90000000000004832 ) ) ;
#98273 = CARTESIAN_POINT ( 'NONE',  ( -21.05000000000000071, 74.83729825007408465, -128.4231074845243086 ) ) ;
#98274 = ORIENTED_EDGE ( 'NONE', *, *, #154702, .T. ) ;
#98276 = CARTESIAN_POINT ( 'NONE',  ( -23.15000000000000213, 1.115600667400684642E-11, -203.0999999999999375 ) ) ;
#98275 = CIRCLE ( 'NONE', #106682, 3.899999999999999467 ) ;
#98277 = DIRECTION ( 'NONE',  ( 0.000000000000000000, 0.000000000000000000, -1.000000000000000000 ) ) ;
#98278 = CIRCLE ( 'NONE', #256672, 0.09999999999998898659 ) ;
#98279 = CYLINDRICAL_SURFACE ( 'NONE', #84560, 0.1000000000000024342 ) ;
#98280 = CIRCLE ( 'NONE', #27459, 0.09999999999998898659 ) ;
#98281 = ADVANCED_FACE ( 'NONE', ( #54359 ), #135169, .F. ) ;
#98282 = DIRECTION ( 'NONE',  ( 1.000000000000000000, 0.000000000000000000, -0.000000000000000000 ) ) ;
#98284 = ORIENTED_EDGE ( 'NONE', *, *, #231761, .T. ) ;
#98283 = DIRECTION ( 'NONE',  ( 4.026293107431335996E-15, 0.8700118002898393765, -0.4930308989875104575 ) ) ;
#98285 = AXIS2_PLACEMENT_3D ( 'NONE', #94716, #171728, #152163 ) ;
#98287 = ORIENTED_EDGE ( 'NONE', *, *, #218301, .F. ) ;
#98286 = CARTESIAN_POINT ( 'NONE',  ( -18.58744394320951798, 85.56638515456029381, -96.20025943064806029 ) ) ;
#98288 = DIRECTION ( 'NONE',  ( 1.000000000000000000, -0.000000000000000000, 0.000000000000000000 ) ) ;
#98289 = CARTESIAN_POINT ( 'NONE',  ( 21.05000000000000071, 10.72371710470752149, -12.16119029412744545 ) ) ;
#98290 = LINE ( 'NONE', #78750, #231779 ) ;
#98291 = DIRECTION ( 'NONE',  ( 0.000000000000000000, -1.000000000000000000, 0.000000000000000000 ) ) ;
#98292 = ADVANCED_FACE ( 'NONE', ( #90918 ), #171784, .T. ) ;
#98294 = DIRECTION ( 'NONE',  ( 0.000000000000000000, 0.1350103645451876666, -0.9908441862701600211 ) ) ;
#98293 = CARTESIAN_POINT ( 'NONE',  ( -16.89935556175702303, 9.950000000011135270, -154.3603236371143055 ) ) ;
#98295 = DIRECTION ( 'NONE',  ( -1.000000000000000000, 0.000000000000000000, -0.000000000000000000 ) ) ;
#98296 = DIRECTION ( 'NONE',  ( -0.000000000000000000, -0.000000000000000000, -1.000000000000000000 ) ) ;
#98297 = CIRCLE ( 'NONE', #178035, 0.5000000000000004441 ) ;
#98298 = DIRECTION ( 'NONE',  ( -1.000000000000000000, -2.952720810173289112E-16, 0.000000000000000000 ) ) ;
#98299 = DIRECTION ( 'NONE',  ( -0.000000000000000000, 0.9594490217226103734, 0.2818822000686205254 ) ) ;
#98300 = CARTESIAN_POINT ( 'NONE',  ( 21.14250536705908345, 10.20666781488608166, -227.9869634596271908 ) ) ;
#98301 = ORIENTED_EDGE ( 'NONE', *, *, #184371, .T. ) ;
#98302 = DIRECTION ( 'NONE',  ( 1.387778780781341167E-13, 0.4721928772776973204, 0.8814952561688629284 ) ) ;
#98303 = ORIENTED_EDGE ( 'NONE', *, *, #166863, .F. ) ;
#98304 = ORIENTED_EDGE ( 'NONE', *, *, #236265, .F. ) ;
#98305 = EDGE_CURVE ( 'NONE', #50040, #88829, #72675, .T. ) ;
#98306 = DIRECTION ( 'NONE',  ( 0.000000000000000000, 0.2128009952263568427, -0.9770955615653322823 ) ) ;
#98307 = CARTESIAN_POINT ( 'NONE',  ( -20.85000000000000142, 7.128833340094563376, -233.7327013124401276 ) ) ;
#98308 = ORIENTED_EDGE ( 'NONE', *, *, #80264, .T. ) ;
#98309 = AXIS2_PLACEMENT_3D ( 'NONE', #5162, #181291, #207270 ) ;
#98310 = AXIS2_PLACEMENT_3D ( 'NONE', #123571, #127421, #47860 ) ;
#98311 = ORIENTED_EDGE ( 'NONE', *, *, #22064, .F. ) ;
#98312 = AXIS2_PLACEMENT_3D ( 'NONE', #2410, #178532, #81924 ) ;
#98313 = AXIS2_PLACEMENT_3D ( 'NONE', #125790, #205314, #224882 ) ;
#98314 = EDGE_CURVE ( 'NONE', #215838, #169929, #67878, .T. ) ;
#98315 = ORIENTED_EDGE ( 'NONE', *, *, #157477, .T. ) ;
#98316 = ORIENTED_EDGE ( 'NONE', *, *, #70841, .F. ) ;
#98317 = CIRCLE ( 'NONE', #56628, 0.09999999999998898659 ) ;
#98318 = DIRECTION ( 'NONE',  ( 1.000000000000000000, 0.000000000000000000, 0.000000000000000000 ) ) ;
#98319 = FACE_OUTER_BOUND ( 'NONE', #4275, .T. ) ;
#98320 = CARTESIAN_POINT ( 'NONE',  ( 21.05000000000000071, 9.083217576421224848, -211.4565844547649931 ) ) ;
#98321 = FACE_OUTER_BOUND ( 'NONE', #28429, .T. ) ;
#98322 = CARTESIAN_POINT ( 'NONE',  ( 21.09610168723073187, 65.52914536258586509, -242.0028871142699245 ) ) ;
#98323 = CARTESIAN_POINT ( 'NONE',  ( 21.13435531349785634, 76.00000000001217870, -143.0168285481170471 ) ) ;
#98325 = ORIENTED_EDGE ( 'NONE', *, *, #156256, .T. ) ;
#98324 = DIRECTION ( 'NONE',  ( 0.000000000000000000, -0.000000000000000000, -1.000000000000000000 ) ) ;
#98326 = LINE ( 'NONE', #74989, #54444 ) ;
#98327 = CYLINDRICAL_SURFACE ( 'NONE', #19351, 0.1000000000000028644 ) ;
#98328 = AXIS2_PLACEMENT_3D ( 'NONE', #133601, #73666, #90613 ) ;
#98329 = VERTEX_POINT ( 'NONE', #56895 ) ;
#98330 = FACE_OUTER_BOUND ( 'NONE', #177249, .T. ) ;
#98331 = DIRECTION ( 'NONE',  ( 1.000000000000000000, 0.000000000000000000, 0.000000000000000000 ) ) ;
#98333 = ORIENTED_EDGE ( 'NONE', *, *, #32797, .T. ) ;
#98332 = AXIS2_PLACEMENT_3D ( 'NONE', #172866, #73741, #133686 ) ;
#98334 = CIRCLE ( 'NONE', #244121, 0.1000000000000028644 ) ;
#98336 = LINE ( 'NONE', #120541, #58231 ) ;
#98335 = DIRECTION ( 'NONE',  ( -0.000000000000000000, -0.8814952561688430555, 0.4721928772777346239 ) ) ;
#98337 = DIRECTION ( 'NONE',  ( 1.000000000000000000, 0.000000000000000000, 0.000000000000000000 ) ) ;
#98338 = CARTESIAN_POINT ( 'NONE',  ( -22.59999999999999787, 64.25043287652329127, -203.6239658536231332 ) ) ;
#98339 = ORIENTED_EDGE ( 'NONE', *, *, #18866, .T. ) ;
#98340 = CARTESIAN_POINT ( 'NONE',  ( 21.14999999999999858, 6.649999999999999467, -12.25000000000000000 ) ) ;
#98341 = CARTESIAN_POINT ( 'NONE',  ( 18.59999999999999787, -8.262584272387851314, 10.47734830970188824 ) ) ;
#98342 = CIRCLE ( 'NONE', #210637, 0.1000000000000028644 ) ;
#98343 = FACE_OUTER_BOUND ( 'NONE', #21502, .T. ) ;
#98344 = DIRECTION ( 'NONE',  ( 0.000000000000000000, -1.000000000000000000, 0.000000000000000000 ) ) ;
#98345 = ORIENTED_EDGE ( 'NONE', *, *, #135217, .F. ) ;
#98346 = EDGE_CURVE ( 'NONE', #69129, #103163, #191342, .T. ) ;
#98347 = DIRECTION ( 'NONE',  ( 0.000000000000000000, 0.000000000000000000, -1.000000000000000000 ) ) ;
#98348 = DIRECTION ( 'NONE',  ( -2.578261006436899437E-14, -0.1350103645451973811, 0.9908441862701586889 ) ) ;
#98349 = CIRCLE ( 'NONE', #106769, 7.800000000000001599 ) ;
#98350 = VECTOR ( 'NONE', #145476, 1000.000000000000227 ) ;
#98351 = CARTESIAN_POINT ( 'NONE',  ( -21.65000000000000213, 7.250000000011139534, -46.15000000000000568 ) ) ;
#98352 = AXIS2_PLACEMENT_3D ( 'NONE', #248930, #48141, #28640 ) ;
#98353 = AXIS2_PLACEMENT_3D ( 'NONE', #256388, #118229, #38700 ) ;
#98354 = CARTESIAN_POINT ( 'NONE',  ( -21.65000000000000213, 9.950000000011140600, -146.6500000000000341 ) ) ;
#98356 = ORIENTED_EDGE ( 'NONE', *, *, #167062, .T. ) ;
#98355 = DIRECTION ( 'NONE',  ( 0.000000000000000000, 0.000000000000000000, 1.000000000000000000 ) ) ;
#98357 = DIRECTION ( 'NONE',  ( 1.000000000000000000, 0.000000000000000000, 0.000000000000000000 ) ) ;
#98358 = DIRECTION ( 'NONE',  ( 0.000000000000000000, 6.982962677686267499E-15, -1.000000000000000000 ) ) ;
#98359 = CYLINDRICAL_SURFACE ( 'NONE', #225298, 0.09999999999999939493 ) ;
#98360 = CARTESIAN_POINT ( 'NONE',  ( -18.79999999999999716, 1.350000000000000089, 16.60000000000000142 ) ) ;
#98361 = EDGE_CURVE ( 'NONE', #167562, #126637, #234274, .T. ) ;
#98363 = ORIENTED_EDGE ( 'NONE', *, *, #229809, .T. ) ;
#98362 = FACE_OUTER_BOUND ( 'NONE', #178454, .T. ) ;
#98364 = DIRECTION ( 'NONE',  ( -0.7071067811865562325, -0.7071067811865388020, 0.000000000000000000 ) ) ;
#98365 = CARTESIAN_POINT ( 'NONE',  ( 19.75857864376268935, 11.65000000001115943, -125.3500000000000512 ) ) ;
#98366 = FACE_OUTER_BOUND ( 'NONE', #239930, .T. ) ;
#98367 = EDGE_CURVE ( 'NONE', #107823, #117400, #212173, .T. ) ;
#98368 = VERTEX_POINT ( 'NONE', #195191 ) ;
#98369 = DIRECTION ( 'NONE',  ( 1.000000000000000000, -0.000000000000000000, 0.000000000000000000 ) ) ;
#98370 = CARTESIAN_POINT ( 'NONE',  ( 21.11825140030056502, 75.99279637937949872, -176.4685150499438180 ) ) ;
#98371 = CARTESIAN_POINT ( 'NONE',  ( 18.49999999999999289, 10.20857864377385127, -192.1499999999999488 ) ) ;
#98372 = LINE ( 'NONE', #203942, #191889 ) ;
#98373 = AXIS2_PLACEMENT_3D ( 'NONE', #252948, #74366, #151317 ) ;
#98374 = AXIS2_PLACEMENT_3D ( 'NONE', #90014, #69206, #170903 ) ;
#98375 = CARTESIAN_POINT ( 'NONE',  ( -18.54159361262911077, 78.20960248048282892, -231.5287758789899044 ) ) ;
#98376 = EDGE_CURVE ( 'NONE', #195218, #44096, #201151, .T. ) ;
#98377 = CARTESIAN_POINT ( 'NONE',  ( 21.14999999999999858, 11.75000000001116263, -67.10000000000005116 ) ) ;
#98378 = ORIENTED_EDGE ( 'NONE', *, *, #170118, .F. ) ;
#98379 = EDGE_LOOP ( 'NONE', ( #202661, #146635, #33216, #190793 ) ) ;
#98380 = ADVANCED_FACE ( 'NONE', ( #94770 ), #84580, .T. ) ;
#98382 = CARTESIAN_POINT ( 'NONE',  ( 21.93340585897773920, -1.558585775483465552, -193.8436084524194314 ) ) ;
#98381 = CIRCLE ( 'NONE', #119100, 0.1000000000000028644 ) ;
#98383 = DIRECTION ( 'NONE',  ( 0.000000000000000000, 0.000000000000000000, -1.000000000000000000 ) ) ;
#98384 = EDGE_CURVE ( 'NONE', #242875, #71337, #131664, .T. ) ;
#98385 = DIRECTION ( 'NONE',  ( 0.000000000000000000, -1.000000000000000000, 0.000000000000000000 ) ) ;
#98386 = CARTESIAN_POINT ( 'NONE',  ( -21.05000000000000071, 0.4879293624014888198, -209.1697915983179428 ) ) ;
#98387 = ORIENTED_EDGE ( 'NONE', *, *, #77577, .F. ) ;
#98388 = EDGE_CURVE ( 'NONE', #87098, #146093, #13100, .T. ) ;
#98389 = DIRECTION ( 'NONE',  ( -1.000000000000000000, 0.000000000000000000, 0.000000000000000000 ) ) ;
#98390 = CARTESIAN_POINT ( 'NONE',  ( 20.22483756094572271, 11.01637091542799674, -206.9310927836460507 ) ) ;
#98391 = ADVANCED_FACE ( 'NONE', ( #210873 ), #196234, .T. ) ;
#98392 = DIRECTION ( 'NONE',  ( 1.040834085586054469E-13, -1.000000000000000000, 0.000000000000000000 ) ) ;
#98393 = CARTESIAN_POINT ( 'NONE',  ( -20.85000000000000142, 87.34033503009941057, -206.5987052159188124 ) ) ;
#98394 = AXIS2_PLACEMENT_3D ( 'NONE', #1420, #80953, #82219 ) ;
#98395 = EDGE_LOOP ( 'NONE', ( #80823, #252055, #101086, #39686 ) ) ;
#98396 = CARTESIAN_POINT ( 'NONE',  ( 22.39999999999999858, 7.790779598384538929, -133.9000000000000057 ) ) ;
#98397 = ORIENTED_EDGE ( 'NONE', *, *, #101141, .F. ) ;
#98398 = CARTESIAN_POINT ( 'NONE',  ( 23.24999999999999645, 23.64630004163636912, -249.2443944789516195 ) ) ;
#98399 = EDGE_LOOP ( 'NONE', ( #27182, #51773, #229091, #103805 ) ) ;
#98400 = CARTESIAN_POINT ( 'NONE',  ( -20.54999999999999716, 67.41730047816177773, -218.5504914523898208 ) ) ;
#98401 = DIRECTION ( 'NONE',  ( 1.000000000000000000, 0.000000000000000000, -0.000000000000000000 ) ) ;
#98402 = CARTESIAN_POINT ( 'NONE',  ( -20.54999999999999716, 87.75000000001226397, -153.2731074845242745 ) ) ;
#98403 = ORIENTED_EDGE ( 'NONE', *, *, #220773, .T. ) ;
#98404 = DIRECTION ( 'NONE',  ( 1.000000000000000000, 0.000000000000000000, 0.000000000000000000 ) ) ;
#98405 = DIRECTION ( 'NONE',  ( 0.000000000000000000, 0.2617529984164506107, 0.9651348961777299618 ) ) ;
#98406 = AXIS2_PLACEMENT_3D ( 'NONE', #128218, #243011, #82626 ) ;
#98407 = CARTESIAN_POINT ( 'NONE',  ( -18.59999999999999787, 76.00000000001213607, -136.5231074845243313 ) ) ;
#98408 = EDGE_LOOP ( 'NONE', ( #157971, #105336, #2736, #243997 ) ) ;
#98409 = EDGE_CURVE ( 'NONE', #38307, #250431, #192168, .T. ) ;
#98410 = DIRECTION ( 'NONE',  ( -1.000000000000000000, -0.000000000000000000, -0.000000000000000000 ) ) ;
#98412 = ORIENTED_EDGE ( 'NONE', *, *, #204734, .T. ) ;
#98411 = CARTESIAN_POINT ( 'NONE',  ( 21.14999999999999858, 69.45934304831089889, -136.5231074845243313 ) ) ;
#98413 = DIRECTION ( 'NONE',  ( -0.000000000000000000, -1.000000000000000000, -6.982962677686266711E-15 ) ) ;
#98414 = CARTESIAN_POINT ( 'NONE',  ( -18.51991288638526711, 85.39243678968618667, -162.8798410805651429 ) ) ;
#98415 = CIRCLE ( 'NONE', #190047, 0.1000000000000022399 ) ;
#98416 = AXIS2_PLACEMENT_3D ( 'NONE', #136229, #112851, #131121 ) ;
#98417 = AXIS2_PLACEMENT_3D ( 'NONE', #125849, #31929, #67179 ) ;
#98418 = ORIENTED_EDGE ( 'NONE', *, *, #244181, .T. ) ;
#98420 = CARTESIAN_POINT ( 'NONE',  ( -23.25000000000000000, -2.598867842139046314, -189.5410128746472083 ) ) ;
#98419 = MECHANICAL_DESIGN_GEOMETRIC_PRESENTATION_REPRESENTATION (  '', ( #148165 ), #248309 ) ;
#98422 = ADVANCED_FACE ( 'NONE', ( #162467 ), #199011, .T. ) ;
#98421 = CARTESIAN_POINT ( 'NONE',  ( 21.05000000000000071, 1.115600667400684642E-11, -136.0000000000000284 ) ) ;
#98423 = FACE_OUTER_BOUND ( 'NONE', #50421, .T. ) ;
#98424 = ORIENTED_EDGE ( 'NONE', *, *, #124554, .T. ) ;
#98425 = CARTESIAN_POINT ( 'NONE',  ( 21.07933241753356768, 6.328645948390904330, -133.9066204095807109 ) ) ;
#98426 = FACE_OUTER_BOUND ( 'NONE', #208003, .T. ) ;
#98427 = DIRECTION ( 'NONE',  ( -0.7071067811865475727, -0.6909108974501237954, -0.1504730267678056066 ) ) ;
#98428 = VERTEX_POINT ( 'NONE', #238122 ) ;
#98429 = ORIENTED_EDGE ( 'NONE', *, *, #182284, .T. ) ;
#98430 = CIRCLE ( 'NONE', #206819, 0.09999999999999939493 ) ;
#98431 = EDGE_CURVE ( 'NONE', #110754, #154576, #217067, .T. ) ;
#98432 = AXIS2_PLACEMENT_3D ( 'NONE', #183210, #80210, #63241 ) ;
#98433 = ORIENTED_EDGE ( 'NONE', *, *, #100390, .F. ) ;
#98434 = AXIS2_PLACEMENT_3D ( 'NONE', #233216, #214906, #92385 ) ;
#98435 = CARTESIAN_POINT ( 'NONE',  ( -18.50000000000000000, 64.35000000001150511, -48.17310748452440095 ) ) ;
#98436 = CARTESIAN_POINT ( 'NONE',  ( 21.04105312098505465, 8.875332623054768888, -45.82850674721203177 ) ) ;
#98439 = EDGE_CURVE ( 'NONE', #118720, #182139, #162949, .T. ) ;
#98438 = EDGE_LOOP ( 'NONE', ( #6543, #97244, #2897, #23546 ) ) ;
#98437 = LINE ( 'NONE', #114196, #8346 ) ;
#98440 = DIRECTION ( 'NONE',  ( 0.000000000000000000, -0.000000000000000000, 1.000000000000000000 ) ) ;
#98442 = AXIS2_PLACEMENT_3D ( 'NONE', #124504, #89211, #44964 ) ;
#98441 = DIRECTION ( 'NONE',  ( -0.000000000000000000, 1.000000000000000000, 6.352154140967427193E-15 ) ) ;
#98443 = CARTESIAN_POINT ( 'NONE',  ( -20.94999999999999929, 70.08587962373171365, -198.1273832143211848 ) ) ;
#98444 = PLANE ( 'NONE',  #114381 ) ;
#98445 = CARTESIAN_POINT ( 'NONE',  ( -23.15000000000000213, 1.115649653272650466E-11, -104.5000000000000568 ) ) ;
#98446 = ADVANCED_FACE ( 'NONE', ( #240707 ), #254476, .F. ) ;
#98447 = DIRECTION ( 'NONE',  ( 1.000000000000000000, 2.952720810173289112E-16, -0.000000000000000000 ) ) ;
#98448 = EDGE_CURVE ( 'NONE', #131148, #187669, #229574, .T. ) ;
#98450 = ORIENTED_EDGE ( 'NONE', *, *, #225730, .T. ) ;
#98449 = CARTESIAN_POINT ( 'NONE',  ( -16.90202395485879805, 66.03405545546173983, -182.6200937632638954 ) ) ;
#98452 = ORIENTED_EDGE ( 'NONE', *, *, #17685, .F. ) ;
#98451 = CARTESIAN_POINT ( 'NONE',  ( -20.00857864376270001, 66.85000000001156195, -57.27310748452438816 ) ) ;
#98454 = CARTESIAN_POINT ( 'NONE',  ( 20.88420186297724257, 10.33025634372637391, -72.58709292826388548 ) ) ;
#98453 = CARTESIAN_POINT ( 'NONE',  ( 23.24999999999999645, 28.36802138732021206, -238.7571110118315971 ) ) ;
#98455 = ORIENTED_EDGE ( 'NONE', *, *, #139117, .F. ) ;
#98456 = VERTEX_POINT ( 'NONE', #179467 ) ;
#98457 = CARTESIAN_POINT ( 'NONE',  ( -20.85000000000000142, -1.835859311432481045, -78.50443916879852679 ) ) ;
#98458 = CARTESIAN_POINT ( 'NONE',  ( -21.14999999999994174, 77.83551161375991967, -47.52760213295649550 ) ) ;
#98459 = VECTOR ( 'NONE', #224649, 1000.000000000000000 ) ;
#98460 = AXIS2_PLACEMENT_3D ( 'NONE', #67232, #221159, #45104 ) ;
#98462 = EDGE_CURVE ( 'NONE', #82116, #148169, #33796, .T. ) ;
#98461 = CARTESIAN_POINT ( 'NONE',  ( 21.05000000000000071, 8.776282895303632259, -167.4999999999999716 ) ) ;
#98463 = B_SPLINE_CURVE_WITH_KNOTS ( 'NONE', 3,
 ( #69671, #47497, #172658, #252129, #250838, #87897, #187055, #108772, #149209, #27991, #50081, #151783, #248288, #127057, #190916, #231312 ),
 .UNSPECIFIED., .F., .F.,
 ( 4, 3, 3, 3, 3, 4 ),
 ( 0.000000000000000000, 2.209075297431583676E-05, 5.594258369009758524E-05, 8.979524372341978606E-05, 0.0001236472815274614761, 0.0001574990747609543624 ),
 .UNSPECIFIED. ) ;
#98464 = FACE_OUTER_BOUND ( 'NONE', #112412, .T. ) ;
#98465 = CARTESIAN_POINT ( 'NONE',  ( 20.85000000000000142, 76.32388570108247450, -136.5655178952103768 ) ) ;
#98466 = CARTESIAN_POINT ( 'NONE',  ( 20.74625933824084711, 67.11708647892832857, -194.9679364604013188 ) ) ;
#98467 = ORIENTED_EDGE ( 'NONE', *, *, #256157, .T. ) ;
#98468 = ORIENTED_EDGE ( 'NONE', *, *, #136510, .T. ) ;
#98469 = CARTESIAN_POINT ( 'NONE',  ( 20.94999999999999929, 5.849999999999949019, -10.13249722427797117 ) ) ;
#98470 = AXIS2_PLACEMENT_3D ( 'NONE', #200274, #19062, #58166 ) ;
#98471 = ORIENTED_EDGE ( 'NONE', *, *, #120101, .T. ) ;
#98472 = CARTESIAN_POINT ( 'NONE',  ( -23.15000000000000213, 76.00000000001195133, -103.0231074845243171 ) ) ;
#98473 = CARTESIAN_POINT ( 'NONE',  ( -17.05016517656313724, 51.59814857156833057, -231.9557487940004705 ) ) ;
#98474 = CARTESIAN_POINT ( 'NONE',  ( -13.54795643572458097, 66.54933111084403663, -54.46756099431704001 ) ) ;
#98475 = LINE ( 'NONE', #677, #9616 ) ;
#98476 = ORIENTED_EDGE ( 'NONE', *, *, #205574, .T. ) ;
#98477 = CARTESIAN_POINT ( 'NONE',  ( -15.66061380678752535, 66.63927620602598267, -119.2091802899176685 ) ) ;
#98478 = ADVANCED_FACE ( 'NONE', ( #122044 ), #3352, .T. ) ;
#98479 = ORIENTED_EDGE ( 'NONE', *, *, #14512, .T. ) ;
#98480 = EDGE_CURVE ( 'NONE', #176041, #140162, #179510, .T. ) ;
#98481 = CARTESIAN_POINT ( 'NONE',  ( 20.85000000000000142, 77.16412189325305349, -95.10825939895268277 ) ) ;
#98482 = EDGE_LOOP ( 'NONE', ( #155420, #217639, #8586, #167993 ) ) ;
#98483 = TOROIDAL_SURFACE ( 'NONE', #190136, 1.900000000000002576, 0.1000000000000000056 ) ;
#98484 = CARTESIAN_POINT ( 'NONE',  ( -16.89268316805465986, 9.951721813253337601, -87.85575247854558256 ) ) ;
#98485 = AXIS2_PLACEMENT_3D ( 'NONE', #146647, #12326, #248343 ) ;
#98486 = CARTESIAN_POINT ( 'NONE',  ( -18.40000000000000213, 64.52683809664929981, -78.77310748452438816 ) ) ;
#98487 = LINE ( 'NONE', #17699, #30514 ) ;
#98488 = AXIS2_PLACEMENT_3D ( 'NONE', #213463, #195221, #175641 ) ;
#98489 = ORIENTED_EDGE ( 'NONE', *, *, #82361, .F. ) ;
#98490 = EDGE_CURVE ( 'NONE', #138337, #59420, #77757, .T. ) ;
#98491 = PLANE ( 'NONE',  #60926 ) ;
#98493 = ORIENTED_EDGE ( 'NONE', *, *, #106482, .T. ) ;
#98492 = CARTESIAN_POINT ( 'NONE',  ( 20.94999999999999574, 1.115600667400684642E-11, -134.0000000000000000 ) ) ;
#98494 = DIRECTION ( 'NONE',  ( 0.000000000000000000, 0.1568667991644355497, 0.9876197685951332295 ) ) ;
#98495 = ORIENTED_EDGE ( 'NONE', *, *, #249228, .T. ) ;
#98496 = AXIS2_PLACEMENT_3D ( 'NONE', #58145, #215943, #218499 ) ;
#98497 = CARTESIAN_POINT ( 'NONE',  ( -16.90137573187933739, 66.05000000001261640, -190.7346900604275675 ) ) ;
#98498 = ORIENTED_EDGE ( 'NONE', *, *, #79808, .F. ) ;
#98499 = CARTESIAN_POINT ( 'NONE',  ( -23.25000000000000000, 76.00000000001247713, -173.9231074845243654 ) ) ;
#98500 = CARTESIAN_POINT ( 'NONE',  ( 21.07954763557399502, 69.67070900997433114, -69.58898340314273412 ) ) ;
#98501 = CIRCLE ( 'NONE', #40342, 0.09999999999998898659 ) ;
#98502 = SPHERICAL_SURFACE ( 'NONE', #199355, 0.1000000000000000056 ) ;
#98503 = CARTESIAN_POINT ( 'NONE',  ( -20.94999999999999929, 77.36087058720467269, -195.4501095574333931 ) ) ;
#98504 = AXIS2_PLACEMENT_3D ( 'NONE', #117232, #172110, #132957 ) ;
#98505 = DIRECTION ( 'NONE',  ( 1.000000000000000000, -0.000000000000000000, 0.000000000000000000 ) ) ;
#98506 = ORIENTED_EDGE ( 'NONE', *, *, #100550, .T. ) ;
#98507 = FACE_OUTER_BOUND ( 'NONE', #144740, .T. ) ;
#98508 = CARTESIAN_POINT ( 'NONE',  ( 21.05000000000000071, 6.258847123090201414, -100.4682416469448469 ) ) ;
#98509 = CARTESIAN_POINT ( 'NONE',  ( -21.14999999999999858, -0.09999999999999939493, 11.64957080754480323 ) ) ;
#98510 = EDGE_CURVE ( 'NONE', #84718, #46280, #100355, .T. ) ;
#98511 = EDGE_LOOP ( 'NONE', ( #40646, #74226, #227013 ) ) ;
#98512 = DIRECTION ( 'NONE',  ( 1.000000000000000000, 0.000000000000000000, 0.000000000000000000 ) ) ;
#98513 = ORIENTED_EDGE ( 'NONE', *, *, #233844, .F. ) ;
#98514 = CARTESIAN_POINT ( 'NONE',  ( 20.94999999999999574, -11.74999999999999112, -2.900000000000003464 ) ) ;
#98515 = EDGE_LOOP ( 'NONE', ( #96625, #87642, #197007, #233496 ) ) ;
#98516 = DIRECTION ( 'NONE',  ( 3.469446951953635015E-14, -0.000000000000000000, 1.000000000000000000 ) ) ;
#98517 = DIRECTION ( 'NONE',  ( 0.000000000000000000, -6.982962677686266711E-15, 1.000000000000000000 ) ) ;
#98518 = VECTOR ( 'NONE', #89293, 1000.000000000000114 ) ;
#98521 = EDGE_LOOP ( 'NONE', ( #37552, #120832, #96885, #97307 ) ) ;
#98520 = EDGE_CURVE ( 'NONE', #33688, #145192, #120783, .T. ) ;
#98519 = CARTESIAN_POINT ( 'NONE',  ( -23.15000000000000213, 86.30329675166747450, -209.4258251677035787 ) ) ;
#98522 = CARTESIAN_POINT ( 'NONE',  ( -17.22361732159831860, 10.34515565861359399, -122.6292154741329199 ) ) ;
#98523 = ORIENTED_EDGE ( 'NONE', *, *, #69030, .T. ) ;
#98524 = CYLINDRICAL_SURFACE ( 'NONE', #77450, 0.1000000000000028644 ) ;
#98525 = ADVANCED_FACE ( 'NONE', ( #43791 ), #256347, .T. ) ;
#98526 = DIRECTION ( 'NONE',  ( 2.952720810173289112E-16, -1.000000000000000000, 0.000000000000000000 ) ) ;
#98527 = ORIENTED_EDGE ( 'NONE', *, *, #163176, .F. ) ;
#98528 = ORIENTED_EDGE ( 'NONE', *, *, #219597, .T. ) ;
#98529 = DIRECTION ( 'NONE',  ( 0.000000000000000000, 1.000000000000000000, 0.000000000000000000 ) ) ;
#98531 = ADVANCED_FACE ( 'NONE', ( #58191 ), #19082, .T. ) ;
#98530 = CARTESIAN_POINT ( 'NONE',  ( -22.50000000000093792, -3.180729737798012824, -228.0957332317256032 ) ) ;
#98532 = B_SPLINE_CURVE_WITH_KNOTS ( 'NONE', 3,
 ( #85725, #23257, #46616, #204415, #161475, #7511, #2360, #123617, #121078, #84430 ),
 .UNSPECIFIED., .F., .F.,
 ( 4, 3, 3, 4 ),
 ( 1.894079734586027345E-15, 3.877043166999228241E-05, 7.336897548477449270E-05, 7.659383120240587149E-05 ),
 .UNSPECIFIED. ) ;
#98533 = EDGE_LOOP ( 'NONE', ( #20395, #120585, #197360, #63076 ) ) ;
#98534 = CARTESIAN_POINT ( 'NONE',  ( 21.05000000000000071, 10.23309999692112804, -228.1193230868212254 ) ) ;
#98535 = VECTOR ( 'NONE', #73398, 1000.000000000000000 ) ;
#98536 = AXIS2_PLACEMENT_3D ( 'NONE', #252272, #117901, #59179 ) ;
#98537 = CIRCLE ( 'NONE', #81796, 0.2000000000000057288 ) ;
#98538 = VERTEX_POINT ( 'NONE', #217264 ) ;
#98539 = ORIENTED_EDGE ( 'NONE', *, *, #25189, .F. ) ;
#98540 = ADVANCED_FACE ( 'NONE', ( #59456 ), #246133, .F. ) ;
#98543 = EDGE_CURVE ( 'NONE', #154251, #149928, #104624, .T. ) ;
#98542 = ADVANCED_FACE ( 'NONE', ( #140298 ), #197720, .F. ) ;
#98541 = CYLINDRICAL_SURFACE ( 'NONE', #22320, 11.79999999999999716 ) ;
#98545 = EDGE_LOOP ( 'NONE', ( #86780, #179330, #172460, #96613 ) ) ;
#98544 = CARTESIAN_POINT ( 'NONE',  ( 18.59999999999999076, 10.20857864377385127, -54.85000000000000142 ) ) ;
#98546 = DIRECTION ( 'NONE',  ( 0.000000000000000000, -0.7397360091702802620, 0.6728971962616779878 ) ) ;
#98547 = FACE_OUTER_BOUND ( 'NONE', #16788, .T. ) ;
#98548 = DIRECTION ( 'NONE',  ( -1.000000000000000000, 0.000000000000000000, 0.000000000000000000 ) ) ;
#98549 = CIRCLE ( 'NONE', #15227, 4.049999999999998934 ) ;
#98551 = DIRECTION ( 'NONE',  ( 0.000000000000000000, -1.000000000000000000, 0.000000000000000000 ) ) ;
#98550 = CARTESIAN_POINT ( 'NONE',  ( 20.95483826173899899, 8.876166204781142710, -42.04627555289950891 ) ) ;
#98552 = PLANE ( 'NONE',  #73798 ) ;
#98553 = DIRECTION ( 'NONE',  ( 0.000000000000000000, -0.1975078988072421216, 0.9803012954743803853 ) ) ;
#98554 = AXIS2_PLACEMENT_3D ( 'NONE', #230520, #247508, #27211 ) ;
#98555 = AXIS2_PLACEMENT_3D ( 'NONE', #2622, #204670, #82144 ) ;
#98556 = CARTESIAN_POINT ( 'NONE',  ( 21.00000000000000000, 6.258114003436814343, 11.90000000000000036 ) ) ;
#98557 = SPHERICAL_SURFACE ( 'NONE', #180067, 0.1000000000000000056 ) ;
#98558 = EDGE_CURVE ( 'NONE', #79286, #183834, #227553, .T. ) ;
#98559 = EDGE_CURVE ( 'NONE', #10010, #36888, #250403, .T. ) ;
#98560 = VERTEX_POINT ( 'NONE', #24246 ) ;
#98561 = AXIS2_PLACEMENT_3D ( 'NONE', #208510, #126381, #109368 ) ;
#98563 = EDGE_LOOP ( 'NONE', ( #147709, #206943, #128381, #232082, #212462, #81575 ) ) ;
#98562 = CARTESIAN_POINT ( 'NONE',  ( 23.14999999999999858, 76.00000000001215028, -138.5231074845243313 ) ) ;
#98564 = ORIENTED_EDGE ( 'NONE', *, *, #199128, .F. ) ;
#98565 = EDGE_CURVE ( 'NONE', #89253, #192243, #96271, .T. ) ;
#98566 = DIRECTION ( 'NONE',  ( 0.000000000000000000, 0.5000683049008606273, 0.8659859643398268858 ) ) ;
#98567 = ORIENTED_EDGE ( 'NONE', *, *, #2783, .T. ) ;
#98568 = FACE_OUTER_BOUND ( 'NONE', #188005, .T. ) ;
#98569 = EDGE_CURVE ( 'NONE', #130475, #32767, #223687, .T. ) ;
#98570 = EDGE_LOOP ( 'NONE', ( #52452, #230176 ) ) ;
#98571 = CARTESIAN_POINT ( 'NONE',  ( 23.15000000000000213, -11.64999999998883595, -131.0000000000000284 ) ) ;
#98572 = EDGE_CURVE ( 'NONE', #63280, #228856, #145441, .T. ) ;
#98575 = EDGE_LOOP ( 'NONE', ( #187935, #31879, #243479, #197654 ) ) ;
#98574 = EDGE_LOOP ( 'NONE', ( #26034, #164338, #96441, #104470 ) ) ;
#98573 = CIRCLE ( 'NONE', #11149, 0.09999999999999939493 ) ;
#98576 = VERTEX_POINT ( 'NONE', #206712 ) ;
#98577 = ORIENTED_EDGE ( 'NONE', *, *, #189774, .F. ) ;
#98578 = DIRECTION ( 'NONE',  ( 0.000000000000000000, -0.9910465087640865089, 0.1335171055202867274 ) ) ;
#98579 = DIRECTION ( 'NONE',  ( 1.000000000000000000, 0.000000000000000000, 0.000000000000000000 ) ) ;
#98581 = ORIENTED_EDGE ( 'NONE', *, *, #50248, .T. ) ;
#98580 = DIRECTION ( 'NONE',  ( 1.000000000000000000, 0.000000000000000000, 0.000000000000000000 ) ) ;
#98582 = CARTESIAN_POINT ( 'NONE',  ( -20.85000000000000142, 7.021664781911246322, -137.8335654018973457 ) ) ;
#98583 = EDGE_CURVE ( 'NONE', #196889, #27581, #21306, .T. ) ;
#98584 = FACE_OUTER_BOUND ( 'NONE', #208921, .T. ) ;
#98586 = VERTEX_POINT ( 'NONE', #149332 ) ;
#98585 = DIRECTION ( 'NONE',  ( -0.000000000000000000, 6.982962677686266711E-15, -1.000000000000000000 ) ) ;
#98587 = CARTESIAN_POINT ( 'NONE',  ( -20.64999999999999858, -8.999999999988846255, -43.39396912265245021 ) ) ;
#98588 = ORIENTED_EDGE ( 'NONE', *, *, #179140, .F. ) ;
#98589 = AXIS2_PLACEMENT_3D ( 'NONE', #15996, #138450, #18538 ) ;
#98591 = ORIENTED_EDGE ( 'NONE', *, *, #187753, .F. ) ;
#98590 = CARTESIAN_POINT ( 'NONE',  ( 23.40000000000005187, 76.00000000001119815, -36.02310748452479316 ) ) ;
#98592 = LINE ( 'NONE', #240722, #64443 ) ;
#98593 = DIRECTION ( 'NONE',  ( 0.000000000000000000, -1.000000000000000000, -8.717686153663073805E-15 ) ) ;
#98594 = CARTESIAN_POINT ( 'NONE',  ( -15.75000000000000355, 9.350000000011140955, -184.2499999999999716 ) ) ;
#98595 = CIRCLE ( 'NONE', #86148, 0.1000000000000072220 ) ;
#98597 = EDGE_CURVE ( 'NONE', #245440, #241978, #9817, .T. ) ;
#98596 = ORIENTED_EDGE ( 'NONE', *, *, #212524, .F. ) ;
#98599 = DIRECTION ( 'NONE',  ( -3.265361837132813093E-16, -0.4088369013363281068, 0.9126074666063770380 ) ) ;
#98598 = CARTESIAN_POINT ( 'NONE',  ( -16.97683810757273193, 9.950000000011137047, -46.76357671246011449 ) ) ;
#98600 = FACE_OUTER_BOUND ( 'NONE', #50109, .T. ) ;
#98601 = CARTESIAN_POINT ( 'NONE',  ( -20.64999999999999858, 62.04148992963929743, -247.7470044306132024 ) ) ;
#98602 = CIRCLE ( 'NONE', #86154, 0.5000000000000007772 ) ;
#98603 = CARTESIAN_POINT ( 'NONE',  ( -18.50000000000000000, 5.949999999999945111, -10.30570230503485796 ) ) ;
#98604 = CARTESIAN_POINT ( 'NONE',  ( 17.23472005113827876, 14.76331920405063869, -220.3480848590899654 ) ) ;
#98605 = ORIENTED_EDGE ( 'NONE', *, *, #74356, .F. ) ;
#98606 = ORIENTED_EDGE ( 'NONE', *, *, #192494, .F. ) ;
#98607 = ORIENTED_EDGE ( 'NONE', *, *, #53381, .F. ) ;
#98608 =( GEOMETRIC_REPRESENTATION_CONTEXT ( 3 ) GLOBAL_UNCERTAINTY_ASSIGNED_CONTEXT ( ( #102614 ) ) GLOBAL_UNIT_ASSIGNED_CONTEXT ( ( #58915, #177649, #248 ) ) REPRESENTATION_CONTEXT ( 'NONE', 'WORKASPACE' ) );
#98609 = DIRECTION ( 'NONE',  ( 0.000000000000000000, -1.000000000000000000, 0.000000000000000000 ) ) ;
#98610 = VECTOR ( 'NONE', #71694, 1000.000000000000000 ) ;
#98611 = ORIENTED_EDGE ( 'NONE', *, *, #19339, .F. ) ;
#98612 = DIRECTION ( 'NONE',  ( -0.000000000000000000, 0.5041370733442164243, 0.8636236514130032349 ) ) ;
#98613 = ORIENTED_EDGE ( 'NONE', *, *, #11019, .T. ) ;
#98614 = ADVANCED_FACE ( 'NONE', ( #108889 ), #42141, .T. ) ;
#98616 = CARTESIAN_POINT ( 'NONE',  ( 20.94999999999999929, 76.00000000001169553, -67.52310748452430289 ) ) ;
#98615 = VECTOR ( 'NONE', #33644, 1000.000000000000000 ) ;
#98617 = CARTESIAN_POINT ( 'NONE',  ( -23.24999999999999645, 77.17949092533254429, -241.9177572069595783 ) ) ;
#98618 = ORIENTED_EDGE ( 'NONE', *, *, #237634, .T. ) ;
#98619 = LINE ( 'NONE', #135204, #215123 ) ;
#98620 = AXIS2_PLACEMENT_3D ( 'NONE', #78212, #18252, #234731 ) ;
#98621 = VERTEX_POINT ( 'NONE', #144147 ) ;
#98622 = ORIENTED_EDGE ( 'NONE', *, *, #53466, .T. ) ;
#98623 = TOROIDAL_SURFACE ( 'NONE', #86170, 0.9750000000000019762, 0.1000000000000000056 ) ;
#98624 = ORIENTED_EDGE ( 'NONE', *, *, #59349, .F. ) ;
#98626 = DIRECTION ( 'NONE',  ( 0.000000000000000000, -6.467318590049456648E-15, 1.000000000000000000 ) ) ;
#98625 = AXIS2_PLACEMENT_3D ( 'NONE', #125311, #24944, #103149 ) ;
#98627 = DIRECTION ( 'NONE',  ( 0.000000000000000000, 0.4930308989875313852, 0.8700118002898274971 ) ) ;
#98628 = CARTESIAN_POINT ( 'NONE',  ( 18.49999999999999645, 46.55954744353147134, -243.3218549665227783 ) ) ;
#98629 = DIRECTION ( 'NONE',  ( 0.000000000000000000, -0.1568667991644693838, -0.9876197685951279004 ) ) ;
#98630 = CIRCLE ( 'NONE', #202906, 0.1000000000000028227 ) ;
#98631 = CARTESIAN_POINT ( 'NONE',  ( 15.73863059295127798, 66.64859682587035650, -119.5435770476858863 ) ) ;
#98633 = DIRECTION ( 'NONE',  ( 0.000000000000000000, -0.9908441862701596881, -0.1350103645451904977 ) ) ;
#98632 = FACE_OUTER_BOUND ( 'NONE', #18109, .T. ) ;
#98634 = CARTESIAN_POINT ( 'NONE',  ( -23.15000000000000213, 76.00000000001237765, -170.0231074845243597 ) ) ;
#98636 = ORIENTED_EDGE ( 'NONE', *, *, #94412, .F. ) ;
#98635 = CARTESIAN_POINT ( 'NONE',  ( 20.94999999999999574, 6.400000000000003020, -9.930424630061574831 ) ) ;
#98637 = DIRECTION ( 'NONE',  ( 0.000000000000000000, -0.9126074666063769270, -0.4088369013363280513 ) ) ;
#98638 = ORIENTED_EDGE ( 'NONE', *, *, #155095, .T. ) ;
#98639 = VECTOR ( 'NONE', #151788, 1000.000000000000000 ) ;
#98640 = FACE_OUTER_BOUND ( 'NONE', #257499, .T. ) ;
#98641 = AXIS2_PLACEMENT_3D ( 'NONE', #56579, #137419, #216953 ) ;
#98642 = ORIENTED_EDGE ( 'NONE', *, *, #234133, .F. ) ;
#98643 = VERTEX_POINT ( 'NONE', #165016 ) ;
#98644 = CARTESIAN_POINT ( 'NONE',  ( -23.25000000000000000, 85.60000000001159037, -59.62913836187181005 ) ) ;
#98645 = DIRECTION ( 'NONE',  ( -1.000000000000000000, 0.000000000000000000, 0.000000000000000000 ) ) ;
#98646 = DIRECTION ( 'NONE',  ( 1.000000000000000000, 0.000000000000000000, 0.000000000000000000 ) ) ;
#98647 = VERTEX_POINT ( 'NONE', #7209 ) ;
#98648 = AXIS2_PLACEMENT_3D ( 'NONE', #22336, #100521, #121442 ) ;
#98649 = CARTESIAN_POINT ( 'NONE',  ( -23.25000000000000000, 70.05000000001177796, -79.82880978955917328 ) ) ;
#98651 = ORIENTED_EDGE ( 'NONE', *, *, #168222, .F. ) ;
#98650 = CIRCLE ( 'NONE', #144453, 2.000000000000001776 ) ;
#98652 = EDGE_LOOP ( 'NONE', ( #196988, #181725, #43649, #1650 ) ) ;
#98653 = CARTESIAN_POINT ( 'NONE',  ( -16.89318236219976654, 9.951535257875130824, -12.64487036789414276 ) ) ;
#98654 = ORIENTED_EDGE ( 'NONE', *, *, #185441, .F. ) ;
#98655 = DIRECTION ( 'NONE',  ( -1.000000000000000000, -0.000000000000000000, -0.000000000000000000 ) ) ;
#98656 = CARTESIAN_POINT ( 'NONE',  ( -18.59999999999999787, 52.13794731297493712, -232.3713824252124880 ) ) ;
#98657 = ORIENTED_EDGE ( 'NONE', *, *, #139451, .F. ) ;
#98658 = DIRECTION ( 'NONE',  ( 0.000000000000000000, 0.000000000000000000, 1.000000000000000000 ) ) ;
#98659 = CARTESIAN_POINT ( 'NONE',  ( -16.83794479845801817, 9.926357419362648926, -121.1964447042223441 ) ) ;
#98660 = CYLINDRICAL_SURFACE ( 'NONE', #250835, 0.1000000000000013656 ) ;
#98661 = ORIENTED_EDGE ( 'NONE', *, *, #31560, .T. ) ;
#98662 = DIRECTION ( 'NONE',  ( 1.000000000000000000, 0.000000000000000000, 0.000000000000000000 ) ) ;
#98664 = EDGE_CURVE ( 'NONE', #165658, #203380, #39364, .T. ) ;
#98663 = FACE_OUTER_BOUND ( 'NONE', #243351, .T. ) ;
#98665 = FACE_OUTER_BOUND ( 'NONE', #91969, .T. ) ;
#98666 = EDGE_LOOP ( 'NONE', ( #189523, #177513, #236430, #4640 ) ) ;
#98667 = AXIS2_PLACEMENT_3D ( 'NONE', #178163, #21641, #120763 ) ;
#98669 = ORIENTED_EDGE ( 'NONE', *, *, #29422, .T. ) ;
#98668 = DIRECTION ( 'NONE',  ( 0.000000000000000000, -1.000000000000000000, 0.000000000000000000 ) ) ;
#98670 = ORIENTED_EDGE ( 'NONE', *, *, #132052, .F. ) ;
#98671 = CARTESIAN_POINT ( 'NONE',  ( -22.39999999999999858, 1.115600667400684642E-11, -67.00000000000004263 ) ) ;
#98672 = DIRECTION ( 'NONE',  ( -0.000000000000000000, 0.000000000000000000, -1.000000000000000000 ) ) ;
#98673 = CARTESIAN_POINT ( 'NONE',  ( 23.15000000000000213, -8.999999999988842703, -191.1060308773475072 ) ) ;
#98675 = VECTOR ( 'NONE', #9702, 1000.000000000000000 ) ;
#98674 = DIRECTION ( 'NONE',  ( 1.000000000000000000, 0.000000000000000000, 0.000000000000000000 ) ) ;
#98676 = CARTESIAN_POINT ( 'NONE',  ( -16.92973740335363075, 9.992503814478597590, -46.09394096479768166 ) ) ;
#98677 = DIRECTION ( 'NONE',  ( -1.000000000000000000, -0.000000000000000000, -0.000000000000000000 ) ) ;
#98678 = EDGE_CURVE ( 'NONE', #9680, #133293, #225252, .T. ) ;
#98679 = EDGE_CURVE ( 'NONE', #15467, #226290, #167056, .T. ) ;
#98681 = ORIENTED_EDGE ( 'NONE', *, *, #161398, .T. ) ;
#98680 = CIRCLE ( 'NONE', #182120, 0.09999999999999741040 ) ;
#98682 = DIRECTION ( 'NONE',  ( 0.000000000000000000, -0.4721928772777346239, -0.8814952561688430555 ) ) ;
#98683 = CARTESIAN_POINT ( 'NONE',  ( 18.39999999999999503, 64.25000000001188027, -90.37310748452439668 ) ) ;
#98684 = AXIS2_PLACEMENT_3D ( 'NONE', #202, #75900, #155478 ) ;
#98685 = AXIS2_PLACEMENT_3D ( 'NONE', #58554, #178555, #79402 ) ;
#98686 = CARTESIAN_POINT ( 'NONE',  ( -23.15000000000000213, -4.656943609564678788, -233.1535107627236414 ) ) ;
#98687 = DIRECTION ( 'NONE',  ( -1.000000000000000000, -3.265361837132813093E-16, 0.000000000000000000 ) ) ;
#98688 = CARTESIAN_POINT ( 'NONE',  ( 20.94999999999999929, 77.83534155023701828, -191.9679561919613491 ) ) ;
#98689 = CIRCLE ( 'NONE', #132051, 0.1000000000000028644 ) ;
#98690 = EDGE_LOOP ( 'NONE', ( #180595, #95685, #110655, #16190 ) ) ;
#98691 = ORIENTED_EDGE ( 'NONE', *, *, #53896, .T. ) ;
#98692 = CARTESIAN_POINT ( 'NONE',  ( 23.15000000000000213, -8.999999999988842703, -158.1060308773475640 ) ) ;
#98693 = CARTESIAN_POINT ( 'NONE',  ( 22.39999999999999503, 64.25000000001213607, -136.4231074845243938 ) ) ;
#98695 = EDGE_CURVE ( 'NONE', #230368, #78926, #87877, .T. ) ;
#98694 = FACE_OUTER_BOUND ( 'NONE', #183198, .T. ) ;
#98696 = DIRECTION ( 'NONE',  ( 0.000000000000000000, -0.000000000000000000, -1.000000000000000000 ) ) ;
#98697 = CARTESIAN_POINT ( 'NONE',  ( -20.94999999999999929, -1.835341550213255957, -145.5551512925629822 ) ) ;
#98698 = EDGE_CURVE ( 'NONE', #233017, #146658, #204127, .T. ) ;
#98699 = ORIENTED_EDGE ( 'NONE', *, *, #132689, .T. ) ;
#98700 = CARTESIAN_POINT ( 'NONE',  ( 18.49999999999999645, 1.736257131608553550, -145.5686523290175387 ) ) ;
#98701 = EDGE_CURVE ( 'NONE', #101967, #41050, #65921, .T. ) ;
#98702 = AXIS2_PLACEMENT_3D ( 'NONE', #6581, #209945, #250335 ) ;
#98703 = DIRECTION ( 'NONE',  ( 0.000000000000000000, -6.938893903907222067E-15, 1.000000000000000000 ) ) ;
#98704 = ORIENTED_EDGE ( 'NONE', *, *, #166601, .T. ) ;
#98705 = DIRECTION ( 'NONE',  ( 0.000000000000000000, -1.000000000000000000, -2.891205793294679805E-16 ) ) ;
#98706 = EDGE_CURVE ( 'NONE', #168941, #185684, #8804, .T. ) ;
#98707 = DIRECTION ( 'NONE',  ( -1.000000000000000000, -0.000000000000000000, 0.000000000000000000 ) ) ;
#98708 = AXIS2_PLACEMENT_3D ( 'NONE', #81421, #180562, #83969 ) ;
#98709 = EDGE_CURVE ( 'NONE', #31018, #74117, #111466, .T. ) ;
#98710 = ORIENTED_EDGE ( 'NONE', *, *, #232770, .F. ) ;
#98711 = PLANE ( 'NONE',  #227491 ) ;
#98712 = VERTEX_POINT ( 'NONE', #131023 ) ;
#98713 = DIRECTION ( 'NONE',  ( 0.000000000000000000, 0.000000000000000000, 1.000000000000000000 ) ) ;
#98714 = DIRECTION ( 'NONE',  ( 0.000000000000000000, 0.1568667991644355497, 0.9876197685951332295 ) ) ;
#98715 = CARTESIAN_POINT ( 'NONE',  ( 20.94999999999999929, -1.164121893230052995, -141.9148480855716343 ) ) ;
#98716 = DIRECTION ( 'NONE',  ( 0.000000000000000000, -1.000000000000000000, 0.000000000000000000 ) ) ;
#98717 = DIRECTION ( 'NONE',  ( -1.000000000000000000, -0.000000000000000000, -0.000000000000000000 ) ) ;
#98718 = DIRECTION ( 'NONE',  ( -0.000000000000000000, -0.000000000000000000, -1.000000000000000000 ) ) ;
#98719 = DIRECTION ( 'NONE',  ( 0.000000000000000000, -7.189901751995769991E-15, 1.000000000000000000 ) ) ;
#98720 = CARTESIAN_POINT ( 'NONE',  ( -21.44999999999999929, 11.60596396992030144, -220.2204734678737168 ) ) ;
#98721 = B_SPLINE_CURVE_WITH_KNOTS ( 'NONE', 3,
 ( #82624, #160932, #220876, #240454, #61823, #121805, #102187, #181769 ),
 .UNSPECIFIED., .F., .F.,
 ( 4, 2, 2, 4 ),
 ( 0.000000000000000000, 0.0002181133598169061188, 0.0003271700397253531610, 0.0004362267196338002031 ),
 .UNSPECIFIED. ) ;
#98722 = ADVANCED_FACE ( 'NONE', ( #93176 ), #110170, .T. ) ;
#98723 = CARTESIAN_POINT ( 'NONE',  ( -23.25000000000000000, 70.05000000001221849, -146.8288097895591875 ) ) ;
#98724 = DIRECTION ( 'NONE',  ( -1.000000000000000000, -0.000000000000000000, 0.000000000000000000 ) ) ;
#98725 = DIRECTION ( 'NONE',  ( -0.000000000000000000, 1.000000000000000000, 8.717686153663073805E-15 ) ) ;
#98726 = CARTESIAN_POINT ( 'NONE',  ( 18.59999999999999432, -1.162701749926853712, -175.5999999999999659 ) ) ;
#98727 = AXIS2_PLACEMENT_3D ( 'NONE', #187591, #68924, #87165 ) ;
#98728 = AXIS2_PLACEMENT_3D ( 'NONE', #40046, #157434, #236928 ) ;
#98729 = CIRCLE ( 'NONE', #232072, 4.900000000000001243 ) ;
#98730 = AXIS2_PLACEMENT_3D ( 'NONE', #125020, #246241, #25917 ) ;
#98731 = CARTESIAN_POINT ( 'NONE',  ( 21.11344571971287465, 10.61787902352919666, -79.24602089239978397 ) ) ;
#98732 = DIRECTION ( 'NONE',  ( 0.000000000000000000, 0.5907332058517377193, -0.8068669527896954463 ) ) ;
#98733 = ORIENTED_EDGE ( 'NONE', *, *, #251721, .T. ) ;
#98734 = DIRECTION ( 'NONE',  ( -0.000000000000000000, -0.9910827722268049644, -0.1332476588733589318 ) ) ;
#98735 = DIRECTION ( 'NONE',  ( 1.000000000000000000, 7.304098846218134667E-16, -0.000000000000000000 ) ) ;
#98736 = LINE ( 'NONE', #252091, #122738 ) ;
#98737 = EDGE_LOOP ( 'NONE', ( #100699, #48735, #27807, #31273 ) ) ;
#98738 = CYLINDRICAL_SURFACE ( 'NONE', #55705, 4.049999999999987388 ) ;
#98739 = CARTESIAN_POINT ( 'NONE',  ( -18.40000000000000213, 59.20211495293902004, -220.5705723384363921 ) ) ;
#98740 = ORIENTED_EDGE ( 'NONE', *, *, #165695, .T. ) ;
#98741 = AXIS2_PLACEMENT_3D ( 'NONE', #226801, #208548, #29917 ) ;
#98742 = CARTESIAN_POINT ( 'NONE',  ( -16.87786941232801396, 9.958154714156124854, -188.3771857997939492 ) ) ;
#98743 = CARTESIAN_POINT ( 'NONE',  ( 18.59999999999999076, 6.550000000011156231, -155.2500000000000284 ) ) ;
#98744 = AXIS2_PLACEMENT_3D ( 'NONE', #146492, #10863, #227330 ) ;
#98745 = ORIENTED_EDGE ( 'NONE', *, *, #126868, .T. ) ;
#98746 = EDGE_CURVE ( 'NONE', #96108, #12116, #194997, .T. ) ;
#98747 = CIRCLE ( 'NONE', #256960, 0.2000000000000057288 ) ;
#98748 = ADVANCED_FACE ( 'NONE', ( #94458 ), #213127, .F. ) ;
#98749 = VERTEX_POINT ( 'NONE', #170210 ) ;
#98750 = FACE_OUTER_BOUND ( 'NONE', #61216, .T. ) ;
#98751 = ORIENTED_EDGE ( 'NONE', *, *, #106662, .T. ) ;
#98752 = EDGE_CURVE ( 'NONE', #44711, #206438, #62967, .T. ) ;
#98754 = ADVANCED_FACE ( 'NONE', ( #35800 ), #254775, .T. ) ;
#98753 = CARTESIAN_POINT ( 'NONE',  ( 21.14999999999999858, -1.124859753953710850E-15, 6.540656951701244282 ) ) ;
#98755 = CARTESIAN_POINT ( 'NONE',  ( -23.25000000000000000, 76.00000000001190870, -103.0231074845243029 ) ) ;
#98756 = FACE_OUTER_BOUND ( 'NONE', #136085, .T. ) ;
#98757 = DIRECTION ( 'NONE',  ( 1.000000000000000000, 0.000000000000000000, 0.000000000000000000 ) ) ;
#98758 = DIRECTION ( 'NONE',  ( 0.000000000000000000, 0.000000000000000000, -1.000000000000000000 ) ) ;
#98759 = CARTESIAN_POINT ( 'NONE',  ( -14.23072895065542731, 46.49260333018393965, -234.7842902611276656 ) ) ;
#98760 = EDGE_CURVE ( 'NONE', #88314, #225371, #71553, .T. ) ;
#98761 = CYLINDRICAL_SURFACE ( 'NONE', #196911, 0.09999999999999982514 ) ;
#98762 = DIRECTION ( 'NONE',  ( 0.000000000000000000, 1.000000000000000000, -0.000000000000000000 ) ) ;
#98764 = ORIENTED_EDGE ( 'NONE', *, *, #37036, .T. ) ;
#98763 = DIRECTION ( 'NONE',  ( 0.000000000000000000, -0.000000000000000000, -1.000000000000000000 ) ) ;
#98765 = ORIENTED_EDGE ( 'NONE', *, *, #108778, .F. ) ;
#98767 = CARTESIAN_POINT ( 'NONE',  ( -21.00250684356851849, 64.25000000001161027, -62.50830171576457417 ) ) ;
#98766 = CARTESIAN_POINT ( 'NONE',  ( 22.49999999999999645, 0.04562336059637162045, 11.65050433855055978 ) ) ;
#98769 = VERTEX_POINT ( 'NONE', #30673 ) ;
#98768 = CARTESIAN_POINT ( 'NONE',  ( 21.09696443733127325, 10.72400988392963228, -146.2347775270482373 ) ) ;
#98770 = EDGE_CURVE ( 'NONE', #27502, #65123, #46563, .T. ) ;
#98771 = ORIENTED_EDGE ( 'NONE', *, *, #145328, .T. ) ;
#98772 = DIRECTION ( 'NONE',  ( 1.000000000000000000, 0.000000000000000000, 0.000000000000000000 ) ) ;
#98773 = EDGE_CURVE ( 'NONE', #195816, #86047, #113035, .T. ) ;
#98774 = CARTESIAN_POINT ( 'NONE',  ( 20.74625933824108870, 8.882913521095431975, -176.0551710241120418 ) ) ;
#98776 = ADVANCED_FACE ( 'NONE', ( #73652 ), #50187, .T. ) ;
#98775 = DIRECTION ( 'NONE',  ( -0.000000000000000000, -0.000000000000000000, 1.000000000000000000 ) ) ;
#98777 = CARTESIAN_POINT ( 'NONE',  ( 20.95000000000005613, 67.65000000001118963, -3.123107484524795474 ) ) ;
#98779 = CARTESIAN_POINT ( 'NONE',  ( -18.40000000000000213, 20.70659057908908096, -227.9750359040556873 ) ) ;
#98778 = VECTOR ( 'NONE', #171569, 1000.000000000000000 ) ;
#98780 = CARTESIAN_POINT ( 'NONE',  ( 23.15000000000000213, 78.50726470275242264, -228.6618886302502176 ) ) ;
#98781 = EDGE_CURVE ( 'NONE', #257876, #146129, #192296, .T. ) ;
#98783 = CIRCLE ( 'NONE', #202869, 0.9000000000000014655 ) ;
#98782 = FACE_OUTER_BOUND ( 'NONE', #34475, .T. ) ;
#98784 = ORIENTED_EDGE ( 'NONE', *, *, #66408, .T. ) ;
#98785 = ORIENTED_EDGE ( 'NONE', *, *, #146572, .T. ) ;
#98786 = CARTESIAN_POINT ( 'NONE',  ( -23.15000000000000213, 4.150000000011156764, -179.8499999999999943 ) ) ;
#98787 = EDGE_CURVE ( 'NONE', #28696, #60057, #13649, .T. ) ;
#98788 = ADVANCED_FACE ( 'NONE', ( #54052 ), #55302, .F. ) ;
#98789 = VECTOR ( 'NONE', #85637, 1000.000000000000000 ) ;
#98790 = ORIENTED_EDGE ( 'NONE', *, *, #6850, .F. ) ;
#98791 = CARTESIAN_POINT ( 'NONE',  ( 18.59999999999999432, 74.73821383144729680, -161.9366085209788935 ) ) ;
#98792 = VERTEX_POINT ( 'NONE', #120485 ) ;
#98793 = DIRECTION ( 'NONE',  ( 1.000000000000000000, 0.000000000000000000, 0.000000000000000000 ) ) ;
#98794 = PRODUCT_DEFINITION_FORMATION_WITH_SPECIFIED_SOURCE ( 'ANY', '', #32833, .NOT_KNOWN. ) ;
#98795 = ADVANCED_FACE ( 'NONE', ( #17492 ), #56588, .F. ) ;
#98796 = AXIS2_PLACEMENT_3D ( 'NONE', #184885, #63651, #25822 ) ;
#98797 = CARTESIAN_POINT ( 'NONE',  ( -13.11924609551135212, 49.48471825922439393, -233.4704840993163373 ) ) ;
#98798 = DIRECTION ( 'NONE',  ( -0.000000000000000000, -0.9126074666063770380, -0.4088369013363281068 ) ) ;
#98799 = AXIS2_PLACEMENT_3D ( 'NONE', #174425, #53137, #210934 ) ;
#98800 = CYLINDRICAL_SURFACE ( 'NONE', #143902, 0.1000000000000055844 ) ;
#98801 = ADVANCED_FACE ( 'NONE', ( #38356 ), #20081, .F. ) ;
#98802 = FACE_OUTER_BOUND ( 'NONE', #116657, .T. ) ;
#98803 = EDGE_LOOP ( 'NONE', ( #185090, #217722, #167026 ) ) ;
#98804 = EDGE_CURVE ( 'NONE', #250208, #178866, #8985, .T. ) ;
#98805 = DIRECTION ( 'NONE',  ( 0.000000000000000000, 0.000000000000000000, -1.000000000000000000 ) ) ;
#98806 = CARTESIAN_POINT ( 'NONE',  ( -20.64999999999999858, 85.00000000001222134, -146.0170766071767332 ) ) ;
#98807 = DIRECTION ( 'NONE',  ( 0.000000000000000000, 0.4583618696494374256, 0.8887656589064814039 ) ) ;
#98808 = CARTESIAN_POINT ( 'NONE',  ( -21.14999999999999858, -0.09999999998884338825, -160.9593430482987344 ) ) ;
#98809 = DIRECTION ( 'NONE',  ( 1.000000000000000000, 0.000000000000000000, -0.000000000000000000 ) ) ;
#98810 = ORIENTED_EDGE ( 'NONE', *, *, #3507, .T. ) ;
#98811 = CARTESIAN_POINT ( 'NONE',  ( -18.39999999999999858, 85.68240343348777799, -29.36626410711147983 ) ) ;
#98812 = AXIS2_PLACEMENT_3D ( 'NONE', #68954, #209730, #225414 ) ;
#98813 = VERTEX_POINT ( 'NONE', #201263 ) ;
#98815 = ORIENTED_EDGE ( 'NONE', *, *, #244905, .T. ) ;
#98814 = CARTESIAN_POINT ( 'NONE',  ( -21.05000000000000071, 1.115600667400684642E-11, -100.5000000000000284 ) ) ;
#98816 = DIRECTION ( 'NONE',  ( 0.000000000000000000, 0.000000000000000000, 1.000000000000000000 ) ) ;
#98817 = CIRCLE ( 'NONE', #73941, 0.09999999999999864553 ) ;
#98818 = AXIS2_PLACEMENT_3D ( 'NONE', #189064, #54676, #152538 ) ;
#98819 = EDGE_LOOP ( 'NONE', ( #225054, #97086, #121415, #50618 ) ) ;
#98820 = AXIS2_PLACEMENT_3D ( 'NONE', #10646, #227105, #167184 ) ;
#98822 = CARTESIAN_POINT ( 'NONE',  ( 5.999999999999995559, -11.25000000000000000, 10.00000000000000178 ) ) ;
#98821 =( BOUNDED_SURFACE ( )  B_SPLINE_SURFACE ( 3, 2, ( 
 ( #251990, #128203, #13397 ),
 ( #113761, #92907, #193317 ),
 ( #189462, #108631, #172517 ),
 ( #34268, #89056, #132049 ),
 ( #14702, #53794, #94191 ),
 ( #188178, #211596, #69528 ) ),
 .UNSPECIFIED., .F., .F., .F. ) 
 B_SPLINE_SURFACE_WITH_KNOTS ( ( 4, 2, 4 ),
 ( 3, 3 ),
 ( 0.0001300404313046710908, 0.0003183318589266662135, 0.0005066232865486613090 ),
 ( 0.000000000000000000, 1.000000000000000000 ),
 .UNSPECIFIED. ) 
 GEOMETRIC_REPRESENTATION_ITEM ( )  RATIONAL_B_SPLINE_SURFACE ( (
 ( 1.000000000000000000, 0.7071067811865597852, 1.000000000000000000),
 ( 1.000000000000000000, 0.7625113560545420111, 1.000000000000000000),
 ( 1.000000000000000000, 0.8126073484681639592, 1.000000000000000000),
 ( 1.000000000000000000, 0.8923049332739299011, 1.000000000000000000),
 ( 1.000000000000000000, 0.9231914937764394979, 1.000000000000000000),
 ( 1.000000000000000000, 0.9238795325112900692, 1.000000000000000000) ) ) 
 REPRESENTATION_ITEM ( '' )  SURFACE ( )  );
#98823 = AXIS2_PLACEMENT_3D ( 'NONE', #36349, #53323, #237095 ) ;
#98824 = DIRECTION ( 'NONE',  ( -1.000000000000000000, 0.000000000000000000, 0.000000000000000000 ) ) ;
#98825 = UNCERTAINTY_MEASURE_WITH_UNIT (LENGTH_MEASURE( 1.000000000000000082E-05 ), #203409, 'distance_accuracy_value', 'NONE');
#98827 = VERTEX_POINT ( 'NONE', #176595 ) ;
#98826 = DIRECTION ( 'NONE',  ( 1.000000000000000000, -3.265361837132813093E-16, -2.280189983783949500E-30 ) ) ;
#98828 = LINE ( 'NONE', #18044, #147668 ) ;
#98829 = EDGE_LOOP ( 'NONE', ( #805, #132543, #105882 ) ) ;
#98830 = CARTESIAN_POINT ( 'NONE',  ( 23.15000000000000213, -8.729782940176418649, -238.4538547387928986 ) ) ;
#98831 = CARTESIAN_POINT ( 'NONE',  ( -16.94333152882356330, 9.990342011468825945, -188.3920315311014519 ) ) ;
#98832 = CARTESIAN_POINT ( 'NONE',  ( -16.81095280782811230, 44.13548170601814746, -235.2989316066078231 ) ) ;
#98833 = AXIS2_PLACEMENT_3D ( 'NONE', #74311, #155132, #237207 ) ;
#98834 = ORIENTED_EDGE ( 'NONE', *, *, #34764, .T. ) ;
#98835 = FACE_OUTER_BOUND ( 'NONE', #58276, .T. ) ;
#98837 = VERTEX_POINT ( 'NONE', #237831 ) ;
#98836 = AXIS2_PLACEMENT_3D ( 'NONE', #215478, #277, #159378 ) ;
#98839 = AXIS2_PLACEMENT_3D ( 'NONE', #179852, #161580, #138117 ) ;
#98838 = CARTESIAN_POINT ( 'NONE',  ( 22.39999999999999503, 65.19201463318205469, -243.3742797652979277 ) ) ;
#98840 = PLANE ( 'NONE',  #247301 ) ;
#98841 = CARTESIAN_POINT ( 'NONE',  ( 23.14999999999999858, 28.40523720341322544, -239.6697522603257937 ) ) ;
#98842 = ORIENTED_EDGE ( 'NONE', *, *, #149409, .F. ) ;
#98843 = CARTESIAN_POINT ( 'NONE',  ( 21.13507111622890022, 22.98723109724109293, -230.0690844087343407 ) ) ;
#98844 = CARTESIAN_POINT ( 'NONE',  ( -21.64999999999999858, 66.65000000001263913, -194.2731074845244166 ) ) ;
#98845 = AXIS2_PLACEMENT_3D ( 'NONE', #75874, #194571, #233678 ) ;
#98846 = EDGE_CURVE ( 'NONE', #22594, #129337, #114147, .T. ) ;
#98847 = DIRECTION ( 'NONE',  ( 0.000000000000000000, 1.000000000000000000, 6.982962677686266711E-15 ) ) ;
#98848 = AXIS2_PLACEMENT_3D ( 'NONE', #223072, #139665, #183953 ) ;
#98849 = ORIENTED_EDGE ( 'NONE', *, *, #154169, .T. ) ;
#98850 = DIRECTION ( 'NONE',  ( 1.000000000000000000, 0.000000000000000000, -0.000000000000000000 ) ) ;
#98852 = ADVANCED_FACE ( 'NONE', ( #137427 ), #70002, .T. ) ;
#98851 = PLANE ( 'NONE',  #223254 ) ;
#98853 = CARTESIAN_POINT ( 'NONE',  ( 21.05000000000000426, 69.58617371119866846, -69.43736654749098136 ) ) ;
#98854 = ORIENTED_EDGE ( 'NONE', *, *, #75607, .T. ) ;
#98855 = CIRCLE ( 'NONE', #169863, 0.3999999999999975797 ) ;
#98856 = EDGE_CURVE ( 'NONE', #19120, #195524, #100532, .T. ) ;
#98857 = DIRECTION ( 'NONE',  ( 0.000000000000000000, -0.000000000000000000, 1.000000000000000000 ) ) ;
#98858 = EDGE_LOOP ( 'NONE', ( #207349, #247140, #141242, #46917 ) ) ;
#98861 = EDGE_CURVE ( 'NONE', #16613, #100689, #179691, .T. ) ;
#98860 = ORIENTED_EDGE ( 'NONE', *, *, #106647, .T. ) ;
#98859 = DIRECTION ( 'NONE',  ( -7.304098846218201720E-16, 1.000000000000000000, 0.000000000000000000 ) ) ;
#98862 = AXIS2_PLACEMENT_3D ( 'NONE', #48532, #105913, #128079 ) ;
#98863 = AXIS2_PLACEMENT_3D ( 'NONE', #140941, #79650, #68776 ) ;
#98866 = ORIENTED_EDGE ( 'NONE', *, *, #207477, .T. ) ;
#98865 = ORIENTED_EDGE ( 'NONE', *, *, #210203, .F. ) ;
#98864 = CARTESIAN_POINT ( 'NONE',  ( -6.099999999999939249, 64.35000000001120668, -22.12310748452479103 ) ) ;
#98867 = CARTESIAN_POINT ( 'NONE',  ( 21.05000000000000071, 65.27628289530437655, -95.35819391543677170 ) ) ;
#98868 = AXIS2_PLACEMENT_3D ( 'NONE', #201967, #25902, #203240 ) ;
#98869 = CARTESIAN_POINT ( 'NONE',  ( -20.89878130938411616, 65.67252876774480796, -30.44570419949946327 ) ) ;
#98870 = AXIS2_PLACEMENT_3D ( 'NONE', #74981, #230169, #94503 ) ;
#98871 = DIRECTION ( 'NONE',  ( -1.000000000000000000, 0.000000000000000000, 0.000000000000000000 ) ) ;
#98872 = TOROIDAL_SURFACE ( 'NONE', #194799, 0.2000000000000000111, 0.1000000000000000056 ) ;
#98873 = CARTESIAN_POINT ( 'NONE',  ( -16.79270642812254977, 12.41271867757595260, -211.2545014300695243 ) ) ;
#98874 = PLANE ( 'NONE',  #136686 ) ;
#98875 = CARTESIAN_POINT ( 'NONE',  ( -21.14999999999999858, 76.00000000001276135, -215.1726782920691505 ) ) ;
#98876 = AXIS2_PLACEMENT_3D ( 'NONE', #49219, #251260, #170512 ) ;
#98877 = DIRECTION ( 'NONE',  ( 0.000000000000000000, -0.4721928772777212457, -0.8814952561688502719 ) ) ;
#98879 = DIRECTION ( 'NONE',  ( -1.000000000000000000, -2.885090398161910739E-16, -6.283419270304611573E-17 ) ) ;
#98878 = CARTESIAN_POINT ( 'NONE',  ( 23.25000000000000000, 87.65000000001165859, -69.52310748452424605 ) ) ;
#98880 = EDGE_CURVE ( 'NONE', #205753, #157859, #67238, .T. ) ;
#98881 = EDGE_LOOP ( 'NONE', ( #86308, #242243, #137274, #218070 ) ) ;
#98882 = ORIENTED_EDGE ( 'NONE', *, *, #66559, .T. ) ;
#98883 = CARTESIAN_POINT ( 'NONE',  ( -20.65000000000000568, 7.250000000011138646, -54.35000000000000142 ) ) ;
#98885 = VERTEX_POINT ( 'NONE', #244232 ) ;
#98884 = LINE ( 'NONE', #181044, #28686 ) ;
#98886 = CARTESIAN_POINT ( 'NONE',  ( 20.85000000000000142, 64.25000000001175238, -76.30697314750248950 ) ) ;
#98887 = ORIENTED_EDGE ( 'NONE', *, *, #9901, .T. ) ;
#98888 = CARTESIAN_POINT ( 'NONE',  ( 23.15000000000000213, -11.74999999998883737, -188.8499999999999659 ) ) ;
#98889 = ORIENTED_EDGE ( 'NONE', *, *, #196269, .T. ) ;
#98890 = CARTESIAN_POINT ( 'NONE',  ( 20.02499999999999858, 63.38346053167636995, -212.7939182281409956 ) ) ;
#98891 = AXIS2_PLACEMENT_3D ( 'NONE', #111601, #72487, #30803 ) ;
#98892 = ADVANCED_FACE ( 'NONE', ( #46042 ), #48611, .F. ) ;
#98893 = ORIENTED_EDGE ( 'NONE', *, *, #163516, .F. ) ;
#98894 = LINE ( 'NONE', #212476, #189539 ) ;
#98895 = CARTESIAN_POINT ( 'NONE',  ( -23.25000000000000000, -11.65000000000000036, 11.75000000000000000 ) ) ;
#98896 = ADVANCED_FACE ( 'NONE', ( #5609 ), #225936, .F. ) ;
#98897 = AXIS2_PLACEMENT_3D ( 'NONE', #202388, #23785, #197250 ) ;
#98899 = VERTEX_POINT ( 'NONE', #47310 ) ;
#98898 = ORIENTED_EDGE ( 'NONE', *, *, #177166, .T. ) ;
#98900 = ORIENTED_EDGE ( 'NONE', *, *, #83790, .T. ) ;
#98901 = CARTESIAN_POINT ( 'NONE',  ( -23.15000000000000213, -11.74999999998884448, -97.40000000000004832 ) ) ;
#98902 = EDGE_LOOP ( 'NONE', ( #240332, #187215, #253677, #70856 ) ) ;
#98903 = ORIENTED_EDGE ( 'NONE', *, *, #155710, .T. ) ;
#98904 = DIRECTION ( 'NONE',  ( 1.000000000000000000, -0.000000000000000000, 0.000000000000000000 ) ) ;
#98906 = VERTEX_POINT ( 'NONE', #108593 ) ;
#98905 = CARTESIAN_POINT ( 'NONE',  ( 23.24999999999999289, 64.35000000001164722, -69.42310748452440805 ) ) ;
#98908 = CARTESIAN_POINT ( 'NONE',  ( -20.64999999999999858, 85.40000000001252545, -179.9170766071767389 ) ) ;
#98907 = DIRECTION ( 'NONE',  ( 1.000000000000000000, 0.000000000000000000, 0.000000000000000000 ) ) ;
#98909 = EDGE_CURVE ( 'NONE', #65963, #32434, #206409, .T. ) ;
#98910 = LINE ( 'NONE', #18124, #65831 ) ;
#98911 = CARTESIAN_POINT ( 'NONE',  ( 21.05000000000000071, 7.128833340094563376, -233.7327013124401276 ) ) ;
#98912 = LINE ( 'NONE', #175948, #146725 ) ;
#98913 = ORIENTED_EDGE ( 'NONE', *, *, #86762, .F. ) ;
#98914 = ADVANCED_FACE ( 'NONE', ( #107302 ), #171511, .T. ) ;
#98915 = ORIENTED_EDGE ( 'NONE', *, *, #183614, .T. ) ;
#98916 = CARTESIAN_POINT ( 'NONE',  ( -23.49999999999994316, 74.14873292176677921, -47.62635315998165453 ) ) ;
#98917 = CARTESIAN_POINT ( 'NONE',  ( -16.89268316805465986, 66.04827818677006235, -149.1673550059788909 ) ) ;
#98918 = DIRECTION ( 'NONE',  ( 4.504528286903032433E-15, 0.1298341882520054891, 0.9915357197604850459 ) ) ;
#98920 = EDGE_CURVE ( 'NONE', #57491, #96608, #233845, .T. ) ;
#98919 = ORIENTED_EDGE ( 'NONE', *, *, #239231, .F. ) ;
#98921 = AXIS2_PLACEMENT_3D ( 'NONE', #50603, #170629, #55711 ) ;
#98922 = AXIS2_PLACEMENT_3D ( 'NONE', #123102, #240468, #86495 ) ;
#98923 = DIRECTION ( 'NONE',  ( -1.000000000000000000, 7.492892343619937423E-30, -1.073024830501117725E-15 ) ) ;
#98924 = VECTOR ( 'NONE', #194303, 1000.000000000000000 ) ;
#98925 = CYLINDRICAL_SURFACE ( 'NONE', #18103, 11.80000000000000426 ) ;
#98926 = LINE ( 'NONE', #41582, #196842 ) ;
#98927 = ORIENTED_EDGE ( 'NONE', *, *, #188970, .T. ) ;
#98928 = VERTEX_POINT ( 'NONE', #4339 ) ;
#98929 =( BOUNDED_SURFACE ( )  B_SPLINE_SURFACE ( 3, 2, ( 
 ( #6478, #85991, #7783 ),
 ( #148573, #246387, #110722 ),
 ( #165579, #145990, #228118 ),
 ( #49469, #225506, #62167 ),
 ( #125977, #221215, #23061 ),
 ( #244637, #145535, #3457 ) ),
 .UNSPECIFIED., .F., .F., .F. ) 
 B_SPLINE_SURFACE_WITH_KNOTS ( ( 4, 2, 4 ),
 ( 3, 3 ),
 ( 0.0001300404313046746687, 0.0003183318589266851870, 0.0005066232865486956782 ),
 ( 0.000000000000000000, 1.000000000000000000 ),
 .UNSPECIFIED. ) 
 GEOMETRIC_REPRESENTATION_ITEM ( )  RATIONAL_B_SPLINE_SURFACE ( (
 ( 1.000000000000000000, 0.7071067811865352493, 1.000000000000000000),
 ( 1.000000000000000000, 0.7625113560541721958, 1.000000000000000000),
 ( 1.000000000000000000, 0.8126073484686229254, 1.000000000000000000),
 ( 1.000000000000000000, 0.8923049332734449557, 1.000000000000000000),
 ( 1.000000000000000000, 0.9231914937768058715, 1.000000000000000000),
 ( 1.000000000000000000, 0.9238795325112977297, 1.000000000000000000) ) ) 
 REPRESENTATION_ITEM ( '' )  SURFACE ( )  );
#98930 = LINE ( 'NONE', #162808, #234293 ) ;
#98931 = CARTESIAN_POINT ( 'NONE',  ( -23.25000000000000000, 6.933893972126341509, -37.28564583437357527 ) ) ;
#98932 = EDGE_LOOP ( 'NONE', ( #159065, #164772, #255706, #49927 ) ) ;
#98933 = DIRECTION ( 'NONE',  ( -1.000000000000000000, -0.000000000000000000, 0.000000000000000000 ) ) ;
#98934 = ORIENTED_EDGE ( 'NONE', *, *, #18790, .T. ) ;
#98935 = EDGE_CURVE ( 'NONE', #45573, #9997, #246318, .T. ) ;
#98936 = CARTESIAN_POINT ( 'NONE',  ( 20.85000000000000142, 7.891440239059407169, -245.4579275668733942 ) ) ;
#98937 = DIRECTION ( 'NONE',  ( 0.000000000000000000, -0.8660254037844411501, -0.4999999999999956146 ) ) ;
#98939 = FILL_AREA_STYLE_COLOUR ( '', #56 ) ;
#98938 = CARTESIAN_POINT ( 'NONE',  ( 21.72449340488910252, 65.71604372252093640, -123.8731074845243683 ) ) ;
#98940 = CARTESIAN_POINT ( 'NONE',  ( 22.39999999999999503, 1.115600667400684642E-11, -55.35042919245524473 ) ) ;
#98942 = EDGE_CURVE ( 'NONE', #239387, #231425, #147727, .T. ) ;
#98941 = DIRECTION ( 'NONE',  ( 0.000000000000000000, 0.7397360091702777085, -0.6728971962616808744 ) ) ;
#98943 = CIRCLE ( 'NONE', #153364, 0.09999999999999820144 ) ;
#98944 = CIRCLE ( 'NONE', #132285, 0.09999999999998708533 ) ;
#98945 = DIRECTION ( 'NONE',  ( -1.000000000000000000, -0.000000000000000000, -0.000000000000000000 ) ) ;
#98947 = EDGE_LOOP ( 'NONE', ( #247025, #198039, #109466, #161129 ) ) ;
#98946 = ORIENTED_EDGE ( 'NONE', *, *, #212768, .F. ) ;
#98948 = AXIS2_PLACEMENT_3D ( 'NONE', #134291, #252962, #96444 ) ;
#98949 = EDGE_LOOP ( 'NONE', ( #98217, #73644, #118498, #100579 ) ) ;
#98950 = CARTESIAN_POINT ( 'NONE',  ( -16.77683809663752257, 66.05416425680736836, -48.68705650362859672 ) ) ;
#98951 = CARTESIAN_POINT ( 'NONE',  ( -22.50485643085238863, 76.07878633908894983, -81.27290242369674900 ) ) ;
#98952 = CYLINDRICAL_SURFACE ( 'NONE', #98685, 0.09999999999999939493 ) ;
#98953 = DIRECTION ( 'NONE',  ( 1.000000000000000000, 0.000000000000000000, 0.000000000000000000 ) ) ;
#98955 = DIRECTION ( 'NONE',  ( 0.000000000000000000, 0.2617529984165031243, 0.9651348961777157509 ) ) ;
#98954 = CARTESIAN_POINT ( 'NONE',  ( 20.97217846901852312, 8.875441724709672187, -8.501227683937228718 ) ) ;
#98956 = ORIENTED_EDGE ( 'NONE', *, *, #125405, .T. ) ;
#98957 = CARTESIAN_POINT ( 'NONE',  ( 23.14999999999999858, 64.35000000001249987, -177.0379132551783812 ) ) ;
#98958 = VERTEX_POINT ( 'NONE', #163436 ) ;
#98959 = CARTESIAN_POINT ( 'NONE',  ( 22.42357213249528769, 33.43151901755100397, -242.5892977220127307 ) ) ;
#98960 = EDGE_LOOP ( 'NONE', ( #141300, #122578, #82114, #131957 ) ) ;
#98961 = ORIENTED_EDGE ( 'NONE', *, *, #224203, .F. ) ;
#98962 = CARTESIAN_POINT ( 'NONE',  ( -23.15000000000000213, 74.07476635515223506, -123.7928639513981892 ) ) ;
#98963 = DIRECTION ( 'NONE',  ( 1.000000000000000000, 0.000000000000000000, 0.000000000000000000 ) ) ;
#98964 = DIRECTION ( 'NONE',  ( -1.000000000000000000, -0.000000000000000000, -0.000000000000000000 ) ) ;
#98965 = DIRECTION ( 'NONE',  ( 0.000000000000000000, 0.000000000000000000, -1.000000000000000000 ) ) ;
#98966 = AXIS2_PLACEMENT_3D ( 'NONE', #131699, #228245, #52144 ) ;
#98967 = AXIS2_PLACEMENT_3D ( 'NONE', #7139, #30594, #69716 ) ;
#98968 = CARTESIAN_POINT ( 'NONE',  ( -21.05000000000000071, 56.02567683926420727, -227.9999002286038774 ) ) ;
#98969 = EDGE_LOOP ( 'NONE', ( #73508, #247708, #36377, #395, #29637 ) ) ;
#98970 = ORIENTED_EDGE ( 'NONE', *, *, #38472, .F. ) ;
#98971 = CARTESIAN_POINT ( 'NONE',  ( 22.39999999999999503, 33.38250548509083870, -242.4821227592189246 ) ) ;
#98972 = ORIENTED_EDGE ( 'NONE', *, *, #238008, .F. ) ;
#98973 = DIRECTION ( 'NONE',  ( 1.000000000000000000, -0.000000000000000000, -0.000000000000000000 ) ) ;
#98974 = CARTESIAN_POINT ( 'NONE',  ( -18.40000000000000213, 64.52683809665002457, -112.3229367329901152 ) ) ;
#98975 = AXIS2_PLACEMENT_3D ( 'NONE', #227347, #128263, #244338 ) ;
#98976 = CARTESIAN_POINT ( 'NONE',  ( 20.95512820512820440, 10.62384868372303615, -41.16491356908760935 ) ) ;
#98977 = FACE_OUTER_BOUND ( 'NONE', #29521, .T. ) ;
#98978 = CARTESIAN_POINT ( 'NONE',  ( -16.78055652883087134, 66.05322308388652175, -90.36231564693194684 ) ) ;
#98979 = LINE ( 'NONE', #80713, #187649 ) ;
#98980 = DIRECTION ( 'NONE',  ( 0.000000000000000000, -1.000000000000000000, -2.891205793294679805E-16 ) ) ;
#98981 = CARTESIAN_POINT ( 'NONE',  ( 20.46382478191414833, 8.901379558713770734, -42.04572809488309559 ) ) ;
#98982 = CIRCLE ( 'NONE', #132320, 4.049999999999994493 ) ;
#98983 = CARTESIAN_POINT ( 'NONE',  ( -21.07954640115345768, 6.170272409895004806, -199.5886254415383974 ) ) ;
#98985 = ADVANCED_FACE ( 'NONE', ( #29104 ), #9485, .T. ) ;
#98984 = CARTESIAN_POINT ( 'NONE',  ( -20.94999999999999929, 46.45388641681647357, -243.1520440498138385 ) ) ;
#98986 = AXIS2_PLACEMENT_3D ( 'NONE', #173948, #194768, #35699 ) ;
#98988 = ORIENTED_EDGE ( 'NONE', *, *, #153309, .T. ) ;
#98987 = CARTESIAN_POINT ( 'NONE',  ( -23.25000000000000000, 1.115650265596050101E-11, -163.4499999999999886 ) ) ;
#98989 = VECTOR ( 'NONE', #191045, 1000.000000000000000 ) ;
#98990 = CIRCLE ( 'NONE', #49119, 0.1000000000000001860 ) ;
#98991 = VERTEX_POINT ( 'NONE', #44773 ) ;
#98992 = CIRCLE ( 'NONE', #244746, 0.09999999999999939493 ) ;
#98993 = CARTESIAN_POINT ( 'NONE',  ( 20.95545211741311320, 10.58641331155510024, -41.08614685958829682 ) ) ;
#98994 = CIRCLE ( 'NONE', #152655, 0.1000000000000055844 ) ;
#98995 = ADVANCED_FACE ( 'NONE', ( #64335 ), #242956, .F. ) ;
#98996 = ORIENTED_EDGE ( 'NONE', *, *, #250555, .F. ) ;
#98997 = CARTESIAN_POINT ( 'NONE',  ( 22.39999999999999503, 11.75000000001115552, -33.50000000000000000 ) ) ;
#98998 = CARTESIAN_POINT ( 'NONE',  ( -18.50000000000000000, 66.65000000001180069, -81.67310748452437963 ) ) ;
#99000 = EDGE_CURVE ( 'NONE', #164666, #29202, #142565, .T. ) ;
#98999 = DIRECTION ( 'NONE',  ( 0.000000000000000000, 0.000000000000000000, 1.000000000000000000 ) ) ;
#99001 = ADVANCED_FACE ( 'NONE', ( #205101 ), #75649, .F. ) ;
#99002 = ORIENTED_EDGE ( 'NONE', *, *, #87891, .T. ) ;
#99003 = CARTESIAN_POINT ( 'NONE',  ( 22.50000000000000000, 11.64957080755595520, -100.4000000000000483 ) ) ;
#99004 = DIRECTION ( 'NONE',  ( 0.000000000000000000, -0.9908441862701782288, -0.1350103645450542456 ) ) ;
#99005 = CARTESIAN_POINT ( 'NONE',  ( 22.47110162079220785, 0.02879741281384913185, -21.85006406331566708 ) ) ;
#99006 = AXIS2_PLACEMENT_3D ( 'NONE', #18604, #137255, #38182 ) ;
#99007 = FACE_OUTER_BOUND ( 'NONE', #94162, .T. ) ;
#99008 = AXIS2_PLACEMENT_3D ( 'NONE', #57835, #151853, #253479 ) ;
#99009 = CARTESIAN_POINT ( 'NONE',  ( 18.47149038651511788, 85.67145715801837014, -62.85032114978587714 ) ) ;
#99010 = CYLINDRICAL_SURFACE ( 'NONE', #223829, 0.09999999999999939493 ) ;
#99011 = AXIS2_PLACEMENT_3D ( 'NONE', #144462, #225280, #45385 ) ;
#99012 = ORIENTED_EDGE ( 'NONE', *, *, #187446, .T. ) ;
#99013 = LINE ( 'NONE', #258071, #183268 ) ;
#99016 = VERTEX_POINT ( 'NONE', #43490 ) ;
#99015 = DIRECTION ( 'NONE',  ( -0.000000000000000000, -0.000000000000000000, -1.000000000000000000 ) ) ;
#99014 = CIRCLE ( 'NONE', #228239, 0.09999999999999939493 ) ;
#99017 = DIRECTION ( 'NONE',  ( 0.000000000000000000, 0.000000000000000000, -1.000000000000000000 ) ) ;
#99018 = EDGE_CURVE ( 'NONE', #201851, #247975, #124312, .T. ) ;
#99019 = CARTESIAN_POINT ( 'NONE',  ( -21.40925344232282512, 69.34148114062192292, -170.1220576731440417 ) ) ;
#99020 = AXIS2_PLACEMENT_3D ( 'NONE', #15174, #95964, #52995 ) ;
#99021 = CYLINDRICAL_SURFACE ( 'NONE', #171282, 11.74999999999999645 ) ;
#99022 = ORIENTED_EDGE ( 'NONE', *, *, #71450, .T. ) ;
#99023 = DIRECTION ( 'NONE',  ( 0.000000000000000000, -1.000000000000000000, -6.982962677686266711E-15 ) ) ;
#99024 = SHAPE_DEFINITION_REPRESENTATION ( #230574, #45219 ) ;
#99025 = CARTESIAN_POINT ( 'NONE',  ( 22.45463910399147878, -2.479040262357760760, -189.6172560672240479 ) ) ;
#99026 = EDGE_LOOP ( 'NONE', ( #108185, #180806, #63031, #119669 ) ) ;
#99027 = DIRECTION ( 'NONE',  ( 1.000000000000000000, 0.000000000000000000, 0.000000000000000000 ) ) ;
#99028 = PLANE ( 'NONE',  #134040 ) ;
#99029 = AXIS2_PLACEMENT_3D ( 'NONE', #90612, #150612, #213140 ) ;
#99030 = CIRCLE ( 'NONE', #248920, 0.1000000000000043771 ) ;
#99031 = CIRCLE ( 'NONE', #61468, 0.09999999999999609201 ) ;
#99032 = CLOSED_SHELL ( 'NONE', ( #15735, #204484, #251805, #200662, #41063, #222422, #42779, #222960, #148939, #84979, #57209, #26768, #203980, #83998, #85038, #144639, #226004, #59037, #129098, #33929, #90841, #189899, #232265, #135346, #66111, #166297, #88791, #169745, #3979, #200432, #170401, #65371, #248033, #175318, #143079, #177061, #80225, #51096, #248923, #39564, #100860, #13383, #251017, #88050, #44585, #226551, #83411, #230922, #62105, #164540, #234010, #58430, #110142 ) ) ;
#99033 = CARTESIAN_POINT ( 'NONE',  ( -20.64999999999999858, 4.250000000011156409, -79.25000000000004263 ) ) ;
#99034 = EDGE_CURVE ( 'NONE', #185637, #188542, #163132, .T. ) ;
#99035 = ORIENTED_EDGE ( 'NONE', *, *, #124392, .F. ) ;
#99036 = EDGE_CURVE ( 'NONE', #72156, #156620, #751, .T. ) ;
#99037 = ORIENTED_EDGE ( 'NONE', *, *, #93165, .T. ) ;
#99038 = CARTESIAN_POINT ( 'NONE',  ( 23.14999999999998437, 1.115600667400684642E-11, -100.5000000000000284 ) ) ;
#99039 = CARTESIAN_POINT ( 'NONE',  ( 23.14999999999999503, 6.550000000011156231, -45.85000000000000142 ) ) ;
#99040 = CYLINDRICAL_SURFACE ( 'NONE', #119711, 11.75000000000000000 ) ;
#99042 = VECTOR ( 'NONE', #105680, 1000.000000000000000 ) ;
#99041 = CARTESIAN_POINT ( 'NONE',  ( -21.44999999999999929, 7.250000000011155521, -188.6499999999999488 ) ) ;
#99043 = CARTESIAN_POINT ( 'NONE',  ( -20.64999999999999858, 74.00000000001186606, -90.29848556176222019 ) ) ;
#99044 = CARTESIAN_POINT ( 'NONE',  ( 22.45305468355011058, -3.275978944803229709, -228.2735455795371422 ) ) ;
#99045 = EDGE_CURVE ( 'NONE', #192176, #48243, #254650, .T. ) ;
#99047 = DIRECTION ( 'NONE',  ( 1.000000000000000000, -0.000000000000000000, 0.000000000000000000 ) ) ;
#99046 = FACE_OUTER_BOUND ( 'NONE', #149719, .T. ) ;
#99048 = CARTESIAN_POINT ( 'NONE',  ( 20.87600722750343252, 65.66887361445283489, -30.43298459182692994 ) ) ;
#99049 = TOROIDAL_SURFACE ( 'NONE', #111550, 0.2000000000000000111, 0.1000000000000000056 ) ;
#99050 = DIRECTION ( 'NONE',  ( -0.000000000000000000, 6.982962677686266711E-15, -1.000000000000000000 ) ) ;
#99051 = FACE_OUTER_BOUND ( 'NONE', #167837, .T. ) ;
#99052 = DIRECTION ( 'NONE',  ( -1.000000000000000000, 0.000000000000000000, 0.000000000000000000 ) ) ;
#99053 = VERTEX_POINT ( 'NONE', #237219 ) ;
#99054 = ORIENTED_EDGE ( 'NONE', *, *, #124575, .F. ) ;
#99055 = DIRECTION ( 'NONE',  ( 0.000000000000000000, 0.000000000000000000, 1.000000000000000000 ) ) ;
#99057 = CARTESIAN_POINT ( 'NONE',  ( 21.14999999999999858, 67.21339244341248786, -191.2731074845244166 ) ) ;
#99056 = CARTESIAN_POINT ( 'NONE',  ( 21.07933241753356768, 69.67135405163190853, -69.61648707494366306 ) ) ;
#99058 = TOROIDAL_SURFACE ( 'NONE', #70065, 0.2000000000000000111, 0.1000000000000000056 ) ;
#99059 = CARTESIAN_POINT ( 'NONE',  ( -21.14999999999999858, 31.85509083104287598, -238.8280249686205536 ) ) ;
#99060 = CARTESIAN_POINT ( 'NONE',  ( 21.87500000000000355, 43.94346684630428967, -235.6041041703296344 ) ) ;
#99061 = FACE_OUTER_BOUND ( 'NONE', #44840, .T. ) ;
#99062 = EDGE_LOOP ( 'NONE', ( #182554, #165325, #187729, #227468 ) ) ;
#99063 = AXIS2_PLACEMENT_3D ( 'NONE', #43747, #202814, #101097 ) ;
#99064 = CARTESIAN_POINT ( 'NONE',  ( 18.59999999999999076, 1.835341550224411922, -11.55515129256298046 ) ) ;
#99065 = VERTEX_POINT ( 'NONE', #228556 ) ;
#99066 = VECTOR ( 'NONE', #7610, 1000.000000000000000 ) ;
#99067 = TOROIDAL_SURFACE ( 'NONE', #24110, 0.2000000000000000111, 0.1000000000000000056 ) ;
#99068 = CYLINDRICAL_SURFACE ( 'NONE', #159599, 0.1000000000000000472 ) ;
#99069 = VECTOR ( 'NONE', #113455, 1000.000000000000114 ) ;
#99070 = ORIENTED_EDGE ( 'NONE', *, *, #18098, .F. ) ;
#99071 = DIRECTION ( 'NONE',  ( -3.440080580676165868E-14, 0.1298341882520054891, 0.9915357197604850459 ) ) ;
#99072 = B_SPLINE_CURVE_WITH_KNOTS ( 'NONE', 3,
 ( #90024, #152612, #153918, #148742, #32679, #49625, #9214, #91331, #187875, #33966, #130443, #129171, #208722, #228277, #113450, #110884, #189138, #173486, #88728 ),
 .UNSPECIFIED., .F., .F.,
 ( 4, 3, 3, 3, 3, 3, 4 ),
 ( 1.387778780781445676E-17, 2.646747978908746686E-05, 5.271166642129237432E-05, 9.008788829885646201E-05, 0.0001426648776561085163, 0.0001897378458660004691, 0.0001917382627806451167 ),
 .UNSPECIFIED. ) ;
#99073 = DIRECTION ( 'NONE',  ( 0.000000000000000000, 0.9910465087640865089, 0.1335171055202867274 ) ) ;
#99074 = EDGE_CURVE ( 'NONE', #34114, #91388, #158359, .T. ) ;
#99075 = EDGE_CURVE ( 'NONE', #228147, #151955, #50656, .T. ) ;
#99076 = VERTEX_POINT ( 'NONE', #254187 ) ;
#99077 = LINE ( 'NONE', #2557, #26885 ) ;
#99078 = ORIENTED_EDGE ( 'NONE', *, *, #146783, .T. ) ;
#99079 = EDGE_CURVE ( 'NONE', #94226, #139128, #29864, .T. ) ;
#99081 = EDGE_CURVE ( 'NONE', #206620, #132097, #183959, .T. ) ;
#99080 = DIRECTION ( 'NONE',  ( 1.000000000000000000, -0.000000000000000000, -0.000000000000000000 ) ) ;
#99082 = CARTESIAN_POINT ( 'NONE',  ( -21.05000000000000071, 87.39257802171759693, -106.0970570643561501 ) ) ;
#99084 = CIRCLE ( 'NONE', #28418, 0.5000000000000004441 ) ;
#99083 = CARTESIAN_POINT ( 'NONE',  ( -21.00000000000000000, 1.212568896937007645, -7.800000000000000711 ) ) ;
#99085 = DIRECTION ( 'NONE',  ( 0.000000000000000000, 0.8814952561688429444, -0.4721928772777345684 ) ) ;
#99086 = LINE ( 'NONE', #178688, #181052 ) ;
#99088 = CARTESIAN_POINT ( 'NONE',  ( 18.50016250449482413, 65.70233904877132147, -131.0487410911965753 ) ) ;
#99087 = CARTESIAN_POINT ( 'NONE',  ( 20.90000000000000213, 6.841561409100513025, 9.675512259591560138 ) ) ;
#99089 = EDGE_CURVE ( 'NONE', #64247, #106553, #159043, .T. ) ;
#99090 = ORIENTED_EDGE ( 'NONE', *, *, #82467, .F. ) ;
#99092 = CARTESIAN_POINT ( 'NONE',  ( -16.87683809663752399, 66.13508655273184900, -116.2988259332204564 ) ) ;
#99091 = PLANE ( 'NONE',  #112014 ) ;
#99093 = ORIENTED_EDGE ( 'NONE', *, *, #188260, .T. ) ;
#99094 = ORIENTED_EDGE ( 'NONE', *, *, #99864, .F. ) ;
#99095 = VECTOR ( 'NONE', #145942, 1000.000000000000000 ) ;
#99096 = EDGE_CURVE ( 'NONE', #78772, #47754, #83949, .T. ) ;
#99097 = ORIENTED_EDGE ( 'NONE', *, *, #183227, .T. ) ;
#99098 = LINE ( 'NONE', #37893, #149213 ) ;
#99100 = ADVANCED_FACE ( 'NONE', ( #95135 ), #208895, .T. ) ;
#99099 = EDGE_CURVE ( 'NONE', #130606, #113797, #4853, .T. ) ;
#99101 = DIRECTION ( 'NONE',  ( 1.000000000000000000, -0.000000000000000000, 0.000000000000000000 ) ) ;
#99102 = LINE ( 'NONE', #17, #76555 ) ;
#99103 = EDGE_LOOP ( 'NONE', ( #113055, #171101, #227287, #146707 ) ) ;
#99104 = CARTESIAN_POINT ( 'NONE',  ( 23.14999999999999858, 76.00000000001190870, -103.0231074845243029 ) ) ;
#99105 = DIRECTION ( 'NONE',  ( 0.000000000000000000, 0.2128009952263605897, -0.9770955615653315052 ) ) ;
#99107 = ADVANCED_FACE ( 'NONE', ( #57264 ), #216357, .T. ) ;
#99106 = DIRECTION ( 'NONE',  ( -1.000000000000000000, -2.081668171172181135E-13, -2.775557561562908012E-13 ) ) ;
#99108 = VERTEX_POINT ( 'NONE', #134243 ) ;
#99109 = DIRECTION ( 'NONE',  ( 1.000000000000000000, 0.000000000000000000, 0.000000000000000000 ) ) ;
#99110 = ADVANCED_FACE ( 'NONE', ( #217618 ), #35202, .F. ) ;
#99111 = CARTESIAN_POINT ( 'NONE',  ( 21.08621493067296271, 6.349294291171669435, 0.05619483947610788566 ) ) ;
#99112 = AXIS2_PLACEMENT_3D ( 'NONE', #185351, #169684, #150099 ) ;
#99113 = ORIENTED_EDGE ( 'NONE', *, *, #248602, .F. ) ;
#99115 = ORIENTED_EDGE ( 'NONE', *, *, #121370, .T. ) ;
#99114 = AXIS2_PLACEMENT_3D ( 'NONE', #220607, #240177, #142334 ) ;
#99116 = CIRCLE ( 'NONE', #99674, 0.9750000000000036415 ) ;
#99117 = DIRECTION ( 'NONE',  ( 0.000000000000000000, 0.2128009952263604787, -0.9770955615653315052 ) ) ;
#99118 = EDGE_CURVE ( 'NONE', #41516, #219374, #192330, .T. ) ;
#99119 = CIRCLE ( 'NONE', #32540, 0.1000000000000028644 ) ;
#99120 = ADVANCED_FACE ( 'NONE', ( #69489 ), #15633, .F. ) ;
#99121 = ORIENTED_EDGE ( 'NONE', *, *, #184730, .F. ) ;
#99122 = CARTESIAN_POINT ( 'NONE',  ( -16.87036670365549540, 9.989418819301647545, -12.52043988269794106 ) ) ;
#99123 = VERTEX_POINT ( 'NONE', #97671 ) ;
#99124 = CARTESIAN_POINT ( 'NONE',  ( 18.59999999999999787, 85.07617159379665850, -214.9471220678560428 ) ) ;
#99125 = ADVANCED_FACE ( 'NONE', ( #192961 ), #153880, .T. ) ;
#99126 = DIRECTION ( 'NONE',  ( -0.000000000000000000, -0.000000000000000000, -1.000000000000000000 ) ) ;
#99127 = CARTESIAN_POINT ( 'NONE',  ( 20.95429402530552210, 60.89549333153017585, -225.3058276775725801 ) ) ;
#99128 = DIRECTION ( 'NONE',  ( 0.000000000000000000, 0.000000000000000000, -1.000000000000000000 ) ) ;
#99129 = EDGE_CURVE ( 'NONE', #33201, #17884, #220972, .T. ) ;
#99130 = VECTOR ( 'NONE', #564, 1000.000000000000000 ) ;
#99131 = EDGE_CURVE ( 'NONE', #36183, #229949, #121062, .T. ) ;
#99133 = AXIS2_PLACEMENT_3D ( 'NONE', #147858, #128293, #51280 ) ;
#99132 = CARTESIAN_POINT ( 'NONE',  ( 18.59999999999999076, 74.25000000001186606, -91.35359592662267403 ) ) ;
#99134 = CARTESIAN_POINT ( 'NONE',  ( -21.55000000000000071, 68.65000000001205649, -124.2731074845243455 ) ) ;
#99135 = DIRECTION ( 'NONE',  ( -0.000000000000000000, -0.1298341882520022694, -0.9915357197604853789 ) ) ;
#99136 = ORIENTED_EDGE ( 'NONE', *, *, #3805, .T. ) ;
#99138 = CARTESIAN_POINT ( 'NONE',  ( 23.24999999999999645, 71.22429906543310096, -181.8718755885703615 ) ) ;
#99137 = CARTESIAN_POINT ( 'NONE',  ( 23.04999999999999716, 61.13752757784637026, -224.6182967272386009 ) ) ;
#99139 = ORIENTED_EDGE ( 'NONE', *, *, #2397, .T. ) ;
#99142 = VERTEX_POINT ( 'NONE', #238492 ) ;
#99141 = DIRECTION ( 'NONE',  ( 0.000000000000000000, -0.5859227990963362664, -0.8103668758649469339 ) ) ;
#99140 = DIRECTION ( 'NONE',  ( 0.000000000000000000, -0.4999999999999088507, 0.8660254037844913322 ) ) ;
#99143 = EDGE_LOOP ( 'NONE', ( #137994, #178942, #20962 ) ) ;
#99144 = VECTOR ( 'NONE', #172109, 1000.000000000000000 ) ;
#99145 = CARTESIAN_POINT ( 'NONE',  ( 23.40000000000005187, 74.83745509109094485, -44.02310748452479316 ) ) ;
#99146 = CARTESIAN_POINT ( 'NONE',  ( 18.59999999999999076, 6.650000000011155876, -88.15000000000004832 ) ) ;
#99147 = CARTESIAN_POINT ( 'NONE',  ( -18.40000000000000213, 64.52683809664954140, -115.6316861282870860 ) ) ;
#99148 = ORIENTED_EDGE ( 'NONE', *, *, #24475, .F. ) ;
#99149 = DIRECTION ( 'NONE',  ( 1.000000000000000000, 0.000000000000000000, 0.000000000000000000 ) ) ;
#99150 = ADVANCED_FACE ( 'NONE', ( #162829 ), #50274, .T. ) ;
#99151 = CARTESIAN_POINT ( 'NONE',  ( 27.30103769104855971, 12.20000000000000284, -347.0000000000001137 ) ) ;
#99153 = CARTESIAN_POINT ( 'NONE',  ( 23.14999999999999503, 14.05000000001115623, -61.48630492923908974 ) ) ;
#99152 = CARTESIAN_POINT ( 'NONE',  ( 21.14999999999999503, 76.10000000001222986, -148.1726782920690937 ) ) ;
#99155 = ORIENTED_EDGE ( 'NONE', *, *, #51606, .T. ) ;
#99154 = FACE_OUTER_BOUND ( 'NONE', #74706, .T. ) ;
#99156 = ORIENTED_EDGE ( 'NONE', *, *, #27473, .F. ) ;
#99157 = VECTOR ( 'NONE', #47991, 1000.000000000000114 ) ;
#99158 = VECTOR ( 'NONE', #133222, 1000.000000000000000 ) ;
#99159 = TOROIDAL_SURFACE ( 'NONE', #215677, 0.2000000000000000111, 0.1000000000000000056 ) ;
#99160 = CARTESIAN_POINT ( 'NONE',  ( -21.05000000000000071, 13.63177590472475487, -238.5351604075707144 ) ) ;
#99161 = EDGE_LOOP ( 'NONE', ( #195187, #18387, #181330, #221118 ) ) ;
#99162 = LINE ( 'NONE', #241286, #56220 ) ;
#99163 = ORIENTED_EDGE ( 'NONE', *, *, #99728, .F. ) ;
#99164 = DIRECTION ( 'NONE',  ( -1.000000000000000000, -1.652117596168391700E-15, -1.153667551319263085E-29 ) ) ;
#99165 = DIRECTION ( 'NONE',  ( -1.000000000000000000, 0.000000000000000000, -0.000000000000000000 ) ) ;
#99166 = DIRECTION ( 'NONE',  ( 0.000000000000000000, -0.000000000000000000, 1.000000000000000000 ) ) ;
#99167 = AXIS2_PLACEMENT_3D ( 'NONE', #94256, #250766, #192103 ) ;
#99168 = ORIENTED_EDGE ( 'NONE', *, *, #13391, .F. ) ;
#99169 = DIRECTION ( 'NONE',  ( 0.000000000000000000, 0.000000000000000000, 1.000000000000000000 ) ) ;
#99170 = ADVANCED_FACE ( 'NONE', ( #79400 ), #166862, .F. ) ;
#99171 = AXIS2_PLACEMENT_3D ( 'NONE', #90180, #44663, #164612 ) ;
#99172 = AXIS2_PLACEMENT_3D ( 'NONE', #43208, #103154, #58881 ) ;
#99174 = EDGE_CURVE ( 'NONE', #161169, #47223, #222650, .T. ) ;
#99173 = CARTESIAN_POINT ( 'NONE',  ( 20.94999999999999929, 87.39257802171813694, -173.0970570643562212 ) ) ;
#99175 = AXIS2_PLACEMENT_3D ( 'NONE', #202721, #98440, #118050 ) ;
#99176 = EDGE_LOOP ( 'NONE', ( #162684, #235322, #60822, #118982 ) ) ;
#99177 = EDGE_LOOP ( 'NONE', ( #29658, #98212, #191996, #68042 ) ) ;
#99178 = AXIS2_PLACEMENT_3D ( 'NONE', #168396, #247875, #151366 ) ;
#99179 = VERTEX_POINT ( 'NONE', #98950 ) ;
#99180 = EDGE_CURVE ( 'NONE', #230047, #48218, #19456, .T. ) ;
#99181 = CARTESIAN_POINT ( 'NONE',  ( 20.94999999999999574, 65.57661458509971908, -196.0310555606543517 ) ) ;
#99182 = ORIENTED_EDGE ( 'NONE', *, *, #223541, .F. ) ;
#99185 = EDGE_CURVE ( 'NONE', #251754, #34877, #225056, .T. ) ;
#99184 = VERTEX_POINT ( 'NONE', #199390 ) ;
#99183 = DIRECTION ( 'NONE',  ( 0.000000000000000000, 0.2617529984165152257, 0.9651348961777124202 ) ) ;
#99186 = APPLICATION_CONTEXT ( 'automotive_design' ) ;
#99187 = VERTEX_POINT ( 'NONE', #64983 ) ;
#99190 = ORIENTED_EDGE ( 'NONE', *, *, #239232, .F. ) ;
#99189 = ORIENTED_EDGE ( 'NONE', *, *, #103593, .F. ) ;
#99188 = CARTESIAN_POINT ( 'NONE',  ( 20.99999999999999645, 61.13238474529445909, -221.0940783352693586 ) ) ;
#99192 = ORIENTED_EDGE ( 'NONE', *, *, #189513, .T. ) ;
#99191 = AXIS2_PLACEMENT_3D ( 'NONE', #6063, #85568, #129569 ) ;
#99193 = FACE_OUTER_BOUND ( 'NONE', #257201, .T. ) ;
#99194 = CIRCLE ( 'NONE', #144990, 0.1000000000000003109 ) ;
#99195 = DIRECTION ( 'NONE',  ( 0.000000000000000000, -0.1575844902526579161, -0.9875055080513779338 ) ) ;
#99196 = EDGE_CURVE ( 'NONE', #192936, #120046, #37857, .T. ) ;
#99197 = AXIS2_PLACEMENT_3D ( 'NONE', #56899, #777, #215992 ) ;
#99198 = COLOUR_RGB ( '', 0.08235294, 0.09019608, 0.10196078) ;
#99199 = AXIS2_PLACEMENT_3D ( 'NONE', #64009, #219218, #22340 ) ;
#99200 = VERTEX_POINT ( 'NONE', #20750 ) ;
#99201 = CIRCLE ( 'NONE', #40993, 0.09999999999999939493 ) ;
#99202 = CARTESIAN_POINT ( 'NONE',  ( -18.59999999999999787, 1.115600667400684642E-11, -167.5000000000000284 ) ) ;
#99204 = ORIENTED_EDGE ( 'NONE', *, *, #160699, .F. ) ;
#99203 = FACE_OUTER_BOUND ( 'NONE', #161985, .T. ) ;
#99205 = CARTESIAN_POINT ( 'NONE',  ( -23.15000000000000213, -8.999999999988846255, -42.89396912265245021 ) ) ;
#99207 = ORIENTED_EDGE ( 'NONE', *, *, #67026, .F. ) ;
#99206 = DIRECTION ( 'NONE',  ( 0.000000000000000000, 0.000000000000000000, -1.000000000000000000 ) ) ;
#99208 = TOROIDAL_SURFACE ( 'NONE', #153443, 0.6000000000000009770, 0.1000000000000000056 ) ;
#99209 = VERTEX_POINT ( 'NONE', #178553 ) ;
#99210 = CARTESIAN_POINT ( 'NONE',  ( 23.25000000000000000, 78.00142589229885459, -228.9845759368473637 ) ) ;
#99211 = CARTESIAN_POINT ( 'NONE',  ( 18.60000000000000142, 85.32100840337318459, -95.78716923544635620 ) ) ;
#99212 = VERTEX_POINT ( 'NONE', #4989 ) ;
#99213 = EDGE_LOOP ( 'NONE', ( #174723, #43882, #122289, #18276 ) ) ;
#99214 = DIRECTION ( 'NONE',  ( -1.000000000000000000, 0.000000000000000000, 0.000000000000000000 ) ) ;
#99215 = CARTESIAN_POINT ( 'NONE',  ( -21.09096482362080138, 0.03944827878515646397, -161.1364556345951655 ) ) ;
#99216 = EDGE_CURVE ( 'NONE', #105461, #88007, #100709, .T. ) ;
#99217 = CIRCLE ( 'NONE', #32654, 0.09999999999999939493 ) ;
#99218 = AXIS2_PLACEMENT_3D ( 'NONE', #63101, #243029, #222162 ) ;
#99220 = EDGE_LOOP ( 'NONE', ( #213342, #18816, #20209, #163084 ) ) ;
#99219 = ORIENTED_EDGE ( 'NONE', *, *, #226906, .T. ) ;
#99221 = EDGE_LOOP ( 'NONE', ( #161087, #36219, #16530, #32338 ) ) ;
#99222 = DIRECTION ( 'NONE',  ( 0.000000000000000000, 0.2617529984165030132, 0.9651348961777157509 ) ) ;
#99223 = EDGE_LOOP ( 'NONE', ( #98205, #191173, #97840, #73224 ) ) ;
#99224 = EDGE_LOOP ( 'NONE', ( #8650, #12888, #207011, #171771 ) ) ;
#99225 = DIRECTION ( 'NONE',  ( 0.000000000000000000, 6.982962677686266711E-15, -1.000000000000000000 ) ) ;
#99226 = ORIENTED_EDGE ( 'NONE', *, *, #219217, .F. ) ;
#99227 = CARTESIAN_POINT ( 'NONE',  ( -16.94309007106719633, 12.44588479347206622, -211.1907070338996277 ) ) ;
#99229 = CARTESIAN_POINT ( 'NONE',  ( -21.05000000000000071, -1.835341550224413698, -11.55515129256298046 ) ) ;
#99228 = CARTESIAN_POINT ( 'NONE',  ( -20.64999999999999858, 68.75000000001253397, -182.3731074845244109 ) ) ;
#99230 = EDGE_CURVE ( 'NONE', #203751, #22319, #200146, .T. ) ;
#99231 = ORIENTED_EDGE ( 'NONE', *, *, #139679, .F. ) ;
#99232 = VECTOR ( 'NONE', #29448, 1000.000000000000000 ) ;
#99233 = EDGE_CURVE ( 'NONE', #200509, #208600, #235154, .T. ) ;
#99235 = B_SPLINE_CURVE_WITH_KNOTS ( 'NONE', 3,
 ( #50542, #212233, #208384, #33627, #11461, #251324, #107982, #51829, #188793, #10169 ),
 .UNSPECIFIED., .F., .F.,
 ( 4, 3, 3, 4 ),
 ( 0.000000000000000000, 0.0002000000000008579659, 0.001000000000082967942, 0.001967863649483335853 ),
 .UNSPECIFIED. ) ;
#99234 = VECTOR ( 'NONE', #149044, 1000.000000000000114 ) ;
#99237 = ORIENTED_EDGE ( 'NONE', *, *, #58658, .F. ) ;
#99236 = ORIENTED_EDGE ( 'NONE', *, *, #93708, .T. ) ;
#99238 = CARTESIAN_POINT ( 'NONE',  ( -21.05000000000000426, 76.02103547655286775, -209.8275633064720296 ) ) ;
#99239 = CARTESIAN_POINT ( 'NONE',  ( -18.69999999999999929, 1.212568896937007645, -8.000000000000000000 ) ) ;
#99240 = AXIS2_PLACEMENT_3D ( 'NONE', #242738, #107084, #182803 ) ;
#99241 = ORIENTED_EDGE ( 'NONE', *, *, #139496, .T. ) ;
#99242 = CIRCLE ( 'NONE', #211511, 0.09999999999999939493 ) ;
#99243 = ADVANCED_FACE ( 'NONE', ( #41604 ), #183666, .T. ) ;
#99244 = DIRECTION ( 'NONE',  ( 0.000000000000000000, -0.8814952561688425003, 0.4721928772777359007 ) ) ;
#99245 = VERTEX_POINT ( 'NONE', #121149 ) ;
#99246 = ORIENTED_EDGE ( 'NONE', *, *, #234795, .T. ) ;
#99247 = DIRECTION ( 'NONE',  ( -2.952720810173289605E-16, -1.000000000000000000, -7.086529944415894657E-15 ) ) ;
#99249 = EDGE_CURVE ( 'NONE', #35963, #248097, #181107, .T. ) ;
#99248 = ORIENTED_EDGE ( 'NONE', *, *, #31213, .T. ) ;
#99250 = CARTESIAN_POINT ( 'NONE',  ( -20.64999999999999858, 1.940186915887848196, -20.67088078894667547 ) ) ;
#99251 = CARTESIAN_POINT ( 'NONE',  ( -20.94999999999999929, 18.51199663233067483, -231.2535697180530292 ) ) ;
#99252 = ORIENTED_EDGE ( 'NONE', *, *, #166485, .F. ) ;
#99253 = VECTOR ( 'NONE', #199989, 1000.000000000000114 ) ;
#99254 = ADVANCED_FACE ( 'NONE', ( #184935 ), #29751, .T. ) ;
#99255 = CARTESIAN_POINT ( 'NONE',  ( -20.85000000000000142, 69.15387683765952431, -132.7853812176745407 ) ) ;
#99256 = LINE ( 'NONE', #157, #82892 ) ;
#99257 = CARTESIAN_POINT ( 'NONE',  ( -16.84793658983413422, 9.950000000011076651, -121.2663533221895875 ) ) ;
#99258 = DIRECTION ( 'NONE',  ( 0.000000000000000000, -0.9770955615653551529, -0.2128009952262517601 ) ) ;
#99259 = TOROIDAL_SURFACE ( 'NONE', #249142, 3.899999999999999467, 0.1000000000000000056 ) ;
#99260 = CARTESIAN_POINT ( 'NONE',  ( 20.94999999999999929, -1.162701749926853712, -141.9000000000000341 ) ) ;
#99262 = ADVANCED_FACE ( 'NONE', ( #7585 ), #89669, .T. ) ;
#99261 = CARTESIAN_POINT ( 'NONE',  ( -18.59999999999999787, -1.135018845899022466, -175.2169768834323520 ) ) ;
#99264 = DIRECTION ( 'NONE',  ( -0.000000000000000000, 0.8660254037844383745, -0.5000000000000003331 ) ) ;
#99263 = CIRCLE ( 'NONE', #224170, 0.09999999999999939493 ) ;
#99266 = ORIENTED_EDGE ( 'NONE', *, *, #15246, .F. ) ;
#99265 = TOROIDAL_SURFACE ( 'NONE', #149193, 4.149999999999999467, 0.1000000000000000056 ) ;
#99268 = ORIENTED_EDGE ( 'NONE', *, *, #152094, .F. ) ;
#99267 = ORIENTED_EDGE ( 'NONE', *, *, #226275, .T. ) ;
#99269 = ORIENTED_EDGE ( 'NONE', *, *, #67848, .F. ) ;
#99270 = ORIENTED_EDGE ( 'NONE', *, *, #244258, .T. ) ;
#99272 = EDGE_CURVE ( 'NONE', #79014, #199454, #107973, .T. ) ;
#99271 = LINE ( 'NONE', #237530, #44733 ) ;
#99273 = LINE ( 'NONE', #217934, #145295 ) ;
#99275 = FACE_OUTER_BOUND ( 'NONE', #113795, .T. ) ;
#99274 = DIRECTION ( 'NONE',  ( 0.000000000000000000, -1.565658005757035267E-14, 1.000000000000000000 ) ) ;
#99276 = CARTESIAN_POINT ( 'NONE',  ( 18.55857864376267941, 33.84113875905941171, -236.2808750561533486 ) ) ;
#99277 = VERTEX_POINT ( 'NONE', #70155 ) ;
#99278 = VECTOR ( 'NONE', #229341, 1000.000000000000000 ) ;
#99279 = CARTESIAN_POINT ( 'NONE',  ( -20.85000000000000142, 10.33248238083634440, -106.0948465439131922 ) ) ;
#99280 = PLANE ( 'NONE',  #199984 ) ;
#99281 = CARTESIAN_POINT ( 'NONE',  ( 21.14999999999999858, 11.75000000001116263, -134.1000000000000227 ) ) ;
#99282 = DIRECTION ( 'NONE',  ( 0.000000000000000000, 0.9126074666063769270, 0.4088369013363280513 ) ) ;
#99283 = ORIENTED_EDGE ( 'NONE', *, *, #162615, .F. ) ;
#99284 = DIRECTION ( 'NONE',  ( 0.000000000000000000, -1.000000000000000000, -7.105427357601001859E-15 ) ) ;
#99285 = DIRECTION ( 'NONE',  ( 0.000000000000000000, 0.8814952561688429444, -0.4721928772777345684 ) ) ;
#99286 = VERTEX_POINT ( 'NONE', #110526 ) ;
#99287 = CARTESIAN_POINT ( 'NONE',  ( -16.88815647973234135, 66.04916738069584881, -56.87589042119839888 ) ) ;
#99288 = FACE_OUTER_BOUND ( 'NONE', #142929, .T. ) ;
#99289 = DIRECTION ( 'NONE',  ( -0.7071067811865475727, -0.7071067811865475727, 0.000000000000000000 ) ) ;
#99290 = CARTESIAN_POINT ( 'NONE',  ( -16.94107738177414291, 10.01423928513661465, -20.94999999999998863 ) ) ;
#99291 = EDGE_LOOP ( 'NONE', ( #6524, #33147, #209188, #124022, #135012, #86078, #5743, #8947, #46522, #191236, #208499, #214719, #177865, #221087, #58657, #83756 ) ) ;
#99292 = CARTESIAN_POINT ( 'NONE',  ( 23.14999999999999503, 56.02567683926420727, -227.9999002286038774 ) ) ;
#99293 = DIRECTION ( 'NONE',  ( 0.000000000000000000, -0.5773469543544729188, -0.8164989248600478255 ) ) ;
#99294 = LINE ( 'NONE', #240126, #12681 ) ;
#99296 = DIRECTION ( 'NONE',  ( -1.000000000000000000, -0.000000000000000000, -0.000000000000000000 ) ) ;
#99295 = SPHERICAL_SURFACE ( 'NONE', #195080, 0.1000000000000000056 ) ;
#99297 = CARTESIAN_POINT ( 'NONE',  ( 20.94999999999999574, 68.58368164137472434, -224.2353459317783120 ) ) ;
#99298 = AXIS2_PLACEMENT_3D ( 'NONE', #87205, #245013, #6399 ) ;
#99299 = CARTESIAN_POINT ( 'NONE',  ( -23.25000000000000000, -1.736705739456431807, -78.51742258762372728 ) ) ;
#99300 = DIRECTION ( 'NONE',  ( -0.000000000000000000, -0.9126074666063770380, -0.4088369013363281068 ) ) ;
#99301 = AXIS2_PLACEMENT_3D ( 'NONE', #231506, #110255, #13729 ) ;
#99302 = VERTEX_POINT ( 'NONE', #229212 ) ;
#99303 = EDGE_LOOP ( 'NONE', ( #124602, #133365, #126576, #29135 ) ) ;
#99304 = AXIS2_PLACEMENT_3D ( 'NONE', #13693, #114070, #208070 ) ;
#99305 = ORIENTED_EDGE ( 'NONE', *, *, #21874, .F. ) ;
#99306 = EDGE_CURVE ( 'NONE', #117062, #17708, #83584, .T. ) ;
#99307 = DIRECTION ( 'NONE',  ( -1.020425574104004196E-15, -0.000000000000000000, -1.000000000000000000 ) ) ;
#99308 = ADVANCED_FACE ( 'NONE', ( #6283 ), #126236, .T. ) ;
#99309 = AXIS2_PLACEMENT_3D ( 'NONE', #242896, #25163, #108524 ) ;
#99311 = EDGE_CURVE ( 'NONE', #106114, #123284, #209637, .T. ) ;
#99310 = AXIS2_PLACEMENT_3D ( 'NONE', #49594, #208689, #75602 ) ;
#99313 = AXIS2_PLACEMENT_3D ( 'NONE', #116129, #210100, #110982 ) ;
#99312 = DIRECTION ( 'NONE',  ( 0.000000000000000000, -0.4930308989874653269, -0.8700118002898649117 ) ) ;
#99314 = DIRECTION ( 'NONE',  ( 0.000000000000000000, 0.000000000000000000, -1.000000000000000000 ) ) ;
#99315 = ORIENTED_EDGE ( 'NONE', *, *, #22188, .F. ) ;
#99316 = TOROIDAL_SURFACE ( 'NONE', #245099, 11.70000000000000107, 0.1000000000000000056 ) ;
#99317 = SPHERICAL_SURFACE ( 'NONE', #22309, 0.1000000000000000056 ) ;
#99318 = CARTESIAN_POINT ( 'NONE',  ( -15.57281606413133623, 9.370655051134644253, -51.02582325598089596 ) ) ;
#99319 = DIRECTION ( 'NONE',  ( 1.000000000000000000, 0.000000000000000000, 0.000000000000000000 ) ) ;
#99320 = CARTESIAN_POINT ( 'NONE',  ( 20.94999999999999929, 71.00000000001151079, -48.02837350343745015 ) ) ;
#99322 = ORIENTED_EDGE ( 'NONE', *, *, #200462, .T. ) ;
#99321 = CARTESIAN_POINT ( 'NONE',  ( -16.93710578446422588, 9.950000000011137047, -188.0811960162001526 ) ) ;
#99324 = DIRECTION ( 'NONE',  ( 1.000000000000000000, 0.000000000000000000, 0.000000000000000000 ) ) ;
#99323 = CARTESIAN_POINT ( 'NONE',  ( -17.11825945287482753, 10.05000000001113847, -146.6500000000000341 ) ) ;
#99325 = EDGE_CURVE ( 'NONE', #181633, #103997, #233488, .T. ) ;
#99326 = CARTESIAN_POINT ( 'NONE',  ( -22.94999999999999929, -1.300000000000000044, -7.900000000000000355 ) ) ;
#99327 = DIRECTION ( 'NONE',  ( 0.000000000000000000, -1.000000000000000000, 0.000000000000000000 ) ) ;
#99329 = EDGE_CURVE ( 'NONE', #104754, #196694, #8606, .T. ) ;
#99328 = CARTESIAN_POINT ( 'NONE',  ( 21.05000000000000071, 1.627786319807488669, -244.0021210468063089 ) ) ;
#99330 = ORIENTED_EDGE ( 'NONE', *, *, #216208, .F. ) ;
#99331 = B_SPLINE_CURVE_WITH_KNOTS ( 'NONE', 3,
 ( #42425, #201486, #22888, #241897, #238049, #98497, #181941, #118112, #82792, #59380 ),
 .UNSPECIFIED., .F., .F.,
 ( 4, 2, 2, 2, 4 ),
 ( 0.000000000000000000, 0.0003916577441626797819, 0.0005874866162440189410, 0.0006854010522846886019, 0.0007833154883253581544 ),
 .UNSPECIFIED. ) ;
#99332 = DIRECTION ( 'NONE',  ( 0.000000000000000000, 0.000000000000000000, 1.000000000000000000 ) ) ;
#99333 = CARTESIAN_POINT ( 'NONE',  ( -20.54999999999999716, -9.500000000000001776, -23.60603087734756045 ) ) ;
#99334 = PRODUCT_DEFINITION ( 'UNKNOWN', '', #173906, #131903 ) ;
#99335 = ORIENTED_EDGE ( 'NONE', *, *, #158321, .T. ) ;
#99336 = AXIS2_PLACEMENT_3D ( 'NONE', #62129, #84185, #85491 ) ;
#99337 = CARTESIAN_POINT ( 'NONE',  ( -16.89268316805465986, 66.04827818677036078, -182.6673550059788909 ) ) ;
#99338 = VERTEX_POINT ( 'NONE', #230489 ) ;
#99339 = TOROIDAL_SURFACE ( 'NONE', #174238, 4.149999999999999467, 0.1000000000000000056 ) ;
#99340 = DIRECTION ( 'NONE',  ( 0.000000000000000000, -0.9654727137038715545, -0.2605042016806676242 ) ) ;
#99341 = EDGE_CURVE ( 'NONE', #51015, #69221, #179318, .T. ) ;
#99342 = DIRECTION ( 'NONE',  ( 0.000000000000000000, 6.982962677686266711E-15, -1.000000000000000000 ) ) ;
#99343 = DIRECTION ( 'NONE',  ( 0.000000000000000000, 2.775557561562812086E-13, -1.000000000000000000 ) ) ;
#99344 = EDGE_CURVE ( 'NONE', #81117, #46286, #229378, .T. ) ;
#99345 = ORIENTED_EDGE ( 'NONE', *, *, #166847, .F. ) ;
#99346 = ADVANCED_FACE ( 'NONE', ( #246199 ), #151499, .T. ) ;
#99347 = AXIS2_PLACEMENT_3D ( 'NONE', #5400, #221886, #66698 ) ;
#99348 = ORIENTED_EDGE ( 'NONE', *, *, #44737, .F. ) ;
#99349 = CARTESIAN_POINT ( 'NONE',  ( -23.49999999999994316, 82.72707916847673459, -26.51159310135756897 ) ) ;
#99350 = DIRECTION ( 'NONE',  ( 1.836970198721029934E-16, -1.000000000000000000, -0.000000000000000000 ) ) ;
#99351 = LINE ( 'NONE', #215465, #182737 ) ;
#99352 = CARTESIAN_POINT ( 'NONE',  ( -21.65000000000000213, 10.20058289318835953, -211.4179224723290815 ) ) ;
#99353 = EDGE_CURVE ( 'NONE', #164187, #123901, #179877, .T. ) ;
#99355 = CARTESIAN_POINT ( 'NONE',  ( -16.94445028196808778, 60.88759175473954599, -221.0718995934454938 ) ) ;
#99354 = DIRECTION ( 'NONE',  ( 0.000000000000000000, -6.982962677686266711E-15, 1.000000000000000000 ) ) ;
#99356 = CIRCLE ( 'NONE', #166048, 0.09999999999999609201 ) ;
#99358 = DIRECTION ( 'NONE',  ( -0.000000000000000000, 6.982962677686266711E-15, -1.000000000000000000 ) ) ;
#99357 = VECTOR ( 'NONE', #85507, 1000.000000000000000 ) ;
#99359 = CARTESIAN_POINT ( 'NONE',  ( -21.05000000000000071, 77.83534155023670564, -158.3679561919613548 ) ) ;
#99360 = DIRECTION ( 'NONE',  ( 0.000000000000000000, 0.9651348961777379554, -0.2617529984164210233 ) ) ;
#99361 = ORIENTED_EDGE ( 'NONE', *, *, #58865, .F. ) ;
#99363 = ORIENTED_EDGE ( 'NONE', *, *, #210018, .T. ) ;
#99362 = CARTESIAN_POINT ( 'NONE',  ( -18.50000000000000000, 85.40000000001167280, -62.64106563635157698 ) ) ;
#99364 = CARTESIAN_POINT ( 'NONE',  ( 20.95017935633852346, 65.52451072038731184, -195.9456676871339482 ) ) ;
#99365 = VECTOR ( 'NONE', #102253, 1000.000000000000000 ) ;
#99366 = CARTESIAN_POINT ( 'NONE',  ( -21.05000000000000071, -1.162701749926853712, -142.1000000000000227 ) ) ;
#99368 = DIRECTION ( 'NONE',  ( 1.000000000000000000, -3.265361837132813093E-16, -2.280189983783949500E-30 ) ) ;
#99367 = CARTESIAN_POINT ( 'NONE',  ( -20.54999999999999716, -6.688413578037177842, -212.5825622730469036 ) ) ;
#99369 = ORIENTED_EDGE ( 'NONE', *, *, #40903, .T. ) ;
#99371 = CARTESIAN_POINT ( 'NONE',  ( -18.59999999999999787, 11.75000000001115197, -45.65000000000000568 ) ) ;
#99370 = CARTESIAN_POINT ( 'NONE',  ( -16.80891096016324227, 66.05000000001157900, -56.89077029179306777 ) ) ;
#99372 = CARTESIAN_POINT ( 'NONE',  ( -23.24999999999999645, 85.60000000001240039, -163.4229180933022576 ) ) ;
#99373 = SPHERICAL_SURFACE ( 'NONE', #196896, 0.1000000000000000056 ) ;
#99374 = LINE ( 'NONE', #117678, #219983 ) ;
#99375 = CARTESIAN_POINT ( 'NONE',  ( -20.64999999999999858, 19.35378350773087419, -238.0802544632095987 ) ) ;
#99376 = ORIENTED_EDGE ( 'NONE', *, *, #177641, .F. ) ;
#99377 = DIRECTION ( 'NONE',  ( 1.000000000000000000, 0.000000000000000000, 0.000000000000000000 ) ) ;
#99378 = AXIS2_PLACEMENT_3D ( 'NONE', #121775, #162187, #40962 ) ;
#99379 = VECTOR ( 'NONE', #35584, 1000.000000000000000 ) ;
#99380 = ORIENTED_EDGE ( 'NONE', *, *, #223064, .T. ) ;
#99381 = EDGE_CURVE ( 'NONE', #186188, #157226, #246497, .T. ) ;
#99382 = DIRECTION ( 'NONE',  ( 0.000000000000000000, 0.9371753822965315228, -0.3488585713686134238 ) ) ;
#99383 = CIRCLE ( 'NONE', #245152, 12.97499999999999964 ) ;
#99384 = VERTEX_POINT ( 'NONE', #247475 ) ;
#99385 = CARTESIAN_POINT ( 'NONE',  ( -20.86777300164945004, 46.46797214202639026, -243.0846070113367432 ) ) ;
#99386 = VERTEX_POINT ( 'NONE', #66283 ) ;
#99387 = VECTOR ( 'NONE', #124009, 1000.000000000000000 ) ;
#99388 = CARTESIAN_POINT ( 'NONE',  ( 22.39999999999999858, 68.20922040163857503, -103.1231074845243540 ) ) ;
#99389 = VECTOR ( 'NONE', #79393, 1000.000000000000227 ) ;
#99390 = VECTOR ( 'NONE', #220502, 1000.000000000000000 ) ;
#99391 = EDGE_CURVE ( 'NONE', #175914, #59363, #32313, .T. ) ;
#99392 = LINE ( 'NONE', #237648, #226627 ) ;
#99393 = ORIENTED_EDGE ( 'NONE', *, *, #84027, .F. ) ;
#99394 = AXIS2_PLACEMENT_3D ( 'NONE', #10757, #130690, #225911 ) ;
#99395 = EDGE_CURVE ( 'NONE', #257097, #248650, #175655, .T. ) ;
#99396 = DIRECTION ( 'NONE',  ( 0.000000000000000000, -0.4721928772777346239, -0.8814952561688430555 ) ) ;
#99397 = LINE ( 'NONE', #308, #53250 ) ;
#99398 = DIRECTION ( 'NONE',  ( 0.000000000000000000, 6.982962677686266711E-15, -1.000000000000000000 ) ) ;
#99399 = DIRECTION ( 'NONE',  ( 0.000000000000000000, 0.2128009952263403282, -0.9770955615653358350 ) ) ;
#99400 = FACE_OUTER_BOUND ( 'NONE', #4269, .T. ) ;
#99401 = CARTESIAN_POINT ( 'NONE',  ( 20.04142135623731136, 62.34315093393703933, -208.9889535843037720 ) ) ;
#99402 = EDGE_LOOP ( 'NONE', ( #250309, #77645, #50218, #152859, #240092, #171192, #91210, #25524, #112047, #121648, #123975, #245559, #120181, #163690, #206617, #93504, #145436, #102802 ) ) ;
#99404 = AXIS2_PLACEMENT_3D ( 'NONE', #5860, #164952, #146648 ) ;
#99403 = FACE_OUTER_BOUND ( 'NONE', #226247, .T. ) ;
#99405 = AXIS2_PLACEMENT_3D ( 'NONE', #233465, #54787, #35285 ) ;
#99406 = ORIENTED_EDGE ( 'NONE', *, *, #76428, .T. ) ;
#99408 = EDGE_LOOP ( 'NONE', ( #173601, #183617, #74368, #205406 ) ) ;
#99407 = CARTESIAN_POINT ( 'NONE',  ( -23.15000000000000213, 11.75000000001115552, -126.9851942293460922 ) ) ;
#99409 = ADVANCED_FACE ( 'NONE', ( #76533 ), #75270, .F. ) ;
#99410 = VERTEX_POINT ( 'NONE', #94815 ) ;
#99411 = LINE ( 'NONE', #138530, #107301 ) ;
#99412 = CIRCLE ( 'NONE', #174499, 2.000000000000001776 ) ;
#99413 = EDGE_CURVE ( 'NONE', #55352, #17420, #241829, .T. ) ;
#99414 = CARTESIAN_POINT ( 'NONE',  ( 20.94999999999999929, -6.688413578037176066, -212.5825622730469036 ) ) ;
#99415 = DIRECTION ( 'NONE',  ( 1.000000000000000000, 0.000000000000000000, -0.000000000000000000 ) ) ;
#99416 = DIRECTION ( 'NONE',  ( 0.000000000000000000, 0.000000000000000000, -1.000000000000000000 ) ) ;
#99417 = DIRECTION ( 'NONE',  ( 0.000000000000000000, -0.000000000000000000, -1.000000000000000000 ) ) ;
#99418 = ORIENTED_EDGE ( 'NONE', *, *, #49750, .T. ) ;
#99419 = CYLINDRICAL_SURFACE ( 'NONE', #51337, 0.09999999999999939493 ) ;
#99420 = DIRECTION ( 'NONE',  ( -3.265361837132813093E-16, -1.000000000000000000, 7.445645354460596589E-46 ) ) ;
#99421 = AXIS2_PLACEMENT_3D ( 'NONE', #196833, #116041, #133037 ) ;
#99423 = ORIENTED_EDGE ( 'NONE', *, *, #239190, .F. ) ;
#99422 = DIRECTION ( 'NONE',  ( 0.000000000000000000, 0.8814952561688429444, -0.4721928772777345684 ) ) ;
#99424 = AXIS2_PLACEMENT_3D ( 'NONE', #58434, #79287, #78013 ) ;
#99425 = ADVANCED_FACE ( 'NONE', ( #17836 ), #236895, .F. ) ;
#99426 = AXIS2_PLACEMENT_3D ( 'NONE', #162933, #242434, #80779 ) ;
#99427 = DIRECTION ( 'NONE',  ( -0.000000000000000000, 0.2128009952263603677, -0.9770955615653313941 ) ) ;
#99428 = ORIENTED_EDGE ( 'NONE', *, *, #105488, .F. ) ;
#99429 = EDGE_CURVE ( 'NONE', #167398, #195393, #255122, .T. ) ;
#99430 = CIRCLE ( 'NONE', #86768, 3.900000000000000355 ) ;
#99431 = CARTESIAN_POINT ( 'NONE',  ( -12.25000000000000178, 66.15000000001155911, -52.77310748452439526 ) ) ;
#99432 = ORIENTED_EDGE ( 'NONE', *, *, #200392, .F. ) ;
#99433 = CARTESIAN_POINT ( 'NONE',  ( 20.94999999999999574, 67.23127455305841238, -235.8551265064783991 ) ) ;
#99434 = EDGE_CURVE ( 'NONE', #19295, #40550, #56942, .T. ) ;
#99435 = DIRECTION ( 'NONE',  ( 0.000000000000000000, 0.2617529984164856383, 0.9651348961777204138 ) ) ;
#99436 = CARTESIAN_POINT ( 'NONE',  ( 20.94999999999999929, 64.25000000001249134, -176.8069731475025890 ) ) ;
#99437 = CARTESIAN_POINT ( 'NONE',  ( 18.49999999999999645, 74.27191306321832087, -216.6386724793566145 ) ) ;
#99438 = CIRCLE ( 'NONE', #245225, 0.09999999999999739653 ) ;
#99439 = EDGE_CURVE ( 'NONE', #26416, #179524, #156112, .T. ) ;
#99440 = VECTOR ( 'NONE', #77381, 1000.000000000000000 ) ;
#99441 = EDGE_CURVE ( 'NONE', #152197, #195076, #212631, .T. ) ;
#99442 = EDGE_LOOP ( 'NONE', ( #64868, #179765, #1260, #205436 ) ) ;
#99443 = CYLINDRICAL_SURFACE ( 'NONE', #157147, 0.5000000000000004441 ) ;
#99444 = ORIENTED_EDGE ( 'NONE', *, *, #15526, .F. ) ;
#99445 = DIRECTION ( 'NONE',  ( -1.000000000000000000, -0.000000000000000000, -0.000000000000000000 ) ) ;
#99446 = CARTESIAN_POINT ( 'NONE',  ( -16.90202395485713893, 9.965944544561935459, -79.59698627874068677 ) ) ;
#99448 = ORIENTED_EDGE ( 'NONE', *, *, #227497, .T. ) ;
#99447 = DIRECTION ( 'NONE',  ( 0.5932847527679310229, -0.8049926720990042694, -6.366092712777067056E-16 ) ) ;
#99449 = DIRECTION ( 'NONE',  ( 0.000000000000000000, 0.1335171055202901413, -0.9910465087640860649 ) ) ;
#99450 = EDGE_CURVE ( 'NONE', #208426, #82909, #133497, .T. ) ;
#99451 = DIRECTION ( 'NONE',  ( -3.265361837132813586E-16, 0.9770955615653357240, 0.2128009952263412996 ) ) ;
#99452 = FACE_OUTER_BOUND ( 'NONE', #193870, .T. ) ;
#99453 = DIRECTION ( 'NONE',  ( -1.000000000000000000, -0.000000000000000000, -0.000000000000000000 ) ) ;
#99454 = FACE_OUTER_BOUND ( 'NONE', #133596, .T. ) ;
#99455 = EDGE_CURVE ( 'NONE', #25682, #65247, #46003, .T. ) ;
#99456 = CIRCLE ( 'NONE', #253028, 0.1000000000000008937 ) ;
#99457 = FACE_OUTER_BOUND ( 'NONE', #45652, .T. ) ;
#99458 = CARTESIAN_POINT ( 'NONE',  ( 18.69999999999999929, 7.800000000000000711, 1.212568896937007867 ) ) ;
#99460 = ORIENTED_EDGE ( 'NONE', *, *, #144972, .T. ) ;
#99459 = DIRECTION ( 'NONE',  ( -1.000000000000000000, -0.000000000000000000, -0.000000000000000000 ) ) ;
#99461 = DIRECTION ( 'NONE',  ( 0.000000000000000000, -0.9915357197604804940, 0.1298341882520397950 ) ) ;
#99462 = ORIENTED_EDGE ( 'NONE', *, *, #113638, .F. ) ;
#99463 = EDGE_LOOP ( 'NONE', ( #209724, #71185, #81455, #123399 ) ) ;
#99464 = CARTESIAN_POINT ( 'NONE',  ( -18.31331870001039874, 85.53629471919262528, -62.65452879353873072 ) ) ;
#99465 = CARTESIAN_POINT ( 'NONE',  ( 21.93340585972004320, 68.67585297715810100, -103.0231074845243597 ) ) ;
#99466 = ORIENTED_EDGE ( 'NONE', *, *, #188313, .T. ) ;
#99467 = DIRECTION ( 'NONE',  ( -1.000000000000000000, 0.000000000000000000, 0.000000000000000000 ) ) ;
#99468 = CARTESIAN_POINT ( 'NONE',  ( -18.50000000000001066, 85.42130820975074812, -62.28074427047331341 ) ) ;
#99469 = VECTOR ( 'NONE', #86867, 1000.000000000000227 ) ;
#99470 = AXIS2_PLACEMENT_3D ( 'NONE', #207381, #245219, #30041 ) ;
#99471 = ORIENTED_EDGE ( 'NONE', *, *, #107963, .F. ) ;
#99472 = CIRCLE ( 'NONE', #149415, 0.09999999999999810429 ) ;
#99473 = AXIS2_PLACEMENT_3D ( 'NONE', #80317, #140307, #41260 ) ;
#99475 = EDGE_CURVE ( 'NONE', #36019, #233212, #92241, .T. ) ;
#99474 = DIRECTION ( 'NONE',  ( -1.000000000000000000, 0.000000000000000000, 0.000000000000000000 ) ) ;
#99476 = FACE_OUTER_BOUND ( 'NONE', #196355, .T. ) ;
#99477 = ORIENTED_EDGE ( 'NONE', *, *, #36456, .T. ) ;
#99478 = AXIS2_PLACEMENT_3D ( 'NONE', #1518, #202305, #242701 ) ;
#99479 = CARTESIAN_POINT ( 'NONE',  ( -21.05000000000000071, 1.750000000011155743, -112.1695115579016857 ) ) ;
#99480 = ORIENTED_EDGE ( 'NONE', *, *, #67315, .T. ) ;
#99481 = DIRECTION ( 'NONE',  ( 0.000000000000000000, 0.000000000000000000, -1.000000000000000000 ) ) ;
#99483 = VERTEX_POINT ( 'NONE', #113103 ) ;
#99482 = DIRECTION ( 'NONE',  ( 1.000000000000000000, 0.000000000000000000, 0.000000000000000000 ) ) ;
#99484 = CARTESIAN_POINT ( 'NONE',  ( 22.39999999999999503, 11.75000000001116263, -100.4000000000000483 ) ) ;
#99485 = ORIENTED_EDGE ( 'NONE', *, *, #60868, .T. ) ;
#99486 = LINE ( 'NONE', #179091, #84797 ) ;
#99487 = AXIS2_PLACEMENT_3D ( 'NONE', #109155, #170486, #67473 ) ;
#99488 = VECTOR ( 'NONE', #62473, 1000.000000000000000 ) ;
#99489 = ORIENTED_EDGE ( 'NONE', *, *, #104764, .T. ) ;
#99491 = EDGE_LOOP ( 'NONE', ( #58807, #203179, #216631, #101018 ) ) ;
#99490 = ORIENTED_EDGE ( 'NONE', *, *, #222848, .F. ) ;
#99493 = CARTESIAN_POINT ( 'NONE',  ( -21.05000000000000071, 85.51932773110476660, -163.0501311079649440 ) ) ;
#99492 = AXIS2_PLACEMENT_3D ( 'NONE', #145936, #24751, #143376 ) ;
#99494 = ORIENTED_EDGE ( 'NONE', *, *, #14823, .T. ) ;
#99495 = EDGE_CURVE ( 'NONE', #7157, #31299, #245937, .T. ) ;
#99496 = CARTESIAN_POINT ( 'NONE',  ( -18.34374000495059676, 64.52683809664949877, -112.2731074845243739 ) ) ;
#99497 = ORIENTED_EDGE ( 'NONE', *, *, #64115, .T. ) ;
#99498 = VECTOR ( 'NONE', #82574, 999.9999999999998863 ) ;
#99499 = VERTEX_POINT ( 'NONE', #97350 ) ;
#99500 = LINE ( 'NONE', #2983, #224362 ) ;
#99501 = DIRECTION ( 'NONE',  ( 0.000000000000000000, 0.000000000000000000, -1.000000000000000000 ) ) ;
#99503 = EDGE_LOOP ( 'NONE', ( #139236, #29990 ) ) ;
#99502 = CARTESIAN_POINT ( 'NONE',  ( -20.64999999999999858, 2.500000000011154633, -87.27537807723794572 ) ) ;
#99504 = LINE ( 'NONE', #79929, #202203 ) ;
#99505 = ORIENTED_EDGE ( 'NONE', *, *, #50722, .T. ) ;
#99506 = DIRECTION ( 'NONE',  ( 1.000000000000000000, -6.938893903907222067E-15, -4.845403715540888588E-29 ) ) ;
#99507 = CARTESIAN_POINT ( 'NONE',  ( -18.59999996769639097, -9.363273769819265624, -74.18149391546575089 ) ) ;
#99508 = DIRECTION ( 'NONE',  ( 0.000000000000000000, 0.000000000000000000, 1.000000000000000000 ) ) ;
#99509 = ORIENTED_EDGE ( 'NONE', *, *, #228588, .T. ) ;
#99510 = DIRECTION ( 'NONE',  ( 1.000000000000000000, -0.000000000000000000, -0.000000000000000000 ) ) ;
#99511 = CARTESIAN_POINT ( 'NONE',  ( -23.25000000000000000, 0.000000000000000000, 0.000000000000000000 ) ) ;
#99512 = CARTESIAN_POINT ( 'NONE',  ( 20.95512820512820440, 44.11820694106860685, -236.4833523840364933 ) ) ;
#99513 = EDGE_LOOP ( 'NONE', ( #175610, #57026, #241062, #10333 ) ) ;
#99514 = CYLINDRICAL_SURFACE ( 'NONE', #142979, 0.5000000000000014433 ) ;
#99515 = ORIENTED_EDGE ( 'NONE', *, *, #87265, .T. ) ;
#99516 = AXIS2_PLACEMENT_3D ( 'NONE', #255367, #80612, #76783 ) ;
#99517 = VERTEX_POINT ( 'NONE', #37436 ) ;
#99518 = VECTOR ( 'NONE', #118693, 999.9999999999998863 ) ;
#99519 = ORIENTED_EDGE ( 'NONE', *, *, #163663, .F. ) ;
#99520 = ORIENTED_EDGE ( 'NONE', *, *, #21293, .F. ) ;
#99521 = DIRECTION ( 'NONE',  ( 0.000000000000000000, -1.000000000000000000, -6.982962677686265922E-15 ) ) ;
#99522 = CARTESIAN_POINT ( 'NONE',  ( -17.22361732159831504, 10.34515565861358866, -156.1292154741328773 ) ) ;
#99523 = EDGE_LOOP ( 'NONE', ( #125143, #33140, #110519, #220774 ) ) ;
#99524 = CIRCLE ( 'NONE', #228749, 0.09999999999999939493 ) ;
#99525 = VERTEX_POINT ( 'NONE', #55653 ) ;
#99526 = CARTESIAN_POINT ( 'NONE',  ( 22.39999999999999503, 7.591056067193221679, -199.2444047917219052 ) ) ;
#99527 = LINE ( 'NONE', #39625, #114835 ) ;
#99528 = ORIENTED_EDGE ( 'NONE', *, *, #79647, .F. ) ;
#99529 = EDGE_CURVE ( 'NONE', #10423, #219183, #133937, .T. ) ;
#99530 = ORIENTED_EDGE ( 'NONE', *, *, #146312, .F. ) ;
#99531 = AXIS2_PLACEMENT_3D ( 'NONE', #149400, #8583, #132374 ) ;
#99532 = VERTEX_POINT ( 'NONE', #115674 ) ;
#99533 = CIRCLE ( 'NONE', #253672, 1.900000000000000799 ) ;
#99534 = ADVANCED_FACE ( 'NONE', ( #116955 ), #71161, .F. ) ;
#99535 = CARTESIAN_POINT ( 'NONE',  ( 15.48841904831874849, 44.70311864748992292, -236.5660131968816984 ) ) ;
#99536 = CYLINDRICAL_SURFACE ( 'NONE', #11693, 0.09999999999999609201 ) ;
#99537 = EDGE_CURVE ( 'NONE', #37631, #92871, #77807, .T. ) ;
#99538 = CARTESIAN_POINT ( 'NONE',  ( 23.14999999999999858, 1.115600667400684642E-11, -134.0000000000000284 ) ) ;
#99539 = DIRECTION ( 'NONE',  ( 1.000000000000000000, 0.000000000000000000, 0.000000000000000000 ) ) ;
#99540 = AXIS2_PLACEMENT_3D ( 'NONE', #17238, #14681, #117602 ) ;
#99542 = CIRCLE ( 'NONE', #132907, 0.2000000000000000944 ) ;
#99541 = CARTESIAN_POINT ( 'NONE',  ( -23.15000000000000213, 0.000000000000000000, 0.000000000000000000 ) ) ;
#99543 = CARTESIAN_POINT ( 'NONE',  ( 18.59999999999999787, 87.75000000001219291, -145.1731074845242802 ) ) ;
#99544 = CARTESIAN_POINT ( 'NONE',  ( -22.47071067811865319, 7.128833340093095217, -233.7327013124392749 ) ) ;
#99546 = CARTESIAN_POINT ( 'NONE',  ( 21.07971444708685738, 6.329792081637704015, -100.4121765636821380 ) ) ;
#99545 = CARTESIAN_POINT ( 'NONE',  ( -16.77828822459933633, 66.05377062495577434, -149.1857357354433589 ) ) ;
#99547 = DIRECTION ( 'NONE',  ( 0.000000000000000000, 0.000000000000000000, 1.000000000000000000 ) ) ;
#99548 = CARTESIAN_POINT ( 'NONE',  ( -16.83558968593875349, 22.98891442405298591, -230.9408738330689062 ) ) ;
#99549 = ADVANCED_FACE ( 'NONE', ( #153565 ), #93532, .F. ) ;
#99550 = CARTESIAN_POINT ( 'NONE',  ( -23.25000000000000000, 64.25000000001269029, -203.5231074845244166 ) ) ;
#99551 = CARTESIAN_POINT ( 'NONE',  ( 20.94999999999999574, 44.47083028126616000, -247.4212268238128161 ) ) ;
#99552 = EDGE_LOOP ( 'NONE', ( #93079, #173310, #21648, #133223 ) ) ;
#99553 = B_SPLINE_CURVE_WITH_KNOTS ( 'NONE', 3,
 ( #233860, #55176, #10962, #213003, #91778, #134732, #132189, #53933, #170078, #31835 ),
 .UNSPECIFIED., .F., .F.,
 ( 4, 2, 2, 2, 4 ),
 ( 5.280516497093958406E-16, 9.930191194499918771E-05, 0.0001986038238894703419, 0.0003972076477784197246, 0.0007944152955563271636 ),
 .UNSPECIFIED. ) ;
#99554 = AXIS2_PLACEMENT_3D ( 'NONE', #119544, #97355, #176964 ) ;
#99555 = AXIS2_PLACEMENT_3D ( 'NONE', #148479, #49377, #128917 ) ;
#99556 = CONICAL_SURFACE ( 'NONE', #203817, 7.750000000000020428, 0.7853981633974531640 ) ;
#99557 = AXIS2_PLACEMENT_3D ( 'NONE', #141921, #140637, #63668 ) ;
#99558 =( BOUNDED_SURFACE ( )  B_SPLINE_SURFACE ( 3, 2, ( 
 ( #110437, #204390, #166594 ),
 ( #249956, #128730, #229110 ),
 ( #67458, #71338, #10054 ),
 ( #90870, #148286, #208273 ) ),
 .UNSPECIFIED., .F., .F., .F. ) 
 B_SPLINE_SURFACE_WITH_KNOTS ( ( 4, 4 ),
 ( 3, 3 ),
 ( 0.04058434257139476031, 0.04256401539001599538 ),
 ( 0.000000000000000000, 1.000000000000000000 ),
 .UNSPECIFIED. ) 
 GEOMETRIC_REPRESENTATION_ITEM ( )  RATIONAL_B_SPLINE_SURFACE ( (
 ( 1.000000000000000000, 0.7103081912007810361, 1.000000000000000000),
 ( 1.000000000000000000, 0.7104998333556836743, 1.000000000000000000),
 ( 1.000000000000000000, 0.7107238315753999780, 1.000000000000000000),
 ( 1.000000000000000000, 0.7110073749539779220, 1.000000000000000000) ) ) 
 REPRESENTATION_ITEM ( '' )  SURFACE ( )  );
#99560 = ORIENTED_EDGE ( 'NONE', *, *, #152130, .F. ) ;
#99559 = DIRECTION ( 'NONE',  ( 0.000000000000000000, 0.000000000000000000, -1.000000000000000000 ) ) ;
#99561 = CIRCLE ( 'NONE', #74700, 0.09999999999999939493 ) ;
#99563 = ADVANCED_FACE ( 'NONE', ( #84177 ), #29660, .T. ) ;
#99562 = CARTESIAN_POINT ( 'NONE',  ( 18.49999999999998934, 10.25000000001115552, -158.6500000000000057 ) ) ;
#99564 = DIRECTION ( 'NONE',  ( 1.000000000000000000, 0.000000000000000000, 0.000000000000000000 ) ) ;
#99565 = CARTESIAN_POINT ( 'NONE',  ( -22.49917693094574389, 64.09964716284724773, -247.0764417527830119 ) ) ;
#99566 = ORIENTED_EDGE ( 'NONE', *, *, #110894, .T. ) ;
#99567 = LINE ( 'NONE', #116596, #241494 ) ;
#99568 = PRODUCT_DEFINITION_SHAPE ( 'NONE', 'NONE',  #258139 ) ;
#99569 = FACE_OUTER_BOUND ( 'NONE', #2350, .T. ) ;
#99570 = AXIS2_PLACEMENT_3D ( 'NONE', #154591, #30787, #50302 ) ;
#99571 = ORIENTED_EDGE ( 'NONE', *, *, #250111, .T. ) ;
#99572 = DIRECTION ( 'NONE',  ( 0.000000000000000000, -6.982962677686266711E-15, 1.000000000000000000 ) ) ;
#99573 = DIRECTION ( 'NONE',  ( 0.000000000000000000, -0.1350103645451904977, -0.9908441862701596881 ) ) ;
#99574 = CARTESIAN_POINT ( 'NONE',  ( -21.14999999999994174, 74.94272479589878344, -8.023107484524793165 ) ) ;
#99575 = DIRECTION ( 'NONE',  ( -0.000000000000000000, -1.000000000000000000, -6.982962677686266711E-15 ) ) ;
#99577 = ORIENTED_EDGE ( 'NONE', *, *, #112491, .F. ) ;
#99576 = LINE ( 'NONE', #237837, #39605 ) ;
#99579 = VERTEX_POINT ( 'NONE', #23016 ) ;
#99578 = CYLINDRICAL_SURFACE ( 'NONE', #227051, 0.09999999999999543976 ) ;
#99580 = AXIS2_PLACEMENT_3D ( 'NONE', #83285, #19505, #221517 ) ;
#99581 = DIRECTION ( 'NONE',  ( 1.000000000000000000, 0.000000000000000000, 0.000000000000000000 ) ) ;
#99582 = B_SPLINE_CURVE_WITH_KNOTS ( 'NONE', 3,
 ( #138844, #178032, #257487, #217111, #39819, #157194, #201420, #240559, #200151, #180585, #197565, #20236, #236685, #159740, #58038, #78883, #61922, #38512, #219694, #22819, #119329, #161030, #237973, #59307, #1919, #158479, #198853, #137578, #99729, #81448 ),
 .UNSPECIFIED., .F., .F.,
 ( 4, 2, 2, 2, 2, 2, 2, 2, 2, 2, 2, 2, 2, 2, 4 ),
 ( 0.000000000000000000, 0.0003422764154113521547, 0.0006845528308227043094, 0.001026829246234056518, 0.001369105661645408619, 0.002053658492468067934, 0.002738211323290727466, 0.003080487738702053762, 0.003422764154113380492, 0.003765040569524707222, 0.004107316984936033519, 0.004449593400347360249, 0.004791869815758686979, 0.005134146231170013709, 0.005476422646581340439 ),
 .UNSPECIFIED. ) ;
#99583 = DIRECTION ( 'NONE',  ( 1.000000000000000000, -0.000000000000000000, 0.000000000000000000 ) ) ;
#99584 = LINE ( 'NONE', #1782, #7467 ) ;
#99585 = CIRCLE ( 'NONE', #37280, 0.09999999999999939493 ) ;
#99586 = CARTESIAN_POINT ( 'NONE',  ( -14.45443560709636088, 9.450592112144859058, -182.5561883188083812 ) ) ;
#99588 = DIRECTION ( 'NONE',  ( 0.000000000000000000, -6.938893903907222067E-15, 1.000000000000000000 ) ) ;
#99587 = CARTESIAN_POINT ( 'NONE',  ( -18.41431012584569160, 64.51252797080363166, -78.74987147142272192 ) ) ;
#99589 = CARTESIAN_POINT ( 'NONE',  ( -16.93658623642905070, 66.01961832835547739, -190.9112047553952038 ) ) ;
#99590 = CIRCLE ( 'NONE', #124579, 11.70000000000000284 ) ;
#99591 = DIRECTION ( 'NONE',  ( -1.000000000000000000, -0.000000000000000000, -0.000000000000000000 ) ) ;
#99592 = CARTESIAN_POINT ( 'NONE',  ( 18.59999999999997655, 1.115600667400684642E-11, -108.4000000000000483 ) ) ;
#99593 = CARTESIAN_POINT ( 'NONE',  ( -18.36527282682052586, 85.50000060001187308, -163.1009585200215781 ) ) ;
#99594 = CARTESIAN_POINT ( 'NONE',  ( 18.39999999999999503, 11.75000000001113953, -188.3499999999999659 ) ) ;
#99596 = ORIENTED_EDGE ( 'NONE', *, *, #25728, .T. ) ;
#99595 = VECTOR ( 'NONE', #123046, 1000.000000000000000 ) ;
#99597 = EDGE_CURVE ( 'NONE', #182549, #222045, #125323, .T. ) ;
#99598 = CARTESIAN_POINT ( 'NONE',  ( 21.05000000000046256, 0.05148288189289713934, -94.19982018208359875 ) ) ;
#99599 = EDGE_LOOP ( 'NONE', ( #161950, #160340, #162387, #69250 ) ) ;
#99600 = ORIENTED_EDGE ( 'NONE', *, *, #99752, .F. ) ;
#99601 = DIRECTION ( 'NONE',  ( 0.000000000000000000, -1.000000000000000000, -0.000000000000000000 ) ) ;
#99602 = CARTESIAN_POINT ( 'NONE',  ( 20.94999999999999574, 77.25000000001232081, -162.0231074845243313 ) ) ;
#99603 = EDGE_LOOP ( 'NONE', ( #230066, #45913, #257589, #158951 ) ) ;
#99604 = EDGE_CURVE ( 'NONE', #16272, #117714, #240761, .T. ) ;
#99605 = AXIS2_PLACEMENT_3D ( 'NONE', #113171, #233149, #192716 ) ;
#99606 = ORIENTED_EDGE ( 'NONE', *, *, #66186, .T. ) ;
#99607 = CIRCLE ( 'NONE', #203867, 0.09999999999999939493 ) ;
#99608 = EDGE_CURVE ( 'NONE', #1095, #122095, #102485, .T. ) ;
#99609 = EDGE_CURVE ( 'NONE', #231430, #62705, #200326, .T. ) ;
#99610 = ORIENTED_EDGE ( 'NONE', *, *, #4667, .T. ) ;
#99611 = CIRCLE ( 'NONE', #78773, 2.099999999999990763 ) ;
#99612 = EDGE_LOOP ( 'NONE', ( #86571, #43501, #7779, #15876 ) ) ;
#99613 = FACE_OUTER_BOUND ( 'NONE', #54784, .T. ) ;
#99614 = CARTESIAN_POINT ( 'NONE',  ( -21.00023020733502932, -5.827586677109586333E-16, 6.390869245268355314 ) ) ;
#99615 = FACE_OUTER_BOUND ( 'NONE', #171390, .T. ) ;
#99616 = DIRECTION ( 'NONE',  ( -1.000000000000000000, -0.000000000000000000, -0.000000000000000000 ) ) ;
#99617 = LINE ( 'NONE', #23989, #185879 ) ;
#99618 = EDGE_CURVE ( 'NONE', #78573, #31642, #163793, .T. ) ;
#99619 = DIRECTION ( 'NONE',  ( 1.000000000000000000, -7.304098846218134667E-16, 0.000000000000000000 ) ) ;
#99620 = DIRECTION ( 'NONE',  ( -0.000000000000000000, 0.4721928772777345684, 0.8814952561688429444 ) ) ;
#99622 = ORIENTED_EDGE ( 'NONE', *, *, #92716, .T. ) ;
#99621 = CARTESIAN_POINT ( 'NONE',  ( -20.64999999999999858, 1.115623935689868526E-11, -98.60000000000005116 ) ) ;
#99624 = DIRECTION ( 'NONE',  ( -1.000000000000000000, 0.000000000000000000, 0.000000000000000000 ) ) ;
#99623 = DIRECTION ( 'NONE',  ( 1.000000000000000000, 0.000000000000000000, 0.000000000000000000 ) ) ;
#99625 = EDGE_CURVE ( 'NONE', #100336, #144129, #8785, .T. ) ;
#99626 = CARTESIAN_POINT ( 'NONE',  ( 20.94999999999999929, 5.000000000011153745, -88.09473398108696074 ) ) ;
#99627 =( BOUNDED_CURVE ( )  B_SPLINE_CURVE ( 3, ( #93660, #94930, #214887, #50659 ),
 .UNSPECIFIED., .F., .F. ) 
 B_SPLINE_CURVE_WITH_KNOTS ( ( 4, 4 ),
 ( 3.141592653589778461, 4.712388980384686121 ),
 .UNSPECIFIED. ) 
 CURVE ( )  GEOMETRIC_REPRESENTATION_ITEM ( )  RATIONAL_B_SPLINE_CURVE ( ( 1.000000000000000000, 0.8047378541243622729, 0.8047378541243622729, 1.000000000000000000 ) ) 
 REPRESENTATION_ITEM ( '' )  );
#99628 = ORIENTED_EDGE ( 'NONE', *, *, #218929, .T. ) ;
#99629 = CARTESIAN_POINT ( 'NONE',  ( -16.91776028072577631, 63.07934927644033252, -213.0999624438847775 ) ) ;
#99630 = ADVANCED_FACE ( 'NONE', ( #41298 ), #154562, .F. ) ;
#99631 = ORIENTED_EDGE ( 'NONE', *, *, #91308, .T. ) ;
#99633 = DIRECTION ( 'NONE',  ( -0.000000000000000000, -0.000000000000000000, -1.000000000000000000 ) ) ;
#99632 = DIRECTION ( 'NONE',  ( 1.000000000000000000, 0.000000000000000000, 0.000000000000000000 ) ) ;
#99634 = VECTOR ( 'NONE', #250186, 1000.000000000000114 ) ;
#99635 = CARTESIAN_POINT ( 'NONE',  ( -21.59142135623730852, 21.72201384040852901, -232.6445455858938658 ) ) ;
#99636 = CARTESIAN_POINT ( 'NONE',  ( 18.49999999999999289, 7.120270961708750512, -104.1595630418393768 ) ) ;
#99637 = ORIENTED_EDGE ( 'NONE', *, *, #248422, .T. ) ;
#99638 = ADVANCED_FACE ( 'NONE', ( #142906 ), #221170, .T. ) ;
#99639 = CARTESIAN_POINT ( 'NONE',  ( 23.24999999999997513, 11.65000000001116298, -193.9851942293460070 ) ) ;
#99640 = EDGE_CURVE ( 'NONE', #163587, #207643, #20439, .T. ) ;
#99641 = CARTESIAN_POINT ( 'NONE',  ( -21.52071067811865746, 68.22071067813065781, -115.2731074845243455 ) ) ;
#99642 = DIRECTION ( 'NONE',  ( -0.000000000000000000, -0.000000000000000000, -1.000000000000000000 ) ) ;
#99644 = EDGE_CURVE ( 'NONE', #116777, #32708, #257682, .T. ) ;
#99643 = DIRECTION ( 'NONE',  ( -0.7071067811865475727, 0.7071067811865475727, 4.937700262164531476E-15 ) ) ;
#99645 = ORIENTED_EDGE ( 'NONE', *, *, #185543, .T. ) ;
#99646 = EDGE_CURVE ( 'NONE', #87279, #215011, #175405, .T. ) ;
#99647 = CARTESIAN_POINT ( 'NONE',  ( -18.50000000000000000, 7.021664781911246322, -104.3335654018973315 ) ) ;
#99648 = CARTESIAN_POINT ( 'NONE',  ( -23.25000000000000000, 76.00000000001213607, -136.5231074845243313 ) ) ;
#99649 = CIRCLE ( 'NONE', #245444, 0.1000000000000028644 ) ;
#99650 = DIRECTION ( 'NONE',  ( -4.336808689941752679E-15, 0.8660254037844482555, 0.4999999999999837907 ) ) ;
#99651 = CARTESIAN_POINT ( 'NONE',  ( -21.29999999999995808, 76.00000000001162448, -65.47310748452431994 ) ) ;
#99652 = CIRCLE ( 'NONE', #220324, 0.3999999999999975797 ) ;
#99653 = VECTOR ( 'NONE', #186, 1000.000000000000000 ) ;
#99654 = DIRECTION ( 'NONE',  ( 1.000000000000000000, 0.000000000000000000, 0.000000000000000000 ) ) ;
#99655 = DIRECTION ( 'NONE',  ( -2.168404344971008868E-16, -0.000000000000000000, -1.000000000000000000 ) ) ;
#99656 =( BOUNDED_SURFACE ( )  B_SPLINE_SURFACE ( 3, 2, ( 
 ( #26479, #6897, #105974 ),
 ( #240386, #182986, #201239 ),
 ( #222062, #185542, #123010 ),
 ( #3030, #164699, #22636 ) ),
 .UNSPECIFIED., .F., .F., .F. ) 
 B_SPLINE_SURFACE_WITH_KNOTS ( ( 4, 4 ),
 ( 3, 3 ),
 ( 3.141592653589793116, 4.712388980384689674 ),
 ( 0.000000000000000000, 1.000000000000000000 ),
 .UNSPECIFIED. ) 
 GEOMETRIC_REPRESENTATION_ITEM ( )  RATIONAL_B_SPLINE_SURFACE ( (
 ( 1.000000000000000000, 0.6447402616204922499, 1.000000000000000000),
 ( 1.000000000000000000, 0.6438648806865591157, 1.000000000000000000),
 ( 1.000000000000000000, 0.6753870962079413509, 1.000000000000000000),
 ( 1.000000000000000000, 0.7071067811865475727, 1.000000000000000000) ) ) 
 REPRESENTATION_ITEM ( '' )  SURFACE ( )  );
#99658 = ORIENTED_EDGE ( 'NONE', *, *, #221880, .F. ) ;
#99657 = LINE ( 'NONE', #121835, #158751 ) ;
#99659 = CARTESIAN_POINT ( 'NONE',  ( -21.14999999999999858, 69.45934304831114048, -170.0231074845243882 ) ) ;
#99661 = EDGE_CURVE ( 'NONE', #224224, #60977, #208726, .T. ) ;
#99660 = CARTESIAN_POINT ( 'NONE',  ( -23.49999999999994316, 73.94408376456904364, -49.16694968567509250 ) ) ;
#99662 = PLANE ( 'NONE',  #254165 ) ;
#99663 = DIRECTION ( 'NONE',  ( 1.000000000000000000, 0.000000000000000000, 0.000000000000000000 ) ) ;
#99664 = ADVANCED_FACE ( 'NONE', ( #197767 ), #79084, .F. ) ;
#99665 = CARTESIAN_POINT ( 'NONE',  ( 21.05000000000000071, 10.56271494673944211, -174.9568021056444138 ) ) ;
#99667 = ORIENTED_EDGE ( 'NONE', *, *, #14282, .T. ) ;
#99666 = CARTESIAN_POINT ( 'NONE',  ( 21.05281448260627641, 67.22398984147393719, -57.34954957271295939 ) ) ;
#99668 = DIRECTION ( 'NONE',  ( 0.000000000000000000, 0.1332476588733589318, -0.9910827722268049644 ) ) ;
#99669 = DIRECTION ( 'NONE',  ( 0.000000000000000000, 0.9910465087640866200, 0.1335171055202867274 ) ) ;
#99670 = CARTESIAN_POINT ( 'NONE',  ( 20.94788355080264353, 67.49401193140447219, -195.5283494629371432 ) ) ;
#99671 = ORIENTED_EDGE ( 'NONE', *, *, #9303, .F. ) ;
#99672 = DIRECTION ( 'NONE',  ( 1.000000000000000000, -0.000000000000000000, -0.000000000000000000 ) ) ;
#99673 = DIRECTION ( 'NONE',  ( 0.000000000000000000, 0.000000000000000000, 1.000000000000000000 ) ) ;
#99674 = AXIS2_PLACEMENT_3D ( 'NONE', #253800, #15223, #137698 ) ;
#99675 = AXIS2_PLACEMENT_3D ( 'NONE', #235953, #209995, #31388 ) ;
#99676 = DIRECTION ( 'NONE',  ( 1.000000000000000000, 0.000000000000000000, 0.000000000000000000 ) ) ;
#99677 = EDGE_CURVE ( 'NONE', #12292, #154382, #54568, .T. ) ;
#99678 = AXIS2_PLACEMENT_3D ( 'NONE', #244719, #84320, #246028 ) ;
#99679 = CARTESIAN_POINT ( 'NONE',  ( -22.59999999999999787, 0.1008583691098682150, -88.75043287651064361 ) ) ;
#99680 = LINE ( 'NONE', #236644, #71895 ) ;
#99681 = VECTOR ( 'NONE', #10789, 999.9999999999998863 ) ;
#99682 = ORIENTED_EDGE ( 'NONE', *, *, #250862, .F. ) ;
#99683 = EDGE_LOOP ( 'NONE', ( #196473, #156345, #167009 ) ) ;
#99684 = DIRECTION ( 'NONE',  ( 0.000000000000000000, 0.000000000000000000, -1.000000000000000000 ) ) ;
#99685 = CARTESIAN_POINT ( 'NONE',  ( -18.59999999999999787, -9.321008403350132809, -174.7359382490778614 ) ) ;
#99686 = LINE ( 'NONE', #219653, #170398 ) ;
#99687 = DIRECTION ( 'NONE',  ( 0.000000000000000000, -0.8700118002898321601, 0.4930308989875230030 ) ) ;
#99688 = ORIENTED_EDGE ( 'NONE', *, *, #194198, .F. ) ;
#99689 = CARTESIAN_POINT ( 'NONE',  ( 20.94999999999999574, 10.47338541492405994, -175.0786544642485012 ) ) ;
#99690 = EDGE_CURVE ( 'NONE', #155591, #214994, #83748, .T. ) ;
#99691 = DIRECTION ( 'NONE',  ( 1.000000000000000000, 0.000000000000000000, 0.000000000000000000 ) ) ;
#99692 = PLANE ( 'NONE',  #16499 ) ;
#99693 = ADVANCED_FACE ( 'NONE', ( #239475 ), #38033, .T. ) ;
#99694 = CARTESIAN_POINT ( 'NONE',  ( -20.94999999999999929, 17.06838326776700399, -224.6250846885016870 ) ) ;
#99696 = CARTESIAN_POINT ( 'NONE',  ( -16.87683809663752399, 9.865889849332424077, -20.23257319293034939 ) ) ;
#99695 = VECTOR ( 'NONE', #114511, 1000.000000000000000 ) ;
#99697 = ORIENTED_EDGE ( 'NONE', *, *, #153853, .F. ) ;
#99698 = CARTESIAN_POINT ( 'NONE',  ( -20.54999999999999716, 85.50000000001149658, -45.91707660717669626 ) ) ;
#99699 = EDGE_CURVE ( 'NONE', #29497, #117921, #146155, .T. ) ;
#99700 = ORIENTED_EDGE ( 'NONE', *, *, #202221, .T. ) ;
#99701 = CARTESIAN_POINT ( 'NONE',  ( -16.77683809663752257, 9.945835743204147761, -20.83605098089580210 ) ) ;
#99702 = EDGE_CURVE ( 'NONE', #82512, #34850, #133677, .T. ) ;
#99703 = VERTEX_POINT ( 'NONE', #29447 ) ;
#99704 = DIRECTION ( 'NONE',  ( 0.000000000000000000, -0.7960711469212456981, 0.6052030477777622375 ) ) ;
#99705 = DIRECTION ( 'NONE',  ( 0.000000000000000000, -0.1298341882519953860, -0.9915357197604862671 ) ) ;
#99706 = CARTESIAN_POINT ( 'NONE',  ( -23.49999999999994316, 84.00000000001119815, -34.86056257560453986 ) ) ;
#99707 = AXIS2_PLACEMENT_3D ( 'NONE', #142276, #44482, #23655 ) ;
#99708 = ORIENTED_EDGE ( 'NONE', *, *, #55893, .F. ) ;
#99709 = LINE ( 'NONE', #39801, #119799 ) ;
#99711 = EDGE_CURVE ( 'NONE', #114510, #70602, #204397, .T. ) ;
#99710 = DIRECTION ( 'NONE',  ( 0.000000000000000000, -1.000000000000000000, 0.000000000000000000 ) ) ;
#99712 = ORIENTED_EDGE ( 'NONE', *, *, #38475, .F. ) ;
#99713 = CARTESIAN_POINT ( 'NONE',  ( 18.59999999999999076, 77.25000000001189449, -95.02310748452430289 ) ) ;
#99715 = ORIENTED_EDGE ( 'NONE', *, *, #239154, .F. ) ;
#99714 = LINE ( 'NONE', #159727, #113342 ) ;
#99716 = CARTESIAN_POINT ( 'NONE',  ( 20.94999999999999929, 62.98048128140160173, -207.0210305352945568 ) ) ;
#99717 = CARTESIAN_POINT ( 'NONE',  ( -18.60000000000000142, 85.32100840337361092, -162.7871692354464415 ) ) ;
#99718 = CIRCLE ( 'NONE', #216450, 0.5000000000000004441 ) ;
#99719 = EDGE_CURVE ( 'NONE', #21472, #77606, #47660, .T. ) ;
#99721 = ADVANCED_FACE ( 'NONE', ( #9839 ), #65964, .T. ) ;
#99720 = CIRCLE ( 'NONE', #16564, 12.87499999999999822 ) ;
#99722 = ORIENTED_EDGE ( 'NONE', *, *, #61977, .T. ) ;
#99723 = CARTESIAN_POINT ( 'NONE',  ( 21.14999999999999858, 13.96869538424789070, -210.3925794786331949 ) ) ;
#99724 = CARTESIAN_POINT ( 'NONE',  ( 21.11701782572533048, 10.72160911601861244, -79.24503742951125673 ) ) ;
#99725 = DIRECTION ( 'NONE',  ( 0.000000000000000000, -7.109473446599835262E-15, 1.000000000000000000 ) ) ;
#99726 = ORIENTED_EDGE ( 'NONE', *, *, #10498, .T. ) ;
#99727 = DIRECTION ( 'NONE',  ( 0.000000000000000000, -0.4721928772777597705, -0.8814952561688296218 ) ) ;
#99728 = EDGE_CURVE ( 'NONE', #50347, #109860, #89358, .T. ) ;
#99729 = CARTESIAN_POINT ( 'NONE',  ( 12.25000000000000000, 48.22675593180859011, -234.1235479764714853 ) ) ;
#99730 = DIRECTION ( 'NONE',  ( 0.000000000000000000, -0.9126074666063602736, -0.4088369013363654103 ) ) ;
#99731 = AXIS2_PLACEMENT_3D ( 'NONE', #15663, #195572, #134273 ) ;
#99732 = CIRCLE ( 'NONE', #191379, 0.5000000000000004441 ) ;
#99733 = ORIENTED_EDGE ( 'NONE', *, *, #248185, .T. ) ;
#99734 = ORIENTED_EDGE ( 'NONE', *, *, #161146, .F. ) ;
#99735 = EDGE_CURVE ( 'NONE', #72740, #148469, #183765, .T. ) ;
#99736 = VECTOR ( 'NONE', #84184, 1000.000000000000000 ) ;
#99737 = VECTOR ( 'NONE', #183998, 1000.000000000000000 ) ;
#99738 = VERTEX_POINT ( 'NONE', #86788 ) ;
#99739 = CIRCLE ( 'NONE', #187095, 0.09999999999999939493 ) ;
#99740 = EDGE_CURVE ( 'NONE', #191031, #81651, #4666, .T. ) ;
#99741 = VERTEX_POINT ( 'NONE', #30719 ) ;
#99742 = DIRECTION ( 'NONE',  ( 0.000000000000000000, 0.2617529984165027912, 0.9651348961777158619 ) ) ;
#99743 = AXIS2_PLACEMENT_3D ( 'NONE', #194890, #154496, #117891 ) ;
#99744 = CARTESIAN_POINT ( 'NONE',  ( 21.05000000000000071, -8.999999999988842703, -57.10603087734755690 ) ) ;
#99746 = ORIENTED_EDGE ( 'NONE', *, *, #74716, .T. ) ;
#99745 = LINE ( 'NONE', #116763, #41675 ) ;
#99747 = EDGE_CURVE ( 'NONE', #131057, #21996, #127223, .T. ) ;
#99748 = CARTESIAN_POINT ( 'NONE',  ( 20.04142135623731136, 11.75000000000000711, -24.76715728752538226 ) ) ;
#99749 = DIRECTION ( 'NONE',  ( -0.000000000000000000, -0.1298341882519953583, -0.9915357197604862671 ) ) ;
#99750 = CARTESIAN_POINT ( 'NONE',  ( -22.50014994444028460, 11.46291945964633818, -198.4184706950396446 ) ) ;
#99751 = DIRECTION ( 'NONE',  ( 0.000000000000000000, 0.000000000000000000, 1.000000000000000000 ) ) ;
#99752 = EDGE_CURVE ( 'NONE', #55413, #214700, #196213, .T. ) ;
#99753 = DIRECTION ( 'NONE',  ( 1.000000000000000000, -1.836970198721029934E-16, -1.282749433769087582E-30 ) ) ;
#99754 = DIRECTION ( 'NONE',  ( 0.000000000000000000, 0.4999999999999966693, -0.8660254037844405950 ) ) ;
#99756 = ORIENTED_EDGE ( 'NONE', *, *, #249589, .F. ) ;
#99755 = DIRECTION ( 'NONE',  ( 0.000000000000000000, 0.000000000000000000, -1.000000000000000000 ) ) ;
#99758 = ORIENTED_EDGE ( 'NONE', *, *, #28529, .F. ) ;
#99757 = CARTESIAN_POINT ( 'NONE',  ( 21.05000000000000071, 68.03098227380377239, -227.7073825336181869 ) ) ;
#99759 = LINE ( 'NONE', #41124, #257869 ) ;
#99760 = VERTEX_POINT ( 'NONE', #11129 ) ;
#99761 = ORIENTED_EDGE ( 'NONE', *, *, #233881, .T. ) ;
#99762 = CARTESIAN_POINT ( 'NONE',  ( 22.60000000000000142, 36.65892442174472876, -249.5511627012454596 ) ) ;
#99763 = COLOUR_RGB ( '', 0.09019608, 0.27058824, 0.51372549) ;
#99764 = CARTESIAN_POINT ( 'NONE',  ( 21.05000000000000071, 4.481636728799211156, -245.1292951062512770 ) ) ;
#99765 = DIRECTION ( 'NONE',  ( 0.000000000000000000, 0.000000000000000000, 1.000000000000000000 ) ) ;
#99766 = CARTESIAN_POINT ( 'NONE',  ( 18.59999999999999076, 64.25000000001220712, -145.1731074845244507 ) ) ;
#99767 = EDGE_CURVE ( 'NONE', #66731, #84841, #90644, .T. ) ;
#99768 = DIRECTION ( 'NONE',  ( -1.000000000000000000, -0.000000000000000000, -0.000000000000000000 ) ) ;
#99769 = CARTESIAN_POINT ( 'NONE',  ( 20.97107704358301916, 67.12452184799133192, -194.9641342551351784 ) ) ;
#99770 = DIRECTION ( 'NONE',  ( 1.000000000000000000, 0.000000000000000000, 0.000000000000000000 ) ) ;
#99771 = ORIENTED_EDGE ( 'NONE', *, *, #127761, .T. ) ;
#99772 = ORIENTED_EDGE ( 'NONE', *, *, #66029, .F. ) ;
#99773 = DIRECTION ( 'NONE',  ( -1.000000000000000000, 0.000000000000000000, -0.000000000000000000 ) ) ;
#99774 = CIRCLE ( 'NONE', #245565, 7.899999999999996803 ) ;
#99775 = EDGE_LOOP ( 'NONE', ( #248514, #30908, #93942, #200953 ) ) ;
#99776 = CARTESIAN_POINT ( 'NONE',  ( 21.14999999999999858, 64.25000000001259082, -191.3731074845244393 ) ) ;
#99777 = CARTESIAN_POINT ( 'NONE',  ( 18.50596464788227280, 68.04082873524789932, -224.1991862745061894 ) ) ;
#99778 = CIRCLE ( 'NONE', #153852, 0.1000000000000028644 ) ;
#99779 = DIRECTION ( 'NONE',  ( 1.000000000000000000, 0.000000000000000000, 0.000000000000000000 ) ) ;
#99780 = DIRECTION ( 'NONE',  ( 0.000000000000000000, -6.982962677686266711E-15, 1.000000000000000000 ) ) ;
#99781 = EDGE_LOOP ( 'NONE', ( #37152, #227510, #189019, #211782 ) ) ;
#99782 = EDGE_CURVE ( 'NONE', #72959, #229996, #243302, .T. ) ;
#99783 = CARTESIAN_POINT ( 'NONE',  ( -16.93433913041102912, 65.99402157848830086, -149.0877420571292760 ) ) ;
#99784 = VERTEX_POINT ( 'NONE', #247153 ) ;
#99785 = DIRECTION ( 'NONE',  ( 0.000000000000000000, 1.000000000000000000, 0.000000000000000000 ) ) ;
#99786 = ORIENTED_EDGE ( 'NONE', *, *, #98746, .T. ) ;
#99787 = CARTESIAN_POINT ( 'NONE',  ( -18.59999999999999787, 10.33248238083634440, -173.0948465439131496 ) ) ;
#99788 = CIRCLE ( 'NONE', #45663, 0.09999999999999939493 ) ;
#99789 = CARTESIAN_POINT ( 'NONE',  ( -16.88495309932521593, 9.954627058484010860, -113.1345486738119490 ) ) ;
#99790 = ORIENTED_EDGE ( 'NONE', *, *, #10772, .F. ) ;
#99791 = CARTESIAN_POINT ( 'NONE',  ( 18.59999999999999787, -9.399999999988843058, -73.88204184817267617 ) ) ;
#99793 = VERTEX_POINT ( 'NONE', #25567 ) ;
#99792 = CARTESIAN_POINT ( 'NONE',  ( -22.24259225415828567, 7.491937870576586889, -100.4009341165472051 ) ) ;
#99794 = EDGE_CURVE ( 'NONE', #229203, #226175, #129600, .T. ) ;
#99795 = DIRECTION ( 'NONE',  ( 0.000000000000000000, -1.000000000000000000, -6.982962677686265922E-15 ) ) ;
#99796 = AXIS2_PLACEMENT_3D ( 'NONE', #47608, #58517, #38997 ) ;
#99797 = VERTEX_POINT ( 'NONE', #5968 ) ;
#99798 = DIRECTION ( 'NONE',  ( 1.000000000000000000, 0.000000000000000000, 0.000000000000000000 ) ) ;
#99799 = VERTEX_POINT ( 'NONE', #206758 ) ;
#99800 = DIRECTION ( 'NONE',  ( 1.000000000000000000, 0.000000000000000000, -1.734723475976817507E-14 ) ) ;
#99801 = DIRECTION ( 'NONE',  ( 1.000000000000000000, 0.000000000000000000, 0.000000000000000000 ) ) ;
#99802 = DIRECTION ( 'NONE',  ( 1.000000000000000000, 0.000000000000000000, 0.000000000000000000 ) ) ;
#99803 = CARTESIAN_POINT ( 'NONE',  ( 18.55807992284871943, 67.49241595948059569, -195.4314365843280541 ) ) ;
#99804 = DIRECTION ( 'NONE',  ( 1.000000000000000000, 0.000000000000000000, 0.000000000000000000 ) ) ;
#99805 = VERTEX_POINT ( 'NONE', #165063 ) ;
#99806 = DIRECTION ( 'NONE',  ( -1.000000000000000000, 0.000000000000000000, -0.000000000000000000 ) ) ;
#99807 = DIRECTION ( 'NONE',  ( -1.000000000000000000, 0.000000000000000000, 0.000000000000000000 ) ) ;
#99808 = CIRCLE ( 'NONE', #208196, 0.1000000000000000472 ) ;
#99809 = DIRECTION ( 'NONE',  ( 0.000000000000000000, 0.2128009952263485993, -0.9770955615653341697 ) ) ;
#99810 = VERTEX_POINT ( 'NONE', #244589 ) ;
#99811 = ORIENTED_EDGE ( 'NONE', *, *, #111124, .T. ) ;
#99812 = DIRECTION ( 'NONE',  ( 0.000000000000000000, 0.000000000000000000, -1.000000000000000000 ) ) ;
#99813 = ORIENTED_EDGE ( 'NONE', *, *, #83952, .T. ) ;
#99814 = B_SPLINE_CURVE_WITH_KNOTS ( 'NONE', 3,
 ( #150281, #248076, #69463, #51134, #149001, #169877, #70758, #15922 ),
 .UNSPECIFIED., .F., .F.,
 ( 4, 2, 2, 4 ),
 ( 0.000000000000000000, 9.550056980124990193E-05, 0.0001910011396024998039, 0.0003820022792049996077 ),
 .UNSPECIFIED. ) ;
#99815 = DIRECTION ( 'NONE',  ( 2.840903330521632269E-16, -0.09425075112713275638, -0.9955484899852801162 ) ) ;
#99816 = DIRECTION ( 'NONE',  ( -0.000000000000000000, 1.000000000000000000, 0.000000000000000000 ) ) ;
#99817 = VERTEX_POINT ( 'NONE', #245894 ) ;
#99819 = ORIENTED_EDGE ( 'NONE', *, *, #129594, .T. ) ;
#99818 = CARTESIAN_POINT ( 'NONE',  ( 5.900000000000059863, 64.35000000001120668, -26.02310748452479316 ) ) ;
#99820 = CARTESIAN_POINT ( 'NONE',  ( -16.97683809663752186, 60.04939757144280321, -224.3231863825903076 ) ) ;
#99821 = ORIENTED_EDGE ( 'NONE', *, *, #65252, .F. ) ;
#99822 = DIRECTION ( 'NONE',  ( 1.000000000000000000, 0.000000000000000000, -0.000000000000000000 ) ) ;
#99823 = ADVANCED_FACE ( 'NONE', ( #225012 ), #46380, .F. ) ;
#99824 = PLANE ( 'NONE',  #135293 ) ;
#99825 = ORIENTED_EDGE ( 'NONE', *, *, #70934, .T. ) ;
#99826 = EDGE_LOOP ( 'NONE', ( #146692, #73279, #103214 ) ) ;
#99827 = VECTOR ( 'NONE', #65748, 1000.000000000000000 ) ;
#99829 = AXIS2_PLACEMENT_3D ( 'NONE', #201278, #82582, #1781 ) ;
#99828 = DIRECTION ( 'NONE',  ( -1.000000000000000000, 2.952720810173289112E-16, 2.061873921506763405E-30 ) ) ;
#99830 = CARTESIAN_POINT ( 'NONE',  ( 23.14999999999999503, 64.35000000001228670, -157.8731074845244393 ) ) ;
#99831 = EDGE_LOOP ( 'NONE', ( #113930, #166327, #20207, #70698 ) ) ;
#99832 = VECTOR ( 'NONE', #8344, 1000.000000000000000 ) ;
#99834 = CARTESIAN_POINT ( 'NONE',  ( -18.59999999999999787, 14.05000000001115623, -106.0136950707610310 ) ) ;
#99833 = AXIS2_PLACEMENT_3D ( 'NONE', #209968, #13063, #31356 ) ;
#99835 = ORIENTED_EDGE ( 'NONE', *, *, #116517, .T. ) ;
#99836 = ORIENTED_EDGE ( 'NONE', *, *, #257107, .F. ) ;
#99837 = CIRCLE ( 'NONE', #220689, 0.1000000000000028644 ) ;
#99838 = LINE ( 'NONE', #197678, #168092 ) ;
#99839 = ADVANCED_FACE ( 'NONE', ( #187216 ), #17177, .T. ) ;
#99840 = EDGE_CURVE ( 'NONE', #23345, #34074, #146749, .T. ) ;
#99842 = VERTEX_POINT ( 'NONE', #74977 ) ;
#99841 = DIRECTION ( 'NONE',  ( -1.000000000000000000, 0.000000000000000000, 0.000000000000000000 ) ) ;
#99843 = CARTESIAN_POINT ( 'NONE',  ( -20.54999999999999716, -7.916456178339619676, -219.8667623501305570 ) ) ;
#99844 = VECTOR ( 'NONE', #203252, 1000.000000000000000 ) ;
#99845 = LINE ( 'NONE', #80278, #181713 ) ;
#99846 = DIRECTION ( 'NONE',  ( 0.000000000000000000, 0.000000000000000000, -1.000000000000000000 ) ) ;
#99847 = CIRCLE ( 'NONE', #137295, 0.1000000000000028644 ) ;
#99849 = CARTESIAN_POINT ( 'NONE',  ( 21.05000000000000071, 79.23417978893664326, -236.1056577391152587 ) ) ;
#99848 = CARTESIAN_POINT ( 'NONE',  ( -16.94107738177415357, 65.98576071487543970, -123.9731074845243768 ) ) ;
#99850 = CARTESIAN_POINT ( 'NONE',  ( -20.94999999999999929, 57.72708596674831938, -226.0092949359174952 ) ) ;
#99851 = CARTESIAN_POINT ( 'NONE',  ( 23.15000000000000213, 62.08148826970417389, -247.6553521922769221 ) ) ;
#99852 = ADVANCED_FACE ( 'NONE', ( #174096 ), #212803, .F. ) ;
#99853 = CARTESIAN_POINT ( 'NONE',  ( 18.47688499308725696, 85.46485595029550097, -29.32175973138686587 ) ) ;
#99854 = CARTESIAN_POINT ( 'NONE',  ( 22.60000000000000142, 11.74956712350054744, -133.8991416309013118 ) ) ;
#99855 = AXIS2_PLACEMENT_3D ( 'NONE', #98634, #58253, #73067 ) ;
#99856 = ORIENTED_EDGE ( 'NONE', *, *, #128117, .F. ) ;
#99857 = ORIENTED_EDGE ( 'NONE', *, *, #27128, .T. ) ;
#99858 = ORIENTED_EDGE ( 'NONE', *, *, #42908, .T. ) ;
#99859 = CARTESIAN_POINT ( 'NONE',  ( -23.25000000000000000, 0.000000000000000000, 0.000000000000000000 ) ) ;
#99860 = ORIENTED_EDGE ( 'NONE', *, *, #238420, .F. ) ;
#99861 = DIRECTION ( 'NONE',  ( 0.000000000000000000, 0.000000000000000000, -1.000000000000000000 ) ) ;
#99862 = EDGE_CURVE ( 'NONE', #30250, #23611, #21285, .T. ) ;
#99863 = ORIENTED_EDGE ( 'NONE', *, *, #170197, .T. ) ;
#99864 = EDGE_CURVE ( 'NONE', #223391, #167778, #246118, .T. ) ;
#99865 = PRESENTATION_STYLE_ASSIGNMENT (( #218540 ) ) ;
#99866 = CARTESIAN_POINT ( 'NONE',  ( -17.29158576265543346, 65.63525233399396086, -91.60586572931654814 ) ) ;
#99867 = VECTOR ( 'NONE', #189888, 1000.000000000000000 ) ;
#99869 = EDGE_LOOP ( 'NONE', ( #193674, #165885, #228020, #208960 ) ) ;
#99868 = ORIENTED_EDGE ( 'NONE', *, *, #124362, .T. ) ;
#99870 = ORIENTED_EDGE ( 'NONE', *, *, #126211, .T. ) ;
#99871 = ORIENTED_EDGE ( 'NONE', *, *, #243872, .F. ) ;
#99872 = DIRECTION ( 'NONE',  ( 0.000000000000000000, -0.9651348961777157509, 0.2617529984165031243 ) ) ;
#99873 = CARTESIAN_POINT ( 'NONE',  ( 21.05000000000000071, -11.48912529306490349, -170.3999999999999773 ) ) ;
#99875 = ORIENTED_EDGE ( 'NONE', *, *, #182360, .T. ) ;
#99874 = CARTESIAN_POINT ( 'NONE',  ( -20.90000000000000213, 0.000000000000000000, 0.000000000000000000 ) ) ;
#99876 = TOROIDAL_SURFACE ( 'NONE', #216624, 11.70000000000000462, 0.1000000000000000056 ) ;
#99877 = CARTESIAN_POINT ( 'NONE',  ( -21.00023020733438983, 34.04610124266385185, -243.7188077099090719 ) ) ;
#99878 = CARTESIAN_POINT ( 'NONE',  ( -18.59999999999999787, 74.36282728704222222, -191.9409541190523498 ) ) ;
#99880 = ORIENTED_EDGE ( 'NONE', *, *, #224505, .T. ) ;
#99879 = CARTESIAN_POINT ( 'NONE',  ( 20.95561247346651967, 10.59500736521470721, -141.5937827669816613 ) ) ;
#99881 = DIRECTION ( 'NONE',  ( -1.000000000000000000, -0.000000000000000000, -0.000000000000000000 ) ) ;
#99882 = ORIENTED_EDGE ( 'NONE', *, *, #161878, .F. ) ;
#99883 = CARTESIAN_POINT ( 'NONE',  ( 20.12500000000000355, 9.258049272928479567, -175.8633388371424076 ) ) ;
#99886 = EDGE_CURVE ( 'NONE', #141973, #77103, #188040, .T. ) ;
#99885 = ORIENTED_EDGE ( 'NONE', *, *, #17319, .T. ) ;
#99884 = CARTESIAN_POINT ( 'NONE',  ( 23.14999999999999858, 5.000000000011153745, -54.59473398108690390 ) ) ;
#99887 = CARTESIAN_POINT ( 'NONE',  ( -20.85000000000000142, 1.115600667400684642E-11, -200.9999999999999432 ) ) ;
#99888 = CARTESIAN_POINT ( 'NONE',  ( 20.94999999999999574, 77.16270174994961906, -61.42310748452431568 ) ) ;
#99889 = CARTESIAN_POINT ( 'NONE',  ( 21.05000000000000071, 11.60000000001116049, -60.07179676972450011 ) ) ;
#99890 = EDGE_LOOP ( 'NONE', ( #21561, #43426, #83466, #199111 ) ) ;
#99892 = CARTESIAN_POINT ( 'NONE',  ( -16.87851181299898684, 44.13533318390521032, -235.2989511082154195 ) ) ;
#99891 = DIRECTION ( 'NONE',  ( 0.000000000000000000, 0.2128009952263485993, -0.9770955615653341697 ) ) ;
#99893 = DIRECTION ( 'NONE',  ( -1.073024830501117725E-15, -0.2617529984165031243, -0.9651348961777157509 ) ) ;
#99894 = TOROIDAL_SURFACE ( 'NONE', #129174, 0.4000000000000012990, 0.1000000000000000056 ) ;
#99895 = CARTESIAN_POINT ( 'NONE',  ( 18.43630871534869797, 85.67980087481544160, -163.3624754165403772 ) ) ;
#99896 = CARTESIAN_POINT ( 'NONE',  ( 18.59999999999999076, 34.53503747617446606, -235.1972745784239578 ) ) ;
#99897 = LINE ( 'NONE', #219875, #18442 ) ;
#99898 = CIRCLE ( 'NONE', #54128, 0.1000000000000055844 ) ;
#99899 = EDGE_LOOP ( 'NONE', ( #194830, #122868, #93243, #81633 ) ) ;
#99900 = ORIENTED_EDGE ( 'NONE', *, *, #63146, .T. ) ;
#99901 = ORIENTED_EDGE ( 'NONE', *, *, #9622, .F. ) ;
#99902 = ADVANCED_FACE ( 'NONE', ( #172812 ), #193616, .T. ) ;
#99903 = CARTESIAN_POINT ( 'NONE',  ( -18.60000000000000142, -8.150000000000005684, 32.89999999999999858 ) ) ;
#99904 = ORIENTED_EDGE ( 'NONE', *, *, #685, .F. ) ;
#99906 = DIRECTION ( 'NONE',  ( -0.000000000000000000, -1.000000000000000000, -0.000000000000000000 ) ) ;
#99905 =( GEOMETRIC_REPRESENTATION_CONTEXT ( 3 ) GLOBAL_UNCERTAINTY_ASSIGNED_CONTEXT ( ( #248576 ) ) GLOBAL_UNIT_ASSIGNED_CONTEXT ( ( #120538, #241739, #100897 ) ) REPRESENTATION_CONTEXT ( 'NONE', 'WORKASPACE' ) );
#99907 = ORIENTED_EDGE ( 'NONE', *, *, #5406, .F. ) ;
#99908 = DIRECTION ( 'NONE',  ( 0.000000000000000000, 0.000000000000000000, 1.000000000000000000 ) ) ;
#99909 = CARTESIAN_POINT ( 'NONE',  ( 20.94999999999999574, 44.52640028187936849, -247.3006740988509193 ) ) ;
#99910 = AXIS2_PLACEMENT_3D ( 'NONE', #27871, #180495, #103496 ) ;
#99911 = ADVANCED_FACE ( 'NONE', ( #230166 ), #114061, .T. ) ;
#99912 = ORIENTED_EDGE ( 'NONE', *, *, #24863, .T. ) ;
#99913 = EDGE_CURVE ( 'NONE', #2960, #162902, #96435, .T. ) ;
#99914 = EDGE_CURVE ( 'NONE', #211426, #242521, #58823, .T. ) ;
#99916 = ORIENTED_EDGE ( 'NONE', *, *, #66169, .F. ) ;
#99915 = AXIS2_PLACEMENT_3D ( 'NONE', #192053, #129494, #51201 ) ;
#99917 = VERTEX_POINT ( 'NONE', #211910 ) ;
#99918 = AXIS2_PLACEMENT_3D ( 'NONE', #133115, #67044, #53574 ) ;
#99919 = CIRCLE ( 'NONE', #91584, 1.900000000000000799 ) ;
#99920 = EDGE_LOOP ( 'NONE', ( #58619, #72721, #237746, #193270 ) ) ;
#99921 = VECTOR ( 'NONE', #17804, 1000.000000000000000 ) ;
#99922 = VECTOR ( 'NONE', #32142, 1000.000000000000000 ) ;
#99923 = CARTESIAN_POINT ( 'NONE',  ( -18.59999999999999787, -1.637172712959223952, -179.0821533654719815 ) ) ;
#99924 = CARTESIAN_POINT ( 'NONE',  ( 15.74999999999999645, 66.65000000001155911, -52.77310748452439526 ) ) ;
#99925 = CARTESIAN_POINT ( 'NONE',  ( -20.94999999999999929, 64.35000000001171827, -69.52310748452438816 ) ) ;
#99926 = CARTESIAN_POINT ( 'NONE',  ( -22.59999999999999787, 11.74987124438766273, -167.4345704089863034 ) ) ;
#99927 = DIRECTION ( 'NONE',  ( 0.000000000000000000, -0.9126074666063770380, -0.4088369013363281068 ) ) ;
#99928 = CARTESIAN_POINT ( 'NONE',  ( 21.05000000000000071, 87.65000000001215597, -139.5231074845243029 ) ) ;
#99929 = CIRCLE ( 'NONE', #182815, 0.09999999999999939493 ) ;
#99930 = ADVANCED_FACE ( 'NONE', ( #131065 ), #94499, .T. ) ;
#99932 = CARTESIAN_POINT ( 'NONE',  ( -18.59999999999999787, 11.65000000001115232, -88.35000000000003695 ) ) ;
#99931 = DIRECTION ( 'NONE',  ( -1.000000000000000000, 0.000000000000000000, 0.000000000000000000 ) ) ;
#99933 = DIRECTION ( 'NONE',  ( 0.000000000000000000, 1.000000000000000000, 2.891205793294679805E-16 ) ) ;
#99935 = EDGE_LOOP ( 'NONE', ( #156613, #222023, #141775, #147171 ) ) ;
#99934 = CARTESIAN_POINT ( 'NONE',  ( 22.42357213249528769, 68.32706761365203363, -103.1221944485259314 ) ) ;
#99936 = FACE_OUTER_BOUND ( 'NONE', #22190, .T. ) ;
#99937 = ORIENTED_EDGE ( 'NONE', *, *, #238439, .F. ) ;
#99938 = CARTESIAN_POINT ( 'NONE',  ( -18.40000000000000568, -9.499999999988851584, -140.9993620971801533 ) ) ;
#99939 = ORIENTED_EDGE ( 'NONE', *, *, #20980, .F. ) ;
#99940 = ORIENTED_EDGE ( 'NONE', *, *, #24196, .T. ) ;
#99941 = FACE_OUTER_BOUND ( 'NONE', #242944, .T. ) ;
#99942 = DIRECTION ( 'NONE',  ( 0.000000000000000000, 0.9908441862701782288, 0.1350103645450542456 ) ) ;
#99944 = EDGE_CURVE ( 'NONE', #180338, #36544, #50644, .T. ) ;
#99943 = SPHERICAL_SURFACE ( 'NONE', #67007, 0.1000000000000000056 ) ;
#99946 = EDGE_CURVE ( 'NONE', #165812, #86432, #175574, .T. ) ;
#99945 = ORIENTED_EDGE ( 'NONE', *, *, #176818, .T. ) ;
#99947 = LINE ( 'NONE', #156134, #67748 ) ;
#99948 = ORIENTED_EDGE ( 'NONE', *, *, #101559, .F. ) ;
#99949 = ORIENTED_EDGE ( 'NONE', *, *, #8978, .T. ) ;
#99950 = EDGE_CURVE ( 'NONE', #143581, #78012, #42289, .T. ) ;
#99951 = LINE ( 'NONE', #81660, #36780 ) ;
#99952 = VERTEX_POINT ( 'NONE', #175364 ) ;
#99953 = CARTESIAN_POINT ( 'NONE',  ( -21.05000000000000071, 11.65000000001115588, -126.9851942293460922 ) ) ;
#99954 = DIRECTION ( 'NONE',  ( 0.000000000000000000, 0.8814952561688430555, -0.4721928772777346239 ) ) ;
#99955 = ORIENTED_EDGE ( 'NONE', *, *, #183333, .F. ) ;
#99956 = LINE ( 'NONE', #176990, #177897 ) ;
#99957 = DIRECTION ( 'NONE',  ( 1.000000000000000000, 0.000000000000000000, 0.000000000000000000 ) ) ;
#99958 = FACE_OUTER_BOUND ( 'NONE', #210842, .T. ) ;
#99959 = ORIENTED_EDGE ( 'NONE', *, *, #176643, .T. ) ;
#99960 = EDGE_CURVE ( 'NONE', #171778, #76379, #154737, .T. ) ;
#99961 = LINE ( 'NONE', #80389, #96023 ) ;
#99962 = CARTESIAN_POINT ( 'NONE',  ( -23.15000000000000213, -8.777002227904194598, -238.5420042644097975 ) ) ;
#99963 = CARTESIAN_POINT ( 'NONE',  ( 20.94999999999999929, 69.55000000001230376, -160.0060803140843859 ) ) ;
#99964 = ORIENTED_EDGE ( 'NONE', *, *, #159570, .F. ) ;
#99966 = ORIENTED_EDGE ( 'NONE', *, *, #212258, .F. ) ;
#99965 = CARTESIAN_POINT ( 'NONE',  ( -20.94999999999999929, 77.83534155023671985, -158.4679561919613491 ) ) ;
#99967 = EDGE_CURVE ( 'NONE', #212994, #3049, #192334, .T. ) ;
#99968 = FACE_OUTER_BOUND ( 'NONE', #91729, .T. ) ;
#99969 = ADVANCED_FACE ( 'NONE', ( #31994 ), #111511, .T. ) ;
#99970 = LINE ( 'NONE', #872, #104567 ) ;
#99971 = FACE_OUTER_BOUND ( 'NONE', #238725, .T. ) ;
#99972 = CARTESIAN_POINT ( 'NONE',  ( -20.94999999999999929, 43.30036367478129478, -245.0872390055602352 ) ) ;
#99973 = CARTESIAN_POINT ( 'NONE',  ( -16.89268316805466341, 66.04827818676987761, -123.8788599630699281 ) ) ;
#99974 = ORIENTED_EDGE ( 'NONE', *, *, #156774, .F. ) ;
#99975 = CARTESIAN_POINT ( 'NONE',  ( 21.14999999999999858, 65.28660755661168480, -57.27310748452439526 ) ) ;
#99976 = VECTOR ( 'NONE', #156043, 1000.000000000000000 ) ;
#99977 = CARTESIAN_POINT ( 'NONE',  ( -16.77902162784673834, 9.946419257218995114, -146.6619912440693554 ) ) ;
#99978 = CARTESIAN_POINT ( 'NONE',  ( 21.05000000000000071, 70.60000000001251408, -179.9170766071768526 ) ) ;
#99979 = CARTESIAN_POINT ( 'NONE',  ( -20.94999999999999929, 64.35000000001245724, -170.0231074845244166 ) ) ;
#99980 = EDGE_CURVE ( 'NONE', #116777, #105984, #4835, .T. ) ;
#99981 = VECTOR ( 'NONE', #36799, 1000.000000000000000 ) ;
#99982 = CARTESIAN_POINT ( 'NONE',  ( 20.74625933824083646, 67.11708647892730539, -60.96793646040334380 ) ) ;
#99983 =( BOUNDED_SURFACE ( )  B_SPLINE_SURFACE ( 3, 2, ( 
 ( #193719, #232859, #17625 ),
 ( #34661, #179313, #158470 ),
 ( #115451, #155900, #77586 ),
 ( #54189, #15083, #237964 ),
 ( #174192, #197556, #18919 ),
 ( #153346, #98414, #218390 ),
 ( #154620, #39808, #198843 ),
 ( #213261, #20223, #99717 ) ),
 .UNSPECIFIED., .F., .F., .T. ) 
 B_SPLINE_SURFACE_WITH_KNOTS ( ( 4, 2, 2, 4 ),
 ( 3, 3 ),
 ( 0.0001723339234021429623, 0.0002782939632049933449, 0.0003842540030078437545, 0.0005961740826135445738 ),
 ( 0.000000000000000000, 1.000000000000000000 ),
 .UNSPECIFIED. ) 
 GEOMETRIC_REPRESENTATION_ITEM ( )  RATIONAL_B_SPLINE_SURFACE ( (
 ( 1.000000000000000000, 0.9504532311154486601, 1.000000000000000000),
 ( 1.000000000000000000, 0.9506023220705525079, 1.000000000000000000),
 ( 1.000000000000000000, 0.9395774818187484501, 1.000000000000000000),
 ( 1.000000000000000000, 0.9079328464641823748, 1.000000000000000000),
 ( 1.000000000000000000, 0.8875702416206456835, 1.000000000000000000),
 ( 1.000000000000000000, 0.8205919608039227153, 1.000000000000000000),
 ( 1.000000000000000000, 0.7666842783598419864, 1.000000000000000000),
 ( 1.000000000000000000, 0.7071067811865088260, 1.000000000000000000) ) ) 
 REPRESENTATION_ITEM ( '' )  SURFACE ( )  );
#99984 = AXIS2_PLACEMENT_3D ( 'NONE', #174104, #22390, #253578 ) ;
#99985 = ORIENTED_EDGE ( 'NONE', *, *, #237813, .T. ) ;
#99986 = ORIENTED_EDGE ( 'NONE', *, *, #146752, .T. ) ;
#99987 = PLANE ( 'NONE',  #220853 ) ;
#99988 = DIRECTION ( 'NONE',  ( -0.000000000000000000, 1.000000000000000000, 6.982962677686266711E-15 ) ) ;
#99989 = DIRECTION ( 'NONE',  ( -1.000000000000000000, 0.000000000000000000, 0.000000000000000000 ) ) ;
#99990 = PLANE ( 'NONE',  #170621 ) ;
#99991 = ORIENTED_EDGE ( 'NONE', *, *, #119643, .F. ) ;
#99992 = DIRECTION ( 'NONE',  ( 0.000000000000000000, 0.9651348961777160840, -0.2617529984165018475 ) ) ;
#99993 = LINE ( 'NONE', #158750, #234316 ) ;
#99994 = EDGE_CURVE ( 'NONE', #215272, #208753, #176638, .T. ) ;
#99995 = DIRECTION ( 'NONE',  ( 1.000000000000000000, 0.000000000000000000, 0.000000000000000000 ) ) ;
#99996 = CIRCLE ( 'NONE', #254135, 0.09999999999999939493 ) ;
#99997 = CIRCLE ( 'NONE', #220825, 0.1000000000000043771 ) ;
#99998 = DIRECTION ( 'NONE',  ( 0.000000000000000000, 0.000000000000000000, -1.000000000000000000 ) ) ;
#99999 = EDGE_CURVE ( 'NONE', #222451, #117081, #63113, .T. ) ;
#100000 = ORIENTED_EDGE ( 'NONE', *, *, #22946, .F. ) ;
#100001 = DIRECTION ( 'NONE',  ( 1.000000000000000000, 0.000000000000000000, 0.000000000000000000 ) ) ;
#100002 = EDGE_CURVE ( 'NONE', #172217, #235108, #100510, .T. ) ;
#100003 = VERTEX_POINT ( 'NONE', #157069 ) ;
#100004 = CARTESIAN_POINT ( 'NONE',  ( 23.14999999999999503, 11.65000000001116298, -79.15000000000004832 ) ) ;
#100005 = CARTESIAN_POINT ( 'NONE',  ( 21.14999999999999858, 87.75000000001205080, -124.2731074845242176 ) ) ;
#100006 = CARTESIAN_POINT ( 'NONE',  ( 18.59999999999999076, 65.75000000001149658, -44.77310748452439526 ) ) ;
#100007 = FACE_OUTER_BOUND ( 'NONE', #124968, .T. ) ;
#100008 = FACE_OUTER_BOUND ( 'NONE', #115470, .T. ) ;
#100010 = EDGE_CURVE ( 'NONE', #143109, #19453, #250395, .T. ) ;
#100009 = CARTESIAN_POINT ( 'NONE',  ( 21.04999999999999716, 18.83004532744374870, -227.9662487122261609 ) ) ;
#100011 = DIRECTION ( 'NONE',  ( 1.000000000000000000, 1.541880601228652843E-16, 2.878400969107353907E-16 ) ) ;
#100012 = CARTESIAN_POINT ( 'NONE',  ( 18.59999999999999076, 65.79142135624907439, -78.27310748452437394 ) ) ;
#100013 = FACE_OUTER_BOUND ( 'NONE', #217429, .T. ) ;
#100014 = VECTOR ( 'NONE', #327, 1000.000000000000000 ) ;
#100015 = CARTESIAN_POINT ( 'NONE',  ( -20.65000000000000568, 9.775875410973588586, -211.8174516384118817 ) ) ;
#100016 = AXIS2_PLACEMENT_3D ( 'NONE', #77175, #112473, #32970 ) ;
#100017 = ADVANCED_FACE ( 'NONE', ( #61809 ), #3090, .T. ) ;
#100018 = FACE_OUTER_BOUND ( 'NONE', #79261, .T. ) ;
#100020 = DIRECTION ( 'NONE',  ( 0.000000000000000000, 0.000000000000000000, -1.000000000000000000 ) ) ;
#100019 = CIRCLE ( 'NONE', #133380, 0.1000000000000024342 ) ;
#100021 = CIRCLE ( 'NONE', #137448, 0.1000000000000028644 ) ;
#100022 = DIRECTION ( 'NONE',  ( 1.000000000000000000, 0.000000000000000000, 0.000000000000000000 ) ) ;
#100023 = CARTESIAN_POINT ( 'NONE',  ( 21.04386569057787426, 56.16954312985733111, -227.9354499029107046 ) ) ;
#100024 = EDGE_CURVE ( 'NONE', #101237, #139650, #97031, .T. ) ;
#100025 = VECTOR ( 'NONE', #149753, 1000.000000000000000 ) ;
#100027 = EDGE_CURVE ( 'NONE', #205600, #16002, #121430, .T. ) ;
#100026 = ADVANCED_FACE ( 'NONE', ( #99613 ), #159626, .F. ) ;
#100028 = EDGE_LOOP ( 'NONE', ( #239348, #173580, #217902, #234514 ) ) ;
#100029 = LINE ( 'NONE', #161336, #181350 ) ;
#100030 = CARTESIAN_POINT ( 'NONE',  ( -21.14999999999994174, 87.50449464844290048, -34.18759587077607165 ) ) ;
#100031 = SHAPE_REPRESENTATION ( 'Snap Open Cable Crossbars 15', ( #2425 ), #77591 ) ;
#100032 = ORIENTED_EDGE ( 'NONE', *, *, #190918, .F. ) ;
#100033 = DIRECTION ( 'NONE',  ( 0.000000000000000000, 0.1350103645451946055, -0.9908441862701591329 ) ) ;
#100034 = CIRCLE ( 'NONE', #20993, 0.1000000000000076522 ) ;
#100036 = CIRCLE ( 'NONE', #54262, 2.099999999999998312 ) ;
#100035 = DIRECTION ( 'NONE',  ( 0.000000000000000000, 0.000000000000000000, -1.000000000000000000 ) ) ;
#100037 = EDGE_LOOP ( 'NONE', ( #149374, #201270, #101353, #6784 ) ) ;
#100038 = CARTESIAN_POINT ( 'NONE',  ( -23.15000000000000213, 2.500000000011156409, -46.72462192276210402 ) ) ;
#100039 = DIRECTION ( 'NONE',  ( 1.000000000000000000, -0.000000000000000000, 0.000000000000000000 ) ) ;
#100040 = ORIENTED_EDGE ( 'NONE', *, *, #186580, .T. ) ;
#100041 = EDGE_CURVE ( 'NONE', #18345, #27940, #229724, .T. ) ;
#100042 = EDGE_CURVE ( 'NONE', #201448, #89956, #54757, .T. ) ;
#100043 = VERTEX_POINT ( 'NONE', #21423 ) ;
#100044 = DIRECTION ( 'NONE',  ( 0.000000000000000000, -7.056502275159890832E-15, 1.000000000000000000 ) ) ;
#100045 = EDGE_CURVE ( 'NONE', #215705, #70620, #25551, .T. ) ;
#100046 = ORIENTED_EDGE ( 'NONE', *, *, #78014, .F. ) ;
#100047 = CARTESIAN_POINT ( 'NONE',  ( 21.11825140030076753, 0.007203620632672789147, 6.445407565420044449 ) ) ;
#100048 = EDGE_CURVE ( 'NONE', #30084, #165694, #160922, .T. ) ;
#100049 = CARTESIAN_POINT ( 'NONE',  ( 18.49999999999999645, 42.96960653111219131, -254.4772109693542745 ) ) ;
#100051 = CARTESIAN_POINT ( 'NONE',  ( 21.11101077988997332, 34.01873560909758254, -243.6951092311880984 ) ) ;
#100050 = PRODUCT_DEFINITION_CONTEXT ( 'detailed design', #95764, 'design' ) ;
#100052 = FACE_OUTER_BOUND ( 'NONE', #51499, .T. ) ;
#100053 = DIRECTION ( 'NONE',  ( 0.000000000000000000, 0.9908441862701420355, 0.1350103645453197554 ) ) ;
#100054 = EDGE_CURVE ( 'NONE', #15812, #31301, #241725, .T. ) ;
#100055 = DIRECTION ( 'NONE',  ( -0.000000000000000000, -0.2617529984165031243, -0.9651348961777157509 ) ) ;
#100056 = FACE_OUTER_BOUND ( 'NONE', #218720, .T. ) ;
#100057 = CARTESIAN_POINT ( 'NONE',  ( 21.93340585898891604, 0.6726324846061126905, -230.2742912564565927 ) ) ;
#100059 = ORIENTED_EDGE ( 'NONE', *, *, #60433, .T. ) ;
#100058 = CARTESIAN_POINT ( 'NONE',  ( -22.39999999999999858, 75.90000000001165859, -69.52310748452431710 ) ) ;
#100060 = ORIENTED_EDGE ( 'NONE', *, *, #247730, .T. ) ;
#100062 = DIRECTION ( 'NONE',  ( 3.616040088954497272E-32, -1.224646799147352961E-16, 1.000000000000000000 ) ) ;
#100061 = CARTESIAN_POINT ( 'NONE',  ( 18.39999999999999858, 37.95493834378066111, -261.2294694241335264 ) ) ;
#100065 = ORIENTED_EDGE ( 'NONE', *, *, #45799, .T. ) ;
#100064 = CARTESIAN_POINT ( 'NONE',  ( 18.59999999999999076, 65.50857864377520912, -178.7731074845244450 ) ) ;
#100063 = DIRECTION ( 'NONE',  ( 1.000000000000000000, 0.000000000000000000, 0.000000000000000000 ) ) ;
#100066 = CIRCLE ( 'NONE', #245836, 0.5000000000000004441 ) ;
#100067 = EDGE_LOOP ( 'NONE', ( #10684, #257038, #83880, #106903 ) ) ;
#100068 = CARTESIAN_POINT ( 'NONE',  ( -16.94333152882356330, 66.00965798855456512, -149.1310759534229646 ) ) ;
#100069 = DIRECTION ( 'NONE',  ( 0.000000000000000000, 6.308085367183347448E-16, 1.000000000000000000 ) ) ;
#100070 = DIRECTION ( 'NONE',  ( 0.000000000000000000, 0.000000000000000000, -1.000000000000000000 ) ) ;
#100071 = DIRECTION ( 'NONE',  ( 1.000000000000000000, 0.000000000000000000, 0.000000000000000000 ) ) ;
#100072 = AXIS2_PLACEMENT_3D ( 'NONE', #85817, #244925, #116975 ) ;
#100073 = DIRECTION ( 'NONE',  ( -0.000000000000000000, -6.982962677686266711E-15, 1.000000000000000000 ) ) ;
#100074 = EDGE_CURVE ( 'NONE', #30038, #44687, #92164, .T. ) ;
#100075 = CARTESIAN_POINT ( 'NONE',  ( 20.85000000000000142, 77.16412189325330928, -128.6082593989527254 ) ) ;
#100076 = CARTESIAN_POINT ( 'NONE',  ( 20.00000000000000355, 4.631764625546179737, 21.90000000000000213 ) ) ;
#100077 = CARTESIAN_POINT ( 'NONE',  ( 21.05000000000000071, 75.24091630460340241, -206.3219986834402846 ) ) ;
#100078 = EDGE_CURVE ( 'NONE', #198610, #102331, #108915, .T. ) ;
#100079 = ORIENTED_EDGE ( 'NONE', *, *, #102915, .T. ) ;
#100080 = ORIENTED_EDGE ( 'NONE', *, *, #239870, .F. ) ;
#100081 = CARTESIAN_POINT ( 'NONE',  ( 13.40000000000000036, -11.75000000000000000, 15.00000000000000355 ) ) ;
#100082 = CIRCLE ( 'NONE', #29417, 3.900000000000000799 ) ;
#100083 = VERTEX_POINT ( 'NONE', #197454 ) ;
#100084 = CARTESIAN_POINT ( 'NONE',  ( 21.05000000000011795, -0.01759718699745431436, -27.05922910633797684 ) ) ;
#100085 = EDGE_LOOP ( 'NONE', ( #131803, #251475, #49885, #129503 ) ) ;
#100086 = CARTESIAN_POINT ( 'NONE',  ( -16.92989507731676824, 14.10952512909879530, -219.0278967931764385 ) ) ;
#100087 = TOROIDAL_SURFACE ( 'NONE', #183510, 11.70000000000000639, 0.1000000000000000056 ) ;
#100088 = CARTESIAN_POINT ( 'NONE',  ( -13.54036565897075661, 49.63592998410995705, -233.3809899335355453 ) ) ;
#100089 = LINE ( 'NONE', #86623, #76504 ) ;
#100090 = ADVANCED_FACE ( 'NONE', ( #158377 ), #198740, .F. ) ;
#100091 = DIRECTION ( 'NONE',  ( -0.7071067811865474617, -0.3338907855510734324, -0.6233112732207618523 ) ) ;
#100092 = DIRECTION ( 'NONE',  ( -1.000000000000000000, 0.000000000000000000, -0.000000000000000000 ) ) ;
#100093 = EDGE_LOOP ( 'NONE', ( #43785, #69041, #51751, #164924 ) ) ;
#100094 = AXIS2_PLACEMENT_3D ( 'NONE', #9545, #167374, #49956 ) ;
#100096 = VECTOR ( 'NONE', #22165, 1000.000000000000000 ) ;
#100095 = DIRECTION ( 'NONE',  ( 1.000000000000000000, 0.000000000000000000, -0.000000000000000000 ) ) ;
#100097 = ORIENTED_EDGE ( 'NONE', *, *, #214294, .T. ) ;
#100098 = FACE_OUTER_BOUND ( 'NONE', #154899, .T. ) ;
#100099 = FACE_OUTER_BOUND ( 'NONE', #102973, .T. ) ;
#100100 = DIRECTION ( 'NONE',  ( 0.000000000000000000, 0.000000000000000000, 1.000000000000000000 ) ) ;
#100101 = FACE_OUTER_BOUND ( 'NONE', #24987, .T. ) ;
#100102 = VERTEX_POINT ( 'NONE', #120524 ) ;
#100103 = CARTESIAN_POINT ( 'NONE',  ( 21.05000000000000071, 39.23476235320398331, -236.9756760510740037 ) ) ;
#100104 = VERTEX_POINT ( 'NONE', #257369 ) ;
#100107 = ORIENTED_EDGE ( 'NONE', *, *, #21347, .F. ) ;
#100106 = FACE_OUTER_BOUND ( 'NONE', #119312, .T. ) ;
#100105 = CARTESIAN_POINT ( 'NONE',  ( -14.00000000000000178, 13.18880795147152440, -215.2702608532411830 ) ) ;
#100108 = CIRCLE ( 'NONE', #66822, 0.5000000000000004441 ) ;
#100109 = CARTESIAN_POINT ( 'NONE',  ( -20.90000000000000213, 7.900000000000000355, 1.300000000000000044 ) ) ;
#100110 = AXIS2_PLACEMENT_3D ( 'NONE', #186727, #5473, #122897 ) ;
#100111 = AXIS2_PLACEMENT_3D ( 'NONE', #200694, #20787, #258044 ) ;
#100112 = CIRCLE ( 'NONE', #237524, 0.09999999999998866740 ) ;
#100113 = VECTOR ( 'NONE', #33959, 1000.000000000000000 ) ;
#100114 = DIRECTION ( 'NONE',  ( 0.000000000000000000, -7.429790795770644761E-15, 1.000000000000000000 ) ) ;
#100115 = VERTEX_POINT ( 'NONE', #1811 ) ;
#100116 = DIRECTION ( 'NONE',  ( 1.000000000000000000, 1.156482317317869556E-14, 3.083952846180985271E-14 ) ) ;
#100117 = FACE_OUTER_BOUND ( 'NONE', #253139, .T. ) ;
#100118 = DIRECTION ( 'NONE',  ( -1.000000000000000000, -0.000000000000000000, -0.000000000000000000 ) ) ;
#100120 = ORIENTED_EDGE ( 'NONE', *, *, #55261, .T. ) ;
#100119 = DIRECTION ( 'NONE',  ( 1.000000000000000000, 0.000000000000000000, 0.000000000000000000 ) ) ;
#100121 = CARTESIAN_POINT ( 'NONE',  ( -22.47071067811865319, 29.57301391503006016, -252.6169816238249552 ) ) ;
#100122 = AXIS2_PLACEMENT_3D ( 'NONE', #180386, #28736, #105622 ) ;
#100123 = EDGE_LOOP ( 'NONE', ( #221221, #103490, #10070, #1598 ) ) ;
#100124 = CARTESIAN_POINT ( 'NONE',  ( -16.89318236219976299, 9.951535257886295227, -180.1448703678941001 ) ) ;
#100125 = CARTESIAN_POINT ( 'NONE',  ( -20.64999999999999858, 4.250000000011156409, -179.8499999999999943 ) ) ;
#100126 = FACE_OUTER_BOUND ( 'NONE', #110696, .T. ) ;
#100127 = EDGE_LOOP ( 'NONE', ( #23001, #135983, #29384, #183378 ) ) ;
#100128 = DIRECTION ( 'NONE',  ( 1.000000000000000000, 0.000000000000000000, 0.000000000000000000 ) ) ;
#100129 = ORIENTED_EDGE ( 'NONE', *, *, #144291, .T. ) ;
#100130 = CARTESIAN_POINT ( 'NONE',  ( 21.14999999999999858, 65.51923798433685420, -242.1677427744926092 ) ) ;
#100131 = FACE_OUTER_BOUND ( 'NONE', #76347, .T. ) ;
#100132 = LINE ( 'NONE', #143119, #14383 ) ;
#100133 = ORIENTED_EDGE ( 'NONE', *, *, #38106, .F. ) ;
#100134 = CARTESIAN_POINT ( 'NONE',  ( 21.06490991615909536, 22.95056430979463968, -230.0412660441067487 ) ) ;
#100135 = AXIS2_PLACEMENT_3D ( 'NONE', #65199, #45648, #245130 ) ;
#100136 = DIRECTION ( 'NONE',  ( 0.000000000000000000, 1.000000000000000000, -6.308085367188393199E-16 ) ) ;
#100137 = ADVANCED_FACE ( 'NONE', ( #18818 ), #125489, .T. ) ;
#100138 = DIRECTION ( 'NONE',  ( 0.000000000000000000, 0.000000000000000000, 1.000000000000000000 ) ) ;
#100139 = ORIENTED_EDGE ( 'NONE', *, *, #166615, .T. ) ;
#100140 = CARTESIAN_POINT ( 'NONE',  ( 23.24999999999999645, 64.25000000001264766, -194.2731074845244450 ) ) ;
#100141 = DIRECTION ( 'NONE',  ( -1.836970198721029934E-16, 1.000000000000000000, 0.000000000000000000 ) ) ;
#100142 = ORIENTED_EDGE ( 'NONE', *, *, #199187, .F. ) ;
#100143 = DIRECTION ( 'NONE',  ( 0.000000000000000000, -1.000000000000000000, 0.000000000000000000 ) ) ;
#100144 = CIRCLE ( 'NONE', #91800, 0.09999999999999939493 ) ;
#100145 = ORIENTED_EDGE ( 'NONE', *, *, #8314, .T. ) ;
#100146 = VECTOR ( 'NONE', #74015, 1000.000000000000000 ) ;
#100147 = EDGE_LOOP ( 'NONE', ( #201249, #42797, #185136, #145741 ) ) ;
#100149 = ORIENTED_EDGE ( 'NONE', *, *, #85396, .F. ) ;
#100148 = CARTESIAN_POINT ( 'NONE',  ( 20.94999999999999929, 85.00000000001251976, -179.4170766071767389 ) ) ;
#100150 = EDGE_CURVE ( 'NONE', #145361, #103375, #21459, .T. ) ;
#100151 = ADVANCED_FACE ( 'NONE', ( #244279 ), #8265, .F. ) ;
#100154 = ORIENTED_EDGE ( 'NONE', *, *, #98388, .F. ) ;
#100153 = VERTEX_POINT ( 'NONE', #125628 ) ;
#100152 = DIRECTION ( 'NONE',  ( 1.000000000000000000, 0.000000000000000000, 0.000000000000000000 ) ) ;
#100155 = CIRCLE ( 'NONE', #204405, 11.74999999999999645 ) ;
#100156 = CARTESIAN_POINT ( 'NONE',  ( 21.04999999999999716, 65.49746832288542464, -95.46427766744905341 ) ) ;
#100157 = LINE ( 'NONE', #177194, #94039 ) ;
#100158 = DIRECTION ( 'NONE',  ( 1.000000000000000000, 0.000000000000000000, 0.000000000000000000 ) ) ;
#100159 = DIRECTION ( 'NONE',  ( -1.000000000000000000, -0.000000000000000000, 0.000000000000000000 ) ) ;
#100160 = AXIS2_PLACEMENT_3D ( 'NONE', #170889, #31363, #66602 ) ;
#100161 = LINE ( 'NONE', #179745, #43334 ) ;
#100162 = AXIS2_PLACEMENT_3D ( 'NONE', #68848, #44142, #148371 ) ;
#100163 = DIRECTION ( 'NONE',  ( 0.000000000000000000, 0.000000000000000000, -1.000000000000000000 ) ) ;
#100165 = CARTESIAN_POINT ( 'NONE',  ( -21.45000000000000284, 68.29142135624984178, -182.2731074845244166 ) ) ;
#100164 = DIRECTION ( 'NONE',  ( 0.000000000000000000, 8.673617379884087537E-15, -1.000000000000000000 ) ) ;
#100166 = VERTEX_POINT ( 'NONE', #206451 ) ;
#100167 = ORIENTED_EDGE ( 'NONE', *, *, #29087, .F. ) ;
#100168 = ADVANCED_FACE ( 'NONE', ( #106038 ), #29851, .T. ) ;
#100169 = DIRECTION ( 'NONE',  ( -1.000000000000000000, -0.000000000000000000, -0.000000000000000000 ) ) ;
#100172 = ORIENTED_EDGE ( 'NONE', *, *, #35004, .F. ) ;
#100171 = EDGE_CURVE ( 'NONE', #24921, #219174, #117311, .T. ) ;
#100170 = PLANE ( 'NONE',  #191148 ) ;
#100173 = DIRECTION ( 'NONE',  ( 0.000000000000000000, 0.000000000000000000, -1.000000000000000000 ) ) ;
#100174 = ORIENTED_EDGE ( 'NONE', *, *, #48729, .F. ) ;
#100175 = CARTESIAN_POINT ( 'NONE',  ( 22.39999999999999858, 7.790779598384538041, -100.5000000000000426 ) ) ;
#100176 = EDGE_LOOP ( 'NONE', ( #50720, #121179, #200515, #146539 ) ) ;
#100177 = CARTESIAN_POINT ( 'NONE',  ( 23.15000000000000213, -11.64999999998883595, -197.9999999999999432 ) ) ;
#100178 = EDGE_CURVE ( 'NONE', #224941, #227874, #83888, .T. ) ;
#100179 = EDGE_LOOP ( 'NONE', ( #157770, #35390, #118538 ) ) ;
#100180 = EDGE_CURVE ( 'NONE', #165186, #174151, #71540, .T. ) ;
#100181 = AXIS2_PLACEMENT_3D ( 'NONE', #199256, #243498, #42733 ) ;
#100182 = CYLINDRICAL_SURFACE ( 'NONE', #177072, 0.09999999999998898659 ) ;
#100183 = DIRECTION ( 'NONE',  ( -1.000000000000000000, 0.000000000000000000, 0.000000000000000000 ) ) ;
#100185 = ORIENTED_EDGE ( 'NONE', *, *, #25043, .T. ) ;
#100184 = ORIENTED_EDGE ( 'NONE', *, *, #5843, .T. ) ;
#100186 = ORIENTED_EDGE ( 'NONE', *, *, #238453, .T. ) ;
#100187 = DIRECTION ( 'NONE',  ( 0.000000000000000000, 0.000000000000000000, -1.000000000000000000 ) ) ;
#100189 = VERTEX_POINT ( 'NONE', #108634 ) ;
#100188 = ADVANCED_FACE ( 'NONE', ( #143900 ), #246849, .T. ) ;
#100190 = ORIENTED_EDGE ( 'NONE', *, *, #182228, .T. ) ;
#100191 = DIRECTION ( 'NONE',  ( 0.000000000000000000, -0.000000000000000000, 1.000000000000000000 ) ) ;
#100193 = ORIENTED_EDGE ( 'NONE', *, *, #151310, .T. ) ;
#100192 = DIRECTION ( 'NONE',  ( -0.000000000000000000, -6.982962677686266711E-15, 1.000000000000000000 ) ) ;
#100195 = CARTESIAN_POINT ( 'NONE',  ( -20.65000000000000568, 7.250000000011138646, -188.3499999999999659 ) ) ;
#100194 = DIRECTION ( 'NONE',  ( -1.000000000000000000, -0.000000000000000000, -0.000000000000000000 ) ) ;
#100196 = CARTESIAN_POINT ( 'NONE',  ( -18.59999999999999787, 11.56851667937982775, -211.1200010790121553 ) ) ;
#100197 = CYLINDRICAL_SURFACE ( 'NONE', #48296, 0.09999999999998898659 ) ;
#100198 = CARTESIAN_POINT ( 'NONE',  ( -17.22767730082392745, 10.34924421247985471, -178.8575713094251967 ) ) ;
#100199 = VERTEX_POINT ( 'NONE', #27852 ) ;
#100201 = ADVANCED_FACE ( 'NONE', ( #107342 ), #233997, .F. ) ;
#100200 = ORIENTED_EDGE ( 'NONE', *, *, #163107, .T. ) ;
#100202 = CARTESIAN_POINT ( 'NONE',  ( 21.05000000000000071, 1.115600667400684642E-11, -67.00000000000004263 ) ) ;
#100204 = CIRCLE ( 'NONE', #108435, 0.09999999999999832634 ) ;
#100203 = DIRECTION ( 'NONE',  ( 0.000000000000000000, 0.2617529984165031243, 0.9651348961777157509 ) ) ;
#100205 = DIRECTION ( 'NONE',  ( -2.252264143451594314E-15, 0.3848449534832963370, 0.9229812358755945523 ) ) ;
#100206 = CIRCLE ( 'NONE', #150321, 0.1000000000000028644 ) ;
#100207 = AXIS2_PLACEMENT_3D ( 'NONE', #23997, #103485, #542 ) ;
#100208 = ORIENTED_EDGE ( 'NONE', *, *, #256977, .F. ) ;
#100209 = DIRECTION ( 'NONE',  ( 0.000000000000000000, 0.000000000000000000, 1.000000000000000000 ) ) ;
#100210 = CARTESIAN_POINT ( 'NONE',  ( -23.25000000000000000, -11.64999999998884483, -130.9000000000000341 ) ) ;
#100211 = AXIS2_PLACEMENT_3D ( 'NONE', #188522, #52852, #111560 ) ;
#100212 = CARTESIAN_POINT ( 'NONE',  ( -21.14999999999999858, 76.10000000001198828, -109.5637644362255543 ) ) ;
#100213 = VERTEX_POINT ( 'NONE', #85178 ) ;
#100214 = VERTEX_POINT ( 'NONE', #65648 ) ;
#100215 = ADVANCED_FACE ( 'NONE', ( #184308 ), #166074, .T. ) ;
#100216 = DIRECTION ( 'NONE',  ( 1.000000000000000000, 0.000000000000000000, 0.000000000000000000 ) ) ;
#100217 = DIRECTION ( 'NONE',  ( -5.778696049164428005E-16, -0.1332476588733650935, 0.9910827722268042983 ) ) ;
#100218 = EDGE_LOOP ( 'NONE', ( #131363, #208909, #127302, #173076 ) ) ;
#100219 = CARTESIAN_POINT ( 'NONE',  ( 18.54999999999999716, 11.24151875332162831, -211.4982501455723138 ) ) ;
#100220 = ORIENTED_EDGE ( 'NONE', *, *, #187011, .F. ) ;
#100221 = DIRECTION ( 'NONE',  ( 1.000000000000000000, 0.000000000000000000, 0.000000000000000000 ) ) ;
#100222 = DIRECTION ( 'NONE',  ( 1.186688945009010077E-16, 0.9651348961777157509, -0.2617529984165031243 ) ) ;
#100224 = PRESENTATION_STYLE_ASSIGNMENT (( #158978 ) ) ;
#100223 = CARTESIAN_POINT ( 'NONE',  ( -21.37071067811865532, 10.49266777380207216, -211.2519653646891413 ) ) ;
#100225 = AXIS2_PLACEMENT_3D ( 'NONE', #31423, #50916, #30123 ) ;
#100226 = CARTESIAN_POINT ( 'NONE',  ( 5.999999999999995559, -11.65000000000000036, 10.00000000000000178 ) ) ;
#100227 = FACE_OUTER_BOUND ( 'NONE', #229831, .T. ) ;
#100228 = ORIENTED_EDGE ( 'NONE', *, *, #117352, .F. ) ;
#100229 = DIRECTION ( 'NONE',  ( 0.000000000000000000, -7.056502275159890043E-15, 1.000000000000000000 ) ) ;
#100230 = ADVANCED_FACE ( 'NONE', ( #29149 ), #100697, .T. ) ;
#100232 = ORIENTED_EDGE ( 'NONE', *, *, #33252, .T. ) ;
#100231 = ORIENTED_EDGE ( 'NONE', *, *, #184433, .F. ) ;
#100233 = ORIENTED_EDGE ( 'NONE', *, *, #160241, .T. ) ;
#100234 = CARTESIAN_POINT ( 'NONE',  ( -16.92132318717937522, 66.03392997600636249, -157.4007008541723565 ) ) ;
#100235 = DIRECTION ( 'NONE',  ( 0.000000000000000000, 0.000000000000000000, -1.000000000000000000 ) ) ;
#100236 = CARTESIAN_POINT ( 'NONE',  ( 18.54999999999999716, 9.949999999999997513, -12.64999999999994529 ) ) ;
#100237 = CARTESIAN_POINT ( 'NONE',  ( -20.54999999999999716, 85.00000000001207923, -126.6291383618717816 ) ) ;
#100238 = DIRECTION ( 'NONE',  ( 1.000000000000000000, -0.000000000000000000, 0.000000000000000000 ) ) ;
#100239 = AXIS2_PLACEMENT_3D ( 'NONE', #128568, #110272, #11188 ) ;
#100240 = EDGE_CURVE ( 'NONE', #116906, #67614, #5650, .T. ) ;
#100242 = CYLINDRICAL_SURFACE ( 'NONE', #215514, 0.1000000000000066530 ) ;
#100241 = CARTESIAN_POINT ( 'NONE',  ( 20.86036036209909383, 10.62104277657096318, -7.666348418505070761 ) ) ;
#100243 = ORIENTED_EDGE ( 'NONE', *, *, #100178, .F. ) ;
#100244 = DIRECTION ( 'NONE',  ( 2.952720810173289112E-16, -0.9770955615653316162, -0.2128009952263598403 ) ) ;
#100245 = ORIENTED_EDGE ( 'NONE', *, *, #234238, .T. ) ;
#100246 = LINE ( 'NONE', #1153, #171665 ) ;
#100247 = EDGE_LOOP ( 'NONE', ( #239371, #15829, #48785, #114721 ) ) ;
#100248 = ORIENTED_EDGE ( 'NONE', *, *, #200961, .F. ) ;
#100249 = FACE_OUTER_BOUND ( 'NONE', #215985, .T. ) ;
#100250 = AXIS2_PLACEMENT_3D ( 'NONE', #163833, #187258, #105093 ) ;
#100251 = SPHERICAL_SURFACE ( 'NONE', #68519, 0.1000000000000000056 ) ;
#100253 = EDGE_CURVE ( 'NONE', #67166, #225035, #44812, .T. ) ;
#100252 = CARTESIAN_POINT ( 'NONE',  ( -18.59999999999999787, 46.02130280899747561, -256.6489974955837852 ) ) ;
#100254 = ADVANCED_FACE ( 'NONE', ( #228312 ), #50917, .T. ) ;
#100255 = CARTESIAN_POINT ( 'NONE',  ( 21.05000000000000071, -10.56629024491939894, -206.4738935375009703 ) ) ;
#100256 = B_SPLINE_CURVE_WITH_KNOTS ( 'NONE', 3,
 ( #236112, #138275, #178752, #199587, #118753, #56173, #213990, #39226, #159176, #95322, #174917, #57460, #254367, #238682 ),
 .UNSPECIFIED., .F., .F.,
 ( 4, 2, 2, 2, 2, 2, 4 ),
 ( 0.000000000000000000, 2.389617747640384587E-05, 4.779235495280769174E-05, 9.558470990564789599E-05, 0.0001911694198113680541, 0.0003823388396228101049, 0.0007646776792456942608 ),
 .UNSPECIFIED. ) ;
#100257 = VECTOR ( 'NONE', #94987, 1000.000000000000114 ) ;
#100258 = ADVANCED_FACE ( 'NONE', ( #30124 ), #26262, .T. ) ;
#100259 = EDGE_CURVE ( 'NONE', #54224, #10328, #90059, .T. ) ;
#100260 = DIRECTION ( 'NONE',  ( 1.000000000000000000, 0.000000000000000000, 0.000000000000000000 ) ) ;
#100261 = ORIENTED_EDGE ( 'NONE', *, *, #8998, .T. ) ;
#100262 = EDGE_LOOP ( 'NONE', ( #252881, #235194, #117222 ) ) ;
#100263 = EDGE_CURVE ( 'NONE', #60084, #141837, #107056, .T. ) ;
#100264 = AXIS2_PLACEMENT_3D ( 'NONE', #127900, #131743, #232146 ) ;
#100265 = DIRECTION ( 'NONE',  ( -1.000000000000000000, 0.000000000000000000, 0.000000000000000000 ) ) ;
#100266 = ORIENTED_EDGE ( 'NONE', *, *, #130596, .T. ) ;
#100267 = DIRECTION ( 'NONE',  ( 0.000000000000000000, -0.2128009952263604232, 0.9770955615653316162 ) ) ;
#100268 = CARTESIAN_POINT ( 'NONE',  ( 23.14999999999999858, 76.00000000001170974, -69.52310748452431710 ) ) ;
#100269 = CARTESIAN_POINT ( 'NONE',  ( 18.49999999999999289, 14.61354176542825201, -235.9279552357344016 ) ) ;
#100270 = CARTESIAN_POINT ( 'NONE',  ( 23.24999999999999289, 80.15000000001214175, -136.5231074845242460 ) ) ;
#100271 = CARTESIAN_POINT ( 'NONE',  ( 21.78635804494511419, 0.09900506551883611617, -59.96433851484686528 ) ) ;
#100272 = CARTESIAN_POINT ( 'NONE',  ( 18.59999999999999076, 0.000000000000000000, -33.50000000000000000 ) ) ;
#100274 = FACE_OUTER_BOUND ( 'NONE', #46810, .T. ) ;
#100273 = CARTESIAN_POINT ( 'NONE',  ( -18.54270223418606633, 85.62410550289501998, -129.7821724341168590 ) ) ;
#100275 = LINE ( 'NONE', #177309, #191612 ) ;
#100276 = CARTESIAN_POINT ( 'NONE',  ( -23.15000000000000213, 47.91013932883114990, -242.3192343197862044 ) ) ;
#100277 = DIRECTION ( 'NONE',  ( -0.000000000000000000, 0.8490545835447373957, 0.5283051335749753274 ) ) ;
#100278 = CARTESIAN_POINT ( 'NONE',  ( -16.91256925476569606, 9.985731158139328656, -54.46764248900526439 ) ) ;
#100279 = AXIS2_PLACEMENT_3D ( 'NONE', #217130, #118053, #197584 ) ;
#100280 = EDGE_CURVE ( 'NONE', #111063, #84368, #127925, .T. ) ;
#100282 = ORIENTED_EDGE ( 'NONE', *, *, #247308, .T. ) ;
#100281 = AXIS2_PLACEMENT_3D ( 'NONE', #160749, #158195, #180283 ) ;
#100283 = CARTESIAN_POINT ( 'NONE',  ( 20.95566103547454517, 10.61824765095822087, -41.13184019298059013 ) ) ;
#100284 = EDGE_LOOP ( 'NONE', ( #253892, #53672, #23008, #188167, #216365 ) ) ;
#100285 = ADVANCED_FACE ( 'NONE', ( #47075 ), #227010, .F. ) ;
#100286 = ADVANCED_FACE ( 'NONE', ( #66667 ), #151355, .F. ) ;
#100287 = CIRCLE ( 'NONE', #108692, 11.64999999999999325 ) ;
#100288 = VECTOR ( 'NONE', #60946, 1000.000000000000000 ) ;
#100289 = CARTESIAN_POINT ( 'NONE',  ( 18.47654891039378455, 85.46527494839439498, -129.3971315793295958 ) ) ;
#100290 = DIRECTION ( 'NONE',  ( 0.000000000000000000, 0.000000000000000000, 1.000000000000000000 ) ) ;
#100291 = CARTESIAN_POINT ( 'NONE',  ( -22.39999999999999858, 76.00000000001170974, -77.31388708289772183 ) ) ;
#100292 = ORIENTED_EDGE ( 'NONE', *, *, #42020, .F. ) ;
#100293 = CARTESIAN_POINT ( 'NONE',  ( 22.50000000000000000, 7.790779598384538929, -167.3999999999999773 ) ) ;
#100294 = DIRECTION ( 'NONE',  ( 0.000000000000000000, 0.000000000000000000, -1.000000000000000000 ) ) ;
#100295 = DIRECTION ( 'NONE',  ( 1.000000000000000000, 0.000000000000000000, -0.000000000000000000 ) ) ;
#100296 = CIRCLE ( 'NONE', #146109, 0.09999999999999939493 ) ;
#100297 = DIRECTION ( 'NONE',  ( 0.000000000000000000, 0.000000000000000000, 1.000000000000000000 ) ) ;
#100298 = VECTOR ( 'NONE', #241261, 1000.000000000000114 ) ;
#100299 = VECTOR ( 'NONE', #92284, 1000.000000000000000 ) ;
#100300 = FACE_OUTER_BOUND ( 'NONE', #39076, .T. ) ;
#100301 = DIRECTION ( 'NONE',  ( 0.000000000000000000, 1.000000000000000000, -6.308085367188393199E-16 ) ) ;
#100302 = VECTOR ( 'NONE', #139060, 1000.000000000000000 ) ;
#100303 = AXIS2_PLACEMENT_3D ( 'NONE', #29789, #43718, #125812 ) ;
#100304 = VERTEX_POINT ( 'NONE', #91370 ) ;
#100305 = FACE_OUTER_BOUND ( 'NONE', #151094, .T. ) ;
#100307 = ORIENTED_EDGE ( 'NONE', *, *, #131688, .F. ) ;
#100306 = DIRECTION ( 'NONE',  ( -0.000000000000000000, 1.000000000000000000, 7.525063763929033127E-15 ) ) ;
#100308 = CARTESIAN_POINT ( 'NONE',  ( 21.05000000000000071, 0.000000000000000000, -33.50000000000000000 ) ) ;
#100309 = CARTESIAN_POINT ( 'NONE',  ( 20.94999999999999929, 1.115600667400684642E-11, -100.5000000000000426 ) ) ;
#100310 = DIRECTION ( 'NONE',  ( -1.000000000000000000, 3.469446951953635015E-14, 0.000000000000000000 ) ) ;
#100311 = ORIENTED_EDGE ( 'NONE', *, *, #164789, .F. ) ;
#100312 = CARTESIAN_POINT ( 'NONE',  ( -18.50000000000000000, 72.08710075277885210, -158.5412845115134246 ) ) ;
#100313 = PRODUCT_CONTEXT ( 'NONE', #127392, 'mechanical' ) ;
#100314 = AXIS2_PLACEMENT_3D ( 'NONE', #96335, #118510, #81890 ) ;
#100315 = CARTESIAN_POINT ( 'NONE',  ( 23.24999999999997513, 11.75000000000000711, -26.48519422934605672 ) ) ;
#100316 = VERTEX_POINT ( 'NONE', #31424 ) ;
#100317 = DIRECTION ( 'NONE',  ( 1.000000000000000000, 0.000000000000000000, 0.000000000000000000 ) ) ;
#100318 = CARTESIAN_POINT ( 'NONE',  ( -23.25000000000000000, 34.80778438379478246, -248.5595576589601592 ) ) ;
#100319 = FACE_OUTER_BOUND ( 'NONE', #138203, .T. ) ;
#100320 = ORIENTED_EDGE ( 'NONE', *, *, #24231, .T. ) ;
#100321 = ORIENTED_EDGE ( 'NONE', *, *, #249016, .T. ) ;
#100322 = DIRECTION ( 'NONE',  ( 0.000000000000000000, 0.000000000000000000, 1.000000000000000000 ) ) ;
#100323 = CYLINDRICAL_SURFACE ( 'NONE', #163380, 0.09999999999998898659 ) ;
#100324 = AXIS2_PLACEMENT_3D ( 'NONE', #40223, #115888, #195445 ) ;
#100325 = CARTESIAN_POINT ( 'NONE',  ( 23.15000000000000213, -11.48912529306489994, -197.9999999999999432 ) ) ;
#100326 = CARTESIAN_POINT ( 'NONE',  ( -21.05000000000000071, 87.29603075034691528, -66.47520832486038955 ) ) ;
#100327 = EDGE_CURVE ( 'NONE', #163036, #63872, #154931, .T. ) ;
#100328 = PLANE ( 'NONE',  #93170 ) ;
#100330 = FACE_OUTER_BOUND ( 'NONE', #225816, .T. ) ;
#100329 = DIRECTION ( 'NONE',  ( 0.000000000000000000, 0.9887567792719329507, 0.1495327102803732933 ) ) ;
#100331 = CARTESIAN_POINT ( 'NONE',  ( 21.30000000000002558, 66.17117490947157421, -239.7639228359981303 ) ) ;
#100332 = EDGE_CURVE ( 'NONE', #74117, #208340, #179864, .T. ) ;
#100333 = FACE_OUTER_BOUND ( 'NONE', #180991, .T. ) ;
#100334 = CARTESIAN_POINT ( 'NONE',  ( 18.52643265882457868, 65.68026841930851845, -30.47257401318894665 ) ) ;
#100335 = DIRECTION ( 'NONE',  ( 0.000000000000000000, -6.982962677686266711E-15, 1.000000000000000000 ) ) ;
#100336 = VERTEX_POINT ( 'NONE', #250427 ) ;
#100337 = CIRCLE ( 'NONE', #162735, 2.100000000000004530 ) ;
#100338 = EDGE_LOOP ( 'NONE', ( #190025, #36728, #85014, #238536, #229105, #103119, #243728, #165728, #141614 ) ) ;
#100339 = CARTESIAN_POINT ( 'NONE',  ( -23.25000000000000000, 31.89597452117651244, -238.9192857152811769 ) ) ;
#100341 = CARTESIAN_POINT ( 'NONE',  ( 20.84999999999999432, 77.16412189325258453, -28.10825939895270764 ) ) ;
#100340 = CARTESIAN_POINT ( 'NONE',  ( -20.54999999999999716, 36.65892442174472876, -249.5511627012454596 ) ) ;
#100342 = ADVANCED_FACE ( 'NONE', ( #11850 ), #84101, .F. ) ;
#100343 = AXIS2_PLACEMENT_3D ( 'NONE', #249738, #133636, #170252 ) ;
#100344 = ADVANCED_FACE ( 'NONE', ( #52216 ), #131765, .F. ) ;
#100345 = DIRECTION ( 'NONE',  ( -0.000000000000000000, -0.000000000000000000, -1.000000000000000000 ) ) ;
#100346 = CARTESIAN_POINT ( 'NONE',  ( 21.05000000000000071, 87.48912529308842068, -166.9231074845242802 ) ) ;
#100347 = LINE ( 'NONE', #80785, #169104 ) ;
#100348 = ORIENTED_EDGE ( 'NONE', *, *, #10641, .T. ) ;
#100349 = CARTESIAN_POINT ( 'NONE',  ( -23.15000000000000213, 11.65000000001115588, -179.6499999999999773 ) ) ;
#100350 = VERTEX_POINT ( 'NONE', #86191 ) ;
#100351 = DIRECTION ( 'NONE',  ( 1.000000000000000000, 0.000000000000000000, 0.000000000000000000 ) ) ;
#100352 = ORIENTED_EDGE ( 'NONE', *, *, #40637, .T. ) ;
#100353 = CARTESIAN_POINT ( 'NONE',  ( -20.94999999999999929, 1.261786168576181755, -41.58649896354548048 ) ) ;
#100354 = AXIS2_PLACEMENT_3D ( 'NONE', #12760, #216054, #34899 ) ;
#100355 = CIRCLE ( 'NONE', #137964, 0.1000000000000002554 ) ;
#100356 = EDGE_CURVE ( 'NONE', #89932, #128108, #189183, .T. ) ;
#100357 = ADVANCED_FACE ( 'NONE', ( #6676 ), #245304, .F. ) ;
#100358 = CARTESIAN_POINT ( 'NONE',  ( 18.33683296300380405, 85.51114997114433436, -29.11740007181401424 ) ) ;
#100359 = VECTOR ( 'NONE', #211075, 1000.000000000000000 ) ;
#100360 = ORIENTED_EDGE ( 'NONE', *, *, #34401, .T. ) ;
#100361 =( BOUNDED_SURFACE ( )  B_SPLINE_SURFACE ( 3, 2, ( 
 ( #59017, #16106, #172640 ),
 ( #194743, #235133, #112619 ),
 ( #133461, #192171, #95610 ),
 ( #156906, #257202, #93046 ) ),
 .UNSPECIFIED., .F., .F., .F. ) 
 B_SPLINE_SURFACE_WITH_KNOTS ( ( 4, 4 ),
 ( 3, 3 ),
 ( 0.0002700421466196708999, 0.0004789321604330827272 ),
 ( 0.000000000000000000, 1.000000000000000000 ),
 .UNSPECIFIED. ) 
 GEOMETRIC_REPRESENTATION_ITEM ( )  RATIONAL_B_SPLINE_SURFACE ( (
 ( 1.000000000000000000, 0.7071067811865475727, 1.000000000000000000),
 ( 1.000000000000000000, 0.7163411249511302259, 1.000000000000000000),
 ( 1.000000000000000000, 0.7221957104842335884, 1.000000000000000000),
 ( 1.000000000000000000, 0.7250110520819756932, 1.000000000000000000) ) ) 
 REPRESENTATION_ITEM ( '' )  SURFACE ( )  );
#100362 = ORIENTED_EDGE ( 'NONE', *, *, #111236, .F. ) ;
#100363 = CARTESIAN_POINT ( 'NONE',  ( -21.53699400379686324, 69.21228820681083960, -69.52310748452437394 ) ) ;
#100364 = LINE ( 'NONE', #182524, #178257 ) ;
#100365 = CARTESIAN_POINT ( 'NONE',  ( -21.29999999999995808, 4.959819536546777642E-16, 4.049999999999998934 ) ) ;
#100366 = DIRECTION ( 'NONE',  ( 1.000000000000000000, 0.000000000000000000, 0.000000000000000000 ) ) ;
#100367 = EDGE_CURVE ( 'NONE', #214553, #185809, #88225, .T. ) ;
#100369 = CARTESIAN_POINT ( 'NONE',  ( -18.40000000000000213, 11.48667500176882328, -143.2500000000000284 ) ) ;
#100368 = CARTESIAN_POINT ( 'NONE',  ( 23.14999999999999503, 11.65000000001116298, -193.9851942293460070 ) ) ;
#100370 = AXIS2_PLACEMENT_3D ( 'NONE', #88250, #249924, #248634 ) ;
#100371 = PLANE ( 'NONE',  #236386 ) ;
#100374 = ORIENTED_EDGE ( 'NONE', *, *, #219703, .T. ) ;
#100373 = ADVANCED_FACE ( 'NONE', ( #67940 ), #28868, .T. ) ;
#100372 = CARTESIAN_POINT ( 'NONE',  ( 20.59588692710267921, 65.63127657884298571, -128.8840263900139576 ) ) ;
#100376 = CARTESIAN_POINT ( 'NONE',  ( 18.59999999999999787, 72.02722222756958104, -225.1832529173024398 ) ) ;
#100375 = DIRECTION ( 'NONE',  ( -1.000000000000000000, 0.000000000000000000, 0.000000000000000000 ) ) ;
#100377 = ORIENTED_EDGE ( 'NONE', *, *, #154282, .F. ) ;
#100379 = ORIENTED_EDGE ( 'NONE', *, *, #20959, .F. ) ;
#100378 = CARTESIAN_POINT ( 'NONE',  ( -18.50000000000000000, 10.29270135741298375, -72.45736188715194714 ) ) ;
#100380 = ORIENTED_EDGE ( 'NONE', *, *, #203043, .F. ) ;
#100381 = LINE ( 'NONE', #80824, #15951 ) ;
#100382 = CARTESIAN_POINT ( 'NONE',  ( 21.05000000000005400, 65.25000000001119815, -3.123107484524795474 ) ) ;
#100383 = CARTESIAN_POINT ( 'NONE',  ( 18.50000000000000000, -9.499999999988842703, -140.6001893912220737 ) ) ;
#100384 = EDGE_LOOP ( 'NONE', ( #122308, #43968, #154791, #103756 ) ) ;
#100385 = DIRECTION ( 'NONE',  ( 2.940209281316621016E-16, 1.000000000000000000, 7.056502275159890832E-15 ) ) ;
#100386 = DIRECTION ( 'NONE',  ( 0.000000000000000000, 0.000000000000000000, -1.000000000000000000 ) ) ;
#100387 = CARTESIAN_POINT ( 'NONE',  ( 20.93284271247462414, 11.75000000001116085, -93.48519422934610645 ) ) ;
#100388 = EDGE_CURVE ( 'NONE', #69713, #188264, #75792, .T. ) ;
#100389 = ORIENTED_EDGE ( 'NONE', *, *, #134969, .F. ) ;
#100390 = EDGE_CURVE ( 'NONE', #165408, #7150, #57343, .T. ) ;
#100391 = DIRECTION ( 'NONE',  ( -1.000000000000000000, -0.000000000000000000, -0.000000000000000000 ) ) ;
#100392 = AXIS2_PLACEMENT_3D ( 'NONE', #94624, #13816, #229022 ) ;
#100393 = AXIS2_PLACEMENT_3D ( 'NONE', #129601, #172628, #134710 ) ;
#100394 = CIRCLE ( 'NONE', #17239, 0.5000000000000004441 ) ;
#100396 = AXIS2_PLACEMENT_3D ( 'NONE', #33669, #146173, #93589 ) ;
#100395 = CARTESIAN_POINT ( 'NONE',  ( 20.85000000000000142, 7.070967871809997973, -171.2465642218683115 ) ) ;
#100397 = EDGE_CURVE ( 'NONE', #208145, #255700, #171499, .T. ) ;
#100398 = ORIENTED_EDGE ( 'NONE', *, *, #133655, .T. ) ;
#100399 = ORIENTED_EDGE ( 'NONE', *, *, #151668, .T. ) ;
#100400 = DIRECTION ( 'NONE',  ( -1.000000000000000000, 0.000000000000000000, 0.000000000000000000 ) ) ;
#100401 = ORIENTED_EDGE ( 'NONE', *, *, #114713, .F. ) ;
#100402 = VECTOR ( 'NONE', #106085, 1000.000000000000114 ) ;
#100403 = CYLINDRICAL_SURFACE ( 'NONE', #96651, 0.09999999999998898659 ) ;
#100404 = EDGE_LOOP ( 'NONE', ( #245114, #247809, #257100, #213039 ) ) ;
#100405 = CARTESIAN_POINT ( 'NONE',  ( -23.15000000000000213, 2.600000000011154278, -53.77537807723790309 ) ) ;
#100406 = CARTESIAN_POINT ( 'NONE',  ( -18.50000000000000000, 77.83534155023598089, -57.96795619196132776 ) ) ;
#100407 = CARTESIAN_POINT ( 'NONE',  ( -1.739115166359751801E-14, 64.35000000001151932, -48.17310748452440095 ) ) ;
#100408 = ADVANCED_FACE ( 'NONE', ( #176061 ), #212604, .T. ) ;
#100409 = CARTESIAN_POINT ( 'NONE',  ( -16.27683809663751191, 44.28952310016010330, -235.8873797767049325 ) ) ;
#100410 = CARTESIAN_POINT ( 'NONE',  ( -16.87786941232801041, 63.08497791849498526, -213.0992491019884483 ) ) ;
#100411 = AXIS2_PLACEMENT_3D ( 'NONE', #122488, #139450, #202016 ) ;
#100412 = ADVANCED_FACE ( 'NONE', ( #76922 ), #18245, .F. ) ;
#100413 = CARTESIAN_POINT ( 'NONE',  ( 22.39999999999999858, 0.1000000000111554016, -25.70922040162662014 ) ) ;
#100414 = CARTESIAN_POINT ( 'NONE',  ( -22.39999999999999858, -0.1008583690875575894, -88.75043287651062940 ) ) ;
#100415 = CARTESIAN_POINT ( 'NONE',  ( -20.94999999999994600, 65.35000000001120668, -4.423107484524790856 ) ) ;
#100416 = ORIENTED_EDGE ( 'NONE', *, *, #63587, .F. ) ;
#100417 = DIRECTION ( 'NONE',  ( 0.000000000000000000, -0.8660254037844383745, 0.5000000000000003331 ) ) ;
#100418 = EDGE_LOOP ( 'NONE', ( #12252, #55820, #69394, #109200, #57552 ) ) ;
#100421 = ORIENTED_EDGE ( 'NONE', *, *, #130925, .F. ) ;
#100420 = DIRECTION ( 'NONE',  ( 1.000000000000000000, 0.000000000000000000, 0.000000000000000000 ) ) ;
#100419 = CARTESIAN_POINT ( 'NONE',  ( -16.87331047859649757, 14.15900158805613884, -219.2550725561364118 ) ) ;
#100422 = ORIENTED_EDGE ( 'NONE', *, *, #6203, .T. ) ;
#100423 = DIRECTION ( 'NONE',  ( 0.000000000000000000, 1.000000000000000000, 0.000000000000000000 ) ) ;
#100424 = CARTESIAN_POINT ( 'NONE',  ( -21.14999999999994174, 79.78873604695631627, -7.297728304630792806 ) ) ;
#100425 = DIRECTION ( 'NONE',  ( 0.000000000000000000, -1.000000000000000000, 0.000000000000000000 ) ) ;
#100426 = ORIENTED_EDGE ( 'NONE', *, *, #210634, .F. ) ;
#100427 = DIRECTION ( 'NONE',  ( -0.000000000000000000, 0.000000000000000000, 1.000000000000000000 ) ) ;
#100428 = AXIS2_PLACEMENT_3D ( 'NONE', #229308, #89771, #50637 ) ;
#100429 = DIRECTION ( 'NONE',  ( -1.000000000000000000, -0.000000000000000000, -0.000000000000000000 ) ) ;
#100431 = CARTESIAN_POINT ( 'NONE',  ( 21.05000000000000071, 68.01971615331018484, -227.7939507667808527 ) ) ;
#100430 = CARTESIAN_POINT ( 'NONE',  ( -21.93642651522410247, 7.327166239336959208, -167.4999999999999716 ) ) ;
#100433 = ORIENTED_EDGE ( 'NONE', *, *, #15828, .T. ) ;
#100432 = SPHERICAL_SURFACE ( 'NONE', #209861, 0.1000000000000000056 ) ;
#100434 = AXIS2_PLACEMENT_3D ( 'NONE', #253317, #51243, #169986 ) ;
#100435 = ORIENTED_EDGE ( 'NONE', *, *, #69755, .T. ) ;
#100436 = CIRCLE ( 'NONE', #71452, 0.5000000000000004441 ) ;
#100437 = DIRECTION ( 'NONE',  ( -6.938893903907222856E-15, 1.000000000000000000, 0.000000000000000000 ) ) ;
#100439 = VERTEX_POINT ( 'NONE', #13118 ) ;
#100438 = AXIS2_PLACEMENT_3D ( 'NONE', #134601, #35557, #12142 ) ;
#100440 = CARTESIAN_POINT ( 'NONE',  ( 18.59999999999999432, 77.16270174995064224, -195.4231074845243370 ) ) ;
#100441 = ORIENTED_EDGE ( 'NONE', *, *, #72612, .T. ) ;
#100442 = PLANE ( 'NONE',  #197359 ) ;
#100443 = AXIS2_PLACEMENT_3D ( 'NONE', #160326, #123746, #62492 ) ;
#100444 = DIRECTION ( 'NONE',  ( 0.000000000000000000, -1.000000000000000000, 0.000000000000000000 ) ) ;
#100445 = DIRECTION ( 'NONE',  ( -0.000000000000000000, 1.000000000000000000, 1.734723475976807292E-15 ) ) ;
#100446 = ORIENTED_EDGE ( 'NONE', *, *, #188020, .T. ) ;
#100447 = DIRECTION ( 'NONE',  ( 1.000000000000000000, -0.000000000000000000, -0.000000000000000000 ) ) ;
#100448 = AXIS2_PLACEMENT_3D ( 'NONE', #76484, #214717, #195192 ) ;
#100449 = ADVANCED_FACE ( 'NONE', ( #195621 ), #15706, .T. ) ;
#100450 = AXIS2_PLACEMENT_3D ( 'NONE', #18310, #220376, #256868 ) ;
#100451 = AXIS2_PLACEMENT_3D ( 'NONE', #126417, #106843, #122590 ) ;
#100452 = ORIENTED_EDGE ( 'NONE', *, *, #130525, .T. ) ;
#100453 = EDGE_LOOP ( 'NONE', ( #720, #213410, #71991, #60258, #195301, #245845, #53243, #236046, #190671, #151, #58128 ) ) ;
#100455 =( BOUNDED_SURFACE ( )  B_SPLINE_SURFACE ( 3, 2, ( 
 ( #208763, #225717, #167093 ),
 ( #129218, #246583, #147495 ),
 ( #70556, #105769, #164504 ),
 ( #165795, #228321, #30135 ),
 ( #28880, #189197, #206184 ),
 ( #90067, #169671, #187914 ) ),
 .UNSPECIFIED., .F., .F., .T. ) 
 B_SPLINE_SURFACE_WITH_KNOTS ( ( 4, 2, 4 ),
 ( 3, 3 ),
 ( 0.0001381104793128107321, 0.0002947094729387620326, 0.0004513084665647133873 ),
 ( 0.000000000000000000, 1.000000000000000000 ),
 .UNSPECIFIED. ) 
 GEOMETRIC_REPRESENTATION_ITEM ( )  RATIONAL_B_SPLINE_SURFACE ( (
 ( 1.000000000000000000, 0.7071067811865475727, 1.000000000000000000),
 ( 1.000000000000000000, 0.6919563088099242032, 1.000000000000000000),
 ( 1.000000000000000000, 0.6959445945717356308, 1.000000000000000000),
 ( 1.000000000000000000, 0.7137882985313203088, 1.000000000000000000),
 ( 1.000000000000000000, 0.7257496306096423710, 1.000000000000000000),
 ( 1.000000000000000000, 0.7250110520819876836, 1.000000000000000000) ) ) 
 REPRESENTATION_ITEM ( '' )  SURFACE ( )  );
#100454 = VECTOR ( 'NONE', #170304, 1000.000000000000000 ) ;
#100456 = EDGE_LOOP ( 'NONE', ( #171079, #92157, #27611, #27442 ) ) ;
#100457 = DIRECTION ( 'NONE',  ( 0.000000000000000000, 1.000000000000000000, 2.891205793294679805E-16 ) ) ;
#100459 = EDGE_CURVE ( 'NONE', #248008, #27458, #59006, .T. ) ;
#100458 = ORIENTED_EDGE ( 'NONE', *, *, #85258, .T. ) ;
#100461 = ORIENTED_EDGE ( 'NONE', *, *, #40915, .T. ) ;
#100460 = LINE ( 'NONE', #22259, #134339 ) ;
#100462 = AXIS2_PLACEMENT_3D ( 'NONE', #185742, #142738, #7091 ) ;
#100463 = VERTEX_POINT ( 'NONE', #136901 ) ;
#100464 = EDGE_CURVE ( 'NONE', #89253, #24478, #114777, .T. ) ;
#100465 = EDGE_CURVE ( 'NONE', #14603, #178965, #254796, .T. ) ;
#100468 = ORIENTED_EDGE ( 'NONE', *, *, #64486, .F. ) ;
#100467 = ORIENTED_EDGE ( 'NONE', *, *, #173309, .T. ) ;
#100466 = DIRECTION ( 'NONE',  ( 0.000000000000000000, 0.000000000000000000, -1.000000000000000000 ) ) ;
#100469 = ORIENTED_EDGE ( 'NONE', *, *, #195233, .T. ) ;
#100470 = DIRECTION ( 'NONE',  ( -1.000000000000000000, 2.952720810173289112E-16, 2.061873921506763405E-30 ) ) ;
#100471 = AXIS2_PLACEMENT_3D ( 'NONE', #63120, #162260, #4435 ) ;
#100472 = COLOUR_RGB ( '', 0.66274510, 0.83137255, 0.94901961) ;
#100473 = CIRCLE ( 'NONE', #246262, 0.1000000000000024342 ) ;
#100474 = DIRECTION ( 'NONE',  ( 1.000000000000000000, 0.000000000000000000, 0.000000000000000000 ) ) ;
#100475 = CARTESIAN_POINT ( 'NONE',  ( -16.84793658983437581, 14.14120149177083263, -219.1733417585090820 ) ) ;
#100476 = ORIENTED_EDGE ( 'NONE', *, *, #6385, .F. ) ;
#100477 = EDGE_CURVE ( 'NONE', #85514, #78573, #246474, .T. ) ;
#100478 = LINE ( 'NONE', #82194, #24847 ) ;
#100481 = EDGE_LOOP ( 'NONE', ( #148252, #42688, #225497, #235347, #63157 ) ) ;
#100480 = EDGE_CURVE ( 'NONE', #48218, #82481, #125667, .T. ) ;
#100479 = CARTESIAN_POINT ( 'NONE',  ( 22.42357213249528769, 7.672932386371071445, -167.4009130359983999 ) ) ;
#100482 = CARTESIAN_POINT ( 'NONE',  ( -20.85000000000000142, -11.65000000000000036, -30.59999999999999432 ) ) ;
#100484 = VERTEX_POINT ( 'NONE', #97743 ) ;
#100483 = DIRECTION ( 'NONE',  ( 0.000000000000000000, -0.9126074666063660468, -0.4088369013363524762 ) ) ;
#100485 = ORIENTED_EDGE ( 'NONE', *, *, #222355, .F. ) ;
#100486 = ORIENTED_EDGE ( 'NONE', *, *, #137946, .F. ) ;
#100487 = ORIENTED_EDGE ( 'NONE', *, *, #255207, .F. ) ;
#100488 = CARTESIAN_POINT ( 'NONE',  ( 21.05000000000000071, -11.64999999998883595, -100.5000000000000284 ) ) ;
#100489 = DIRECTION ( 'NONE',  ( 1.000000000000000000, 0.000000000000000000, 0.000000000000000000 ) ) ;
#100491 = ORIENTED_EDGE ( 'NONE', *, *, #55589, .T. ) ;
#100490 = ORIENTED_EDGE ( 'NONE', *, *, #141251, .T. ) ;
#100492 = ORIENTED_EDGE ( 'NONE', *, *, #8991, .F. ) ;
#100493 = CARTESIAN_POINT ( 'NONE',  ( 21.13920837816993270, 61.96073055383985206, -221.7331827770995574 ) ) ;
#100495 = ORIENTED_EDGE ( 'NONE', *, *, #150660, .T. ) ;
#100494 = EDGE_CURVE ( 'NONE', #119565, #134457, #159029, .T. ) ;
#100496 = VERTEX_POINT ( 'NONE', #37833 ) ;
#100497 = CARTESIAN_POINT ( 'NONE',  ( -20.94999999999999929, 70.15000000001148805, -46.15560470880229360 ) ) ;
#100498 = ORIENTED_EDGE ( 'NONE', *, *, #56272, .T. ) ;
#100499 = SPHERICAL_SURFACE ( 'NONE', #106471, 0.1000000000000000056 ) ;
#100501 = DIRECTION ( 'NONE',  ( 0.000000000000000000, -0.9908441862701605762, 0.1350103645451835310 ) ) ;
#100500 = CARTESIAN_POINT ( 'NONE',  ( -23.25000000000000355, 64.25000000001190870, -93.77310748452438816 ) ) ;
#100502 = VECTOR ( 'NONE', #218492, 1000.000000000000000 ) ;
#100503 = ORIENTED_EDGE ( 'NONE', *, *, #81788, .F. ) ;
#100506 = EDGE_CURVE ( 'NONE', #182918, #34173, #177353, .T. ) ;
#100505 = VERTEX_POINT ( 'NONE', #133065 ) ;
#100504 = EDGE_LOOP ( 'NONE', ( #26639, #202217, #61256, #200880 ) ) ;
#100507 = CARTESIAN_POINT ( 'NONE',  ( -21.05000000000000071, 75.96636726467907863, -209.7819246792057868 ) ) ;
#100508 = DIRECTION ( 'NONE',  ( -1.000000000000000000, -0.000000000000000000, -0.000000000000000000 ) ) ;
#100509 = ORIENTED_EDGE ( 'NONE', *, *, #131424, .T. ) ;
#100510 = CIRCLE ( 'NONE', #104603, 0.09999999999999939493 ) ;
#100511 = FACE_OUTER_BOUND ( 'NONE', #228470, .T. ) ;
#100512 = EDGE_LOOP ( 'NONE', ( #109611, #229725, #40235, #154232 ) ) ;
#100513 = ORIENTED_EDGE ( 'NONE', *, *, #252822, .F. ) ;
#100514 = DIRECTION ( 'NONE',  ( 0.000000000000000000, 0.2128009952263601179, -0.9770955615653315052 ) ) ;
#100515 = ORIENTED_EDGE ( 'NONE', *, *, #138189, .T. ) ;
#100516 = DIRECTION ( 'NONE',  ( -1.020425574104004394E-15, -0.9126074666063769270, -0.4088369013363280513 ) ) ;
#100517 = DIRECTION ( 'NONE',  ( 0.000000000000000000, 0.1455152366551500653, 0.9893560106964507384 ) ) ;
#100518 = ORIENTED_EDGE ( 'NONE', *, *, #210232, .F. ) ;
#100519 = CARTESIAN_POINT ( 'NONE',  ( -23.15000000000000213, 76.00000000001170974, -69.52310748452431710 ) ) ;
#100520 = DIRECTION ( 'NONE',  ( -1.000000000000000000, -0.000000000000000000, -0.000000000000000000 ) ) ;
#100522 = DIRECTION ( 'NONE',  ( 0.000000000000000000, 0.000000000000000000, 1.000000000000000000 ) ) ;
#100521 = DIRECTION ( 'NONE',  ( -1.000000000000000000, 0.000000000000000000, 0.000000000000000000 ) ) ;
#100523 = CARTESIAN_POINT ( 'NONE',  ( 18.59999999999999076, 28.95347087985017609, -237.9930060266852081 ) ) ;
#100524 = EDGE_CURVE ( 'NONE', #94156, #233837, #56056, .T. ) ;
#100525 = DIRECTION ( 'NONE',  ( -0.000000000000000000, -1.000000000000000000, 0.000000000000000000 ) ) ;
#100526 = CARTESIAN_POINT ( 'NONE',  ( -16.90138253750127362, 63.04949597677561712, -213.2612322484624485 ) ) ;
#100527 = LINE ( 'NONE', #203524, #182107 ) ;
#100528 = CARTESIAN_POINT ( 'NONE',  ( 21.05000000000000071, 75.96513199699909080, -142.7931933482134070 ) ) ;
#100529 = FACE_OUTER_BOUND ( 'NONE', #239252, .T. ) ;
#100530 = CIRCLE ( 'NONE', #58843, 0.1000000000000088318 ) ;
#100531 = EDGE_LOOP ( 'NONE', ( #3122, #248632 ) ) ;
#100532 = CIRCLE ( 'NONE', #217244, 11.89999999999999325 ) ;
#100533 = EDGE_CURVE ( 'NONE', #69026, #233212, #79859, .T. ) ;
#100535 = ORIENTED_EDGE ( 'NONE', *, *, #52489, .T. ) ;
#100534 = ORIENTED_EDGE ( 'NONE', *, *, #227326, .T. ) ;
#100536 = ORIENTED_EDGE ( 'NONE', *, *, #255632, .T. ) ;
#100538 = EDGE_LOOP ( 'NONE', ( #257810, #68261, #46077, #169779 ) ) ;
#100537 = EDGE_CURVE ( 'NONE', #162828, #114115, #146498, .T. ) ;
#100539 = CARTESIAN_POINT ( 'NONE',  ( 20.94999999999999574, 1.250000000011155299, -108.5000000000000426 ) ) ;
#100540 = DIRECTION ( 'NONE',  ( 1.000000000000000000, 0.000000000000000000, 0.000000000000000000 ) ) ;
#100541 = EDGE_CURVE ( 'NONE', #74935, #139316, #58630, .T. ) ;
#100542 = ADVANCED_FACE ( 'NONE', ( #1220, #23410 ), #99028, .F. ) ;
#100544 = DIRECTION ( 'NONE',  ( -0.000000000000000000, 0.9667078373770138233, 0.2558827019434041783 ) ) ;
#100543 = DIRECTION ( 'NONE',  ( 0.000000000000000000, 1.000000000000000000, 6.853228547068871147E-15 ) ) ;
#100545 = DIRECTION ( 'NONE',  ( 0.000000000000000000, 0.2617529984165035684, 0.9651348961777156399 ) ) ;
#100546 = VERTEX_POINT ( 'NONE', #100318 ) ;
#100547 = DIRECTION ( 'NONE',  ( 0.000000000000000000, 6.982962677686266711E-15, -1.000000000000000000 ) ) ;
#100548 = PLANE ( 'NONE',  #229206 ) ;
#100549 = AXIS2_PLACEMENT_3D ( 'NONE', #253964, #171918, #170650 ) ;
#100550 = EDGE_CURVE ( 'NONE', #189014, #104609, #198156, .T. ) ;
#100551 = ORIENTED_EDGE ( 'NONE', *, *, #101853, .F. ) ;
#100552 = EDGE_CURVE ( 'NONE', #226290, #117519, #40410, .T. ) ;
#100554 = ADVANCED_FACE ( 'NONE', ( #121234 ), #24688, .F. ) ;
#100553 = ADVANCED_FACE ( 'NONE', ( #80758 ), #203296, .T. ) ;
#100555 = CARTESIAN_POINT ( 'NONE',  ( 20.00000000000000355, 1.350000000000000089, 16.60000000000000142 ) ) ;
#100556 = DIRECTION ( 'NONE',  ( 1.186688945009009831E-16, 1.000000000000000000, 6.982962677686266711E-15 ) ) ;
#100557 = ORIENTED_EDGE ( 'NONE', *, *, #124653, .T. ) ;
#100558 = FACE_OUTER_BOUND ( 'NONE', #82493, .T. ) ;
#100559 = DIRECTION ( 'NONE',  ( 1.000000000000000000, 0.000000000000000000, -0.000000000000000000 ) ) ;
#100560 = CARTESIAN_POINT ( 'NONE',  ( -17.01825945287481545, 66.05000000001224691, -149.2731074845244450 ) ) ;
#100561 = DIRECTION ( 'NONE',  ( 0.000000000000000000, -7.272083257015735086E-15, 1.000000000000000000 ) ) ;
#100562 = CARTESIAN_POINT ( 'NONE',  ( -18.44085059012131822, 11.51401249348380063, -24.24030531912154629 ) ) ;
#100563 = ORIENTED_EDGE ( 'NONE', *, *, #166800, .F. ) ;
#100564 = CARTESIAN_POINT ( 'NONE',  ( -23.15000000000000213, 76.00000000001149658, -47.82310748452432847 ) ) ;
#100565 = SPHERICAL_SURFACE ( 'NONE', #71446, 0.1000000000000000056 ) ;
#100566 = LINE ( 'NONE', #75908, #170935 ) ;
#100567 = EDGE_CURVE ( 'NONE', #148919, #109963, #83312, .T. ) ;
#100570 = CARTESIAN_POINT ( 'NONE',  ( 23.15000000000000213, 87.75000000001251976, -182.1731074845242802 ) ) ;
#100569 = AXIS2_PLACEMENT_3D ( 'NONE', #28955, #208827, #169738 ) ;
#100568 = DIRECTION ( 'NONE',  ( 0.000000000000000000, -6.467318590049456648E-15, 1.000000000000000000 ) ) ;
#100571 = DIRECTION ( 'NONE',  ( 0.000000000000000000, 0.000000000000000000, -1.000000000000000000 ) ) ;
#100572 = CIRCLE ( 'NONE', #192201, 0.1000000000000028644 ) ;
#100573 = LINE ( 'NONE', #202283, #99737 ) ;
#100574 = CARTESIAN_POINT ( 'NONE',  ( -23.15000000000000213, 69.05648948627110428, -235.0374527038057977 ) ) ;
#100575 = FACE_OUTER_BOUND ( 'NONE', #38782, .T. ) ;
#100576 = ADVANCED_FACE ( 'NONE', ( #182468 ), #138166, .F. ) ;
#100577 = EDGE_CURVE ( 'NONE', #103860, #4003, #162914, .T. ) ;
#100578 = VERTEX_POINT ( 'NONE', #258083 ) ;
#100579 = ORIENTED_EDGE ( 'NONE', *, *, #37310, .F. ) ;
#100580 = EDGE_CURVE ( 'NONE', #96459, #54193, #159063, .T. ) ;
#100581 = ORIENTED_EDGE ( 'NONE', *, *, #197105, .F. ) ;
#100582 = DIRECTION ( 'NONE',  ( 0.000000000000000000, 0.9126074666063777041, 0.4088369013363266080 ) ) ;
#100583 = EDGE_CURVE ( 'NONE', #18233, #51864, #242410, .T. ) ;
#100584 = CIRCLE ( 'NONE', #154631, 0.1000000000000028644 ) ;
#100585 = DIRECTION ( 'NONE',  ( -0.000000000000000000, 0.07893460099011784248, -0.9968797965484760271 ) ) ;
#100586 = CARTESIAN_POINT ( 'NONE',  ( -18.50000000000000000, 65.70711192142317714, -30.56510546851221477 ) ) ;
#100587 = CARTESIAN_POINT ( 'NONE',  ( 21.46681500598292658, 65.43630044540458357, -242.4735498273664689 ) ) ;
#100588 = ORIENTED_EDGE ( 'NONE', *, *, #183826, .F. ) ;
#100589 = CARTESIAN_POINT ( 'NONE',  ( 20.94999999999999929, 76.00000000001247713, -174.0231074845243882 ) ) ;
#100590 = DIRECTION ( 'NONE',  ( 0.000000000000000000, 0.2617529984165152257, 0.9651348961777124202 ) ) ;
#100591 = CARTESIAN_POINT ( 'NONE',  ( -20.64999999999999858, -4.259020970815408091, -226.0869574510824123 ) ) ;
#100592 = DIRECTION ( 'NONE',  ( 0.000000000000000000, 0.9126074666064812879, 0.4088369013360954596 ) ) ;
#100594 = EDGE_LOOP ( 'NONE', ( #740, #181913, #139053, #220532 ) ) ;
#100593 = DIRECTION ( 'NONE',  ( -1.000000000000000000, -1.652117596168391700E-15, -1.153667551319263085E-29 ) ) ;
#100596 = CARTESIAN_POINT ( 'NONE',  ( -23.15000000000000213, 85.60000000001198828, -112.9170766071766820 ) ) ;
#100595 = CARTESIAN_POINT ( 'NONE',  ( 18.59999999999999787, -11.74999999998883737, -192.3499999999999659 ) ) ;
#100598 = DIRECTION ( 'NONE',  ( -2.915501640297154283E-16, 1.000000000000000000, 0.000000000000000000 ) ) ;
#100597 = AXIS2_PLACEMENT_3D ( 'NONE', #85435, #4634, #146705 ) ;
#100599 = CARTESIAN_POINT ( 'NONE',  ( 18.59999999999999787, 72.02722222756958104, -225.1832529173024398 ) ) ;
#100600 = ORIENTED_EDGE ( 'NONE', *, *, #142996, .F. ) ;
#100601 = CIRCLE ( 'NONE', #29940, 0.09999999999999939493 ) ;
#100602 = DIRECTION ( 'NONE',  ( 0.000000000000000000, 0.000000000000000000, 1.000000000000000000 ) ) ;
#100603 = DIRECTION ( 'NONE',  ( 0.000000000000000000, -0.1298341882519953583, -0.9915357197604861561 ) ) ;
#100604 = DIRECTION ( 'NONE',  ( 0.000000000000000000, -0.2128009952263605897, 0.9770955615653313941 ) ) ;
#100605 = VERTEX_POINT ( 'NONE', #179900 ) ;
#100606 = AXIS2_PLACEMENT_3D ( 'NONE', #133069, #172235, #213879 ) ;
#100607 = CARTESIAN_POINT ( 'NONE',  ( -20.94999999999999929, -0.2561057920810652089, -33.46510355832771211 ) ) ;
#100608 = DIRECTION ( 'NONE',  ( 0.000000000000000000, 1.000000000000000000, 0.000000000000000000 ) ) ;
#100609 = ORIENTED_EDGE ( 'NONE', *, *, #234903, .T. ) ;
#100610 = CARTESIAN_POINT ( 'NONE',  ( 22.39999999999999503, 29.50811709945092076, -252.6450601445781103 ) ) ;
#100611 = AXIS2_PLACEMENT_3D ( 'NONE', #10536, #48362, #127913 ) ;
#100613 = FACE_OUTER_BOUND ( 'NONE', #119548, .T. ) ;
#100612 = CIRCLE ( 'NONE', #38306, 0.1000000000000010186 ) ;
#100614 = CARTESIAN_POINT ( 'NONE',  ( -20.54999999999999716, 52.73346022503534414, -255.2251647023667260 ) ) ;
#100615 = ORIENTED_EDGE ( 'NONE', *, *, #146188, .F. ) ;
#100616 = ORIENTED_EDGE ( 'NONE', *, *, #182493, .F. ) ;
#100617 = AXIS2_PLACEMENT_3D ( 'NONE', #199999, #22664, #21377 ) ;
#100619 = CIRCLE ( 'NONE', #121540, 11.80000000000000426 ) ;
#100618 = CARTESIAN_POINT ( 'NONE',  ( -21.07928932188134041, 69.67148334361864670, -103.1220026301787414 ) ) ;
#100620 = CARTESIAN_POINT ( 'NONE',  ( -18.59999999999999787, 77.16270174994961906, -61.42310748452431568 ) ) ;
#100621 = EDGE_CURVE ( 'NONE', #5154, #223523, #81370, .T. ) ;
#100622 = CARTESIAN_POINT ( 'NONE',  ( 20.94999999999999929, 10.72371710471867701, -121.7500000000000426 ) ) ;
#100623 = CARTESIAN_POINT ( 'NONE',  ( 18.59999999999999076, 14.77103648604101593, -236.4083752604500717 ) ) ;
#100625 = CARTESIAN_POINT ( 'NONE',  ( 20.97224591636398827, 10.62515341616362363, -12.24992590466357534 ) ) ;
#100624 = CARTESIAN_POINT ( 'NONE',  ( -20.94999999999999929, 1.162701749949165642, -74.90000000000004832 ) ) ;
#100626 = VECTOR ( 'NONE', #106489, 1000.000000000000114 ) ;
#100627 = CARTESIAN_POINT ( 'NONE',  ( -18.54270223418606633, -9.624105502882903451, -40.24093505040743679 ) ) ;
#100628 = EDGE_CURVE ( 'NONE', #2004, #87393, #254963, .T. ) ;
#100629 = CARTESIAN_POINT ( 'NONE',  ( -16.87683809663752399, 66.15000000001157332, -56.12074346632808641 ) ) ;
#100631 = CARTESIAN_POINT ( 'NONE',  ( 18.41416235934318024, -9.499999999988842703, -107.1001893912220879 ) ) ;
#100630 = AXIS2_PLACEMENT_3D ( 'NONE', #20615, #100100, #194122 ) ;
#100632 = EDGE_LOOP ( 'NONE', ( #46559, #61412, #135993, #108006 ) ) ;
#100633 = DIRECTION ( 'NONE',  ( 0.000000000000000000, 0.000000000000000000, 1.000000000000000000 ) ) ;
#100635 = VERTEX_POINT ( 'NONE', #164180 ) ;
#100634 = CARTESIAN_POINT ( 'NONE',  ( 21.05000000000000071, 87.48912529308852015, -173.1231074845242688 ) ) ;
#100636 = DIRECTION ( 'NONE',  ( 0.000000000000000000, 0.000000000000000000, -1.000000000000000000 ) ) ;
#100637 = DIRECTION ( 'NONE',  ( 1.000000000000000000, -0.000000000000000000, -0.000000000000000000 ) ) ;
#100639 = CYLINDRICAL_SURFACE ( 'NONE', #170097, 7.900000000000010125 ) ;
#100638 = CARTESIAN_POINT ( 'NONE',  ( 23.14999999999998437, 36.65892442174472876, -249.5511627012454596 ) ) ;
#100640 = VECTOR ( 'NONE', #125981, 1000.000000000000114 ) ;
#100641 = EDGE_CURVE ( 'NONE', #165624, #138330, #183738, .T. ) ;
#100642 = EDGE_CURVE ( 'NONE', #22041, #86026, #222433, .T. ) ;
#100643 = EDGE_LOOP ( 'NONE', ( #255345, #157295, #148913, #240694, #92130, #177795, #51644 ) ) ;
#100645 = CARTESIAN_POINT ( 'NONE',  ( -16.94445028196808778, 22.96031635112858282, -230.8778361528912058 ) ) ;
#100644 = DIRECTION ( 'NONE',  ( 0.000000000000000000, 1.000000000000000000, 0.000000000000000000 ) ) ;
#100646 = FACE_OUTER_BOUND ( 'NONE', #186540, .T. ) ;
#100647 = LINE ( 'NONE', #182811, #230394 ) ;
#100648 = DIRECTION ( 'NONE',  ( 1.000000000000000000, 0.000000000000000000, 0.000000000000000000 ) ) ;
#100649 = DIRECTION ( 'NONE',  ( -4.391705002472929091E-16, 1.000000000000000000, 0.000000000000000000 ) ) ;
#100650 = ORIENTED_EDGE ( 'NONE', *, *, #86334, .T. ) ;
#100651 = ORIENTED_EDGE ( 'NONE', *, *, #180549, .F. ) ;
#100652 = CARTESIAN_POINT ( 'NONE',  ( -16.77779411440718604, 9.946101447118758543, -54.33694258299546220 ) ) ;
#100653 = ORIENTED_EDGE ( 'NONE', *, *, #79742, .T. ) ;
#100655 = DIRECTION ( 'NONE',  ( 0.000000000000000000, -0.2617529984165036239, -0.9651348961777156399 ) ) ;
#100654 = AXIS2_PLACEMENT_3D ( 'NONE', #135000, #49403, #17639 ) ;
#100656 = AXIS2_PLACEMENT_3D ( 'NONE', #220304, #63778, #85879 ) ;
#100657 = ORIENTED_EDGE ( 'NONE', *, *, #178243, .F. ) ;
#100658 = AXIS2_PLACEMENT_3D ( 'NONE', #208157, #230257, #186005 ) ;
#100659 = ADVANCED_FACE ( 'NONE', ( #174162 ), #188391, .T. ) ;
#100660 = DIRECTION ( 'NONE',  ( 0.000000000000000000, 0.9126074666063771490, 0.4088369013363281623 ) ) ;
#100661 = AXIS2_PLACEMENT_3D ( 'NONE', #66608, #67884, #247806 ) ;
#100662 = ADVANCED_FACE ( 'NONE', ( #133698 ), #54152, .T. ) ;
#100663 = LINE ( 'NONE', #19896, #193334 ) ;
#100664 = ORIENTED_EDGE ( 'NONE', *, *, #22618, .F. ) ;
#100665 = DIRECTION ( 'NONE',  ( -1.836970198721029934E-16, 1.000000000000000000, 0.000000000000000000 ) ) ;
#100666 = CARTESIAN_POINT ( 'NONE',  ( -18.60000000000000142, -8.250000000000005329, 10.52591260281975138 ) ) ;
#100667 = DIRECTION ( 'NONE',  ( 0.000000000000000000, -6.467318590049456648E-15, 1.000000000000000000 ) ) ;
#100668 = DIRECTION ( 'NONE',  ( 0.000000000000000000, 0.000000000000000000, -1.000000000000000000 ) ) ;
#100669 = EDGE_CURVE ( 'NONE', #244131, #27688, #142588, .T. ) ;
#100670 = CARTESIAN_POINT ( 'NONE',  ( -20.64999999999999858, 76.00000000001142553, -36.02310748452432421 ) ) ;
#100671 = DIRECTION ( 'NONE',  ( 0.000000000000000000, 0.4088369013363345461, -0.9126074666063741514 ) ) ;
#100673 = ORIENTED_EDGE ( 'NONE', *, *, #110435, .T. ) ;
#100672 = EDGE_CURVE ( 'NONE', #64541, #9313, #152014, .T. ) ;
#100674 = AXIS2_PLACEMENT_3D ( 'NONE', #50198, #56303, #36797 ) ;
#100675 = DIRECTION ( 'NONE',  ( 1.000000000000000000, 0.000000000000000000, 0.000000000000000000 ) ) ;
#100676 = VERTEX_POINT ( 'NONE', #89429 ) ;
#100678 = VERTEX_POINT ( 'NONE', #51559 ) ;
#100677 = CARTESIAN_POINT ( 'NONE',  ( -16.86578989773641979, 66.01519019875307492, -90.48777237114661887 ) ) ;
#100679 = EDGE_LOOP ( 'NONE', ( #65555, #241916, #144150, #209105, #247902 ) ) ;
#100680 = LINE ( 'NONE', #180262, #198889 ) ;
#100681 = CARTESIAN_POINT ( 'NONE',  ( -1.739115166359751801E-14, 11.65000000001114699, -179.7499999999999716 ) ) ;
#100682 = CARTESIAN_POINT ( 'NONE',  ( 15.70340296795548518, 66.64411154551001459, -187.2344645877464018 ) ) ;
#100683 = DIRECTION ( 'NONE',  ( -0.000000000000000000, 0.000000000000000000, 1.000000000000000000 ) ) ;
#100684 = DIRECTION ( 'NONE',  ( 0.7071067811865475727, -0.2890913453342130457, 0.6453109281988448354 ) ) ;
#100685 = ORIENTED_EDGE ( 'NONE', *, *, #168237, .T. ) ;
#100686 = DIRECTION ( 'NONE',  ( 0.000000000000000000, 6.982962677686266711E-15, -1.000000000000000000 ) ) ;
#100687 = CARTESIAN_POINT ( 'NONE',  ( 20.94999999999999929, 77.83534155023671985, -158.4679561919613491 ) ) ;
#100688 = EDGE_CURVE ( 'NONE', #85966, #37312, #34310, .T. ) ;
#100689 = VERTEX_POINT ( 'NONE', #73755 ) ;
#100690 = ADVANCED_FACE ( 'NONE', ( #169019 ), #221692, .F. ) ;
#100691 = CARTESIAN_POINT ( 'NONE',  ( 18.49351773456767134, -9.443025695134084074, -174.6853255260267872 ) ) ;
#100692 = CARTESIAN_POINT ( 'NONE',  ( -16.80621392010904103, 9.942202577518958861, -79.68959196541678125 ) ) ;
#100693 = EDGE_CURVE ( 'NONE', #193738, #11451, #55091, .T. ) ;
#100694 = ORIENTED_EDGE ( 'NONE', *, *, #122302, .F. ) ;
#100695 = CARTESIAN_POINT ( 'NONE',  ( 23.15000000000000213, -6.937571600298355179, -224.3614019333310807 ) ) ;
#100696 = EDGE_CURVE ( 'NONE', #171236, #191879, #150996, .T. ) ;
#100697 = TOROIDAL_SURFACE ( 'NONE', #63301, 11.65000000000000036, 0.1000000000000000056 ) ;
#100698 = DIRECTION ( 'NONE',  ( 0.000000000000000000, 0.8753622295931610120, -0.4834676483506316624 ) ) ;
#100699 = ORIENTED_EDGE ( 'NONE', *, *, #87222, .T. ) ;
#100700 = SPHERICAL_SURFACE ( 'NONE', #229492, 0.1000000000000000056 ) ;
#100701 = DIRECTION ( 'NONE',  ( 0.000000000000000000, -0.9525900758537791946, 0.3042567129660267988 ) ) ;
#100703 = CYLINDRICAL_SURFACE ( 'NONE', #68160, 0.09999999999999939493 ) ;
#100702 = APPLICATION_CONTEXT ( 'automotive_design' ) ;
#100704 = ADVANCED_FACE ( 'NONE', ( #150701 ), #52866, .F. ) ;
#100705 = DIRECTION ( 'NONE',  ( 0.000000000000000000, 1.000000000000000000, 0.000000000000000000 ) ) ;
#100706 = EDGE_CURVE ( 'NONE', #5450, #16939, #192495, .T. ) ;
#100707 = CIRCLE ( 'NONE', #30048, 0.1999999999999987899 ) ;
#100708 = DIRECTION ( 'NONE',  ( -1.000000000000000000, 0.000000000000000000, 0.000000000000000000 ) ) ;
#100709 = CIRCLE ( 'NONE', #167417, 4.049999999999998046 ) ;
#100711 = EDGE_LOOP ( 'NONE', ( #82622, #128790, #10845, #137373 ) ) ;
#100710 = AXIS2_PLACEMENT_3D ( 'NONE', #22491, #101971, #45878 ) ;
#100712 = SURFACE_STYLE_USAGE ( .BOTH. , #203709 ) ;
#100713 = ORIENTED_EDGE ( 'NONE', *, *, #189155, .T. ) ;
#100714 = CARTESIAN_POINT ( 'NONE',  ( -18.44448725179914916, 85.49008171549576218, -163.3941471904618083 ) ) ;
#100716 = EDGE_CURVE ( 'NONE', #225961, #235379, #15057, .T. ) ;
#100715 = CARTESIAN_POINT ( 'NONE',  ( -16.94878442675511820, 9.991729103002155554, -79.61178042436216629 ) ) ;
#100718 = EDGE_LOOP ( 'NONE', ( #256993, #100685, #236488 ) ) ;
#100717 = CARTESIAN_POINT ( 'NONE',  ( 21.14999999999999858, 11.65000000001116298, -146.1500000000000341 ) ) ;
#100719 = CARTESIAN_POINT ( 'NONE',  ( -20.94999999999999929, 36.65892442174935439, -249.5511627012433848 ) ) ;
#100720 = CARTESIAN_POINT ( 'NONE',  ( 22.49806830649814060, 64.35011034517287953, -103.1005718008498917 ) ) ;
#100721 = CARTESIAN_POINT ( 'NONE',  ( 21.07928932188134397, 75.90110485435759813, -109.3516241409176217 ) ) ;
#100722 = DIRECTION ( 'NONE',  ( -0.000000000000000000, -0.000000000000000000, -1.000000000000000000 ) ) ;
#100723 = DIRECTION ( 'NONE',  ( -0.1538461538461484146, -0.9880948137434723000, 0.000000000000000000 ) ) ;
#100724 = CYLINDRICAL_SURFACE ( 'NONE', #178105, 0.09999999999999939493 ) ;
#100726 = ORIENTED_EDGE ( 'NONE', *, *, #162371, .F. ) ;
#100725 = CARTESIAN_POINT ( 'NONE',  ( -23.15000000000000213, 8.772386841380839684, -220.8375963540301257 ) ) ;
#100727 = VECTOR ( 'NONE', #249980, 1000.000000000000000 ) ;
#100728 = B_SPLINE_CURVE_WITH_KNOTS ( 'NONE', 3,
 ( #51987, #209806, #31209, #54567, #111999, #114553, #50694 ),
 .UNSPECIFIED., .F., .F.,
 ( 4, 3, 4 ),
 ( 0.000000000000000000, 3.357501770814503222E-05, 5.199112466349739759E-05 ),
 .UNSPECIFIED. ) ;
#100729 = DIRECTION ( 'NONE',  ( 0.000000000000000000, -1.000000000000000000, 0.000000000000000000 ) ) ;
#100730 = ORIENTED_EDGE ( 'NONE', *, *, #58973, .F. ) ;
#100731 = ORIENTED_EDGE ( 'NONE', *, *, #233999, .T. ) ;
#100732 = CARTESIAN_POINT ( 'NONE',  ( -18.40000000000000213, 85.50000000001168132, -62.92291809330220786 ) ) ;
#100733 = CARTESIAN_POINT ( 'NONE',  ( -18.46946985241234529, 85.50931722872408614, -196.5364449190244613 ) ) ;
#100734 = ORIENTED_EDGE ( 'NONE', *, *, #157850, .F. ) ;
#100735 = FACE_OUTER_BOUND ( 'NONE', #113760, .T. ) ;
#100736 = AXIS2_PLACEMENT_3D ( 'NONE', #82675, #145243, #123135 ) ;
#100737 = CARTESIAN_POINT ( 'NONE',  ( -18.40000000000000568, 85.50000000001162448, -62.52374538734409981 ) ) ;
#100738 = ORIENTED_EDGE ( 'NONE', *, *, #65994, .T. ) ;
#100739 = CYLINDRICAL_SURFACE ( 'NONE', #231118, 0.1000000000000002554 ) ;
#100740 = CARTESIAN_POINT ( 'NONE',  ( 22.39999999999999858, 65.09550114356429162, -243.3481044654562879 ) ) ;
#100741 = ORIENTED_EDGE ( 'NONE', *, *, #51974, .F. ) ;
#100742 = ORIENTED_EDGE ( 'NONE', *, *, #167510, .T. ) ;
#100743 = DIRECTION ( 'NONE',  ( -1.000000000000000000, -0.000000000000000000, -0.000000000000000000 ) ) ;
#100744 = ORIENTED_EDGE ( 'NONE', *, *, #45161, .T. ) ;
#100745 = CARTESIAN_POINT ( 'NONE',  ( -21.14999999999999858, 76.00000000001242029, -176.5637644362255969 ) ) ;
#100747 = ADVANCED_FACE ( 'NONE', ( #157140 ), #16347, .T. ) ;
#100746 = ORIENTED_EDGE ( 'NONE', *, *, #219347, .F. ) ;
#100749 = ORIENTED_EDGE ( 'NONE', *, *, #56439, .T. ) ;
#100748 = CARTESIAN_POINT ( 'NONE',  ( -21.52071067811865746, 65.25928687755708779, -213.4062711467677502 ) ) ;
#100750 = AXIS2_PLACEMENT_3D ( 'NONE', #73770, #228973, #50305 ) ;
#100751 = CARTESIAN_POINT ( 'NONE',  ( -18.50000000000000000, 66.75000000001223555, -148.6731074845244223 ) ) ;
#100752 = EDGE_LOOP ( 'NONE', ( #69355, #171832, #5705, #60098 ) ) ;
#100753 = EDGE_CURVE ( 'NONE', #228873, #142411, #63481, .T. ) ;
#100754 = DIRECTION ( 'NONE',  ( 0.000000000000000000, 0.2617529984164915779, 0.9651348961777189706 ) ) ;
#100755 = ADVANCED_FACE ( 'NONE', ( #253628 ), #154583, .T. ) ;
#100756 = VERTEX_POINT ( 'NONE', #56694 ) ;
#100758 = EDGE_LOOP ( 'NONE', ( #60112, #173988, #235925, #77896 ) ) ;
#100757 = ORIENTED_EDGE ( 'NONE', *, *, #228281, .T. ) ;
#100759 = CARTESIAN_POINT ( 'NONE',  ( -20.94999999999999929, 18.18127959618848521, -237.5711165786817389 ) ) ;
#100760 = CARTESIAN_POINT ( 'NONE',  ( -16.94445028196807002, 14.20918193489391790, -219.2878138714100373 ) ) ;
#100761 = VERTEX_POINT ( 'NONE', #55410 ) ;
#100762 = AXIS2_PLACEMENT_3D ( 'NONE', #221749, #62713, #99244 ) ;
#100763 = ORIENTED_EDGE ( 'NONE', *, *, #49642, .T. ) ;
#100764 = EDGE_CURVE ( 'NONE', #147015, #22594, #171875, .T. ) ;
#100765 = DIRECTION ( 'NONE',  ( 0.000000000000000000, -0.8660254037844383745, 0.5000000000000003331 ) ) ;
#100767 = DIRECTION ( 'NONE',  ( -0.000000000000000000, 0.2617529984165031243, 0.9651348961777157509 ) ) ;
#100766 = CIRCLE ( 'NONE', #246554, 0.1000000000000057648 ) ;
#100769 = EDGE_LOOP ( 'NONE', ( #1081, #40689 ) ) ;
#100768 = FACE_OUTER_BOUND ( 'NONE', #57348, .T. ) ;
#100770 = CARTESIAN_POINT ( 'NONE',  ( 21.00000000000000000, 66.25000000001229239, -157.6731074845244223 ) ) ;
#100771 = ORIENTED_EDGE ( 'NONE', *, *, #113320, .F. ) ;
#100772 = CARTESIAN_POINT ( 'NONE',  ( -18.57399277249657032, 65.66887361445355964, -130.9329845918269370 ) ) ;
#100773 = CIRCLE ( 'NONE', #254877, 0.1000000000000032391 ) ;
#100774 = ORIENTED_EDGE ( 'NONE', *, *, #137461, .F. ) ;
#100775 = CYLINDRICAL_SURFACE ( 'NONE', #167045, 11.75000000000000000 ) ;
#100776 = DIRECTION ( 'NONE',  ( 0.000000000000000000, 0.000000000000000000, 1.000000000000000000 ) ) ;
#100777 = SPHERICAL_SURFACE ( 'NONE', #161423, 0.1000000000000000056 ) ;
#100778 = AXIS2_PLACEMENT_3D ( 'NONE', #6485, #239985, #103011 ) ;
#100779 = AXIS2_PLACEMENT_3D ( 'NONE', #169818, #12007, #91526 ) ;
#100781 = ORIENTED_EDGE ( 'NONE', *, *, #117134, .T. ) ;
#100780 = VECTOR ( 'NONE', #36746, 1000.000000000000227 ) ;
#100782 = FACE_OUTER_BOUND ( 'NONE', #213439, .T. ) ;
#100783 = ORIENTED_EDGE ( 'NONE', *, *, #222094, .F. ) ;
#100784 = ORIENTED_EDGE ( 'NONE', *, *, #79157, .F. ) ;
#100785 = AXIS2_PLACEMENT_3D ( 'NONE', #100308, #221534, #99017 ) ;
#100786 = CARTESIAN_POINT ( 'NONE',  ( 21.05000000000000071, 7.128833340094563376, -233.7327013124401276 ) ) ;
#100787 = ORIENTED_EDGE ( 'NONE', *, *, #45538, .F. ) ;
#100788 = ORIENTED_EDGE ( 'NONE', *, *, #60527, .T. ) ;
#100789 = CARTESIAN_POINT ( 'NONE',  ( -21.05000000000000071, 5.900000000011102586, -177.7190997646563915 ) ) ;
#100790 = ADVANCED_FACE ( 'NONE', ( #197514 ), #119286, .F. ) ;
#100791 = DIRECTION ( 'NONE',  ( -0.000000000000000000, -0.000000000000000000, 1.000000000000000000 ) ) ;
#100792 = EDGE_LOOP ( 'NONE', ( #87240, #32861, #213424, #29098 ) ) ;
#100793 = EDGE_CURVE ( 'NONE', #6205, #156110, #209236, .T. ) ;
#100794 = ORIENTED_EDGE ( 'NONE', *, *, #172059, .F. ) ;
#100795 = DIRECTION ( 'NONE',  ( 0.000000000000000000, -1.000000000000000000, 0.000000000000000000 ) ) ;
#100796 = AXIS2_PLACEMENT_3D ( 'NONE', #53758, #34229, #22033 ) ;
#100797 = DIRECTION ( 'NONE',  ( 0.000000000000000000, -0.6728971962616412394, -0.7397360091703134577 ) ) ;
#100799 = VERTEX_POINT ( 'NONE', #219644 ) ;
#100798 = VECTOR ( 'NONE', #124065, 1000.000000000000000 ) ;
#100801 = ADVANCED_FACE ( 'NONE', ( #198803 ), #96785, .T. ) ;
#100800 = ORIENTED_EDGE ( 'NONE', *, *, #156774, .T. ) ;
#100802 = AXIS2_PLACEMENT_3D ( 'NONE', #24445, #42692, #183495 ) ;
#100803 = AXIS2_PLACEMENT_3D ( 'NONE', #14736, #207803, #12168 ) ;
#100804 = VERTEX_POINT ( 'NONE', #98377 ) ;
#100805 = AXIS2_PLACEMENT_3D ( 'NONE', #37179, #17580, #257427 ) ;
#100806 = CARTESIAN_POINT ( 'NONE',  ( -16.91256925476570672, 66.01426884188362010, -82.05546499551910244 ) ) ;
#100807 = CARTESIAN_POINT ( 'NONE',  ( 18.51565452909167675, 85.35285933884784981, -196.3281981632918587 ) ) ;
#100808 = CARTESIAN_POINT ( 'NONE',  ( -18.59999999999999787, 1.340746217944851715, -56.72713749457886223 ) ) ;
#100809 = DIRECTION ( 'NONE',  ( -1.000000000000000000, 0.000000000000000000, 0.000000000000000000 ) ) ;
#100810 = CARTESIAN_POINT ( 'NONE',  ( 20.95595624212450048, 65.37610879691814603, -162.3934745703977001 ) ) ;
#100811 = CARTESIAN_POINT ( 'NONE',  ( -23.15000000000000213, 67.23127455305835554, -235.8551265064784559 ) ) ;
#100813 = ADVANCED_FACE ( 'NONE', ( #138791 ), #218349, .F. ) ;
#100812 = DIRECTION ( 'NONE',  ( -1.000000000000000000, -0.000000000000000000, -0.000000000000000000 ) ) ;
#100815 = CYLINDRICAL_SURFACE ( 'NONE', #132759, 0.09999999999999939493 ) ;
#100814 = CYLINDRICAL_SURFACE ( 'NONE', #82048, 2.000000000000013323 ) ;
#100816 = CARTESIAN_POINT ( 'NONE',  ( 23.14999999999999858, 64.35000000001195986, -110.0379132551783243 ) ) ;
#100817 = FACE_OUTER_BOUND ( 'NONE', #163644, .T. ) ;
#100818 = DIRECTION ( 'NONE',  ( -1.000000000000000000, 0.000000000000000000, 0.000000000000000000 ) ) ;
#100819 = B_SPLINE_CURVE_WITH_KNOTS ( 'NONE', 3,
 ( #123822, #241209, #61273, #101643 ),
 .UNSPECIFIED., .F., .F.,
 ( 4, 4 ),
 ( 0.000000000000000000, 0.001767853679387133359 ),
 .UNSPECIFIED. ) ;
#100820 = CARTESIAN_POINT ( 'NONE',  ( -23.15000000000000213, 52.91185528119410009, -244.1460391050142960 ) ) ;
#100821 = CIRCLE ( 'NONE', #9292, 0.09999999999999939493 ) ;
#100823 = VERTEX_POINT ( 'NONE', #215788 ) ;
#100822 = AXIS2_PLACEMENT_3D ( 'NONE', #87861, #147877, #5755 ) ;
#100824 = CIRCLE ( 'NONE', #142384, 0.1000000000000028644 ) ;
#100825 = EDGE_CURVE ( 'NONE', #57105, #211497, #37191, .T. ) ;
#100827 = VERTEX_POINT ( 'NONE', #137534 ) ;
#100826 = CYLINDRICAL_SURFACE ( 'NONE', #7424, 0.09999999999999939493 ) ;
#100828 = LINE ( 'NONE', #180420, #249138 ) ;
#100829 = CARTESIAN_POINT ( 'NONE',  ( -23.15000000000000213, 73.40000000001204228, -114.7731074845243171 ) ) ;
#100830 = EDGE_CURVE ( 'NONE', #207360, #89242, #200867, .T. ) ;
#100831 = EDGE_CURVE ( 'NONE', #203294, #41556, #99680, .T. ) ;
#100832 = DIRECTION ( 'NONE',  ( 1.000000000000000000, 0.000000000000000000, 0.000000000000000000 ) ) ;
#100833 = ORIENTED_EDGE ( 'NONE', *, *, #66719, .F. ) ;
#100834 = CARTESIAN_POINT ( 'NONE',  ( -23.39999999999994529, 79.78873604695631627, -7.297728304630792806 ) ) ;
#100835 = DIRECTION ( 'NONE',  ( 0.000000000000000000, -5.956132106358135699E-15, 1.000000000000000000 ) ) ;
#100836 = AXIS2_PLACEMENT_3D ( 'NONE', #86817, #165094, #46414 ) ;
#100837 = ORIENTED_EDGE ( 'NONE', *, *, #137316, .T. ) ;
#100838 = EDGE_CURVE ( 'NONE', #7674, #131827, #230089, .T. ) ;
#100839 = CARTESIAN_POINT ( 'NONE',  ( -18.56579813702276027, 10.33025634372637569, -206.5870929282638429 ) ) ;
#100840 = LINE ( 'NONE', #240408, #21558 ) ;
#100841 = EDGE_CURVE ( 'NONE', #223565, #175784, #138483, .T. ) ;
#100842 = DIRECTION ( 'NONE',  ( 0.000000000000000000, -0.2617529984164506107, -0.9651348961777299618 ) ) ;
#100843 = CARTESIAN_POINT ( 'NONE',  ( 21.05000000000000071, 40.73959002362250459, -238.0637172570269513 ) ) ;
#100845 = EDGE_LOOP ( 'NONE', ( #51361, #14307, #90238 ) ) ;
#100844 = DIRECTION ( 'NONE',  ( 1.000000000000000000, 0.000000000000000000, -0.000000000000000000 ) ) ;
#100846 = EDGE_CURVE ( 'NONE', #137039, #119848, #105140, .T. ) ;
#100848 = VERTEX_POINT ( 'NONE', #41049 ) ;
#100847 = DIRECTION ( 'NONE',  ( -1.020425574104004196E-15, -1.210927747993693964E-31, -1.000000000000000000 ) ) ;
#100849 = CARTESIAN_POINT ( 'NONE',  ( -18.59999999999999787, 61.95000000001265050, -198.0094124137634708 ) ) ;
#100850 = LINE ( 'NONE', #219548, #28360 ) ;
#100851 = DIRECTION ( 'NONE',  ( -1.000000000000000000, 0.000000000000000000, -0.000000000000000000 ) ) ;
#100852 = ADVANCED_FACE ( 'NONE', ( #120582 ), #159200, .T. ) ;
#100854 = DIRECTION ( 'NONE',  ( 1.000000000000000000, -0.000000000000000000, -0.000000000000000000 ) ) ;
#100853 = CARTESIAN_POINT ( 'NONE',  ( -18.50000000000000000, 85.40000000001138858, -29.10844914155459762 ) ) ;
#100855 = CARTESIAN_POINT ( 'NONE',  ( -18.59999999999999787, 7.120270961708750512, -171.1595630418393625 ) ) ;
#100856 = CARTESIAN_POINT ( 'NONE',  ( -18.40000000000000213, 51.05395640845380711, -230.6854822754303314 ) ) ;
#100857 = CARTESIAN_POINT ( 'NONE',  ( -18.53317502108577131, 10.32263460346243811, -39.06059579686719729 ) ) ;
#100858 = DIRECTION ( 'NONE',  ( 0.000000000000000000, 0.000000000000000000, -1.000000000000000000 ) ) ;
#100859 = DIRECTION ( 'NONE',  ( -0.000000000000000000, 0.9770955615653313941, 0.2128009952263603954 ) ) ;
#100860 = ADVANCED_FACE ( 'NONE', ( #21480 ), #116460, .F. ) ;
#100861 = EDGE_CURVE ( 'NONE', #156221, #138899, #225790, .T. ) ;
#100862 = ORIENTED_EDGE ( 'NONE', *, *, #39632, .T. ) ;
#100864 = AXIS2_PLACEMENT_3D ( 'NONE', #20188, #176698, #77550 ) ;
#100863 = CYLINDRICAL_SURFACE ( 'NONE', #238885, 0.09999999999999867328 ) ;
#100865 = VERTEX_POINT ( 'NONE', #25334 ) ;
#100866 = ORIENTED_EDGE ( 'NONE', *, *, #86729, .F. ) ;
#100867 = ADVANCED_FACE ( 'NONE', ( #202659 ), #106104, .T. ) ;
#100868 = CARTESIAN_POINT ( 'NONE',  ( -20.96077737575330957, 11.62390063400468776, -26.64079195710655412 ) ) ;
#100869 = CARTESIAN_POINT ( 'NONE',  ( -20.85000000000000142, -11.64999999998884483, -67.00000000000000000 ) ) ;
#100870 = ORIENTED_EDGE ( 'NONE', *, *, #78522, .T. ) ;
#100871 = EDGE_CURVE ( 'NONE', #81393, #74489, #234171, .T. ) ;
#100872 = ADVANCED_FACE ( 'NONE', ( #82677 ), #67003, .T. ) ;
#100873 = ORIENTED_EDGE ( 'NONE', *, *, #218829, .F. ) ;
#100874 = SHAPE_REPRESENTATION_RELATIONSHIP ( 'NONE' , 'NONE' ,  #88607, #225623 ) ;
#100875 = EDGE_CURVE ( 'NONE', #88008, #8033, #80207, .T. ) ;
#100876 = VECTOR ( 'NONE', #57001, 1000.000000000000000 ) ;
#100877 = ORIENTED_EDGE ( 'NONE', *, *, #92959, .T. ) ;
#100878 = LINE ( 'NONE', #81325, #41869 ) ;
#100879 = ORIENTED_EDGE ( 'NONE', *, *, #246539, .T. ) ;
#100880 = VECTOR ( 'NONE', #213941, 1000.000000000000000 ) ;
#100881 = DIRECTION ( 'NONE',  ( 0.000000000000000000, 0.000000000000000000, -1.000000000000000000 ) ) ;
#100882 = CARTESIAN_POINT ( 'NONE',  ( -20.64999999999999858, 1.925233644870972816, -46.23024353312612789 ) ) ;
#100883 = CARTESIAN_POINT ( 'NONE',  ( -16.77683809663752257, 66.05416425680765258, -82.18705650362858250 ) ) ;
#100884 = DIRECTION ( 'NONE',  ( 0.7070776581709139474, -0.7071359030027652981, -2.453168425935592377E-14 ) ) ;
#100885 = DIRECTION ( 'NONE',  ( 1.000000000000000000, 0.000000000000000000, 0.000000000000000000 ) ) ;
#100886 = CIRCLE ( 'NONE', #142608, 0.09999999999999939493 ) ;
#100887 = CARTESIAN_POINT ( 'NONE',  ( 23.24999999999997513, 64.35000000001176090, -76.53791325517833855 ) ) ;
#100888 = DIRECTION ( 'NONE',  ( 0.000000000000000000, 0.000000000000000000, 1.000000000000000000 ) ) ;
#100890 = ORIENTED_EDGE ( 'NONE', *, *, #246282, .T. ) ;
#100889 = DIRECTION ( 'NONE',  ( -2.578261006436900068E-14, 0.1350103645451904977, -0.9908441862701597991 ) ) ;
#100892 = LINE ( 'NONE', #142614, #46063 ) ;
#100891 = CARTESIAN_POINT ( 'NONE',  ( 20.95052659398289308, 65.52017563223169816, -61.94786872865878991 ) ) ;
#100893 = ADVANCED_FACE ( 'NONE', ( #126981 ), #101035, .F. ) ;
#100894 = DIRECTION ( 'NONE',  ( 1.000000000000000000, 3.265361837132813093E-16, -0.000000000000000000 ) ) ;
#100895 = ORIENTED_EDGE ( 'NONE', *, *, #257353, .T. ) ;
#100896 = CARTESIAN_POINT ( 'NONE',  ( -18.49499033040907037, 9.017344637215625625, -245.4513013645828039 ) ) ;
#100897 =( NAMED_UNIT ( * ) SI_UNIT ( $, .STERADIAN. ) SOLID_ANGLE_UNIT ( ) );
#100898 = ORIENTED_EDGE ( 'NONE', *, *, #194184, .F. ) ;
#100899 = CIRCLE ( 'NONE', #59388, 0.1000000000000032113 ) ;
#100902 = DIRECTION ( 'NONE',  ( -0.000000000000000000, 0.1350103645451945777, -0.9908441862701590219 ) ) ;
#100901 = CIRCLE ( 'NONE', #80060, 0.5000000000000004441 ) ;
#100900 = CARTESIAN_POINT ( 'NONE',  ( 23.24999999999999289, 64.35000000001176090, -76.53791325517833855 ) ) ;
#100903 = DIRECTION ( 'NONE',  ( 0.000000000000000000, 0.000000000000000000, -1.000000000000000000 ) ) ;
#100904 = ORIENTED_EDGE ( 'NONE', *, *, #63167, .T. ) ;
#100905 = FILL_AREA_STYLE ('',( #64403 ) ) ;
#100906 = DIRECTION ( 'NONE',  ( 0.000000000000000000, 0.000000000000000000, -1.000000000000000000 ) ) ;
#100907 = VECTOR ( 'NONE', #22198, 1000.000000000000227 ) ;
#100908 = CARTESIAN_POINT ( 'NONE',  ( -22.50047199487802629, 0.04490605193094060477, -21.74995258108075902 ) ) ;
#100909 = DIRECTION ( 'NONE',  ( 1.000000000000000000, -2.849773892568378313E-16, 7.728835255496647986E-17 ) ) ;
#100910 = EDGE_LOOP ( 'NONE', ( #98418, #169335, #236560, #9134 ) ) ;
#100911 = CIRCLE ( 'NONE', #155177, 0.2000000000000057288 ) ;
#100912 = AXIS2_PLACEMENT_3D ( 'NONE', #144931, #224476, #66704 ) ;
#100913 = AXIS2_PLACEMENT_3D ( 'NONE', #78086, #57227, #117233 ) ;
#100914 = CARTESIAN_POINT ( 'NONE',  ( -16.92209698673619300, 66.05000000001255955, -182.7337430515784433 ) ) ;
#100915 = EDGE_CURVE ( 'NONE', #180985, #200249, #225960, .T. ) ;
#100916 = CARTESIAN_POINT ( 'NONE',  ( 20.94999999999999574, 74.16465844978715438, -57.96795619196135618 ) ) ;
#100917 = CARTESIAN_POINT ( 'NONE',  ( 18.60000000000000142, 85.32100840337338354, -129.2871692354463278 ) ) ;
#100918 = DIRECTION ( 'NONE',  ( -2.557131231893036985E-16, 0.8660254037844384856, -0.5000000000000002220 ) ) ;
#100919 = EDGE_CURVE ( 'NONE', #6405, #188719, #143963, .T. ) ;
#100920 = CARTESIAN_POINT ( 'NONE',  ( -18.41353343127310893, 85.50000000001232081, -162.9910380878245917 ) ) ;
#100921 = ORIENTED_EDGE ( 'NONE', *, *, #39399, .T. ) ;
#100922 = DIRECTION ( 'NONE',  ( 1.000000000000000000, -0.000000000000000000, 0.000000000000000000 ) ) ;
#100923 = LINE ( 'NONE', #16327, #50327 ) ;
#100924 = CARTESIAN_POINT ( 'NONE',  ( 20.94999999999999574, -11.39257802169451672, -36.57394957983193251 ) ) ;
#100925 = CARTESIAN_POINT ( 'NONE',  ( 21.05000000000000071, 10.48459288120550070, -174.9567135705834460 ) ) ;
#100927 = ORIENTED_EDGE ( 'NONE', *, *, #10195, .F. ) ;
#100926 = PLANE ( 'NONE',  #156677 ) ;
#100928 = PLANE ( 'NONE',  #117360 ) ;
#100929 = DIRECTION ( 'NONE',  ( 0.000000000000000000, -1.000000000000000000, -0.000000000000000000 ) ) ;
#100930 = CARTESIAN_POINT ( 'NONE',  ( 23.14999999999999503, 11.65000000001116298, -155.3500000000000227 ) ) ;
#100931 = ORIENTED_EDGE ( 'NONE', *, *, #35526, .F. ) ;
#100932 = CARTESIAN_POINT ( 'NONE',  ( 23.14999999999999503, 16.02417409648693436, -219.3605785455116006 ) ) ;
#100933 = DIRECTION ( 'NONE',  ( 0.000000000000000000, 1.000000000000000000, 0.000000000000000000 ) ) ;
#100934 = DIRECTION ( 'NONE',  ( -1.000000000000000000, 0.000000000000000000, 0.000000000000000000 ) ) ;
#100935 = EDGE_CURVE ( 'NONE', #250992, #173183, #176138, .T. ) ;
#100936 = AXIS2_PLACEMENT_3D ( 'NONE', #235127, #133455, #110032 ) ;
#100937 = CARTESIAN_POINT ( 'NONE',  ( 20.94999999999999929, 10.38178547073510316, -106.0078453638842149 ) ) ;
#100938 = VECTOR ( 'NONE', #121126, 1000.000000000000000 ) ;
#100939 = CARTESIAN_POINT ( 'NONE',  ( -11.59999999999994458, 64.35000000001120668, -21.02310748452479316 ) ) ;
#100940 = ORIENTED_EDGE ( 'NONE', *, *, #10747, .F. ) ;
#100941 = VERTEX_POINT ( 'NONE', #170009 ) ;
#100942 = CARTESIAN_POINT ( 'NONE',  ( 21.76363531954645936, 60.43693072858058457, -234.1150195010416724 ) ) ;
#100943 = CARTESIAN_POINT ( 'NONE',  ( -21.07946286933444213, 34.00139816787577018, -243.8065871723481735 ) ) ;
#100944 = CIRCLE ( 'NONE', #188477, 4.049999999999998046 ) ;
#100945 = CARTESIAN_POINT ( 'NONE',  ( -23.25000000000000000, 70.22659352830977753, -197.9852579278363578 ) ) ;
#100946 = DIRECTION ( 'NONE',  ( 0.000000000000000000, -7.147358527629766941E-15, 1.000000000000000000 ) ) ;
#100947 = VERTEX_POINT ( 'NONE', #72161 ) ;
#100948 = CARTESIAN_POINT ( 'NONE',  ( 20.95265033839679347, 10.51225083247831371, -175.0657637560299236 ) ) ;
#100949 = CIRCLE ( 'NONE', #167670, 11.74999999999999645 ) ;
#100950 = CARTESIAN_POINT ( 'NONE',  ( 21.05000000000000071, 76.10000000001268461, -203.5231074845243597 ) ) ;
#100951 = CONICAL_SURFACE ( 'NONE', #92622, 4.049999999999996270, 0.7853981633974604915 ) ;
#100952 = DIRECTION ( 'NONE',  ( 0.000000000000000000, 0.2617529984165023471, 0.9651348961777159730 ) ) ;
#100953 = AXIS2_PLACEMENT_3D ( 'NONE', #192890, #53371, #174657 ) ;
#100954 = CIRCLE ( 'NONE', #184389, 0.1000000000000128147 ) ;
#100955 = CARTESIAN_POINT ( 'NONE',  ( 20.95462737510932882, 10.55678195165489441, -108.0699500565623339 ) ) ;
#100956 = CYLINDRICAL_SURFACE ( 'NONE', #223703, 0.09999999999999939493 ) ;
#100957 = AXIS2_PLACEMENT_3D ( 'NONE', #8632, #206824, #28224 ) ;
#100958 = VERTEX_POINT ( 'NONE', #111277 ) ;
#100960 = ORIENTED_EDGE ( 'NONE', *, *, #39020, .T. ) ;
#100959 = CARTESIAN_POINT ( 'NONE',  ( 21.05000000000000071, 4.184122562697137226, -245.3714803909117279 ) ) ;
#100961 = CIRCLE ( 'NONE', #21920, 0.09999999999999939493 ) ;
#100962 = VERTEX_POINT ( 'NONE', #70893 ) ;
#100963 = CARTESIAN_POINT ( 'NONE',  ( -23.25000000000000000, 4.313202326203128933, -245.5540684919841681 ) ) ;
#100964 = ORIENTED_EDGE ( 'NONE', *, *, #153591, .T. ) ;
#100965 = CARTESIAN_POINT ( 'NONE',  ( 18.59999999999997655, -1.164121893230052995, -208.9148480855715775 ) ) ;
#100966 = FACE_OUTER_BOUND ( 'NONE', #91595, .T. ) ;
#100967 = LINE ( 'NONE', #240536, #203911 ) ;
#100968 = ORIENTED_EDGE ( 'NONE', *, *, #148429, .T. ) ;
#100969 = LINE ( 'NONE', #24083, #144709 ) ;
#100970 = CYLINDRICAL_SURFACE ( 'NONE', #163628, 0.09999999999999939493 ) ;
#100971 = AXIS2_PLACEMENT_3D ( 'NONE', #178241, #199062, #257684 ) ;
#100972 = EDGE_CURVE ( 'NONE', #185172, #248947, #255158, .T. ) ;
#100973 = VERTEX_POINT ( 'NONE', #108704 ) ;
#100974 = CARTESIAN_POINT ( 'NONE',  ( -15.66061380678752180, 9.360723793997191677, -151.3139271946067481 ) ) ;
#100975 = CIRCLE ( 'NONE', #234288, 4.000000000000000000 ) ;
#100977 = VERTEX_POINT ( 'NONE', #186985 ) ;
#100976 = CARTESIAN_POINT ( 'NONE',  ( -18.69999999999999929, 0.000000000000000000, 0.000000000000000000 ) ) ;
#100979 = EDGE_CURVE ( 'NONE', #152772, #140846, #30386, .T. ) ;
#100978 = LINE ( 'NONE', #256181, #131573 ) ;
#100980 = CIRCLE ( 'NONE', #55204, 0.1000000000000096922 ) ;
#100981 = ORIENTED_EDGE ( 'NONE', *, *, #65270, .F. ) ;
#100982 = AXIS2_PLACEMENT_3D ( 'NONE', #75988, #113822, #252052 ) ;
#100983 = CARTESIAN_POINT ( 'NONE',  ( 23.14999999999998437, 87.75000000001213607, -136.5231074845242176 ) ) ;
#100985 = ADVANCED_FACE ( 'NONE', ( #87826 ), #167416, .F. ) ;
#100984 = CARTESIAN_POINT ( 'NONE',  ( -18.40000000000000213, 11.48667500175767131, -24.25000000000000000 ) ) ;
#100986 = DIRECTION ( 'NONE',  ( 0.000000000000000000, 2.664535259100343354E-15, -1.000000000000000000 ) ) ;
#100987 = ORIENTED_EDGE ( 'NONE', *, *, #175817, .T. ) ;
#100988 = CARTESIAN_POINT ( 'NONE',  ( -23.25000000000000000, -11.64999999998884483, -97.40000000000004832 ) ) ;
#100989 = AXIS2_PLACEMENT_3D ( 'NONE', #2073, #161174, #240708 ) ;
#100991 = ADVANCED_FACE ( 'NONE', ( #252061 ), #250775, .T. ) ;
#100990 = CARTESIAN_POINT ( 'NONE',  ( 22.60000000000000142, 1.115600667400684642E-11, -134.0000000000000000 ) ) ;
#100992 = DIRECTION ( 'NONE',  ( 0.000000000000000000, -0.000000000000000000, 1.000000000000000000 ) ) ;
#100993 = EDGE_CURVE ( 'NONE', #40059, #35313, #196947, .T. ) ;
#100994 = ORIENTED_EDGE ( 'NONE', *, *, #127667, .T. ) ;
#100995 = EDGE_CURVE ( 'NONE', #140961, #118915, #76141, .T. ) ;
#100996 = TOROIDAL_SURFACE ( 'NONE', #221655, 4.099999999999999645, 0.1000000000000000056 ) ;
#100997 = VECTOR ( 'NONE', #5111, 1000.000000000000000 ) ;
#100998 = AXIS2_PLACEMENT_3D ( 'NONE', #76557, #137800, #59530 ) ;
#100999 = VERTEX_POINT ( 'NONE', #188241 ) ;
#101000 = ORIENTED_EDGE ( 'NONE', *, *, #126415, .T. ) ;
#101001 = CARTESIAN_POINT ( 'NONE',  ( -22.57320508075687115, 11.65000000001115588, -33.50000000000002842 ) ) ;
#101003 = ADVANCED_FACE ( 'NONE', ( #12198 ), #132123, .T. ) ;
#101002 = CARTESIAN_POINT ( 'NONE',  ( 21.06086055315970285, 8.774707514967413857, -45.70232215515390806 ) ) ;
#101005 = ORIENTED_EDGE ( 'NONE', *, *, #24452, .F. ) ;
#101004 = CARTESIAN_POINT ( 'NONE',  ( 12.29592348164039528, 25.90710817316709580, -233.1781447626814838 ) ) ;
#101006 = CARTESIAN_POINT ( 'NONE',  ( 21.05000000000000071, 11.60000000001116049, -127.0717967697245427 ) ) ;
#101007 = DIRECTION ( 'NONE',  ( 0.000000000000000000, 0.000000000000000000, 1.000000000000000000 ) ) ;
#101008 = CARTESIAN_POINT ( 'NONE',  ( 21.05000000000000071, 85.00000000001222134, -145.9170766071767389 ) ) ;
#101009 = CARTESIAN_POINT ( 'NONE',  ( -20.94999999999999929, 1.115600667400684642E-11, -67.00000000000000000 ) ) ;
#101010 = CARTESIAN_POINT ( 'NONE',  ( -20.99142135623731065, 64.40000000001249703, -176.9513107147999449 ) ) ;
#101011 = CYLINDRICAL_SURFACE ( 'NONE', #238803, 0.1000000000000035305 ) ;
#101013 = ORIENTED_EDGE ( 'NONE', *, *, #230473, .F. ) ;
#101012 = CARTESIAN_POINT ( 'NONE',  ( 23.14999999999998437, 87.75000000001165290, -69.52310748452424605 ) ) ;
#101015 = ORIENTED_EDGE ( 'NONE', *, *, #140603, .T. ) ;
#101014 = CARTESIAN_POINT ( 'NONE',  ( -27.30103769104855971, 12.19999999999999574, -347.0000000000001137 ) ) ;
#101016 = DIRECTION ( 'NONE',  ( -1.000000000000000000, 3.265361837132813093E-16, 2.280189983783949500E-30 ) ) ;
#101017 = VERTEX_POINT ( 'NONE', #33071 ) ;
#101018 = ORIENTED_EDGE ( 'NONE', *, *, #196211, .F. ) ;
#101019 = DIRECTION ( 'NONE',  ( 1.645090726704136556E-14, -0.1618390714546045217, -0.9868171638914230437 ) ) ;
#101020 = AXIS2_PLACEMENT_3D ( 'NONE', #125901, #142880, #122069 ) ;
#101021 = CARTESIAN_POINT ( 'NONE',  ( -21.52071067811865746, 7.779289321892505882, -88.25000000000005684 ) ) ;
#101022 = LINE ( 'NONE', #180619, #117604 ) ;
#101023 = VECTOR ( 'NONE', #110947, 1000.000000000000227 ) ;
#101024 = DIRECTION ( 'NONE',  ( 1.000000000000000000, 0.000000000000000000, 0.000000000000000000 ) ) ;
#101025 = DIRECTION ( 'NONE',  ( -0.000000000000000000, 0.4791956752371485107, 0.8777080977375185666 ) ) ;
#101026 = CARTESIAN_POINT ( 'NONE',  ( -21.05000000000000071, 87.75000000001143974, -39.12310748452424747 ) ) ;
#101027 = DIRECTION ( 'NONE',  ( 1.000000000000000000, 0.000000000000000000, 0.000000000000000000 ) ) ;
#101028 = VERTEX_POINT ( 'NONE', #91710 ) ;
#101029 = ORIENTED_EDGE ( 'NONE', *, *, #229601, .T. ) ;
#101030 = EDGE_LOOP ( 'NONE', ( #139572, #240893, #78678, #49544 ) ) ;
#101031 = CARTESIAN_POINT ( 'NONE',  ( -20.85000000000000142, 77.16412189325360771, -162.1082593989527254 ) ) ;
#101032 = DIRECTION ( 'NONE',  ( 0.000000000000000000, 1.000000000000000000, 0.000000000000000000 ) ) ;
#101034 = EDGE_CURVE ( 'NONE', #136073, #97044, #167761, .T. ) ;
#101033 = FACE_OUTER_BOUND ( 'NONE', #31900, .T. ) ;
#101035 = TOROIDAL_SURFACE ( 'NONE', #96957, 0.2000000000000000111, 0.1000000000000000056 ) ;
#101036 = CARTESIAN_POINT ( 'NONE',  ( -21.93340585899711215, -1.558585775479259139, -193.8436084524387297 ) ) ;
#101037 = VERTEX_POINT ( 'NONE', #153004 ) ;
#101038 = CARTESIAN_POINT ( 'NONE',  ( -16.93521499325732194, 66.00521388020870006, -149.1159989434308955 ) ) ;
#101039 = ORIENTED_EDGE ( 'NONE', *, *, #88488, .F. ) ;
#101041 = ADVANCED_FACE ( 'NONE', ( #246916 ), #130304, .F. ) ;
#101040 = LINE ( 'NONE', #41154, #8891 ) ;
#101042 = ORIENTED_EDGE ( 'NONE', *, *, #83445, .T. ) ;
#101043 = CARTESIAN_POINT ( 'NONE',  ( 23.24999999999999645, 67.17743825834520521, -60.27310748452438816 ) ) ;
#101044 = EDGE_CURVE ( 'NONE', #160000, #50839, #229935, .T. ) ;
#101045 = CARTESIAN_POINT ( 'NONE',  ( 13.76927104934457802, 9.455987233623901034, -182.5115311668978393 ) ) ;
#101046 = EDGE_CURVE ( 'NONE', #101652, #40848, #13616, .T. ) ;
#101047 = ORIENTED_EDGE ( 'NONE', *, *, #183769, .F. ) ;
#101049 = FACE_OUTER_BOUND ( 'NONE', #141137, .T. ) ;
#101048 = AXIS2_PLACEMENT_3D ( 'NONE', #138784, #39761, #179269 ) ;
#101051 = VERTEX_POINT ( 'NONE', #92986 ) ;
#101050 = LINE ( 'NONE', #202774, #55588 ) ;
#101052 = CARTESIAN_POINT ( 'NONE',  ( -16.87683809663752399, 61.23280479334025017, -220.3417702668379832 ) ) ;
#101053 = ORIENTED_EDGE ( 'NONE', *, *, #257021, .F. ) ;
#101054 = AXIS2_PLACEMENT_3D ( 'NONE', #38858, #115818, #37577 ) ;
#101055 = CIRCLE ( 'NONE', #30403, 0.09999999999999913125 ) ;
#101057 = DIRECTION ( 'NONE',  ( 0.000000000000000000, -1.000000000000000000, -6.789366196018718420E-15 ) ) ;
#101056 =( BOUNDED_CURVE ( )  B_SPLINE_CURVE ( 3, ( #182871, #238979, #159445, #81156 ),
 .UNSPECIFIED., .F., .F. ) 
 B_SPLINE_CURVE_WITH_KNOTS ( ( 4, 4 ),
 ( 0.3000847527772381729, 0.5497968875596822569 ),
 .UNSPECIFIED. ) 
 CURVE ( )  GEOMETRIC_REPRESENTATION_ITEM ( )  RATIONAL_B_SPLINE_CURVE ( ( 1.000000000000000000, 0.9948104011409419911, 0.9948104011409419911, 1.000000000000000000 ) ) 
 REPRESENTATION_ITEM ( '' )  );
#101058 = ORIENTED_EDGE ( 'NONE', *, *, #105269, .T. ) ;
#101059 = ADVANCED_FACE ( 'NONE', ( #69595 ), #217782, .T. ) ;
#101060 = DIRECTION ( 'NONE',  ( 0.000000000000000000, 0.000000000000000000, -1.000000000000000000 ) ) ;
#101061 = DIRECTION ( 'NONE',  ( 1.000000000000000000, 0.000000000000000000, 0.000000000000000000 ) ) ;
#101062 = DIRECTION ( 'NONE',  ( -1.000000000000000000, 0.000000000000000000, -0.000000000000000000 ) ) ;
#101063 = CARTESIAN_POINT ( 'NONE',  ( -20.94999999999999929, 87.65000000001266756, -200.5231074845242745 ) ) ;
#101064 = EDGE_CURVE ( 'NONE', #53620, #199698, #201054, .T. ) ;
#101065 = CARTESIAN_POINT ( 'NONE',  ( -20.64999999999999858, 25.94586868676353575, -241.5435999122864530 ) ) ;
#101066 = AXIS2_PLACEMENT_3D ( 'NONE', #91267, #125565, #245527 ) ;
#101067 = ORIENTED_EDGE ( 'NONE', *, *, #74707, .F. ) ;
#101068 = CIRCLE ( 'NONE', #205166, 0.2000000000000057288 ) ;
#101069 = LINE ( 'NONE', #45005, #256712 ) ;
#101070 = CYLINDRICAL_SURFACE ( 'NONE', #82811, 0.09999999999999939493 ) ;
#101071 = CARTESIAN_POINT ( 'NONE',  ( 22.24259225415828567, 0.5715038522256311593, -230.1077355066391306 ) ) ;
#101072 = ORIENTED_EDGE ( 'NONE', *, *, #208362, .T. ) ;
#101073 = DIRECTION ( 'NONE',  ( -1.000000000000000000, 7.709882115452463178E-15, -3.083952846180985271E-14 ) ) ;
#101074 = ORIENTED_EDGE ( 'NONE', *, *, #185387, .T. ) ;
#101075 = DIRECTION ( 'NONE',  ( 1.000000000000000000, 0.000000000000000000, 0.000000000000000000 ) ) ;
#101076 = ORIENTED_EDGE ( 'NONE', *, *, #184894, .F. ) ;
#101077 = CARTESIAN_POINT ( 'NONE',  ( 21.05000000000000071, 47.95459712139159336, -246.5019368548292675 ) ) ;
#101078 = CARTESIAN_POINT ( 'NONE',  ( -23.25000000000000000, 76.00000000001165290, -69.52310748452431710 ) ) ;
#101079 = EDGE_CURVE ( 'NONE', #120967, #141295, #109453, .T. ) ;
#101081 = ORIENTED_EDGE ( 'NONE', *, *, #79899, .T. ) ;
#101080 = AXIS2_PLACEMENT_3D ( 'NONE', #184916, #148363, #85778 ) ;
#101083 = ORIENTED_EDGE ( 'NONE', *, *, #94548, .T. ) ;
#101082 = DIRECTION ( 'NONE',  ( 0.000000000000000000, 0.000000000000000000, 1.000000000000000000 ) ) ;
#101084 = ADVANCED_FACE ( 'NONE', ( #113833 ), #96806, .F. ) ;
#101085 = DIRECTION ( 'NONE',  ( 0.000000000000000000, 0.000000000000000000, -1.000000000000000000 ) ) ;
#101086 = ORIENTED_EDGE ( 'NONE', *, *, #246036, .F. ) ;
#101087 = EDGE_CURVE ( 'NONE', #196849, #199913, #38636, .T. ) ;
#101088 = CARTESIAN_POINT ( 'NONE',  ( -23.15000000000000213, 11.75000000001115552, -179.7499999999999716 ) ) ;
#101089 = AXIS2_PLACEMENT_3D ( 'NONE', #197685, #19059, #257609 ) ;
#101090 = TOROIDAL_SURFACE ( 'NONE', #92945, 0.2000000000000000111, 0.1000000000000000056 ) ;
#101091 = VECTOR ( 'NONE', #211039, 1000.000000000000000 ) ;
#101092 = CYLINDRICAL_SURFACE ( 'NONE', #35400, 0.09999999999999950595 ) ;
#101093 = ORIENTED_EDGE ( 'NONE', *, *, #158665, .T. ) ;
#101094 = AXIS2_PLACEMENT_3D ( 'NONE', #109199, #191352, #70119 ) ;
#101095 = EDGE_LOOP ( 'NONE', ( #233493, #190979, #177966 ) ) ;
#101096 = FACE_OUTER_BOUND ( 'NONE', #122091, .T. ) ;
#101097 = DIRECTION ( 'NONE',  ( 0.000000000000000000, 0.000000000000000000, 1.000000000000000000 ) ) ;
#101098 = ORIENTED_EDGE ( 'NONE', *, *, #398, .F. ) ;
#101099 = VERTEX_POINT ( 'NONE', #194696 ) ;
#101100 = DIRECTION ( 'NONE',  ( 0.000000000000000000, 0.000000000000000000, -1.000000000000000000 ) ) ;
#101102 = VERTEX_POINT ( 'NONE', #78552 ) ;
#101101 = CARTESIAN_POINT ( 'NONE',  ( -16.80100426158790228, 9.943150520407293413, -46.18294575283405834 ) ) ;
#101103 = CARTESIAN_POINT ( 'NONE',  ( -23.25000000000000000, 64.25000000001222134, -148.2731074845243882 ) ) ;
#101104 = DIRECTION ( 'NONE',  ( 1.000000000000000000, -0.000000000000000000, -0.000000000000000000 ) ) ;
#101106 = EDGE_CURVE ( 'NONE', #34181, #33467, #88599, .T. ) ;
#101105 = CARTESIAN_POINT ( 'NONE',  ( 18.49999999999999645, 76.00000000001190870, -103.0231074845243029 ) ) ;
#101107 = CARTESIAN_POINT ( 'NONE',  ( -16.94037747912386394, 65.98646061752553749, -90.47197652654890021 ) ) ;
#101108 = DIRECTION ( 'NONE',  ( -1.000000000000000000, -5.840638543281469327E-15, 6.917008051451466668E-14 ) ) ;
#101109 = CARTESIAN_POINT ( 'NONE',  ( 21.97500000000000497, 30.46448808713892831, -235.1722212069449256 ) ) ;
#101110 = AXIS2_PLACEMENT_3D ( 'NONE', #352, #98137, #219392 ) ;
#101111 = DIRECTION ( 'NONE',  ( 0.000000000000000000, 0.000000000000000000, 1.000000000000000000 ) ) ;
#101112 = CARTESIAN_POINT ( 'NONE',  ( 22.59999999999999432, -3.180729737797947099, -228.0957332317254895 ) ) ;
#101113 = VERTEX_POINT ( 'NONE', #178992 ) ;
#101114 = AXIS2_PLACEMENT_3D ( 'NONE', #6183, #106555, #85689 ) ;
#101115 = ORIENTED_EDGE ( 'NONE', *, *, #116570, .F. ) ;
#101116 = EDGE_CURVE ( 'NONE', #19842, #176730, #230263, .T. ) ;
#101118 = DIRECTION ( 'NONE',  ( 0.000000000000000000, -0.000000000000000000, 1.000000000000000000 ) ) ;
#101117 = CIRCLE ( 'NONE', #176216, 0.5000000000000004441 ) ;
#101119 = ORIENTED_EDGE ( 'NONE', *, *, #120735, .T. ) ;
#101120 =( BOUNDED_SURFACE ( )  B_SPLINE_SURFACE ( 3, 2, ( 
 ( #9335, #169741, #88855 ),
 ( #247945, #125450, #87576 ),
 ( #245398, #249249, #66759 ),
 ( #167171, #130563, #228406 ),
 ( #229681, #185417, #31510 ),
 ( #204955, #51002, #126724 ) ),
 .UNSPECIFIED., .F., .F., .F. ) 
 B_SPLINE_SURFACE_WITH_KNOTS ( ( 4, 2, 4 ),
 ( 3, 3 ),
 ( -1.776356839400250465E-15, 0.7853981633974468357, 1.570796326794895448 ),
 ( 0.000000000000000000, 1.000000000000000000 ),
 .UNSPECIFIED. ) 
 GEOMETRIC_REPRESENTATION_ITEM ( )  RATIONAL_B_SPLINE_SURFACE ( (
 ( 1.000000000000000000, 0.5000000000000154321, 1.000000000000000000),
 ( 1.000000000000000000, 0.4993418825333872935, 1.000000000000000000),
 ( 1.000000000000000000, 0.5278258667058143283, 1.000000000000000000),
 ( 1.000000000000000000, 0.6092287576696161500, 1.000000000000000000),
 ( 1.000000000000000000, 0.6611148371778734489, 1.000000000000000000),
 ( 1.000000000000000000, 0.7071067811865597852, 1.000000000000000000) ) ) 
 REPRESENTATION_ITEM ( '' )  SURFACE ( )  );
#101121 = CARTESIAN_POINT ( 'NONE',  ( -16.88560720703333473, 9.950564843760847822, -146.6481119208637551 ) ) ;
#101122 = VECTOR ( 'NONE', #233456, 1000.000000000000000 ) ;
#101123 = ADVANCED_FACE ( 'NONE', ( #134659 ), #158149, .T. ) ;
#101124 = ORIENTED_EDGE ( 'NONE', *, *, #6324, .F. ) ;
#101125 = CIRCLE ( 'NONE', #246926, 0.09999999999998900047 ) ;
#101127 = AXIS2_PLACEMENT_3D ( 'NONE', #209239, #127144, #129708 ) ;
#101126 =( NAMED_UNIT ( * ) SI_UNIT ( $, .STERADIAN. ) SOLID_ANGLE_UNIT ( ) );
#101129 = EDGE_CURVE ( 'NONE', #71313, #220835, #188038, .T. ) ;
#101128 = CARTESIAN_POINT ( 'NONE',  ( 20.89878130938411616, 65.67252876774553272, -130.9457041994994881 ) ) ;
#101130 = AXIS2_PLACEMENT_3D ( 'NONE', #153520, #251267, #133896 ) ;
#101132 = VERTEX_POINT ( 'NONE', #75998 ) ;
#101131 = ORIENTED_EDGE ( 'NONE', *, *, #159609, .T. ) ;
#101133 = ORIENTED_EDGE ( 'NONE', *, *, #88738, .T. ) ;
#101134 = ORIENTED_EDGE ( 'NONE', *, *, #41818, .F. ) ;
#101135 = AXIS2_PLACEMENT_3D ( 'NONE', #218453, #238028, #221029 ) ;
#101136 = EDGE_CURVE ( 'NONE', #99741, #126102, #192691, .T. ) ;
#101137 = CARTESIAN_POINT ( 'NONE',  ( -21.14999999999999858, 87.65000000001165859, -69.52310748452424605 ) ) ;
#101138 = CARTESIAN_POINT ( 'NONE',  ( -21.08198257630413508, 75.92735667622740436, -109.3597042185393775 ) ) ;
#101141 = EDGE_CURVE ( 'NONE', #7674, #158615, #1112, .T. ) ;
#101140 = EDGE_LOOP ( 'NONE', ( #15854, #211432, #243980, #78208 ) ) ;
#101139 = DIRECTION ( 'NONE',  ( 0.000000000000000000, 0.2605042016806715099, 0.9654727137038706664 ) ) ;
#101142 = CARTESIAN_POINT ( 'NONE',  ( 20.30531438145591139, 39.64564273954285767, -237.1493556402196248 ) ) ;
#101143 = CARTESIAN_POINT ( 'NONE',  ( 18.59999999999999787, -11.65000000000000036, 5.900000000000001243 ) ) ;
#101145 = VERTEX_POINT ( 'NONE', #215501 ) ;
#101144 = DIRECTION ( 'NONE',  ( 0.000000000000000000, 0.000000000000000000, -1.000000000000000000 ) ) ;
#101146 = ORIENTED_EDGE ( 'NONE', *, *, #207561, .T. ) ;
#101147 = TOROIDAL_SURFACE ( 'NONE', #188508, 0.2000000000000000111, 0.1000000000000000056 ) ;
#101149 = ORIENTED_EDGE ( 'NONE', *, *, #27430, .F. ) ;
#101148 = DIRECTION ( 'NONE',  ( 1.000000000000000000, 0.000000000000000000, 0.000000000000000000 ) ) ;
#101150 = CIRCLE ( 'NONE', #226083, 0.1000000000000028644 ) ;
#101151 = CARTESIAN_POINT ( 'NONE',  ( -23.25000000000000000, 84.59626168225477727, -78.97323500167452437 ) ) ;
#101152 = DIRECTION ( 'NONE',  ( 1.000000000000000000, 0.000000000000000000, 0.000000000000000000 ) ) ;
#101153 = DIRECTION ( 'NONE',  ( 0.000000000000000000, 0.9893560106964510714, -0.1455152366551481502 ) ) ;
#101154 = ORIENTED_EDGE ( 'NONE', *, *, #108831, .F. ) ;
#101155 = AXIS2_PLACEMENT_3D ( 'NONE', #81529, #62014, #710 ) ;
#101157 = CARTESIAN_POINT ( 'NONE',  ( 20.97438252431638972, 8.925423506087151182, -108.9723706890108446 ) ) ;
#101156 = DIRECTION ( 'NONE',  ( 2.465190328815662439E-32, -0.2617529984165030132, -0.9651348961777158619 ) ) ;
#101158 = CARTESIAN_POINT ( 'NONE',  ( 23.04999999999999716, 64.17386235947780904, -213.4227319315771183 ) ) ;
#101159 = CYLINDRICAL_SURFACE ( 'NONE', #243386, 0.09999999999999939493 ) ;
#101160 = ADVANCED_FACE ( 'NONE', ( #159398 ), #137249, .F. ) ;
#101161 = CARTESIAN_POINT ( 'NONE',  ( 21.07928932188134397, 76.00000000001213607, -136.5231074845242745 ) ) ;
#101162 = CARTESIAN_POINT ( 'NONE',  ( -18.59999999999999787, 16.52766025697963315, -240.8672687545768270 ) ) ;
#101163 = EDGE_CURVE ( 'NONE', #216037, #186212, #9510, .T. ) ;
#101165 = VERTEX_POINT ( 'NONE', #116418 ) ;
#101164 = AXIS2_PLACEMENT_3D ( 'NONE', #222674, #79313, #238408 ) ;
#101166 = ORIENTED_EDGE ( 'NONE', *, *, #204280, .F. ) ;
#101168 =( BOUNDED_CURVE ( )  B_SPLINE_CURVE ( 3, ( #61469, #241400, #62753, #142280 ),
 .UNSPECIFIED., .F., .F. ) 
 B_SPLINE_CURVE_WITH_KNOTS ( ( 4, 4 ),
 ( 3.141592653589793116, 4.712388980384689674 ),
 .UNSPECIFIED. ) 
 CURVE ( )  GEOMETRIC_REPRESENTATION_ITEM ( )  RATIONAL_B_SPLINE_CURVE ( ( 1.000000000000000000, 0.8047378541243649375, 0.8047378541243649375, 1.000000000000000000 ) ) 
 REPRESENTATION_ITEM ( '' )  );
#101167 = VECTOR ( 'NONE', #21180, 1000.000000000000000 ) ;
#101170 = VERTEX_POINT ( 'NONE', #216781 ) ;
#101169 = VECTOR ( 'NONE', #135722, 1000.000000000000000 ) ;
#101171 = CYLINDRICAL_SURFACE ( 'NONE', #13844, 0.5000000000000004441 ) ;
#101172 = CIRCLE ( 'NONE', #230397, 11.80000000000000426 ) ;
#101173 = EDGE_LOOP ( 'NONE', ( #191259, #31238, #200556, #44727 ) ) ;
#101174 = FACE_OUTER_BOUND ( 'NONE', #158375, .T. ) ;
#101175 = EDGE_LOOP ( 'NONE', ( #243499, #34829, #213936, #230347 ) ) ;
#101176 = EDGE_CURVE ( 'NONE', #49507, #168528, #4152, .T. ) ;
#101177 = CARTESIAN_POINT ( 'NONE',  ( -22.39999999999999858, 7.790779598384559357, -100.5000000000000426 ) ) ;
#101178 = CARTESIAN_POINT ( 'NONE',  ( 18.49999999999999289, 65.79142135624910281, -81.67310748452439384 ) ) ;
#101179 = ADVANCED_FACE ( 'NONE', ( #25032 ), #155301, .T. ) ;
#101180 = VERTEX_POINT ( 'NONE', #5410 ) ;
#101181 = CARTESIAN_POINT ( 'NONE',  ( 20.94999999999999929, 4.999999999999997335, -21.09473398108690390 ) ) ;
#101182 = EDGE_CURVE ( 'NONE', #111080, #91045, #62849, .T. ) ;
#101183 = CIRCLE ( 'NONE', #238612, 4.000000000000000000 ) ;
#101184 = AXIS2_PLACEMENT_3D ( 'NONE', #177087, #256534, #77943 ) ;
#101185 = EDGE_LOOP ( 'NONE', ( #82735, #169585, #236519, #171143 ) ) ;
#101186 = AXIS2_PLACEMENT_3D ( 'NONE', #160138, #59701, #24480 ) ;
#101188 = ORIENTED_EDGE ( 'NONE', *, *, #26632, .T. ) ;
#101187 = CIRCLE ( 'NONE', #42990, 0.5000000000000004441 ) ;
#101189 = ORIENTED_EDGE ( 'NONE', *, *, #126500, .F. ) ;
#101190 = ADVANCED_FACE ( 'NONE', ( #124123 ), #163249, .T. ) ;
#101191 = DIRECTION ( 'NONE',  ( -1.000000000000000000, 0.000000000000000000, -0.000000000000000000 ) ) ;
#101192 = DIRECTION ( 'NONE',  ( 0.000000000000000000, -6.982962677686266711E-15, 1.000000000000000000 ) ) ;
#101193 = DIRECTION ( 'NONE',  ( 0.9880948137434723000, -0.1538461538461484146, -1.074301950413233906E-15 ) ) ;
#101194 = CARTESIAN_POINT ( 'NONE',  ( -22.57320508075687115, 11.75000000001115552, -167.4999999999999716 ) ) ;
#101195 = DIRECTION ( 'NONE',  ( 0.000000000000000000, -6.853228547068871147E-15, 1.000000000000000000 ) ) ;
#101196 = CARTESIAN_POINT ( 'NONE',  ( 23.14999999999999858, 1.115600667400684642E-11, -167.5000000000000284 ) ) ;
#101198 = DIRECTION ( 'NONE',  ( 2.952720810173290591E-16, -0.4721928772777342354, -0.8814952561688433885 ) ) ;
#101197 = DIRECTION ( 'NONE',  ( 1.000000000000000000, -1.335000415235279464E-16, 2.979993593738922200E-16 ) ) ;
#101199 = LINE ( 'NONE', #97357, #20809 ) ;
#101201 = ORIENTED_EDGE ( 'NONE', *, *, #118024, .F. ) ;
#101200 = DIRECTION ( 'NONE',  ( 0.000000000000000000, 0.9910827722268049644, 0.1332476588733589318 ) ) ;
#101202 = CARTESIAN_POINT ( 'NONE',  ( 21.07933241753356768, 69.67135405163219275, -103.1164870749436488 ) ) ;
#101203 = CARTESIAN_POINT ( 'NONE',  ( 20.94999999999999929, -11.48912529306489994, -131.1000000000000227 ) ) ;
#101204 = EDGE_CURVE ( 'NONE', #34477, #212023, #238466, .T. ) ;
#101205 = VERTEX_POINT ( 'NONE', #64138 ) ;
#101206 = ORIENTED_EDGE ( 'NONE', *, *, #36726, .F. ) ;
#101207 = CARTESIAN_POINT ( 'NONE',  ( -16.94132844910800983, 66.00756324483117510, -48.62690572854207716 ) ) ;
#101208 = DIRECTION ( 'NONE',  ( 0.000000000000000000, -1.000000000000000000, 0.000000000000000000 ) ) ;
#101209 = DIRECTION ( 'NONE',  ( -1.000000000000000000, 0.000000000000000000, 0.000000000000000000 ) ) ;
#101210 = ORIENTED_EDGE ( 'NONE', *, *, #146126, .F. ) ;
#101211 = DIRECTION ( 'NONE',  ( 1.000000000000000000, 0.000000000000000000, 0.000000000000000000 ) ) ;
#101212 = VERTEX_POINT ( 'NONE', #220649 ) ;
#101213 = ORIENTED_EDGE ( 'NONE', *, *, #186778, .T. ) ;
#101214 = AXIS2_PLACEMENT_3D ( 'NONE', #83976, #81428, #143990 ) ;
#101215 = DIRECTION ( 'NONE',  ( -1.000000000000000000, 0.000000000000000000, 0.000000000000000000 ) ) ;
#101216 = ORIENTED_EDGE ( 'NONE', *, *, #221183, .F. ) ;
#101217 = DIRECTION ( 'NONE',  ( -0.000000000000000000, 0.1350103645451649625, -0.9908441862701631297 ) ) ;
#101218 = DIRECTION ( 'NONE',  ( 1.000000000000000000, 0.000000000000000000, 0.000000000000000000 ) ) ;
#101219 = CARTESIAN_POINT ( 'NONE',  ( -16.85939681242906119, 9.905225185936462395, -121.0399219551915166 ) ) ;
#101220 = FACE_OUTER_BOUND ( 'NONE', #14910, .T. ) ;
#101221 = ORIENTED_EDGE ( 'NONE', *, *, #17947, .T. ) ;
#101222 = DIRECTION ( 'NONE',  ( 0.000000000000000000, -5.880418562633242623E-15, 1.000000000000000000 ) ) ;
#101223 = CARTESIAN_POINT ( 'NONE',  ( -23.25000000000000000, 27.73205844876672899, -240.0613753537626565 ) ) ;
#101224 = DIRECTION ( 'NONE',  ( 0.000000000000000000, -6.467318590049456648E-15, 1.000000000000000000 ) ) ;
#101225 = VECTOR ( 'NONE', #38883, 1000.000000000000000 ) ;
#101227 = ORIENTED_EDGE ( 'NONE', *, *, #154890, .T. ) ;
#101226 = CIRCLE ( 'NONE', #151374, 0.1000000000000055844 ) ;
#101230 = EDGE_LOOP ( 'NONE', ( #68059, #131968, #119575, #79244 ) ) ;
#101229 = EDGE_CURVE ( 'NONE', #101170, #94186, #61572, .T. ) ;
#101228 = DIRECTION ( 'NONE',  ( 0.000000000000000000, 0.000000000000000000, -1.000000000000000000 ) ) ;
#101231 = DIRECTION ( 'NONE',  ( 0.000000000000000000, 0.000000000000000000, -1.000000000000000000 ) ) ;
#101232 = CARTESIAN_POINT ( 'NONE',  ( 18.50000000000000000, 78.21362219944487038, -231.2727646510690533 ) ) ;
#101233 = CARTESIAN_POINT ( 'NONE',  ( -17.01825945287482966, 60.84284427644114146, -221.0155524357444108 ) ) ;
#101234 = LINE ( 'NONE', #180836, #21517 ) ;
#101235 = CARTESIAN_POINT ( 'NONE',  ( 18.59999999999999432, 2.859758780633683273, -208.6670499591424459 ) ) ;
#101236 = CARTESIAN_POINT ( 'NONE',  ( 21.05000000000000071, 74.65091558138561822, -195.5366085209788878 ) ) ;
#101237 = VERTEX_POINT ( 'NONE', #204911 ) ;
#101238 = CARTESIAN_POINT ( 'NONE',  ( -16.94878442675511110, 63.05546222811283030, -213.0798118229344595 ) ) ;
#101239 = CARTESIAN_POINT ( 'NONE',  ( -20.64999999999999858, -9.000000000000001776, -23.60603087734756045 ) ) ;
#101240 = FACE_OUTER_BOUND ( 'NONE', #180256, .T. ) ;
#101241 = FACE_OUTER_BOUND ( 'NONE', #174234, .T. ) ;
#101242 = AXIS2_PLACEMENT_3D ( 'NONE', #51257, #175144, #112563 ) ;
#101243 = ADVANCED_FACE ( 'NONE', ( #143660 ), #181532, .T. ) ;
#101244 = DIRECTION ( 'NONE',  ( 0.000000000000000000, 0.000000000000000000, -1.000000000000000000 ) ) ;
#101246 = CARTESIAN_POINT ( 'NONE',  ( 20.12518398540832010, 66.02491127934389681, -61.52643923205447862 ) ) ;
#101245 = CIRCLE ( 'NONE', #147071, 0.2000000000000057288 ) ;
#101247 = ORIENTED_EDGE ( 'NONE', *, *, #204532, .F. ) ;
#101248 = ORIENTED_EDGE ( 'NONE', *, *, #218391, .F. ) ;
#101249 = CARTESIAN_POINT ( 'NONE',  ( 21.05000000000000071, 65.57661458509899433, -95.53105556065429482 ) ) ;
#101251 = CARTESIAN_POINT ( 'NONE',  ( 21.97500000000000497, 43.94346684630428967, -235.6041041703296344 ) ) ;
#101250 = AXIS2_PLACEMENT_3D ( 'NONE', #83128, #38926, #162725 ) ;
#101252 = CARTESIAN_POINT ( 'NONE',  ( -20.00857864376270001, 30.18117236077229038, -235.7011183606462339 ) ) ;
#101253 = DIRECTION ( 'NONE',  ( -1.000000000000000000, -0.000000000000000000, -0.000000000000000000 ) ) ;
#101254 = VERTEX_POINT ( 'NONE', #2858 ) ;
#101255 = CARTESIAN_POINT ( 'NONE',  ( -17.22361732159831149, 65.65484434140982728, -147.8938920103915962 ) ) ;
#101256 = CIRCLE ( 'NONE', #72110, 0.1999999999999987899 ) ;
#101257 = AXIS2_PLACEMENT_3D ( 'NONE', #22595, #83788, #60409 ) ;
#101258 = DIRECTION ( 'NONE',  ( 0.000000000000000000, 1.000000000000000000, 0.000000000000000000 ) ) ;
#101259 = AXIS2_PLACEMENT_3D ( 'NONE', #12221, #188262, #112590 ) ;
#101260 = DIRECTION ( 'NONE',  ( 1.000000000000000000, 0.000000000000000000, 0.000000000000000000 ) ) ;
#101261 = ORIENTED_EDGE ( 'NONE', *, *, #176747, .F. ) ;
#101262 = CARTESIAN_POINT ( 'NONE',  ( 22.39999999999999858, 59.68594599439719417, -233.9123800762197902 ) ) ;
#101263 = AXIS2_PLACEMENT_3D ( 'NONE', #13672, #228876, #233996 ) ;
#101264 = EDGE_LOOP ( 'NONE', ( #114531, #212326, #212200, #223372 ) ) ;
#101265 = SPHERICAL_SURFACE ( 'NONE', #247442, 0.1000000000000000056 ) ;
#101266 = CARTESIAN_POINT ( 'NONE',  ( 21.04999999999999716, 69.70076908992551523, -170.1215449845244052 ) ) ;
#101267 = CARTESIAN_POINT ( 'NONE',  ( -21.05000000000000071, 10.30543449102040654, -228.0143625250146329 ) ) ;
#101268 = DIRECTION ( 'NONE',  ( 0.000000000000000000, 0.000000000000000000, 1.000000000000000000 ) ) ;
#101270 = TOROIDAL_SURFACE ( 'NONE', #72123, 0.2000000000000000111, 0.1000000000000000056 ) ;
#101269 = PLANE ( 'NONE',  #111223 ) ;
#101271 = CARTESIAN_POINT ( 'NONE',  ( -23.15000000000000213, 1.115600667400684642E-11, -163.5000000000000284 ) ) ;
#101273 = CARTESIAN_POINT ( 'NONE',  ( -18.59999999999999787, 36.65892442174472876, -249.5511627012454596 ) ) ;
#101272 = CIRCLE ( 'NONE', #9557, 0.1000000000000043771 ) ;
#101274 = DIRECTION ( 'NONE',  ( 1.000000000000000000, 0.000000000000000000, 0.000000000000000000 ) ) ;
#101276 = CARTESIAN_POINT ( 'NONE',  ( -23.15000000000000213, 11.65000000001115588, -59.98519422934606382 ) ) ;
#101275 = VECTOR ( 'NONE', #228943, 1000.000000000000000 ) ;
#101277 = DIRECTION ( 'NONE',  ( 1.000000000000000000, -0.000000000000000000, -0.000000000000000000 ) ) ;
#101279 = ADVANCED_FACE ( 'NONE', ( #184076 ), #213702, .F. ) ;
#101278 = DIRECTION ( 'NONE',  ( -0.000000000000000000, 0.8814952561688430555, -0.4721928772777346239 ) ) ;
#101280 = LINE ( 'NONE', #102585, #173030 ) ;
#101281 = CARTESIAN_POINT ( 'NONE',  ( -21.05000000000000071, 69.74168394267961446, -69.58880909484646793 ) ) ;
#101282 = CARTESIAN_POINT ( 'NONE',  ( 19.75857864376268935, 11.75000000001115907, -158.8500000000000227 ) ) ;
#101283 = ORIENTED_EDGE ( 'NONE', *, *, #67135, .F. ) ;
#101284 = DIRECTION ( 'NONE',  ( 0.000000000000000000, 0.000000000000000000, 1.000000000000000000 ) ) ;
#101286 = ADVANCED_FACE ( 'NONE', ( #203644 ), #142946, .T. ) ;
#101285 = CARTESIAN_POINT ( 'NONE',  ( 23.14999999999999503, 61.54970422893870108, -212.2965875311496688 ) ) ;
#101287 = VERTEX_POINT ( 'NONE', #1577 ) ;
#101289 = EDGE_CURVE ( 'NONE', #65641, #156710, #9688, .T. ) ;
#101288 = DIRECTION ( 'NONE',  ( 0.000000000000000000, -0.4999999999999088507, 0.8660254037844913322 ) ) ;
#101290 = CARTESIAN_POINT ( 'NONE',  ( -16.91256925476568540, 9.985731158139326880, -188.4676424890052431 ) ) ;
#101291 = TOROIDAL_SURFACE ( 'NONE', #117905, 0.4000000000000009104, 0.1000000000000000056 ) ;
#101292 = ORIENTED_EDGE ( 'NONE', *, *, #195968, .F. ) ;
#101293 = CARTESIAN_POINT ( 'NONE',  ( -20.64999999999999858, 70.73902226565648732, -215.2805781460175467 ) ) ;
#101294 = SPHERICAL_SURFACE ( 'NONE', #251679, 0.1000000000000000056 ) ;
#101295 = AXIS2_PLACEMENT_3D ( 'NONE', #131711, #92568, #74345 ) ;
#101296 = EDGE_CURVE ( 'NONE', #171102, #53900, #238655, .T. ) ;
#101298 = ORIENTED_EDGE ( 'NONE', *, *, #205081, .F. ) ;
#101297 = CIRCLE ( 'NONE', #43104, 0.1000000000000028644 ) ;
#101299 = ORIENTED_EDGE ( 'NONE', *, *, #1505, .T. ) ;
#101301 = DIRECTION ( 'NONE',  ( 1.000000000000000000, 0.000000000000000000, 0.000000000000000000 ) ) ;
#101300 = AXIS2_PLACEMENT_3D ( 'NONE', #107546, #207964, #244491 ) ;
#101302 = CIRCLE ( 'NONE', #92991, 0.09999999999998898659 ) ;
#101303 = ORIENTED_EDGE ( 'NONE', *, *, #42824, .F. ) ;
#101304 = ADVANCED_FACE ( 'NONE', ( #122841 ), #201074, .T. ) ;
#101305 = DIRECTION ( 'NONE',  ( 0.000000000000000000, -0.000000000000000000, -1.000000000000000000 ) ) ;
#101306 = CARTESIAN_POINT ( 'NONE',  ( -18.40000000000000213, 62.49259387941005173, -209.4439336506227960 ) ) ;
#101308 = CIRCLE ( 'NONE', #43119, 0.5000000000000000000 ) ;
#101307 = CARTESIAN_POINT ( 'NONE',  ( 21.08376601933332495, 34.00789988715292367, -243.7895282553435550 ) ) ;
#101309 = DIRECTION ( 'NONE',  ( 0.000000000000000000, 0.000000000000000000, 1.000000000000000000 ) ) ;
#101310 = DIRECTION ( 'NONE',  ( -0.000000000000000000, -0.000000000000000000, 1.000000000000000000 ) ) ;
#101311 = DIRECTION ( 'NONE',  ( 0.000000000000000000, -0.4856429311786307768, -0.8741572761215384846 ) ) ;
#101312 = CIRCLE ( 'NONE', #213810, 0.09999999999999939493 ) ;
#101313 = DIRECTION ( 'NONE',  ( -0.000000000000000000, -1.000000000000000000, 0.000000000000000000 ) ) ;
#101315 = CARTESIAN_POINT ( 'NONE',  ( 21.53699400387813512, 1.145497594119514240, -230.5275921507054022 ) ) ;
#101314 = TOROIDAL_SURFACE ( 'NONE', #9224, 0.4000000000000017431, 0.1000000000000000056 ) ;
#101316 = VECTOR ( 'NONE', #123618, 1000.000000000000000 ) ;
#101318 = ORIENTED_EDGE ( 'NONE', *, *, #58589, .F. ) ;
#101317 = CARTESIAN_POINT ( 'NONE',  ( -18.40000000000000568, -9.499999999988851584, -40.49936209718013203 ) ) ;
#101319 = VERTEX_POINT ( 'NONE', #125399 ) ;
#101321 = CARTESIAN_POINT ( 'NONE',  ( 23.14999999999999503, 11.75000000001116263, -88.35000000000003695 ) ) ;
#101320 = DIRECTION ( 'NONE',  ( -0.000000000000000000, 1.000000000000000000, 1.734723475976807292E-15 ) ) ;
#101322 = AXIS2_PLACEMENT_3D ( 'NONE', #186843, #231113, #185544 ) ;
#101324 = ORIENTED_EDGE ( 'NONE', *, *, #95561, .T. ) ;
#101323 = CARTESIAN_POINT ( 'NONE',  ( 20.95159278453404283, 8.907896337960206523, -108.9847201851092819 ) ) ;
#101325 = ORIENTED_EDGE ( 'NONE', *, *, #221688, .T. ) ;
#101326 = CARTESIAN_POINT ( 'NONE',  ( -21.65000000000000213, 52.72272256579932304, -234.4105091754867942 ) ) ;
#101327 = DIRECTION ( 'NONE',  ( -1.000000000000000000, -1.836970198721029934E-16, 0.000000000000000000 ) ) ;
#101328 = VECTOR ( 'NONE', #109443, 1000.000000000000114 ) ;
#101329 = CARTESIAN_POINT ( 'NONE',  ( -22.50000000000000000, 0.1000000000111554016, -134.0000000000000000 ) ) ;
#101330 = PLANE ( 'NONE',  #215018 ) ;
#101331 = DIRECTION ( 'NONE',  ( 0.000000000000000000, 0.8814952561688437216, -0.4721928772777334582 ) ) ;
#101332 = CARTESIAN_POINT ( 'NONE',  ( -18.40000000000000213, 11.33174054713633261, -87.85000000000003695 ) ) ;
#101333 = ADVANCED_FACE ( 'NONE', ( #65413 ), #161976, .T. ) ;
#101334 = CARTESIAN_POINT ( 'NONE',  ( 20.85000000000000142, 80.78317333349157536, -192.9003134612049166 ) ) ;
#101335 = AXIS2_PLACEMENT_3D ( 'NONE', #129061, #74253, #148635 ) ;
#101336 = EDGE_LOOP ( 'NONE', ( #93842, #84629, #86177, #180458 ) ) ;
#101337 = ORIENTED_EDGE ( 'NONE', *, *, #130543, .T. ) ;
#101338 = DIRECTION ( 'NONE',  ( 2.952720810173289112E-16, 0.9651348961777157509, -0.2617529984165031243 ) ) ;
#101339 = ORIENTED_EDGE ( 'NONE', *, *, #94230, .F. ) ;
#101340 = CARTESIAN_POINT ( 'NONE',  ( 21.05000000000000426, 0.09843750001147442974, -27.20076908990770903 ) ) ;
#101341 = ORIENTED_EDGE ( 'NONE', *, *, #256543, .F. ) ;
#101343 = AXIS2_PLACEMENT_3D ( 'NONE', #78993, #59421, #101100 ) ;
#101342 = LINE ( 'NONE', #256569, #76530 ) ;
#101344 = CIRCLE ( 'NONE', #213839, 0.1000000000000043493 ) ;
#101345 = EDGE_CURVE ( 'NONE', #85652, #198608, #26300, .T. ) ;
#101346 = CIRCLE ( 'NONE', #247137, 0.09999999999998898659 ) ;
#101347 = DIRECTION ( 'NONE',  ( 0.7071067811865487940, -0.2890913453342118800, 0.6453109281988440582 ) ) ;
#101348 = LINE ( 'NONE', #45283, #198261 ) ;
#101349 = CARTESIAN_POINT ( 'NONE',  ( 22.57320508075688537, 11.65000000001115588, -134.0000000000000000 ) ) ;
#101350 = ORIENTED_EDGE ( 'NONE', *, *, #187712, .T. ) ;
#101352 = ADVANCED_FACE ( 'NONE', ( #103237 ), #130514, .T. ) ;
#101351 = CARTESIAN_POINT ( 'NONE',  ( -20.94999999999999929, 1.162701749938009677, -8.099999999999999645 ) ) ;
#101353 = ORIENTED_EDGE ( 'NONE', *, *, #111554, .F. ) ;
#101354 = LINE ( 'NONE', #79257, #38162 ) ;
#101355 = FACE_OUTER_BOUND ( 'NONE', #3108, .T. ) ;
#101356 = CARTESIAN_POINT ( 'NONE',  ( 21.05000000000000071, 5.500000000011153745, -112.9052660189131245 ) ) ;
#101357 = CARTESIAN_POINT ( 'NONE',  ( 18.49999999999999645, 1.115600667400684642E-11, -134.0000000000000284 ) ) ;
#101358 = EDGE_CURVE ( 'NONE', #168569, #48752, #178151, .T. ) ;
#101359 = ORIENTED_EDGE ( 'NONE', *, *, #149482, .F. ) ;
#101360 = DIRECTION ( 'NONE',  ( 0.000000000000000000, 0.2128009952263604510, -0.9770955615653315052 ) ) ;
#101361 = AXIS2_PLACEMENT_3D ( 'NONE', #250238, #233272, #190279 ) ;
#101362 = EDGE_LOOP ( 'NONE', ( #74731, #242556, #253527, #169615 ) ) ;
#101365 = ORIENTED_EDGE ( 'NONE', *, *, #177242, .T. ) ;
#101364 = DIRECTION ( 'NONE',  ( -7.304098846218132695E-16, -0.4721928772777346794, -0.8814952561688431665 ) ) ;
#101363 = FACE_OUTER_BOUND ( 'NONE', #162571, .T. ) ;
#101366 = VECTOR ( 'NONE', #209451, 1000.000000000000000 ) ;
#101367 = VECTOR ( 'NONE', #104915, 1000.000000000000000 ) ;
#101368 = CARTESIAN_POINT ( 'NONE',  ( -18.39999999999999858, 85.60000000001190301, -95.99103808782457747 ) ) ;
#101369 = AXIS2_PLACEMENT_3D ( 'NONE', #70071, #32225, #50450 ) ;
#101370 = ORIENTED_EDGE ( 'NONE', *, *, #131970, .F. ) ;
#101371 = FACE_OUTER_BOUND ( 'NONE', #180239, .T. ) ;
#101372 = ORIENTED_EDGE ( 'NONE', *, *, #117572, .T. ) ;
#101373 = DIRECTION ( 'NONE',  ( -1.000000000000000000, -0.000000000000000000, 0.000000000000000000 ) ) ;
#101375 = ADVANCED_FACE ( 'NONE', ( #48410 ), #176325, .F. ) ;
#101374 = FACE_OUTER_BOUND ( 'NONE', #1351, .T. ) ;
#101376 = DIRECTION ( 'NONE',  ( 0.000000000000000000, 0.000000000000000000, -1.000000000000000000 ) ) ;
#101378 = ORIENTED_EDGE ( 'NONE', *, *, #20813, .T. ) ;
#101377 = DIRECTION ( 'NONE',  ( 1.000000000000000000, 0.000000000000000000, 0.000000000000000000 ) ) ;
#101379 = EDGE_CURVE ( 'NONE', #214529, #147404, #13156, .T. ) ;
#101380 = EDGE_CURVE ( 'NONE', #163267, #106852, #170987, .T. ) ;
#101381 = CARTESIAN_POINT ( 'NONE',  ( -23.15000000000000213, 64.35000000001254250, -182.1731074845244507 ) ) ;
#101382 = EDGE_LOOP ( 'NONE', ( #120627, #121069, #37763, #257162 ) ) ;
#101383 = LINE ( 'NONE', #257889, #124391 ) ;
#101384 = CARTESIAN_POINT ( 'NONE',  ( 21.53699400377785622, 60.68021703623425367, -234.0784225921813686 ) ) ;
#101385 = CARTESIAN_POINT ( 'NONE',  ( -18.36527282682067863, -9.500000599987966865, -140.9221489645001668 ) ) ;
#101386 = ORIENTED_EDGE ( 'NONE', *, *, #171852, .T. ) ;
#101387 = DIRECTION ( 'NONE',  ( 1.000000000000000000, -0.000000000000000000, -0.000000000000000000 ) ) ;
#101388 = ORIENTED_EDGE ( 'NONE', *, *, #216467, .T. ) ;
#101389 = CARTESIAN_POINT ( 'NONE',  ( -18.59999999999999787, 13.59055429284667404, -238.6121134008722038 ) ) ;
#101390 = EDGE_CURVE ( 'NONE', #168114, #233652, #150113, .T. ) ;
#101391 = AXIS2_PLACEMENT_3D ( 'NONE', #147553, #131838, #49734 ) ;
#101392 = CARTESIAN_POINT ( 'NONE',  ( -21.00000000000000000, 7.973296578895943121, 1.410778198689825347 ) ) ;
#101393 = DIRECTION ( 'NONE',  ( 0.000000000000000000, -0.1350103645451876666, -0.9908441862701600211 ) ) ;
#101394 = ORIENTED_EDGE ( 'NONE', *, *, #189787, .T. ) ;
#101395 = EDGE_CURVE ( 'NONE', #134457, #214442, #88784, .T. ) ;
#101396 = DIRECTION ( 'NONE',  ( -1.000000000000000000, -0.000000000000000000, 0.000000000000000000 ) ) ;
#101397 = EDGE_CURVE ( 'NONE', #103754, #139562, #249202, .T. ) ;
#101398 = DIRECTION ( 'NONE',  ( -1.000000000000000000, 0.000000000000000000, 0.000000000000000000 ) ) ;
#101399 = CARTESIAN_POINT ( 'NONE',  ( -18.59999999999999787, 1.115600667400684642E-11, -67.00000000000000000 ) ) ;
#101400 = ORIENTED_EDGE ( 'NONE', *, *, #142811, .F. ) ;
#101401 = DIRECTION ( 'NONE',  ( 0.000000000000000000, -1.000000000000000000, 0.000000000000000000 ) ) ;
#101402 = DIRECTION ( 'NONE',  ( 0.000000000000000000, 0.9126074666063545004, 0.4088369013363783999 ) ) ;
#101403 = ORIENTED_EDGE ( 'NONE', *, *, #178631, .T. ) ;
#101405 = DIRECTION ( 'NONE',  ( 0.7071067811865474617, -0.7071067811865474617, -4.937700262164531476E-15 ) ) ;
#101404 = CIRCLE ( 'NONE', #113922, 0.09999999999999939493 ) ;
#101406 = ORIENTED_EDGE ( 'NONE', *, *, #159960, .F. ) ;
#101407 = VERTEX_POINT ( 'NONE', #251755 ) ;
#101408 = CIRCLE ( 'NONE', #168155, 1.899999999999999023 ) ;
#101409 = DIRECTION ( 'NONE',  ( 1.000000000000000000, 0.000000000000000000, 0.000000000000000000 ) ) ;
#101410 = VERTEX_POINT ( 'NONE', #230932 ) ;
#101412 = ORIENTED_EDGE ( 'NONE', *, *, #61908, .T. ) ;
#101411 = DIRECTION ( 'NONE',  ( 0.000000000000000000, 0.000000000000000000, -1.000000000000000000 ) ) ;
#101413 = EDGE_CURVE ( 'NONE', #129536, #14749, #76313, .T. ) ;
#101414 = EDGE_CURVE ( 'NONE', #161543, #36183, #222047, .T. ) ;
#101417 = VERTEX_POINT ( 'NONE', #210075 ) ;
#101416 = ORIENTED_EDGE ( 'NONE', *, *, #49365, .F. ) ;
#101415 = DIRECTION ( 'NONE',  ( -0.000000000000000000, 0.2128009952263603677, -0.9770955615653313941 ) ) ;
#101418 = FACE_OUTER_BOUND ( 'NONE', #210189, .T. ) ;
#101419 = CYLINDRICAL_SURFACE ( 'NONE', #252244, 1.749999999999999778 ) ;
#101421 = EDGE_CURVE ( 'NONE', #220753, #89546, #101226, .T. ) ;
#101420 = FACE_OUTER_BOUND ( 'NONE', #232348, .T. ) ;
#101422 = AXIS2_PLACEMENT_3D ( 'NONE', #117737, #159447, #115175 ) ;
#101424 = DIRECTION ( 'NONE',  ( 1.000000000000000000, 0.000000000000000000, 0.000000000000000000 ) ) ;
#101423 = DIRECTION ( 'NONE',  ( -1.000000000000000000, -0.000000000000000000, 0.000000000000000000 ) ) ;
#101425 = FACE_OUTER_BOUND ( 'NONE', #175572, .T. ) ;
#101426 = DIRECTION ( 'NONE',  ( 0.000000000000000000, -1.000000000000000000, -2.891205793294679805E-16 ) ) ;
#101427 = DIRECTION ( 'NONE',  ( 0.000000000000000000, 0.000000000000000000, 1.000000000000000000 ) ) ;
#101429 = DIRECTION ( 'NONE',  ( 1.000000000000000000, 0.000000000000000000, 0.000000000000000000 ) ) ;
#101428 = LINE ( 'NONE', #135457, #1014 ) ;
#101430 = ORIENTED_EDGE ( 'NONE', *, *, #59247, .F. ) ;
#101431 = ORIENTED_EDGE ( 'NONE', *, *, #17849, .F. ) ;
#101432 = AXIS2_PLACEMENT_3D ( 'NONE', #130301, #248997, #70375 ) ;
#101433 = DIRECTION ( 'NONE',  ( 0.000000000000000000, 0.000000000000000000, -1.000000000000000000 ) ) ;
#101435 = ORIENTED_EDGE ( 'NONE', *, *, #120913, .F. ) ;
#101434 = DIRECTION ( 'NONE',  ( 1.186688945009009831E-16, -1.000000000000000000, 0.000000000000000000 ) ) ;
#101436 = ORIENTED_EDGE ( 'NONE', *, *, #94931, .T. ) ;
#101437 = CARTESIAN_POINT ( 'NONE',  ( -16.77977881697927032, 12.41313456322023967, -211.2547300165144009 ) ) ;
#101438 = ORIENTED_EDGE ( 'NONE', *, *, #254699, .F. ) ;
#101439 = DIRECTION ( 'NONE',  ( -0.7071067811865301422, 0.7071067811865648922, 0.000000000000000000 ) ) ;
#101440 = AXIS2_PLACEMENT_3D ( 'NONE', #11427, #107943, #205751 ) ;
#101441 = ADVANCED_FACE ( 'NONE', ( #11890 ), #247009, .F. ) ;
#101442 = AXIS2_PLACEMENT_3D ( 'NONE', #196283, #257483, #61918 ) ;
#101443 = EDGE_LOOP ( 'NONE', ( #123316, #112660, #32283, #234580 ) ) ;
#101444 = CIRCLE ( 'NONE', #172284, 0.1000000000000028644 ) ;
#101445 = CARTESIAN_POINT ( 'NONE',  ( 20.94999999999999929, 10.72371710471867701, -188.7499999999999716 ) ) ;
#101447 = EDGE_CURVE ( 'NONE', #247446, #229414, #97135, .T. ) ;
#101446 = DIRECTION ( 'NONE',  ( 1.000000000000000000, 0.000000000000000000, 0.000000000000000000 ) ) ;
#101449 = EDGE_LOOP ( 'NONE', ( #190549, #2857, #187749, #68480 ) ) ;
#101448 = ORIENTED_EDGE ( 'NONE', *, *, #181788, .T. ) ;
#101450 = ORIENTED_EDGE ( 'NONE', *, *, #141561, .T. ) ;
#101451 = DIRECTION ( 'NONE',  ( 1.000000000000000000, 0.000000000000000000, 0.000000000000000000 ) ) ;
#101452 = ORIENTED_EDGE ( 'NONE', *, *, #75517, .F. ) ;
#101453 = VERTEX_POINT ( 'NONE', #168422 ) ;
#101454 = CARTESIAN_POINT ( 'NONE',  ( -17.04761207306817994, 12.48873323627475074, -211.2266201293557231 ) ) ;
#101457 = EDGE_CURVE ( 'NONE', #235213, #145941, #131804, .T. ) ;
#101456 = VERTEX_POINT ( 'NONE', #9291 ) ;
#101455 = CARTESIAN_POINT ( 'NONE',  ( 18.54271179734052666, -9.624084290087616012, -107.2409648527002730 ) ) ;
#101459 = CYLINDRICAL_SURFACE ( 'NONE', #48556, 0.1000000000000013933 ) ;
#101458 = CARTESIAN_POINT ( 'NONE',  ( -21.14999999999999858, 64.35000000001166143, -69.42310748452440805 ) ) ;
#101460 = DIRECTION ( 'NONE',  ( 0.000000000000000000, -1.000000000000000000, 0.000000000000000000 ) ) ;
#101461 = DIRECTION ( 'NONE',  ( 0.000000000000000000, 0.000000000000000000, 1.000000000000000000 ) ) ;
#101462 = CARTESIAN_POINT ( 'NONE',  ( 23.14999999999999858, 1.115600667400684642E-11, -200.9999999999999432 ) ) ;
#101463 = ORIENTED_EDGE ( 'NONE', *, *, #221811, .F. ) ;
#101464 = VECTOR ( 'NONE', #160370, 1000.000000000000000 ) ;
#101465 = EDGE_CURVE ( 'NONE', #116437, #121217, #107105, .T. ) ;
#101466 = VECTOR ( 'NONE', #162621, 1000.000000000000000 ) ;
#101467 = ORIENTED_EDGE ( 'NONE', *, *, #199128, .T. ) ;
#101469 = VECTOR ( 'NONE', #186314, 1000.000000000000000 ) ;
#101468 = FACE_OUTER_BOUND ( 'NONE', #71798, .T. ) ;
#101470 = DIRECTION ( 'NONE',  ( 0.000000000000000000, -0.9126074666063660468, -0.4088369013363524762 ) ) ;
#101471 = LINE ( 'NONE', #44118, #141284 ) ;
#101472 = EDGE_CURVE ( 'NONE', #205047, #83796, #16953, .T. ) ;
#101473 = VERTEX_POINT ( 'NONE', #228351 ) ;
#101474 = CARTESIAN_POINT ( 'NONE',  ( 21.13461538461538325, 10.61458296203669427, -45.74999999999999289 ) ) ;
#101475 = EDGE_CURVE ( 'NONE', #82597, #164288, #242919, .T. ) ;
#101476 = DIRECTION ( 'NONE',  ( 1.000000000000000000, -0.000000000000000000, -0.000000000000000000 ) ) ;
#101477 = CARTESIAN_POINT ( 'NONE',  ( -20.54999999999999716, 84.66355140188123585, -126.9990063664569391 ) ) ;
#101479 = EDGE_CURVE ( 'NONE', #46658, #132077, #133099, .T. ) ;
#101478 = EDGE_CURVE ( 'NONE', #229990, #85055, #43031, .T. ) ;
#101480 = ORIENTED_EDGE ( 'NONE', *, *, #171061, .T. ) ;
#101481 = EDGE_LOOP ( 'NONE', ( #27123, #255072, #207004 ) ) ;
#101482 = DIRECTION ( 'NONE',  ( 0.000000000000000000, 0.000000000000000000, -1.000000000000000000 ) ) ;
#101483 = CARTESIAN_POINT ( 'NONE',  ( 23.14999999999999147, 80.15000000001268177, -203.5231074845243313 ) ) ;
#101484 = ORIENTED_EDGE ( 'NONE', *, *, #197931, .F. ) ;
#101485 = DIRECTION ( 'NONE',  ( -1.020425574104004196E-15, 6.982962677686266711E-15, -1.000000000000000000 ) ) ;
#101486 = ORIENTED_EDGE ( 'NONE', *, *, #177704, .F. ) ;
#101487 = EDGE_CURVE ( 'NONE', #110634, #2822, #116109, .T. ) ;
#101488 = CYLINDRICAL_SURFACE ( 'NONE', #64890, 0.09999999999999939493 ) ;
#101489 = LINE ( 'NONE', #118558, #24888 ) ;
#101491 = CARTESIAN_POINT ( 'NONE',  ( -21.05000000000000071, 64.25000000001250555, -176.8647081744215370 ) ) ;
#101490 = CARTESIAN_POINT ( 'NONE',  ( -20.64999999999999858, 85.00000000001179501, -79.41707660717668205 ) ) ;
#101492 = CARTESIAN_POINT ( 'NONE',  ( 20.94999999999999929, 76.00000000001192291, -104.9231074845242944 ) ) ;
#101493 = CARTESIAN_POINT ( 'NONE',  ( -20.94999999999999929, 1.115600667400684642E-11, -67.00000000000000000 ) ) ;
#101494 = CIRCLE ( 'NONE', #5644, 0.09999999999999489853 ) ;
#101495 = VECTOR ( 'NONE', #239307, 1000.000000000000000 ) ;
#101496 = VERTEX_POINT ( 'NONE', #17013 ) ;
#101497 = CARTESIAN_POINT ( 'NONE',  ( -18.43707690579160996, 85.68240343348810484, -62.86626410711147628 ) ) ;
#101498 = AXIS2_PLACEMENT_3D ( 'NONE', #50665, #170693, #71565 ) ;
#101499 = EDGE_CURVE ( 'NONE', #125207, #24834, #197134, .T. ) ;
#101500 = EDGE_CURVE ( 'NONE', #212474, #68538, #38934, .T. ) ;
#101501 =( BOUNDED_CURVE ( )  B_SPLINE_CURVE ( 3, ( #69865, #225037, #67269, #146787 ),
 .UNSPECIFIED., .F., .T. ) 
 B_SPLINE_CURVE_WITH_KNOTS ( ( 4, 4 ),
 ( 1.570796326794892339, 3.141592653589784678 ),
 .UNSPECIFIED. ) 
 CURVE ( )  GEOMETRIC_REPRESENTATION_ITEM ( )  RATIONAL_B_SPLINE_CURVE ( ( 1.000000000000000000, 0.8047378541243659367, 0.8047378541243659367, 1.000000000000000000 ) ) 
 REPRESENTATION_ITEM ( '' )  );
#101503 = ORIENTED_EDGE ( 'NONE', *, *, #2597, .F. ) ;
#101502 = ORIENTED_EDGE ( 'NONE', *, *, #158983, .F. ) ;
#101504 = EDGE_LOOP ( 'NONE', ( #175096, #213582, #202570, #233467, #17176, #2297, #8558, #231186, #14248, #170414, #185371 ) ) ;
#101505 = ORIENTED_EDGE ( 'NONE', *, *, #152095, .F. ) ;
#101506 = AXIS2_PLACEMENT_3D ( 'NONE', #95253, #133108, #11896 ) ;
#101507 = ADVANCED_FACE ( 'NONE', ( #255551 ), #5573, .T. ) ;
#101508 = CARTESIAN_POINT ( 'NONE',  ( -20.90000000000000213, 7.886648289447972360, 1.399104650876408451 ) ) ;
#101509 = DIRECTION ( 'NONE',  ( -0.000000000000000000, 1.000000000000000000, 6.982962677686266711E-15 ) ) ;
#101510 = CIRCLE ( 'NONE', #205780, 0.1000000000000002970 ) ;
#101511 = DIRECTION ( 'NONE',  ( -0.000000000000000000, 1.000000000000000000, -0.000000000000000000 ) ) ;
#101512 = LINE ( 'NONE', #221476, #61316 ) ;
#101513 = LINE ( 'NONE', #181113, #146691 ) ;
#101515 = DIRECTION ( 'NONE',  ( 1.000000000000000000, -3.265361837132813093E-16, -2.280189983783949500E-30 ) ) ;
#101514 = CARTESIAN_POINT ( 'NONE',  ( 20.97438252431638972, 8.925423506075993885, -8.472370689010807254 ) ) ;
#101516 = EDGE_CURVE ( 'NONE', #150821, #258086, #255342, .T. ) ;
#101518 = EDGE_LOOP ( 'NONE', ( #201140, #204745, #115744, #236727 ) ) ;
#101517 = CARTESIAN_POINT ( 'NONE',  ( -20.64999999999999858, 68.75000000001158185, -57.27310748452437394 ) ) ;
#101519 = LINE ( 'NONE', #244916, #103935 ) ;
#101520 = ORIENTED_EDGE ( 'NONE', *, *, #68529, .F. ) ;
#101521 = VECTOR ( 'NONE', #244660, 1000.000000000000227 ) ;
#101522 = CARTESIAN_POINT ( 'NONE',  ( -22.59066674512245498, 11.75000000001115552, -66.96949587636947854 ) ) ;
#101523 = EDGE_CURVE ( 'NONE', #228133, #161032, #35318, .T. ) ;
#101524 = ORIENTED_EDGE ( 'NONE', *, *, #25067, .T. ) ;
#101525 = EDGE_LOOP ( 'NONE', ( #50606, #199460, #95672, #248686, #223048, #89046, #50383 ) ) ;
#101526 = CARTESIAN_POINT ( 'NONE',  ( 18.59999999999997655, 1.115600667400684642E-11, -74.90000000000000568 ) ) ;
#101527 = AXIS2_PLACEMENT_3D ( 'NONE', #148341, #209601, #190039 ) ;
#101528 = CARTESIAN_POINT ( 'NONE',  ( -20.85000000000000142, 78.57744179526842743, -232.8011145694030972 ) ) ;
#101529 = CARTESIAN_POINT ( 'NONE',  ( 20.94999999999999929, 1.115600667400684642E-11, -138.1000000000000227 ) ) ;
#101530 = AXIS2_PLACEMENT_3D ( 'NONE', #102897, #65077, #3823 ) ;
#101531 = CARTESIAN_POINT ( 'NONE',  ( 14.22821877134046353, 9.456028260519072859, -82.01119803506577455 ) ) ;
#101532 = AXIS2_PLACEMENT_3D ( 'NONE', #242004, #67219, #25543 ) ;
#101533 = AXIS2_PLACEMENT_3D ( 'NONE', #252809, #195441, #14235 ) ;
#101534 = DIRECTION ( 'NONE',  ( 0.000000000000000000, 0.9770955615652963111, 0.2128009952265221549 ) ) ;
#101535 = EDGE_LOOP ( 'NONE', ( #222283, #135377, #198912, #239340 ) ) ;
#101536 = ORIENTED_EDGE ( 'NONE', *, *, #239184, .T. ) ;
#101537 = DIRECTION ( 'NONE',  ( -1.000000000000000000, 0.000000000000000000, 0.000000000000000000 ) ) ;
#101539 = EDGE_CURVE ( 'NONE', #138653, #100083, #217967, .T. ) ;
#101538 = ORIENTED_EDGE ( 'NONE', *, *, #88863, .F. ) ;
#101540 = FACE_OUTER_BOUND ( 'NONE', #27477, .T. ) ;
#101541 = DIRECTION ( 'NONE',  ( 0.000000000000000000, -0.8814952561688430555, 0.4721928772777346239 ) ) ;
#101543 = AXIS2_PLACEMENT_3D ( 'NONE', #162894, #23389, #239847 ) ;
#101542 = DIRECTION ( 'NONE',  ( 0.000000000000000000, 0.000000000000000000, -1.000000000000000000 ) ) ;
#101544 = CARTESIAN_POINT ( 'NONE',  ( -17.11825945287482753, 66.05000000001207638, -123.8731074845243683 ) ) ;
#101545 = LINE ( 'NONE', #140704, #92436 ) ;
#101546 = FACE_OUTER_BOUND ( 'NONE', #22425, .T. ) ;
#101547 = DIRECTION ( 'NONE',  ( 1.000000000000000000, -3.265361837132813093E-16, -2.280189983783949500E-30 ) ) ;
#101548 = CARTESIAN_POINT ( 'NONE',  ( -23.25000000000000355, 10.05000000001113847, -121.2500000000000426 ) ) ;
#101550 = EDGE_CURVE ( 'NONE', #75757, #203324, #109643, .T. ) ;
#101549 = FACE_OUTER_BOUND ( 'NONE', #224639, .T. ) ;
#101551 = CIRCLE ( 'NONE', #247310, 0.1000000000000055844 ) ;
#101552 = CARTESIAN_POINT ( 'NONE',  ( -22.50014994444008209, 11.74971973190334040, -133.9169198432812777 ) ) ;
#101553 = CARTESIAN_POINT ( 'NONE',  ( -17.78241384942201364, 10.85557575279799991, -56.75096232754270886 ) ) ;
#101554 = AXIS2_PLACEMENT_3D ( 'NONE', #173039, #36064, #252514 ) ;
#101555 = AXIS2_PLACEMENT_3D ( 'NONE', #252156, #202476, #1686 ) ;
#101556 = ORIENTED_EDGE ( 'NONE', *, *, #182508, .F. ) ;
#101557 = AXIS2_PLACEMENT_3D ( 'NONE', #251072, #188544, #171581 ) ;
#101559 = EDGE_CURVE ( 'NONE', #159889, #242169, #93073, .T. ) ;
#101558 = CARTESIAN_POINT ( 'NONE',  ( -16.88593481969334320, 30.20824341629028709, -234.8074353544413100 ) ) ;
#101560 = ORIENTED_EDGE ( 'NONE', *, *, #180379, .F. ) ;
#101561 =( BOUNDED_SURFACE ( )  B_SPLINE_SURFACE ( 3, 2, ( 
 ( #86823, #162557, #184654 ),
 ( #123412, #163826, #245930 ),
 ( #144232, #64714, #122132 ),
 ( #202939, #161268, #204219 ),
 ( #141679, #24329, #62157 ),
 ( #206798, #25602, #223776 ) ),
 .UNSPECIFIED., .F., .F., .F. ) 
 B_SPLINE_SURFACE_WITH_KNOTS ( ( 4, 2, 4 ),
 ( 3, 3 ),
 ( 3.141592653589793116, 3.926990816987241395, 4.712388980384689674 ),
 ( 0.000000000000000000, 1.000000000000000000 ),
 .UNSPECIFIED. ) 
 GEOMETRIC_REPRESENTATION_ITEM ( )  RATIONAL_B_SPLINE_SURFACE ( (
 ( 1.000000000000000000, 0.9238795325112820755, 1.000000000000000000),
 ( 1.000000000000000000, 0.9240297172239192447, 1.000000000000000000),
 ( 1.000000000000000000, 0.9038128468044981378, 1.000000000000000000),
 ( 1.000000000000000000, 0.8282379607644450026, 1.000000000000000000),
 ( 1.000000000000000000, 0.7727932973495568181, 1.000000000000000000),
 ( 1.000000000000000000, 0.7071067811864494290, 1.000000000000000000) ) ) 
 REPRESENTATION_ITEM ( '' )  SURFACE ( )  );
#101562 = DIRECTION ( 'NONE',  ( 0.000000000000000000, 0.000000000000000000, -1.000000000000000000 ) ) ;
#101563 = LINE ( 'NONE', #66331, #35695 ) ;
#101564 = DIRECTION ( 'NONE',  ( -1.000000000000000000, -1.394253735153569469E-16, -2.602809386958778209E-16 ) ) ;
#101565 = EDGE_LOOP ( 'NONE', ( #69111, #33665, #127561, #251170 ) ) ;
#101566 = CARTESIAN_POINT ( 'NONE',  ( -18.79999999999999716, 5.586869315528661062, 16.41686199900910736 ) ) ;
#101567 = DIRECTION ( 'NONE',  ( -1.000000000000000000, 0.000000000000000000, 0.000000000000000000 ) ) ;
#101568 = DIRECTION ( 'NONE',  ( -0.000000000000000000, 0.000000000000000000, -1.000000000000000000 ) ) ;
#101569 = CIRCLE ( 'NONE', #89132, 0.09999999999998898659 ) ;
#101570 = EDGE_CURVE ( 'NONE', #76299, #122995, #113748, .T. ) ;
#101571 = AXIS2_PLACEMENT_3D ( 'NONE', #47799, #129913, #50363 ) ;
#101572 = CARTESIAN_POINT ( 'NONE',  ( -21.07928932188134041, 69.67148334361908724, -170.1220026301787982 ) ) ;
#101573 = LINE ( 'NONE', #187260, #103539 ) ;
#101574 = CARTESIAN_POINT ( 'NONE',  ( 18.59999999999999076, 46.45388641681647357, -243.1520440498138385 ) ) ;
#101575 = ORIENTED_EDGE ( 'NONE', *, *, #85405, .T. ) ;
#101576 = FACE_OUTER_BOUND ( 'NONE', #224502, .T. ) ;
#101578 = ORIENTED_EDGE ( 'NONE', *, *, #94623, .F. ) ;
#101577 = DIRECTION ( 'NONE',  ( -1.000000000000000000, -0.000000000000000000, -0.000000000000000000 ) ) ;
#101579 = FACE_OUTER_BOUND ( 'NONE', #174554, .T. ) ;
#101580 = FACE_OUTER_BOUND ( 'NONE', #59207, .T. ) ;
#101581 = CYLINDRICAL_SURFACE ( 'NONE', #246245, 0.09999999999999939493 ) ;
#101582 = VERTEX_POINT ( 'NONE', #135644 ) ;
#101583 = CARTESIAN_POINT ( 'NONE',  ( -22.47120815636973745, 75.97109617810833981, -148.1730394732777825 ) ) ;
#101584 = ITEM_DEFINED_TRANSFORMATION ( 'NONE', 'NONE', #131965,  #2425 ) ;
#101585 = CARTESIAN_POINT ( 'NONE',  ( 22.50000000000000000, 0.000000000000000000, 0.000000000000000000 ) ) ;
#101586 = ORIENTED_EDGE ( 'NONE', *, *, #140415, .T. ) ;
#101587 = DIRECTION ( 'NONE',  ( -1.000000000000000000, 9.012599976028471648E-15, 6.882867235861662930E-14 ) ) ;
#101588 = DIRECTION ( 'NONE',  ( 1.000000000000000000, 0.000000000000000000, -0.000000000000000000 ) ) ;
#101589 = FACE_OUTER_BOUND ( 'NONE', #7925, .T. ) ;
#101590 = ORIENTED_EDGE ( 'NONE', *, *, #208045, .T. ) ;
#101591 = ORIENTED_EDGE ( 'NONE', *, *, #169316, .T. ) ;
#101592 = FACE_OUTER_BOUND ( 'NONE', #80140, .T. ) ;
#101593 = CARTESIAN_POINT ( 'NONE',  ( -22.39999999999999858, 64.35000000001214460, -136.4231074845243938 ) ) ;
#101594 = DIRECTION ( 'NONE',  ( 0.000000000000000000, 0.5000000000000144329, 0.8660254037844302699 ) ) ;
#101595 = CARTESIAN_POINT ( 'NONE',  ( 20.85000000000000142, 87.75000000001190870, -106.0231074845242176 ) ) ;
#101596 = CYLINDRICAL_SURFACE ( 'NONE', #245341, 0.09999999999999939493 ) ;
#101597 = EDGE_CURVE ( 'NONE', #135643, #138430, #1307, .T. ) ;
#101598 = DIRECTION ( 'NONE',  ( 0.000000000000000000, 0.9126074666063844765, 0.4088369013363113980 ) ) ;
#101600 = FACE_OUTER_BOUND ( 'NONE', #218769, .T. ) ;
#101599 = DIRECTION ( 'NONE',  ( -0.000000000000000000, 0.7672646620070624479, -0.6413305999523086776 ) ) ;
#101601 = CARTESIAN_POINT ( 'NONE',  ( 20.94999027547553894, 65.70673848566926267, -30.56382523348290547 ) ) ;
#101602 = DIRECTION ( 'NONE',  ( 0.000000000000000000, 1.000000000000000000, 6.938893903907222067E-15 ) ) ;
#101603 = FACE_BOUND ( 'NONE', #108552, .T. ) ;
#101605 = LINE ( 'NONE', #121256, #101464 ) ;
#101604 = VECTOR ( 'NONE', #79609, 1000.000000000000000 ) ;
#101606 = VERTEX_POINT ( 'NONE', #213908 ) ;
#101607 = CIRCLE ( 'NONE', #60118, 0.2000000000000048683 ) ;
#101608 = EDGE_LOOP ( 'NONE', ( #55167, #242146, #220353, #226045 ) ) ;
#101609 = DIRECTION ( 'NONE',  ( 0.000000000000000000, 0.000000000000000000, -1.000000000000000000 ) ) ;
#101612 = CARTESIAN_POINT ( 'NONE',  ( 21.07964655665547227, 67.22511038503405700, -191.3011909015603749 ) ) ;
#101611 = DIRECTION ( 'NONE',  ( -1.000000000000000000, 0.000000000000000000, 0.000000000000000000 ) ) ;
#101610 = AXIS2_PLACEMENT_3D ( 'NONE', #76857, #134254, #57278 ) ;
#101613 = CIRCLE ( 'NONE', #126770, 0.1000000000000013933 ) ;
#101614 = DIRECTION ( 'NONE',  ( 1.000000000000000000, 0.000000000000000000, 0.000000000000000000 ) ) ;
#101616 = ADVANCED_FACE ( 'NONE', ( #174838 ), #147053, .T. ) ;
#101615 = CARTESIAN_POINT ( 'NONE',  ( -21.05000000000000071, 1.148907358139439339E-11, -201.0000000000015064 ) ) ;
#101617 = CARTESIAN_POINT ( 'NONE',  ( 23.25000000000000000, -11.74999999998883560, -155.7499999999999716 ) ) ;
#101618 = ORIENTED_EDGE ( 'NONE', *, *, #130095, .F. ) ;
#101619 = ORIENTED_EDGE ( 'NONE', *, *, #155840, .F. ) ;
#101620 = ADVANCED_FACE ( 'NONE', ( #53559 ), #201228, .T. ) ;
#101622 = VECTOR ( 'NONE', #135695, 1000.000000000000000 ) ;
#101621 = CARTESIAN_POINT ( 'NONE',  ( 18.39999999999999503, 8.822561741677553471, -158.2500000000000284 ) ) ;
#101623 = ORIENTED_EDGE ( 'NONE', *, *, #17888, .T. ) ;
#101624 = CARTESIAN_POINT ( 'NONE',  ( 20.95512820512820440, 67.12384868372377866, -94.46447848938342418 ) ) ;
#101625 = EDGE_CURVE ( 'NONE', #208529, #130019, #122135, .T. ) ;
#101626 = TOROIDAL_SURFACE ( 'NONE', #189154, 3.899999999999999467, 0.1000000000000000056 ) ;
#101628 = DIRECTION ( 'NONE',  ( 0.7071067811865474617, -0.7071067811865474617, -4.937700262164531476E-15 ) ) ;
#101627 = AXIS2_PLACEMENT_3D ( 'NONE', #76691, #2278, #175826 ) ;
#101629 = TOROIDAL_SURFACE ( 'NONE', #189160, 0.2000000000000000111, 0.1000000000000000056 ) ;
#101630 = EDGE_CURVE ( 'NONE', #253651, #5146, #164011, .T. ) ;
#101631 = VECTOR ( 'NONE', #215186, 1000.000000000000000 ) ;
#101632 = EDGE_CURVE ( 'NONE', #109631, #147068, #193802, .T. ) ;
#101633 = ORIENTED_EDGE ( 'NONE', *, *, #243572, .F. ) ;
#101634 = DIRECTION ( 'NONE',  ( 0.000000000000000000, -0.8814952561688437216, 0.4721928772777334582 ) ) ;
#101635 = ORIENTED_EDGE ( 'NONE', *, *, #25419, .F. ) ;
#101636 = EDGE_CURVE ( 'NONE', #70728, #82204, #226333, .T. ) ;
#101637 = CARTESIAN_POINT ( 'NONE',  ( -18.50000000000000000, 64.25000000001246292, -181.7731074845244450 ) ) ;
#101638 = DIRECTION ( 'NONE',  ( -0.000000000000000000, -1.000000000000000000, -0.000000000000000000 ) ) ;
#101639 = DIRECTION ( 'NONE',  ( 0.000000000000000000, 0.000000000000000000, 1.000000000000000000 ) ) ;
#101640 = AXIS2_PLACEMENT_3D ( 'NONE', #159930, #60790, #41277 ) ;
#101642 = CARTESIAN_POINT ( 'NONE',  ( -23.25000000000000000, 76.00000000001197975, -107.0731074845243143 ) ) ;
#101641 = AXIS2_PLACEMENT_3D ( 'NONE', #46195, #104850, #187028 ) ;
#101643 = CARTESIAN_POINT ( 'NONE',  ( -22.39999999999999858, 1.115600667400684642E-11, -92.70922040162662370 ) ) ;
#101644 = CARTESIAN_POINT ( 'NONE',  ( -16.86133551771148475, 66.05000000001255955, -182.7217640499777644 ) ) ;
#101645 = EDGE_CURVE ( 'NONE', #149929, #5997, #30755, .T. ) ;
#101646 = FACE_OUTER_BOUND ( 'NONE', #100338, .T. ) ;
#101648 = EDGE_LOOP ( 'NONE', ( #159902, #101895, #233480, #56661 ) ) ;
#101647 = DIRECTION ( 'NONE',  ( 0.000000000000000000, -2.775557561562888827E-14, 1.000000000000000000 ) ) ;
#101650 = DIRECTION ( 'NONE',  ( 0.000000000000000000, 0.8814952561688437216, -0.4721928772777334582 ) ) ;
#101649 = DIRECTION ( 'NONE',  ( -2.827886303505248766E-16, 0.8660254037844411501, 0.4999999999999956146 ) ) ;
#101651 = CIRCLE ( 'NONE', #139063, 0.1000000000000002554 ) ;
#101652 = VERTEX_POINT ( 'NONE', #241198 ) ;
#101654 = VERTEX_POINT ( 'NONE', #101624 ) ;
#101653 = LINE ( 'NONE', #78260, #44160 ) ;
#101655 = ORIENTED_EDGE ( 'NONE', *, *, #61602, .F. ) ;
#101656 = DIRECTION ( 'NONE',  ( -1.000000000000000000, 7.667232114526941871E-17, -1.711482807214921537E-16 ) ) ;
#101657 = CARTESIAN_POINT ( 'NONE',  ( 18.39999999999999503, 11.75000000001113953, -46.15000000000000568 ) ) ;
#101658 = LINE ( 'NONE', #107777, #89206 ) ;
#101659 = CIRCLE ( 'NONE', #159982, 0.09999999999998898659 ) ;
#101660 = VERTEX_POINT ( 'NONE', #20877 ) ;
#101661 = CARTESIAN_POINT ( 'NONE',  ( -20.94999999999999929, 5.850000000011105428, -144.1324972242779836 ) ) ;
#101662 = LINE ( 'NONE', #41750, #134914 ) ;
#101663 = CARTESIAN_POINT ( 'NONE',  ( 21.87500000000000355, 66.25000000001179501, -81.77310748452437394 ) ) ;
#101664 = TOROIDAL_SURFACE ( 'NONE', #51585, 0.2000000000000000111, 0.1000000000000000056 ) ;
#101665 = DIRECTION ( 'NONE',  ( 0.000000000000000000, 0.3994087351226822125, 0.9167729611565227366 ) ) ;
#101666 = CIRCLE ( 'NONE', #172485, 0.09999999999999817368 ) ;
#101668 = EDGE_CURVE ( 'NONE', #140695, #206043, #204604, .T. ) ;
#101667 = CARTESIAN_POINT ( 'NONE',  ( 22.39999999999999503, 0.1000000000111554016, -25.70922040162662014 ) ) ;
#101669 = CIRCLE ( 'NONE', #176731, 0.1000000000000054040 ) ;
#101670 = DIRECTION ( 'NONE',  ( 1.000000000000000000, -0.000000000000000000, -0.000000000000000000 ) ) ;
#101671 = ORIENTED_EDGE ( 'NONE', *, *, #170730, .F. ) ;
#101672 = VERTEX_POINT ( 'NONE', #142064 ) ;
#101673 = LINE ( 'NONE', #144671, #181146 ) ;
#101674 = ORIENTED_EDGE ( 'NONE', *, *, #191308, .T. ) ;
#101675 = CARTESIAN_POINT ( 'NONE',  ( 18.50000000000000000, -9.399999999988843058, -140.9992856778388841 ) ) ;
#101676 = ORIENTED_EDGE ( 'NONE', *, *, #145352, .T. ) ;
#101677 = CARTESIAN_POINT ( 'NONE',  ( 20.87600722750343252, 10.33112638556969465, -173.0901228926974795 ) ) ;
#101678 = EDGE_CURVE ( 'NONE', #1991, #235864, #213892, .T. ) ;
#101679 = FACE_OUTER_BOUND ( 'NONE', #140874, .T. ) ;
#101680 = CYLINDRICAL_SURFACE ( 'NONE', #43591, 11.79999999999999716 ) ;
#101681 = CARTESIAN_POINT ( 'NONE',  ( 21.05000000000000071, 76.00000000001168132, -65.52310748452430289 ) ) ;
#101682 = LINE ( 'NONE', #157893, #195512 ) ;
#101683 = ORIENTED_EDGE ( 'NONE', *, *, #180761, .T. ) ;
#101684 = DIRECTION ( 'NONE',  ( 3.265361837132813093E-16, -1.000000000000000000, -0.000000000000000000 ) ) ;
#101685 = CIRCLE ( 'NONE', #214152, 0.1000000000000035305 ) ;
#101686 = CIRCLE ( 'NONE', #180844, 0.09999999999999062417 ) ;
#101687 = CARTESIAN_POINT ( 'NONE',  ( 19.97071067811864609, 34.48027702911268477, -235.0877241633741050 ) ) ;
#101688 = FACE_OUTER_BOUND ( 'NONE', #50481, .T. ) ;
#101689 = DIRECTION ( 'NONE',  ( 0.000000000000000000, -0.9126074666063770380, -0.4088369013363281068 ) ) ;
#101690 = VERTEX_POINT ( 'NONE', #203343 ) ;
#101692 = CARTESIAN_POINT ( 'NONE',  ( -20.94999999999999929, 87.65000000001215597, -139.5231074845243029 ) ) ;
#101691 = CYLINDRICAL_SURFACE ( 'NONE', #128941, 0.09999999999999939493 ) ;
#101693 = ORIENTED_EDGE ( 'NONE', *, *, #169692, .F. ) ;
#101696 = ORIENTED_EDGE ( 'NONE', *, *, #228286, .F. ) ;
#101695 = DIRECTION ( 'NONE',  ( 5.421010862427554711E-16, 1.000000000000000000, 1.023556919514279895E-14 ) ) ;
#101694 = CARTESIAN_POINT ( 'NONE',  ( -21.05000000000000071, 1.261786168576181755, -41.58649896354548048 ) ) ;
#101697 = ADVANCED_FACE ( 'NONE', ( #22153 ), #59948, .F. ) ;
#101698 = VERTEX_POINT ( 'NONE', #84621 ) ;
#101699 = FACE_OUTER_BOUND ( 'NONE', #126801, .T. ) ;
#101700 = AXIS2_PLACEMENT_3D ( 'NONE', #210135, #227100, #151449 ) ;
#101701 = FACE_OUTER_BOUND ( 'NONE', #189113, .T. ) ;
#101702 = CARTESIAN_POINT ( 'NONE',  ( -22.50000000000000000, 11.64957080754479968, 0.09999999999999592548 ) ) ;
#101703 = AXIS2_PLACEMENT_3D ( 'NONE', #185891, #84166, #240744 ) ;
#101704 = ORIENTED_EDGE ( 'NONE', *, *, #205105, .T. ) ;
#101705 = DIRECTION ( 'NONE',  ( 0.000000000000000000, -6.467318590049456648E-15, 1.000000000000000000 ) ) ;
#101707 = ADVANCED_FACE ( 'NONE', ( #220347 ), #222886, .F. ) ;
#101706 = DIRECTION ( 'NONE',  ( 1.000000000000000000, -0.000000000000000000, -0.000000000000000000 ) ) ;
#101708 = AXIS2_PLACEMENT_3D ( 'NONE', #202667, #104816, #168737 ) ;
#101710 = CARTESIAN_POINT ( 'NONE',  ( -20.64999999999999858, 11.15983666280819975, -246.1019239270423213 ) ) ;
#101709 = DIRECTION ( 'NONE',  ( 1.000000000000000000, -1.186688945009009831E-16, -8.286604613020806758E-31 ) ) ;
#101712 = ORIENTED_EDGE ( 'NONE', *, *, #205993, .F. ) ;
#101711 = DIRECTION ( 'NONE',  ( 1.000000000000000000, 0.000000000000000000, 0.000000000000000000 ) ) ;
#101713 = CIRCLE ( 'NONE', #226632, 0.1000000000000028644 ) ;
#101714 = EDGE_CURVE ( 'NONE', #188196, #110731, #184838, .T. ) ;
#101715 = EDGE_CURVE ( 'NONE', #96043, #177157, #113925, .T. ) ;
#101716 = AXIS2_PLACEMENT_3D ( 'NONE', #93315, #216793, #98104 ) ;
#101717 = AXIS2_PLACEMENT_3D ( 'NONE', #103751, #223709, #226266 ) ;
#101718 = VERTEX_POINT ( 'NONE', #100353 ) ;
#101719 = CARTESIAN_POINT ( 'NONE',  ( 22.57856590037849287, -2.504457907796295402, -189.5199485407344753 ) ) ;
#101720 = VECTOR ( 'NONE', #41189, 1000.000000000000000 ) ;
#101721 = FACE_OUTER_BOUND ( 'NONE', #8395, .T. ) ;
#101722 = EDGE_LOOP ( 'NONE', ( #46912, #82558, #176181, #162650, #72543, #62866 ) ) ;
#101723 = CARTESIAN_POINT ( 'NONE',  ( -23.15000000000000213, -11.65000000000000036, 11.75000000000000000 ) ) ;
#101724 = ORIENTED_EDGE ( 'NONE', *, *, #54153, .T. ) ;
#101725 = EDGE_CURVE ( 'NONE', #208687, #68456, #18264, .T. ) ;
#101726 = CARTESIAN_POINT ( 'NONE',  ( -18.59999999999999787, 8.882751598337863541, -187.0399955572217721 ) ) ;
#101727 = DIRECTION ( 'NONE',  ( -0.000000000000000000, -2.891205793294679805E-16, 1.000000000000000000 ) ) ;
#101728 = CARTESIAN_POINT ( 'NONE',  ( -16.77683809663752257, 26.68086916408615750, -212.3318337774905160 ) ) ;
#101729 = CIRCLE ( 'NONE', #197419, 0.09999999999999344136 ) ;
#101730 = ORIENTED_EDGE ( 'NONE', *, *, #212501, .F. ) ;
#101731 = AXIS2_PLACEMENT_3D ( 'NONE', #119466, #193863, #256321 ) ;
#101732 = DIRECTION ( 'NONE',  ( 1.000000000000000000, -0.000000000000000000, -0.000000000000000000 ) ) ;
#101733 = AXIS2_PLACEMENT_3D ( 'NONE', #235227, #161819, #77414 ) ;
#101734 = EDGE_CURVE ( 'NONE', #40972, #22332, #82069, .T. ) ;
#101735 = VERTEX_POINT ( 'NONE', #83355 ) ;
#101736 = AXIS2_PLACEMENT_3D ( 'NONE', #189540, #50014, #209089 ) ;
#101737 = ORIENTED_EDGE ( 'NONE', *, *, #256767, .F. ) ;
#101738 = ORIENTED_EDGE ( 'NONE', *, *, #231985, .T. ) ;
#101739 = CARTESIAN_POINT ( 'NONE',  ( -20.00857864376270001, 9.350000000011156942, -112.8500000000000369 ) ) ;
#101740 = ORIENTED_EDGE ( 'NONE', *, *, #149164, .F. ) ;
#101742 = ORIENTED_EDGE ( 'NONE', *, *, #123184, .F. ) ;
#101741 = DIRECTION ( 'NONE',  ( 0.000000000000000000, -0.1455152366551721865, -0.9893560106964475187 ) ) ;
#101743 = ADVANCED_FACE ( 'NONE', ( #179936 ), #1502, .T. ) ;
#101744 = ADVANCED_FACE ( 'NONE', ( #239907 ), #118215, .T. ) ;
#101745 = ORIENTED_EDGE ( 'NONE', *, *, #34380, .T. ) ;
#101748 = ORIENTED_EDGE ( 'NONE', *, *, #208697, .T. ) ;
#101747 = VERTEX_POINT ( 'NONE', #102927 ) ;
#101746 = CARTESIAN_POINT ( 'NONE',  ( 18.60000000000001563, 78.14847862149032665, -231.3763292744987723 ) ) ;
#101749 = VERTEX_POINT ( 'NONE', #200767 ) ;
#101750 = FACE_OUTER_BOUND ( 'NONE', #222207, .T. ) ;
#101751 = AXIS2_PLACEMENT_3D ( 'NONE', #253200, #135812, #134526 ) ;
#101752 = CARTESIAN_POINT ( 'NONE',  ( 18.59999999999999787, -10.35479209691423996, -94.25654098307380480 ) ) ;
#101753 = CARTESIAN_POINT ( 'NONE',  ( 20.94999999999999929, 11.65000000001115943, -167.5000000000000284 ) ) ;
#101754 = EDGE_LOOP ( 'NONE', ( #28601, #59778, #151549 ) ) ;
#101755 = CARTESIAN_POINT ( 'NONE',  ( 20.94999999999999929, 85.00000000001197975, -112.9170766071766820 ) ) ;
#101756 = CIRCLE ( 'NONE', #147589, 0.09999999999998898659 ) ;
#101758 = ORIENTED_EDGE ( 'NONE', *, *, #191577, .F. ) ;
#101757 = LINE ( 'NONE', #237456, #240836 ) ;
#101759 = DIRECTION ( 'NONE',  ( 0.000000000000000000, 0.2280421351061330537, -0.9736512643735621975 ) ) ;
#101761 = VERTEX_POINT ( 'NONE', #182512 ) ;
#101760 = CARTESIAN_POINT ( 'NONE',  ( 18.59999999999999076, 65.79142135624982757, -178.8731074845244109 ) ) ;
#101762 = ORIENTED_EDGE ( 'NONE', *, *, #46609, .F. ) ;
#101763 = DIRECTION ( 'NONE',  ( 0.000000000000000000, 1.000000000000000000, 2.891205793294679805E-16 ) ) ;
#101765 = EDGE_CURVE ( 'NONE', #228258, #162005, #3855, .T. ) ;
#101764 = CARTESIAN_POINT ( 'NONE',  ( -23.25000000000000000, 55.39363411790988323, -234.6384634766556303 ) ) ;
#101766 = ORIENTED_EDGE ( 'NONE', *, *, #72571, .T. ) ;
#101767 = ORIENTED_EDGE ( 'NONE', *, *, #208725, .F. ) ;
#101768 = CARTESIAN_POINT ( 'NONE',  ( -16.85697194749123540, 9.908543714134728120, -180.4350042676138060 ) ) ;
#101770 = ADVANCED_FACE ( 'NONE', ( #208492 ), #159732, .T. ) ;
#101769 = CARTESIAN_POINT ( 'NONE',  ( -20.64999999999999858, 84.73084112150681335, -45.62118220350859588 ) ) ;
#101772 = ORIENTED_EDGE ( 'NONE', *, *, #39366, .T. ) ;
#101771 = VERTEX_POINT ( 'NONE', #188908 ) ;
#101773 = ORIENTED_EDGE ( 'NONE', *, *, #77842, .F. ) ;
#101774 = DIRECTION ( 'NONE',  ( 1.734723475976817507E-14, 0.000000000000000000, -1.000000000000000000 ) ) ;
#101775 = ORIENTED_EDGE ( 'NONE', *, *, #220276, .F. ) ;
#101776 = ORIENTED_EDGE ( 'NONE', *, *, #213058, .F. ) ;
#101777 = DIRECTION ( 'NONE',  ( 0.000000000000000000, 0.2617529984165031243, 0.9651348961777157509 ) ) ;
#101780 = ADVANCED_FACE ( 'NONE', ( #250169 ), #131495, .F. ) ;
#101779 = ORIENTED_EDGE ( 'NONE', *, *, #257701, .F. ) ;
#101778 = DIRECTION ( 'NONE',  ( 1.000000000000000000, 0.000000000000000000, 0.000000000000000000 ) ) ;
#101781 = CARTESIAN_POINT ( 'NONE',  ( -18.59999999999999787, 42.90983634497241894, -254.2202269430244996 ) ) ;
#101783 = CARTESIAN_POINT ( 'NONE',  ( 22.47071067811865319, 1.115600667400684642E-11, -134.0000000000000000 ) ) ;
#101782 = DIRECTION ( 'NONE',  ( -1.000000000000000000, 0.000000000000000000, 0.000000000000000000 ) ) ;
#101784 = ORIENTED_EDGE ( 'NONE', *, *, #257293, .T. ) ;
#101785 = EDGE_CURVE ( 'NONE', #81210, #236966, #139015, .T. ) ;
#101787 = ORIENTED_EDGE ( 'NONE', *, *, #10472, .T. ) ;
#101786 = EDGE_LOOP ( 'NONE', ( #121825, #173393, #234177, #80200 ) ) ;
#101788 = CARTESIAN_POINT ( 'NONE',  ( -21.05000000000000071, 75.90220970870393558, -209.7809220950004772 ) ) ;
#101789 = CARTESIAN_POINT ( 'NONE',  ( 20.85000000000000142, 36.65892442174935439, -249.5511627012433848 ) ) ;
#101790 = EDGE_CURVE ( 'NONE', #117385, #91478, #80582, .T. ) ;
#101791 = B_SPLINE_CURVE_WITH_KNOTS ( 'NONE', 3,
 ( #80286, #233005, #54326, #133874 ),
 .UNSPECIFIED., .F., .F.,
 ( 4, 4 ),
 ( 0.000000000000000000, 0.0001048066582182440823 ),
 .UNSPECIFIED. ) ;
#101792 = CIRCLE ( 'NONE', #26841, 0.09999999999999939493 ) ;
#101793 = VERTEX_POINT ( 'NONE', #151070 ) ;
#101794 = VECTOR ( 'NONE', #88847, 1000.000000000000000 ) ;
#101795 = CIRCLE ( 'NONE', #247583, 7.799999999999997158 ) ;
#101796 = CIRCLE ( 'NONE', #168515, 0.1000000000000004496 ) ;
#101797 = ADVANCED_FACE ( 'NONE', ( #110651 ), #64057, .F. ) ;
#101798 = CARTESIAN_POINT ( 'NONE',  ( -21.44999999999999929, 7.150000000011155876, -88.15000000000004832 ) ) ;
#101799 = EDGE_CURVE ( 'NONE', #233023, #94400, #148504, .T. ) ;
#101800 = EDGE_LOOP ( 'NONE', ( #169132, #55340, #151400, #151645 ) ) ;
#101801 = EDGE_LOOP ( 'NONE', ( #220431, #197176, #150664 ) ) ;
#101802 = PRESENTATION_LAYER_ASSIGNMENT (  '', '', ( #51925 ) ) ;
#101803 = LINE ( 'NONE', #138367, #229386 ) ;
#101804 = ORIENTED_EDGE ( 'NONE', *, *, #166583, .F. ) ;
#101805 = DIRECTION ( 'NONE',  ( 3.616040088954490704E-32, 7.105427357601001859E-15, -1.000000000000000000 ) ) ;
#101806 = CARTESIAN_POINT ( 'NONE',  ( 21.05000000000000071, 34.07612324756792077, -243.5412266404783566 ) ) ;
#101807 = ORIENTED_EDGE ( 'NONE', *, *, #54510, .T. ) ;
#101808 = CARTESIAN_POINT ( 'NONE',  ( 20.94999999999999929, 87.48912529308749697, -38.92310748452424463 ) ) ;
#101809 = CARTESIAN_POINT ( 'NONE',  ( 18.47149038651510367, 85.67145715801882488, -129.8503211497859127 ) ) ;
#101811 = CARTESIAN_POINT ( 'NONE',  ( -16.88783316861814399, 9.950000000011137047, -121.2477359580202716 ) ) ;
#101810 = DIRECTION ( 'NONE',  ( 0.000000000000000000, 6.308085367182471812E-16, 1.000000000000000000 ) ) ;
#101812 = DIRECTION ( 'NONE',  ( 1.000000000000000000, 0.000000000000000000, 0.000000000000000000 ) ) ;
#101813 = CARTESIAN_POINT ( 'NONE',  ( 21.11701782572532693, 65.27839088400483547, -157.7780700550132167 ) ) ;
#101814 = CYLINDRICAL_SURFACE ( 'NONE', #73983, 0.09999999999999811817 ) ;
#101815 = AXIS2_PLACEMENT_3D ( 'NONE', #170733, #205948, #145967 ) ;
#101816 = LINE ( 'NONE', #62729, #107588 ) ;
#101817 = CARTESIAN_POINT ( 'NONE',  ( 21.14999999999999858, 6.550000000000000711, -12.35000000000000320 ) ) ;
#101818 = AXIS2_PLACEMENT_3D ( 'NONE', #184906, #225288, #63667 ) ;
#101819 = ORIENTED_EDGE ( 'NONE', *, *, #181399, .T. ) ;
#101820 = EDGE_CURVE ( 'NONE', #127088, #5545, #48105, .T. ) ;
#101821 = EDGE_CURVE ( 'NONE', #159212, #109684, #147250, .T. ) ;
#101822 = VECTOR ( 'NONE', #239322, 1000.000000000000000 ) ;
#101823 = AXIS2_PLACEMENT_3D ( 'NONE', #180696, #138953, #218498 ) ;
#101825 = ORIENTED_EDGE ( 'NONE', *, *, #240373, .F. ) ;
#101824 = ORIENTED_EDGE ( 'NONE', *, *, #50686, .T. ) ;
#101826 = ORIENTED_EDGE ( 'NONE', *, *, #171915, .F. ) ;
#101828 = EDGE_LOOP ( 'NONE', ( #54299, #101824, #99428 ) ) ;
#101827 = AXIS2_PLACEMENT_3D ( 'NONE', #14448, #178664, #194539 ) ;
#101829 = CARTESIAN_POINT ( 'NONE',  ( -20.54999999999999716, 71.65000000001199965, -115.3731074845243256 ) ) ;
#101830 = DIRECTION ( 'NONE',  ( 0.000000000000000000, 0.000000000000000000, 1.000000000000000000 ) ) ;
#101832 = CARTESIAN_POINT ( 'NONE',  ( -16.95709691156916321, 9.950000000011137047, -146.6600575625134297 ) ) ;
#101831 = CARTESIAN_POINT ( 'NONE',  ( -20.85000000000000142, 77.26327546522891510, -61.62124281777789037 ) ) ;
#101833 = CARTESIAN_POINT ( 'NONE',  ( -21.10320863425827298, 75.97497774878509347, -142.9233848709835115 ) ) ;
#101834 = ORIENTED_EDGE ( 'NONE', *, *, #197806, .F. ) ;
#101835 = CIRCLE ( 'NONE', #247606, 0.09999999999998898659 ) ;
#101836 = CIRCLE ( 'NONE', #176709, 0.2000000000000057288 ) ;
#101837 = DIRECTION ( 'NONE',  ( -1.000000000000000000, 0.000000000000000000, 0.000000000000000000 ) ) ;
#101838 = TOROIDAL_SURFACE ( 'NONE', #201812, 11.65000000000000036, 0.1000000000000000056 ) ;
#101839 = EDGE_CURVE ( 'NONE', #67744, #58852, #134752, .T. ) ;
#101841 = CIRCLE ( 'NONE', #235151, 0.1000000000000028644 ) ;
#101840 = FACE_OUTER_BOUND ( 'NONE', #133879, .T. ) ;
#101842 = CARTESIAN_POINT ( 'NONE',  ( 18.59999999999999787, -1.736705739467587772, -45.01742258762372728 ) ) ;
#101843 = EDGE_CURVE ( 'NONE', #56940, #138993, #43217, .T. ) ;
#101844 = LINE ( 'NONE', #204806, #166411 ) ;
#101846 = ORIENTED_EDGE ( 'NONE', *, *, #243929, .F. ) ;
#101845 = VECTOR ( 'NONE', #68933, 1000.000000000000114 ) ;
#101847 = DIRECTION ( 'NONE',  ( 0.000000000000000000, 0.000000000000000000, -1.000000000000000000 ) ) ;
#101848 = CIRCLE ( 'NONE', #122561, 0.1000000000000089567 ) ;
#101849 = CARTESIAN_POINT ( 'NONE',  ( -21.05000000000000071, -0.08579911626291911175, -94.08602111851160998 ) ) ;
#101850 = VERTEX_POINT ( 'NONE', #51936 ) ;
#101851 = CARTESIAN_POINT ( 'NONE',  ( -16.87851181299898684, 66.04995707600383525, -56.87325099989131871 ) ) ;
#101852 = CARTESIAN_POINT ( 'NONE',  ( -18.59999999999999787, 11.65000000001115232, -141.0148057706539930 ) ) ;
#101853 = EDGE_CURVE ( 'NONE', #4064, #195562, #39133, .T. ) ;
#101854 = CARTESIAN_POINT ( 'NONE',  ( 18.59999999999999076, 61.95000000001263629, -198.0094124137634708 ) ) ;
#101855 = CARTESIAN_POINT ( 'NONE',  ( 20.94999999999999929, 5.400000000011154988, -90.60603087734760663 ) ) ;
#101856 = AXIS2_PLACEMENT_3D ( 'NONE', #14223, #175857, #35086 ) ;
#101857 = CYLINDRICAL_SURFACE ( 'NONE', #179189, 12.87499999999999822 ) ;
#101859 = ORIENTED_EDGE ( 'NONE', *, *, #3205, .T. ) ;
#101858 = CIRCLE ( 'NONE', #10123, 0.09999999999999817368 ) ;
#101860 = DIRECTION ( 'NONE',  ( -0.000000000000000000, 0.000000000000000000, 1.000000000000000000 ) ) ;
#101861 = CARTESIAN_POINT ( 'NONE',  ( -23.25000000000000000, 77.83585931145546510, -91.51866831572576189 ) ) ;
#101862 = DIRECTION ( 'NONE',  ( -0.7071067811865475727, 0.7071067811865475727, 4.937700262164531476E-15 ) ) ;
#101864 = DIRECTION ( 'NONE',  ( 0.000000000000000000, 0.8814952561688437216, -0.4721928772777331806 ) ) ;
#101863 = DIRECTION ( 'NONE',  ( 0.000000000000000000, -1.000000000000000000, -6.982962677686265922E-15 ) ) ;
#101865 = CARTESIAN_POINT ( 'NONE',  ( 21.03670563405601968, 10.62482368933940258, -45.82554688620915329 ) ) ;
#101867 = ADVANCED_FACE ( 'NONE', ( #85919 ), #93258, .T. ) ;
#101866 = DIRECTION ( 'NONE',  ( 0.000000000000000000, 0.1575844902526560010, 0.9875055080513781558 ) ) ;
#101868 = DIRECTION ( 'NONE',  ( 1.000000000000000000, 0.000000000000000000, 0.000000000000000000 ) ) ;
#101869 = CARTESIAN_POINT ( 'NONE',  ( 18.47688499308725696, -9.464855950272969665, -207.7013477531374406 ) ) ;
#101871 = ORIENTED_EDGE ( 'NONE', *, *, #97434, .F. ) ;
#101870 = DIRECTION ( 'NONE',  ( 0.000000000000000000, 2.891205793294679805E-16, -1.000000000000000000 ) ) ;
#101872 = VERTEX_POINT ( 'NONE', #11572 ) ;
#101873 = EDGE_CURVE ( 'NONE', #15176, #88490, #245028, .T. ) ;
#101874 = FACE_OUTER_BOUND ( 'NONE', #58927, .T. ) ;
#101875 = VECTOR ( 'NONE', #55794, 1000.000000000000000 ) ;
#101876 = CIRCLE ( 'NONE', #247652, 11.64999999999999325 ) ;
#101877 = CARTESIAN_POINT ( 'NONE',  ( 20.05000000000002913, 7.250000000011171508, -76.25000000000004263 ) ) ;
#101878 = AXIS2_PLACEMENT_3D ( 'NONE', #199885, #40823, #22532 ) ;
#101879 = LINE ( 'NONE', #61507, #104539 ) ;
#101880 = EDGE_LOOP ( 'NONE', ( #49840, #162052, #231792, #243496 ) ) ;
#101881 = DIRECTION ( 'NONE',  ( 1.000000000000000000, 0.000000000000000000, 0.000000000000000000 ) ) ;
#101882 = CARTESIAN_POINT ( 'NONE',  ( -21.14999999999999858, -11.65000000000000036, 0.000000000000000000 ) ) ;
#101883 = CARTESIAN_POINT ( 'NONE',  ( -22.00356870069947135, 76.00000000001202238, -110.2773498462699564 ) ) ;
#101884 = VECTOR ( 'NONE', #210473, 1000.000000000000000 ) ;
#101885 = AXIS2_PLACEMENT_3D ( 'NONE', #220550, #241406, #199723 ) ;
#101886 = ORIENTED_EDGE ( 'NONE', *, *, #95632, .T. ) ;
#101887 = DIRECTION ( 'NONE',  ( 0.000000000000000000, -0.5000000000000016653, 0.8660254037844377084 ) ) ;
#101889 = ORIENTED_EDGE ( 'NONE', *, *, #216023, .F. ) ;
#101888 = DIRECTION ( 'NONE',  ( -0.000000000000000000, 0.8096735173027139743, -0.5868805631290339164 ) ) ;
#101891 = DIRECTION ( 'NONE',  ( 0.000000000000000000, -0.1350103645451945777, 0.9908441862701591329 ) ) ;
#101890 = DIRECTION ( 'NONE',  ( -1.000000000000000000, -0.000000000000000000, -0.000000000000000000 ) ) ;
#101892 = CARTESIAN_POINT ( 'NONE',  ( 20.21494484322215968, 66.69682926214346708, -161.6828422927512179 ) ) ;
#101893 =( BOUNDED_SURFACE ( )  B_SPLINE_SURFACE ( 3, 2, ( 
 ( #6096, #203021, #103903 ),
 ( #25684, #146882, #183475 ),
 ( #4802, #243434, #165188 ),
 ( #126042, #244708, #66084 ) ),
 .UNSPECIFIED., .F., .F., .F. ) 
 B_SPLINE_SURFACE_WITH_KNOTS ( ( 4, 4 ),
 ( 3, 3 ),
 ( -2.710505431213761085E-20, 0.0003124336600439507920 ),
 ( 0.000000000000000000, 1.000000000000000000 ),
 .UNSPECIFIED. ) 
 GEOMETRIC_REPRESENTATION_ITEM ( )  RATIONAL_B_SPLINE_SURFACE ( (
 ( 1.000000000000000000, 0.7071067811865475727, 1.000000000000000000),
 ( 1.000000000000000000, 0.7089187706049818738, 1.000000000000000000),
 ( 1.000000000000000000, 0.7039288185052217095, 1.000000000000000000),
 ( 1.000000000000000000, 0.7040654476015687502, 1.000000000000000000) ) ) 
 REPRESENTATION_ITEM ( '' )  SURFACE ( )  );
#101894 = DIRECTION ( 'NONE',  ( 0.7071067811865475727, -0.7071067811865475727, -4.937700262164531476E-15 ) ) ;
#101895 = ORIENTED_EDGE ( 'NONE', *, *, #133837, .F. ) ;
#101896 = VECTOR ( 'NONE', #219541, 1000.000000000000000 ) ;
#101897 = DIRECTION ( 'NONE',  ( 0.000000000000000000, 0.000000000000000000, 1.000000000000000000 ) ) ;
#101898 = DIRECTION ( 'NONE',  ( 1.000000000000000000, 0.000000000000000000, 0.000000000000000000 ) ) ;
#101899 = CIRCLE ( 'NONE', #176404, 0.09999999999999810429 ) ;
#101900 = FACE_OUTER_BOUND ( 'NONE', #160185, .T. ) ;
#101901 = VECTOR ( 'NONE', #98299, 1000.000000000000227 ) ;
#101902 = ORIENTED_EDGE ( 'NONE', *, *, #160197, .T. ) ;
#101903 = CARTESIAN_POINT ( 'NONE',  ( -23.25000000000000000, 70.22659352830977753, -197.9852579278363578 ) ) ;
#101904 = DIRECTION ( 'NONE',  ( -0.000000000000000000, 0.9126074666063771490, 0.4088369013363281623 ) ) ;
#101905 = DIRECTION ( 'NONE',  ( 0.000000000000000000, 0.9915357197604972583, -0.1298341882519109536 ) ) ;
#101906 = PLANE ( 'NONE',  #86925 ) ;
#101907 = VERTEX_POINT ( 'NONE', #91093 ) ;
#101908 = AXIS2_PLACEMENT_3D ( 'NONE', #246896, #49991, #70874 ) ;
#101909 = ORIENTED_EDGE ( 'NONE', *, *, #122122, .T. ) ;
#101910 = CARTESIAN_POINT ( 'NONE',  ( -21.40925344232282512, 69.34148114062149659, -103.1220576731440133 ) ) ;
#101912 = CIRCLE ( 'NONE', #26962, 0.1000000000000056677 ) ;
#101911 = DIRECTION ( 'NONE',  ( 0.000000000000000000, 0.000000000000000000, -1.000000000000000000 ) ) ;
#101913 = FACE_OUTER_BOUND ( 'NONE', #228429, .T. ) ;
#101914 = CARTESIAN_POINT ( 'NONE',  ( -18.59999999999999787, 11.65000000001115232, -107.5148057706540357 ) ) ;
#101915 = ADVANCED_FACE ( 'NONE', ( #106789 ), #186351, .T. ) ;
#101917 = CARTESIAN_POINT ( 'NONE',  ( 22.39999999999999858, 0.1000000000111554016, -159.7092204016265669 ) ) ;
#101916 = DIRECTION ( 'NONE',  ( -1.000000000000000000, -0.000000000000000000, -0.000000000000000000 ) ) ;
#101918 = CARTESIAN_POINT ( 'NONE',  ( -18.59999999999999787, 68.11887992016828264, -227.8068560890360175 ) ) ;
#101919 = DIRECTION ( 'NONE',  ( 0.000000000000000000, -0.8814952561688437216, 0.4721928772777334582 ) ) ;
#101920 = CARTESIAN_POINT ( 'NONE',  ( 22.45463910399149299, 76.00000000001311662, -148.1726782947081631 ) ) ;
#101921 = TOROIDAL_SURFACE ( 'NONE', #143456, 7.800000000000000711, 0.1000000000000000056 ) ;
#101922 = ORIENTED_EDGE ( 'NONE', *, *, #58949, .T. ) ;
#101923 = CARTESIAN_POINT ( 'NONE',  ( -16.89268316805466341, 66.04827818676939444, -56.87885996306994230 ) ) ;
#101924 = AXIS2_PLACEMENT_3D ( 'NONE', #244839, #66220, #200590 ) ;
#101926 = ORIENTED_EDGE ( 'NONE', *, *, #189380, .T. ) ;
#101925 = CARTESIAN_POINT ( 'NONE',  ( 13.88638282980483041, 62.94602368561173478, -215.5245807872942407 ) ) ;
#101927 = AXIS2_PLACEMENT_3D ( 'NONE', #212647, #35320, #215195 ) ;
#101928 = LINE ( 'NONE', #61553, #181067 ) ;
#101929 = CARTESIAN_POINT ( 'NONE',  ( -18.50000000000000000, 85.40000000001209912, -129.6410656363516125 ) ) ;
#101930 = CARTESIAN_POINT ( 'NONE',  ( -17.11825945287482753, 10.05000000001113847, -79.75000000000004263 ) ) ;
#101931 = ORIENTED_EDGE ( 'NONE', *, *, #185689, .F. ) ;
#101933 = DIRECTION ( 'NONE',  ( 0.000000000000000000, -7.116814260417668513E-15, 1.000000000000000000 ) ) ;
#101932 = CARTESIAN_POINT ( 'NONE',  ( -16.83558968593870020, 66.05000000001157900, -56.86080229690766430 ) ) ;
#101934 = LINE ( 'NONE', #181524, #133078 ) ;
#101935 = CARTESIAN_POINT ( 'NONE',  ( -23.25000000000000000, 71.85000000001224407, -148.7731074845243882 ) ) ;
#101936 = DIRECTION ( 'NONE',  ( -0.000000000000000000, -0.9910465087640865089, 0.1335171055202867274 ) ) ;
#101937 = DIRECTION ( 'NONE',  ( -1.000000000000000000, 0.000000000000000000, 0.000000000000000000 ) ) ;
#101938 = EDGE_LOOP ( 'NONE', ( #59016, #27194 ) ) ;
#101940 = EDGE_CURVE ( 'NONE', #236931, #254860, #207202, .T. ) ;
#101939 = ORIENTED_EDGE ( 'NONE', *, *, #199179, .T. ) ;
#101941 = CYLINDRICAL_SURFACE ( 'NONE', #17734, 0.1000000000000013656 ) ;
#101942 = ORIENTED_EDGE ( 'NONE', *, *, #1673, .F. ) ;
#101943 = DIRECTION ( 'NONE',  ( -0.000000000000000000, -0.000000000000000000, 1.000000000000000000 ) ) ;
#101944 = VECTOR ( 'NONE', #156081, 1000.000000000000000 ) ;
#101945 = ORIENTED_EDGE ( 'NONE', *, *, #250377, .T. ) ;
#101946 = DIRECTION ( 'NONE',  ( -1.000000000000000000, 0.000000000000000000, 0.000000000000000000 ) ) ;
#101947 = EDGE_CURVE ( 'NONE', #25296, #230954, #187642, .T. ) ;
#101948 = CIRCLE ( 'NONE', #160274, 0.09999999999999063804 ) ;
#101950 = EDGE_CURVE ( 'NONE', #82676, #219130, #195352, .T. ) ;
#101949 = CARTESIAN_POINT ( 'NONE',  ( -20.99551997958407057, 62.86709121503487552, -207.0570825002662332 ) ) ;
#101951 = ORIENTED_EDGE ( 'NONE', *, *, #163903, .F. ) ;
#101952 = ADVANCED_FACE ( 'NONE', ( #173246 ), #111958, .T. ) ;
#101953 = DIRECTION ( 'NONE',  ( -0.000000000000000000, 0.9770955615653313941, 0.2128009952263603954 ) ) ;
#101954 = DIRECTION ( 'NONE',  ( -1.000000000000000000, -0.000000000000000000, -0.000000000000000000 ) ) ;
#101955 = CYLINDRICAL_SURFACE ( 'NONE', #228414, 0.09999999999999939493 ) ;
#101956 = CARTESIAN_POINT ( 'NONE',  ( -16.90137573187933029, 44.26180248075819890, -235.2423414558488162 ) ) ;
#101957 = DIRECTION ( 'NONE',  ( -3.265361837132813093E-16, 1.000000000000000000, 0.000000000000000000 ) ) ;
#101958 = ADVANCED_FACE ( 'NONE', ( #191509 ), #22385, .T. ) ;
#101959 = CARTESIAN_POINT ( 'NONE',  ( 19.97071067811865674, 62.37141908057010653, -208.9966201521277753 ) ) ;
#101960 = ORIENTED_EDGE ( 'NONE', *, *, #43772, .T. ) ;
#101962 = CARTESIAN_POINT ( 'NONE',  ( -22.49072729836729678, 75.94351806727914322, -215.1731157336793103 ) ) ;
#101961 = PLANE ( 'NONE',  #203401 ) ;
#101963 = ORIENTED_EDGE ( 'NONE', *, *, #14011, .F. ) ;
#101965 = ORIENTED_EDGE ( 'NONE', *, *, #145546, .T. ) ;
#101964 = CARTESIAN_POINT ( 'NONE',  ( -20.85000000000000142, -1.164121893230052995, -108.4148480855716485 ) ) ;
#101966 = AXIS2_PLACEMENT_3D ( 'NONE', #28375, #128727, #223951 ) ;
#101967 = VERTEX_POINT ( 'NONE', #196595 ) ;
#101968 = VECTOR ( 'NONE', #98153, 1000.000000000000000 ) ;
#101969 = CARTESIAN_POINT ( 'NONE',  ( 21.05000000000000071, 44.52640028187936849, -247.3006740988509193 ) ) ;
#101970 = EDGE_CURVE ( 'NONE', #156620, #228338, #171951, .T. ) ;
#101971 = DIRECTION ( 'NONE',  ( 1.000000000000000000, 0.000000000000000000, 0.000000000000000000 ) ) ;
#101972 = CARTESIAN_POINT ( 'NONE',  ( 21.12400247839529399, 60.09006653341421611, -221.2258423852895817 ) ) ;
#101973 = CARTESIAN_POINT ( 'NONE',  ( -21.40925344232282512, 60.77900513643817249, -234.2077395100402839 ) ) ;
#101974 = VERTEX_POINT ( 'NONE', #76650 ) ;
#101975 = DIRECTION ( 'NONE',  ( 0.000000000000000000, 0.000000000000000000, 1.000000000000000000 ) ) ;
#101976 = DIRECTION ( 'NONE',  ( 0.000000000000000000, 0.000000000000000000, -1.000000000000000000 ) ) ;
#101977 = EDGE_LOOP ( 'NONE', ( #88659, #86111, #117968 ) ) ;
#101979 = EDGE_CURVE ( 'NONE', #221635, #37340, #201411, .T. ) ;
#101978 = CARTESIAN_POINT ( 'NONE',  ( -21.44999999999999929, 7.150000000011155876, -146.3500000000000227 ) ) ;
#101981 = VECTOR ( 'NONE', #252494, 1000.000000000000000 ) ;
#101980 = DIRECTION ( 'NONE',  ( 0.000000000000000000, 0.000000000000000000, -1.000000000000000000 ) ) ;
#101982 = ORIENTED_EDGE ( 'NONE', *, *, #4222, .F. ) ;
#101984 = CARTESIAN_POINT ( 'NONE',  ( -20.94999999999999929, 1.115600667400684642E-11, -100.5000000000000284 ) ) ;
#101983 = VECTOR ( 'NONE', #106828, 1000.000000000000114 ) ;
#101985 = AXIS2_PLACEMENT_3D ( 'NONE', #48977, #89377, #88077 ) ;
#101986 = AXIS2_PLACEMENT_3D ( 'NONE', #47020, #87438, #211254 ) ;
#101987 = LINE ( 'NONE', #142425, #71587 ) ;
#101988 = ORIENTED_EDGE ( 'NONE', *, *, #19494, .F. ) ;
#101989 = DIRECTION ( 'NONE',  ( 0.000000000000000000, -0.4930308989874718772, -0.8700118002898612479 ) ) ;
#101990 =( BOUNDED_SURFACE ( )  B_SPLINE_SURFACE ( 3, 2, ( 
 ( #225374, #46743, #27230 ),
 ( #184986, #50586, #106709 ),
 ( #248821, #190130, #11498 ),
 ( #65030, #169315, #149736 ) ),
 .UNSPECIFIED., .F., .F., .T. ) 
 B_SPLINE_SURFACE_WITH_KNOTS ( ( 4, 4 ),
 ( 3, 3 ),
 ( 4.712388980384689674, 5.765869716888531116 ),
 ( 0.000000000000000000, 1.000000000000000000 ),
 .UNSPECIFIED. ) 
 GEOMETRIC_REPRESENTATION_ITEM ( )  RATIONAL_B_SPLINE_SURFACE ( (
 ( 1.000000000000000000, 0.7071067811865475727, 1.000000000000000000),
 ( 1.000000000000000000, 0.7953136715913589061, 1.000000000000000000),
 ( 1.000000000000000000, 0.8646876308614964701, 1.000000000000000000),
 ( 1.000000000000000000, 0.8984936768950676500, 1.000000000000000000) ) ) 
 REPRESENTATION_ITEM ( '' )  SURFACE ( )  );
#101991 = PRESENTATION_LAYER_ASSIGNMENT (  '', '', ( #243672 ) ) ;
#101992 = DIRECTION ( 'NONE',  ( 1.000000000000000000, 2.952720810173289112E-16, -0.000000000000000000 ) ) ;
#101993 = DIRECTION ( 'NONE',  ( -4.391705002472927119E-16, -1.000000000000000000, -7.026728003956683390E-15 ) ) ;
#101994 = DIRECTION ( 'NONE',  ( 1.301042606982683734E-14, -0.1022405907414274118, -0.9947597004326442782 ) ) ;
#101995 = CARTESIAN_POINT ( 'NONE',  ( 21.14999999999999858, -0.09999999998884338825, -33.50000000000000000 ) ) ;
#101996 = CARTESIAN_POINT ( 'NONE',  ( -20.09999999673964410, 4.627350251755220079, 22.02580456186781177 ) ) ;
#101997 = AXIS2_PLACEMENT_3D ( 'NONE', #71633, #195438, #230703 ) ;
#101998 = ORIENTED_EDGE ( 'NONE', *, *, #27407, .F. ) ;
#102000 = CARTESIAN_POINT ( 'NONE',  ( 23.14999999999999503, 62.82351852614503684, -207.2177435922979214 ) ) ;
#101999 = SURFACE_STYLE_FILL_AREA ( #141170 ) ;
#102001 = VECTOR ( 'NONE', #209587, 1000.000000000000000 ) ;
#102002 = EDGE_CURVE ( 'NONE', #162201, #176943, #122311, .T. ) ;
#102004 = ADVANCED_FACE ( 'NONE', ( #214881 ), #255238, .F. ) ;
#102003 = AXIS2_PLACEMENT_3D ( 'NONE', #214871, #131485, #194051 ) ;
#102005 = ORIENTED_EDGE ( 'NONE', *, *, #46092, .T. ) ;
#102006 = LINE ( 'NONE', #241549, #110234 ) ;
#102007 = DIRECTION ( 'NONE',  ( -1.000000000000000000, 0.000000000000000000, -0.000000000000000000 ) ) ;
#102009 = ORIENTED_EDGE ( 'NONE', *, *, #60183, .F. ) ;
#102008 = DIRECTION ( 'NONE',  ( 1.073024830501117725E-15, 6.982962677686266711E-15, -1.000000000000000000 ) ) ;
#102010 = CARTESIAN_POINT ( 'NONE',  ( -18.46907102845853998, 85.47372736477618105, -129.8470727457877558 ) ) ;
#102012 = EDGE_CURVE ( 'NONE', #228214, #197595, #9875, .T. ) ;
#102011 = CARTESIAN_POINT ( 'NONE',  ( 18.39999999999999858, 46.91436717984746707, -255.3877622108296634 ) ) ;
#102014 = ADVANCED_FACE ( 'NONE', ( #12858 ), #230860, .T. ) ;
#102013 = DIRECTION ( 'NONE',  ( 0.000000000000000000, -1.000000000000000000, -6.982962677686265922E-15 ) ) ;
#102015 = CARTESIAN_POINT ( 'NONE',  ( -16.87683809663752754, 9.864913778549567525, -80.27571563563854795 ) ) ;
#102016 = VECTOR ( 'NONE', #139839, 1000.000000000000000 ) ;
#102017 = DIRECTION ( 'NONE',  ( 1.000000000000000000, 0.000000000000000000, 0.000000000000000000 ) ) ;
#102018 = AXIS2_PLACEMENT_3D ( 'NONE', #143029, #43950, #203017 ) ;
#102019 = CIRCLE ( 'NONE', #177084, 1.500000000000001332 ) ;
#102021 = EDGE_LOOP ( 'NONE', ( #12204, #46429, #55641, #202207, #92806, #140422, #153501, #24558, #222908, #36097 ) ) ;
#102020 = CARTESIAN_POINT ( 'NONE',  ( -5.899999999999938183, 64.65000000001120384, -25.92310748452479174 ) ) ;
#102022 = CIRCLE ( 'NONE', #64459, 0.1000000000000124678 ) ;
#102023 = EDGE_CURVE ( 'NONE', #242320, #70449, #201591, .T. ) ;
#102024 = EDGE_CURVE ( 'NONE', #227883, #96658, #234930, .T. ) ;
#102026 = EDGE_CURVE ( 'NONE', #15176, #12050, #1670, .T. ) ;
#102025 = EDGE_CURVE ( 'NONE', #204167, #200518, #68341, .T. ) ;
#102027 = DIRECTION ( 'NONE',  ( 4.336808689942128177E-15, 0.8660254037844330455, -0.5000000000000096589 ) ) ;
#102028 = CIRCLE ( 'NONE', #56244, 0.1000000000000028644 ) ;
#102029 = ORIENTED_EDGE ( 'NONE', *, *, #7036, .T. ) ;
#102030 = VERTEX_POINT ( 'NONE', #15421 ) ;
#102031 = AXIS2_PLACEMENT_3D ( 'NONE', #237956, #59283, #16373 ) ;
#102032 = EDGE_CURVE ( 'NONE', #129552, #53634, #194062, .T. ) ;
#102033 = DIRECTION ( 'NONE',  ( 0.000000000000000000, 0.000000000000000000, -1.000000000000000000 ) ) ;
#102034 = CARTESIAN_POINT ( 'NONE',  ( 19.90621891164687440, 34.56325637860300759, -235.0989470665489876 ) ) ;
#102035 = CIRCLE ( 'NONE', #235327, 11.80000000000000426 ) ;
#102037 = VERTEX_POINT ( 'NONE', #93654 ) ;
#102036 = AXIS2_PLACEMENT_3D ( 'NONE', #135370, #256557, #74168 ) ;
#102038 = CARTESIAN_POINT ( 'NONE',  ( 13.40000000000005898, 64.35000000001120668, -23.72310748452479601 ) ) ;
#102039 = EDGE_CURVE ( 'NONE', #92040, #2004, #77929, .T. ) ;
#102040 = DIRECTION ( 'NONE',  ( -0.000000000000000000, 1.000000000000000000, -0.000000000000000000 ) ) ;
#102041 = EDGE_LOOP ( 'NONE', ( #10315, #61133, #19355, #83057 ) ) ;
#102042 = EDGE_CURVE ( 'NONE', #6106, #157579, #85039, .T. ) ;
#102043 = ADVANCED_FACE ( 'NONE', ( #137894 ), #217427, .F. ) ;
#102044 = CARTESIAN_POINT ( 'NONE',  ( -23.15000000000000213, 66.36210077474692071, -222.8232602954134336 ) ) ;
#102045 = LINE ( 'NONE', #163342, #101328 ) ;
#102046 = ADVANCED_FACE ( 'NONE', ( #143021 ), #63495, .T. ) ;
#102047 = ORIENTED_EDGE ( 'NONE', *, *, #12277, .T. ) ;
#102048 = ORIENTED_EDGE ( 'NONE', *, *, #167257, .F. ) ;
#102049 = EDGE_LOOP ( 'NONE', ( #251793, #58628, #63624, #227421 ) ) ;
#102050 = CARTESIAN_POINT ( 'NONE',  ( 21.05000000000000071, 46.45388641681647357, -243.1520440498138385 ) ) ;
#102051 = ORIENTED_EDGE ( 'NONE', *, *, #95341, .T. ) ;
#102053 = ORIENTED_EDGE ( 'NONE', *, *, #7181, .T. ) ;
#102052 = CARTESIAN_POINT ( 'NONE',  ( -22.39999999999999858, 11.75000000001115552, -100.4000000000000483 ) ) ;
#102054 = EDGE_CURVE ( 'NONE', #240530, #231902, #35049, .T. ) ;
#102055 = EDGE_CURVE ( 'NONE', #93742, #50892, #160070, .T. ) ;
#102056 = DIRECTION ( 'NONE',  ( 1.000000000000000000, 0.000000000000000000, 0.000000000000000000 ) ) ;
#102057 = VERTEX_POINT ( 'NONE', #222560 ) ;
#102058 = VECTOR ( 'NONE', #140487, 999.9999999999998863 ) ;
#102059 = CARTESIAN_POINT ( 'NONE',  ( -22.10000000000000142, -3.262756495241484158E-15, 33.00000000000000000 ) ) ;
#102060 = ORIENTED_EDGE ( 'NONE', *, *, #203559, .T. ) ;
#102061 = AXIS2_PLACEMENT_3D ( 'NONE', #102677, #183533, #148247 ) ;
#102063 = ORIENTED_EDGE ( 'NONE', *, *, #217061, .T. ) ;
#102062 = ORIENTED_EDGE ( 'NONE', *, *, #128000, .T. ) ;
#102064 = DIRECTION ( 'NONE',  ( 0.000000000000000000, -0.2128009952263604232, 0.9770955615653316162 ) ) ;
#102065 = AXIS2_PLACEMENT_3D ( 'NONE', #192826, #254057, #178415 ) ;
#102066 = CARTESIAN_POINT ( 'NONE',  ( -16.90987985657661952, 14.17073459112586598, -219.2722564374412286 ) ) ;
#102067 = VERTEX_POINT ( 'NONE', #180899 ) ;
#102068 = VECTOR ( 'NONE', #92769, 1000.000000000000000 ) ;
#102069 = AXIS2_PLACEMENT_3D ( 'NONE', #186261, #45452, #247507 ) ;
#102070 = ORIENTED_EDGE ( 'NONE', *, *, #73082, .F. ) ;
#102071 = CARTESIAN_POINT ( 'NONE',  ( 16.87683809663750267, 44.13548170601895038, -235.2989316066074821 ) ) ;
#102072 = CARTESIAN_POINT ( 'NONE',  ( 20.94999999999999929, 85.00000000001179501, -79.41707660717668205 ) ) ;
#102074 = VERTEX_POINT ( 'NONE', #239590 ) ;
#102073 = CARTESIAN_POINT ( 'NONE',  ( 22.39999999999999503, 64.25000000001237765, -170.1231074845244393 ) ) ;
#102075 = CARTESIAN_POINT ( 'NONE',  ( 22.39999999999999858, 33.38250548509083870, -242.4821227592188961 ) ) ;
#102076 = ORIENTED_EDGE ( 'NONE', *, *, #237068, .F. ) ;
#102077 = FACE_OUTER_BOUND ( 'NONE', #190337, .T. ) ;
#102078 = DIRECTION ( 'NONE',  ( 0.000000000000000000, 0.2128009952263605620, -0.9770955615653315052 ) ) ;
#102079 = AXIS2_PLACEMENT_3D ( 'NONE', #123699, #182393, #83247 ) ;
#102080 = ORIENTED_EDGE ( 'NONE', *, *, #218554, .F. ) ;
#102081 = DIRECTION ( 'NONE',  ( 0.000000000000000000, 3.122502256758250246E-14, -1.000000000000000000 ) ) ;
#102082 = CARTESIAN_POINT ( 'NONE',  ( -23.25000000000000000, 85.68240343348826116, -96.36626410711143365 ) ) ;
#102083 = DIRECTION ( 'NONE',  ( 0.000000000000000000, -0.000000000000000000, -1.000000000000000000 ) ) ;
#102084 = ORIENTED_EDGE ( 'NONE', *, *, #147422, .T. ) ;
#102085 = CARTESIAN_POINT ( 'NONE',  ( -23.15000000000000213, 71.85000000001245724, -181.7731074845243882 ) ) ;
#102086 = ORIENTED_EDGE ( 'NONE', *, *, #241751, .F. ) ;
#102087 = ORIENTED_EDGE ( 'NONE', *, *, #127522, .T. ) ;
#102088 = VERTEX_POINT ( 'NONE', #238286 ) ;
#102089 = CARTESIAN_POINT ( 'NONE',  ( 20.94999999999999929, 87.48912529308852015, -173.0231074845243029 ) ) ;
#102090 = ORIENTED_EDGE ( 'NONE', *, *, #88815, .T. ) ;
#102091 = CARTESIAN_POINT ( 'NONE',  ( -16.77683809663752257, 9.945835743215303282, -54.33605098089579855 ) ) ;
#102092 = AXIS2_PLACEMENT_3D ( 'NONE', #155243, #93943, #233484 ) ;
#102093 = ORIENTED_EDGE ( 'NONE', *, *, #22427, .T. ) ;
#102094 = DIRECTION ( 'NONE',  ( 0.000000000000000000, 0.8814952561688476074, -0.4721928772777262417 ) ) ;
#102095 = FACE_OUTER_BOUND ( 'NONE', #58633, .T. ) ;
#102096 = ORIENTED_EDGE ( 'NONE', *, *, #71889, .F. ) ;
#102097 = EDGE_CURVE ( 'NONE', #82879, #216709, #43944, .T. ) ;
#102098 = ORIENTED_EDGE ( 'NONE', *, *, #154775, .T. ) ;
#102099 = EDGE_CURVE ( 'NONE', #54306, #50212, #105892, .T. ) ;
#102100 = ORIENTED_EDGE ( 'NONE', *, *, #171509, .F. ) ;
#102101 = AXIS2_PLACEMENT_3D ( 'NONE', #234941, #253202, #232389 ) ;
#102102 = AXIS2_PLACEMENT_3D ( 'NONE', #161016, #145279, #224820 ) ;
#102103 = ADVANCED_FACE ( 'NONE', ( #24409 ), #60933, .F. ) ;
#102104 = CARTESIAN_POINT ( 'NONE',  ( -16.86445178670700784, 66.03778837089569720, -82.13233004640675006 ) ) ;
#102105 = ADVANCED_FACE ( 'NONE', ( #23125 ), #101294, .T. ) ;
#102106 = EDGE_LOOP ( 'NONE', ( #99726, #61607, #39250, #159536 ) ) ;
#102107 = CARTESIAN_POINT ( 'NONE',  ( 22.39999999999999503, 76.00000000001219291, -144.3138870828976792 ) ) ;
#102108 = DIRECTION ( 'NONE',  ( 0.000000000000000000, -1.000000000000000000, 0.000000000000000000 ) ) ;
#102109 = CARTESIAN_POINT ( 'NONE',  ( -20.99749315643150638, 11.75000000001115197, -126.9851942312421045 ) ) ;
#102110 = CARTESIAN_POINT ( 'NONE',  ( -20.85000000000000142, -1.149570369564537842, -108.3159124845020074 ) ) ;
#102111 = DIRECTION ( 'NONE',  ( -1.000000000000000000, -7.304098846218134667E-16, 4.217023435051678980E-16 ) ) ;
#102112 = CARTESIAN_POINT ( 'NONE',  ( -23.30000000000000426, 3.332938107839114927, -347.0000000000001137 ) ) ;
#102114 = CARTESIAN_POINT ( 'NONE',  ( 21.08621493067296271, 6.349294291182824068, -100.4438051605239224 ) ) ;
#102113 = CARTESIAN_POINT ( 'NONE',  ( -23.25000000000000000, 77.14957036958807635, -162.2071950000224092 ) ) ;
#102115 = FACE_OUTER_BOUND ( 'NONE', #251918, .T. ) ;
#102116 = PLANE ( 'NONE',  #140388 ) ;
#102117 = CARTESIAN_POINT ( 'NONE',  ( -20.54999999999999716, -3.770473190032741062, -225.9805569534692324 ) ) ;
#102118 = DIRECTION ( 'NONE',  ( 0.000000000000000000, -0.9698110461157734008, -0.2438576117980102709 ) ) ;
#102119 = VECTOR ( 'NONE', #252253, 1000.000000000000000 ) ;
#102120 = VERTEX_POINT ( 'NONE', #140468 ) ;
#102121 = EDGE_CURVE ( 'NONE', #138601, #73041, #240873, .T. ) ;
#102122 = AXIS2_PLACEMENT_3D ( 'NONE', #258101, #119960, #42963 ) ;
#102124 = EDGE_LOOP ( 'NONE', ( #145653, #155268, #128460, #217084 ) ) ;
#102123 = CYLINDRICAL_SURFACE ( 'NONE', #215543, 0.1000000000000106914 ) ;
#102125 = EDGE_LOOP ( 'NONE', ( #20551, #137588, #63482, #246923 ) ) ;
#102126 = DIRECTION ( 'NONE',  ( 0.000000000000000000, 0.000000000000000000, -1.000000000000000000 ) ) ;
#102127 = DIRECTION ( 'NONE',  ( 0.000000000000000000, 0.4999999999999088507, 0.8660254037844913322 ) ) ;
#102128 = ORIENTED_EDGE ( 'NONE', *, *, #240121, .T. ) ;
#102129 =( NAMED_UNIT ( * ) PLANE_ANGLE_UNIT ( ) SI_UNIT ( $, .RADIAN. ) );
#102130 = ADVANCED_FACE ( 'NONE', ( #199172 ), #106506, .T. ) ;
#102131 = FACE_OUTER_BOUND ( 'NONE', #166335, .T. ) ;
#102132 = EDGE_CURVE ( 'NONE', #187737, #68820, #180762, .T. ) ;
#102133 = CARTESIAN_POINT ( 'NONE',  ( -21.65000000000000213, 68.25000000001260503, -191.1731074845243938 ) ) ;
#102134 = VERTEX_POINT ( 'NONE', #80463 ) ;
#102136 = CARTESIAN_POINT ( 'NONE',  ( -18.58222699835055280, 10.33200063080771969, -206.5931674956642610 ) ) ;
#102135 = AXIS2_PLACEMENT_3D ( 'NONE', #147982, #245797, #22919 ) ;
#102137 = AXIS2_PLACEMENT_3D ( 'NONE', #58606, #199447, #61194 ) ;
#102138 = CARTESIAN_POINT ( 'NONE',  ( -18.59999999999999787, 7.021664781911246322, -70.63356540189728605 ) ) ;
#102139 = DIRECTION ( 'NONE',  ( 8.673617379884087537E-15, -0.000000000000000000, 1.000000000000000000 ) ) ;
#102140 = DIRECTION ( 'NONE',  ( 0.000000000000000000, 6.982962677686266711E-15, -1.000000000000000000 ) ) ;
#102142 = ORIENTED_EDGE ( 'NONE', *, *, #71002, .T. ) ;
#102141 = DIRECTION ( 'NONE',  ( 1.000000000000000000, 0.000000000000000000, 0.000000000000000000 ) ) ;
#102143 = EDGE_CURVE ( 'NONE', #108747, #193967, #30945, .T. ) ;
#102145 = ORIENTED_EDGE ( 'NONE', *, *, #60651, .F. ) ;
#102144 = DIRECTION ( 'NONE',  ( 0.000000000000000000, -0.9941044884914576052, 0.1084263158146461931 ) ) ;
#102146 = DIRECTION ( 'NONE',  ( 1.000000000000000000, 0.000000000000000000, 0.000000000000000000 ) ) ;
#102147 = DIRECTION ( 'NONE',  ( 1.000000000000000000, -0.000000000000000000, -0.000000000000000000 ) ) ;
#102148 = CARTESIAN_POINT ( 'NONE',  ( -16.93230518875208190, 65.99924963859245963, -157.4473291364229226 ) ) ;
#102149 = EDGE_CURVE ( 'NONE', #59445, #224509, #214073, .T. ) ;
#102150 = CARTESIAN_POINT ( 'NONE',  ( -13.54795643572458097, 9.450668889178684751, -182.5555464902073197 ) ) ;
#102152 = FACE_OUTER_BOUND ( 'NONE', #116543, .T. ) ;
#102151 = CARTESIAN_POINT ( 'NONE',  ( -18.59999999999999787, 10.33248238083634440, -139.5948465439131780 ) ) ;
#102153 = CARTESIAN_POINT ( 'NONE',  ( -21.05000000000000071, 34.07612324756792077, -243.5412266404783566 ) ) ;
#102154 = CARTESIAN_POINT ( 'NONE',  ( -20.54999999999999716, 67.23127455305835554, -235.8551265064784559 ) ) ;
#102155 = AXIS2_PLACEMENT_3D ( 'NONE', #245789, #167560, #87964 ) ;
#102157 = EDGE_CURVE ( 'NONE', #51883, #77430, #141752, .T. ) ;
#102156 = CARTESIAN_POINT ( 'NONE',  ( -21.05439746398122836, 64.25000000001233502, -163.0331909970394406 ) ) ;
#102158 = CARTESIAN_POINT ( 'NONE',  ( 21.05000000000000071, 67.23127455305835554, -235.8551265064784559 ) ) ;
#102159 = AXIS2_PLACEMENT_3D ( 'NONE', #7416, #187366, #11285 ) ;
#102160 = CARTESIAN_POINT ( 'NONE',  ( 22.48660254037844197, 11.37252324248628987, -198.4720136275361426 ) ) ;
#102161 = TOROIDAL_SURFACE ( 'NONE', #168879, 0.6000000000000009770, 0.1000000000000000056 ) ;
#102162 = VERTEX_POINT ( 'NONE', #186026 ) ;
#102163 = DIRECTION ( 'NONE',  ( 0.000000000000000000, 1.734723475976997999E-14, -1.000000000000000000 ) ) ;
#102164 = ORIENTED_EDGE ( 'NONE', *, *, #201124, .F. ) ;
#102165 = ORIENTED_EDGE ( 'NONE', *, *, #199289, .F. ) ;
#102166 = DIRECTION ( 'NONE',  ( 1.000000000000000000, 0.000000000000000000, 0.000000000000000000 ) ) ;
#102167 = CYLINDRICAL_SURFACE ( 'NONE', #211128, 0.09999999999999986677 ) ;
#102168 = ORIENTED_EDGE ( 'NONE', *, *, #202366, .F. ) ;
#102169 = EDGE_CURVE ( 'NONE', #232695, #235134, #139212, .T. ) ;
#102170 = ORIENTED_EDGE ( 'NONE', *, *, #220121, .T. ) ;
#102171 = EDGE_CURVE ( 'NONE', #13509, #10114, #101607, .T. ) ;
#102172 = SURFACE_STYLE_USAGE ( .BOTH. , #141335 ) ;
#102173 = ORIENTED_EDGE ( 'NONE', *, *, #161292, .F. ) ;
#102174 = AXIS2_PLACEMENT_3D ( 'NONE', #242225, #144389, #29640 ) ;
#102175 = ORIENTED_EDGE ( 'NONE', *, *, #109785, .T. ) ;
#102176 = CARTESIAN_POINT ( 'NONE',  ( 18.49999999999996803, 68.92903212821357783, -166.2765432626560766 ) ) ;
#102177 = CARTESIAN_POINT ( 'NONE',  ( 20.94999999999999929, 28.67750504931771616, -258.3094128005139396 ) ) ;
#102178 = CIRCLE ( 'NONE', #247960, 0.09999999999999939493 ) ;
#102179 = DIRECTION ( 'NONE',  ( 1.000000000000000000, 1.875376730785737719E-16, 0.000000000000000000 ) ) ;
#102180 = LINE ( 'NONE', #82617, #81792 ) ;
#102181 = DIRECTION ( 'NONE',  ( 0.000000000000000000, 0.8814952561688429444, -0.4721928772777345684 ) ) ;
#102182 = CARTESIAN_POINT ( 'NONE',  ( 18.59999999999999787, -10.72142460728770352, 6.051435706882140053 ) ) ;
#102185 = ORIENTED_EDGE ( 'NONE', *, *, #17484, .F. ) ;
#102184 = LINE ( 'NONE', #197461, #113314 ) ;
#102183 = VECTOR ( 'NONE', #195001, 1000.000000000000000 ) ;
#102187 = CARTESIAN_POINT ( 'NONE',  ( 18.43709777086140278, 85.68240343348777799, -29.36626410711147273 ) ) ;
#102186 = CARTESIAN_POINT ( 'NONE',  ( -17.27223548805033460, 63.04010829898014379, -211.7852720176618675 ) ) ;
#102188 = CARTESIAN_POINT ( 'NONE',  ( 21.05000000000000071, 64.35000000001164722, -69.42310748452440805 ) ) ;
#102189 = EDGE_LOOP ( 'NONE', ( #193885, #196551, #158489, #83318 ) ) ;
#102190 = CIRCLE ( 'NONE', #202187, 1.900000000000005906 ) ;
#102191 = FACE_OUTER_BOUND ( 'NONE', #138005, .T. ) ;
#102192 = DIRECTION ( 'NONE',  ( 0.000000000000000000, 0.2128009952263403282, -0.9770955615653358350 ) ) ;
#102193 = AXIS2_PLACEMENT_3D ( 'NONE', #212690, #112308, #13209 ) ;
#102195 = VERTEX_POINT ( 'NONE', #107767 ) ;
#102194 = AXIS2_PLACEMENT_3D ( 'NONE', #215340, #198348, #36748 ) ;
#102197 = CARTESIAN_POINT ( 'NONE',  ( 22.47007471830798053, 76.00000000001169553, -77.24381813645078410 ) ) ;
#102196 = DIRECTION ( 'NONE',  ( -1.073024830501117725E-15, 6.982962677686266711E-15, -1.000000000000000000 ) ) ;
#102198 = CARTESIAN_POINT ( 'NONE',  ( -22.32929514600008503, 75.90092432189808846, -110.6017550499008166 ) ) ;
#102199 = ORIENTED_EDGE ( 'NONE', *, *, #37160, .F. ) ;
#102200 = VECTOR ( 'NONE', #120425, 1000.000000000000000 ) ;
#102201 = CARTESIAN_POINT ( 'NONE',  ( 21.05000000000000071, 6.299230910098045477, -66.90156250000005400 ) ) ;
#102202 = DIRECTION ( 'NONE',  ( 0.000000000000000000, 6.938893903907222067E-15, -1.000000000000000000 ) ) ;
#102203 = AXIS2_PLACEMENT_3D ( 'NONE', #105926, #124250, #83777 ) ;
#102204 = DIRECTION ( 'NONE',  ( 1.000000000000000000, 2.952720810173289112E-16, -0.000000000000000000 ) ) ;
#102205 = CARTESIAN_POINT ( 'NONE',  ( -22.50875500270928953, -0.1008579137641102963, -122.2504328726021328 ) ) ;
#102206 = ORIENTED_EDGE ( 'NONE', *, *, #220050, .F. ) ;
#102207 = VECTOR ( 'NONE', #19233, 1000.000000000000000 ) ;
#102208 = TOROIDAL_SURFACE ( 'NONE', #10504, 11.90000000000000213, 0.1000000000000000056 ) ;
#102209 = FACE_OUTER_BOUND ( 'NONE', #138925, .T. ) ;
#102210 = CARTESIAN_POINT ( 'NONE',  ( -21.14999999999999858, 67.23127455305841238, -235.8551265064783991 ) ) ;
#102211 = CARTESIAN_POINT ( 'NONE',  ( -20.94999999999999929, -1.835341550213255957, -179.0551512925629538 ) ) ;
#102212 = DIRECTION ( 'NONE',  ( 0.000000000000000000, 0.000000000000000000, 1.000000000000000000 ) ) ;
#102213 = CARTESIAN_POINT ( 'NONE',  ( 18.49999999999999289, 7.120270961708750512, -137.6595630418393625 ) ) ;
#102215 = ORIENTED_EDGE ( 'NONE', *, *, #183081, .F. ) ;
#102214 = CARTESIAN_POINT ( 'NONE',  ( 21.09706851349342216, 8.775842513484549912, -179.7355662163996328 ) ) ;
#102216 = CARTESIAN_POINT ( 'NONE',  ( -21.05000000000000071, 6.540656951712400691, -33.60000000000000142 ) ) ;
#102217 = CARTESIAN_POINT ( 'NONE',  ( 20.84999999999998721, 65.66751761918692409, -130.9282609406112670 ) ) ;
#102218 = CARTESIAN_POINT ( 'NONE',  ( 18.59999999999999432, 74.73821383144705521, -128.4366085209788366 ) ) ;
#102219 = CARTESIAN_POINT ( 'NONE',  ( 18.49999999999999645, 1.835341550235567887, -45.05515129256298223 ) ) ;
#102220 = EDGE_CURVE ( 'NONE', #9287, #213770, #247374, .T. ) ;
#102221 = DIRECTION ( 'NONE',  ( 0.7071067811865493491, -0.7071067811865456854, -4.937700262164518065E-15 ) ) ;
#102223 = ORIENTED_EDGE ( 'NONE', *, *, #45505, .F. ) ;
#102222 = SPHERICAL_SURFACE ( 'NONE', #206703, 0.1000000000000000056 ) ;
#102224 = CARTESIAN_POINT ( 'NONE',  ( -18.59999999999999787, 76.00000000001207923, -128.6231074845243540 ) ) ;
#102225 = CARTESIAN_POINT ( 'NONE',  ( -17.04295772865306446, 63.01344430405035268, -213.1080164377868300 ) ) ;
#102226 = CARTESIAN_POINT ( 'NONE',  ( -21.64999999999999858, 9.809744668562228043, -211.5030428704195913 ) ) ;
#102227 = VERTEX_POINT ( 'NONE', #184726 ) ;
#102228 = CARTESIAN_POINT ( 'NONE',  ( -12.48127053791145435, 66.62341902196833132, -152.3961612375125014 ) ) ;
#102229 = CIRCLE ( 'NONE', #110646, 0.09999999999999817368 ) ;
#102230 = CARTESIAN_POINT ( 'NONE',  ( 21.04999999999999716, 75.90156250001210481, -176.3223383946166507 ) ) ;
#102231 = ADVANCED_FACE ( 'NONE', ( #149490 ), #188583, .F. ) ;
#102232 = EDGE_CURVE ( 'NONE', #29869, #65240, #29553, .T. ) ;
#102234 = AXIS2_PLACEMENT_3D ( 'NONE', #53972, #133514, #168836 ) ;
#102233 = FACE_OUTER_BOUND ( 'NONE', #155372, .T. ) ;
#102235 = CIRCLE ( 'NONE', #98141, 0.1000000000000002554 ) ;
#102236 = FACE_OUTER_BOUND ( 'NONE', #257798, .T. ) ;
#102237 = CARTESIAN_POINT ( 'NONE',  ( -23.15000000000000213, -9.599999999988844124, -155.7499999999999716 ) ) ;
#102238 = EDGE_LOOP ( 'NONE', ( #213712, #11033, #132372, #204164 ) ) ;
#102239 = EDGE_LOOP ( 'NONE', ( #146978, #142063, #126150 ) ) ;
#102240 = VECTOR ( 'NONE', #45650, 1000.000000000000000 ) ;
#102241 = CARTESIAN_POINT ( 'NONE',  ( 20.94999999999999929, 85.40000000001158753, -59.62913836187181715 ) ) ;
#102242 = CARTESIAN_POINT ( 'NONE',  ( 20.95000000000005613, 67.85000000001119247, -3.023107484524792277 ) ) ;
#102243 = EDGE_CURVE ( 'NONE', #183810, #109070, #145601, .T. ) ;
#102244 = CARTESIAN_POINT ( 'NONE',  ( -21.05000000000000071, 76.00000000001240608, -174.3231074845243427 ) ) ;
#102245 = CARTESIAN_POINT ( 'NONE',  ( 23.14999999999999858, 5.600000000011153389, -155.0947339810869323 ) ) ;
#102246 = ORIENTED_EDGE ( 'NONE', *, *, #98223, .T. ) ;
#102247 = AXIS2_PLACEMENT_3D ( 'NONE', #147697, #142541, #181691 ) ;
#102249 = AXIS2_PLACEMENT_3D ( 'NONE', #38718, #118245, #84187 ) ;
#102248 = CARTESIAN_POINT ( 'NONE',  ( 20.95496329884391784, 10.56743320610419623, -175.0743099322847911 ) ) ;
#102250 = CARTESIAN_POINT ( 'NONE',  ( 20.53930447207953236, 10.56810606003652708, -207.3387900815227169 ) ) ;
#102251 = TOROIDAL_SURFACE ( 'NONE', #248036, 0.2000000000000000111, 0.1000000000000000056 ) ;
#102252 = CARTESIAN_POINT ( 'NONE',  ( -16.79184697841823848, 9.948761661658393152, -12.65414227060253083 ) ) ;
#102253 = DIRECTION ( 'NONE',  ( 1.000000000000000000, 0.000000000000000000, 0.000000000000000000 ) ) ;
#102254 = CARTESIAN_POINT ( 'NONE',  ( 21.05000000000000071, 56.02567683926420727, -227.9999002286038774 ) ) ;
#102255 = CARTESIAN_POINT ( 'NONE',  ( -22.47071067811865319, 7.720074744509219933, -66.90090754529744288 ) ) ;
#102256 = ORIENTED_EDGE ( 'NONE', *, *, #39419, .F. ) ;
#102258 = ORIENTED_EDGE ( 'NONE', *, *, #104750, .T. ) ;
#102257 = DIRECTION ( 'NONE',  ( -1.000000000000000000, 0.000000000000000000, 0.000000000000000000 ) ) ;
#102259 = VERTEX_POINT ( 'NONE', #50338 ) ;
#102260 = CARTESIAN_POINT ( 'NONE',  ( -21.05000000000000071, 11.60000000001115339, -93.57179676972452853 ) ) ;
#102261 = ORIENTED_EDGE ( 'NONE', *, *, #193584, .T. ) ;
#102262 = EDGE_CURVE ( 'NONE', #168057, #133004, #205876, .T. ) ;
#102263 = CARTESIAN_POINT ( 'NONE',  ( -18.59999999999999787, 74.14897176987119565, -124.8691942151018139 ) ) ;
#102264 = DIRECTION ( 'NONE',  ( 0.000000000000000000, 0.000000000000000000, -1.000000000000000000 ) ) ;
#102265 = EDGE_CURVE ( 'NONE', #254405, #165054, #22549, .T. ) ;
#102266 = CARTESIAN_POINT ( 'NONE',  ( -21.05000000000000071, 62.00000000001146105, -41.45020001490689765 ) ) ;
#102268 = VERTEX_POINT ( 'NONE', #244698 ) ;
#102267 = CIRCLE ( 'NONE', #185515, 11.74999999999999645 ) ;
#102269 = FACE_OUTER_BOUND ( 'NONE', #99442, .T. ) ;
#102270 = CARTESIAN_POINT ( 'NONE',  ( 18.59999999999999432, 74.27191306321800823, -183.1386724793566145 ) ) ;
#102271 = ORIENTED_EDGE ( 'NONE', *, *, #113325, .T. ) ;
#102272 = DIRECTION ( 'NONE',  ( 1.000000000000000000, 0.000000000000000000, 0.000000000000000000 ) ) ;
#102274 = ORIENTED_EDGE ( 'NONE', *, *, #151024, .T. ) ;
#102273 = DIRECTION ( 'NONE',  ( -1.000000000000000000, 0.000000000000000000, 0.000000000000000000 ) ) ;
#102275 = CARTESIAN_POINT ( 'NONE',  ( 20.94999999999999929, 5.500000000011153745, -121.5947339810869465 ) ) ;
#102277 = ADVANCED_FACE ( 'NONE', ( #9954, #169070 ), #45228, .T. ) ;
#102276 = DIRECTION ( 'NONE',  ( 0.000000000000000000, 0.000000000000000000, -1.000000000000000000 ) ) ;
#102278 = AXIS2_PLACEMENT_3D ( 'NONE', #150365, #135900, #194646 ) ;
#102279 = VECTOR ( 'NONE', #168285, 999.9999999999998863 ) ;
#102280 = CIRCLE ( 'NONE', #69024, 0.1000000000000046824 ) ;
#102281 = CIRCLE ( 'NONE', #15422, 0.09999999999998898659 ) ;
#102282 = ORIENTED_EDGE ( 'NONE', *, *, #64909, .T. ) ;
#102283 = CARTESIAN_POINT ( 'NONE',  ( -20.85000000000000142, 17.15380675273576117, -224.5473919504296703 ) ) ;
#102284 = CARTESIAN_POINT ( 'NONE',  ( 21.05563370358598263, 10.72423035585766549, -79.18309081596311216 ) ) ;
#102285 = LINE ( 'NONE', #200147, #247411 ) ;
#102286 = ORIENTED_EDGE ( 'NONE', *, *, #16924, .F. ) ;
#102287 = DIRECTION ( 'NONE',  ( 1.000000000000000000, 0.000000000000000000, 0.000000000000000000 ) ) ;
#102288 = DIRECTION ( 'NONE',  ( 1.000000000000000000, 0.000000000000000000, 0.000000000000000000 ) ) ;
#102289 = DIRECTION ( 'NONE',  ( 0.000000000000000000, 0.000000000000000000, -1.000000000000000000 ) ) ;
#102290 = EDGE_CURVE ( 'NONE', #161272, #177338, #64228, .T. ) ;
#102291 = VERTEX_POINT ( 'NONE', #66072 ) ;
#102292 = CIRCLE ( 'NONE', #144015, 0.09999999999999854838 ) ;
#102293 = ORIENTED_EDGE ( 'NONE', *, *, #236537, .F. ) ;
#102294 = EDGE_CURVE ( 'NONE', #155996, #154183, #122511, .T. ) ;
#102295 = CIRCLE ( 'NONE', #214763, 11.65000000000000036 ) ;
#102296 = EDGE_CURVE ( 'NONE', #89589, #197727, #155830, .T. ) ;
#102297 = EDGE_LOOP ( 'NONE', ( #149703, #1665, #195088, #250865 ) ) ;
#102298 = DIRECTION ( 'NONE',  ( 0.000000000000000000, 0.1455152366551500653, 0.9893560106964507384 ) ) ;
#102299 = DIRECTION ( 'NONE',  ( 0.000000000000000000, 0.000000000000000000, -1.000000000000000000 ) ) ;
#102301 = VERTEX_POINT ( 'NONE', #209431 ) ;
#102300 = CARTESIAN_POINT ( 'NONE',  ( -16.80100426158789872, 9.943150520407289861, -146.6829457528340299 ) ) ;
#102302 = FACE_OUTER_BOUND ( 'NONE', #57519, .T. ) ;
#102303 = SPHERICAL_SURFACE ( 'NONE', #240564, 0.1000000000000000056 ) ;
#102304 = EDGE_CURVE ( 'NONE', #150964, #200908, #189142, .T. ) ;
#102306 = ADVANCED_FACE ( 'NONE', ( #124779 ), #189877, .F. ) ;
#102305 = CARTESIAN_POINT ( 'NONE',  ( -20.94999999999999929, 1.116121084443477685E-11, -36.39999999999999147 ) ) ;
#102307 = CARTESIAN_POINT ( 'NONE',  ( 23.14999999999999503, 11.75000000000000711, -26.48519422934605672 ) ) ;
#102308 = CARTESIAN_POINT ( 'NONE',  ( 22.59999999999999432, 31.79543193779693055, -238.8548925032096122 ) ) ;
#102309 = CARTESIAN_POINT ( 'NONE',  ( 21.05000000000000071, 65.27628289530413497, -69.52310748452438816 ) ) ;
#102311 = ORIENTED_EDGE ( 'NONE', *, *, #84274, .T. ) ;
#102310 = CARTESIAN_POINT ( 'NONE',  ( 18.49999999999999645, -1.835341550213255957, -45.05515129256298223 ) ) ;
#102313 = ORIENTED_EDGE ( 'NONE', *, *, #37160, .T. ) ;
#102312 = DIRECTION ( 'NONE',  ( 1.000000000000000000, -0.000000000000000000, -0.000000000000000000 ) ) ;
#102314 = DIRECTION ( 'NONE',  ( 1.000000000000000000, 0.000000000000000000, -0.000000000000000000 ) ) ;
#102315 = ORIENTED_EDGE ( 'NONE', *, *, #62645, .F. ) ;
#102316 = VERTEX_POINT ( 'NONE', #71233 ) ;
#102317 = LINE ( 'NONE', #125764, #134827 ) ;
#102318 = ADVANCED_FACE ( 'NONE', ( #67364 ), #146872, .F. ) ;
#102319 = CIRCLE ( 'NONE', #156568, 12.87499999999999822 ) ;
#102320 = AXIS2_PLACEMENT_3D ( 'NONE', #233139, #212279, #132742 ) ;
#102321 = EDGE_CURVE ( 'NONE', #75595, #208696, #18440, .T. ) ;
#102322 = CARTESIAN_POINT ( 'NONE',  ( 20.94999999999999929, 71.00000000001199396, -115.4283735034374274 ) ) ;
#102323 = DIRECTION ( 'NONE',  ( -2.952720810173289112E-16, 1.000000000000000000, -0.000000000000000000 ) ) ;
#102324 = CYLINDRICAL_SURFACE ( 'NONE', #117954, 0.1000000000000046685 ) ;
#102325 = EDGE_CURVE ( 'NONE', #242592, #146074, #212025, .T. ) ;
#102326 = CARTESIAN_POINT ( 'NONE',  ( -20.07928932188135107, 11.63760776912483763, -211.1049537763353783 ) ) ;
#102327 = ORIENTED_EDGE ( 'NONE', *, *, #60059, .T. ) ;
#102328 = CYLINDRICAL_SURFACE ( 'NONE', #77118, 0.09999999999998898659 ) ;
#102330 = ORIENTED_EDGE ( 'NONE', *, *, #13753, .T. ) ;
#102329 = EDGE_CURVE ( 'NONE', #200951, #73306, #214269, .T. ) ;
#102331 = VERTEX_POINT ( 'NONE', #115467 ) ;
#102332 = AXIS2_PLACEMENT_3D ( 'NONE', #67358, #28267, #123480 ) ;
#102333 = CIRCLE ( 'NONE', #231018, 0.09999999999999939493 ) ;
#102334 = EDGE_LOOP ( 'NONE', ( #33408, #99237, #130644, #153102 ) ) ;
#102335 = EDGE_CURVE ( 'NONE', #161618, #73607, #193435, .T. ) ;
#102336 = EDGE_CURVE ( 'NONE', #96257, #36482, #135123, .T. ) ;
#102337 = AXIS2_PLACEMENT_3D ( 'NONE', #208121, #46444, #7327 ) ;
#102338 = AXIS2_PLACEMENT_3D ( 'NONE', #106, #100470, #194494 ) ;
#102339 = CARTESIAN_POINT ( 'NONE',  ( 22.39999999999999503, 76.00000000001243450, -177.8138870828977360 ) ) ;
#102340 = CARTESIAN_POINT ( 'NONE',  ( 21.14999999999998082, 87.75000000001237765, -170.0231074845242745 ) ) ;
#102341 = EDGE_CURVE ( 'NONE', #118551, #133788, #197674, .T. ) ;
#102342 = ORIENTED_EDGE ( 'NONE', *, *, #203339, .F. ) ;
#102343 = CARTESIAN_POINT ( 'NONE',  ( -16.93353400591626112, 65.99538760383930480, -149.0904230143190148 ) ) ;
#102344 = ORIENTED_EDGE ( 'NONE', *, *, #253384, .F. ) ;
#102345 = CARTESIAN_POINT ( 'NONE',  ( -12.29659703204452370, 9.355888454513703323, -49.78864289677800770 ) ) ;
#102346 = ORIENTED_EDGE ( 'NONE', *, *, #188029, .T. ) ;
#102347 = EDGE_CURVE ( 'NONE', #142140, #51264, #210173, .T. ) ;
#102348 = DIRECTION ( 'NONE',  ( 0.7071067811865475727, -0.2890913453342130457, 0.6453109281988449464 ) ) ;
#102350 = ORIENTED_EDGE ( 'NONE', *, *, #112382, .F. ) ;
#102349 = EDGE_CURVE ( 'NONE', #105736, #130702, #222598, .T. ) ;
#102351 = LINE ( 'NONE', #159813, #157003 ) ;
#102353 = ORIENTED_EDGE ( 'NONE', *, *, #207502, .T. ) ;
#102352 = CARTESIAN_POINT ( 'NONE',  ( -23.25000000000000000, 1.115600667400684642E-11, -100.5000000000000426 ) ) ;
#102354 = CARTESIAN_POINT ( 'NONE',  ( 21.09546886439536451, 67.12144688699764572, -191.2860136339689632 ) ) ;
#102356 = ORIENTED_EDGE ( 'NONE', *, *, #245029, .F. ) ;
#102355 = VECTOR ( 'NONE', #136370, 1000.000000000000000 ) ;
#102357 = CIRCLE ( 'NONE', #214631, 0.09999999999999609201 ) ;
#102358 = DIRECTION ( 'NONE',  ( 3.265361837132813093E-16, 1.000000000000000000, 6.982962677686266711E-15 ) ) ;
#102359 = EDGE_LOOP ( 'NONE', ( #222713, #170269, #11446 ) ) ;
#102360 = VECTOR ( 'NONE', #56433, 1000.000000000000000 ) ;
#102361 = EDGE_CURVE ( 'NONE', #71546, #110479, #32111, .T. ) ;
#102362 = CARTESIAN_POINT ( 'NONE',  ( -23.25000000000000000, -1.149570369564537842, -108.3159124845020074 ) ) ;
#102363 = CARTESIAN_POINT ( 'NONE',  ( 19.90621891164687440, 64.25000000001250555, -178.6946622066474504 ) ) ;
#102364 = LINE ( 'NONE', #162394, #3696 ) ;
#102365 = CARTESIAN_POINT ( 'NONE',  ( -21.05000000000000071, -11.74999999998884448, -131.0000000000000284 ) ) ;
#102366 = VECTOR ( 'NONE', #151104, 1000.000000000000000 ) ;
#102367 = CIRCLE ( 'NONE', #98268, 0.09999999999999939493 ) ;
#102368 = DIRECTION ( 'NONE',  ( 0.000000000000000000, -0.2128009952263601456, 0.9770955615653316162 ) ) ;
#102369 = DIRECTION ( 'NONE',  ( 1.000000000000000000, 2.312964634635739111E-14, -6.167905692361970542E-14 ) ) ;
#102370 = VERTEX_POINT ( 'NONE', #232879 ) ;
#102371 = LINE ( 'NONE', #145378, #233481 ) ;
#102372 = DIRECTION ( 'NONE',  ( 1.000000000000000000, -0.000000000000000000, -0.000000000000000000 ) ) ;
#102373 = CARTESIAN_POINT ( 'NONE',  ( 21.05000000000000071, 6.257814610487288043, -100.4022097086912311 ) ) ;
#102374 = CARTESIAN_POINT ( 'NONE',  ( 16.27683809663750125, 66.65000000001191438, -93.77310748452437394 ) ) ;
#102375 = VERTEX_POINT ( 'NONE', #37241 ) ;
#102376 = CARTESIAN_POINT ( 'NONE',  ( 20.94983749550516450, 68.01715840423028681, -224.2192812407665201 ) ) ;
#102377 = ORIENTED_EDGE ( 'NONE', *, *, #236833, .F. ) ;
#102378 = CARTESIAN_POINT ( 'NONE',  ( -18.39999999999999858, -7.785976468740645196, -209.8926132507865816 ) ) ;
#102379 = VERTEX_POINT ( 'NONE', #252396 ) ;
#102380 = VECTOR ( 'NONE', #213394, 1000.000000000000000 ) ;
#102381 = CIRCLE ( 'NONE', #114904, 0.09999999999999892308 ) ;
#102382 = DIRECTION ( 'NONE',  ( 0.000000000000000000, -0.9915357197604892647, 0.1298341882519715440 ) ) ;
#102383 = CARTESIAN_POINT ( 'NONE',  ( -20.94999027547553894, 10.29326151435327219, -72.45928225104148623 ) ) ;
#102384 = EDGE_LOOP ( 'NONE', ( #156428, #88806, #214432, #154928 ) ) ;
#102386 = VERTEX_POINT ( 'NONE', #95896 ) ;
#102385 = CARTESIAN_POINT ( 'NONE',  ( -21.05000000000000071, -1.162701749926853712, -41.60000000000000142 ) ) ;
#102387 = CARTESIAN_POINT ( 'NONE',  ( 20.85000000000000142, -1.835859311432481045, -112.0044391687985694 ) ) ;
#102388 = ORIENTED_EDGE ( 'NONE', *, *, #87008, .F. ) ;
#102389 = CIRCLE ( 'NONE', #218948, 0.1000000000000024342 ) ;
#102390 = AXIS2_PLACEMENT_3D ( 'NONE', #189178, #110915, #11846 ) ;
#102391 = FACE_OUTER_BOUND ( 'NONE', #205615, .T. ) ;
#102392 = CARTESIAN_POINT ( 'NONE',  ( -20.94999999999999929, 1.835341550235569663, -179.0551512925629538 ) ) ;
#102393 = VERTEX_POINT ( 'NONE', #16395 ) ;
#102394 = EDGE_LOOP ( 'NONE', ( #173976, #182385, #148936, #99955 ) ) ;
#102395 = EDGE_CURVE ( 'NONE', #166406, #133646, #249682, .T. ) ;
#102396 = CARTESIAN_POINT ( 'NONE',  ( -23.15000000000000213, 4.350000000011156054, -112.8500000000000369 ) ) ;
#102397 = CARTESIAN_POINT ( 'NONE',  ( -16.90202395485622944, 14.18586230441212770, -219.3034790129322289 ) ) ;
#102398 = CARTESIAN_POINT ( 'NONE',  ( -16.87845715379269507, 66.04214188611504710, -123.8993068334654737 ) ) ;
#102399 = ADVANCED_FACE ( 'NONE', ( #55459 ), #108084, .F. ) ;
#102400 = ORIENTED_EDGE ( 'NONE', *, *, #101799, .F. ) ;
#102401 = EDGE_LOOP ( 'NONE', ( #11611, #36979, #48007, #81215 ) ) ;
#102402 = CARTESIAN_POINT ( 'NONE',  ( -23.25000000000000000, 80.78317333349157536, -192.9003134612049166 ) ) ;
#102403 = ADVANCED_FACE ( 'NONE', ( #54207 ), #21230, .T. ) ;
#102404 = ADVANCED_FACE ( 'NONE', ( #180280 ), #134707, .F. ) ;
#102406 = ORIENTED_EDGE ( 'NONE', *, *, #81512, .F. ) ;
#102405 = CARTESIAN_POINT ( 'NONE',  ( 20.94999999999999929, 67.22371710471938400, -90.87310748452436826 ) ) ;
#102407 = AXIS2_PLACEMENT_3D ( 'NONE', #10351, #169449, #91151 ) ;
#102408 = CARTESIAN_POINT ( 'NONE',  ( -22.47071067811865319, 0.000000000000000000, 0.000000000000000000 ) ) ;
#102409 = CARTESIAN_POINT ( 'NONE',  ( -20.05000000000000426, 66.75000000001223555, -148.8731074845244393 ) ) ;
#102410 = VECTOR ( 'NONE', #49820, 1000.000000000000227 ) ;
#102411 = CARTESIAN_POINT ( 'NONE',  ( -22.39999999999999858, 26.06832281015329755, -254.4051978787608732 ) ) ;
#102413 = DIRECTION ( 'NONE',  ( 0.000000000000000000, 0.000000000000000000, -1.000000000000000000 ) ) ;
#102412 = CARTESIAN_POINT ( 'NONE',  ( -16.93230518875208190, 65.99924963859201910, -90.44732913642287997 ) ) ;
#102415 = AXIS2_PLACEMENT_3D ( 'NONE', #192631, #152243, #13998 ) ;
#102414 = CARTESIAN_POINT ( 'NONE',  ( -21.13422380239120457, 76.00000000001219291, -143.0164339993295073 ) ) ;
#102416 = AXIS2_PLACEMENT_3D ( 'NONE', #213036, #55216, #194789 ) ;
#102417 = DIRECTION ( 'NONE',  ( 0.000000000000000000, -0.9908441862701610203, 0.1350103645451807555 ) ) ;
#102418 = DIRECTION ( 'NONE',  ( 1.186688945009010077E-16, -0.9770955615653316162, -0.2128009952263604232 ) ) ;
#102419 = CARTESIAN_POINT ( 'NONE',  ( 22.59999954896768770, -3.233352942053706158, -228.1919768569983660 ) ) ;
#102421 = ORIENTED_EDGE ( 'NONE', *, *, #122282, .F. ) ;
#102420 = VECTOR ( 'NONE', #88280, 1000.000000000000000 ) ;
#102422 = ORIENTED_EDGE ( 'NONE', *, *, #59591, .F. ) ;
#102423 = CARTESIAN_POINT ( 'NONE',  ( 18.49999999999999645, 74.83729825007462466, -195.4231074845243654 ) ) ;
#102424 = ORIENTED_EDGE ( 'NONE', *, *, #172448, .T. ) ;
#102425 = CIRCLE ( 'NONE', #56642, 0.1000000000000066946 ) ;
#102426 = CARTESIAN_POINT ( 'NONE',  ( -20.94999999999999574, 64.37928932189309705, -76.39152413686537102 ) ) ;
#102427 = ORIENTED_EDGE ( 'NONE', *, *, #212464, .F. ) ;
#102428 = CIRCLE ( 'NONE', #223271, 0.1000000000000028644 ) ;
#102429 = SURFACE_STYLE_FILL_AREA ( #240696 ) ;
#102430 = CARTESIAN_POINT ( 'NONE',  ( -21.04999999999999716, 69.69257478044694665, -170.0062876161386782 ) ) ;
#102432 = VERTEX_POINT ( 'NONE', #104550 ) ;
#102431 = ORIENTED_EDGE ( 'NONE', *, *, #184231, .T. ) ;
#102433 = ADVANCED_FACE ( 'NONE', ( #61609 ), #22505, .T. ) ;
#102434 = DIRECTION ( 'NONE',  ( -0.1538461538461546041, 0.4665713331247552942, 0.8710008909598968563 ) ) ;
#102435 = ORIENTED_EDGE ( 'NONE', *, *, #167520, .T. ) ;
#102436 = ORIENTED_EDGE ( 'NONE', *, *, #60324, .T. ) ;
#102437 = DIRECTION ( 'NONE',  ( 1.000000000000000000, 0.000000000000000000, 0.000000000000000000 ) ) ;
#102438 = LINE ( 'NONE', #82872, #225902 ) ;
#102440 = ORIENTED_EDGE ( 'NONE', *, *, #53978, .F. ) ;
#102439 = DIRECTION ( 'NONE',  ( -0.000000000000000000, 1.000000000000000000, 1.734723475976757554E-14 ) ) ;
#102441 = CARTESIAN_POINT ( 'NONE',  ( -22.39999999999999858, 10.80758397488570743, -226.8651660546161111 ) ) ;
#102442 = CARTESIAN_POINT ( 'NONE',  ( 19.83283456528358002, 11.75000000001116263, -158.8499999994178040 ) ) ;
#102444 = ORIENTED_EDGE ( 'NONE', *, *, #220677, .T. ) ;
#102443 = DIRECTION ( 'NONE',  ( 0.000000000000000000, 1.000000000000000000, 0.000000000000000000 ) ) ;
#102445 = CARTESIAN_POINT ( 'NONE',  ( -21.05000000000000071, 1.115653327213047955E-11, -29.20000000000004547 ) ) ;
#102446 = EDGE_LOOP ( 'NONE', ( #50820, #77442, #238761, #122430 ) ) ;
#102447 = CARTESIAN_POINT ( 'NONE',  ( 20.85000000000000142, -1.851617760457748618, -179.1031897196036766 ) ) ;
#102448 = EDGE_CURVE ( 'NONE', #141039, #50377, #201770, .T. ) ;
#102450 = ORIENTED_EDGE ( 'NONE', *, *, #195079, .T. ) ;
#102449 = CARTESIAN_POINT ( 'NONE',  ( 18.54999999999999716, 8.750000000011173285, -79.65000000000004832 ) ) ;
#102451 = CARTESIAN_POINT ( 'NONE',  ( 18.50000324121758055, 10.29307482169091870, -172.9586421466939896 ) ) ;
#102452 = CARTESIAN_POINT ( 'NONE',  ( -12.26136940704872380, 26.51187484352280777, -233.5070971077067838 ) ) ;
#102453 = EDGE_CURVE ( 'NONE', #46648, #56214, #25079, .T. ) ;
#102454 = CARTESIAN_POINT ( 'NONE',  ( 21.05000000000000071, 10.42338541492406279, -74.49205192387015018 ) ) ;
#102455 = EDGE_LOOP ( 'NONE', ( #18174, #241197, #109147 ) ) ;
#102457 = CARTESIAN_POINT ( 'NONE',  ( 20.75572585718142093, 8.882316728412554596, -108.9972583987020442 ) ) ;
#102456 = DIRECTION ( 'NONE',  ( 0.000000000000000000, 0.2128009952263403282, -0.9770955615653358350 ) ) ;
#102458 = CARTESIAN_POINT ( 'NONE',  ( -15.06720934482788188, 66.58230930894875144, -84.88150678775981817 ) ) ;
#102459 = DIRECTION ( 'NONE',  ( -0.000000000000000000, 1.000000000000000000, -1.224646799147352961E-16 ) ) ;
#102460 = TOROIDAL_SURFACE ( 'NONE', #110693, 0.2000000000000000111, 0.1000000000000000056 ) ;
#102461 = CIRCLE ( 'NONE', #248256, 0.1000000000000021844 ) ;
#102463 = FACE_OUTER_BOUND ( 'NONE', #10610, .T. ) ;
#102462 = AXIS2_PLACEMENT_3D ( 'NONE', #233385, #11768, #249087 ) ;
#102464 = EDGE_LOOP ( 'NONE', ( #12816, #75796, #47433 ) ) ;
#102465 = ORIENTED_EDGE ( 'NONE', *, *, #46324, .F. ) ;
#102466 = VERTEX_POINT ( 'NONE', #146267 ) ;
#102467 = EDGE_CURVE ( 'NONE', #29920, #6405, #203689, .T. ) ;
#102468 = FACE_OUTER_BOUND ( 'NONE', #173126, .T. ) ;
#102469 = ORIENTED_EDGE ( 'NONE', *, *, #127329, .T. ) ;
#102470 = LINE ( 'NONE', #24276, #55912 ) ;
#102471 = ORIENTED_EDGE ( 'NONE', *, *, #21088, .F. ) ;
#102472 = CARTESIAN_POINT ( 'NONE',  ( 18.50000000000000000, 85.50000000001233502, -162.9910380878246201 ) ) ;
#102473 = DIRECTION ( 'NONE',  ( 0.000000000000000000, -6.982962677686266711E-15, 1.000000000000000000 ) ) ;
#102474 = EDGE_CURVE ( 'NONE', #90293, #230635, #126955, .T. ) ;
#102475 = EDGE_CURVE ( 'NONE', #163200, #15934, #85219, .T. ) ;
#102476 = ORIENTED_EDGE ( 'NONE', *, *, #211398, .F. ) ;
#102477 = EDGE_CURVE ( 'NONE', #165408, #181106, #147614, .T. ) ;
#102478 = TOROIDAL_SURFACE ( 'NONE', #90034, 0.2000000000000000111, 0.1000000000000000056 ) ;
#102479 = CARTESIAN_POINT ( 'NONE',  ( 14.88075390448864255, 9.431689550535255151, -152.2792900322359912 ) ) ;
#102480 =( LENGTH_UNIT ( ) NAMED_UNIT ( * ) SI_UNIT ( .MILLI., .METRE. ) );
#102481 = VECTOR ( 'NONE', #137155, 1000.000000000000000 ) ;
#102482 = ORIENTED_EDGE ( 'NONE', *, *, #97703, .T. ) ;
#102483 = EDGE_LOOP ( 'NONE', ( #195245, #14409, #3566, #12886, #185896, #100495, #193536, #115053, #61589, #128679, #169935, #119775, #164586, #56239, #140633, #218924 ) ) ;
#102484 = ORIENTED_EDGE ( 'NONE', *, *, #158991, .T. ) ;
#102485 = LINE ( 'NONE', #161223, #104440 ) ;
#102486 = CARTESIAN_POINT ( 'NONE',  ( 22.46250603428203618, 75.97885582387397108, -215.1729705818644334 ) ) ;
#102487 = AXIS2_PLACEMENT_3D ( 'NONE', #224819, #167458, #183152 ) ;
#102488 = CARTESIAN_POINT ( 'NONE',  ( 20.94999999999999929, 0.000000000000000000, -33.50000000000000000 ) ) ;
#102489 = DIRECTION ( 'NONE',  ( 1.000000000000000000, 7.304098846218134667E-16, -0.000000000000000000 ) ) ;
#102490 = CARTESIAN_POINT ( 'NONE',  ( -21.07928932188134041, 61.09751618602744827, -234.2940654522722639 ) ) ;
#102491 = LINE ( 'NONE', #199064, #113598 ) ;
#102492 = EDGE_CURVE ( 'NONE', #209999, #97109, #180939, .T. ) ;
#102494 = DIRECTION ( 'NONE',  ( 1.000000000000000000, 0.000000000000000000, 0.000000000000000000 ) ) ;
#102493 = DIRECTION ( 'NONE',  ( 0.000000000000000000, -0.2128009952263604232, 0.9770955615653316162 ) ) ;
#102495 = CARTESIAN_POINT ( 'NONE',  ( -23.15000000000000213, 7.980037321000002848, -237.6410835587014390 ) ) ;
#102497 = VERTEX_POINT ( 'NONE', #245392 ) ;
#102496 = CARTESIAN_POINT ( 'NONE',  ( -21.05000000000000071, 1.115650877919449575E-11, -205.0999999999999375 ) ) ;
#102498 = CARTESIAN_POINT ( 'NONE',  ( -21.05000000000000071, 1.835341550235567887, -78.65515129256301918 ) ) ;
#102499 = CARTESIAN_POINT ( 'NONE',  ( -20.94999999999999929, 76.00000000001213607, -136.5231074845242745 ) ) ;
#102500 = ORIENTED_EDGE ( 'NONE', *, *, #85816, .T. ) ;
#102501 = DIRECTION ( 'NONE',  ( 0.000000000000000000, 0.2617529984165152257, 0.9651348961777124202 ) ) ;
#102502 = CARTESIAN_POINT ( 'NONE',  ( -21.13614978966382196, 69.50089529817788048, -69.52310748452437394 ) ) ;
#102503 = DIRECTION ( 'NONE',  ( -1.000000000000000000, -3.265361837132813093E-16, 0.000000000000000000 ) ) ;
#102504 = ORIENTED_EDGE ( 'NONE', *, *, #131760, .F. ) ;
#102505 = AXIS2_PLACEMENT_3D ( 'NONE', #166971, #88648, #10434 ) ;
#102506 = CARTESIAN_POINT ( 'NONE',  ( -20.64999999999999858, -4.161311414658873886, -226.0656773515597706 ) ) ;
#102507 = CARTESIAN_POINT ( 'NONE',  ( -23.25000000000000000, 64.35000000001228670, -157.8731074845244393 ) ) ;
#102508 = ORIENTED_EDGE ( 'NONE', *, *, #75087, .T. ) ;
#102509 = VERTEX_POINT ( 'NONE', #141155 ) ;
#102510 = CARTESIAN_POINT ( 'NONE',  ( -21.56666275994540172, -1.480534921131848813, -194.2019862094511780 ) ) ;
#102511 = VERTEX_POINT ( 'NONE', #225789 ) ;
#102512 = CARTESIAN_POINT ( 'NONE',  ( 19.90000000000000213, 5.572646938319268273, 16.50000000000000000 ) ) ;
#102513 = CARTESIAN_POINT ( 'NONE',  ( -18.44204374631832977, -9.491036389587206301, -174.1262012702210598 ) ) ;
#102514 = DIRECTION ( 'NONE',  ( -0.000000000000000000, 1.000000000000000000, -0.000000000000000000 ) ) ;
#102515 = CARTESIAN_POINT ( 'NONE',  ( -15.55912972643740488, 8.490870273573721150, -188.4499999999999886 ) ) ;
#102516 = ORIENTED_EDGE ( 'NONE', *, *, #228592, .F. ) ;
#102517 = DIRECTION ( 'NONE',  ( -1.000000000000000000, 0.000000000000000000, -0.000000000000000000 ) ) ;
#102518 = FACE_OUTER_BOUND ( 'NONE', #29315, .T. ) ;
#102519 = DIRECTION ( 'NONE',  ( 2.710505431213777355E-16, -1.000000000000000000, 0.000000000000000000 ) ) ;
#102520 = CARTESIAN_POINT ( 'NONE',  ( -20.85000000000000142, 17.06838326776700399, -224.6250846885016870 ) ) ;
#102521 = AXIS2_PLACEMENT_3D ( 'NONE', #231526, #55404, #134946 ) ;
#102522 = CIRCLE ( 'NONE', #244021, 0.1000000000000028644 ) ;
#102523 = ADVANCED_FACE ( 'NONE', ( #206258 ), #27655, .F. ) ;
#102524 = VERTEX_POINT ( 'NONE', #240261 ) ;
#102525 = COLOUR_RGB ( '', 0.31764706, 0.68627451, 0.89019608) ;
#102527 = ORIENTED_EDGE ( 'NONE', *, *, #65009, .F. ) ;
#102526 = CARTESIAN_POINT ( 'NONE',  ( 20.94999999999999574, 44.12194005689738674, -258.6913704466671788 ) ) ;
#102528 = CARTESIAN_POINT ( 'NONE',  ( -20.64999999999999858, 46.15118611352045974, -240.5321844900040844 ) ) ;
#102529 = DIRECTION ( 'NONE',  ( 0.000000000000000000, -0.5000000000000209832, -0.8660254037844264952 ) ) ;
#102530 = EDGE_CURVE ( 'NONE', #11158, #89225, #231031, .T. ) ;
#102531 = DIRECTION ( 'NONE',  ( -1.000000000000000000, 0.000000000000000000, 0.000000000000000000 ) ) ;
#102532 = DIRECTION ( 'NONE',  ( 1.000000000000000000, 0.000000000000000000, 0.000000000000000000 ) ) ;
#102533 = DIRECTION ( 'NONE',  ( 0.000000000000000000, 0.000000000000000000, -1.000000000000000000 ) ) ;
#102534 = CARTESIAN_POINT ( 'NONE',  ( -20.64999999999999858, 78.50726470275243685, -228.6618886302502176 ) ) ;
#102535 = ORIENTED_EDGE ( 'NONE', *, *, #81872, .T. ) ;
#102536 = CARTESIAN_POINT ( 'NONE',  ( -16.87036670365548474, 63.08160062417908165, -212.9922606024214531 ) ) ;
#102537 = DIRECTION ( 'NONE',  ( -1.000000000000000000, 0.000000000000000000, 0.000000000000000000 ) ) ;
#102538 = EDGE_CURVE ( 'NONE', #39792, #208354, #143517, .T. ) ;
#102539 = ADVANCED_FACE ( 'NONE', ( #10628 ), #226719, .T. ) ;
#102540 = CARTESIAN_POINT ( 'NONE',  ( -18.59999994787167310, 77.40586390956570995, -241.7326700300080802 ) ) ;
#102541 = CARTESIAN_POINT ( 'NONE',  ( -18.50000000000000000, 68.87972903831429505, -99.36354444268502561 ) ) ;
#102542 = CARTESIAN_POINT ( 'NONE',  ( 20.09999999999999787, 9.750000000011137757, -54.34999999999999432 ) ) ;
#102543 = AXIS2_PLACEMENT_3D ( 'NONE', #225756, #126678, #88809 ) ;
#102544 = CARTESIAN_POINT ( 'NONE',  ( 13.40000000000005898, 67.72071067812984779, -21.02310748452479316 ) ) ;
#102545 = CIRCLE ( 'NONE', #135712, 0.1000000000000032530 ) ;
#102546 = ORIENTED_EDGE ( 'NONE', *, *, #173328, .F. ) ;
#102547 = EDGE_LOOP ( 'NONE', ( #240244, #170537, #78529, #29803 ) ) ;
#102549 = VECTOR ( 'NONE', #28308, 1000.000000000000000 ) ;
#102548 = DIRECTION ( 'NONE',  ( 1.000000000000000000, -2.952720810173289112E-16, -2.061873921506763405E-30 ) ) ;
#102550 = CARTESIAN_POINT ( 'NONE',  ( -21.07928932188134041, 6.162520550847337297, -199.5566553493351307 ) ) ;
#102551 = FACE_OUTER_BOUND ( 'NONE', #117349, .T. ) ;
#102552 = VECTOR ( 'NONE', #168132, 1000.000000000000000 ) ;
#102553 = EDGE_CURVE ( 'NONE', #39887, #201875, #68515, .T. ) ;
#102554 = ORIENTED_EDGE ( 'NONE', *, *, #10457, .F. ) ;
#102555 = CARTESIAN_POINT ( 'NONE',  ( -17.71734398241073549, 65.15764277154767115, -146.7979692315188345 ) ) ;
#102556 = VECTOR ( 'NONE', #131530, 1000.000000000000000 ) ;
#102557 = ADVANCED_FACE ( 'NONE', ( #167162 ), #151435, .F. ) ;
#102558 = AXIS2_PLACEMENT_3D ( 'NONE', #124606, #67193, #183290 ) ;
#102559 = DIRECTION ( 'NONE',  ( -1.000000000000000000, -0.000000000000000000, 0.000000000000000000 ) ) ;
#102560 = FACE_OUTER_BOUND ( 'NONE', #195172, .T. ) ;
#102561 = PRODUCT_RELATED_PRODUCT_CATEGORY ( 'part', '', ( #28562 ) ) ;
#102562 = CARTESIAN_POINT ( 'NONE',  ( 21.05000000000000071, 76.00000000001237765, -170.0231074845243597 ) ) ;
#102563 = AXIS2_PLACEMENT_3D ( 'NONE', #224944, #183273, #144117 ) ;
#102564 = CIRCLE ( 'NONE', #177656, 0.09999999999999939493 ) ;
#102565 = VERTEX_POINT ( 'NONE', #251794 ) ;
#102567 = CIRCLE ( 'NONE', #135907, 12.77499999999998259 ) ;
#102566 = SPHERICAL_SURFACE ( 'NONE', #23547, 0.1000000000000000056 ) ;
#102568 = EDGE_CURVE ( 'NONE', #157387, #234543, #87570, .T. ) ;
#102569 = ORIENTED_EDGE ( 'NONE', *, *, #151110, .T. ) ;
#102570 = EDGE_CURVE ( 'NONE', #210699, #96622, #218504, .T. ) ;
#102571 = CARTESIAN_POINT ( 'NONE',  ( -20.54999999999999716, 85.50000000001232081, -160.1291383618718385 ) ) ;
#102572 = EDGE_CURVE ( 'NONE', #204007, #41070, #139411, .T. ) ;
#102573 = CARTESIAN_POINT ( 'NONE',  ( 21.05000000000000426, -0.03753606328566945483, 6.332272273935667606 ) ) ;
#102574 = CARTESIAN_POINT ( 'NONE',  ( -18.50000000000000000, 9.350000000011156942, -121.8500000000000369 ) ) ;
#102575 = CIRCLE ( 'NONE', #202563, 7.900000000000003908 ) ;
#102576 = FACE_OUTER_BOUND ( 'NONE', #173821, .T. ) ;
#102577 = CARTESIAN_POINT ( 'NONE',  ( 20.94999999999999574, 79.23417978893664326, -236.1056577391152587 ) ) ;
#102578 = DIRECTION ( 'NONE',  ( 1.000000000000000000, 0.000000000000000000, 0.000000000000000000 ) ) ;
#102579 = CARTESIAN_POINT ( 'NONE',  ( -20.64999999999999858, 1.999999999999998224, -20.77537807723789953 ) ) ;
#102580 = DIRECTION ( 'NONE',  ( 0.000000000000000000, -0.1495327102803180597, -0.9887567792719412774 ) ) ;
#102581 = CARTESIAN_POINT ( 'NONE',  ( -21.53752568617674967, 6.786807874515073280, -66.90102553872934266 ) ) ;
#102582 = CYLINDRICAL_SURFACE ( 'NONE', #175544, 0.09999999999999939493 ) ;
#102583 = CARTESIAN_POINT ( 'NONE',  ( -20.85000000000000142, 75.83895117929372987, -170.3072973288845731 ) ) ;
#102584 = AXIS2_PLACEMENT_3D ( 'NONE', #111752, #188712, #75214 ) ;
#102586 = EDGE_CURVE ( 'NONE', #3185, #230388, #32790, .T. ) ;
#102585 = CARTESIAN_POINT ( 'NONE',  ( -21.14999999999999858, 87.75000000001237765, -170.0231074845242745 ) ) ;
#102587 = CARTESIAN_POINT ( 'NONE',  ( 21.05000000000000071, 87.75000000001247713, -173.1231074845242688 ) ) ;
#102588 = CARTESIAN_POINT ( 'NONE',  ( 20.85000000000000142, 6.982009704856448451, -37.19615211825629331 ) ) ;
#102589 = ORIENTED_EDGE ( 'NONE', *, *, #172270, .F. ) ;
#102590 = DIRECTION ( 'NONE',  ( 3.469446951953514477E-14, 0.9999176327611370985, 0.01283462868040226822 ) ) ;
#102591 = DIRECTION ( 'NONE',  ( -1.000000000000000000, 0.000000000000000000, 0.000000000000000000 ) ) ;
#102592 = ORIENTED_EDGE ( 'NONE', *, *, #123253, .T. ) ;
#102593 = LINE ( 'NONE', #123479, #130758 ) ;
#102594 = CARTESIAN_POINT ( 'NONE',  ( 21.05543885634738643, 67.22422895316475433, -157.8387230138097266 ) ) ;
#102595 = CIRCLE ( 'NONE', #152925, 0.1000000000000096922 ) ;
#102596 = CIRCLE ( 'NONE', #219140, 0.1000000000000003386 ) ;
#102597 = ADVANCED_FACE ( 'NONE', ( #112301 ), #111005, .T. ) ;
#102598 = DIRECTION ( 'NONE',  ( -0.000000000000000000, -0.4721928772777346239, -0.8814952561688430555 ) ) ;
#102599 = VERTEX_POINT ( 'NONE', #168467 ) ;
#102601 = AXIS2_PLACEMENT_3D ( 'NONE', #10792, #249410, #31667 ) ;
#102600 = CARTESIAN_POINT ( 'NONE',  ( 20.94999999999999574, 77.16270174995034381, -162.0231074845243313 ) ) ;
#102602 = CARTESIAN_POINT ( 'NONE',  ( -23.25000000000000000, 11.75000000001115552, -93.48519422934610645 ) ) ;
#102603 = AXIS2_PLACEMENT_3D ( 'NONE', #182389, #198081, #121152 ) ;
#102604 = ORIENTED_EDGE ( 'NONE', *, *, #207512, .T. ) ;
#102605 = AXIS2_PLACEMENT_3D ( 'NONE', #17160, #135783, #18417 ) ;
#102606 = VERTEX_POINT ( 'NONE', #53601 ) ;
#102607 = FACE_OUTER_BOUND ( 'NONE', #57213, .T. ) ;
#102608 = ADVANCED_FACE ( 'NONE', ( #208824 ), #152732, .T. ) ;
#102609 =( BOUNDED_SURFACE ( )  B_SPLINE_SURFACE ( 3, 2, ( 
 ( #38428, #94533, #119258 ),
 ( #137502, #136203, #198771 ),
 ( #20158, #217039, #560 ),
 ( #174132, #253603, #134923 ) ),
 .UNSPECIFIED., .F., .F., .T. ) 
 B_SPLINE_SURFACE_WITH_KNOTS ( ( 4, 4 ),
 ( 3, 3 ),
 ( 0.3000847527772381729, 0.5552748953338751958 ),
 ( 0.000000000000000000, 1.000000000000000000 ),
 .UNSPECIFIED. ) 
 GEOMETRIC_REPRESENTATION_ITEM ( )  RATIONAL_B_SPLINE_SURFACE ( (
 ( 1.000000000000000000, 0.9152888060719386321, 1.000000000000000000),
 ( 1.000000000000000000, 0.9104333467450184125, 1.000000000000000000),
 ( 1.000000000000000000, 0.9035312726220658952, 1.000000000000000000),
 ( 1.000000000000000000, 0.8946697475932153809, 1.000000000000000000) ) ) 
 REPRESENTATION_ITEM ( '' )  SURFACE ( )  );
#102610 = ORIENTED_EDGE ( 'NONE', *, *, #210505, .F. ) ;
#102612 = TOROIDAL_SURFACE ( 'NONE', #31778, 0.6000000000000009770, 0.1000000000000000056 ) ;
#102611 = DIRECTION ( 'NONE',  ( 1.000000000000000000, 0.000000000000000000, 0.000000000000000000 ) ) ;
#102613 = DIRECTION ( 'NONE',  ( 1.186688945009010077E-16, -1.000000000000000000, -0.000000000000000000 ) ) ;
#102615 = FACE_OUTER_BOUND ( 'NONE', #28022, .T. ) ;
#102614 = UNCERTAINTY_MEASURE_WITH_UNIT (LENGTH_MEASURE( 1.000000000000000082E-05 ), #58915, 'distance_accuracy_value', 'NONE');
#102616 = EDGE_CURVE ( 'NONE', #221113, #92818, #148863, .T. ) ;
#102617 = DIRECTION ( 'NONE',  ( 0.000000000000000000, 0.1575844902526560010, 0.9875055080513781558 ) ) ;
#102618 = TOROIDAL_SURFACE ( 'NONE', #140049, 0.2000000000000000111, 0.1000000000000000056 ) ;
#102619 = FACE_OUTER_BOUND ( 'NONE', #50863, .T. ) ;
#102620 = CARTESIAN_POINT ( 'NONE',  ( -20.94999999999999929, 11.65000000001115232, -194.2161343370218560 ) ) ;
#102621 = AXIS2_PLACEMENT_3D ( 'NONE', #219314, #18562, #120264 ) ;
#102622 = CARTESIAN_POINT ( 'NONE',  ( 21.05000000000000071, 36.65892442174935439, -249.5511627012433848 ) ) ;
#102623 = FACE_OUTER_BOUND ( 'NONE', #123811, .T. ) ;
#102625 = ORIENTED_EDGE ( 'NONE', *, *, #67546, .T. ) ;
#102624 = CARTESIAN_POINT ( 'NONE',  ( 18.69999999999999929, -10.84999999999999076, 31.50000000000000000 ) ) ;
#102626 = ORIENTED_EDGE ( 'NONE', *, *, #111611, .T. ) ;
#102628 = DIRECTION ( 'NONE',  ( 0.000000000000000000, -1.000000000000000000, -1.224646799147353207E-16 ) ) ;
#102627 = CARTESIAN_POINT ( 'NONE',  ( -19.89999999999999858, 1.350000000000000089, 16.50000000000000000 ) ) ;
#102630 = ORIENTED_EDGE ( 'NONE', *, *, #207593, .F. ) ;
#102629 = CARTESIAN_POINT ( 'NONE',  ( 13.40000000000000036, -8.350000000000004974, 10.95857864376269397 ) ) ;
#102631 = EDGE_LOOP ( 'NONE', ( #202513, #224363, #77981, #41296 ) ) ;
#102632 = CARTESIAN_POINT ( 'NONE',  ( 20.00000000000000355, 5.454087299794355914, 16.60000000000000142 ) ) ;
#102633 = CARTESIAN_POINT ( 'NONE',  ( 18.59999999999996945, 65.66751761918619934, -30.42826094061123854 ) ) ;
#102634 = ADVANCED_FACE ( 'NONE', ( #90133 ), #64417, .T. ) ;
#102635 = EDGE_CURVE ( 'NONE', #96396, #173426, #172314, .T. ) ;
#102636 = CARTESIAN_POINT ( 'NONE',  ( 18.59999999999999432, 0.5876173420563349792, -209.1618981382189588 ) ) ;
#102638 = CARTESIAN_POINT ( 'NONE',  ( -16.94107738177415712, 10.01423928514777728, -79.55000000000005400 ) ) ;
#102637 = CIRCLE ( 'NONE', #69373, 0.09999999999998986089 ) ;
#102639 = PLANE ( 'NONE',  #158227 ) ;
#102640 = DIRECTION ( 'NONE',  ( 0.000000000000000000, -0.07893460099014820708, 0.9968797965484735846 ) ) ;
#102641 = LINE ( 'NONE', #186066, #210235 ) ;
#102642 = EDGE_LOOP ( 'NONE', ( #196755, #94015, #158263, #14328, #228373 ) ) ;
#102643 = VERTEX_POINT ( 'NONE', #73195 ) ;
#102644 = CARTESIAN_POINT ( 'NONE',  ( -20.00857864376270001, 66.85000000001205933, -124.1731074845243512 ) ) ;
#102645 = CIRCLE ( 'NONE', #235955, 11.80000000000000426 ) ;
#102646 = VECTOR ( 'NONE', #245875, 1000.000000000000000 ) ;
#102647 = ORIENTED_EDGE ( 'NONE', *, *, #45806, .T. ) ;
#102648 = CIRCLE ( 'NONE', #32159, 0.1999999999999987899 ) ;
#102650 = DIRECTION ( 'NONE',  ( -0.7071067811865475727, 0.7071067811865475727, 4.937700262164531476E-15 ) ) ;
#102649 = CIRCLE ( 'NONE', #73504, 0.1000000000000028644 ) ;
#102652 = EDGE_CURVE ( 'NONE', #140921, #208514, #189321, .T. ) ;
#102651 = ORIENTED_EDGE ( 'NONE', *, *, #173799, .T. ) ;
#102653 = CARTESIAN_POINT ( 'NONE',  ( -16.87372397896795562, 9.880599536652891146, -154.3507245100357750 ) ) ;
#102654 = CARTESIAN_POINT ( 'NONE',  ( 20.94999999999999929, 55.59258605799641373, -234.6589115948038966 ) ) ;
#102655 = ADVANCED_FACE ( 'NONE', ( #48456 ), #246650, .F. ) ;
#102656 = CARTESIAN_POINT ( 'NONE',  ( 18.49999999999999289, 65.79142135624879018, -44.87310748452439668 ) ) ;
#102657 = CARTESIAN_POINT ( 'NONE',  ( -21.08134388332232589, 75.92418108250575415, -209.8577880650423140 ) ) ;
#102658 = ORIENTED_EDGE ( 'NONE', *, *, #255799, .T. ) ;
#102659 = CARTESIAN_POINT ( 'NONE',  ( -23.25000000000000000, 64.25000000001158185, -57.37310748452440379 ) ) ;
#102660 = ORIENTED_EDGE ( 'NONE', *, *, #215668, .T. ) ;
#102661 = B_SPLINE_CURVE_WITH_KNOTS ( 'NONE', 3,
 ( #181290, #1323, #63887, #143419, #237393, #238671, #80860, #160451, #58720, #39215 ),
 .UNSPECIFIED., .F., .F.,
 ( 4, 3, 3, 4 ),
 ( 0.000000000000000000, 0.0002000000000002785953, 0.001000000000045107602, 0.001967863649472123035 ),
 .UNSPECIFIED. ) ;
#102662 = CARTESIAN_POINT ( 'NONE',  ( 22.47110162079220785, 0.02879741281384913879, -122.3500640633156991 ) ) ;
#102663 = FACE_OUTER_BOUND ( 'NONE', #248797, .T. ) ;
#102664 = ADVANCED_FACE ( 'NONE', ( #68026 ), #8313, .T. ) ;
#102665 = CARTESIAN_POINT ( 'NONE',  ( 23.24999999999999289, 6.650000000011155876, -54.85000000000000142 ) ) ;
#102666 = CIRCLE ( 'NONE', #223492, 0.5000000000000004441 ) ;
#102667 = DIRECTION ( 'NONE',  ( 0.000000000000000000, -0.000000000000000000, 1.000000000000000000 ) ) ;
#102669 = ORIENTED_EDGE ( 'NONE', *, *, #204734, .F. ) ;
#102668 = EDGE_CURVE ( 'NONE', #248715, #190923, #40493, .T. ) ;
#102670 = CIRCLE ( 'NONE', #190205, 0.09999999999998898659 ) ;
#102672 = CARTESIAN_POINT ( 'NONE',  ( -21.14999999999999858, 64.25000000001189449, -96.23924182154622997 ) ) ;
#102671 = AXIS2_PLACEMENT_3D ( 'NONE', #256909, #78308, #198263 ) ;
#102673 = VERTEX_POINT ( 'NONE', #233537 ) ;
#102676 = VERTEX_POINT ( 'NONE', #173602 ) ;
#102675 = CARTESIAN_POINT ( 'NONE',  ( 18.39999999999999858, -9.682403433465241349, -107.1568433774128408 ) ) ;
#102674 = CARTESIAN_POINT ( 'NONE',  ( -22.59066674512268946, 64.25000000001267608, -203.5536116081548244 ) ) ;
#102677 = CARTESIAN_POINT ( 'NONE',  ( 18.59999999999999076, 6.450000000011156587, -144.0170271704400307 ) ) ;
#102678 = VERTEX_POINT ( 'NONE', #74486 ) ;
#102679 = CARTESIAN_POINT ( 'NONE',  ( -21.14999999999999858, 26.06832281015329755, -254.4051978787608732 ) ) ;
#102680 = AXIS2_PLACEMENT_3D ( 'NONE', #216172, #252731, #76666 ) ;
#102681 = ORIENTED_EDGE ( 'NONE', *, *, #95962, .T. ) ;
#102682 = DIRECTION ( 'NONE',  ( 1.000000000000000000, 0.000000000000000000, 0.000000000000000000 ) ) ;
#102683 = EDGE_CURVE ( 'NONE', #137100, #105632, #247579, .T. ) ;
#102684 = LINE ( 'NONE', #182264, #113481 ) ;
#102685 =( BOUNDED_SURFACE ( )  B_SPLINE_SURFACE ( 3, 2, ( 
 ( #206691, #243232, #28083 ),
 ( #207995, #84112, #29380 ),
 ( #108870, #241956, #183278 ),
 ( #142831, #43763, #202831 ),
 ( #24220, #103707, #54031 ),
 ( #31931, #30645, #11057 ) ),
 .UNSPECIFIED., .F., .F., .F. ) 
 B_SPLINE_SURFACE_WITH_KNOTS ( ( 4, 2, 4 ),
 ( 3, 3 ),
 ( 6.719893378901017553E-05, 0.0002757154632485521472, 0.0004842319927080941189 ),
 ( 0.000000000000000000, 1.000000000000000000 ),
 .UNSPECIFIED. ) 
 GEOMETRIC_REPRESENTATION_ITEM ( )  RATIONAL_B_SPLINE_SURFACE ( (
 ( 1.000000000000000000, 0.7250110520819756932, 1.000000000000000000),
 ( 1.000000000000000000, 0.7277932058368639101, 1.000000000000000000),
 ( 1.000000000000000000, 0.7278452872604711521, 1.000000000000000000),
 ( 1.000000000000000000, 0.7221445671562100044, 1.000000000000000000),
 ( 1.000000000000000000, 0.7163662143769800039, 1.000000000000000000),
 ( 1.000000000000000000, 0.7071067811865475727, 1.000000000000000000) ) ) 
 REPRESENTATION_ITEM ( '' )  SURFACE ( )  );
#102686 = ADVANCED_FACE ( 'NONE', ( #95289 ), #174884, .T. ) ;
#102687 = CARTESIAN_POINT ( 'NONE',  ( -18.39999999999999858, -9.519327731081281385, -73.97297637655937308 ) ) ;
#102688 = CARTESIAN_POINT ( 'NONE',  ( -21.05000000000000071, 74.25000000001229239, -158.3535959266227451 ) ) ;
#102689 = ORIENTED_EDGE ( 'NONE', *, *, #193021, .F. ) ;
#102690 = CARTESIAN_POINT ( 'NONE',  ( 20.99999999999999645, 12.21861431488691707, -211.2854491503459826 ) ) ;
#102691 = DIRECTION ( 'NONE',  ( 0.000000000000000000, 0.000000000000000000, 1.000000000000000000 ) ) ;
#102692 = DIRECTION ( 'NONE',  ( -1.000000000000000000, 0.000000000000000000, 0.000000000000000000 ) ) ;
#102693 = AXIS2_PLACEMENT_3D ( 'NONE', #132295, #228844, #34511 ) ;
#102694 = ORIENTED_EDGE ( 'NONE', *, *, #158848, .F. ) ;
#102695 = LINE ( 'NONE', #63591, #242770 ) ;
#102696 = ORIENTED_EDGE ( 'NONE', *, *, #250129, .F. ) ;
#102697 = LINE ( 'NONE', #79293, #14770 ) ;
#102698 = CARTESIAN_POINT ( 'NONE',  ( 21.14999999999999503, 11.75000000001115552, -167.4999999999999716 ) ) ;
#102699 = CARTESIAN_POINT ( 'NONE',  ( 21.05000000000000071, 36.02367271998545561, -235.8812521208699025 ) ) ;
#102701 = ORIENTED_EDGE ( 'NONE', *, *, #112382, .T. ) ;
#102700 = CARTESIAN_POINT ( 'NONE',  ( -40.23850191057533010, 65.35000000001120668, -4.423107484524790856 ) ) ;
#102702 = DIRECTION ( 'NONE',  ( 1.000000000000000000, 0.000000000000000000, 0.000000000000000000 ) ) ;
#102703 = TOROIDAL_SURFACE ( 'NONE', #94528, 2.699999999999999734, 0.1000000000000000056 ) ;
#102704 = DIRECTION ( 'NONE',  ( 0.000000000000000000, 0.000000000000000000, 1.000000000000000000 ) ) ;
#102705 = LINE ( 'NONE', #2333, #237577 ) ;
#102706 = ORIENTED_EDGE ( 'NONE', *, *, #214845, .T. ) ;
#102707 = VECTOR ( 'NONE', #92018, 1000.000000000000000 ) ;
#102708 = DIRECTION ( 'NONE',  ( 0.000000000000000000, 0.000000000000000000, 1.000000000000000000 ) ) ;
#102709 = CARTESIAN_POINT ( 'NONE',  ( -21.05000000000000071, 1.115600667400684642E-11, -100.5000000000000284 ) ) ;
#102710 = ORIENTED_EDGE ( 'NONE', *, *, #97412, .T. ) ;
#102711 = CARTESIAN_POINT ( 'NONE',  ( -20.94999999999999929, 77.36242903720497566, -61.63422623660309796 ) ) ;
#102712 = CIRCLE ( 'NONE', #231945, 0.1000000000000028644 ) ;
#102713 = EDGE_CURVE ( 'NONE', #122621, #210362, #254342, .T. ) ;
#102714 = EDGE_LOOP ( 'NONE', ( #213037, #83238, #71962, #241158, #109618, #147816, #8951, #109899, #10535, #135733 ) ) ;
#102715 =( BOUNDED_CURVE ( )  B_SPLINE_CURVE ( 3, ( #145009, #184142, #165900, #242836 ),
 .UNSPECIFIED., .F., .T. ) 
 B_SPLINE_CURVE_WITH_KNOTS ( ( 4, 4 ),
 ( 0.000000000000000000, 1.570796326794895892 ),
 .UNSPECIFIED. ) 
 CURVE ( )  GEOMETRIC_REPRESENTATION_ITEM ( )  RATIONAL_B_SPLINE_CURVE ( ( 1.000000000000000000, 0.8047378541243652705, 0.8047378541243652705, 1.000000000000000000 ) ) 
 REPRESENTATION_ITEM ( '' )  );
#102716 = PRESENTATION_LAYER_ASSIGNMENT (  '', '', ( #202701 ) ) ;
#102717 = DIRECTION ( 'NONE',  ( 1.000000000000000000, 0.000000000000000000, 0.000000000000000000 ) ) ;
#102718 = ORIENTED_EDGE ( 'NONE', *, *, #109380, .T. ) ;
#102720 = VERTEX_POINT ( 'NONE', #255595 ) ;
#102719 = CARTESIAN_POINT ( 'NONE',  ( 23.14999999999999858, 67.23127455305835554, -235.8551265064784559 ) ) ;
#102723 = ORIENTED_EDGE ( 'NONE', *, *, #173967, .F. ) ;
#102722 = VERTEX_POINT ( 'NONE', #157883 ) ;
#102721 = LINE ( 'NONE', #165293, #1265 ) ;
#102724 = CARTESIAN_POINT ( 'NONE',  ( 21.05000000000000071, 70.60000000001228670, -157.6178414656113205 ) ) ;
#102725 = CARTESIAN_POINT ( 'NONE',  ( -23.15000000000000213, 2.000000000011154189, -187.7753780772378889 ) ) ;
#102726 = DIRECTION ( 'NONE',  ( 1.186688945009009831E-16, 1.000000000000000000, 6.982962677686266711E-15 ) ) ;
#102728 = CARTESIAN_POINT ( 'NONE',  ( -20.94999999999999929, -4.914013037343267776, -233.1828366659746905 ) ) ;
#102727 = CARTESIAN_POINT ( 'NONE',  ( 20.94999999999999929, 46.33035574435032800, -243.0552603638194853 ) ) ;
#102730 = ADVANCED_FACE ( 'NONE', ( #156588 ), #57431, .T. ) ;
#102729 = SPHERICAL_SURFACE ( 'NONE', #157595, 0.1000000000000000056 ) ;
#102731 = VECTOR ( 'NONE', #83618, 1000.000000000000000 ) ;
#102732 = CARTESIAN_POINT ( 'NONE',  ( -18.44085059012131822, 64.48598750652780609, -60.26341280364594155 ) ) ;
#102733 = SPHERICAL_SURFACE ( 'NONE', #172352, 0.1000000000000000056 ) ;
#102735 = DIRECTION ( 'NONE',  ( 1.441126678808781001E-14, -0.9876197685951241256, -0.1568667991644932258 ) ) ;
#102734 = DIRECTION ( 'NONE',  ( 1.000000000000000000, 3.265361837132813093E-16, -0.000000000000000000 ) ) ;
#102736 = AXIS2_PLACEMENT_3D ( 'NONE', #103637, #198907, #39868 ) ;
#102737 = ORIENTED_EDGE ( 'NONE', *, *, #94860, .F. ) ;
#102738 = VERTEX_POINT ( 'NONE', #75741 ) ;
#102740 = FACE_OUTER_BOUND ( 'NONE', #241740, .T. ) ;
#102739 = AXIS2_PLACEMENT_3D ( 'NONE', #203556, #83571, #200991 ) ;
#102742 = ORIENTED_EDGE ( 'NONE', *, *, #47559, .F. ) ;
#102741 = CARTESIAN_POINT ( 'NONE',  ( 21.05000000000000071, 87.65000000001246860, -172.9231074845242802 ) ) ;
#102743 = CIRCLE ( 'NONE', #77607, 11.70000000000000284 ) ;
#102744 = ORIENTED_EDGE ( 'NONE', *, *, #130796, .F. ) ;
#102745 = CARTESIAN_POINT ( 'NONE',  ( -21.00023020733437917, 6.390869245267705168, -6.911788849595090767E-16 ) ) ;
#102746 = ORIENTED_EDGE ( 'NONE', *, *, #40528, .T. ) ;
#102747 = CARTESIAN_POINT ( 'NONE',  ( -23.15000000000000213, 85.00000000001261924, -193.6291383618718385 ) ) ;
#102748 = CIRCLE ( 'NONE', #85997, 0.5999999999999894307 ) ;
#102749 = CIRCLE ( 'NONE', #181891, 0.09999999999999939493 ) ;
#102750 = EDGE_LOOP ( 'NONE', ( #124273, #230725, #28247, #124382 ) ) ;
#102751 = CARTESIAN_POINT ( 'NONE',  ( -21.07928932188134041, 75.90110485435802445, -176.3516241409176644 ) ) ;
#102752 = CYLINDRICAL_SURFACE ( 'NONE', #40699, 0.1000000000000106498 ) ;
#102755 = ORIENTED_EDGE ( 'NONE', *, *, #179759, .F. ) ;
#102754 = ORIENTED_EDGE ( 'NONE', *, *, #11070, .F. ) ;
#102753 = CIRCLE ( 'NONE', #23715, 11.65000000000000036 ) ;
#102756 = VERTEX_POINT ( 'NONE', #216518 ) ;
#102757 = LINE ( 'NONE', #1089, #11355 ) ;
#102758 = AXIS2_PLACEMENT_3D ( 'NONE', #199419, #162863, #2465 ) ;
#102759 = ORIENTED_EDGE ( 'NONE', *, *, #13153, .F. ) ;
#102760 = AXIS2_PLACEMENT_3D ( 'NONE', #42328, #218370, #162291 ) ;
#102761 = VERTEX_POINT ( 'NONE', #193122 ) ;
#102762 = CARTESIAN_POINT ( 'NONE',  ( -20.94999999999999929, 87.48912529308769592, -66.52310748452423184 ) ) ;
#102764 = VERTEX_POINT ( 'NONE', #217780 ) ;
#102763 = CARTESIAN_POINT ( 'NONE',  ( 18.49362639424898447, -9.442604367876999305, -107.2644409335118070 ) ) ;
#102766 = CARTESIAN_POINT ( 'NONE',  ( -20.64999999999999858, 63.56320957583155717, -222.0641766000055668 ) ) ;
#102765 = DIRECTION ( 'NONE',  ( -0.000000000000000000, -0.000000000000000000, 1.000000000000000000 ) ) ;
#102767 = LINE ( 'NONE', #243588, #103412 ) ;
#102768 = DIRECTION ( 'NONE',  ( 7.304098846218134667E-16, 1.000000000000000000, 6.982962677686266711E-15 ) ) ;
#102769 = EDGE_LOOP ( 'NONE', ( #107754, #96948, #11739, #40812 ) ) ;
#102770 = ORIENTED_EDGE ( 'NONE', *, *, #218969, .T. ) ;
#102771 = CARTESIAN_POINT ( 'NONE',  ( -16.88460203013674388, 66.04524099677652771, -149.1572156749861904 ) ) ;
#102772 = CARTESIAN_POINT ( 'NONE',  ( -18.59999999999999787, -1.866714910046153308, -145.7526752462820241 ) ) ;
#102773 = ADVANCED_FACE ( 'NONE', ( #155299 ), #253068, .T. ) ;
#102774 = VECTOR ( 'NONE', #155738, 1000.000000000000000 ) ;
#102775 = ORIENTED_EDGE ( 'NONE', *, *, #233308, .T. ) ;
#102776 = CARTESIAN_POINT ( 'NONE',  ( 21.22070241538126467, 0.09891903054618129965, -27.03005372713038312 ) ) ;
#102777 = LINE ( 'NONE', #1113, #134431 ) ;
#102778 = FACE_OUTER_BOUND ( 'NONE', #165149, .T. ) ;
#102779 = ORIENTED_EDGE ( 'NONE', *, *, #99434, .T. ) ;
#102780 = ORIENTED_EDGE ( 'NONE', *, *, #242099, .F. ) ;
#102781 = EDGE_CURVE ( 'NONE', #37588, #84975, #116155, .T. ) ;
#102782 = DIRECTION ( 'NONE',  ( 1.000000000000000000, 0.000000000000000000, 0.000000000000000000 ) ) ;
#102783 = SPHERICAL_SURFACE ( 'NONE', #119216, 0.1000000000000000056 ) ;
#102784 = ORIENTED_EDGE ( 'NONE', *, *, #29649, .F. ) ;
#102785 = FACE_OUTER_BOUND ( 'NONE', #216247, .T. ) ;
#102786 = ORIENTED_EDGE ( 'NONE', *, *, #40444, .T. ) ;
#102787 = CARTESIAN_POINT ( 'NONE',  ( -18.59999999999999787, 66.85000000001156195, -57.17310748452438673 ) ) ;
#102788 = CARTESIAN_POINT ( 'NONE',  ( 21.05000000000000071, 76.10000000001170406, -76.06376443622556849 ) ) ;
#102790 = DIRECTION ( 'NONE',  ( 1.000000000000000000, 0.000000000000000000, 0.000000000000000000 ) ) ;
#102789 = CARTESIAN_POINT ( 'NONE',  ( -21.14999999999999858, 10.21728496540352182, -227.9671432372868765 ) ) ;
#102791 = EDGE_CURVE ( 'NONE', #52077, #208014, #14741, .T. ) ;
#102792 = AXIS2_PLACEMENT_3D ( 'NONE', #185779, #89237, #52675 ) ;
#102793 = DIRECTION ( 'NONE',  ( 0.000000000000000000, 0.000000000000000000, 1.000000000000000000 ) ) ;
#102794 = AXIS2_PLACEMENT_3D ( 'NONE', #189964, #11323, #150830 ) ;
#102795 = DIRECTION ( 'NONE',  ( 0.000000000000000000, 2.891205793294679805E-16, -1.000000000000000000 ) ) ;
#102796 = CIRCLE ( 'NONE', #248560, 0.3999999999999975797 ) ;
#102797 = AXIS2_PLACEMENT_3D ( 'NONE', #235918, #61141, #81950 ) ;
#102798 = ORIENTED_EDGE ( 'NONE', *, *, #125107, .T. ) ;
#102799 = EDGE_CURVE ( 'NONE', #196143, #35500, #117427, .T. ) ;
#102800 = CARTESIAN_POINT ( 'NONE',  ( 18.54271179734040942, -9.624084290087520088, -207.7409648527003299 ) ) ;
#102801 = VECTOR ( 'NONE', #218859, 1000.000000000000000 ) ;
#102803 = EDGE_LOOP ( 'NONE', ( #195744, #104505, #195728, #82752, #63583 ) ) ;
#102802 = ORIENTED_EDGE ( 'NONE', *, *, #163025, .T. ) ;
#102804 = ORIENTED_EDGE ( 'NONE', *, *, #13309, .F. ) ;
#102805 = VERTEX_POINT ( 'NONE', #198234 ) ;
#102806 = CARTESIAN_POINT ( 'NONE',  ( -16.93658623642909689, 66.01961832835519317, -157.4112047553951754 ) ) ;
#102807 = DIRECTION ( 'NONE',  ( -1.000000000000000000, 0.000000000000000000, 0.000000000000000000 ) ) ;
#102808 = DIRECTION ( 'NONE',  ( 0.000000000000000000, -1.000000000000000000, 0.000000000000000000 ) ) ;
#102809 = DIRECTION ( 'NONE',  ( 0.000000000000000000, -7.124650136758292359E-15, 1.000000000000000000 ) ) ;
#102810 = CARTESIAN_POINT ( 'NONE',  ( -18.59999999999999787, 70.17424292862648372, -198.1782849070719124 ) ) ;
#102811 = ADVANCED_FACE ( 'NONE', ( #154035 ), #106264, .T. ) ;
#102812 = CIRCLE ( 'NONE', #61143, 11.90000000000000391 ) ;
#102814 = CARTESIAN_POINT ( 'NONE',  ( 21.05000000000000071, 59.06404522663466139, -225.9140184048775950 ) ) ;
#102813 = DIRECTION ( 'NONE',  ( -1.000000000000000000, 0.000000000000000000, -0.000000000000000000 ) ) ;
#102816 = ORIENTED_EDGE ( 'NONE', *, *, #186063, .F. ) ;
#102815 = CARTESIAN_POINT ( 'NONE',  ( 18.60000000000000142, 77.44184265367995579, -241.6694879557322508 ) ) ;
#102817 = CARTESIAN_POINT ( 'NONE',  ( -21.07928932188134041, 6.328516656409858498, -167.4011048543453342 ) ) ;
#102818 = EDGE_LOOP ( 'NONE', ( #142139, #113663, #10241, #61586 ) ) ;
#102819 = DIRECTION ( 'NONE',  ( -0.000000000000000000, 0.000000000000000000, 1.000000000000000000 ) ) ;
#102820 = AXIS2_PLACEMENT_3D ( 'NONE', #27471, #71704, #86076 ) ;
#102821 = ORIENTED_EDGE ( 'NONE', *, *, #70519, .F. ) ;
#102822 = ORIENTED_EDGE ( 'NONE', *, *, #112424, .F. ) ;
#102823 = DIRECTION ( 'NONE',  ( -1.000000000000000000, -0.000000000000000000, -0.000000000000000000 ) ) ;
#102824 = AXIS2_PLACEMENT_3D ( 'NONE', #76934, #117355, #196880 ) ;
#102825 = CARTESIAN_POINT ( 'NONE',  ( 21.05000000000000426, 6.413826288812974674, -0.08574093703339950856 ) ) ;
#102826 = DIRECTION ( 'NONE',  ( 0.000000000000000000, 1.000000000000000000, -6.938893903907240999E-14 ) ) ;
#102827 = CARTESIAN_POINT ( 'NONE',  ( 13.88302573338718560, 9.457410944778565920, -82.00008397379008329 ) ) ;
#102828 = CIRCLE ( 'NONE', #249175, 11.79999999999999716 ) ;
#102829 = DIRECTION ( 'NONE',  ( 1.000000000000000000, 7.304098846218133681E-16, 5.311601492717083645E-30 ) ) ;
#102830 = VERTEX_POINT ( 'NONE', #178718 ) ;
#102831 = EDGE_LOOP ( 'NONE', ( #223337, #157417, #144654 ) ) ;
#102832 = CARTESIAN_POINT ( 'NONE',  ( 20.94999999999999574, 43.52285900727589762, -245.0935880436369985 ) ) ;
#102833 = VERTEX_POINT ( 'NONE', #97823 ) ;
#102834 = CARTESIAN_POINT ( 'NONE',  ( 20.85000000000000142, -4.254329952141540971, -236.2118329068272260 ) ) ;
#102835 = CARTESIAN_POINT ( 'NONE',  ( -18.40000000000000213, 64.52132590001208712, -112.2978007008649826 ) ) ;
#102836 = DIRECTION ( 'NONE',  ( 7.589415207398578370E-15, 0.4088369013363281623, -0.9126074666063771490 ) ) ;
#102837 = DIRECTION ( 'NONE',  ( 0.000000000000000000, 0.000000000000000000, 1.000000000000000000 ) ) ;
#102838 = DIRECTION ( 'NONE',  ( 0.000000000000000000, 0.000000000000000000, 1.000000000000000000 ) ) ;
#102839 = DIRECTION ( 'NONE',  ( 1.000000000000000000, 0.000000000000000000, 0.000000000000000000 ) ) ;
#102840 = CYLINDRICAL_SURFACE ( 'NONE', #20668, 0.09999999999998898659 ) ;
#102841 = CARTESIAN_POINT ( 'NONE',  ( 20.85000000000000142, 77.26327546522863088, -28.12124281777790813 ) ) ;
#102842 = CARTESIAN_POINT ( 'NONE',  ( -21.13435531349860241, 6.344986029290462959, -199.6181296949467594 ) ) ;
#102843 = CARTESIAN_POINT ( 'NONE',  ( -18.69999999999999929, 1.212568896937007645, -7.800000000000000711 ) ) ;
#102844 = AXIS2_PLACEMENT_3D ( 'NONE', #23693, #19832, #99319 ) ;
#102846 = CIRCLE ( 'NONE', #161136, 0.9750000000000036415 ) ;
#102845 = DIRECTION ( 'NONE',  ( 0.000000000000000000, -7.056502275159890832E-15, 1.000000000000000000 ) ) ;
#102847 = TOROIDAL_SURFACE ( 'NONE', #48689, 4.099999999999999645, 0.1000000000000000056 ) ;
#102848 = AXIS2_PLACEMENT_3D ( 'NONE', #148066, #12426, #208056 ) ;
#102849 = ADVANCED_FACE ( 'NONE', ( #79558 ), #159146, .T. ) ;
#102850 = ORIENTED_EDGE ( 'NONE', *, *, #77921, .F. ) ;
#102851 = CARTESIAN_POINT ( 'NONE',  ( -18.40000000000000213, 23.63051550414076729, -229.7170656735756324 ) ) ;
#102852 = ORIENTED_EDGE ( 'NONE', *, *, #137499, .T. ) ;
#102853 = EDGE_CURVE ( 'NONE', #208072, #200257, #101673, .T. ) ;
#102854 = CYLINDRICAL_SURFACE ( 'NONE', #83540, 0.09999999999999939493 ) ;
#102855 = DIRECTION ( 'NONE',  ( 0.000000000000000000, 0.8814952561688428334, -0.4721928772777348460 ) ) ;
#102856 = DIRECTION ( 'NONE',  ( 0.000000000000000000, 0.000000000000000000, -1.000000000000000000 ) ) ;
#102857 = ORIENTED_EDGE ( 'NONE', *, *, #127930, .F. ) ;
#102858 = DIRECTION ( 'NONE',  ( -0.000000000000000000, 0.000000000000000000, -1.000000000000000000 ) ) ;
#102860 = VECTOR ( 'NONE', #40716, 1000.000000000000000 ) ;
#102859 = FACE_OUTER_BOUND ( 'NONE', #83509, .T. ) ;
#102861 = EDGE_CURVE ( 'NONE', #257618, #15694, #64582, .T. ) ;
#102862 = CARTESIAN_POINT ( 'NONE',  ( -18.50000000000000000, 11.64999999999999680, 11.75000000000000000 ) ) ;
#102863 = DIRECTION ( 'NONE',  ( 1.000000000000000000, 0.000000000000000000, 0.000000000000000000 ) ) ;
#102864 = AXIS2_PLACEMENT_3D ( 'NONE', #33018, #192061, #172530 ) ;
#102865 = AXIS2_PLACEMENT_3D ( 'NONE', #109945, #150381, #108670 ) ;
#102866 = CYLINDRICAL_SURFACE ( 'NONE', #118139, 0.1000000000000072220 ) ;
#102867 = CARTESIAN_POINT ( 'NONE',  ( 22.19999999999999929, -11.65000000000000036, -15.00000000000000000 ) ) ;
#102868 = FACE_OUTER_BOUND ( 'NONE', #241329, .T. ) ;
#102869 = CIRCLE ( 'NONE', #48721, 0.1000000000000028644 ) ;
#102870 = ORIENTED_EDGE ( 'NONE', *, *, #242159, .T. ) ;
#102871 = CARTESIAN_POINT ( 'NONE',  ( 21.93642651522410603, 68.67283376068634482, -136.5231074845243313 ) ) ;
#102873 = VERTEX_POINT ( 'NONE', #143401 ) ;
#102872 = DIRECTION ( 'NONE',  ( 0.000000000000000000, -0.4721928772777346239, -0.8814952561688430555 ) ) ;
#102874 = CYLINDRICAL_SURFACE ( 'NONE', #71631, 0.9000000000000014655 ) ;
#102875 = EDGE_CURVE ( 'NONE', #176716, #130825, #258051, .T. ) ;
#102876 = DIRECTION ( 'NONE',  ( 1.000000000000000000, -0.000000000000000000, -0.000000000000000000 ) ) ;
#102877 = FACE_OUTER_BOUND ( 'NONE', #238470, .T. ) ;
#102878 = EDGE_LOOP ( 'NONE', ( #29252, #193190, #51845, #194447 ) ) ;
#102879 = FACE_OUTER_BOUND ( 'NONE', #104236, .T. ) ;
#102880 = ADVANCED_FACE ( 'NONE', ( #203384 ), #164571, .T. ) ;
#102881 = CYLINDRICAL_SURFACE ( 'NONE', #63075, 0.09999999999999609201 ) ;
#102882 = ORIENTED_EDGE ( 'NONE', *, *, #43636, .F. ) ;
#102883 = DIRECTION ( 'NONE',  ( 6.938893903907030216E-14, 0.000000000000000000, 1.000000000000000000 ) ) ;
#102884 = DIRECTION ( 'NONE',  ( -1.000000000000000000, -0.000000000000000000, -0.000000000000000000 ) ) ;
#102885 = CIRCLE ( 'NONE', #23833, 0.3999999999999975797 ) ;
#102886 = EDGE_CURVE ( 'NONE', #68571, #49762, #224212, .T. ) ;
#102887 = CARTESIAN_POINT ( 'NONE',  ( -23.25000000000000355, 10.05000000001113847, -87.75000000000005684 ) ) ;
#102888 = ORIENTED_EDGE ( 'NONE', *, *, #181332, .T. ) ;
#102889 = VERTEX_POINT ( 'NONE', #84667 ) ;
#102890 = EDGE_CURVE ( 'NONE', #86338, #118577, #121317, .T. ) ;
#102891 = CARTESIAN_POINT ( 'NONE',  ( 20.94999999999999929, 10.47338541492405461, -74.57865446424858646 ) ) ;
#102892 = EDGE_CURVE ( 'NONE', #75446, #220769, #82115, .T. ) ;
#102893 = AXIS2_PLACEMENT_3D ( 'NONE', #245947, #46440, #6025 ) ;
#102894 = DIRECTION ( 'NONE',  ( 0.000000000000000000, -7.056502275159890043E-15, 1.000000000000000000 ) ) ;
#102895 = CARTESIAN_POINT ( 'NONE',  ( 20.04142135623730070, 11.65000000001115943, -155.3500000000000227 ) ) ;
#102896 = LINE ( 'NONE', #127625, #90364 ) ;
#102897 = CARTESIAN_POINT ( 'NONE',  ( 18.59999999999999787, 23.48572414787547302, -255.8242635727748677 ) ) ;
#102900 = DIRECTION ( 'NONE',  ( 1.000000000000000000, -0.000000000000000000, -0.000000000000000000 ) ) ;
#102899 = AXIS2_PLACEMENT_3D ( 'NONE', #87842, #145257, #147857 ) ;
#102898 = CARTESIAN_POINT ( 'NONE',  ( -16.87683809663752399, 26.68086916408615750, -212.3318337774905160 ) ) ;
#102901 = CYLINDRICAL_SURFACE ( 'NONE', #19550, 0.09999999999999939493 ) ;
#102902 = CARTESIAN_POINT ( 'NONE',  ( -23.15000000000000213, 64.35000000001187459, -90.87310748452438247 ) ) ;
#102903 = LINE ( 'NONE', #145892, #112917 ) ;
#102904 = CARTESIAN_POINT ( 'NONE',  ( 20.94999999999999929, 1.115600667400684642E-11, -134.0000000000000284 ) ) ;
#102905 = TOROIDAL_SURFACE ( 'NONE', #82046, 0.4000000000000003553, 0.1000000000000000056 ) ;
#102906 = ORIENTED_EDGE ( 'NONE', *, *, #185888, .T. ) ;
#102907 = AXIS2_PLACEMENT_3D ( 'NONE', #81270, #180406, #23924 ) ;
#102908 = ORIENTED_EDGE ( 'NONE', *, *, #79480, .F. ) ;
#102909 = CARTESIAN_POINT ( 'NONE',  ( -23.15000000000000213, 71.75000000001205080, -124.2731074845243313 ) ) ;
#102910 = DIRECTION ( 'NONE',  ( 1.000000000000000000, 0.000000000000000000, 0.000000000000000000 ) ) ;
#102912 = CARTESIAN_POINT ( 'NONE',  ( 18.39999999999999503, 30.92555476183550311, -233.4643850126089148 ) ) ;
#102911 = DIRECTION ( 'NONE',  ( -1.000000000000000000, 0.000000000000000000, -0.000000000000000000 ) ) ;
#102913 = EDGE_CURVE ( 'NONE', #132241, #216057, #123071, .T. ) ;
#102914 = AXIS2_PLACEMENT_3D ( 'NONE', #79353, #21982, #141904 ) ;
#102915 = EDGE_CURVE ( 'NONE', #70163, #4833, #243666, .T. ) ;
#102916 = DIRECTION ( 'NONE',  ( 1.296989514748957922E-15, -0.9887567792719341719, 0.1495327102803664099 ) ) ;
#102918 = EDGE_CURVE ( 'NONE', #155020, #231084, #131222, .T. ) ;
#102917 = CARTESIAN_POINT ( 'NONE',  ( 21.05000000000000071, 10.45765418377745526, -207.3040725013013912 ) ) ;
#102919 = CIRCLE ( 'NONE', #131972, 0.2000000000000100586 ) ;
#102920 = PLANE ( 'NONE',  #123279 ) ;
#102921 = VERTEX_POINT ( 'NONE', #140840 ) ;
#102922 = CYLINDRICAL_SURFACE ( 'NONE', #251579, 7.900000000000003908 ) ;
#102923 = ORIENTED_EDGE ( 'NONE', *, *, #125789, .F. ) ;
#102924 = EDGE_CURVE ( 'NONE', #135040, #60684, #147812, .T. ) ;
#102925 = CARTESIAN_POINT ( 'NONE',  ( -14.87770893841227071, 9.430637101696738966, -18.26826061806095325 ) ) ;
#102926 = ORIENTED_EDGE ( 'NONE', *, *, #133395, .T. ) ;
#102927 = CARTESIAN_POINT ( 'NONE',  ( -18.59999999999999787, 43.00579525902548994, -254.2551217332645876 ) ) ;
#102928 = AXIS2_PLACEMENT_3D ( 'NONE', #255520, #251726, #73124 ) ;
#102929 = AXIS2_PLACEMENT_3D ( 'NONE', #102700, #44044, #165269 ) ;
#102930 = CARTESIAN_POINT ( 'NONE',  ( 18.54271179734060127, 85.62408429011018995, -29.28214263182405830 ) ) ;
#102931 = AXIS2_PLACEMENT_3D ( 'NONE', #220553, #143582, #41936 ) ;
#102933 = ORIENTED_EDGE ( 'NONE', *, *, #27489, .F. ) ;
#102932 = MECHANICAL_DESIGN_GEOMETRIC_PRESENTATION_REPRESENTATION (  '', ( #148764 ), #219459 ) ;
#102934 = CARTESIAN_POINT ( 'NONE',  ( -16.95709691156823240, 66.05000000001261640, -190.8630499220105321 ) ) ;
#102935 = VERTEX_POINT ( 'NONE', #61301 ) ;
#102936 = AXIS2_PLACEMENT_3D ( 'NONE', #112640, #236116, #150490 ) ;
#102937 = DIRECTION ( 'NONE',  ( 0.000000000000000000, 0.000000000000000000, 1.000000000000000000 ) ) ;
#102938 = CIRCLE ( 'NONE', #244422, 0.09999999999999543976 ) ;
#102939 = CARTESIAN_POINT ( 'NONE',  ( -21.46681500593007641, 69.14248884062448042, -69.52310748452435973 ) ) ;
#102940 = CYLINDRICAL_SURFACE ( 'NONE', #74215, 0.09999999999999939493 ) ;
#102941 = EDGE_CURVE ( 'NONE', #142313, #55595, #127134, .T. ) ;
#102942 = CARTESIAN_POINT ( 'NONE',  ( -23.15000000000000213, 11.75000000001115552, -93.48519422934610645 ) ) ;
#102943 = CARTESIAN_POINT ( 'NONE',  ( -20.54999999999999716, 68.75000000001223555, -148.8731074845244109 ) ) ;
#102945 = CARTESIAN_POINT ( 'NONE',  ( -21.55000000000000071, 7.350000000011155166, -121.6500000000000341 ) ) ;
#102944 = CARTESIAN_POINT ( 'NONE',  ( -22.16821283564876666, 7.558973340791935058, -134.0000000000000000 ) ) ;
#102946 = DIRECTION ( 'NONE',  ( 0.000000000000000000, 0.000000000000000000, 1.000000000000000000 ) ) ;
#102947 = EDGE_CURVE ( 'NONE', #98142, #166990, #204644, .T. ) ;
#102949 = ORIENTED_EDGE ( 'NONE', *, *, #123914, .F. ) ;
#102948 = CARTESIAN_POINT ( 'NONE',  ( 21.10642757222115407, 65.27684371085399562, -191.2824099607392156 ) ) ;
#102951 = CARTESIAN_POINT ( 'NONE',  ( -14.00000000000000178, 9.850000000011133849, -184.2499999999999716 ) ) ;
#102950 = DIRECTION ( 'NONE',  ( 0.000000000000000000, 0.2617529984165152257, 0.9651348961777124202 ) ) ;
#102952 = VERTEX_POINT ( 'NONE', #22192 ) ;
#102954 = EDGE_LOOP ( 'NONE', ( #134783, #97679, #134667, #91319 ) ) ;
#102953 = DIRECTION ( 'NONE',  ( 0.000000000000000000, 0.8496786552930077896, 0.5273008465188220306 ) ) ;
#102955 = TOROIDAL_SURFACE ( 'NONE', #19600, 1.900000000000002576, 0.1000000000000000056 ) ;
#102956 = ORIENTED_EDGE ( 'NONE', *, *, #77556, .T. ) ;
#102957 = CARTESIAN_POINT ( 'NONE',  ( 18.54999999999999716, 9.949999999999997513, -20.85000000000005471 ) ) ;
#102958 = AXIS2_PLACEMENT_3D ( 'NONE', #178583, #79429, #61169 ) ;
#102959 = DIRECTION ( 'NONE',  ( -1.000000000000000000, -0.000000000000000000, 1.073024830501117725E-15 ) ) ;
#102960 = DIRECTION ( 'NONE',  ( 1.186688945009009831E-16, -1.000000000000000000, 0.000000000000000000 ) ) ;
#102961 = ADVANCED_FACE ( 'NONE', ( #242496 ), #114486, .T. ) ;
#102962 = VERTEX_POINT ( 'NONE', #85962 ) ;
#102963 = EDGE_CURVE ( 'NONE', #189866, #228775, #245069, .T. ) ;
#102964 = DIRECTION ( 'NONE',  ( 1.000000000000000000, 0.000000000000000000, 0.000000000000000000 ) ) ;
#102965 = DIRECTION ( 'NONE',  ( 0.000000000000000000, 0.2128009952263601456, -0.9770955615653316162 ) ) ;
#102966 = ADVANCED_FACE ( 'NONE', ( #66436 ), #62591, .T. ) ;
#102967 = EDGE_LOOP ( 'NONE', ( #217859, #157437, #78965 ) ) ;
#102968 = DIRECTION ( 'NONE',  ( 0.000000000000000000, -6.467318590049456648E-15, 1.000000000000000000 ) ) ;
#102969 = CIRCLE ( 'NONE', #132204, 0.6000000000000015321 ) ;
#102970 = CIRCLE ( 'NONE', #3010, 0.09999999999998898659 ) ;
#102971 = CARTESIAN_POINT ( 'NONE',  ( 23.40000000000005187, 82.84256550613280012, -26.34830530078816935 ) ) ;
#102972 = ORIENTED_EDGE ( 'NONE', *, *, #208054, .T. ) ;
#102973 = EDGE_LOOP ( 'NONE', ( #210861, #162232 ) ) ;
#102974 = EDGE_CURVE ( 'NONE', #152549, #50255, #252032, .T. ) ;
#102975 = ORIENTED_EDGE ( 'NONE', *, *, #35491, .F. ) ;
#102976 = CARTESIAN_POINT ( 'NONE',  ( 22.39999999999999503, 1.115600667400684642E-11, -25.74999999999999645 ) ) ;
#102978 = EDGE_CURVE ( 'NONE', #196419, #191888, #130244, .T. ) ;
#102977 = EDGE_LOOP ( 'NONE', ( #104981, #118748, #129364, #131330 ) ) ;
#102979 = CARTESIAN_POINT ( 'NONE',  ( -18.59999999999999787, 66.65000000001259650, -191.1731074845244223 ) ) ;
#102980 = SPHERICAL_SURFACE ( 'NONE', #202188, 0.1000000000000000056 ) ;
#102981 = DIRECTION ( 'NONE',  ( 0.000000000000000000, 0.1569827930593259702, -0.9876013379310970564 ) ) ;
#102982 = EDGE_CURVE ( 'NONE', #191945, #173788, #231212, .T. ) ;
#102983 = CARTESIAN_POINT ( 'NONE',  ( -21.08198257630413508, 30.84639965801013517, -252.0755024353131830 ) ) ;
#102984 = CARTESIAN_POINT ( 'NONE',  ( 22.57320508075687115, 11.75000000001115552, -33.50000000000000000 ) ) ;
#102985 = ORIENTED_EDGE ( 'NONE', *, *, #155266, .T. ) ;
#102986 = CIRCLE ( 'NONE', #207063, 0.09999999999999939493 ) ;
#102987 = AXIS2_PLACEMENT_3D ( 'NONE', #250596, #188071, #150243 ) ;
#102988 = DIRECTION ( 'NONE',  ( 0.000000000000000000, -6.769652589177784668E-15, 1.000000000000000000 ) ) ;
#102989 = CYLINDRICAL_SURFACE ( 'NONE', #75573, 4.049999999999995381 ) ;
#102990 = CARTESIAN_POINT ( 'NONE',  ( -21.08134388332232589, 0.07581891751813416014, -27.16531941948202444 ) ) ;
#102991 = DIRECTION ( 'NONE',  ( 1.000000000000000000, -0.000000000000000000, -0.000000000000000000 ) ) ;
#102993 = ORIENTED_EDGE ( 'NONE', *, *, #84316, .F. ) ;
#102992 = EDGE_CURVE ( 'NONE', #188456, #227500, #226908, .T. ) ;
#102995 = CARTESIAN_POINT ( 'NONE',  ( 23.14999999999999858, 0.000000000000000000, -33.50000000000000000 ) ) ;
#102994 = DIRECTION ( 'NONE',  ( -1.000000000000000000, 0.000000000000000000, 0.000000000000000000 ) ) ;
#102996 = ORIENTED_EDGE ( 'NONE', *, *, #168433, .T. ) ;
#102999 = ORIENTED_EDGE ( 'NONE', *, *, #32846, .F. ) ;
#102998 = CYLINDRICAL_SURFACE ( 'NONE', #167004, 1.749999999999998002 ) ;
#102997 = LINE ( 'NONE', #101694, #57329 ) ;
#103000 = AXIS2_PLACEMENT_3D ( 'NONE', #157667, #179768, #177217 ) ;
#103001 = EDGE_LOOP ( 'NONE', ( #37592, #64364, #35237, #207592 ) ) ;
#103002 = DIRECTION ( 'NONE',  ( 0.000000000000000000, 0.000000000000000000, 1.000000000000000000 ) ) ;
#103003 = CARTESIAN_POINT ( 'NONE',  ( 20.85000000000000142, 74.34961279258810407, -232.6661986760551315 ) ) ;
#103004 = EDGE_CURVE ( 'NONE', #192577, #257956, #131437, .T. ) ;
#103005 = CARTESIAN_POINT ( 'NONE',  ( 20.99999999999999645, 60.24242455067834356, -224.3755369822736156 ) ) ;
#103006 = VERTEX_POINT ( 'NONE', #92403 ) ;
#103007 = CARTESIAN_POINT ( 'NONE',  ( 19.75857864376269291, 16.64998792410003858, -222.7039835543563981 ) ) ;
#103008 = CARTESIAN_POINT ( 'NONE',  ( 21.15000000000005542, 83.90000000001120384, -34.86056257560453986 ) ) ;
#103009 = EDGE_CURVE ( 'NONE', #247434, #5863, #81310, .T. ) ;
#103011 = DIRECTION ( 'NONE',  ( 0.000000000000000000, -0.4088369013363494231, 0.9126074666063672680 ) ) ;
#103010 = CARTESIAN_POINT ( 'NONE',  ( -21.70464131381649509, 7.095358018979010417, -167.4999999999999716 ) ) ;
#103012 = EDGE_CURVE ( 'NONE', #177267, #50255, #171997, .T. ) ;
#103014 = ORIENTED_EDGE ( 'NONE', *, *, #23722, .F. ) ;
#103013 = LINE ( 'NONE', #180018, #201653 ) ;
#103015 = AXIS2_PLACEMENT_3D ( 'NONE', #252370, #153337, #33383 ) ;
#103016 = VERTEX_POINT ( 'NONE', #49438 ) ;
#103017 = DIRECTION ( 'NONE',  ( 0.000000000000000000, 0.9908441862701596881, -0.1350103645451904977 ) ) ;
#103018 = CARTESIAN_POINT ( 'NONE',  ( 21.05000000000000071, -11.48912529306489994, -164.6000000000000227 ) ) ;
#103019 = AXIS2_PLACEMENT_3D ( 'NONE', #47444, #150441, #164854 ) ;
#103020 = LINE ( 'NONE', #83441, #184149 ) ;
#103021 = ORIENTED_EDGE ( 'NONE', *, *, #12376, .F. ) ;
#103022 = CARTESIAN_POINT ( 'NONE',  ( 20.94999999999999574, 74.16465844978765176, -124.9679561919613207 ) ) ;
#103023 = VERTEX_POINT ( 'NONE', #127700 ) ;
#103024 = CARTESIAN_POINT ( 'NONE',  ( 18.54999999999999716, 67.25000000001156764, -60.27310748452438816 ) ) ;
#103026 = ADVANCED_FACE ( 'NONE', ( #248937 ), #205941, .T. ) ;
#103025 = CARTESIAN_POINT ( 'NONE',  ( -18.59999999999999787, 6.982009704867601307, -104.1961521182563359 ) ) ;
#103027 = DIRECTION ( 'NONE',  ( 0.000000000000000000, 0.3427706569149635007, -0.9394191166662961834 ) ) ;
#103028 = EDGE_LOOP ( 'NONE', ( #234614, #65138 ) ) ;
#103029 = DIRECTION ( 'NONE',  ( 0.000000000000000000, 0.000000000000000000, -1.000000000000000000 ) ) ;
#103030 = EDGE_CURVE ( 'NONE', #48880, #252796, #11612, .T. ) ;
#103031 = AXIS2_PLACEMENT_3D ( 'NONE', #196510, #19162, #178271 ) ;
#103032 = CARTESIAN_POINT ( 'NONE',  ( 23.14999999999999858, 76.00000000001142553, -36.02310748452432421 ) ) ;
#103033 = AXIS2_PLACEMENT_3D ( 'NONE', #84545, #204531, #247521 ) ;
#103034 = ORIENTED_EDGE ( 'NONE', *, *, #244451, .T. ) ;
#103035 = ORIENTED_EDGE ( 'NONE', *, *, #145426, .T. ) ;
#103036 = ORIENTED_EDGE ( 'NONE', *, *, #175401, .T. ) ;
#103037 = CARTESIAN_POINT ( 'NONE',  ( -20.94999999999999929, 87.75000000001192291, -106.1231074845242262 ) ) ;
#103038 = EDGE_CURVE ( 'NONE', #127078, #95921, #46848, .T. ) ;
#103039 = ORIENTED_EDGE ( 'NONE', *, *, #238285, .T. ) ;
#103041 = ORIENTED_EDGE ( 'NONE', *, *, #125729, .T. ) ;
#103040 = DIRECTION ( 'NONE',  ( -0.000000000000000000, 0.000000000000000000, 1.000000000000000000 ) ) ;
#103042 = ORIENTED_EDGE ( 'NONE', *, *, #241327, .T. ) ;
#103045 = ORIENTED_EDGE ( 'NONE', *, *, #78493, .F. ) ;
#103044 = ORIENTED_EDGE ( 'NONE', *, *, #180106, .F. ) ;
#103043 = FACE_OUTER_BOUND ( 'NONE', #253712, .T. ) ;
#103046 = AXIS2_PLACEMENT_3D ( 'NONE', #176151, #54876, #77016 ) ;
#103047 = AXIS2_PLACEMENT_3D ( 'NONE', #163560, #154926, #183133 ) ;
#103048 = ORIENTED_EDGE ( 'NONE', *, *, #132873, .F. ) ;
#103049 = DIRECTION ( 'NONE',  ( 1.000000000000000000, 0.000000000000000000, 0.000000000000000000 ) ) ;
#103050 = EDGE_CURVE ( 'NONE', #194584, #235005, #161392, .T. ) ;
#103051 = DIRECTION ( 'NONE',  ( -3.265361837132813093E-16, 1.000000000000000000, 0.000000000000000000 ) ) ;
#103052 =( BOUNDED_SURFACE ( )  B_SPLINE_SURFACE ( 3, 2, ( 
 ( #118386, #38852, #256540 ),
 ( #177093, #17980, #36292 ),
 ( #213617, #76670, #197900 ),
 ( #134074, #156250, #173270 ),
 ( #174557, #233214, #98767 ),
 ( #115811, #19274, #218735 ) ),
 .UNSPECIFIED., .F., .F., .T. ) 
 B_SPLINE_SURFACE_WITH_KNOTS ( ( 4, 2, 4 ),
 ( 3, 3 ),
 ( 1.570796326794895448, 2.356194490192343505, 3.141592653589791784 ),
 ( 0.000000000000000000, 1.000000000000000000 ),
 .UNSPECIFIED. ) 
 GEOMETRIC_REPRESENTATION_ITEM ( )  RATIONAL_B_SPLINE_SURFACE ( (
 ( 1.000000000000000000, 0.7071067811865475727, 1.000000000000000000),
 ( 1.000000000000000000, 0.6611148371776105481, 1.000000000000000000),
 ( 1.000000000000000000, 0.6092287576700083918, 1.000000000000000000),
 ( 1.000000000000000000, 0.5278258667053740139, 1.000000000000000000),
 ( 1.000000000000000000, 0.4993418825337004874, 1.000000000000000000),
 ( 1.000000000000000000, 0.5000000000000154321, 1.000000000000000000) ) ) 
 REPRESENTATION_ITEM ( '' )  SURFACE ( )  );
#103053 = CARTESIAN_POINT ( 'NONE',  ( -18.44204374631830490, 86.89455847109682907, -199.6122366425948655 ) ) ;
#103054 = ORIENTED_EDGE ( 'NONE', *, *, #185399, .T. ) ;
#103055 = CARTESIAN_POINT ( 'NONE',  ( -23.25000000000000000, -4.356730526971936079, -226.1082375506050539 ) ) ;
#103057 = EDGE_LOOP ( 'NONE', ( #133067, #219748, #209063, #27561 ) ) ;
#103056 = DIRECTION ( 'NONE',  ( -1.000000000000000000, -0.000000000000000000, 0.000000000000000000 ) ) ;
#103058 = CARTESIAN_POINT ( 'NONE',  ( -16.86578989773640913, 14.21741489235582634, -219.3597035475708594 ) ) ;
#103060 = ORIENTED_EDGE ( 'NONE', *, *, #172455, .F. ) ;
#103059 = CARTESIAN_POINT ( 'NONE',  ( 23.14999999999999858, 1.115600667400684642E-11, -67.00000000000004263 ) ) ;
#103061 = ORIENTED_EDGE ( 'NONE', *, *, #253733, .F. ) ;
#103062 = ORIENTED_EDGE ( 'NONE', *, *, #90035, .T. ) ;
#103063 = EDGE_LOOP ( 'NONE', ( #13177, #115928, #152923, #161536 ) ) ;
#103064 = DIRECTION ( 'NONE',  ( -1.000000000000000000, -0.000000000000000000, -0.000000000000000000 ) ) ;
#103065 = CARTESIAN_POINT ( 'NONE',  ( -23.25000000000000000, 76.00000000001195133, -103.0231074845243171 ) ) ;
#103066 = AXIS2_PLACEMENT_3D ( 'NONE', #118878, #26192, #86118 ) ;
#103067 = CIRCLE ( 'NONE', #11530, 0.1000000000000013933 ) ;
#103069 = VERTEX_POINT ( 'NONE', #207246 ) ;
#103068 = EDGE_LOOP ( 'NONE', ( #37370, #172397, #79252, #143375 ) ) ;
#103070 = ORIENTED_EDGE ( 'NONE', *, *, #203386, .F. ) ;
#103071 = DIRECTION ( 'NONE',  ( 2.952720810173288619E-16, -0.4721928772777346239, -0.8814952561688430555 ) ) ;
#103072 = ORIENTED_EDGE ( 'NONE', *, *, #218763, .F. ) ;
#103073 = ORIENTED_EDGE ( 'NONE', *, *, #212820, .T. ) ;
#103074 = CARTESIAN_POINT ( 'NONE',  ( 21.05000000000000071, 65.27628289530443340, -103.0231074845243882 ) ) ;
#103076 = ORIENTED_EDGE ( 'NONE', *, *, #1262, .T. ) ;
#103075 = CARTESIAN_POINT ( 'NONE',  ( -20.64999999999999858, 2.499999999999998668, -20.27537807723789953 ) ) ;
#103077 = CYLINDRICAL_SURFACE ( 'NONE', #156442, 0.09999999999999939493 ) ;
#103078 = VECTOR ( 'NONE', #235345, 1000.000000000000000 ) ;
#103080 = DIRECTION ( 'NONE',  ( 1.000000000000000000, 0.000000000000000000, 0.000000000000000000 ) ) ;
#103079 = CARTESIAN_POINT ( 'NONE',  ( -16.94333152886236959, 22.96006607477043104, -230.8796551298197528 ) ) ;
#103081 = VERTEX_POINT ( 'NONE', #246359 ) ;
#103082 = EDGE_CURVE ( 'NONE', #172562, #114431, #149840, .T. ) ;
#103084 = ORIENTED_EDGE ( 'NONE', *, *, #91757, .F. ) ;
#103083 = ORIENTED_EDGE ( 'NONE', *, *, #256079, .F. ) ;
#103085 = AXIS2_PLACEMENT_3D ( 'NONE', #14474, #70601, #90110 ) ;
#103086 = SPHERICAL_SURFACE ( 'NONE', #227632, 0.1000000000000000056 ) ;
#103087 = CARTESIAN_POINT ( 'NONE',  ( -18.59999999999999787, 11.75000000000000000, 31.50000000000000000 ) ) ;
#103088 = ORIENTED_EDGE ( 'NONE', *, *, #178913, .F. ) ;
#103089 = CIRCLE ( 'NONE', #57305, 0.5000000000000007772 ) ;
#103090 = AXIS2_PLACEMENT_3D ( 'NONE', #231753, #73985, #132646 ) ;
#103091 = AXIS2_PLACEMENT_3D ( 'NONE', #21835, #24424, #162633 ) ;
#103092 = DIRECTION ( 'NONE',  ( 1.000000000000000000, 0.000000000000000000, 0.000000000000000000 ) ) ;
#103093 = CIRCLE ( 'NONE', #119906, 0.1000000000000028644 ) ;
#103094 = ORIENTED_EDGE ( 'NONE', *, *, #140030, .T. ) ;
#103095 = EDGE_LOOP ( 'NONE', ( #44039, #157981, #166285, #257262 ) ) ;
#103096 = ADVANCED_FACE ( 'NONE', ( #109394 ), #6329, .F. ) ;
#103097 = DIRECTION ( 'NONE',  ( 1.000000000000000000, -0.000000000000000000, -0.000000000000000000 ) ) ;
#103098 = AXIS2_PLACEMENT_3D ( 'NONE', #222450, #243317, #28166 ) ;
#103099 = ORIENTED_EDGE ( 'NONE', *, *, #90468, .T. ) ;
#103100 = DIRECTION ( 'NONE',  ( 0.000000000000000000, 0.9394191166662619885, 0.3427706569150576477 ) ) ;
#103101 = FACE_OUTER_BOUND ( 'NONE', #32113, .T. ) ;
#103102 = EDGE_LOOP ( 'NONE', ( #190684, #187431, #160937, #10399 ) ) ;
#103103 = DIRECTION ( 'NONE',  ( 0.000000000000000000, 0.8814952561688429444, -0.4721928772777348460 ) ) ;
#103104 = DIRECTION ( 'NONE',  ( 0.000000000000000000, 0.000000000000000000, 1.000000000000000000 ) ) ;
#103106 = CARTESIAN_POINT ( 'NONE',  ( -16.87683809663752399, 9.865889849343686180, -120.7325731929305732 ) ) ;
#103105 = DIRECTION ( 'NONE',  ( 1.000000000000000000, -7.304098846218163263E-16, 4.217023435051626718E-16 ) ) ;
#103107 = EDGE_CURVE ( 'NONE', #200766, #255325, #230652, .T. ) ;
#103108 = CARTESIAN_POINT ( 'NONE',  ( -21.05000000000000071, 76.00000000001244871, -170.0231074845243597 ) ) ;
#103109 = CARTESIAN_POINT ( 'NONE',  ( -22.39999999999999858, 76.00000000001267608, -203.5231074845243597 ) ) ;
#103110 = CARTESIAN_POINT ( 'NONE',  ( 21.72449340488910252, 40.89608266988597052, -236.3842060787925163 ) ) ;
#103111 = DIRECTION ( 'NONE',  ( 0.000000000000000000, 0.000000000000000000, -1.000000000000000000 ) ) ;
#103112 = DIRECTION ( 'NONE',  ( -1.836970198721029441E-16, 0.4721928772777346239, 0.8814952561688430555 ) ) ;
#103114 = ADVANCED_FACE ( 'NONE', ( #51983 ), #131536, .F. ) ;
#103113 = AXIS2_PLACEMENT_3D ( 'NONE', #187613, #29835, #31129 ) ;
#103115 = ORIENTED_EDGE ( 'NONE', *, *, #102121, .T. ) ;
#103116 = VECTOR ( 'NONE', #12340, 1000.000000000000000 ) ;
#103117 = EDGE_CURVE ( 'NONE', #14587, #22794, #10443, .T. ) ;
#103120 = ORIENTED_EDGE ( 'NONE', *, *, #177970, .T. ) ;
#103119 = ORIENTED_EDGE ( 'NONE', *, *, #86502, .F. ) ;
#103118 = CIRCLE ( 'NONE', #61446, 0.4999999999999970024 ) ;
#103121 = EDGE_LOOP ( 'NONE', ( #170371, #64284, #117666, #235225 ) ) ;
#103122 = AXIS2_PLACEMENT_3D ( 'NONE', #8156, #242900, #227186 ) ;
#103123 = EDGE_CURVE ( 'NONE', #253828, #224235, #135314, .T. ) ;
#103124 = VECTOR ( 'NONE', #73212, 1000.000000000000000 ) ;
#103125 = CARTESIAN_POINT ( 'NONE',  ( 23.25000000000000000, -8.999999999988844479, -76.89396912265249284 ) ) ;
#103126 = DIRECTION ( 'NONE',  ( 1.000000000000000000, 0.000000000000000000, 0.000000000000000000 ) ) ;
#103127 = ADVANCED_FACE ( 'NONE', ( #53292 ), #38872, .T. ) ;
#103129 = CARTESIAN_POINT ( 'NONE',  ( -13.12432614554022869, 9.430764995422318719, -15.23053739475045987 ) ) ;
#103128 = FACE_OUTER_BOUND ( 'NONE', #98829, .T. ) ;
#103130 = CARTESIAN_POINT ( 'NONE',  ( -21.08198257630413508, 75.92735667622760332, -142.8597042185393491 ) ) ;
#103131 = ORIENTED_EDGE ( 'NONE', *, *, #34362, .T. ) ;
#103132 = CARTESIAN_POINT ( 'NONE',  ( -20.94999675878240808, 10.29307482169070909, -105.9586421466940749 ) ) ;
#103133 = DIRECTION ( 'NONE',  ( -1.000000000000000000, -7.125593699324843413E-30, 1.020425574104004196E-15 ) ) ;
#103134 = EDGE_CURVE ( 'NONE', #75338, #71516, #77966, .T. ) ;
#103135 = DIRECTION ( 'NONE',  ( 0.000000000000000000, -0.2617529984165152257, -0.9651348961777124202 ) ) ;
#103136 = CARTESIAN_POINT ( 'NONE',  ( -16.93935632781549572, 9.984730499736244269, -87.88966074871035516 ) ) ;
#103137 = ORIENTED_EDGE ( 'NONE', *, *, #197969, .T. ) ;
#103138 = CIRCLE ( 'NONE', #248917, 4.299999999999970512 ) ;
#103139 = CIRCLE ( 'NONE', #90672, 0.2000000000000057288 ) ;
#103140 = AXIS2_PLACEMENT_3D ( 'NONE', #132387, #30746, #253597 ) ;
#103141 = CYLINDRICAL_SURFACE ( 'NONE', #1379, 0.1000000000000072220 ) ;
#103142 = ORIENTED_EDGE ( 'NONE', *, *, #177165, .T. ) ;
#103143 = CARTESIAN_POINT ( 'NONE',  ( -16.87331047859651179, 66.05000000001157900, -56.87310748452438958 ) ) ;
#103144 = DIRECTION ( 'NONE',  ( 0.000000000000000000, -6.938893903907222067E-15, 1.000000000000000000 ) ) ;
#103145 = CARTESIAN_POINT ( 'NONE',  ( 21.05000000000000071, 77.36087058720413268, -128.4501095574333362 ) ) ;
#103146 = CARTESIAN_POINT ( 'NONE',  ( 18.39999999999997371, 20.83093076766827423, -227.7429161672744442 ) ) ;
#103147 = DIRECTION ( 'NONE',  ( -1.000000000000000000, 0.000000000000000000, -0.000000000000000000 ) ) ;
#103148 = ORIENTED_EDGE ( 'NONE', *, *, #144397, .F. ) ;
#103149 = DIRECTION ( 'NONE',  ( 0.000000000000000000, -1.000000000000000000, 0.000000000000000000 ) ) ;
#103150 = CARTESIAN_POINT ( 'NONE',  ( 21.72449340488910607, 65.71604372252096482, -127.2731074845243597 ) ) ;
#103152 = EDGE_CURVE ( 'NONE', #199664, #121900, #137937, .T. ) ;
#103151 = CARTESIAN_POINT ( 'NONE',  ( 20.95429693346633471, 11.91077973133057277, -206.1440789982873127 ) ) ;
#103153 = VECTOR ( 'NONE', #158993, 1000.000000000000000 ) ;
#103155 = DIRECTION ( 'NONE',  ( 0.000000000000000000, 0.9915357197604971473, -0.1298341882519111479 ) ) ;
#103154 = DIRECTION ( 'NONE',  ( -1.000000000000000000, 0.000000000000000000, 0.000000000000000000 ) ) ;
#103156 = CARTESIAN_POINT ( 'NONE',  ( 20.12500000000000000, 66.25000000001263345, -195.4113362024101548 ) ) ;
#103157 = CIRCLE ( 'NONE', #153277, 0.1000000000000024342 ) ;
#103158 = DIRECTION ( 'NONE',  ( 0.000000000000000000, 0.2617529984165039569, 0.9651348961777155289 ) ) ;
#103159 = LINE ( 'NONE', #143588, #134776 ) ;
#103161 = CARTESIAN_POINT ( 'NONE',  ( -20.54999999999999716, -9.499999999988848032, -76.89396912265249284 ) ) ;
#103160 = AXIS2_PLACEMENT_3D ( 'NONE', #22750, #124404, #167400 ) ;
#103163 = VERTEX_POINT ( 'NONE', #235761 ) ;
#103162 = DIRECTION ( 'NONE',  ( 0.7071067811865475727, -0.7071067811865475727, -4.937700262164531476E-15 ) ) ;
#103164 = ORIENTED_EDGE ( 'NONE', *, *, #32463, .F. ) ;
#103165 = EDGE_CURVE ( 'NONE', #181798, #238125, #189506, .T. ) ;
#103166 = AXIS2_PLACEMENT_3D ( 'NONE', #204091, #163703, #85398 ) ;
#103167 = DIRECTION ( 'NONE',  ( -1.000000000000000000, 0.000000000000000000, -0.000000000000000000 ) ) ;
#103168 = VECTOR ( 'NONE', #67580, 1000.000000000000000 ) ;
#103169 = AXIS2_PLACEMENT_3D ( 'NONE', #137472, #100884, #80045 ) ;
#103170 = DIRECTION ( 'NONE',  ( -1.000000000000000000, -3.265361837132813093E-16, 0.000000000000000000 ) ) ;
#103171 = TOROIDAL_SURFACE ( 'NONE', #140797, 11.65000000000000036, 0.1000000000000000056 ) ;
#103172 = ADVANCED_FACE ( 'NONE', ( #94972 ), #255278, .T. ) ;
#103173 = CARTESIAN_POINT ( 'NONE',  ( 12.25000000000000000, 9.350000000011140955, -150.7500000000000284 ) ) ;
#103174 = VERTEX_POINT ( 'NONE', #135374 ) ;
#103175 = VECTOR ( 'NONE', #234265, 1000.000000000000000 ) ;
#103176 = EDGE_CURVE ( 'NONE', #234175, #236406, #31320, .T. ) ;
#103177 = CYLINDRICAL_SURFACE ( 'NONE', #16103, 0.1000000000000124678 ) ;
#103178 = CARTESIAN_POINT ( 'NONE',  ( -20.99142135623731065, 11.59999999999999787, -26.57179676972450011 ) ) ;
#103179 = ORIENTED_EDGE ( 'NONE', *, *, #52697, .T. ) ;
#103180 = SPHERICAL_SURFACE ( 'NONE', #12240, 0.1000000000000000056 ) ;
#103182 = ORIENTED_EDGE ( 'NONE', *, *, #6043, .F. ) ;
#103181 = DIRECTION ( 'NONE',  ( 0.000000000000000000, -0.3488585713686133682, -0.9371753822965315228 ) ) ;
#103184 = FACE_OUTER_BOUND ( 'NONE', #76818, .T. ) ;
#103183 = DIRECTION ( 'NONE',  ( -0.000000000000000000, -0.000000000000000000, -1.000000000000000000 ) ) ;
#103185 = EDGE_CURVE ( 'NONE', #207918, #13818, #252202, .T. ) ;
#103186 = LINE ( 'NONE', #219296, #83519 ) ;
#103187 = ORIENTED_EDGE ( 'NONE', *, *, #225224, .F. ) ;
#103188 = TOROIDAL_SURFACE ( 'NONE', #49036, 0.2000000000000000111, 0.1000000000000000056 ) ;
#103189 = ADVANCED_FACE ( 'NONE', ( #118405 ), #177114, .F. ) ;
#103190 = DIRECTION ( 'NONE',  ( 1.000000000000000000, 0.000000000000000000, 0.000000000000000000 ) ) ;
#103191 = CYLINDRICAL_SURFACE ( 'NONE', #196168, 0.09999999999999939493 ) ;
#103192 = EDGE_CURVE ( 'NONE', #5925, #87825, #73194, .T. ) ;
#103193 = FACE_OUTER_BOUND ( 'NONE', #132608, .T. ) ;
#103194 = ORIENTED_EDGE ( 'NONE', *, *, #103134, .T. ) ;
#103195 = AXIS2_PLACEMENT_3D ( 'NONE', #107129, #68008, #45877 ) ;
#103196 = CARTESIAN_POINT ( 'NONE',  ( -20.64999999999999858, 7.150000000011155876, -45.75000000000000000 ) ) ;
#103197 = EDGE_CURVE ( 'NONE', #9387, #96528, #156271, .T. ) ;
#103198 = FACE_OUTER_BOUND ( 'NONE', #89939, .T. ) ;
#103199 = CARTESIAN_POINT ( 'NONE',  ( -22.49510344025093644, 0.06712767820541534758, -122.3500298948857647 ) ) ;
#103200 = ORIENTED_EDGE ( 'NONE', *, *, #31243, .F. ) ;
#103201 = VERTEX_POINT ( 'NONE', #136656 ) ;
#103202 = CARTESIAN_POINT ( 'NONE',  ( 22.59999999999999432, 75.89914163091302157, -81.27267460801373034 ) ) ;
#103203 = FACE_OUTER_BOUND ( 'NONE', #68632, .T. ) ;
#103204 = DIRECTION ( 'NONE',  ( 4.408576920032447355E-17, -0.1350103645451876666, -0.9908441862701600211 ) ) ;
#103205 = CARTESIAN_POINT ( 'NONE',  ( 21.05000000000000071, -12.41227409413852811, -97.50000000000004263 ) ) ;
#103206 = DIRECTION ( 'NONE',  ( -0.000000000000000000, 0.000000000000000000, 1.000000000000000000 ) ) ;
#103208 = CARTESIAN_POINT ( 'NONE',  ( -22.59999999999999787, 31.79543193779693055, -238.8548925032096122 ) ) ;
#103207 = DIRECTION ( 'NONE',  ( 0.000000000000000000, -0.4999999999999949485, 0.8660254037844415942 ) ) ;
#103209 = TOROIDAL_SURFACE ( 'NONE', #236498, 0.2000000000000000111, 0.1000000000000000056 ) ;
#103210 = SPHERICAL_SURFACE ( 'NONE', #106824, 0.1000000000000000056 ) ;
#103211 = CARTESIAN_POINT ( 'NONE',  ( -16.80468759584937288, 66.05784632487743124, -56.83308861832274772 ) ) ;
#103212 = CIRCLE ( 'NONE', #90743, 11.75000000000000000 ) ;
#103213 = CARTESIAN_POINT ( 'NONE',  ( 22.50046968638157807, 75.95483015287236128, -148.2731526389930252 ) ) ;
#103214 = ORIENTED_EDGE ( 'NONE', *, *, #111204, .F. ) ;
#103215 = FACE_OUTER_BOUND ( 'NONE', #128058, .T. ) ;
#103217 = EDGE_LOOP ( 'NONE', ( #118291, #166760, #157958 ) ) ;
#103216 = CARTESIAN_POINT ( 'NONE',  ( -21.05000000000000071, 36.65892442174472876, -249.5511627012454596 ) ) ;
#103218 = CARTESIAN_POINT ( 'NONE',  ( 23.14999999999999503, 64.25000000001276135, -215.2731074845244450 ) ) ;
#103219 = DIRECTION ( 'NONE',  ( 0.000000000000000000, 0.000000000000000000, -1.000000000000000000 ) ) ;
#103221 = DIRECTION ( 'NONE',  ( 0.000000000000000000, 0.000000000000000000, -1.000000000000000000 ) ) ;
#103220 = DIRECTION ( 'NONE',  ( -1.000000000000000000, -0.000000000000000000, -0.000000000000000000 ) ) ;
#103222 = EDGE_CURVE ( 'NONE', #238413, #237228, #143876, .T. ) ;
#103223 = EDGE_LOOP ( 'NONE', ( #12296, #245723, #240050, #140917 ) ) ;
#103225 = LINE ( 'NONE', #58952, #92587 ) ;
#103224 = CARTESIAN_POINT ( 'NONE',  ( -16.89155683852344936, 66.05000000001156479, -56.24573563498483963 ) ) ;
#103227 = EDGE_CURVE ( 'NONE', #111464, #96293, #192809, .T. ) ;
#103226 = CARTESIAN_POINT ( 'NONE',  ( 18.59999999999999432, -1.299733671230788756, 9.971870477130599042 ) ) ;
#103228 = DIRECTION ( 'NONE',  ( 1.000000000000000000, 0.000000000000000000, 0.000000000000000000 ) ) ;
#103229 = CARTESIAN_POINT ( 'NONE',  ( 20.94999999999999929, 1.115600667400684642E-11, -67.00000000000000000 ) ) ;
#103230 = DIRECTION ( 'NONE',  ( 0.000000000000000000, 0.000000000000000000, 1.000000000000000000 ) ) ;
#103231 = ORIENTED_EDGE ( 'NONE', *, *, #225261, .T. ) ;
#103232 = ORIENTED_EDGE ( 'NONE', *, *, #235663, .F. ) ;
#103233 = CIRCLE ( 'NONE', #249015, 0.9750000000000036415 ) ;
#103234 = EDGE_CURVE ( 'NONE', #31271, #137759, #246437, .T. ) ;
#103235 = CARTESIAN_POINT ( 'NONE',  ( -21.05000000000000071, 1.835341550235567887, -78.65515129256301918 ) ) ;
#103236 = ORIENTED_EDGE ( 'NONE', *, *, #245113, .T. ) ;
#103237 = FACE_OUTER_BOUND ( 'NONE', #32311, .T. ) ;
#103238 = ORIENTED_EDGE ( 'NONE', *, *, #178307, .F. ) ;
#103240 = PLANE ( 'NONE',  #135257 ) ;
#103239 = AXIS2_PLACEMENT_3D ( 'NONE', #187796, #20051, #219502 ) ;
#103241 = PLANE ( 'NONE',  #38824 ) ;
#103242 = ORIENTED_EDGE ( 'NONE', *, *, #214338, .F. ) ;
#103243 = CARTESIAN_POINT ( 'NONE',  ( -22.39999999999999858, -2.479040261793999722, -189.6172560698084624 ) ) ;
#103244 = DIRECTION ( 'NONE',  ( -0.7071067811865474617, 0.7071067811865474617, 5.142139384388980375E-15 ) ) ;
#103245 = CARTESIAN_POINT ( 'NONE',  ( 20.87155475150661132, 11.75000000001115907, -160.5955865291576572 ) ) ;
#103246 = CARTESIAN_POINT ( 'NONE',  ( -20.94999999999999929, 0.000000000000000000, -33.50000000000000000 ) ) ;
#103247 = DIRECTION ( 'NONE',  ( 0.000000000000000000, 0.2128009952263268945, -0.9770955615653388326 ) ) ;
#103248 = CARTESIAN_POINT ( 'NONE',  ( 22.49999999999999645, 12.55148283907650608, -223.4215551264213104 ) ) ;
#103249 = EDGE_CURVE ( 'NONE', #213843, #100823, #257849, .T. ) ;
#103250 = AXIS2_PLACEMENT_3D ( 'NONE', #214769, #59516, #38716 ) ;
#103251 = ORIENTED_EDGE ( 'NONE', *, *, #105227, .F. ) ;
#103253 = CARTESIAN_POINT ( 'NONE',  ( -22.50000000000000000, 75.90736249940329117, -215.1728046915651191 ) ) ;
#103252 = DIRECTION ( 'NONE',  ( 1.836970198721029934E-16, 1.000000000000000000, 6.982962677686266711E-15 ) ) ;
#103255 = ORIENTED_EDGE ( 'NONE', *, *, #218792, .T. ) ;
#103254 = VECTOR ( 'NONE', #14884, 1000.000000000000114 ) ;
#103257 = ORIENTED_EDGE ( 'NONE', *, *, #71125, .T. ) ;
#103256 = CARTESIAN_POINT ( 'NONE',  ( -23.25000000000000000, 85.60000000001149090, -45.91707660717669626 ) ) ;
#103258 = CIRCLE ( 'NONE', #249042, 0.09999999999999939493 ) ;
#103259 = ORIENTED_EDGE ( 'NONE', *, *, #221440, .T. ) ;
#103260 = CARTESIAN_POINT ( 'NONE',  ( 18.54116936837188234, -9.463564198372441894, -7.048542490888269896 ) ) ;
#103261 = DIRECTION ( 'NONE',  ( 0.000000000000000000, 0.5859227990963362664, 0.8103668758649469339 ) ) ;
#103262 = FACE_OUTER_BOUND ( 'NONE', #231035, .T. ) ;
#103263 = CARTESIAN_POINT ( 'NONE',  ( -20.65000000000000568, 7.250000000011138646, -109.7500000000000426 ) ) ;
#103264 = EDGE_LOOP ( 'NONE', ( #220225, #82227, #133284, #45020 ) ) ;
#103265 = EDGE_CURVE ( 'NONE', #76926, #111084, #15462, .T. ) ;
#103266 = DIRECTION ( 'NONE',  ( 0.000000000000000000, 0.3116596277708317264, 0.9501938099239264357 ) ) ;
#103267 = CIRCLE ( 'NONE', #169970, 0.09999999999999939493 ) ;
#103268 = DIRECTION ( 'NONE',  ( -3.265361837132813093E-16, 1.000000000000000000, -0.000000000000000000 ) ) ;
#103269 = EDGE_CURVE ( 'NONE', #222763, #44904, #148161, .T. ) ;
#103270 = ORIENTED_EDGE ( 'NONE', *, *, #205510, .F. ) ;
#103271 = DIRECTION ( 'NONE',  ( -1.000000000000000000, 0.000000000000000000, 0.000000000000000000 ) ) ;
#103272 = ADVANCED_FACE ( 'NONE', ( #24455 ), #173169, .T. ) ;
#103273 = DIRECTION ( 'NONE',  ( 2.840903330521633255E-16, -0.8700118002898322711, 0.4930308989875231696 ) ) ;
#103274 = AXIS2_PLACEMENT_3D ( 'NONE', #54910, #112349, #134442 ) ;
#103275 = ORIENTED_EDGE ( 'NONE', *, *, #72962, .F. ) ;
#103276 = CIRCLE ( 'NONE', #149104, 4.099999999999992539 ) ;
#103277 = DIRECTION ( 'NONE',  ( 0.000000000000000000, -0.000000000000000000, 1.000000000000000000 ) ) ;
#103278 = AXIS2_PLACEMENT_3D ( 'NONE', #56757, #94627, #215846 ) ;
#103279 = ADVANCED_FACE ( 'NONE', ( #144338 ), #223889, .T. ) ;
#103280 = DIRECTION ( 'NONE',  ( 0.000000000000000000, 0.8267009638119992010, 0.5626415523513276229 ) ) ;
#103284 = EDGE_CURVE ( 'NONE', #82597, #8870, #93992, .T. ) ;
#103283 = EDGE_CURVE ( 'NONE', #202553, #184620, #84342, .T. ) ;
#103282 = EDGE_LOOP ( 'NONE', ( #160746, #97951, #15807, #75942 ) ) ;
#103281 = AXIS2_PLACEMENT_3D ( 'NONE', #100624, #60241, #115094 ) ;
#103285 = DIRECTION ( 'NONE',  ( -1.000000000000000000, 7.304098846218134667E-16, 5.100424963727256530E-30 ) ) ;
#103286 = CARTESIAN_POINT ( 'NONE',  ( 21.05000000000000071, 6.477067021135912483, -134.1000000000000227 ) ) ;
#103287 = FACE_OUTER_BOUND ( 'NONE', #139223, .T. ) ;
#103288 = CARTESIAN_POINT ( 'NONE',  ( -22.39999999999999858, 7.612336166715881092, -199.3421143478784359 ) ) ;
#103289 = TOROIDAL_SURFACE ( 'NONE', #236567, 4.099999999999999645, 0.1000000000000000056 ) ;
#103290 = DIRECTION ( 'NONE',  ( 0.000000000000000000, 0.9126074666063791474, 0.4088369013363231663 ) ) ;
#103291 = DIRECTION ( 'NONE',  ( 0.000000000000000000, 0.1575844902526835067, 0.9875055080513738259 ) ) ;
#103292 = EDGE_CURVE ( 'NONE', #64683, #138152, #193979, .T. ) ;
#103295 = ADVANCED_FACE ( 'NONE', ( #238334, #40169 ), #21868, .F. ) ;
#103294 = CARTESIAN_POINT ( 'NONE',  ( -23.25000000000000000, 1.115600667400684642E-11, -134.0000000000000284 ) ) ;
#103293 = VECTOR ( 'NONE', #249350, 1000.000000000000000 ) ;
#103296 = ORIENTED_EDGE ( 'NONE', *, *, #187421, .T. ) ;
#103298 = DIRECTION ( 'NONE',  ( -3.265361837132813093E-16, 1.000000000000000000, 0.000000000000000000 ) ) ;
#103297 =( NAMED_UNIT ( * ) PLANE_ANGLE_UNIT ( ) SI_UNIT ( $, .RADIAN. ) );
#103299 = VECTOR ( 'NONE', #216312, 1000.000000000000000 ) ;
#103300 = VECTOR ( 'NONE', #154381, 1000.000000000000000 ) ;
#103301 = ORIENTED_EDGE ( 'NONE', *, *, #74356, .T. ) ;
#103302 = AXIS2_PLACEMENT_3D ( 'NONE', #231973, #191568, #254065 ) ;
#103303 = LINE ( 'NONE', #86298, #122916 ) ;
#103304 = EDGE_CURVE ( 'NONE', #50473, #67123, #169792, .T. ) ;
#103305 = CARTESIAN_POINT ( 'NONE',  ( -18.79999999999999716, 0.000000000000000000, 0.000000000000000000 ) ) ;
#103307 = ORIENTED_EDGE ( 'NONE', *, *, #23538, .T. ) ;
#103306 = FACE_OUTER_BOUND ( 'NONE', #16336, .T. ) ;
#103309 = ORIENTED_EDGE ( 'NONE', *, *, #195110, .T. ) ;
#103308 = CARTESIAN_POINT ( 'NONE',  ( 21.06277459767440163, 67.12713756174332502, -57.31910829216806746 ) ) ;
#103310 = AXIS2_PLACEMENT_3D ( 'NONE', #221048, #20314, #18999 ) ;
#103311 = FACE_OUTER_BOUND ( 'NONE', #238310, .T. ) ;
#103312 = FACE_OUTER_BOUND ( 'NONE', #49270, .T. ) ;
#103313 = CARTESIAN_POINT ( 'NONE',  ( -17.11825945287482753, 9.950000000011138823, -180.2499999999999716 ) ) ;
#103314 = CARTESIAN_POINT ( 'NONE',  ( 18.59999999999999432, 86.96699927712941758, -199.3055931863049182 ) ) ;
#103315 = EDGE_CURVE ( 'NONE', #5771, #146300, #242181, .T. ) ;
#103317 = ORIENTED_EDGE ( 'NONE', *, *, #16060, .T. ) ;
#103316 = CARTESIAN_POINT ( 'NONE',  ( -23.15000000000000213, -8.596261682231835621, -143.4501275171502925 ) ) ;
#103318 = EDGE_CURVE ( 'NONE', #180552, #103723, #43929, .T. ) ;
#103319 = AXIS2_PLACEMENT_3D ( 'NONE', #106614, #47936, #187481 ) ;
#103320 = AXIS2_PLACEMENT_3D ( 'NONE', #215459, #214188, #99343 ) ;
#103321 = CARTESIAN_POINT ( 'NONE',  ( -20.94999999999999929, 1.115600667400684642E-11, -100.5000000000000426 ) ) ;
#103322 = ORIENTED_EDGE ( 'NONE', *, *, #198157, .F. ) ;
#103323 = ORIENTED_EDGE ( 'NONE', *, *, #42807, .F. ) ;
#103325 = EDGE_CURVE ( 'NONE', #62684, #60562, #59672, .T. ) ;
#103324 = CARTESIAN_POINT ( 'NONE',  ( -18.46154800491010306, 85.48020627425367479, -62.86565664614276727 ) ) ;
#103326 = FACE_OUTER_BOUND ( 'NONE', #5949, .T. ) ;
#103327 = ORIENTED_EDGE ( 'NONE', *, *, #218201, .T. ) ;
#103328 = DIRECTION ( 'NONE',  ( -0.000000000000000000, -0.000000000000000000, 1.000000000000000000 ) ) ;
#103329 = CIRCLE ( 'NONE', #78395, 4.299999999999966960 ) ;
#103330 = TOROIDAL_SURFACE ( 'NONE', #132578, 1.900000000000002576, 0.1000000000000000056 ) ;
#103331 = CYLINDRICAL_SURFACE ( 'NONE', #90852, 0.5000000000000004441 ) ;
#103332 = EDGE_CURVE ( 'NONE', #192766, #188576, #152298, .T. ) ;
#103333 = VERTEX_POINT ( 'NONE', #163944 ) ;
#103334 = CARTESIAN_POINT ( 'NONE',  ( 21.08134388332232234, 6.173453938067205549, -199.5778913402473904 ) ) ;
#103335 = VECTOR ( 'NONE', #223365, 1000.000000000000114 ) ;
#103336 = EDGE_LOOP ( 'NONE', ( #100964, #170149, #104579, #224802 ) ) ;
#103337 = ORIENTED_EDGE ( 'NONE', *, *, #102668, .T. ) ;
#103338 = LINE ( 'NONE', #239022, #65347 ) ;
#103339 = ORIENTED_EDGE ( 'NONE', *, *, #213206, .F. ) ;
#103341 = EDGE_CURVE ( 'NONE', #204834, #176771, #64827, .T. ) ;
#103340 = CARTESIAN_POINT ( 'NONE',  ( 18.59999999999999432, -0.6576273345615495369, -242.5323337003318898 ) ) ;
#103342 = ORIENTED_EDGE ( 'NONE', *, *, #150859, .F. ) ;
#103344 = ORIENTED_EDGE ( 'NONE', *, *, #22129, .T. ) ;
#103343 = CARTESIAN_POINT ( 'NONE',  ( -21.55000000000000426, 7.750000000011159074, -54.75000000000000000 ) ) ;
#103345 = AXIS2_PLACEMENT_3D ( 'NONE', #3040, #123020, #85125 ) ;
#103346 = CYLINDRICAL_SURFACE ( 'NONE', #2670, 1.749999999999999778 ) ;
#103347 = ORIENTED_EDGE ( 'NONE', *, *, #121235, .T. ) ;
#103348 = CARTESIAN_POINT ( 'NONE',  ( 22.40000000000010516, 1.020945751984553285E-11, -88.85042919245492499 ) ) ;
#103349 = CIRCLE ( 'NONE', #20001, 0.09999999999999939493 ) ;
#103350 = CIRCLE ( 'NONE', #74376, 0.09999999999999939493 ) ;
#103351 = EDGE_LOOP ( 'NONE', ( #122051, #59219, #109344, #97976 ) ) ;
#103353 = EDGE_LOOP ( 'NONE', ( #125231, #250960 ) ) ;
#103352 = VERTEX_POINT ( 'NONE', #204330 ) ;
#103354 = CARTESIAN_POINT ( 'NONE',  ( 20.94999999999999574, 74.26374286841466699, -124.9544551555068068 ) ) ;
#103355 = AXIS2_PLACEMENT_3D ( 'NONE', #94329, #214295, #175215 ) ;
#103356 = CARTESIAN_POINT ( 'NONE',  ( -20.94560253601877164, 56.04839098492278993, -227.9897245711966036 ) ) ;
#103357 = ORIENTED_EDGE ( 'NONE', *, *, #178427, .T. ) ;
#103358 = AXIS2_PLACEMENT_3D ( 'NONE', #208609, #226863, #27426 ) ;
#103359 = ORIENTED_EDGE ( 'NONE', *, *, #202456, .F. ) ;
#103360 = LINE ( 'NONE', #61690, #78605 ) ;
#103361 = CARTESIAN_POINT ( 'NONE',  ( -21.05000000000000071, 55.59258605799641373, -234.6589115948038966 ) ) ;
#103363 = ORIENTED_EDGE ( 'NONE', *, *, #52792, .T. ) ;
#103362 = DIRECTION ( 'NONE',  ( -0.000000000000000000, 0.4721928772777345684, 0.8814952561688429444 ) ) ;
#103364 = DIRECTION ( 'NONE',  ( 0.9880948137434723000, 0.07264505804272584910, 0.1356146547952018777 ) ) ;
#103365 = ORIENTED_EDGE ( 'NONE', *, *, #114051, .F. ) ;
#103366 = CARTESIAN_POINT ( 'NONE',  ( -17.78043020864321022, 65.14640788800579685, -46.36005831880417816 ) ) ;
#103367 = DIRECTION ( 'NONE',  ( 1.000000000000000000, 0.000000000000000000, 0.000000000000000000 ) ) ;
#103368 = CIRCLE ( 'NONE', #199076, 11.74999999999999289 ) ;
#103369 = ORIENTED_EDGE ( 'NONE', *, *, #81730, .F. ) ;
#103370 = FACE_OUTER_BOUND ( 'NONE', #174347, .T. ) ;
#103371 = DIRECTION ( 'NONE',  ( -1.000000000000000000, 0.000000000000000000, 0.000000000000000000 ) ) ;
#103372 = VERTEX_POINT ( 'NONE', #25712 ) ;
#103373 = CARTESIAN_POINT ( 'NONE',  ( 18.59999999999999076, 69.35000000001180354, -81.87310748452435405 ) ) ;
#103374 = ORIENTED_EDGE ( 'NONE', *, *, #147678, .T. ) ;
#103376 = ORIENTED_EDGE ( 'NONE', *, *, #123892, .T. ) ;
#103375 = VERTEX_POINT ( 'NONE', #141791 ) ;
#103377 = EDGE_LOOP ( 'NONE', ( #27138, #58346, #129063, #136511 ) ) ;
#103378 = CARTESIAN_POINT ( 'NONE',  ( -16.77683809663752257, 23.65833333333332433, -16.75000000000000000 ) ) ;
#103379 = ORIENTED_EDGE ( 'NONE', *, *, #169525, .T. ) ;
#103380 = CYLINDRICAL_SURFACE ( 'NONE', #92441, 0.09999999999999939493 ) ;
#103381 = ORIENTED_EDGE ( 'NONE', *, *, #68990, .T. ) ;
#103382 = CYLINDRICAL_SURFACE ( 'NONE', #139815, 0.09999999999999543976 ) ;
#103383 = CARTESIAN_POINT ( 'NONE',  ( 18.59999999999999076, 65.50857864377491069, -145.1731074845244507 ) ) ;
#103384 = EDGE_LOOP ( 'NONE', ( #121341, #133300, #14125, #17686 ) ) ;
#103385 = EDGE_CURVE ( 'NONE', #208884, #38262, #52287, .T. ) ;
#103386 = EDGE_LOOP ( 'NONE', ( #45964, #146704, #176463, #103444 ) ) ;
#103387 = CIRCLE ( 'NONE', #65810, 0.1000000000000028644 ) ;
#103388 = VECTOR ( 'NONE', #199777, 1000.000000000000000 ) ;
#103389 = CIRCLE ( 'NONE', #208051, 11.89999999999999858 ) ;
#103390 = AXIS2_PLACEMENT_3D ( 'NONE', #102520, #103818, #183392 ) ;
#103391 = ORIENTED_EDGE ( 'NONE', *, *, #161467, .F. ) ;
#103392 = CARTESIAN_POINT ( 'NONE',  ( -16.89318236219975944, 66.04846474213667307, -82.16797785241854513 ) ) ;
#103393 = ORIENTED_EDGE ( 'NONE', *, *, #8795, .F. ) ;
#103394 = EDGE_CURVE ( 'NONE', #6846, #71198, #239756, .T. ) ;
#103395 = CARTESIAN_POINT ( 'NONE',  ( 21.13461538461538325, 12.99955419111918253, -210.8083363671015604 ) ) ;
#103396 = CARTESIAN_POINT ( 'NONE',  ( -23.25000000000000000, 6.982009704867601307, -171.1961521182563217 ) ) ;
#103397 = CARTESIAN_POINT ( 'NONE',  ( -16.97683809663752186, 19.98098358856834977, -229.3296076283783407 ) ) ;
#103398 = FACE_OUTER_BOUND ( 'NONE', #86108, .T. ) ;
#103399 = DIRECTION ( 'NONE',  ( 1.000000000000000000, 0.000000000000000000, 0.000000000000000000 ) ) ;
#103400 = DIRECTION ( 'NONE',  ( -1.000000000000000000, 0.000000000000000000, 0.000000000000000000 ) ) ;
#103401 = EDGE_CURVE ( 'NONE', #145808, #154503, #81488, .T. ) ;
#103402 = DIRECTION ( 'NONE',  ( 0.000000000000000000, 0.000000000000000000, 1.000000000000000000 ) ) ;
#103405 = CARTESIAN_POINT ( 'NONE',  ( 21.05000000000000071, 34.07612324756792077, -243.5412266404783566 ) ) ;
#103404 = AXIS2_PLACEMENT_3D ( 'NONE', #151689, #113808, #51238 ) ;
#103403 = LINE ( 'NONE', #182983, #15464 ) ;
#103406 = CARTESIAN_POINT ( 'NONE',  ( -18.59999999999999787, 1.340746217944851715, -123.7271374945788409 ) ) ;
#103407 = LINE ( 'NONE', #4316, #236077 ) ;
#103408 = AXIS2_PLACEMENT_3D ( 'NONE', #179955, #2571, #216495 ) ;
#103409 = FACE_OUTER_BOUND ( 'NONE', #209541, .T. ) ;
#103410 = DIRECTION ( 'NONE',  ( 1.000000000000000000, 0.000000000000000000, 0.000000000000000000 ) ) ;
#103411 = ORIENTED_EDGE ( 'NONE', *, *, #140843, .F. ) ;
#103412 = VECTOR ( 'NONE', #147039, 1000.000000000000000 ) ;
#103413 = ADVANCED_FACE ( 'NONE', ( #60975 ), #80511, .F. ) ;
#103415 = ORIENTED_EDGE ( 'NONE', *, *, #15006, .F. ) ;
#103414 = CARTESIAN_POINT ( 'NONE',  ( 20.27550659511089037, 9.216043722520002035, -46.15000000000000568 ) ) ;
#103416 = EDGE_CURVE ( 'NONE', #171778, #142483, #225165, .T. ) ;
#103417 = ORIENTED_EDGE ( 'NONE', *, *, #243551, .F. ) ;
#103418 = DIRECTION ( 'NONE',  ( -1.000000000000000000, 0.000000000000000000, 0.000000000000000000 ) ) ;
#103419 =( BOUNDED_SURFACE ( )  B_SPLINE_SURFACE ( 3, 2, ( 
 ( #80692, #44169, #141963 ),
 ( #23342, #143245, #123703 ),
 ( #118579, #61149, #101522 ),
 ( #239801, #140684, #258014 ) ),
 .UNSPECIFIED., .F., .F., .F. ) 
 B_SPLINE_SURFACE_WITH_KNOTS ( ( 4, 4 ),
 ( 3, 3 ),
 ( 0.0006461284895273902403, 0.0007503702773986321546 ),
 ( 0.000000000000000000, 1.000000000000000000 ),
 .UNSPECIFIED. ) 
 GEOMETRIC_REPRESENTATION_ITEM ( )  RATIONAL_B_SPLINE_SURFACE ( (
 ( 1.000000000000000000, 0.7071067811865475727, 1.000000000000000000),
 ( 1.000000000000000000, 0.7076476444648814867, 1.000000000000000000),
 ( 1.000000000000000000, 0.7075727925191799272, 1.000000000000000000),
 ( 1.000000000000000000, 0.7071067811865475727, 1.000000000000000000) ) ) 
 REPRESENTATION_ITEM ( '' )  SURFACE ( )  );
#103420 = ADVANCED_FACE ( 'NONE', ( #51661 ), #27023, .T. ) ;
#103421 = CARTESIAN_POINT ( 'NONE',  ( 18.59999999999999787, -10.74999999999999289, 32.89999999999999858 ) ) ;
#103422 = ORIENTED_EDGE ( 'NONE', *, *, #175378, .T. ) ;
#103423 =( LENGTH_UNIT ( ) NAMED_UNIT ( * ) SI_UNIT ( .MILLI., .METRE. ) );
#103424 = LINE ( 'NONE', #44768, #216534 ) ;
#103425 = EDGE_CURVE ( 'NONE', #138366, #71227, #198048, .T. ) ;
#103426 =( GEOMETRIC_REPRESENTATION_CONTEXT ( 3 ) GLOBAL_UNCERTAINTY_ASSIGNED_CONTEXT ( ( #218796 ) ) GLOBAL_UNIT_ASSIGNED_CONTEXT ( ( #159335, #60196, #34565 ) ) REPRESENTATION_CONTEXT ( 'NONE', 'WORKASPACE' ) );
#103427 = DIRECTION ( 'NONE',  ( -1.000000000000000000, 0.000000000000000000, -0.000000000000000000 ) ) ;
#103428 = VERTEX_POINT ( 'NONE', #189922 ) ;
#103429 = CIRCLE ( 'NONE', #224257, 0.1000000000000124678 ) ;
#103430 = VECTOR ( 'NONE', #89450, 1000.000000000000000 ) ;
#103431 = DIRECTION ( 'NONE',  ( 1.000000000000000000, 0.000000000000000000, 0.000000000000000000 ) ) ;
#103432 = DIRECTION ( 'NONE',  ( 0.000000000000000000, 1.000000000000000000, 0.000000000000000000 ) ) ;
#103433 = EDGE_CURVE ( 'NONE', #68319, #195886, #227272, .T. ) ;
#103434 = DIRECTION ( 'NONE',  ( 0.000000000000000000, -1.265107689135680095E-16, 1.000000000000000000 ) ) ;
#103435 = FACE_OUTER_BOUND ( 'NONE', #167167, .T. ) ;
#103437 = ORIENTED_EDGE ( 'NONE', *, *, #234884, .T. ) ;
#103436 = CARTESIAN_POINT ( 'NONE',  ( -23.39999999999994529, 64.35000000001120668, -36.02310748452479316 ) ) ;
#103438 = AXIS2_PLACEMENT_3D ( 'NONE', #130046, #132639, #36114 ) ;
#103439 = FACE_OUTER_BOUND ( 'NONE', #142967, .T. ) ;
#103441 = EDGE_LOOP ( 'NONE', ( #123057, #193489, #154318, #156988 ) ) ;
#103440 = DIRECTION ( 'NONE',  ( -0.000000000000000000, 1.000000000000000000, -0.000000000000000000 ) ) ;
#103442 = CARTESIAN_POINT ( 'NONE',  ( 21.14999999999999858, 76.00000000001237765, -170.0231074845243597 ) ) ;
#103443 = DIRECTION ( 'NONE',  ( 1.000000000000000000, -0.000000000000000000, -0.000000000000000000 ) ) ;
#103444 = ORIENTED_EDGE ( 'NONE', *, *, #148271, .T. ) ;
#103445 = CARTESIAN_POINT ( 'NONE',  ( -16.93262454970420094, 65.99797953208192780, -157.4501837107617348 ) ) ;
#103447 = EDGE_CURVE ( 'NONE', #103678, #132498, #28314, .T. ) ;
#103446 = PLANE ( 'NONE',  #210996 ) ;
#103449 = CYLINDRICAL_SURFACE ( 'NONE', #54163, 0.1000000000000024342 ) ;
#103448 = CARTESIAN_POINT ( 'NONE',  ( -21.29999999999995808, 76.00000000001267608, -203.5231074845243597 ) ) ;
#103450 = LINE ( 'NONE', #186886, #45468 ) ;
#103451 = CARTESIAN_POINT ( 'NONE',  ( -17.11825945287482753, 23.06621698515930063, -230.9822826988504119 ) ) ;
#103452 = CARTESIAN_POINT ( 'NONE',  ( -20.94684162548487194, 64.25000000001233502, -163.1814634889771014 ) ) ;
#103453 = FACE_OUTER_BOUND ( 'NONE', #82186, .T. ) ;
#103454 = AXIS2_PLACEMENT_3D ( 'NONE', #142166, #101727, #61349 ) ;
#103455 = TOROIDAL_SURFACE ( 'NONE', #232498, 0.2000000000000000111, 0.1000000000000000056 ) ;
#103456 = CARTESIAN_POINT ( 'NONE',  ( 23.24999999999999289, 17.01923898301590654, -224.3994341343041867 ) ) ;
#103457 = CIRCLE ( 'NONE', #203444, 2.000000000000001776 ) ;
#103458 = ORIENTED_EDGE ( 'NONE', *, *, #28620, .T. ) ;
#103459 = CARTESIAN_POINT ( 'NONE',  ( 20.94999999999999929, 45.93587830916155212, -239.9163948487882863 ) ) ;
#103460 = TOROIDAL_SURFACE ( 'NONE', #86885, 11.65000000000000036, 0.1000000000000000056 ) ;
#103461 = EDGE_LOOP ( 'NONE', ( #211947, #148986, #156643, #78680 ) ) ;
#103462 = VERTEX_POINT ( 'NONE', #46536 ) ;
#103463 = DIRECTION ( 'NONE',  ( 1.000000000000000000, 0.000000000000000000, 0.000000000000000000 ) ) ;
#103464 = CARTESIAN_POINT ( 'NONE',  ( -18.59999999999999787, -1.162701749926853712, -75.10000000000003695 ) ) ;
#103465 = ORIENTED_EDGE ( 'NONE', *, *, #170737, .T. ) ;
#103466 = AXIS2_PLACEMENT_3D ( 'NONE', #178956, #237614, #160667 ) ;
#103467 = ORIENTED_EDGE ( 'NONE', *, *, #171295, .T. ) ;
#103468 = CIRCLE ( 'NONE', #61801, 0.1000000000000121764 ) ;
#103469 = VERTEX_POINT ( 'NONE', #110371 ) ;
#103470 = CARTESIAN_POINT ( 'NONE',  ( -18.59999999999999787, 1.637172712981537659, -78.58215336547205254 ) ) ;
#103471 = ORIENTED_EDGE ( 'NONE', *, *, #241188, .F. ) ;
#103472 = EDGE_CURVE ( 'NONE', #138871, #35121, #145640, .T. ) ;
#103474 = DIRECTION ( 'NONE',  ( -1.000000000000000000, -0.000000000000000000, -0.000000000000000000 ) ) ;
#103473 = VECTOR ( 'NONE', #255078, 1000.000000000000000 ) ;
#103475 = FACE_OUTER_BOUND ( 'NONE', #225514, .T. ) ;
#103476 = CIRCLE ( 'NONE', #149316, 0.1000000000000028644 ) ;
#103477 = CARTESIAN_POINT ( 'NONE',  ( 20.85000000000000142, -1.362429037182151470, -141.8888812479212334 ) ) ;
#103478 = DIRECTION ( 'NONE',  ( 0.000000000000000000, 0.000000000000000000, -1.000000000000000000 ) ) ;
#103479 = AXIS2_PLACEMENT_3D ( 'NONE', #64849, #88243, #163969 ) ;
#103480 = FACE_OUTER_BOUND ( 'NONE', #241287, .T. ) ;
#103481 = LINE ( 'NONE', #185612, #124472 ) ;
#103483 = VERTEX_POINT ( 'NONE', #129925 ) ;
#103482 = SPHERICAL_SURFACE ( 'NONE', #200624, 0.1000000000000000056 ) ;
#103485 = DIRECTION ( 'NONE',  ( 1.000000000000000000, 0.000000000000000000, 0.000000000000000000 ) ) ;
#103484 = DIRECTION ( 'NONE',  ( 0.000000000000000000, -1.000000000000000000, -0.000000000000000000 ) ) ;
#103486 = VECTOR ( 'NONE', #83647, 1000.000000000000000 ) ;
#103487 = ADVANCED_FACE ( 'NONE', ( #230321 ), #229057, .T. ) ;
#103488 = CARTESIAN_POINT ( 'NONE',  ( 21.00000000000000000, 9.750000000011153745, -112.7500000000000284 ) ) ;
#103489 = EDGE_CURVE ( 'NONE', #16838, #9164, #69994, .T. ) ;
#103490 = ORIENTED_EDGE ( 'NONE', *, *, #2040, .F. ) ;
#103491 = FACE_OUTER_BOUND ( 'NONE', #7561, .T. ) ;
#103492 = DIRECTION ( 'NONE',  ( 0.000000000000000000, 0.8700118002898393765, -0.4930308989875104575 ) ) ;
#103493 = ORIENTED_EDGE ( 'NONE', *, *, #178275, .T. ) ;
#103494 = EDGE_CURVE ( 'NONE', #20283, #42426, #135497, .T. ) ;
#103496 = DIRECTION ( 'NONE',  ( 1.000000000000000000, 0.000000000000000000, 0.000000000000000000 ) ) ;
#103495 = CARTESIAN_POINT ( 'NONE',  ( 18.39999999999999503, 70.35000000001224407, -149.1731074845243938 ) ) ;
#103497 = EDGE_CURVE ( 'NONE', #138550, #6498, #170410, .T. ) ;
#103498 = EDGE_CURVE ( 'NONE', #123340, #221, #202155, .T. ) ;
#103499 = DIRECTION ( 'NONE',  ( 0.000000000000000000, -7.086529944415894657E-15, 1.000000000000000000 ) ) ;
#103501 = EDGE_CURVE ( 'NONE', #215192, #54944, #23107, .T. ) ;
#103500 = AXIS2_PLACEMENT_3D ( 'NONE', #35094, #115876, #75490 ) ;
#103503 = EDGE_LOOP ( 'NONE', ( #94483, #246340, #33167, #252397 ) ) ;
#103502 = CIRCLE ( 'NONE', #211865, 0.1000000000000016431 ) ;
#103504 = FACE_OUTER_BOUND ( 'NONE', #249531, .T. ) ;
#103505 = EDGE_CURVE ( 'NONE', #244339, #253988, #56384, .T. ) ;
#103506 = DIRECTION ( 'NONE',  ( 0.000000000000000000, -1.000000000000000000, 0.000000000000000000 ) ) ;
#103507 = CARTESIAN_POINT ( 'NONE',  ( -21.05000000000000071, 76.10000000001241460, -176.5637644362255969 ) ) ;
#103508 = ORIENTED_EDGE ( 'NONE', *, *, #93607, .T. ) ;
#103509 = VERTEX_POINT ( 'NONE', #205614 ) ;
#103510 = AXIS2_PLACEMENT_3D ( 'NONE', #23985, #185606, #6962 ) ;
#103511 = AXIS2_PLACEMENT_3D ( 'NONE', #98830, #80558, #160158 ) ;
#103512 = DIRECTION ( 'NONE',  ( 0.000000000000000000, -0.5000000000000078826, -0.8660254037844340447 ) ) ;
#103513 = FACE_OUTER_BOUND ( 'NONE', #140367, .T. ) ;
#103514 = DIRECTION ( 'NONE',  ( 1.000000000000000000, 0.000000000000000000, 0.000000000000000000 ) ) ;
#103515 = AXIS2_PLACEMENT_3D ( 'NONE', #10268, #109333, #11557 ) ;
#103516 = DIRECTION ( 'NONE',  ( 0.000000000000000000, 0.000000000000000000, 1.000000000000000000 ) ) ;
#103517 = DIRECTION ( 'NONE',  ( 0.000000000000000000, 0.000000000000000000, -1.000000000000000000 ) ) ;
#103518 = AXIS2_PLACEMENT_3D ( 'NONE', #164399, #65287, #224357 ) ;
#103519 = ADVANCED_FACE ( 'NONE', ( #127381 ), #191233, .F. ) ;
#103521 = VERTEX_POINT ( 'NONE', #166535 ) ;
#103520 = DIRECTION ( 'NONE',  ( 0.000000000000000000, 0.9126074666063773710, 0.4088369013363274962 ) ) ;
#103522 = CARTESIAN_POINT ( 'NONE',  ( -21.05000000000000071, 6.299230910103437608, -33.40156249999967741 ) ) ;
#103523 = LINE ( 'NONE', #83927, #40683 ) ;
#103524 = DIRECTION ( 'NONE',  ( 0.000000000000000000, -6.454785026890489601E-15, 1.000000000000000000 ) ) ;
#103525 = FACE_OUTER_BOUND ( 'NONE', #75005, .T. ) ;
#103526 = DIRECTION ( 'NONE',  ( 1.000000000000000000, 2.952720810173289112E-16, -0.000000000000000000 ) ) ;
#103527 = ADVANCED_FACE ( 'NONE', ( #67401, #29592 ), #128675, .T. ) ;
#103529 = EDGE_LOOP ( 'NONE', ( #181671, #2738, #148528, #201377 ) ) ;
#103528 = CARTESIAN_POINT ( 'NONE',  ( -20.65000000000000568, 5.650000000011139001, -143.2500000000000284 ) ) ;
#103530 = CARTESIAN_POINT ( 'NONE',  ( -23.49999999999994316, 77.75000000001119815, -47.64205752314703801 ) ) ;
#103532 = EDGE_CURVE ( 'NONE', #216635, #110447, #167820, .T. ) ;
#103531 = CARTESIAN_POINT ( 'NONE',  ( 21.12769345151713196, 10.71928767695172624, -179.7474803461974489 ) ) ;
#103533 = AXIS2_PLACEMENT_3D ( 'NONE', #60150, #22350, #158032 ) ;
#103534 = DIRECTION ( 'NONE',  ( -1.000000000000000000, -3.265361837132813093E-16, 0.000000000000000000 ) ) ;
#103535 = DIRECTION ( 'NONE',  ( 0.000000000000000000, 0.2617529984165032908, 0.9651348961777156399 ) ) ;
#103536 = ORIENTED_EDGE ( 'NONE', *, *, #249144, .F. ) ;
#103537 = CARTESIAN_POINT ( 'NONE',  ( -14.87770893841225295, 66.56936289831551790, -151.7548468664634811 ) ) ;
#103538 = CARTESIAN_POINT ( 'NONE',  ( -16.87683809663752399, 66.13411015068005838, -116.2905342915937581 ) ) ;
#103539 = VECTOR ( 'NONE', #226341, 1000.000000000000000 ) ;
#103540 = DIRECTION ( 'NONE',  ( 0.000000000000000000, 0.000000000000000000, -1.000000000000000000 ) ) ;
#103541 = CIRCLE ( 'NONE', #145061, 0.09999999999999971412 ) ;
#103542 = CONTEXT_DEPENDENT_SHAPE_REPRESENTATION ( #234005, #62197 ) ;
#103543 = DIRECTION ( 'NONE',  ( 0.000000000000000000, 0.000000000000000000, -1.000000000000000000 ) ) ;
#103544 = EDGE_LOOP ( 'NONE', ( #121661, #204294, #252989, #235574 ) ) ;
#103545 = CARTESIAN_POINT ( 'NONE',  ( 20.85000000000000142, 62.98048128140160173, -207.0210305352945568 ) ) ;
#103546 = ORIENTED_EDGE ( 'NONE', *, *, #21163, .F. ) ;
#103547 = CARTESIAN_POINT ( 'NONE',  ( 21.53752568622118346, -1.347531963294298585, -194.3475782847248183 ) ) ;
#103548 = DIRECTION ( 'NONE',  ( 1.000000000000000000, 0.000000000000000000, 0.000000000000000000 ) ) ;
#103549 = CARTESIAN_POINT ( 'NONE',  ( 15.48841904831874849, 67.43841904833058720, -82.17310748452437963 ) ) ;
#103550 = ORIENTED_EDGE ( 'NONE', *, *, #159485, .F. ) ;
#103551 = CIRCLE ( 'NONE', #141011, 0.1000000000000117045 ) ;
#103552 = CYLINDRICAL_SURFACE ( 'NONE', #217486, 0.5000000000000004441 ) ;
#103553 = CARTESIAN_POINT ( 'NONE',  ( 21.09793522318420855, 13.08351628660398980, -210.6767460175381359 ) ) ;
#103554 = CARTESIAN_POINT ( 'NONE',  ( 21.14999999999999858, 2.585532092011767702, -212.8717110730202933 ) ) ;
#103555 = CARTESIAN_POINT ( 'NONE',  ( -16.87401514999228525, 9.949999999999983302, -20.78001799253221193 ) ) ;
#103556 = DIRECTION ( 'NONE',  ( 0.000000000000000000, -0.9915357197604982575, 0.1298341882519033486 ) ) ;
#103557 = ORIENTED_EDGE ( 'NONE', *, *, #99180, .T. ) ;
#103559 = EDGE_LOOP ( 'NONE', ( #127662, #190698, #90922, #29845 ) ) ;
#103558 = DIRECTION ( 'NONE',  ( -4.391705002472929091E-16, 1.000000000000000000, 0.000000000000000000 ) ) ;
#103560 = ORIENTED_EDGE ( 'NONE', *, *, #168853, .T. ) ;
#103561 = DIRECTION ( 'NONE',  ( -1.000000000000000000, 0.000000000000000000, 0.000000000000000000 ) ) ;
#103562 = ORIENTED_EDGE ( 'NONE', *, *, #8493, .T. ) ;
#103563 = CARTESIAN_POINT ( 'NONE',  ( 21.05000000000000071, 65.27628289530454708, -124.3619171903969374 ) ) ;
#103564 = CYLINDRICAL_SURFACE ( 'NONE', #133376, 12.87499999999999822 ) ;
#103565 = VERTEX_POINT ( 'NONE', #227751 ) ;
#103566 = DIRECTION ( 'NONE',  ( 0.000000000000000000, 0.4930308989874980785, 0.8700118002898462599 ) ) ;
#103567 = FACE_OUTER_BOUND ( 'NONE', #60095, .T. ) ;
#103568 = EDGE_LOOP ( 'NONE', ( #195373, #250369, #80588, #30162 ) ) ;
#103569 = CARTESIAN_POINT ( 'NONE',  ( -15.75000000000000355, 9.350000000011139178, -150.8642676076160569 ) ) ;
#103570 = EDGE_CURVE ( 'NONE', #246750, #254486, #222986, .T. ) ;
#103572 = VERTEX_POINT ( 'NONE', #154674 ) ;
#103571 = DIRECTION ( 'NONE',  ( 0.000000000000000000, -1.000000000000000000, 0.000000000000000000 ) ) ;
#103573 = DIRECTION ( 'NONE',  ( 1.000000000000000000, -0.000000000000000000, -0.000000000000000000 ) ) ;
#103574 = CARTESIAN_POINT ( 'NONE',  ( -20.85000000000000142, 67.85909929089923764, -227.8797997985275856 ) ) ;
#103575 = CIRCLE ( 'NONE', #249361, 0.09999999999999939493 ) ;
#103576 = ADVANCED_FACE ( 'NONE', ( #253725 ), #38551, .T. ) ;
#103577 = AXIS2_PLACEMENT_3D ( 'NONE', #102210, #25300, #185644 ) ;
#103578 = ORIENTED_EDGE ( 'NONE', *, *, #160744, .T. ) ;
#103579 = CARTESIAN_POINT ( 'NONE',  ( -20.64999999999999858, 74.07476635515241981, -149.2533510176504876 ) ) ;
#103581 = ADVANCED_FACE ( 'NONE', ( #171676 ), #172965, .T. ) ;
#103580 = LINE ( 'NONE', #65764, #141989 ) ;
#103582 = AXIS2_PLACEMENT_3D ( 'NONE', #64386, #202607, #220872 ) ;
#103583 = CARTESIAN_POINT ( 'NONE',  ( -21.44999999999999929, 11.58468387039766512, -220.1227639117171861 ) ) ;
#103585 = ADVANCED_FACE ( 'NONE', ( #34724 ), #61611, .T. ) ;
#103584 = ORIENTED_EDGE ( 'NONE', *, *, #21819, .T. ) ;
#103586 = DIRECTION ( 'NONE',  ( 1.441126678808781001E-14, 0.9876197685951252359, 0.1568667991644863424 ) ) ;
#103587 = LINE ( 'NONE', #46199, #201425 ) ;
#103588 = VERTEX_POINT ( 'NONE', #175515 ) ;
#103589 = AXIS2_PLACEMENT_3D ( 'NONE', #244167, #184195, #143788 ) ;
#103590 = CIRCLE ( 'NONE', #74439, 0.09999999999999724387 ) ;
#103591 = AXIS2_PLACEMENT_3D ( 'NONE', #191525, #70296, #11591 ) ;
#103593 = EDGE_CURVE ( 'NONE', #186764, #26765, #51897, .T. ) ;
#103592 = VECTOR ( 'NONE', #138691, 1000.000000000000000 ) ;
#103594 = EDGE_CURVE ( 'NONE', #52949, #178394, #197655, .T. ) ;
#103595 = EDGE_LOOP ( 'NONE', ( #138460, #95366, #122528 ) ) ;
#103596 = VERTEX_POINT ( 'NONE', #116800 ) ;
#103597 = DIRECTION ( 'NONE',  ( 0.000000000000000000, 0.000000000000000000, -1.000000000000000000 ) ) ;
#103598 = CARTESIAN_POINT ( 'NONE',  ( -16.87333278164146577, 66.11739021543380090, -183.1562752906779110 ) ) ;
#103600 = ORIENTED_EDGE ( 'NONE', *, *, #43173, .T. ) ;
#103599 = CARTESIAN_POINT ( 'NONE',  ( 20.94999999999999929, 48.89266972451527948, -253.5637804087949121 ) ) ;
#103601 = CYLINDRICAL_SURFACE ( 'NONE', #86697, 0.09999999999999939493 ) ;
#103602 = DIRECTION ( 'NONE',  ( -0.000000000000000000, -0.000000000000000000, -1.000000000000000000 ) ) ;
#103603 = DIRECTION ( 'NONE',  ( -6.938893903907222067E-15, -1.000000000000000000, -7.272083257015735086E-15 ) ) ;
#103604 = DIRECTION ( 'NONE',  ( -1.836970198721029934E-16, -1.000000000000000000, -6.982962677686266711E-15 ) ) ;
#103605 = DIRECTION ( 'NONE',  ( -3.265361837132813093E-16, -0.9651348961777158619, 0.2617529984165024026 ) ) ;
#103606 = CARTESIAN_POINT ( 'NONE',  ( 18.60000000000000497, 1.148907358139439339E-11, -201.0000000000015064 ) ) ;
#103609 = EDGE_LOOP ( 'NONE', ( #23280, #117182, #233145, #165460 ) ) ;
#103608 = EDGE_CURVE ( 'NONE', #88576, #47933, #102333, .T. ) ;
#103607 = CARTESIAN_POINT ( 'NONE',  ( -18.58693740092133240, -9.406432150242029167, -107.6248164565011081 ) ) ;
#103611 = ORIENTED_EDGE ( 'NONE', *, *, #201371, .T. ) ;
#103610 = CARTESIAN_POINT ( 'NONE',  ( -23.25000000000000000, -11.74999999998884448, -130.9000000000000341 ) ) ;
#103612 = DIRECTION ( 'NONE',  ( -1.000000000000000000, -0.000000000000000000, -0.000000000000000000 ) ) ;
#103613 = ORIENTED_EDGE ( 'NONE', *, *, #57050, .F. ) ;
#103614 = EDGE_CURVE ( 'NONE', #9130, #103755, #44123, .T. ) ;
#103615 = CARTESIAN_POINT ( 'NONE',  ( 20.95512820512820440, 65.37615131629998189, -90.87310748452438247 ) ) ;
#103616 = CIRCLE ( 'NONE', #61957, 0.1000000000000032391 ) ;
#103617 = AXIS2_PLACEMENT_3D ( 'NONE', #50969, #174849, #130526 ) ;
#103618 = DIRECTION ( 'NONE',  ( 1.000000000000000000, 0.000000000000000000, 0.000000000000000000 ) ) ;
#103619 = CARTESIAN_POINT ( 'NONE',  ( -21.05000000000000071, 5.850000000011105428, -43.63249722427796939 ) ) ;
#103621 = DIRECTION ( 'NONE',  ( -1.000000000000000000, -0.000000000000000000, -0.000000000000000000 ) ) ;
#103620 = VECTOR ( 'NONE', #75252, 1000.000000000000000 ) ;
#103623 = ADVANCED_FACE ( 'NONE', ( #33456 ), #17684, .T. ) ;
#103622 = CARTESIAN_POINT ( 'NONE',  ( 20.21494484322215968, 66.69682926214377972, -195.1828422927512179 ) ) ;
#103624 = VERTEX_POINT ( 'NONE', #193770 ) ;
#103625 = EDGE_CURVE ( 'NONE', #129928, #192087, #112955, .T. ) ;
#103626 = ORIENTED_EDGE ( 'NONE', *, *, #165463, .T. ) ;
#103627 = FACE_OUTER_BOUND ( 'NONE', #230717, .T. ) ;
#103628 = ADVANCED_FACE ( 'NONE', ( #97187 ), #176794, .F. ) ;
#103629 = AXIS2_PLACEMENT_3D ( 'NONE', #205332, #28034, #145373 ) ;
#103630 = AXIS2_PLACEMENT_3D ( 'NONE', #91323, #131725, #194296 ) ;
#103631 = EDGE_LOOP ( 'NONE', ( #226892, #89430, #169217, #225285 ) ) ;
#103632 = CIRCLE ( 'NONE', #153608, 12.87499999999999822 ) ;
#103633 = DIRECTION ( 'NONE',  ( 1.000000000000000000, -0.000000000000000000, -0.000000000000000000 ) ) ;
#103634 = CIRCLE ( 'NONE', #70382, 11.80000000000000426 ) ;
#103635 = CARTESIAN_POINT ( 'NONE',  ( -16.97683809663752186, 61.13629130372252973, -220.3155949669961444 ) ) ;
#103636 = ORIENTED_EDGE ( 'NONE', *, *, #160789, .T. ) ;
#103637 = CARTESIAN_POINT ( 'NONE',  ( 23.14999999999999858, 7.128833340094563376, -233.7327013124401276 ) ) ;
#103638 = VERTEX_POINT ( 'NONE', #82765 ) ;
#103639 = EDGE_CURVE ( 'NONE', #197037, #243103, #123223, .T. ) ;
#103640 = FACE_OUTER_BOUND ( 'NONE', #68872, .T. ) ;
#103641 = VERTEX_POINT ( 'NONE', #178077 ) ;
#103642 = AXIS2_PLACEMENT_3D ( 'NONE', #123778, #27277, #125066 ) ;
#103643 = CARTESIAN_POINT ( 'NONE',  ( 21.14999999999999858, 11.75000000000000711, 11.75000000000000000 ) ) ;
#103644 = EDGE_CURVE ( 'NONE', #201073, #87677, #181506, .T. ) ;
#103645 = CARTESIAN_POINT ( 'NONE',  ( 14.77516762759921853, 9.436674251854007878, -182.6768619309992800 ) ) ;
#103646 = ORIENTED_EDGE ( 'NONE', *, *, #193982, .T. ) ;
#103647 = LINE ( 'NONE', #42415, #2664 ) ;
#103648 = AXIS2_PLACEMENT_3D ( 'NONE', #194072, #255247, #54534 ) ;
#103650 = VERTEX_POINT ( 'NONE', #20281 ) ;
#103649 = DIRECTION ( 'NONE',  ( -1.073024830501117725E-15, -0.000000000000000000, -1.000000000000000000 ) ) ;
#103651 = CARTESIAN_POINT ( 'NONE',  ( -22.50047199487871197, 75.95509394808482284, -215.2731549034355680 ) ) ;
#103652 = EDGE_LOOP ( 'NONE', ( #26852, #40647, #6518, #145046 ) ) ;
#103653 = AXIS2_PLACEMENT_3D ( 'NONE', #190410, #70482, #150004 ) ;
#103654 = VECTOR ( 'NONE', #3825, 1000.000000000000000 ) ;
#103655 = AXIS2_PLACEMENT_3D ( 'NONE', #222755, #81936, #23319 ) ;
#103656 = CIRCLE ( 'NONE', #170369, 0.1000000000000028644 ) ;
#103657 = EDGE_LOOP ( 'NONE', ( #207821, #213327, #176738, #148942 ) ) ;
#103658 = CARTESIAN_POINT ( 'NONE',  ( -20.54999999999999716, 36.65892442174935439, -249.5511627012433848 ) ) ;
#103659 = CARTESIAN_POINT ( 'NONE',  ( 22.46250603428203974, 26.01852785471617935, -254.2947602979349142 ) ) ;
#103660 = DIRECTION ( 'NONE',  ( 0.000000000000000000, 0.000000000000000000, -1.000000000000000000 ) ) ;
#103661 = CARTESIAN_POINT ( 'NONE',  ( -20.85000000000000142, 64.35000000001147669, -42.80697314750250371 ) ) ;
#103662 = CARTESIAN_POINT ( 'NONE',  ( 23.15000000000000213, -11.48912529307605546, -30.39999999999999503 ) ) ;
#103663 = EDGE_LOOP ( 'NONE', ( #165980, #30173, #102170, #18478, #66509, #249349, #177914, #226304, #167308, #69537, #82211, #101939, #201170, #43114 ) ) ;
#103664 = CARTESIAN_POINT ( 'NONE',  ( -16.89268316805465986, 66.04827818677036078, -182.6673550059788909 ) ) ;
#103665 = DIRECTION ( 'NONE',  ( -1.000000000000000000, 2.952720810173289112E-16, 2.061873921506763405E-30 ) ) ;
#103666 = CARTESIAN_POINT ( 'NONE',  ( -21.05000000000000071, 1.851028230152016674, -45.15391326942250316 ) ) ;
#103667 = CARTESIAN_POINT ( 'NONE',  ( 21.07928932188134397, 1.596973512272234830, -230.6572452218043736 ) ) ;
#103668 = ORIENTED_EDGE ( 'NONE', *, *, #143330, .T. ) ;
#103669 = DIRECTION ( 'NONE',  ( 0.000000000000000000, 0.2617529984165036239, 0.9651348961777156399 ) ) ;
#103670 = ORIENTED_EDGE ( 'NONE', *, *, #225396, .T. ) ;
#103672 = AXIS2_PLACEMENT_3D ( 'NONE', #159703, #181826, #220932 ) ;
#103671 = DIRECTION ( 'NONE',  ( 0.000000000000000000, -1.000000000000000000, 0.000000000000000000 ) ) ;
#103673 = VERTEX_POINT ( 'NONE', #42399 ) ;
#103674 = DIRECTION ( 'NONE',  ( 0.000000000000000000, 0.008583690987124697677, -0.9999631594459055250 ) ) ;
#103675 = FACE_OUTER_BOUND ( 'NONE', #212532, .T. ) ;
#103676 = ORIENTED_EDGE ( 'NONE', *, *, #32369, .T. ) ;
#103678 = VERTEX_POINT ( 'NONE', #222284 ) ;
#103677 = CARTESIAN_POINT ( 'NONE',  ( -18.59999999999999787, 80.82423061532404063, -192.8091306798888525 ) ) ;
#103679 = DIRECTION ( 'NONE',  ( -0.7071067811865475727, -0.7071067811865475727, 0.000000000000000000 ) ) ;
#103680 = ORIENTED_EDGE ( 'NONE', *, *, #230400, .T. ) ;
#103681 = SPHERICAL_SURFACE ( 'NONE', #60904, 0.1000000000000000056 ) ;
#103682 = AXIS2_PLACEMENT_3D ( 'NONE', #37796, #213841, #156472 ) ;
#103683 = CYLINDRICAL_SURFACE ( 'NONE', #39846, 0.09999999999999817368 ) ;
#103684 = AXIS2_PLACEMENT_3D ( 'NONE', #92720, #154044, #233546 ) ;
#103685 = ORIENTED_EDGE ( 'NONE', *, *, #244603, .F. ) ;
#103686 = VERTEX_POINT ( 'NONE', #81485 ) ;
#103687 = DIRECTION ( 'NONE',  ( -0.000000000000000000, -0.000000000000000000, -1.000000000000000000 ) ) ;
#103688 = EDGE_CURVE ( 'NONE', #210551, #131243, #202752, .T. ) ;
#103689 = AXIS2_PLACEMENT_3D ( 'NONE', #50642, #231893, #130186 ) ;
#103690 = FACE_OUTER_BOUND ( 'NONE', #135799, .T. ) ;
#103691 = MANIFOLD_SOLID_BREP ( 'Stock-MAS-200-1', #120133 ) ;
#103692 = VERTEX_POINT ( 'NONE', #201462 ) ;
#103693 = EDGE_LOOP ( 'NONE', ( #90917, #149284, #180011, #64367 ) ) ;
#103694 = FACE_OUTER_BOUND ( 'NONE', #240315, .T. ) ;
#103695 = EDGE_CURVE ( 'NONE', #230514, #19319, #243161, .T. ) ;
#103697 = VERTEX_POINT ( 'NONE', #119377 ) ;
#103696 = DIRECTION ( 'NONE',  ( 0.000000000000000000, 0.000000000000000000, 1.000000000000000000 ) ) ;
#103698 = EDGE_CURVE ( 'NONE', #84780, #55595, #238019, .T. ) ;
#103699 = DIRECTION ( 'NONE',  ( 0.000000000000000000, -6.982962677686266711E-15, 1.000000000000000000 ) ) ;
#103701 = EDGE_CURVE ( 'NONE', #84718, #256719, #181914, .T. ) ;
#103700 = AXIS2_PLACEMENT_3D ( 'NONE', #178618, #177342, #36547 ) ;
#103702 = DIRECTION ( 'NONE',  ( 1.000000000000000000, 0.000000000000000000, -0.000000000000000000 ) ) ;
#103703 = CARTESIAN_POINT ( 'NONE',  ( 11.60000000000006182, 67.75000000001118394, -23.62310748452479103 ) ) ;
#103704 = AXIS2_PLACEMENT_3D ( 'NONE', #125514, #8144, #205021 ) ;
#103706 = DIRECTION ( 'NONE',  ( 0.000000000000000000, -7.086529944415894657E-15, 1.000000000000000000 ) ) ;
#103705 = CARTESIAN_POINT ( 'NONE',  ( -18.41431012584568450, 64.51252797080390167, -127.2963434976260686 ) ) ;
#103707 = CARTESIAN_POINT ( 'NONE',  ( 21.04999999999999716, 10.50253167713731628, -108.0588298170750647 ) ) ;
#103708 = CARTESIAN_POINT ( 'NONE',  ( 18.49999999999999289, 70.22659352830977753, -197.9852579278363578 ) ) ;
#103709 = CARTESIAN_POINT ( 'NONE',  ( -16.86337532320261801, 60.88454159514807174, -221.1293591871273350 ) ) ;
#103710 = DIRECTION ( 'NONE',  ( -1.000000000000000000, -0.000000000000000000, -0.000000000000000000 ) ) ;
#103711 = AXIS2_PLACEMENT_3D ( 'NONE', #246681, #249272, #107172 ) ;
#103712 = ORIENTED_EDGE ( 'NONE', *, *, #40244, .F. ) ;
#103713 = ORIENTED_EDGE ( 'NONE', *, *, #89613, .F. ) ;
#103714 = EDGE_CURVE ( 'NONE', #127304, #247235, #10807, .T. ) ;
#103715 = CARTESIAN_POINT ( 'NONE',  ( 18.59999999999999432, 5.699452464332755319, -54.45772604343021328 ) ) ;
#103716 = ORIENTED_EDGE ( 'NONE', *, *, #27236, .T. ) ;
#103717 = CARTESIAN_POINT ( 'NONE',  ( -20.96077737575351918, 64.37609936600742344, -143.3823155274181147 ) ) ;
#103718 = EDGE_LOOP ( 'NONE', ( #192295, #6534, #57146 ) ) ;
#103719 = SURFACE_SIDE_STYLE ('',( #2064 ) ) ;
#103720 = DIRECTION ( 'NONE',  ( 1.000000000000000000, 0.000000000000000000, 0.000000000000000000 ) ) ;
#103721 = EDGE_LOOP ( 'NONE', ( #227828, #76486, #53675, #101951 ) ) ;
#103722 = CARTESIAN_POINT ( 'NONE',  ( -21.10257677756355932, 6.246520857501153934, -199.6140387306917603 ) ) ;
#103723 = VERTEX_POINT ( 'NONE', #64525 ) ;
#103724 = ORIENTED_EDGE ( 'NONE', *, *, #229472, .T. ) ;
#103725 = B_SPLINE_CURVE_WITH_KNOTS ( 'NONE', 3,
 ( #49475, #67755, #187723, #226823 ),
 .UNSPECIFIED., .F., .F.,
 ( 4, 4 ),
 ( 0.000000000000000000, 7.713889350929744009E-05 ),
 .UNSPECIFIED. ) ;
#103726 = DIRECTION ( 'NONE',  ( -1.000000000000000000, 0.000000000000000000, 0.000000000000000000 ) ) ;
#103727 = CARTESIAN_POINT ( 'NONE',  ( -21.13498764882296044, 75.99834360528066668, -109.5187256279982506 ) ) ;
#103729 = ORIENTED_EDGE ( 'NONE', *, *, #239841, .F. ) ;
#103728 = DIRECTION ( 'NONE',  ( 0.000000000000000000, 0.2128009952263485993, -0.9770955615653341697 ) ) ;
#103730 = ADVANCED_FACE ( 'NONE', ( #103627 ), #210157, .F. ) ;
#103731 = DIRECTION ( 'NONE',  ( -1.000000000000000000, 0.000000000000000000, 0.000000000000000000 ) ) ;
#103733 = ORIENTED_EDGE ( 'NONE', *, *, #248371, .T. ) ;
#103732 = DIRECTION ( 'NONE',  ( 0.000000000000000000, 0.000000000000000000, 1.000000000000000000 ) ) ;
#103734 = CARTESIAN_POINT ( 'NONE',  ( 20.01093837587850288, 11.75000000001116263, -125.2543974345976778 ) ) ;
#103735 = VERTEX_POINT ( 'NONE', #183203 ) ;
#103736 = CARTESIAN_POINT ( 'NONE',  ( -23.15000000000000213, 1.115600667400684642E-11, -67.00000000000000000 ) ) ;
#103738 = ORIENTED_EDGE ( 'NONE', *, *, #109596, .F. ) ;
#103737 = CARTESIAN_POINT ( 'NONE',  ( -18.59999999999999787, 76.00000000001142553, -36.02310748452432421 ) ) ;
#103739 = CARTESIAN_POINT ( 'NONE',  ( 21.00000000000000000, 66.25000000001179501, -81.77310748452437394 ) ) ;
#103740 = CARTESIAN_POINT ( 'NONE',  ( -15.66061380678752535, 26.81104512947605656, -233.6567807927322917 ) ) ;
#103742 = ADVANCED_FACE ( 'NONE', ( #39856 ), #144044, .T. ) ;
#103741 = DIRECTION ( 'NONE',  ( 0.000000000000000000, -0.4088369013363783999, 0.9126074666063545004 ) ) ;
#103743 = ORIENTED_EDGE ( 'NONE', *, *, #108779, .F. ) ;
#103744 = AXIS2_PLACEMENT_3D ( 'NONE', #88143, #244670, #184701 ) ;
#103747 = CARTESIAN_POINT ( 'NONE',  ( -21.13614978966382196, 69.50089529817890366, -203.5231074845243882 ) ) ;
#103746 = AXIS2_PLACEMENT_3D ( 'NONE', #64001, #208670, #86096 ) ;
#103745 = FACE_OUTER_BOUND ( 'NONE', #162108, .T. ) ;
#103748 = DIRECTION ( 'NONE',  ( 0.000000000000000000, 0.000000000000000000, -1.000000000000000000 ) ) ;
#103749 = VECTOR ( 'NONE', #232837, 1000.000000000000000 ) ;
#103750 = CIRCLE ( 'NONE', #91333, 11.65000000000000036 ) ;
#103751 = CARTESIAN_POINT ( 'NONE',  ( 18.59999999999999076, 65.79142135624952914, -148.6731074845244223 ) ) ;
#103752 = DIRECTION ( 'NONE',  ( 0.000000000000000000, -6.982962677686266711E-15, 1.000000000000000000 ) ) ;
#103753 = CARTESIAN_POINT ( 'NONE',  ( 18.39999999999999503, 8.822561741677553471, -91.25000000000005684 ) ) ;
#103754 = VERTEX_POINT ( 'NONE', #120678 ) ;
#103755 = VERTEX_POINT ( 'NONE', #200195 ) ;
#103756 = ORIENTED_EDGE ( 'NONE', *, *, #46370, .F. ) ;
#103757 = CYLINDRICAL_SURFACE ( 'NONE', #84720, 7.900000000000003908 ) ;
#103758 = CIRCLE ( 'NONE', #132846, 0.5000000000000004441 ) ;
#103759 = EDGE_LOOP ( 'NONE', ( #72422, #37889, #53658 ) ) ;
#103760 = CARTESIAN_POINT ( 'NONE',  ( -23.15000000000000213, 71.75000000001199396, -115.3731074845243256 ) ) ;
#103761 = ORIENTED_EDGE ( 'NONE', *, *, #203072, .T. ) ;
#103762 = DIRECTION ( 'NONE',  ( 0.000000000000000000, 0.2128009952263602289, -0.9770955615653316162 ) ) ;
#103763 = FILL_AREA_STYLE_COLOUR ( '', #81715 ) ;
#103764 = EDGE_CURVE ( 'NONE', #83171, #226085, #21563, .T. ) ;
#103765 = AXIS2_PLACEMENT_3D ( 'NONE', #87661, #69417, #246737 ) ;
#103766 = AXIS2_PLACEMENT_3D ( 'NONE', #33965, #53480, #195578 ) ;
#103767 = EDGE_LOOP ( 'NONE', ( #175686, #195418, #96065, #109492 ) ) ;
#103768 = TOROIDAL_SURFACE ( 'NONE', #70523, 0.6000000000000013101, 0.1000000000000000056 ) ;
#103769 = CARTESIAN_POINT ( 'NONE',  ( 15.73863059295127798, 9.351403174152812525, -150.9795304368385302 ) ) ;
#103770 = SURFACE_STYLE_USAGE ( .BOTH. , #24287 ) ;
#103771 = ORIENTED_EDGE ( 'NONE', *, *, #65192, .F. ) ;
#103772 = AXIS2_PLACEMENT_3D ( 'NONE', #154196, #233699, #236249 ) ;
#103773 = ORIENTED_EDGE ( 'NONE', *, *, #240097, .F. ) ;
#103774 = EDGE_LOOP ( 'NONE', ( #251594, #85901, #86106, #93652 ) ) ;
#103775 = ADVANCED_FACE ( 'NONE', ( #5817 ), #107498, .T. ) ;
#103776 = DIRECTION ( 'NONE',  ( -1.000000000000000000, 0.000000000000000000, 0.000000000000000000 ) ) ;
#103777 = FACE_OUTER_BOUND ( 'NONE', #83427, .T. ) ;
#103778 = DIRECTION ( 'NONE',  ( 0.000000000000000000, 0.2128009952263403282, -0.9770955615653358350 ) ) ;
#103779 = EDGE_CURVE ( 'NONE', #182882, #45390, #97687, .T. ) ;
#103780 = CARTESIAN_POINT ( 'NONE',  ( 15.69410316191958898, 26.71170214840295287, -233.6080780108829629 ) ) ;
#103781 = CARTESIAN_POINT ( 'NONE',  ( 23.40000000000005542, 82.64476912853859858, -26.37791261425322986 ) ) ;
#103782 = DIRECTION ( 'NONE',  ( 0.000000000000000000, -1.000000000000000000, -7.272083257015735086E-15 ) ) ;
#103784 = DIRECTION ( 'NONE',  ( 0.000000000000000000, 0.000000000000000000, 1.000000000000000000 ) ) ;
#103783 = CARTESIAN_POINT ( 'NONE',  ( 20.94999999999999929, 11.01970663298110154, -220.3481540650095098 ) ) ;
#103785 = CYLINDRICAL_SURFACE ( 'NONE', #253813, 1.749999999999999778 ) ;
#103787 = ORIENTED_EDGE ( 'NONE', *, *, #208715, .F. ) ;
#103786 = DIRECTION ( 'NONE',  ( 1.000000000000000000, 0.000000000000000000, 0.000000000000000000 ) ) ;
#103789 = CARTESIAN_POINT ( 'NONE',  ( 21.09316766718127667, 69.62984668753753681, -103.0623708868390622 ) ) ;
#103788 = CARTESIAN_POINT ( 'NONE',  ( 21.05000000000000071, 5.850000000000001421, -23.36750277572207679 ) ) ;
#103790 = EDGE_CURVE ( 'NONE', #109188, #6219, #233500, .T. ) ;
#103791 = CARTESIAN_POINT ( 'NONE',  ( 21.05000000000000071, 7.128833340093095217, -233.7327013124392749 ) ) ;
#103792 = EDGE_CURVE ( 'NONE', #151240, #94361, #243455, .T. ) ;
#103793 = ORIENTED_EDGE ( 'NONE', *, *, #165306, .F. ) ;
#103794 = CARTESIAN_POINT ( 'NONE',  ( -23.25000000000000000, 80.78317333349157536, -192.9003134612049166 ) ) ;
#103795 = FACE_OUTER_BOUND ( 'NONE', #209879, .T. ) ;
#103796 = CARTESIAN_POINT ( 'NONE',  ( 19.94784844284953707, 64.28691006698250021, -44.82090876722581640 ) ) ;
#103797 = ORIENTED_EDGE ( 'NONE', *, *, #24531, .T. ) ;
#103798 = EDGE_CURVE ( 'NONE', #224378, #106650, #73377, .T. ) ;
#103799 = AXIS2_PLACEMENT_3D ( 'NONE', #155270, #233507, #234768 ) ;
#103800 = ADVANCED_FACE ( 'NONE', ( #187067 ), #189862, .F. ) ;
#103801 = DIRECTION ( 'NONE',  ( -1.000000000000000000, -0.000000000000000000, -0.000000000000000000 ) ) ;
#103802 = DIRECTION ( 'NONE',  ( -0.000000000000000000, 1.000000000000000000, 6.982962677686266711E-15 ) ) ;
#103804 = EDGE_CURVE ( 'NONE', #10810, #48863, #47514, .T. ) ;
#103803 = EDGE_CURVE ( 'NONE', #208786, #60353, #90497, .T. ) ;
#103805 = ORIENTED_EDGE ( 'NONE', *, *, #19281, .F. ) ;
#103806 = ORIENTED_EDGE ( 'NONE', *, *, #70319, .T. ) ;
#103807 = ORIENTED_EDGE ( 'NONE', *, *, #250068, .T. ) ;
#103808 = CARTESIAN_POINT ( 'NONE',  ( 18.39999999999999503, 11.75000000001113953, -87.85000000000003695 ) ) ;
#103810 = CYLINDRICAL_SURFACE ( 'NONE', #24141, 0.1000000000000124678 ) ;
#103809 = CIRCLE ( 'NONE', #153778, 0.09999999999999939493 ) ;
#103811 = CARTESIAN_POINT ( 'NONE',  ( -23.25000000000000000, 11.75000000000000000, -26.48519422934605672 ) ) ;
#103812 = CARTESIAN_POINT ( 'NONE',  ( -16.77683809663752257, 42.27269979661959098, -221.1123729563994402 ) ) ;
#103813 = VERTEX_POINT ( 'NONE', #85342 ) ;
#103814 = DIRECTION ( 'NONE',  ( -1.000000000000000000, -0.000000000000000000, 0.000000000000000000 ) ) ;
#103815 = EDGE_CURVE ( 'NONE', #71995, #69705, #209167, .T. ) ;
#103816 = CARTESIAN_POINT ( 'NONE',  ( -18.59999999999999787, 11.65000000001115232, -100.5000000000000426 ) ) ;
#103817 = DIRECTION ( 'NONE',  ( 0.000000000000000000, -0.8814952561688430555, 0.4721928772777346239 ) ) ;
#103818 = DIRECTION ( 'NONE',  ( -0.000000000000000000, 0.2128009952263604232, -0.9770955615653316162 ) ) ;
#103819 = CIRCLE ( 'NONE', #149089, 0.09999999999999693856 ) ;
#103820 = ADVANCED_FACE ( 'NONE', ( #29297 ), #10975, .T. ) ;
#103821 = ADVANCED_FACE ( 'NONE', ( #206605 ), #228754, .T. ) ;
#103822 = AXIS2_PLACEMENT_3D ( 'NONE', #229926, #133399, #212931 ) ;
#103823 = ORIENTED_EDGE ( 'NONE', *, *, #192496, .T. ) ;
#103824 = AXIS2_PLACEMENT_3D ( 'NONE', #49719, #129261, #174855 ) ;
#103825 = ADVANCED_FACE ( 'NONE', ( #170095 ), #249597, .T. ) ;
#103827 = EDGE_LOOP ( 'NONE', ( #52396, #151899, #52680, #20485, #98237 ) ) ;
#103826 = CARTESIAN_POINT ( 'NONE',  ( 21.05000000000000071, 62.08591502004790641, -248.5699171172615820 ) ) ;
#103828 = DIRECTION ( 'NONE',  ( 0.000000000000000000, 0.000000000000000000, 1.000000000000000000 ) ) ;
#103829 = CARTESIAN_POINT ( 'NONE',  ( 18.47073956224749480, 78.23349094678856375, -231.4735393943770134 ) ) ;
#103830 = LINE ( 'NONE', #66011, #229515 ) ;
#103831 = FACE_OUTER_BOUND ( 'NONE', #113047, .T. ) ;
#103832 = EDGE_CURVE ( 'NONE', #41846, #48436, #164915, .T. ) ;
#103833 = VECTOR ( 'NONE', #52468, 1000.000000000000000 ) ;
#103834 = CYLINDRICAL_SURFACE ( 'NONE', #54867, 1.749999999999999778 ) ;
#103835 = CARTESIAN_POINT ( 'NONE',  ( 23.25000000000000000, -8.596261682231833845, -176.9501275171502641 ) ) ;
#103836 = AXIS2_PLACEMENT_3D ( 'NONE', #55440, #228987, #210697 ) ;
#103837 = ORIENTED_EDGE ( 'NONE', *, *, #72673, .F. ) ;
#103838 = DIRECTION ( 'NONE',  ( 1.000000000000000000, 0.000000000000000000, 0.000000000000000000 ) ) ;
#103839 = EDGE_CURVE ( 'NONE', #198094, #84743, #202332, .T. ) ;
#103840 = DIRECTION ( 'NONE',  ( 1.000000000000000000, 0.000000000000000000, 0.000000000000000000 ) ) ;
#103841 = SPHERICAL_SURFACE ( 'NONE', #196449, 0.1000000000000000056 ) ;
#103842 = CARTESIAN_POINT ( 'NONE',  ( -16.94107738177414291, 10.01423928514777373, -188.4499999999999886 ) ) ;
#103843 = VECTOR ( 'NONE', #34986, 1000.000000000000000 ) ;
#103845 = VERTEX_POINT ( 'NONE', #8416 ) ;
#103844 = AXIS2_PLACEMENT_3D ( 'NONE', #179195, #504, #176615 ) ;
#103846 = ORIENTED_EDGE ( 'NONE', *, *, #100846, .F. ) ;
#103847 = DIRECTION ( 'NONE',  ( 1.000000000000000000, 0.000000000000000000, 0.000000000000000000 ) ) ;
#103848 = VECTOR ( 'NONE', #209608, 1000.000000000000000 ) ;
#103849 = CARTESIAN_POINT ( 'NONE',  ( -18.59999999999999787, 7.668827189579289438, -241.6142244293585009 ) ) ;
#103850 = CARTESIAN_POINT ( 'NONE',  ( 21.53752568622130781, 0.09897446127749356948, -127.2131921254514566 ) ) ;
#103851 = CARTESIAN_POINT ( 'NONE',  ( 21.04386569057732004, 17.15049515251717338, -224.5321864300209427 ) ) ;
#103852 = AXIS2_PLACEMENT_3D ( 'NONE', #167946, #110500, #247448 ) ;
#103853 = ORIENTED_EDGE ( 'NONE', *, *, #174835, .F. ) ;
#103854 = CARTESIAN_POINT ( 'NONE',  ( 18.49999999999999289, 65.79142135624977072, -181.7731074845244450 ) ) ;
#103855 = DIRECTION ( 'NONE',  ( -0.000000000000000000, 6.982962677686266711E-15, -1.000000000000000000 ) ) ;
#103856 = CARTESIAN_POINT ( 'NONE',  ( 23.15000000000000213, -9.499999999988844479, -124.1060308773475924 ) ) ;
#103857 = PRODUCT_DEFINITION_SHAPE ( 'NONE', 'NONE',  #258127 ) ;
#103858 = CARTESIAN_POINT ( 'NONE',  ( -21.05000000000000071, 17.15380675273573985, -224.5473919504296703 ) ) ;
#103859 = AXIS2_PLACEMENT_3D ( 'NONE', #126549, #64003, #69164 ) ;
#103860 = VERTEX_POINT ( 'NONE', #87917 ) ;
#103861 = CARTESIAN_POINT ( 'NONE',  ( 21.05000000000000071, 76.00000000001195133, -102.9231074845243228 ) ) ;
#103862 = EDGE_LOOP ( 'NONE', ( #235284, #150093, #72736, #240669 ) ) ;
#103863 = CYLINDRICAL_SURFACE ( 'NONE', #168391, 0.09999999999999999167 ) ;
#103864 = CARTESIAN_POINT ( 'NONE',  ( -21.14999999999999858, -11.48087284838115707, -203.5004116939112464 ) ) ;
#103865 = CARTESIAN_POINT ( 'NONE',  ( 20.94999999999999929, 76.00000000001170974, -69.52310748452431710 ) ) ;
#103866 = CYLINDRICAL_SURFACE ( 'NONE', #73938, 0.5000000000000004441 ) ;
#103867 = CARTESIAN_POINT ( 'NONE',  ( -18.59999999999999787, 26.73568686665825567, -252.5275129665054408 ) ) ;
#103868 = CARTESIAN_POINT ( 'NONE',  ( 20.84999999999999432, 7.021664781911246322, -137.8335654018973457 ) ) ;
#103869 = FACE_OUTER_BOUND ( 'NONE', #47519, .T. ) ;
#103870 = CYLINDRICAL_SURFACE ( 'NONE', #210095, 0.8750000000000007772 ) ;
#103871 = AXIS2_PLACEMENT_3D ( 'NONE', #234813, #140853, #220396 ) ;
#103872 = DIRECTION ( 'NONE',  ( 0.000000000000000000, 0.000000000000000000, 1.000000000000000000 ) ) ;
#103873 = EDGE_CURVE ( 'NONE', #154195, #223089, #18614, .T. ) ;
#103874 = DIRECTION ( 'NONE',  ( -1.000000000000000000, 7.304098846218135653E-16, -4.607487905232624742E-31 ) ) ;
#103875 = TOROIDAL_SURFACE ( 'NONE', #212260, 0.6000000000000013101, 0.1000000000000000056 ) ;
#103876 = CARTESIAN_POINT ( 'NONE',  ( -21.05000000000000071, 76.00000000001165290, -69.52310748452431710 ) ) ;
#103877 = CARTESIAN_POINT ( 'NONE',  ( 18.45139536634708577, -9.486081720281200447, -40.14051161781065957 ) ) ;
#103878 = ADVANCED_FACE ( 'NONE', ( #192199 ), #98236, .T. ) ;
#103879 = CARTESIAN_POINT ( 'NONE',  ( 18.59999999999999787, -6.192768117006094641, -227.7812363988097388 ) ) ;
#103880 = CARTESIAN_POINT ( 'NONE',  ( -18.59999999999999787, 16.02417409648692725, -219.3605785455116006 ) ) ;
#103881 = CIRCLE ( 'NONE', #253731, 0.5000000000000004441 ) ;
#103882 = VERTEX_POINT ( 'NONE', #55199 ) ;
#103883 = DIRECTION ( 'NONE',  ( 0.000000000000000000, 0.000000000000000000, -1.000000000000000000 ) ) ;
#103885 = ADVANCED_FACE ( 'NONE', ( #171379 ), #213022, .T. ) ;
#103884 = DIRECTION ( 'NONE',  ( 0.000000000000000000, -7.116814260417668513E-15, 1.000000000000000000 ) ) ;
#103886 = ADVANCED_FACE ( 'NONE', ( #175232 ), #250851, .T. ) ;
#103887 = VERTEX_POINT ( 'NONE', #254673 ) ;
#103888 = CARTESIAN_POINT ( 'NONE',  ( -22.39999999999999858, 1.115600667400684642E-11, -55.35042919245524473 ) ) ;
#103889 = LINE ( 'NONE', #167769, #93990 ) ;
#103890 = AXIS2_PLACEMENT_3D ( 'NONE', #34957, #58307, #174487 ) ;
#103891 = DIRECTION ( 'NONE',  ( 1.000000000000000000, 0.000000000000000000, 0.000000000000000000 ) ) ;
#103892 = VECTOR ( 'NONE', #182634, 1000.000000000000000 ) ;
#103893 = EDGE_LOOP ( 'NONE', ( #192968, #108505, #48886, #103148 ) ) ;
#103894 = DIRECTION ( 'NONE',  ( 0.000000000000000000, 0.9915357197604804940, -0.1298341882520397950 ) ) ;
#103895 = CARTESIAN_POINT ( 'NONE',  ( 22.49999999999999645, 31.80488924422933295, -238.9605610896540213 ) ) ;
#103896 = ORIENTED_EDGE ( 'NONE', *, *, #92128, .F. ) ;
#103897 = CIRCLE ( 'NONE', #16646, 0.09999999999999939493 ) ;
#103898 = EDGE_CURVE ( 'NONE', #142573, #247975, #56186, .T. ) ;
#103899 = ORIENTED_EDGE ( 'NONE', *, *, #59997, .F. ) ;
#103900 = DIRECTION ( 'NONE',  ( 1.000000000000000000, 0.000000000000000000, 0.000000000000000000 ) ) ;
#103901 = VERTEX_POINT ( 'NONE', #93067 ) ;
#103902 = CARTESIAN_POINT ( 'NONE',  ( -25.10847955711010115, 9.068702471349579852, -347.0000000000001137 ) ) ;
#103903 = CARTESIAN_POINT ( 'NONE',  ( 22.59999999999999432, 0.1008583691098678542, -21.75043287651060808 ) ) ;
#103904 = DIRECTION ( 'NONE',  ( -0.000000000000000000, -0.000000000000000000, -1.000000000000000000 ) ) ;
#103905 = DIRECTION ( 'NONE',  ( 0.000000000000000000, 0.000000000000000000, 1.000000000000000000 ) ) ;
#103906 = CARTESIAN_POINT ( 'NONE',  ( -20.64999999999999858, 6.857177884343597540, -212.0437362999421680 ) ) ;
#103907 = CARTESIAN_POINT ( 'NONE',  ( -16.85697194749129935, 66.09145628588862564, -157.0881032169105822 ) ) ;
#103908 = CARTESIAN_POINT ( 'NONE',  ( -21.55000000000000071, 7.150000000000000355, -21.25000000000000000 ) ) ;
#103909 = DIRECTION ( 'NONE',  ( 0.000000000000000000, 0.000000000000000000, 1.000000000000000000 ) ) ;
#103911 = ORIENTED_EDGE ( 'NONE', *, *, #28471, .T. ) ;
#103910 = CARTESIAN_POINT ( 'NONE',  ( 18.46932045258648714, 87.08041872038211295, -199.6132627942399438 ) ) ;
#103912 = ORIENTED_EDGE ( 'NONE', *, *, #149399, .F. ) ;
#103915 = CARTESIAN_POINT ( 'NONE',  ( -20.94999999999999929, 79.26035508877831148, -236.0091442494974956 ) ) ;
#103914 = DIRECTION ( 'NONE',  ( 0.000000000000000000, 0.000000000000000000, 1.000000000000000000 ) ) ;
#103913 = AXIS2_PLACEMENT_3D ( 'NONE', #165198, #83049, #107786 ) ;
#103917 = ORIENTED_EDGE ( 'NONE', *, *, #87905, .T. ) ;
#103916 = CARTESIAN_POINT ( 'NONE',  ( -16.77180007708459186, 60.93559221856046548, -221.0556120513950873 ) ) ;
#103918 = ORIENTED_EDGE ( 'NONE', *, *, #235089, .T. ) ;
#103919 = ADVANCED_FACE ( 'NONE', ( #76077 ), #12281, .F. ) ;
#103920 = CARTESIAN_POINT ( 'NONE',  ( 23.50000000000005684, 74.83745509109094485, -44.02310748452479316 ) ) ;
#103921 = CARTESIAN_POINT ( 'NONE',  ( 20.21567752745019320, 10.19811410124265905, -175.3826203476516241 ) ) ;
#103922 = DIRECTION ( 'NONE',  ( 0.000000000000000000, 0.2128009952263485993, -0.9770955615653341697 ) ) ;
#103923 = CARTESIAN_POINT ( 'NONE',  ( -18.50000000000000000, 1.835341550235567887, -145.5551512925629822 ) ) ;
#103924 = CARTESIAN_POINT ( 'NONE',  ( -21.05000000000000071, 10.71906255309368383, -222.4921384173655383 ) ) ;
#103926 = EDGE_CURVE ( 'NONE', #240913, #79572, #231326, .T. ) ;
#103925 = FACE_OUTER_BOUND ( 'NONE', #74799, .T. ) ;
#103927 = EDGE_CURVE ( 'NONE', #13961, #9287, #214316, .T. ) ;
#103928 = CARTESIAN_POINT ( 'NONE',  ( -20.85000000000000142, 36.18002604163306302, -236.0784499204090991 ) ) ;
#103929 = AXIS2_PLACEMENT_3D ( 'NONE', #52895, #152030, #132441 ) ;
#103930 = ORIENTED_EDGE ( 'NONE', *, *, #100524, .F. ) ;
#103931 = ORIENTED_EDGE ( 'NONE', *, *, #212427, .T. ) ;
#103932 = TOROIDAL_SURFACE ( 'NONE', #33104, 11.70000000000000107, 0.1000000000000000056 ) ;
#103933 = CARTESIAN_POINT ( 'NONE',  ( -21.04999999999994387, 65.25000000001119815, -3.123107484524795474 ) ) ;
#103934 = AXIS2_PLACEMENT_3D ( 'NONE', #246927, #143974, #223506 ) ;
#103935 = VECTOR ( 'NONE', #44166, 1000.000000000000000 ) ;
#103936 = ORIENTED_EDGE ( 'NONE', *, *, #99434, .F. ) ;
#103937 = CARTESIAN_POINT ( 'NONE',  ( 22.57320508075687115, 64.25000000001237765, -170.0231074845244166 ) ) ;
#103938 = EDGE_LOOP ( 'NONE', ( #124409, #156827, #88495, #212921 ) ) ;
#103939 = DIRECTION ( 'NONE',  ( 0.000000000000000000, 0.000000000000000000, 1.000000000000000000 ) ) ;
#103940 = ADVANCED_FACE ( 'NONE', ( #34422 ), #256048, .F. ) ;
#103941 = CARTESIAN_POINT ( 'NONE',  ( -21.56666275994539816, 76.00000000001169553, -76.48047589141765457 ) ) ;
#103942 = CARTESIAN_POINT ( 'NONE',  ( -0.8999999999999437339, 67.65000000001118963, -10.02310748452479139 ) ) ;
#103943 = EDGE_CURVE ( 'NONE', #55329, #14291, #81134, .T. ) ;
#103944 = DIRECTION ( 'NONE',  ( 0.000000000000000000, 0.2617529984165031243, 0.9651348961777157509 ) ) ;
#103945 = ORIENTED_EDGE ( 'NONE', *, *, #233745, .T. ) ;
#103946 = ADVANCED_FACE ( 'NONE', ( #72243 ), #14852, .F. ) ;
#103947 = CARTESIAN_POINT ( 'NONE',  ( -18.69999999999999929, -9.749999999999996447, 31.39999999999999858 ) ) ;
#103948 = EDGE_LOOP ( 'NONE', ( #36931, #41349, #184923, #144401 ) ) ;
#103949 = CARTESIAN_POINT ( 'NONE',  ( 22.50000000000000000, 0.1000000000111554016, -122.3504291924552234 ) ) ;
#103950 = AXIS2_PLACEMENT_3D ( 'NONE', #244945, #243663, #65022 ) ;
#103951 = CARTESIAN_POINT ( 'NONE',  ( 18.39999999999999503, 5.650000000011139001, -57.75000000000000711 ) ) ;
#103953 = VECTOR ( 'NONE', #199574, 1000.000000000000000 ) ;
#103952 = DIRECTION ( 'NONE',  ( -1.000000000000000000, -7.125593699324843413E-30, 1.020425574104004196E-15 ) ) ;
#103954 = EDGE_CURVE ( 'NONE', #172545, #165339, #168686, .T. ) ;
#103955 = CARTESIAN_POINT ( 'NONE',  ( 21.05000000000000071, 7.128833340093095217, -233.7327013124392749 ) ) ;
#103956 = VERTEX_POINT ( 'NONE', #94346 ) ;
#103957 = DIRECTION ( 'NONE',  ( 1.186688945009009831E-16, 1.000000000000000000, 6.982962677686266711E-15 ) ) ;
#103958 = ORIENTED_EDGE ( 'NONE', *, *, #166570, .T. ) ;
#103961 = EDGE_LOOP ( 'NONE', ( #122660, #67064, #116899, #67845 ) ) ;
#103960 = DIRECTION ( 'NONE',  ( 0.000000000000000000, 0.8814952561688444987, -0.4721928772777320149 ) ) ;
#103959 = DIRECTION ( 'NONE',  ( 0.000000000000000000, 1.000000000000000000, 6.982962677686266711E-15 ) ) ;
#103962 = AXIS2_PLACEMENT_3D ( 'NONE', #116963, #52162, #79092 ) ;
#103963 = DIRECTION ( 'NONE',  ( -1.000000000000000000, -0.000000000000000000, -0.000000000000000000 ) ) ;
#103964 = EDGE_LOOP ( 'NONE', ( #133749, #242281, #119068, #166179, #178126 ) ) ;
#103965 = CARTESIAN_POINT ( 'NONE',  ( 23.24999999999999289, 6.650000000011155876, -155.1500000000000057 ) ) ;
#103966 = ORIENTED_EDGE ( 'NONE', *, *, #38552, .T. ) ;
#103967 = DIRECTION ( 'NONE',  ( 0.000000000000000000, 0.4999999999999943379, 0.8660254037844420383 ) ) ;
#103968 = EDGE_CURVE ( 'NONE', #232908, #173371, #201962, .T. ) ;
#103969 = CARTESIAN_POINT ( 'NONE',  ( -14.00000000000000178, 66.15000000001228386, -153.2731074845244166 ) ) ;
#103970 = DIRECTION ( 'NONE',  ( -1.000000000000000000, -0.000000000000000000, -0.000000000000000000 ) ) ;
#103971 = SPHERICAL_SURFACE ( 'NONE', #43441, 0.1000000000000000056 ) ;
#103972 = CARTESIAN_POINT ( 'NONE',  ( -16.88815647973234135, 9.950832619315736594, -12.64721706332599638 ) ) ;
#103973 = ORIENTED_EDGE ( 'NONE', *, *, #90626, .T. ) ;
#103974 = DIRECTION ( 'NONE',  ( -1.000000000000000000, -0.000000000000000000, -0.000000000000000000 ) ) ;
#103975 = LINE ( 'NONE', #182270, #24441 ) ;
#103976 = CARTESIAN_POINT ( 'NONE',  ( -14.45443560709638220, 66.54940788787860129, -154.9669191657160354 ) ) ;
#103977 = CIRCLE ( 'NONE', #37383, 0.1000000000000035305 ) ;
#103978 = ORIENTED_EDGE ( 'NONE', *, *, #166206, .F. ) ;
#103979 = CARTESIAN_POINT ( 'NONE',  ( -18.59999999999999787, 77.85161776048096272, -124.9199177649206689 ) ) ;
#103980 = ORIENTED_EDGE ( 'NONE', *, *, #173899, .T. ) ;
#103981 = FACE_OUTER_BOUND ( 'NONE', #86865, .T. ) ;
#103982 = DIRECTION ( 'NONE',  ( -1.000000000000000000, -0.000000000000000000, -0.000000000000000000 ) ) ;
#103983 = CARTESIAN_POINT ( 'NONE',  ( -21.05000000000000071, -11.64999999998884306, -198.0999999999999659 ) ) ;
#103984 = VECTOR ( 'NONE', #25223, 1000.000000000000000 ) ;
#103986 = ORIENTED_EDGE ( 'NONE', *, *, #208341, .T. ) ;
#103985 = CARTESIAN_POINT ( 'NONE',  ( -16.87683809663752754, 44.73333735360450447, -235.1232642955197605 ) ) ;
#103987 = CARTESIAN_POINT ( 'NONE',  ( 21.14999999999999503, -0.09999999999999939493, 11.64957080754479968 ) ) ;
#103988 = PLANE ( 'NONE',  #44373 ) ;
#103989 = DIRECTION ( 'NONE',  ( 0.000000000000000000, -1.000000000000000000, 0.000000000000000000 ) ) ;
#103990 = ORIENTED_EDGE ( 'NONE', *, *, #230667, .F. ) ;
#103991 = CARTESIAN_POINT ( 'NONE',  ( -23.15000000000000213, -11.74999999998884448, -134.0000000000000000 ) ) ;
#103992 = DIRECTION ( 'NONE',  ( 0.000000000000000000, 0.000000000000000000, -1.000000000000000000 ) ) ;
#103993 = ORIENTED_EDGE ( 'NONE', *, *, #168405, .F. ) ;
#103994 = CARTESIAN_POINT ( 'NONE',  ( -18.59999999999999787, 64.25000000001186606, -90.87310748452438247 ) ) ;
#103995 = AXIS2_PLACEMENT_3D ( 'NONE', #173548, #253022, #148806 ) ;
#103996 = AXIS2_PLACEMENT_3D ( 'NONE', #88819, #168441, #54834 ) ;
#103997 = VERTEX_POINT ( 'NONE', #51344 ) ;
#103998 = DIRECTION ( 'NONE',  ( 1.000000000000000000, 0.000000000000000000, 0.000000000000000000 ) ) ;
#104000 = EDGE_LOOP ( 'NONE', ( #3210, #185292, #161842, #131647 ) ) ;
#103999 = CARTESIAN_POINT ( 'NONE',  ( 23.24999999999999289, 64.35000000001258513, -191.3731074845244393 ) ) ;
#104001 = VECTOR ( 'NONE', #232775, 1000.000000000000000 ) ;
#104002 = EDGE_CURVE ( 'NONE', #255780, #163705, #63605, .T. ) ;
#104003 = AXIS2_PLACEMENT_3D ( 'NONE', #97700, #192994, #252942 ) ;
#104004 = AXIS2_PLACEMENT_3D ( 'NONE', #253043, #18290, #96519 ) ;
#104007 = ORIENTED_EDGE ( 'NONE', *, *, #43207, .T. ) ;
#104006 = ORIENTED_EDGE ( 'NONE', *, *, #228592, .T. ) ;
#104005 = LINE ( 'NONE', #124892, #188717 ) ;
#104008 = EDGE_CURVE ( 'NONE', #150585, #254139, #44050, .T. ) ;
#104009 = CARTESIAN_POINT ( 'NONE',  ( -22.39999999999999858, 29.54900078958453236, -252.7363208912387051 ) ) ;
#104010 = EDGE_CURVE ( 'NONE', #57105, #224804, #193574, .T. ) ;
#104011 = CARTESIAN_POINT ( 'NONE',  ( -23.25000000000000000, 36.02367271998545561, -235.8812521208699309 ) ) ;
#104012 = CARTESIAN_POINT ( 'NONE',  ( -21.05000000000000071, 72.02722222756958104, -225.1832529173024398 ) ) ;
#104014 = CARTESIAN_POINT ( 'NONE',  ( -16.94107738177414291, 10.01423928513661821, -20.94999999999999929 ) ) ;
#104013 = DIRECTION ( 'NONE',  ( 1.000000000000000000, -0.000000000000000000, -0.000000000000000000 ) ) ;
#104015 = DIRECTION ( 'NONE',  ( -1.000000000000000000, -0.000000000000000000, -0.000000000000000000 ) ) ;
#104016 = DIRECTION ( 'NONE',  ( 0.000000000000000000, 0.000000000000000000, -1.000000000000000000 ) ) ;
#104017 = AXIS2_PLACEMENT_3D ( 'NONE', #161231, #82930, #5976 ) ;
#104018 = CARTESIAN_POINT ( 'NONE',  ( -21.64999999999999858, 7.350000000011155166, -179.7499999999999716 ) ) ;
#104019 = FACE_OUTER_BOUND ( 'NONE', #204436, .T. ) ;
#104020 = AXIS2_PLACEMENT_3D ( 'NONE', #114826, #213929, #172285 ) ;
#104021 = ORIENTED_EDGE ( 'NONE', *, *, #10172, .F. ) ;
#104022 = CIRCLE ( 'NONE', #137350, 0.09999999999999939493 ) ;
#104024 = ORIENTED_EDGE ( 'NONE', *, *, #172929, .F. ) ;
#104023 = AXIS2_PLACEMENT_3D ( 'NONE', #63525, #127367, #106484 ) ;
#104025 = CARTESIAN_POINT ( 'NONE',  ( 21.05000000000000071, 87.48912529308822172, -139.6231074845242688 ) ) ;
#104027 = EDGE_LOOP ( 'NONE', ( #245983, #195268, #198937 ) ) ;
#104026 = CYLINDRICAL_SURFACE ( 'NONE', #107730, 0.1000000000000000472 ) ;
#104028 = ORIENTED_EDGE ( 'NONE', *, *, #59514, .T. ) ;
#104029 = EDGE_CURVE ( 'NONE', #71652, #23382, #67454, .T. ) ;
#104030 = CIRCLE ( 'NONE', #49887, 7.800000000000001599 ) ;
#104031 = CARTESIAN_POINT ( 'NONE',  ( -23.15000000000000213, 76.00000000001213607, -136.5231074845243313 ) ) ;
#104032 = ORIENTED_EDGE ( 'NONE', *, *, #179562, .T. ) ;
#104033 = DIRECTION ( 'NONE',  ( 0.000000000000000000, -0.9550021345545507412, 0.2965989261549202838 ) ) ;
#104034 = ORIENTED_EDGE ( 'NONE', *, *, #31191, .T. ) ;
#104035 = CYLINDRICAL_SURFACE ( 'NONE', #247782, 11.74999999999999645 ) ;
#104036 = LINE ( 'NONE', #246147, #36399 ) ;
#104038 = VERTEX_POINT ( 'NONE', #206973 ) ;
#104037 = ORIENTED_EDGE ( 'NONE', *, *, #69279, .F. ) ;
#104039 = VERTEX_POINT ( 'NONE', #10051 ) ;
#104040 = CARTESIAN_POINT ( 'NONE',  ( 22.39999999999999503, 7.790779598384535376, -100.5000000000000284 ) ) ;
#104041 = ORIENTED_EDGE ( 'NONE', *, *, #178777, .T. ) ;
#104042 = ORIENTED_EDGE ( 'NONE', *, *, #56662, .T. ) ;
#104043 = SPHERICAL_SURFACE ( 'NONE', #184565, 0.1000000000000000056 ) ;
#104044 = DIRECTION ( 'NONE',  ( -0.000000000000000000, -0.1350103645451876666, 0.9908441862701600211 ) ) ;
#104046 = ORIENTED_EDGE ( 'NONE', *, *, #216038, .T. ) ;
#104045 = CARTESIAN_POINT ( 'NONE',  ( 18.49999999999999645, -9.480686695267818820, -107.4411151687579036 ) ) ;
#104047 = EDGE_CURVE ( 'NONE', #153891, #53948, #109139, .T. ) ;
#104048 = EDGE_CURVE ( 'NONE', #104618, #69302, #60291, .T. ) ;
#104050 = CARTESIAN_POINT ( 'NONE',  ( -16.88815647973233780, 60.93782573408322634, -221.0441957042815773 ) ) ;
#104049 = SPHERICAL_SURFACE ( 'NONE', #78180, 0.1000000000000000056 ) ;
#104051 = PLANE ( 'NONE',  #49269 ) ;
#104053 = VERTEX_POINT ( 'NONE', #29652 ) ;
#104052 = DIRECTION ( 'NONE',  ( 0.000000000000000000, -0.9553114395363172529, -0.2956011730204217702 ) ) ;
#104054 = CARTESIAN_POINT ( 'NONE',  ( -21.40925344232282512, 6.658518859401606704, -66.90104981138040330 ) ) ;
#104055 = ORIENTED_EDGE ( 'NONE', *, *, #107422, .T. ) ;
#104056 = DIRECTION ( 'NONE',  ( 0.000000000000000000, -0.1455152366551721865, -0.9893560106964475187 ) ) ;
#104057 = AXIS2_PLACEMENT_3D ( 'NONE', #2282, #41458, #143081 ) ;
#104058 = ORIENTED_EDGE ( 'NONE', *, *, #147244, .F. ) ;
#104059 = DIRECTION ( 'NONE',  ( 1.000000000000000000, 3.190570557967288456E-16, 6.948722487160391713E-17 ) ) ;
#104060 = DIRECTION ( 'NONE',  ( 0.7071067811865463515, 0.2890913453342135453, -0.6453109281988460566 ) ) ;
#104061 = AXIS2_PLACEMENT_3D ( 'NONE', #2658, #198299, #79621 ) ;
#104062 = EDGE_CURVE ( 'NONE', #224583, #33354, #6306, .T. ) ;
#104063 = VERTEX_POINT ( 'NONE', #45328 ) ;
#104064 = DIRECTION ( 'NONE',  ( 0.000000000000000000, 0.000000000000000000, -1.000000000000000000 ) ) ;
#104065 = AXIS2_PLACEMENT_3D ( 'NONE', #32675, #31386, #14378 ) ;
#104066 = DIRECTION ( 'NONE',  ( -1.000000000000000000, -0.000000000000000000, 0.000000000000000000 ) ) ;
#104067 = DIRECTION ( 'NONE',  ( 0.000000000000000000, 0.8660254037844309360, -0.5000000000000134337 ) ) ;
#104068 = EDGE_LOOP ( 'NONE', ( #111306, #160381, #82456, #17862, #118404 ) ) ;
#104069 = ORIENTED_EDGE ( 'NONE', *, *, #233015, .F. ) ;
#104070 = DIRECTION ( 'NONE',  ( -0.000000000000000000, -0.2605042016806452532, -0.9654727137038777718 ) ) ;
#104071 = DIRECTION ( 'NONE',  ( 0.000000000000000000, 0.000000000000000000, 1.000000000000000000 ) ) ;
#104072 = ORIENTED_EDGE ( 'NONE', *, *, #244060, .F. ) ;
#104073 = DIRECTION ( 'NONE',  ( -0.000000000000000000, 1.000000000000000000, 0.000000000000000000 ) ) ;
#104074 = ORIENTED_EDGE ( 'NONE', *, *, #174940, .F. ) ;
#104075 = CARTESIAN_POINT ( 'NONE',  ( -20.54999999999999716, -8.663551401858001100, -57.47589888193270014 ) ) ;
#104076 = FACE_OUTER_BOUND ( 'NONE', #152212, .T. ) ;
#104078 = LINE ( 'NONE', #227905, #116950 ) ;
#104077 = CARTESIAN_POINT ( 'NONE',  ( -20.64999999999999858, 85.50000000001261924, -193.6291383618718385 ) ) ;
#104079 = CIRCLE ( 'NONE', #237384, 0.1000000000000028644 ) ;
#104080 = DIRECTION ( 'NONE',  ( 4.336808689942017736E-16, -0.000000000000000000, 1.000000000000000000 ) ) ;
#104081 = ADVANCED_FACE ( 'NONE', ( #188686 ), #124872, .F. ) ;
#104082 = DIRECTION ( 'NONE',  ( -0.000000000000000000, -6.982962677686266711E-15, 1.000000000000000000 ) ) ;
#104083 = AXIS2_PLACEMENT_3D ( 'NONE', #55911, #213728, #252848 ) ;
#104084 = VERTEX_POINT ( 'NONE', #84401 ) ;
#104085 = DIRECTION ( 'NONE',  ( -1.000000000000000000, 9.012599976028471648E-15, 6.882867235861662930E-14 ) ) ;
#104086 = B_SPLINE_CURVE_WITH_KNOTS ( 'NONE', 3,
 ( #100883, #222130, #160924, #240447, #61811, #108635, #207758, #52495, #90344, #149069 ),
 .UNSPECIFIED., .F., .F.,
 ( 4, 3, 3, 4 ),
 ( -2.000561356209491534E-06, 0.000000000000000000, 1.787822682428948123E-05, 4.206475347090082037E-05 ),
 .UNSPECIFIED. ) ;
#104088 = ORIENTED_EDGE ( 'NONE', *, *, #174037, .F. ) ;
#104087 = VERTEX_POINT ( 'NONE', #204388 ) ;
#104089 = ORIENTED_EDGE ( 'NONE', *, *, #213108, .F. ) ;
#104090 = EDGE_LOOP ( 'NONE', ( #256509, #218447, #174574, #215189 ) ) ;
#104091 = EDGE_CURVE ( 'NONE', #18932, #225036, #10421, .T. ) ;
#104092 = CARTESIAN_POINT ( 'NONE',  ( 21.07928932188134397, 6.328516656404459262, -33.40110485434561127 ) ) ;
#104093 = CARTESIAN_POINT ( 'NONE',  ( 23.25000000000000000, -11.74999999999999112, 11.75000000000000000 ) ) ;
#104094 = CARTESIAN_POINT ( 'NONE',  ( 20.27550659511088682, 66.78395627750303731, -93.77310748452437394 ) ) ;
#104095 = CARTESIAN_POINT ( 'NONE',  ( -18.59999999999999787, 5.899999999999947065, -10.21909976465641456 ) ) ;
#104097 = CARTESIAN_POINT ( 'NONE',  ( -18.79999999999999716, 11.49641995933507843, 1.885425182446135883 ) ) ;
#104096 = CARTESIAN_POINT ( 'NONE',  ( 22.14074124539698829, 68.60992214896791097, -69.62216038036844168 ) ) ;
#104099 = VERTEX_POINT ( 'NONE', #66176 ) ;
#104098 = CARTESIAN_POINT ( 'NONE',  ( -20.54999999999999716, -9.400000000000002132, -23.60603087734756045 ) ) ;
#104100 = CARTESIAN_POINT ( 'NONE',  ( -21.05000000000000071, 6.304961112695768755, -167.5213855659370665 ) ) ;
#104101 = ORIENTED_EDGE ( 'NONE', *, *, #167040, .F. ) ;
#104102 = EDGE_CURVE ( 'NONE', #154701, #24665, #43730, .T. ) ;
#104103 = LINE ( 'NONE', #183678, #228028 ) ;
#104104 = EDGE_CURVE ( 'NONE', #226316, #235224, #88275, .T. ) ;
#104105 = ORIENTED_EDGE ( 'NONE', *, *, #153866, .T. ) ;
#104106 = VERTEX_POINT ( 'NONE', #25770 ) ;
#104107 = CARTESIAN_POINT ( 'NONE',  ( -20.85000000000000142, 80.78317333349157536, -192.9003134612048882 ) ) ;
#104108 = CARTESIAN_POINT ( 'NONE',  ( 21.05000000000000426, 6.258817194681471463, 0.03363273533363692058 ) ) ;
#104109 = CARTESIAN_POINT ( 'NONE',  ( -16.77180007708460963, 66.05000000001153637, -48.65872160347922204 ) ) ;
#104110 = CARTESIAN_POINT ( 'NONE',  ( 21.04999999999999716, 65.31569084252754465, -195.9964106941975786 ) ) ;
#104111 = AXIS2_PLACEMENT_3D ( 'NONE', #143046, #221296, #67381 ) ;
#104112 = CIRCLE ( 'NONE', #249875, 0.5000000000000004441 ) ;
#104114 = EDGE_CURVE ( 'NONE', #231902, #64347, #247368, .T. ) ;
#104113 = EDGE_CURVE ( 'NONE', #54081, #98041, #145698, .T. ) ;
#104115 = CARTESIAN_POINT ( 'NONE',  ( -20.65000000000000568, 45.23934133962703186, -237.7629717664446787 ) ) ;
#104116 = EDGE_CURVE ( 'NONE', #178218, #46929, #189489, .T. ) ;
#104117 = ORIENTED_EDGE ( 'NONE', *, *, #150187, .T. ) ;
#104118 = ORIENTED_EDGE ( 'NONE', *, *, #91347, .T. ) ;
#104119 = DIRECTION ( 'NONE',  ( 1.000000000000000000, 0.000000000000000000, 0.000000000000000000 ) ) ;
#104120 = EDGE_LOOP ( 'NONE', ( #66950, #207069, #51664, #121402 ) ) ;
#104121 = DIRECTION ( 'NONE',  ( -1.000000000000000000, -1.794895427898103559E-16, -3.909090864890002444E-17 ) ) ;
#104122 = CARTESIAN_POINT ( 'NONE',  ( -16.94333152886235894, 9.990342011461638805, -46.10796846894559309 ) ) ;
#104123 = DIRECTION ( 'NONE',  ( -1.000000000000000000, 0.000000000000000000, 0.000000000000000000 ) ) ;
#104125 = EDGE_CURVE ( 'NONE', #226085, #79888, #6192, .T. ) ;
#104124 = CARTESIAN_POINT ( 'NONE',  ( -20.90000000000000213, 0.000000000000000000, 0.000000000000000000 ) ) ;
#104126 = CARTESIAN_POINT ( 'NONE',  ( -17.11825945287482753, 65.95000000001208207, -123.8731074845243683 ) ) ;
#104127 = CARTESIAN_POINT ( 'NONE',  ( 22.39999999999999503, 7.790779598384535376, -67.00000000000004263 ) ) ;
#104128 = CARTESIAN_POINT ( 'NONE',  ( 18.59999999999999076, 61.95000000001233076, -164.5094124137634708 ) ) ;
#104129 = CARTESIAN_POINT ( 'NONE',  ( 18.49999999999999645, 76.00000000001213607, -136.5231074845242745 ) ) ;
#104130 = DIRECTION ( 'NONE',  ( -0.000000000000000000, -0.000000000000000000, 1.000000000000000000 ) ) ;
#104131 = DIRECTION ( 'NONE',  ( -0.000000000000000000, 0.8660254037844377084, 0.5000000000000016653 ) ) ;
#104132 = CIRCLE ( 'NONE', #174941, 0.09999999999999939493 ) ;
#104133 = ADVANCED_FACE ( 'NONE', ( #183565 ), #64567, .F. ) ;
#104134 = CARTESIAN_POINT ( 'NONE',  ( -18.60000000000001208, 85.36424052760280290, -95.84285890268347430 ) ) ;
#104135 = CIRCLE ( 'NONE', #125019, 0.1000000000000055844 ) ;
#104136 = TOROIDAL_SURFACE ( 'NONE', #195760, 7.791421356237316687, 0.1000000000000000056 ) ;
#104137 = DIRECTION ( 'NONE',  ( -1.000000000000000000, 0.000000000000000000, 0.000000000000000000 ) ) ;
#104138 = EDGE_CURVE ( 'NONE', #157985, #47066, #205672, .T. ) ;
#104139 = EDGE_CURVE ( 'NONE', #139646, #95988, #114463, .T. ) ;
#104140 = VERTEX_POINT ( 'NONE', #12646 ) ;
#104141 = AXIS2_PLACEMENT_3D ( 'NONE', #161299, #122159, #183418 ) ;
#104142 = EDGE_CURVE ( 'NONE', #249282, #144177, #114287, .T. ) ;
#104143 = CARTESIAN_POINT ( 'NONE',  ( 20.95576188350343116, 10.60898054497455689, -41.11123372275429944 ) ) ;
#104144 = ORIENTED_EDGE ( 'NONE', *, *, #205065, .F. ) ;
#104145 =( REPRESENTATION_RELATIONSHIP ('NONE','NONE', #36900, #171686 ) REPRESENTATION_RELATIONSHIP_WITH_TRANSFORMATION ( #169342 )SHAPE_REPRESENTATION_RELATIONSHIP( ) );
#104146 = CARTESIAN_POINT ( 'NONE',  ( -33.72168855820452649, 48.78215419113038109, -213.4964773079645681 ) ) ;
#104147 = EDGE_CURVE ( 'NONE', #129130, #129914, #154729, .T. ) ;
#104148 = DIRECTION ( 'NONE',  ( 1.000000000000000000, -0.000000000000000000, -0.000000000000000000 ) ) ;
#104149 = FACE_OUTER_BOUND ( 'NONE', #240498, .T. ) ;
#104150 = CIRCLE ( 'NONE', #220697, 0.09999999999999939493 ) ;
#104151 = ADVANCED_FACE ( 'NONE', ( #229108 ), #13917, .T. ) ;
#104152 = VERTEX_POINT ( 'NONE', #50438 ) ;
#104154 = TOROIDAL_SURFACE ( 'NONE', #25091, 12.77499999999999858, 0.1000000000000000056 ) ;
#104153 = CARTESIAN_POINT ( 'NONE',  ( -21.05000000000000071, 74.83729825007431202, -161.9231074845243654 ) ) ;
#104156 = EDGE_CURVE ( 'NONE', #253143, #4110, #126940, .T. ) ;
#104155 = DIRECTION ( 'NONE',  ( 1.000000000000000000, -0.000000000000000000, -0.000000000000000000 ) ) ;
#104157 = DIRECTION ( 'NONE',  ( 1.000000000000000000, 0.000000000000000000, 0.000000000000000000 ) ) ;
#104158 = CARTESIAN_POINT ( 'NONE',  ( 18.50000000000000000, 85.40000000001165859, -62.64106563635156277 ) ) ;
#104159 = CARTESIAN_POINT ( 'NONE',  ( 20.94999999999999574, 11.62071067812981795, -60.13158334765904556 ) ) ;
#104160 = EDGE_LOOP ( 'NONE', ( #164808, #220294, #5289, #96564 ) ) ;
#104161 = DIRECTION ( 'NONE',  ( -1.000000000000000000, 0.000000000000000000, 0.000000000000000000 ) ) ;
#104163 = ORIENTED_EDGE ( 'NONE', *, *, #4722, .F. ) ;
#104162 = CARTESIAN_POINT ( 'NONE',  ( 22.49436431346199683, 11.64995094766461392, -167.4330964702777180 ) ) ;
#104164 = CARTESIAN_POINT ( 'NONE',  ( 22.59999954896768770, -0.008828232233025335232, -122.2494913259320128 ) ) ;
#104165 =( BOUNDED_SURFACE ( )  B_SPLINE_SURFACE ( 3, 2, ( 
 ( #173629, #253094, #74518 ),
 ( #54890, #208847, #198262 ),
 ( #75768, #219099, #59 ),
 ( #256908, #120049, #57458 ),
 ( #95319, #78307, #37936 ),
 ( #155326, #217807, #58729 ) ),
 .UNSPECIFIED., .F., .F., .F. ) 
 B_SPLINE_SURFACE_WITH_KNOTS ( ( 4, 2, 4 ),
 ( 3, 3 ),
 ( 0.0001300404313046639351, 0.0003183318589266644245, 0.0005066232865486648869 ),
 ( 0.000000000000000000, 1.000000000000000000 ),
 .UNSPECIFIED. ) 
 GEOMETRIC_REPRESENTATION_ITEM ( )  RATIONAL_B_SPLINE_SURFACE ( (
 ( 1.000000000000000000, 0.7071067811865475727, 1.000000000000000000),
 ( 1.000000000000000000, 0.7625113560541101343, 1.000000000000000000),
 ( 1.000000000000000000, 0.8126073484687262871, 1.000000000000000000),
 ( 1.000000000000000000, 0.8923049332733591354, 1.000000000000000000),
 ( 1.000000000000000000, 0.9231914937768681551, 1.000000000000000000),
 ( 1.000000000000000000, 0.9238795325112909573, 1.000000000000000000) ) ) 
 REPRESENTATION_ITEM ( '' )  SURFACE ( )  );
#104166 = CYLINDRICAL_SURFACE ( 'NONE', #62050, 3.999999999999996447 ) ;
#104167 = EDGE_CURVE ( 'NONE', #241189, #157564, #191292, .T. ) ;
#104168 = CARTESIAN_POINT ( 'NONE',  ( -21.05000000000000071, 1.115653327213047955E-11, -129.7000000000000455 ) ) ;
#104169 = ORIENTED_EDGE ( 'NONE', *, *, #163323, .T. ) ;
#104170 = CARTESIAN_POINT ( 'NONE',  ( -18.59999999999999787, 77.63717271298244782, -124.9409541190522788 ) ) ;
#104171 = EDGE_CURVE ( 'NONE', #178016, #219323, #171732, .T. ) ;
#104172 = ITEM_DEFINED_TRANSFORMATION ( 'NONE', 'NONE', #36132,  #2425 ) ;
#104173 = CARTESIAN_POINT ( 'NONE',  ( -18.39999999999999858, -9.499999999988849808, -40.49928567783884858 ) ) ;
#104174 = EDGE_LOOP ( 'NONE', ( #204908, #198324, #106377, #154078 ) ) ;
#104175 = DIRECTION ( 'NONE',  ( 0.000000000000000000, 0.000000000000000000, 1.000000000000000000 ) ) ;
#104176 = DIRECTION ( 'NONE',  ( 1.000000000000000000, 7.304098846218135653E-16, 5.311601492717085047E-30 ) ) ;
#104177 = VECTOR ( 'NONE', #227714, 999.9999999999998863 ) ;
#104178 = CARTESIAN_POINT ( 'NONE',  ( -12.25000000000000178, 62.10905854918435409, -217.1108499610990918 ) ) ;
#104179 = ORIENTED_EDGE ( 'NONE', *, *, #33667, .F. ) ;
#104180 = AXIS2_PLACEMENT_3D ( 'NONE', #11790, #170891, #151292 ) ;
#104181 = ORIENTED_EDGE ( 'NONE', *, *, #115449, .T. ) ;
#104182 = LINE ( 'NONE', #143319, #147306 ) ;
#104183 = CARTESIAN_POINT ( 'NONE',  ( 21.05000000000000071, 1.115623935689868526E-11, -132.1000000000000227 ) ) ;
#104184 = CARTESIAN_POINT ( 'NONE',  ( 21.15000000000005187, 74.16448838626247664, -47.62760213295649692 ) ) ;
#104185 = CARTESIAN_POINT ( 'NONE',  ( -23.15000000000000213, 71.75000000001156764, -57.17310748452435121 ) ) ;
#104186 = CARTESIAN_POINT ( 'NONE',  ( -17.11825945287481332, 14.13772148853350252, -219.1573629999798811 ) ) ;
#104187 = DIRECTION ( 'NONE',  ( 1.000000000000000000, -0.000000000000000000, -0.000000000000000000 ) ) ;
#104188 = CYLINDRICAL_SURFACE ( 'NONE', #101530, 0.09999999999999939493 ) ;
#104190 = LINE ( 'NONE', #165482, #91222 ) ;
#104189 = CARTESIAN_POINT ( 'NONE',  ( 20.95378194480896639, 65.46508800846910958, -95.45805333637652268 ) ) ;
#104191 = ADVANCED_FACE ( 'NONE', ( #132577 ), #133196, .F. ) ;
#104192 = CARTESIAN_POINT ( 'NONE',  ( 21.14999999999999858, 22.07612373182271881, -231.7717111801312342 ) ) ;
#104193 = FACE_OUTER_BOUND ( 'NONE', #114874, .T. ) ;
#104194 = CARTESIAN_POINT ( 'NONE',  ( -21.14999999999994174, 83.98667523412385094, -37.28476067066772970 ) ) ;
#104195 = DIRECTION ( 'NONE',  ( 0.000000000000000000, -0.1022405907414166426, -0.9947597004326453884 ) ) ;
#104196 = VECTOR ( 'NONE', #97771, 1000.000000000000000 ) ;
#104197 = VERTEX_POINT ( 'NONE', #195140 ) ;
#104198 = EDGE_CURVE ( 'NONE', #219574, #227124, #110434, .T. ) ;
#104199 = ORIENTED_EDGE ( 'NONE', *, *, #123596, .F. ) ;
#104200 = FACE_OUTER_BOUND ( 'NONE', #15711, .T. ) ;
#104201 = AXIS2_PLACEMENT_3D ( 'NONE', #100368, #236054, #155274 ) ;
#104202 = DIRECTION ( 'NONE',  ( -1.000000000000000000, 0.000000000000000000, 0.000000000000000000 ) ) ;
#104204 = DIRECTION ( 'NONE',  ( 0.000000000000000000, -0.9770955615653315052, -0.2128009952263603954 ) ) ;
#104203 = DIRECTION ( 'NONE',  ( 1.000000000000000000, 0.000000000000000000, 0.000000000000000000 ) ) ;
#104205 = AXIS2_PLACEMENT_3D ( 'NONE', #13415, #176350, #92924 ) ;
#104206 = DIRECTION ( 'NONE',  ( 3.265361837132813093E-16, 0.9651348961777157509, -0.2617529984165031243 ) ) ;
#104207 = CARTESIAN_POINT ( 'NONE',  ( -18.59999999999999787, 61.47936603916259912, -212.1738987416902376 ) ) ;
#104208 = CIRCLE ( 'NONE', #66633, 4.049999999999998046 ) ;
#104209 = DIRECTION ( 'NONE',  ( 0.000000000000000000, 0.000000000000000000, 1.000000000000000000 ) ) ;
#104210 = CIRCLE ( 'NONE', #208285, 0.09999999999998898659 ) ;
#104211 = VERTEX_POINT ( 'NONE', #30936 ) ;
#104212 = CARTESIAN_POINT ( 'NONE',  ( -20.64999999999999858, 54.14029358995846053, -238.9803212882090691 ) ) ;
#104213 = ORIENTED_EDGE ( 'NONE', *, *, #180665, .F. ) ;
#104214 = ADVANCED_FACE ( 'NONE', ( #11341 ), #147796, .T. ) ;
#104215 = CARTESIAN_POINT ( 'NONE',  ( -18.43707690579160641, -9.682403433465239573, -73.65684337741278398 ) ) ;
#104216 = AXIS2_PLACEMENT_3D ( 'NONE', #44817, #222136, #83894 ) ;
#104217 = AXIS2_PLACEMENT_3D ( 'NONE', #165883, #182883, #4207 ) ;
#104219 = CIRCLE ( 'NONE', #100111, 0.09999999999999939493 ) ;
#104218 = CARTESIAN_POINT ( 'NONE',  ( -18.59999999999999787, 14.78417726655519360, -235.8865342417136333 ) ) ;
#104220 = ORIENTED_EDGE ( 'NONE', *, *, #135608, .T. ) ;
#104221 = CARTESIAN_POINT ( 'NONE',  ( -18.55807992284872299, 18.40923646582965389, -236.9894833875398206 ) ) ;
#104222 = EDGE_LOOP ( 'NONE', ( #80751, #146022, #151036, #38310 ) ) ;
#104223 = CARTESIAN_POINT ( 'NONE',  ( -21.05000000000000071, 64.25000000001249134, -177.0379132551784096 ) ) ;
#104224 = DIRECTION ( 'NONE',  ( 0.000000000000000000, -0.9876197685951265681, -0.1568667991644790149 ) ) ;
#104225 = FACE_OUTER_BOUND ( 'NONE', #119448, .T. ) ;
#104226 = CARTESIAN_POINT ( 'NONE',  ( -18.59999999999999787, 3.912899247244609580, -78.48182297301100618 ) ) ;
#104227 = FACE_OUTER_BOUND ( 'NONE', #181677, .T. ) ;
#104228 = AXIS2_PLACEMENT_3D ( 'NONE', #87970, #207970, #171431 ) ;
#104229 = DIRECTION ( 'NONE',  ( -1.000000000000000000, 0.000000000000000000, 0.000000000000000000 ) ) ;
#104230 = DIRECTION ( 'NONE',  ( -1.000000000000000000, -0.000000000000000000, -0.000000000000000000 ) ) ;
#104231 = VERTEX_POINT ( 'NONE', #170465 ) ;
#104233 = CARTESIAN_POINT ( 'NONE',  ( 18.49999999999999289, 6.650000000011155876, -121.8500000000000369 ) ) ;
#104232 = CARTESIAN_POINT ( 'NONE',  ( -22.50000000000000000, 1.115600667400684642E-11, -94.25000000000002842 ) ) ;
#104234 = ORIENTED_EDGE ( 'NONE', *, *, #23504, .T. ) ;
#104236 = EDGE_LOOP ( 'NONE', ( #20900, #203864, #64137, #251262 ) ) ;
#104235 = CARTESIAN_POINT ( 'NONE',  ( 21.05000000000000071, 67.12338541492553645, -195.1380270056797599 ) ) ;
#104237 = ORIENTED_EDGE ( 'NONE', *, *, #34436, .T. ) ;
#104238 = FACE_OUTER_BOUND ( 'NONE', #206929, .T. ) ;
#104239 = DIRECTION ( 'NONE',  ( 0.000000000000000000, 0.000000000000000000, 1.000000000000000000 ) ) ;
#104240 = ORIENTED_EDGE ( 'NONE', *, *, #200378, .T. ) ;
#104241 = CARTESIAN_POINT ( 'NONE',  ( 21.05000000000000071, -11.74999999998883560, -64.10000000000000853 ) ) ;
#104242 = CARTESIAN_POINT ( 'NONE',  ( -20.54999999999999716, 2.000000000011154189, -53.77537807723790309 ) ) ;
#104243 = DIRECTION ( 'NONE',  ( 0.000000000000000000, 6.982962677686266711E-15, -1.000000000000000000 ) ) ;
#104244 = ORIENTED_EDGE ( 'NONE', *, *, #148365, .F. ) ;
#104245 = EDGE_CURVE ( 'NONE', #43771, #196423, #178137, .T. ) ;
#104246 = AXIS2_PLACEMENT_3D ( 'NONE', #40841, #119069, #78631 ) ;
#104247 = CARTESIAN_POINT ( 'NONE',  ( -2.995603634470891112E-16, 69.35000000001222986, -148.7731074845244166 ) ) ;
#104248 = CIRCLE ( 'NONE', #16804, 0.1000000000000000472 ) ;
#104249 = EDGE_CURVE ( 'NONE', #79334, #98643, #81548, .T. ) ;
#104250 = DIRECTION ( 'NONE',  ( 0.000000000000000000, -0.9126074666063733742, -0.4088369013363362114 ) ) ;
#104251 = EDGE_LOOP ( 'NONE', ( #2411, #126358, #182695, #12335 ) ) ;
#104252 = ORIENTED_EDGE ( 'NONE', *, *, #161579, .F. ) ;
#104253 = DIRECTION ( 'NONE',  ( 0.000000000000000000, 0.000000000000000000, 1.000000000000000000 ) ) ;
#104254 = CIRCLE ( 'NONE', #95882, 12.87499999999999822 ) ;
#104255 = ORIENTED_EDGE ( 'NONE', *, *, #240748, .F. ) ;
#104256 = CARTESIAN_POINT ( 'NONE',  ( -18.79999999999999716, 11.49641995933507843, -1.885425182446133885 ) ) ;
#104257 = ORIENTED_EDGE ( 'NONE', *, *, #243435, .F. ) ;
#104258 = CARTESIAN_POINT ( 'NONE',  ( -20.94999999999999929, 4.481636728799211156, -245.1292951062512770 ) ) ;
#104259 =( BOUNDED_SURFACE ( )  B_SPLINE_SURFACE ( 3, 2, ( 
 ( #166998, #61438, #116925 ),
 ( #96059, #247775, #190394 ),
 ( #226928, #151262, #129119 ),
 ( #216003, #109534, #175631 ),
 ( #209953, #31338, #131680 ),
 ( #207384, #36120, #115642 ) ),
 .UNSPECIFIED., .F., .F., .F. ) 
 B_SPLINE_SURFACE_WITH_KNOTS ( ( 4, 2, 4 ),
 ( 3, 3 ),
 ( 4.712388980384689674, 5.497787143782137953, 6.283185307179586232 ),
 ( 0.000000000000000000, 1.000000000000000000 ),
 .UNSPECIFIED. ) 
 GEOMETRIC_REPRESENTATION_ITEM ( )  RATIONAL_B_SPLINE_SURFACE ( (
 ( 1.000000000000000000, 0.7071067811865536790, 1.000000000000000000),
 ( 1.000000000000000000, 0.7727932973486136836, 1.000000000000000000),
 ( 1.000000000000000000, 0.8282379607656571441, 1.000000000000000000),
 ( 1.000000000000000000, 0.9038128468032184948, 1.000000000000000000),
 ( 1.000000000000000000, 0.9240297172249232194, 1.000000000000000000),
 ( 1.000000000000000000, 0.9238795325112914014, 1.000000000000000000) ) ) 
 REPRESENTATION_ITEM ( '' )  SURFACE ( )  );
#104260 = EDGE_CURVE ( 'NONE', #200406, #2987, #80260, .T. ) ;
#104261 = CARTESIAN_POINT ( 'NONE',  ( 19.97071067811865674, 11.72071067811866385, -24.65000000000000213 ) ) ;
#104262 = CARTESIAN_POINT ( 'NONE',  ( -21.93340585972178758, 68.67585297715976367, -103.0231074845243597 ) ) ;
#104263 = CARTESIAN_POINT ( 'NONE',  ( -21.14999999999999858, 30.68987205111127281, -252.2252246220829193 ) ) ;
#104264 = ADVANCED_FACE ( 'NONE', ( #200248 ), #101092, .F. ) ;
#104265 = CARTESIAN_POINT ( 'NONE',  ( 20.95512820512820440, 10.62384868372303259, -179.6499999999999773 ) ) ;
#104266 = ORIENTED_EDGE ( 'NONE', *, *, #222705, .T. ) ;
#104267 = LINE ( 'NONE', #27367, #111668 ) ;
#104268 = CARTESIAN_POINT ( 'NONE',  ( -16.87036670365548474, 66.01058118071090064, -182.5435473672224020 ) ) ;
#104269 = ADVANCED_FACE ( 'NONE', ( #21620 ), #120737, .F. ) ;
#104270 = CARTESIAN_POINT ( 'NONE',  ( 18.58703555224997928, 85.40633674080056892, -62.39816284327772422 ) ) ;
#104271 = DIRECTION ( 'NONE',  ( 1.000000000000000000, 0.000000000000000000, 0.000000000000000000 ) ) ;
#104272 = ORIENTED_EDGE ( 'NONE', *, *, #229081, .T. ) ;
#104275 = DIRECTION ( 'NONE',  ( -1.000000000000000000, 1.836970198721029934E-16, 1.282749433769087582E-30 ) ) ;
#104274 = DIRECTION ( 'NONE',  ( 0.000000000000000000, 0.000000000000000000, -1.000000000000000000 ) ) ;
#104273 = AXIS2_PLACEMENT_3D ( 'NONE', #258017, #63715, #140687 ) ;
#104276 = VERTEX_POINT ( 'NONE', #77708 ) ;
#104279 = ORIENTED_EDGE ( 'NONE', *, *, #50887, .F. ) ;
#104278 = DIRECTION ( 'NONE',  ( 0.000000000000000000, 0.9770955615653316162, 0.2128009952263604232 ) ) ;
#104277 = DIRECTION ( 'NONE',  ( 0.000000000000000000, -6.547589603894034005E-15, 1.000000000000000000 ) ) ;
#104280 = CIRCLE ( 'NONE', #54210, 0.1000000000000009354 ) ;
#104281 = ORIENTED_EDGE ( 'NONE', *, *, #55510, .F. ) ;
#104282 = CARTESIAN_POINT ( 'NONE',  ( 21.13461538461538325, 65.38541703798675542, -157.6731074845244223 ) ) ;
#104283 = VECTOR ( 'NONE', #227217, 999.9999999999998863 ) ;
#104284 = CARTESIAN_POINT ( 'NONE',  ( -18.40000000000000213, 53.98582189624752914, -228.9137301112145622 ) ) ;
#104285 = DIRECTION ( 'NONE',  ( -3.265361837132813093E-16, -1.000000000000000000, -6.982962677686266711E-15 ) ) ;
#104286 = ORIENTED_EDGE ( 'NONE', *, *, #118265, .F. ) ;
#104287 = CARTESIAN_POINT ( 'NONE',  ( 20.94999999999999574, -11.74999999998883560, -103.6000000000000369 ) ) ;
#104288 = ADVANCED_FACE ( 'NONE', ( #118141 ), #159854, .T. ) ;
#104289 = DIRECTION ( 'NONE',  ( 0.000000000000000000, 0.000000000000000000, -1.000000000000000000 ) ) ;
#104291 = CARTESIAN_POINT ( 'NONE',  ( -23.25000000000000355, 10.05000000001113847, -54.25000000000000711 ) ) ;
#104290 = DIRECTION ( 'NONE',  ( 1.000000000000000000, -7.304098846218135653E-16, -5.100424963727256530E-30 ) ) ;
#104293 = EDGE_LOOP ( 'NONE', ( #164706, #157946, #128780, #60717 ) ) ;
#104292 = DIRECTION ( 'NONE',  ( 0.000000000000000000, -0.9651348961777157509, 0.2617529984165031243 ) ) ;
#104294 = CIRCLE ( 'NONE', #112518, 11.75000000000000000 ) ;
#104295 = ORIENTED_EDGE ( 'NONE', *, *, #249562, .T. ) ;
#104296 = DIRECTION ( 'NONE',  ( 2.952720810173289112E-16, 1.000000000000000000, -6.088138035986627436E-46 ) ) ;
#104297 = CARTESIAN_POINT ( 'NONE',  ( -20.54999999999999716, 55.48145342050126061, -241.1189016111836736 ) ) ;
#104298 = DIRECTION ( 'NONE',  ( -1.000000000000000000, 0.000000000000000000, 0.000000000000000000 ) ) ;
#104299 = ORIENTED_EDGE ( 'NONE', *, *, #194553, .T. ) ;
#104300 = DIRECTION ( 'NONE',  ( 1.000000000000000000, 0.000000000000000000, 0.000000000000000000 ) ) ;
#104301 = ORIENTED_EDGE ( 'NONE', *, *, #145570, .T. ) ;
#104302 = CARTESIAN_POINT ( 'NONE',  ( 23.24999999999999645, 76.00000000001126921, -203.5231074845248997 ) ) ;
#104303 = CARTESIAN_POINT ( 'NONE',  ( -18.40000000000000213, 70.35000000001224407, -149.1731074845243938 ) ) ;
#104304 = CARTESIAN_POINT ( 'NONE',  ( -23.25000000000000000, 73.40000000001180069, -82.74772940728642823 ) ) ;
#104305 = EDGE_LOOP ( 'NONE', ( #195030, #100781, #68822, #213224 ) ) ;
#104306 = DIRECTION ( 'NONE',  ( 0.000000000000000000, -6.982962677686267499E-15, 1.000000000000000000 ) ) ;
#104307 = TOROIDAL_SURFACE ( 'NONE', #29360, 0.2000000000000000111, 0.1000000000000000056 ) ;
#104308 = AXIS2_PLACEMENT_3D ( 'NONE', #207424, #69207, #107006 ) ;
#104309 = CIRCLE ( 'NONE', #233534, 0.09999999999999516220 ) ;
#104310 = DIRECTION ( 'NONE',  ( 0.000000000000000000, -1.000000000000000000, -6.982962677686265922E-15 ) ) ;
#104311 = ADVANCED_FACE ( 'NONE', ( #180691 ), #99824, .F. ) ;
#104312 = ORIENTED_EDGE ( 'NONE', *, *, #88488, .T. ) ;
#104313 = TOROIDAL_SURFACE ( 'NONE', #154280, 0.2000000000000000111, 0.1000000000000000056 ) ;
#104314 = ORIENTED_EDGE ( 'NONE', *, *, #145944, .F. ) ;
#104315 = EDGE_LOOP ( 'NONE', ( #134554, #32205, #109407 ) ) ;
#104316 = DIRECTION ( 'NONE',  ( 0.000000000000000000, 6.982962677686267499E-15, -1.000000000000000000 ) ) ;
#104317 = VERTEX_POINT ( 'NONE', #140247 ) ;
#104319 = VERTEX_POINT ( 'NONE', #62032 ) ;
#104318 = DIRECTION ( 'NONE',  ( 0.000000000000000000, 0.000000000000000000, 1.000000000000000000 ) ) ;
#104320 = ADVANCED_FACE ( 'NONE', ( #41200 ), #141547, .T. ) ;
#104321 = EDGE_LOOP ( 'NONE', ( #173909, #186113, #112568, #14986, #21078 ) ) ;
#104322 = VECTOR ( 'NONE', #228311, 999.9999999999998863 ) ;
#104325 = ORIENTED_EDGE ( 'NONE', *, *, #51178, .T. ) ;
#104324 = ORIENTED_EDGE ( 'NONE', *, *, #217612, .F. ) ;
#104323 = DIRECTION ( 'NONE',  ( 0.000000000000000000, -0.2617529984161274248, -0.9651348961778176694 ) ) ;
#104326 = EDGE_CURVE ( 'NONE', #194632, #107433, #68881, .T. ) ;
#104327 = EDGE_CURVE ( 'NONE', #152504, #165054, #235510, .T. ) ;
#104328 = DIRECTION ( 'NONE',  ( -1.836970198721029934E-16, -0.9651348961777157509, 0.2617529984165031243 ) ) ;
#104329 = VERTEX_POINT ( 'NONE', #56845 ) ;
#104330 = DIRECTION ( 'NONE',  ( -1.000000000000000000, 0.000000000000000000, 0.000000000000000000 ) ) ;
#104331 = CARTESIAN_POINT ( 'NONE',  ( 20.94999999999999929, 67.07338541492552508, -195.0514244653012952 ) ) ;
#104332 = CARTESIAN_POINT ( 'NONE',  ( -18.43459694179560060, 86.89521445562479585, -199.6219428230616870 ) ) ;
#104333 = ORIENTED_EDGE ( 'NONE', *, *, #43332, .F. ) ;
#104334 = LINE ( 'NONE', #27436, #8079 ) ;
#104336 = VERTEX_POINT ( 'NONE', #136382 ) ;
#104335 = DIRECTION ( 'NONE',  ( 1.000000000000000000, 0.000000000000000000, 0.000000000000000000 ) ) ;
#104337 = DIRECTION ( 'NONE',  ( 0.000000000000000000, -0.1350103645451876666, -0.9908441862701600211 ) ) ;
#104339 = EDGE_LOOP ( 'NONE', ( #119948, #196904, #139441, #38574 ) ) ;
#104338 = CARTESIAN_POINT ( 'NONE',  ( 18.59999999999999076, 68.48451787451661232, -224.2224406095231757 ) ) ;
#104340 = EDGE_CURVE ( 'NONE', #121302, #77215, #39918, .T. ) ;
#104341 = AXIS2_PLACEMENT_3D ( 'NONE', #228954, #66020, #145547 ) ;
#104342 = EDGE_LOOP ( 'NONE', ( #148329, #192300, #78887, #174442 ) ) ;
#104343 = EDGE_CURVE ( 'NONE', #226091, #225564, #77221, .T. ) ;
#104344 = CIRCLE ( 'NONE', #233571, 0.1999999999999999833 ) ;
#104345 = ORIENTED_EDGE ( 'NONE', *, *, #118512, .T. ) ;
#104346 = VERTEX_POINT ( 'NONE', #95991 ) ;
#104347 = CYLINDRICAL_SURFACE ( 'NONE', #89356, 9.500000000000001776 ) ;
#104348 = LINE ( 'NONE', #203480, #90343 ) ;
#104350 = ORIENTED_EDGE ( 'NONE', *, *, #48822, .F. ) ;
#104349 = VERTEX_POINT ( 'NONE', #215938 ) ;
#104351 = VERTEX_POINT ( 'NONE', #37338 ) ;
#104352 = CARTESIAN_POINT ( 'NONE',  ( 20.85000000000000142, 87.65000000001141700, -36.02310748452423894 ) ) ;
#104353 = ORIENTED_EDGE ( 'NONE', *, *, #103695, .T. ) ;
#104354 = EDGE_LOOP ( 'NONE', ( #222774, #85735, #215588, #25956 ) ) ;
#104355 = EDGE_CURVE ( 'NONE', #184724, #63280, #196384, .T. ) ;
#104356 = DIRECTION ( 'NONE',  ( -0.000000000000000000, -0.000000000000000000, -1.000000000000000000 ) ) ;
#104357 = AXIS2_PLACEMENT_3D ( 'NONE', #203871, #23982, #146450 ) ;
#104359 = ORIENTED_EDGE ( 'NONE', *, *, #248291, .F. ) ;
#104358 = FACE_OUTER_BOUND ( 'NONE', #220133, .T. ) ;
#104360 = ADVANCED_FACE ( 'NONE', ( #137679 ), #256295, .F. ) ;
#104361 = CARTESIAN_POINT ( 'NONE',  ( 20.90000000000000213, 1.800000000000000044, -11.61130914238355771 ) ) ;
#104362 = EDGE_CURVE ( 'NONE', #59075, #143156, #85559, .T. ) ;
#104364 = CARTESIAN_POINT ( 'NONE',  ( 18.43473516226073983, -9.494942282747041773, -107.5458986833495203 ) ) ;
#104363 = CARTESIAN_POINT ( 'NONE',  ( -16.94445028196808778, 22.96031635112858282, -230.8778361528912058 ) ) ;
#104365 = EDGE_LOOP ( 'NONE', ( #23682, #216641, #104074, #179205 ) ) ;
#104367 = ORIENTED_EDGE ( 'NONE', *, *, #179802, .F. ) ;
#104366 = EDGE_LOOP ( 'NONE', ( #92310, #250951, #91513, #190110 ) ) ;
#104368 = DIRECTION ( 'NONE',  ( -1.000000000000000000, -0.000000000000000000, -0.000000000000000000 ) ) ;
#104369 = DIRECTION ( 'NONE',  ( 0.000000000000000000, 0.000000000000000000, 1.000000000000000000 ) ) ;
#104371 = ORIENTED_EDGE ( 'NONE', *, *, #30050, .F. ) ;
#104370 = AXIS2_PLACEMENT_3D ( 'NONE', #192760, #74119, #88484 ) ;
#104372 = CIRCLE ( 'NONE', #4425, 0.09999999999999939493 ) ;
#104373 = AXIS2_PLACEMENT_3D ( 'NONE', #77311, #74805, #56457 ) ;
#104374 = DIRECTION ( 'NONE',  ( -0.000000000000000000, -0.1350103645451835865, -0.9908441862701606873 ) ) ;
#104375 = ORIENTED_EDGE ( 'NONE', *, *, #250201, .T. ) ;
#104376 = ORIENTED_EDGE ( 'NONE', *, *, #93471, .T. ) ;
#104377 = ORIENTED_EDGE ( 'NONE', *, *, #57573, .T. ) ;
#104378 = CARTESIAN_POINT ( 'NONE',  ( -21.05439746398122836, 11.75000000001115197, -107.4899164874846065 ) ) ;
#104379 = CARTESIAN_POINT ( 'NONE',  ( -21.55000000000000071, 9.809744668562228043, -211.5030428704195913 ) ) ;
#104380 = ORIENTED_EDGE ( 'NONE', *, *, #47147, .F. ) ;
#104381 = CARTESIAN_POINT ( 'NONE',  ( 19.94784844284954417, 64.28691006698312549, -145.3209087672257454 ) ) ;
#104383 = CIRCLE ( 'NONE', #12853, 0.2000000000000111688 ) ;
#104382 = CARTESIAN_POINT ( 'NONE',  ( 18.59999999999999432, 1.261786168565025568, -8.086498963545480478 ) ) ;
#104385 = DIRECTION ( 'NONE',  ( 1.000000000000000000, 0.000000000000000000, 0.000000000000000000 ) ) ;
#104384 = DIRECTION ( 'NONE',  ( 0.000000000000000000, 0.000000000000000000, -1.000000000000000000 ) ) ;
#104386 = FACE_OUTER_BOUND ( 'NONE', #217115, .T. ) ;
#104387 = LINE ( 'NONE', #166999, #20163 ) ;
#104388 = LINE ( 'NONE', #62728, #40680 ) ;
#104389 = EDGE_CURVE ( 'NONE', #98885, #172803, #227070, .T. ) ;
#104390 = DIRECTION ( 'NONE',  ( -1.000000000000000000, 0.000000000000000000, 0.000000000000000000 ) ) ;
#104391 = EDGE_LOOP ( 'NONE', ( #212800, #173727, #6334, #133844 ) ) ;
#104392 = AXIS2_PLACEMENT_3D ( 'NONE', #180834, #140399, #238221 ) ;
#104393 = VECTOR ( 'NONE', #164588, 999.9999999999998863 ) ;
#104394 = AXIS2_PLACEMENT_3D ( 'NONE', #187569, #208413, #170604 ) ;
#104395 = AXIS2_PLACEMENT_3D ( 'NONE', #29770, #93550, #149707 ) ;
#104397 = ORIENTED_EDGE ( 'NONE', *, *, #5446, .F. ) ;
#104396 = ORIENTED_EDGE ( 'NONE', *, *, #14294, .F. ) ;
#104398 = ORIENTED_EDGE ( 'NONE', *, *, #170301, .F. ) ;
#104399 = ADVANCED_FACE ( 'NONE', ( #166294 ), #8477, .T. ) ;
#104400 = LINE ( 'NONE', #100539, #136869 ) ;
#104401 = DIRECTION ( 'NONE',  ( 1.000000000000000000, 0.000000000000000000, 0.000000000000000000 ) ) ;
#104403 = CARTESIAN_POINT ( 'NONE',  ( 21.51976009735019346, 6.910458441659201867, 1.166362318020008541E-16 ) ) ;
#104402 = CARTESIAN_POINT ( 'NONE',  ( 20.27550659511088682, 9.216043722520002035, -76.25000000000004263 ) ) ;
#104404 = DIRECTION ( 'NONE',  ( 0.000000000000000000, 0.9126074666063769270, 0.4088369013363283844 ) ) ;
#104405 = ORIENTED_EDGE ( 'NONE', *, *, #125972, .F. ) ;
#104406 = EDGE_CURVE ( 'NONE', #148114, #80096, #206238, .T. ) ;
#104407 = DIRECTION ( 'NONE',  ( 1.000000000000000000, 0.000000000000000000, 0.000000000000000000 ) ) ;
#104408 = CIRCLE ( 'NONE', #100314, 0.09999999999999939493 ) ;
#104409 = CARTESIAN_POINT ( 'NONE',  ( -21.05000000000000071, 77.25000000001263345, -195.5231074845243313 ) ) ;
#104410 = CARTESIAN_POINT ( 'NONE',  ( -16.97683809663752186, 66.05000000001187743, -89.62074346632789457 ) ) ;
#104411 = EDGE_CURVE ( 'NONE', #199698, #217161, #110547, .T. ) ;
#104412 = DIRECTION ( 'NONE',  ( -1.000000000000000000, 0.000000000000000000, 0.000000000000000000 ) ) ;
#104413 = ORIENTED_EDGE ( 'NONE', *, *, #145040, .T. ) ;
#104414 = CARTESIAN_POINT ( 'NONE',  ( -18.59999999999999787, 72.08710075277885210, -158.5412845115134246 ) ) ;
#104415 = ADVANCED_FACE ( 'NONE', ( #163698 ), #172956, .F. ) ;
#104416 = LINE ( 'NONE', #23659, #172035 ) ;
#104417 = EDGE_CURVE ( 'NONE', #138284, #68660, #123028, .T. ) ;
#104418 = ORIENTED_EDGE ( 'NONE', *, *, #153652, .T. ) ;
#104419 = PLANE ( 'NONE',  #253629 ) ;
#104420 = DIRECTION ( 'NONE',  ( 0.000000000000000000, 6.982962677686266711E-15, -1.000000000000000000 ) ) ;
#104421 = SPHERICAL_SURFACE ( 'NONE', #77866, 0.1000000000000000056 ) ;
#104422 = DIRECTION ( 'NONE',  ( 0.000000000000000000, -0.000000000000000000, 1.000000000000000000 ) ) ;
#104423 = DIRECTION ( 'NONE',  ( 0.000000000000000000, -0.2617529984165152257, -0.9651348961777124202 ) ) ;
#104424 = ORIENTED_EDGE ( 'NONE', *, *, #3741, .F. ) ;
#104425 = CARTESIAN_POINT ( 'NONE',  ( -21.14999999999999858, 12.71802988599559292, -223.5105008658000258 ) ) ;
#104426 = LINE ( 'NONE', #81018, #13167 ) ;
#104427 = AXIS2_PLACEMENT_3D ( 'NONE', #160484, #60058, #139579 ) ;
#104428 = CARTESIAN_POINT ( 'NONE',  ( -21.13422380239058640, 1.115662971600936638E-11, -60.50667348519461797 ) ) ;
#104430 = CARTESIAN_POINT ( 'NONE',  ( -20.85000000000000142, -1.164121893230052995, -208.9148480855715775 ) ) ;
#104429 = CARTESIAN_POINT ( 'NONE',  ( -16.87683809663752399, 66.15000000001205649, -123.1207434663280651 ) ) ;
#104431 = FACE_OUTER_BOUND ( 'NONE', #60147, .T. ) ;
#104432 = LINE ( 'NONE', #1496, #37432 ) ;
#104433 = CARTESIAN_POINT ( 'NONE',  ( 20.10000000000000853, 4.625944962820097039, 22.03401928653448749 ) ) ;
#104434 = DIRECTION ( 'NONE',  ( 0.000000000000000000, -6.853228547068871147E-15, 1.000000000000000000 ) ) ;
#104437 = EDGE_LOOP ( 'NONE', ( #82763, #185559, #112859, #144982 ) ) ;
#104436 = VECTOR ( 'NONE', #158275, 1000.000000000000114 ) ;
#104435 = CARTESIAN_POINT ( 'NONE',  ( -23.25000000000000000, 5.950000000011163692, -123.6942976949652149 ) ) ;
#104438 = EDGE_CURVE ( 'NONE', #140891, #95981, #10611, .T. ) ;
#104439 = ADVANCED_FACE ( 'NONE', ( #183256 ), #241930, .T. ) ;
#104440 = VECTOR ( 'NONE', #21711, 1000.000000000000114 ) ;
#104441 = EDGE_CURVE ( 'NONE', #66665, #5506, #118946, .T. ) ;
#104442 = DIRECTION ( 'NONE',  ( 0.000000000000000000, 7.026728003956695223E-15, -1.000000000000000000 ) ) ;
#104443 = AXIS2_PLACEMENT_3D ( 'NONE', #4016, #58828, #123982 ) ;
#104444 = EDGE_CURVE ( 'NONE', #5997, #160190, #206670, .T. ) ;
#104445 = CARTESIAN_POINT ( 'NONE',  ( 18.49999999999999645, 1.115600667400684642E-11, -67.00000000000000000 ) ) ;
#104446 = EDGE_CURVE ( 'NONE', #177256, #254325, #63292, .T. ) ;
#104447 = CARTESIAN_POINT ( 'NONE',  ( -18.50000000000000000, 55.91711482281190371, -232.6830152854666949 ) ) ;
#104448 = VECTOR ( 'NONE', #56961, 1000.000000000000227 ) ;
#104449 = EDGE_LOOP ( 'NONE', ( #8434, #86257, #10749, #74928 ) ) ;
#104450 = CIRCLE ( 'NONE', #129421, 0.1000000000000028644 ) ;
#104451 = DIRECTION ( 'NONE',  ( -1.000000000000000000, 0.000000000000000000, -0.000000000000000000 ) ) ;
#104452 = DIRECTION ( 'NONE',  ( 0.000000000000000000, 7.086529944415886769E-15, -1.000000000000000000 ) ) ;
#104454 = LINE ( 'NONE', #147459, #169554 ) ;
#104453 = AXIS2_PLACEMENT_3D ( 'NONE', #7746, #91122, #87252 ) ;
#104455 = ADVANCED_FACE ( 'NONE', ( #7164 ), #26775, .F. ) ;
#104456 = ORIENTED_EDGE ( 'NONE', *, *, #236818, .T. ) ;
#104457 = CARTESIAN_POINT ( 'NONE',  ( -20.64999999999999858, 74.00000000001151079, -49.24772940728643533 ) ) ;
#104459 = VERTEX_POINT ( 'NONE', #5878 ) ;
#104458 = LINE ( 'NONE', #5355, #155043 ) ;
#104461 = CARTESIAN_POINT ( 'NONE',  ( -16.81931177881022066, 66.06300394050791169, -82.24988960590717113 ) ) ;
#104460 = CARTESIAN_POINT ( 'NONE',  ( 21.12230431290520016, -1.369086087588080813, -194.6892316229322262 ) ) ;
#104462 = DIRECTION ( 'NONE',  ( 0.000000000000000000, -0.9910827722268049644, -0.1332476588733589318 ) ) ;
#104463 = ORIENTED_EDGE ( 'NONE', *, *, #182724, .F. ) ;
#104464 = CARTESIAN_POINT ( 'NONE',  ( -21.64999999999999858, 60.62847850914943848, -224.4802381816402317 ) ) ;
#104465 = ADVANCED_FACE ( 'NONE', ( #244503 ), #156374, .T. ) ;
#104466 = CARTESIAN_POINT ( 'NONE',  ( 21.14999999999999858, 76.00000000001205080, -124.3731074845242972 ) ) ;
#104467 = CARTESIAN_POINT ( 'NONE',  ( 22.39999999999999503, 76.00000000001170974, -77.27310748452433131 ) ) ;
#104468 = DIRECTION ( 'NONE',  ( 5.603264701231745086E-32, -1.897661533703520636E-16, 1.000000000000000000 ) ) ;
#104469 = CIRCLE ( 'NONE', #196084, 0.1999999999999996503 ) ;
#104470 = ORIENTED_EDGE ( 'NONE', *, *, #115605, .F. ) ;
#104471 = DIRECTION ( 'NONE',  ( 0.000000000000000000, -1.000000000000000000, 0.000000000000000000 ) ) ;
#104472 = PLANE ( 'NONE',  #176446 ) ;
#104473 = CARTESIAN_POINT ( 'NONE',  ( 20.94999999999999929, -9.399999999988844834, -90.60603087734760663 ) ) ;
#104474 = ORIENTED_EDGE ( 'NONE', *, *, #152170, .T. ) ;
#104475 = EDGE_LOOP ( 'NONE', ( #89420, #46973, #221647, #117514 ) ) ;
#104476 = CARTESIAN_POINT ( 'NONE',  ( 22.49999999999999645, 75.89914163091300736, -81.27267460801373034 ) ) ;
#104477 = DIRECTION ( 'NONE',  ( 0.000000000000000000, 0.000000000000000000, -1.000000000000000000 ) ) ;
#104478 = CARTESIAN_POINT ( 'NONE',  ( 21.05000000000000071, 76.00000000001267608, -203.5231074845243597 ) ) ;
#104479 = CIRCLE ( 'NONE', #241872, 2.100000000000002309 ) ;
#104480 = CARTESIAN_POINT ( 'NONE',  ( 21.00000000000000000, -0.3305886640091971196, 0.04453801223857078301 ) ) ;
#104482 = CARTESIAN_POINT ( 'NONE',  ( -18.40000000000000213, 11.47316190337362940, -79.60857864376274051 ) ) ;
#104481 = AXIS2_PLACEMENT_3D ( 'NONE', #11803, #252938, #172182 ) ;
#104483 = VECTOR ( 'NONE', #222211, 1000.000000000000000 ) ;
#104486 = DIRECTION ( 'NONE',  ( 1.000000000000000000, 0.000000000000000000, 0.000000000000000000 ) ) ;
#104485 = CIRCLE ( 'NONE', #4542, 0.1000000000000032113 ) ;
#104484 = CARTESIAN_POINT ( 'NONE',  ( -23.15000000000000213, 52.81534179157633702, -244.1198638051726277 ) ) ;
#104487 = DIRECTION ( 'NONE',  ( 1.000000000000000000, 0.000000000000000000, 0.000000000000000000 ) ) ;
#104488 = CARTESIAN_POINT ( 'NONE',  ( -21.05000000000000071, 76.10000000001218723, -143.0637644362255401 ) ) ;
#104489 = CARTESIAN_POINT ( 'NONE',  ( -18.58693740092193636, 47.00678169108851989, -255.2226550330250348 ) ) ;
#104490 = DIRECTION ( 'NONE',  ( 1.186688945009010077E-16, -1.000000000000000000, -0.000000000000000000 ) ) ;
#104492 = EDGE_LOOP ( 'NONE', ( #146330, #253532, #39772, #172835 ) ) ;
#104491 = CARTESIAN_POINT ( 'NONE',  ( -20.54999999999999716, 71.65000000001222702, -148.8731074845244109 ) ) ;
#104493 = AXIS2_PLACEMENT_3D ( 'NONE', #167401, #124405, #24031 ) ;
#104494 = FACE_OUTER_BOUND ( 'NONE', #194543, .T. ) ;
#104495 = DIRECTION ( 'NONE',  ( 1.000000000000000000, 0.000000000000000000, 0.000000000000000000 ) ) ;
#104497 = CARTESIAN_POINT ( 'NONE',  ( 22.10000000000000142, -11.65000000000000036, 12.09999999999999609 ) ) ;
#104496 = DIRECTION ( 'NONE',  ( 0.000000000000000000, -0.000000000000000000, 1.000000000000000000 ) ) ;
#104498 = ADVANCED_FACE ( 'NONE', ( #107554 ), #103683, .F. ) ;
#104499 = VERTEX_POINT ( 'NONE', #45025 ) ;
#104500 = DIRECTION ( 'NONE',  ( 0.000000000000000000, 8.896017825522085641E-15, -1.000000000000000000 ) ) ;
#104501 = CARTESIAN_POINT ( 'NONE',  ( -17.22361732159832215, 10.34515565861359221, -111.8707845258671654 ) ) ;
#104502 = DIRECTION ( 'NONE',  ( -0.000000000000000000, -0.8700118002898321601, 0.4930308989875230030 ) ) ;
#104503 = LINE ( 'NONE', #45843, #195264 ) ;
#104504 = CARTESIAN_POINT ( 'NONE',  ( -20.94999999999999929, 1.162701749949165642, -142.0000000000000284 ) ) ;
#104505 = ORIENTED_EDGE ( 'NONE', *, *, #204809, .T. ) ;
#104507 = ORIENTED_EDGE ( 'NONE', *, *, #80809, .T. ) ;
#104506 = TOROIDAL_SURFACE ( 'NONE', #250276, 0.6000000000000004219, 0.1000000000000000056 ) ;
#104508 = DIRECTION ( 'NONE',  ( 0.000000000000000000, -0.4721928772777346239, -0.8814952561688430555 ) ) ;
#104509 = ORIENTED_EDGE ( 'NONE', *, *, #116054, .F. ) ;
#104510 = EDGE_CURVE ( 'NONE', #242308, #173093, #58844, .T. ) ;
#104511 = CARTESIAN_POINT ( 'NONE',  ( -20.54999999999999716, -4.259020970815408091, -226.0869574510824123 ) ) ;
#104512 = VERTEX_POINT ( 'NONE', #113977 ) ;
#104513 = CARTESIAN_POINT ( 'NONE',  ( -23.15000000000000213, -11.39257802169451139, -130.9260504201681101 ) ) ;
#104514 = CARTESIAN_POINT ( 'NONE',  ( 21.05000000000000071, -8.999999999988842703, -124.1060308773475924 ) ) ;
#104515 = FACE_OUTER_BOUND ( 'NONE', #166382, .T. ) ;
#104516 = ORIENTED_EDGE ( 'NONE', *, *, #77976, .T. ) ;
#104517 = AXIS2_PLACEMENT_3D ( 'NONE', #66374, #22133, #162928 ) ;
#104518 = LINE ( 'NONE', #207523, #215865 ) ;
#104519 = LINE ( 'NONE', #26310, #209128 ) ;
#104520 = CARTESIAN_POINT ( 'NONE',  ( 20.94999999999999574, 16.52766025697963315, -240.8672687545768270 ) ) ;
#104521 = AXIS2_PLACEMENT_3D ( 'NONE', #171276, #151695, #30445 ) ;
#104522 = FACE_OUTER_BOUND ( 'NONE', #90373, .T. ) ;
#104523 = LINE ( 'NONE', #86249, #122795 ) ;
#104524 = CARTESIAN_POINT ( 'NONE',  ( 23.24999999999999289, 70.05000000001197691, -113.3288097895591591 ) ) ;
#104526 = CARTESIAN_POINT ( 'NONE',  ( 14.77516762759922386, 62.09620004573545771, -218.7373296619003327 ) ) ;
#104525 = AXIS2_PLACEMENT_3D ( 'NONE', #157581, #160125, #237073 ) ;
#104527 = ORIENTED_EDGE ( 'NONE', *, *, #93467, .F. ) ;
#104529 = CARTESIAN_POINT ( 'NONE',  ( -16.87036670365549895, 9.989418819312803066, -46.02043988269794994 ) ) ;
#104528 = DIRECTION ( 'NONE',  ( -0.000000000000000000, -0.2617529984165031243, -0.9651348961777157509 ) ) ;
#104530 = ORIENTED_EDGE ( 'NONE', *, *, #88027, .T. ) ;
#104532 = ORIENTED_EDGE ( 'NONE', *, *, #248577, .T. ) ;
#104531 = CARTESIAN_POINT ( 'NONE',  ( 21.14999999999999858, 67.21339244341174890, -90.67310748452436542 ) ) ;
#104533 = ORIENTED_EDGE ( 'NONE', *, *, #12557, .T. ) ;
#104534 = CARTESIAN_POINT ( 'NONE',  ( 18.59999999999999787, -11.65000000000000036, 29.89999999999999858 ) ) ;
#104535 = AXIS2_PLACEMENT_3D ( 'NONE', #1821, #103484, #138739 ) ;
#104536 = DIRECTION ( 'NONE',  ( 0.000000000000000000, 0.000000000000000000, 1.000000000000000000 ) ) ;
#104537 = DIRECTION ( 'NONE',  ( 1.000000000000000000, 0.000000000000000000, 0.000000000000000000 ) ) ;
#104538 = CARTESIAN_POINT ( 'NONE',  ( -6.000000000000003553, -11.65000000000000036, 10.10000000000000142 ) ) ;
#104539 = VECTOR ( 'NONE', #141047, 1000.000000000000000 ) ;
#104540 = VERTEX_POINT ( 'NONE', #112710 ) ;
#104541 = CARTESIAN_POINT ( 'NONE',  ( 20.94999999999999574, 14.00000000001115730, -72.42709253038259476 ) ) ;
#104542 = DIRECTION ( 'NONE',  ( 1.296989514748957922E-15, 0.9887567792719351711, -0.1495327102803594987 ) ) ;
#104543 = VERTEX_POINT ( 'NONE', #250914 ) ;
#104544 = EDGE_CURVE ( 'NONE', #4905, #123054, #43910, .T. ) ;
#104545 = CARTESIAN_POINT ( 'NONE',  ( -20.87600722750343252, 10.33112638555853913, -39.09012289269746532 ) ) ;
#104546 = EDGE_CURVE ( 'NONE', #217161, #192398, #93787, .T. ) ;
#104547 = CARTESIAN_POINT ( 'NONE',  ( -23.15000000000000213, 62.99095723518624368, -207.1734234082435080 ) ) ;
#104548 = ORIENTED_EDGE ( 'NONE', *, *, #139478, .T. ) ;
#104549 = MANIFOLD_SOLID_BREP ( 'Stock-MAS-200-1', #70045 ) ;
#104550 = CARTESIAN_POINT ( 'NONE',  ( 23.25000000000000000, 62.12148660976905745, -247.5636999539406133 ) ) ;
#104551 = AXIS2_PLACEMENT_3D ( 'NONE', #255609, #40510, #220400 ) ;
#104552 = ORIENTED_EDGE ( 'NONE', *, *, #235174, .F. ) ;
#104553 = LINE ( 'NONE', #82422, #113255 ) ;
#104554 = ORIENTED_EDGE ( 'NONE', *, *, #212162, .T. ) ;
#104555 = DIRECTION ( 'NONE',  ( -1.000000000000000000, 0.000000000000000000, -0.000000000000000000 ) ) ;
#104556 = AXIS2_PLACEMENT_3D ( 'NONE', #86181, #11840, #169650 ) ;
#104557 = EDGE_CURVE ( 'NONE', #40263, #224619, #73177, .T. ) ;
#104558 = CARTESIAN_POINT ( 'NONE',  ( 18.59999999999999787, 18.27574494880468592, -237.6039235467692947 ) ) ;
#104559 = DIRECTION ( 'NONE',  ( 0.000000000000000000, 0.2128009952263403282, -0.9770955615653358350 ) ) ;
#104560 = AXIS2_PLACEMENT_3D ( 'NONE', #251237, #70081, #173051 ) ;
#104561 = AXIS2_PLACEMENT_3D ( 'NONE', #39833, #140166, #158497 ) ;
#104562 = EDGE_CURVE ( 'NONE', #138911, #251327, #143850, .T. ) ;
#104563 = DIRECTION ( 'NONE',  ( 2.715809747126116508E-16, -1.000000000000000000, -2.172647797700893206E-15 ) ) ;
#104564 = ADVANCED_FACE ( 'NONE', ( #69743 ), #149287, .T. ) ;
#104565 = CARTESIAN_POINT ( 'NONE',  ( -18.59999999999999787, 64.35000000001259934, -191.3731074845244393 ) ) ;
#104566 = DIRECTION ( 'NONE',  ( 0.000000000000000000, 0.000000000000000000, 1.000000000000000000 ) ) ;
#104567 = VECTOR ( 'NONE', #216086, 1000.000000000000000 ) ;
#104569 = DIRECTION ( 'NONE',  ( 1.000000000000000000, 0.000000000000000000, -0.000000000000000000 ) ) ;
#104568 = CIRCLE ( 'NONE', #46320, 11.80000000000000426 ) ;
#104570 = AXIS2_PLACEMENT_3D ( 'NONE', #146183, #47072, #57961 ) ;
#104571 = EDGE_LOOP ( 'NONE', ( #67665, #216913, #251070, #24290 ) ) ;
#104573 = DIRECTION ( 'NONE',  ( 0.000000000000000000, 0.2617529984165014589, 0.9651348961777161950 ) ) ;
#104572 = DIRECTION ( 'NONE',  ( -0.000000000000000000, 0.4088369013363281623, -0.9126074666063771490 ) ) ;
#104574 = AXIS2_PLACEMENT_3D ( 'NONE', #89769, #92344, #207177 ) ;
#104575 = ORIENTED_EDGE ( 'NONE', *, *, #191410, .T. ) ;
#104576 = CARTESIAN_POINT ( 'NONE',  ( -16.85718274719434007, 12.42113698003434585, -211.1526569265139699 ) ) ;
#104577 = LINE ( 'NONE', #8091, #233157 ) ;
#104579 = ORIENTED_EDGE ( 'NONE', *, *, #188421, .F. ) ;
#104578 = CARTESIAN_POINT ( 'NONE',  ( -21.14999999999999858, -11.74999999998884448, -36.39999999999999858 ) ) ;
#104581 = EDGE_LOOP ( 'NONE', ( #34704, #172989, #34123 ) ) ;
#104580 = SPHERICAL_SURFACE ( 'NONE', #87164, 0.1000000000000000056 ) ;
#104582 = ADVANCED_FACE ( 'NONE', ( #111424 ), #171436, .F. ) ;
#104583 = CARTESIAN_POINT ( 'NONE',  ( 18.60000000000000142, 47.07326788871598922, -255.0992659944397190 ) ) ;
#104584 = DIRECTION ( 'NONE',  ( 0.000000000000000000, -1.000000000000000000, 1.387778780781442047E-14 ) ) ;
#104585 = FACE_OUTER_BOUND ( 'NONE', #87847, .T. ) ;
#104586 = CARTESIAN_POINT ( 'NONE',  ( -18.59999999999999787, 1.835341550224411922, -11.65515129256298010 ) ) ;
#104588 = ORIENTED_EDGE ( 'NONE', *, *, #245717, .T. ) ;
#104587 = LINE ( 'NONE', #184146, #81991 ) ;
#104589 = CARTESIAN_POINT ( 'NONE',  ( -18.40000000000000213, 64.52683809664959824, -123.9145288407616903 ) ) ;
#104590 = ORIENTED_EDGE ( 'NONE', *, *, #45917, .F. ) ;
#104591 = VERTEX_POINT ( 'NONE', #213081 ) ;
#104592 = CARTESIAN_POINT ( 'NONE',  ( 23.14999999999999503, 11.65000000000000746, -21.35000000000000142 ) ) ;
#104593 = FACE_OUTER_BOUND ( 'NONE', #58877, .T. ) ;
#104594 = ORIENTED_EDGE ( 'NONE', *, *, #158632, .F. ) ;
#104595 = CARTESIAN_POINT ( 'NONE',  ( 13.40000000000005898, 67.65000000001120384, -16.98168612828748891 ) ) ;
#104596 = CIRCLE ( 'NONE', #92154, 0.09999999999999609201 ) ;
#104597 = ADVANCED_FACE ( 'NONE', ( #154439 ), #218860, .T. ) ;
#104598 = CARTESIAN_POINT ( 'NONE',  ( -16.87368910959167678, 9.961273816702552963, -180.1124930966405771 ) ) ;
#104599 = VERTEX_POINT ( 'NONE', #233934 ) ;
#104600 = DIRECTION ( 'NONE',  ( -0.000000000000000000, -2.891205793294679805E-16, 1.000000000000000000 ) ) ;
#104601 = FACE_OUTER_BOUND ( 'NONE', #46089, .T. ) ;
#104602 = EDGE_CURVE ( 'NONE', #55100, #248447, #14724, .T. ) ;
#104604 = ORIENTED_EDGE ( 'NONE', *, *, #190695, .T. ) ;
#104603 = AXIS2_PLACEMENT_3D ( 'NONE', #63078, #39703, #237873 ) ;
#104605 = ORIENTED_EDGE ( 'NONE', *, *, #13951, .F. ) ;
#104606 = FACE_OUTER_BOUND ( 'NONE', #149910, .T. ) ;
#104607 = ORIENTED_EDGE ( 'NONE', *, *, #248993, .T. ) ;
#104608 = LINE ( 'NONE', #47220, #229591 ) ;
#104609 = VERTEX_POINT ( 'NONE', #196099 ) ;
#104611 = ORIENTED_EDGE ( 'NONE', *, *, #181101, .F. ) ;
#104610 = CARTESIAN_POINT ( 'NONE',  ( 18.59999999999999076, 62.96704557978079464, -212.5773704035085814 ) ) ;
#104612 = ADVANCED_FACE ( 'NONE', ( #199961 ), #137387, .F. ) ;
#104613 = DIRECTION ( 'NONE',  ( -1.000000000000000000, 0.000000000000000000, 0.000000000000000000 ) ) ;
#104614 = ORIENTED_EDGE ( 'NONE', *, *, #112946, .F. ) ;
#104615 = FACE_OUTER_BOUND ( 'NONE', #98399, .T. ) ;
#104616 = ORIENTED_EDGE ( 'NONE', *, *, #107528, .T. ) ;
#104618 = VERTEX_POINT ( 'NONE', #116559 ) ;
#104617 = EDGE_LOOP ( 'NONE', ( #193495, #156094, #35851 ) ) ;
#104619 = DIRECTION ( 'NONE',  ( 0.000000000000000000, 0.000000000000000000, -1.000000000000000000 ) ) ;
#104620 = EDGE_CURVE ( 'NONE', #20936, #26458, #193761, .T. ) ;
#104621 = CARTESIAN_POINT ( 'NONE',  ( -23.15000000000000213, -3.363022478626109368, -226.2703567425896267 ) ) ;
#104622 = VECTOR ( 'NONE', #60829, 1000.000000000000000 ) ;
#104623 = ORIENTED_EDGE ( 'NONE', *, *, #164017, .F. ) ;
#104624 = CIRCLE ( 'NONE', #212826, 0.09999999999999939493 ) ;
#104625 = CIRCLE ( 'NONE', #208896, 0.1999999999999987899 ) ;
#104626 = VERTEX_POINT ( 'NONE', #216923 ) ;
#104627 = DIRECTION ( 'NONE',  ( -1.000000000000000000, 0.000000000000000000, 0.000000000000000000 ) ) ;
#104628 = EDGE_CURVE ( 'NONE', #188126, #200601, #441, .T. ) ;
#104630 = ORIENTED_EDGE ( 'NONE', *, *, #222865, .T. ) ;
#104629 = DIRECTION ( 'NONE',  ( 0.000000000000000000, -0.7397360091702744889, 0.6728971962616842051 ) ) ;
#104631 = DIRECTION ( 'NONE',  ( 0.000000000000000000, -0.8814952561688430555, 0.4721928772777346239 ) ) ;
#104632 = ORIENTED_EDGE ( 'NONE', *, *, #7332, .F. ) ;
#104633 = CARTESIAN_POINT ( 'NONE',  ( -23.15000000000000213, 7.128833340093095217, -233.7327013124392749 ) ) ;
#104634 = DIRECTION ( 'NONE',  ( 0.000000000000000000, 0.000000000000000000, -1.000000000000000000 ) ) ;
#104636 = ORIENTED_EDGE ( 'NONE', *, *, #19690, .T. ) ;
#104635 = EDGE_CURVE ( 'NONE', #179506, #254110, #148143, .T. ) ;
#104637 = EDGE_CURVE ( 'NONE', #82079, #113827, #256009, .T. ) ;
#104638 = FACE_OUTER_BOUND ( 'NONE', #198300, .T. ) ;
#104639 = DIRECTION ( 'NONE',  ( 1.000000000000000000, 1.646408749285562691E-14, 1.073024830501117725E-15 ) ) ;
#104640 = TOROIDAL_SURFACE ( 'NONE', #171371, 1.900000000000002576, 0.1000000000000000056 ) ;
#104641 = ORIENTED_EDGE ( 'NONE', *, *, #59246, .F. ) ;
#104642 = CARTESIAN_POINT ( 'NONE',  ( -37.88850191057539973, -10.64999999999999325, 31.59999999999999787 ) ) ;
#104643 = ORIENTED_EDGE ( 'NONE', *, *, #106361, .T. ) ;
#104644 = EDGE_CURVE ( 'NONE', #132574, #236269, #167905, .T. ) ;
#104646 = ORIENTED_EDGE ( 'NONE', *, *, #52792, .F. ) ;
#104645 = ORIENTED_EDGE ( 'NONE', *, *, #244651, .T. ) ;
#104647 = EDGE_LOOP ( 'NONE', ( #15858, #167920, #229473, #228562 ) ) ;
#104648 = CARTESIAN_POINT ( 'NONE',  ( -21.05000000000000071, 0.03363273534480443888, -127.7411828053185161 ) ) ;
#104649 = ORIENTED_EDGE ( 'NONE', *, *, #190017, .T. ) ;
#104650 = LINE ( 'NONE', #202507, #63403 ) ;
#104651 = EDGE_LOOP ( 'NONE', ( #235215, #90407, #75718, #195021, #169352 ) ) ;
#104652 = EDGE_CURVE ( 'NONE', #143115, #101180, #99527, .T. ) ;
#104653 = DIRECTION ( 'NONE',  ( 1.000000000000000000, 0.000000000000000000, 0.000000000000000000 ) ) ;
#104654 = EDGE_CURVE ( 'NONE', #223762, #171936, #236494, .T. ) ;
#104655 = DIRECTION ( 'NONE',  ( 1.000000000000000000, 0.000000000000000000, 0.000000000000000000 ) ) ;
#104656 = EDGE_LOOP ( 'NONE', ( #86529, #133210, #56232, #122905, #27937 ) ) ;
#104657 = CIRCLE ( 'NONE', #87915, 11.74999999999999645 ) ;
#104658 = CIRCLE ( 'NONE', #75501, 12.97499999999999787 ) ;
#104659 = ORIENTED_EDGE ( 'NONE', *, *, #14512, .F. ) ;
#104660 = ORIENTED_EDGE ( 'NONE', *, *, #156696, .F. ) ;
#104661 = CARTESIAN_POINT ( 'NONE',  ( -20.85000000000000142, -11.64999999999999858, -33.50000000000000000 ) ) ;
#104662 = EDGE_CURVE ( 'NONE', #34419, #232297, #181488, .T. ) ;
#104663 = VERTEX_POINT ( 'NONE', #96952 ) ;
#104664 = EDGE_CURVE ( 'NONE', #33536, #170111, #93976, .T. ) ;
#104665 = CARTESIAN_POINT ( 'NONE',  ( 18.59999999999999787, 67.23127455305841238, -235.8551265064783991 ) ) ;
#104667 = ORIENTED_EDGE ( 'NONE', *, *, #251366, .T. ) ;
#104666 = CARTESIAN_POINT ( 'NONE',  ( -18.38817693311004575, 33.92657181652015908, -235.0624982814158841 ) ) ;
#104668 = DIRECTION ( 'NONE',  ( 1.000000000000000000, 0.000000000000000000, 0.000000000000000000 ) ) ;
#104669 = CARTESIAN_POINT ( 'NONE',  ( -20.94999999999999574, 11.75000000001114842, -127.2161343370219555 ) ) ;
#104670 = DIRECTION ( 'NONE',  ( 1.000000000000000000, 0.000000000000000000, 0.000000000000000000 ) ) ;
#104671 = CIRCLE ( 'NONE', #192213, 0.1000000000000028644 ) ;
#104672 = DIRECTION ( 'NONE',  ( -1.000000000000000000, -0.000000000000000000, -0.000000000000000000 ) ) ;
#104673 = CARTESIAN_POINT ( 'NONE',  ( -20.54999999999999716, 4.625797360122408719, -213.1224017332881431 ) ) ;
#104675 = DIRECTION ( 'NONE',  ( 0.000000000000000000, 1.000000000000000000, 7.272083257015735086E-15 ) ) ;
#104674 = CARTESIAN_POINT ( 'NONE',  ( 23.14999999999999147, -4.149999999988843058, -134.0000000000000000 ) ) ;
#104676 = DIRECTION ( 'NONE',  ( 0.000000000000000000, -0.1350103645451876944, -0.9908441862701601321 ) ) ;
#104677 = DIRECTION ( 'NONE',  ( -0.000000000000000000, 1.000000000000000000, 0.000000000000000000 ) ) ;
#104678 = EDGE_CURVE ( 'NONE', #39469, #84969, #117832, .T. ) ;
#104679 = CARTESIAN_POINT ( 'NONE',  ( 22.50000000000000000, 7.750000000011162626, -66.90000000000004832 ) ) ;
#104680 = CARTESIAN_POINT ( 'NONE',  ( 23.15000000000000213, 24.26958830762006514, -252.6664436919618879 ) ) ;
#104681 = VERTEX_POINT ( 'NONE', #57843 ) ;
#104683 = ORIENTED_EDGE ( 'NONE', *, *, #143894, .F. ) ;
#104682 = CARTESIAN_POINT ( 'NONE',  ( 20.94999999999999574, 62.00000000001264056, -198.0960149541419071 ) ) ;
#104684 = ORIENTED_EDGE ( 'NONE', *, *, #30635, .F. ) ;
#104685 = CYLINDRICAL_SURFACE ( 'NONE', #174330, 0.09999999999999939493 ) ;
#104686 = DIRECTION ( 'NONE',  ( 1.000000000000000000, 1.646408749285562691E-14, 1.073024830501117725E-15 ) ) ;
#104687 = CARTESIAN_POINT ( 'NONE',  ( -20.64999999999999858, 76.00000000001244871, -170.0231074845243597 ) ) ;
#104688 = ORIENTED_EDGE ( 'NONE', *, *, #35863, .F. ) ;
#104689 = CIRCLE ( 'NONE', #150533, 0.09999999999999938105 ) ;
#104690 = ADVANCED_FACE ( 'NONE', ( #79962 ), #134810, .T. ) ;
#104691 = CARTESIAN_POINT ( 'NONE',  ( 20.95512820512820440, 10.62384868372303615, -179.6499999999999773 ) ) ;
#104692 = AXIS2_PLACEMENT_3D ( 'NONE', #219751, #254969, #234176 ) ;
#104693 = ADVANCED_FACE ( 'NONE', ( #60421 ), #219494, .F. ) ;
#104694 = CARTESIAN_POINT ( 'NONE',  ( -18.59999999999999787, 1.736257131608553550, -145.5686523290175387 ) ) ;
#104695 = ORIENTED_EDGE ( 'NONE', *, *, #179841, .T. ) ;
#104696 = DIRECTION ( 'NONE',  ( 0.000000000000000000, 0.000000000000000000, -1.000000000000000000 ) ) ;
#104697 = CARTESIAN_POINT ( 'NONE',  ( 21.33487959338958717, 69.27444184810046579, -69.52310748452435973 ) ) ;
#104698 = CIRCLE ( 'NONE', #167311, 0.09999999999999939493 ) ;
#104699 = CARTESIAN_POINT ( 'NONE',  ( 20.94999999999999929, 65.52661458509871295, -61.94445302027585143 ) ) ;
#104700 = CIRCLE ( 'NONE', #8895, 0.1000000000000000472 ) ;
#104701 = EDGE_CURVE ( 'NONE', #416, #34831, #139752, .T. ) ;
#104702 = CARTESIAN_POINT ( 'NONE',  ( 21.05000000000085336, 40.76780962062015590, -237.9639380751402200 ) ) ;
#104704 = ORIENTED_EDGE ( 'NONE', *, *, #246349, .F. ) ;
#104703 = DIRECTION ( 'NONE',  ( -0.000000000000000000, -0.8103668758649578141, 0.5859227990963212784 ) ) ;
#104705 = CARTESIAN_POINT ( 'NONE',  ( 23.40000000000005542, 83.98667523412385094, -34.76145429838185663 ) ) ;
#104706 = SPHERICAL_SURFACE ( 'NONE', #119097, 0.1000000000000000056 ) ;
#104708 = ADVANCED_FACE ( 'NONE', ( #254735 ), #76138, .T. ) ;
#104707 = DIRECTION ( 'NONE',  ( 1.000000000000000000, 0.000000000000000000, 0.000000000000000000 ) ) ;
#104710 = CIRCLE ( 'NONE', #238015, 0.1000000000000028644 ) ;
#104709 = CARTESIAN_POINT ( 'NONE',  ( -22.39999999999999858, 11.65000000001115588, -134.1000000000000227 ) ) ;
#104711 = ORIENTED_EDGE ( 'NONE', *, *, #213651, .F. ) ;
#104712 = FACE_OUTER_BOUND ( 'NONE', #11930, .T. ) ;
#104713 = DIRECTION ( 'NONE',  ( 0.000000000000000000, -1.000000000000000000, -6.860497997771532351E-15 ) ) ;
#104715 = CARTESIAN_POINT ( 'NONE',  ( -23.25000000000000000, 76.00000000001141132, -33.92310748452431568 ) ) ;
#104714 = CARTESIAN_POINT ( 'NONE',  ( -18.59999999999999787, 18.92285928089247804, -233.3572654221044900 ) ) ;
#104717 = EDGE_CURVE ( 'NONE', #74878, #145938, #90273, .T. ) ;
#104716 = DIRECTION ( 'NONE',  ( 0.000000000000000000, 0.000000000000000000, -1.000000000000000000 ) ) ;
#104718 = CARTESIAN_POINT ( 'NONE',  ( 23.24999999999999289, 64.25000000001172396, -81.27310748452440237 ) ) ;
#104720 = CARTESIAN_POINT ( 'NONE',  ( -18.50000000000000000, 10.29270135740182823, -38.95736188715194714 ) ) ;
#104719 = CIRCLE ( 'NONE', #242121, 4.000000000000003553 ) ;
#104721 = CYLINDRICAL_SURFACE ( 'NONE', #27130, 0.09999999999999990841 ) ;
#104722 = CARTESIAN_POINT ( 'NONE',  ( -23.15000000000000213, 65.40605961984560679, -236.6728003091511425 ) ) ;
#104723 = AXIS2_PLACEMENT_3D ( 'NONE', #208547, #11632, #9042 ) ;
#104724 = VERTEX_POINT ( 'NONE', #184223 ) ;
#104725 = EDGE_CURVE ( 'NONE', #127092, #123340, #145088, .T. ) ;
#104726 = CARTESIAN_POINT ( 'NONE',  ( -20.54999999999999716, 0.000000000000000000, -33.50000000000000000 ) ) ;
#104728 = ADVANCED_FACE ( 'NONE', ( #22613 ), #27760, .F. ) ;
#104727 = EDGE_CURVE ( 'NONE', #206992, #45948, #256412, .T. ) ;
#104729 = ORIENTED_EDGE ( 'NONE', *, *, #130697, .T. ) ;
#104730 = ORIENTED_EDGE ( 'NONE', *, *, #58228, .T. ) ;
#104731 = CARTESIAN_POINT ( 'NONE',  ( -21.05000000000000071, 11.74999999999999645, -26.48519422934605672 ) ) ;
#104732 = DIRECTION ( 'NONE',  ( 1.000000000000000000, 0.000000000000000000, 0.000000000000000000 ) ) ;
#104733 = EDGE_LOOP ( 'NONE', ( #100563, #10906, #132459, #58967 ) ) ;
#104734 = AXIS2_PLACEMENT_3D ( 'NONE', #116482, #99453, #180303 ) ;
#104735 = VERTEX_POINT ( 'NONE', #105953 ) ;
#104737 = ORIENTED_EDGE ( 'NONE', *, *, #256472, .F. ) ;
#104736 = CIRCLE ( 'NONE', #17321, 12.77500000000000213 ) ;
#104738 = ADVANCED_FACE ( 'NONE', ( #244186 ), #225890, .F. ) ;
#104739 = DIRECTION ( 'NONE',  ( -2.342056488767301376E-15, -0.1350103645451904977, 0.9908441862701596881 ) ) ;
#104740 = EDGE_CURVE ( 'NONE', #17324, #14256, #214783, .T. ) ;
#104741 = AXIS2_PLACEMENT_3D ( 'NONE', #101585, #224126, #45500 ) ;
#104742 = ORIENTED_EDGE ( 'NONE', *, *, #138212, .F. ) ;
#104743 = CIRCLE ( 'NONE', #250527, 0.5000000000000004441 ) ;
#104744 = DIRECTION ( 'NONE',  ( 0.000000000000000000, -6.982962677686266711E-15, 1.000000000000000000 ) ) ;
#104745 = DIRECTION ( 'NONE',  ( -1.000000000000000000, 2.952720810173289112E-16, 2.061873921506763405E-30 ) ) ;
#104747 = DIRECTION ( 'NONE',  ( 1.000000000000000000, 0.000000000000000000, 0.000000000000000000 ) ) ;
#104746 = AXIS2_PLACEMENT_3D ( 'NONE', #189120, #10491, #90005 ) ;
#104748 = DIRECTION ( 'NONE',  ( 0.000000000000000000, 0.9274965247785529332, -0.3738317757009255171 ) ) ;
#104749 = CARTESIAN_POINT ( 'NONE',  ( -21.11101077989000530, 1.473603314416399579, -230.6860092427866959 ) ) ;
#104750 = EDGE_CURVE ( 'NONE', #62040, #218484, #102319, .T. ) ;
#104751 = DIRECTION ( 'NONE',  ( 0.000000000000000000, 2.168404344971021884E-15, -1.000000000000000000 ) ) ;
#104752 = DIRECTION ( 'NONE',  ( 1.000000000000000000, -3.965082230804126670E-15, 0.000000000000000000 ) ) ;
#104754 = VERTEX_POINT ( 'NONE', #66854 ) ;
#104753 = DIRECTION ( 'NONE',  ( 0.000000000000000000, -6.982962677686266711E-15, 1.000000000000000000 ) ) ;
#104756 = CARTESIAN_POINT ( 'NONE',  ( 20.04142135623730070, 11.65000000000000391, -21.35000000000000142 ) ) ;
#104755 = DIRECTION ( 'NONE',  ( -0.000000000000000000, 0.9126074666063771490, 0.4088369013363281623 ) ) ;
#104757 = FACE_OUTER_BOUND ( 'NONE', #217577, .T. ) ;
#104758 = ADVANCED_FACE ( 'NONE', ( #61720 ), #202316, .T. ) ;
#104759 = EDGE_LOOP ( 'NONE', ( #212975, #36939, #210224, #242453 ) ) ;
#104760 = CARTESIAN_POINT ( 'NONE',  ( 21.00000000000000000, 0.000000000000000000, 0.000000000000000000 ) ) ;
#104761 = DIRECTION ( 'NONE',  ( -1.000000000000000000, 0.000000000000000000, -0.000000000000000000 ) ) ;
#104762 = FACE_OUTER_BOUND ( 'NONE', #169447, .T. ) ;
#104763 = ORIENTED_EDGE ( 'NONE', *, *, #17851, .F. ) ;
#104764 = EDGE_CURVE ( 'NONE', #214553, #94097, #19153, .T. ) ;
#104766 = CARTESIAN_POINT ( 'NONE',  ( 21.07016717457011623, 76.00000000001170974, -75.84404832262522689 ) ) ;
#104765 = DIRECTION ( 'NONE',  ( 1.000000000000000000, 0.000000000000000000, 0.000000000000000000 ) ) ;
#104767 = CYLINDRICAL_SURFACE ( 'NONE', #202287, 0.09999999999999939493 ) ;
#104768 = CIRCLE ( 'NONE', #75779, 0.09999999999999939493 ) ;
#104769 = ORIENTED_EDGE ( 'NONE', *, *, #124554, .F. ) ;
#104770 = CARTESIAN_POINT ( 'NONE',  ( 21.05000000000000071, 6.257814610487288043, -66.90220970869125949 ) ) ;
#104771 = DIRECTION ( 'NONE',  ( -1.000000000000000000, 2.952720810173289112E-16, 2.061873921506763405E-30 ) ) ;
#104772 = CARTESIAN_POINT ( 'NONE',  ( 21.05000000000000071, 1.115600667400684642E-11, -200.9999999999999432 ) ) ;
#104773 = FACE_OUTER_BOUND ( 'NONE', #141906, .T. ) ;
#104774 = ADVANCED_FACE ( 'NONE', ( #102095 ), #164905, .T. ) ;
#104775 = EDGE_LOOP ( 'NONE', ( #176952, #122705, #197281, #23643 ) ) ;
#104776 = ORIENTED_EDGE ( 'NONE', *, *, #27113, .F. ) ;
#104777 = AXIS2_PLACEMENT_3D ( 'NONE', #253776, #103679, #240650 ) ;
#104779 = ADVANCED_FACE ( 'NONE', ( #65562 ), #198218, .T. ) ;
#104778 = CARTESIAN_POINT ( 'NONE',  ( 21.06086055315979522, 67.22529248505564681, -90.82078532937038062 ) ) ;
#104780 = CARTESIAN_POINT ( 'NONE',  ( 21.05000000000000426, 10.56275983745102032, -7.456813957918630109 ) ) ;
#104781 = DIRECTION ( 'NONE',  ( 0.000000000000000000, -7.056502275159890832E-15, 1.000000000000000000 ) ) ;
#104782 = DIRECTION ( 'NONE',  ( -1.000000000000000000, -0.000000000000000000, -0.000000000000000000 ) ) ;
#104783 = CARTESIAN_POINT ( 'NONE',  ( -16.27683809663751191, 66.65000000001161595, -60.27310748452442368 ) ) ;
#104784 = ORIENTED_EDGE ( 'NONE', *, *, #244473, .F. ) ;
#104785 = CARTESIAN_POINT ( 'NONE',  ( -20.15000000000000568, 9.291421356248463326, -188.7499999999999716 ) ) ;
#104786 = AXIS2_PLACEMENT_3D ( 'NONE', #164762, #126920, #186916 ) ;
#104788 = VERTEX_POINT ( 'NONE', #223341 ) ;
#104787 = DIRECTION ( 'NONE',  ( 0.000000000000000000, -1.156482317317873105E-15, 1.000000000000000000 ) ) ;
#104789 = CARTESIAN_POINT ( 'NONE',  ( -21.05000000000000071, 6.300179817925682713, -33.44851711811818262 ) ) ;
#104790 = DIRECTION ( 'NONE',  ( -1.000000000000000000, -0.000000000000000000, -0.000000000000000000 ) ) ;
#104791 = DIRECTION ( 'NONE',  ( 0.000000000000000000, 0.000000000000000000, 1.000000000000000000 ) ) ;
#104792 = DIRECTION ( 'NONE',  ( 0.000000000000000000, 0.7071067811865472397, -0.7071067811865479058 ) ) ;
#104793 = EDGE_CURVE ( 'NONE', #205599, #78573, #60644, .T. ) ;
#104794 = FACE_OUTER_BOUND ( 'NONE', #54879, .T. ) ;
#104796 = ORIENTED_EDGE ( 'NONE', *, *, #219243, .T. ) ;
#104795 = CARTESIAN_POINT ( 'NONE',  ( 20.94999999999999929, 87.29603075034764004, -166.9752083248604038 ) ) ;
#104797 = FACE_OUTER_BOUND ( 'NONE', #177, .T. ) ;
#104798 = DIRECTION ( 'NONE',  ( 0.000000000000000000, 6.982962677686266711E-15, -1.000000000000000000 ) ) ;
#104799 = CARTESIAN_POINT ( 'NONE',  ( 18.59999999999999787, -1.835341550213255957, -179.0551512925629538 ) ) ;
#104800 = FACE_OUTER_BOUND ( 'NONE', #105112, .T. ) ;
#104801 = ORIENTED_EDGE ( 'NONE', *, *, #61711, .F. ) ;
#104802 = DIRECTION ( 'NONE',  ( 1.000000000000000000, 0.000000000000000000, 0.000000000000000000 ) ) ;
#104803 = CARTESIAN_POINT ( 'NONE',  ( 21.14999999999999858, 76.00000000001205080, -124.3731074845242972 ) ) ;
#104804 = DIRECTION ( 'NONE',  ( 1.000000000000000000, 0.000000000000000000, 0.000000000000000000 ) ) ;
#104806 = AXIS2_PLACEMENT_3D ( 'NONE', #127899, #187880, #228288 ) ;
#104805 = CARTESIAN_POINT ( 'NONE',  ( -23.15000000000000213, 1.115600667400684642E-11, -200.9999999999999432 ) ) ;
#104807 = ORIENTED_EDGE ( 'NONE', *, *, #251411, .T. ) ;
#104808 = EDGE_CURVE ( 'NONE', #118480, #100463, #223150, .T. ) ;
#104810 = VECTOR ( 'NONE', #232715, 1000.000000000000000 ) ;
#104809 = CARTESIAN_POINT ( 'NONE',  ( -20.64999999999999858, 65.86663596189677605, -213.5709895136416776 ) ) ;
#104811 = ORIENTED_EDGE ( 'NONE', *, *, #189146, .F. ) ;
#104812 = CIRCLE ( 'NONE', #138146, 0.1000000000000028644 ) ;
#104813 = CARTESIAN_POINT ( 'NONE',  ( -2.995603634470829482E-16, 52.64219947837469959, -255.2660483925003803 ) ) ;
#104814 = DIRECTION ( 'NONE',  ( 0.000000000000000000, -0.8368562265788574983, -0.5474227397872651890 ) ) ;
#104815 = FACE_OUTER_BOUND ( 'NONE', #238072, .T. ) ;
#104816 = DIRECTION ( 'NONE',  ( 1.000000000000000000, 0.000000000000000000, 0.000000000000000000 ) ) ;
#104817 = ORIENTED_EDGE ( 'NONE', *, *, #153999, .F. ) ;
#104818 = FACE_OUTER_BOUND ( 'NONE', #14658, .T. ) ;
#104819 = VECTOR ( 'NONE', #19221, 1000.000000000000000 ) ;
#104820 = CARTESIAN_POINT ( 'NONE',  ( 21.14999999999999858, 6.550000000011156231, -45.85000000000000142 ) ) ;
#104821 = DIRECTION ( 'NONE',  ( -0.000000000000000000, -0.8660254037844420383, 0.4999999999999943379 ) ) ;
#104822 = CARTESIAN_POINT ( 'NONE',  ( 21.14999999999999858, 23.34004772283015328, -229.2004250369967338 ) ) ;
#104823 = CARTESIAN_POINT ( 'NONE',  ( 18.51024323315077069, 10.31104185824063713, -206.5204516983105520 ) ) ;
#104824 = ORIENTED_EDGE ( 'NONE', *, *, #88207, .F. ) ;
#104826 = VERTEX_POINT ( 'NONE', #64288 ) ;
#104825 = FACE_OUTER_BOUND ( 'NONE', #130930, .T. ) ;
#104827 = ORIENTED_EDGE ( 'NONE', *, *, #158598, .F. ) ;
#104828 = CARTESIAN_POINT ( 'NONE',  ( 18.59999999999999787, 7.128833340093095217, -233.7327013124392749 ) ) ;
#104829 = ORIENTED_EDGE ( 'NONE', *, *, #109358, .F. ) ;
#104830 = CARTESIAN_POINT ( 'NONE',  ( -23.25000000000000000, 1.115600667400684642E-11, -167.4999999999999716 ) ) ;
#104831 = CARTESIAN_POINT ( 'NONE',  ( 20.85000000000000142, 1.115600667400684642E-11, -134.0000000000000284 ) ) ;
#104832 = FACE_OUTER_BOUND ( 'NONE', #111222, .T. ) ;
#104833 = VERTEX_POINT ( 'NONE', #162123 ) ;
#104834 = CYLINDRICAL_SURFACE ( 'NONE', #211368, 4.000000000000003553 ) ;
#104835 = FACE_OUTER_BOUND ( 'NONE', #27207, .T. ) ;
#104836 = DIRECTION ( 'NONE',  ( 2.952720810173288619E-16, 0.4088369013363282178, -0.9126074666063768159 ) ) ;
#104837 = ORIENTED_EDGE ( 'NONE', *, *, #221272, .F. ) ;
#104838 = CARTESIAN_POINT ( 'NONE',  ( -16.86420534634261514, 9.970615445602874161, -54.41833654923738095 ) ) ;
#104840 = EDGE_LOOP ( 'NONE', ( #120643, #26596, #46637, #66026 ) ) ;
#104839 = DIRECTION ( 'NONE',  ( 0.000000000000000000, 0.5986962832864934914, 0.8009761297185696849 ) ) ;
#104841 = AXIS2_PLACEMENT_3D ( 'NONE', #45899, #162018, #125445 ) ;
#104843 = EDGE_CURVE ( 'NONE', #246816, #132867, #139938, .T. ) ;
#104842 = CIRCLE ( 'NONE', #179721, 0.5000000000000004441 ) ;
#104844 = DIRECTION ( 'NONE',  ( 1.000000000000000000, 0.000000000000000000, 0.000000000000000000 ) ) ;
#104845 = CARTESIAN_POINT ( 'NONE',  ( 20.94999999999999929, 77.83534155023599510, -57.96795619196132776 ) ) ;
#104846 = CIRCLE ( 'NONE', #200745, 0.09999999999999854838 ) ;
#104847 = ORIENTED_EDGE ( 'NONE', *, *, #118778, .F. ) ;
#104848 = LINE ( 'NONE', #123177, #135126 ) ;
#104849 = DIRECTION ( 'NONE',  ( 1.000000000000000000, 0.000000000000000000, 0.000000000000000000 ) ) ;
#104850 = DIRECTION ( 'NONE',  ( 1.000000000000000000, 0.000000000000000000, -0.000000000000000000 ) ) ;
#104851 = VERTEX_POINT ( 'NONE', #4294 ) ;
#104852 = ADVANCED_FACE ( 'NONE', ( #143809 ), #188087, .T. ) ;
#104853 = CARTESIAN_POINT ( 'NONE',  ( -23.15000000000000213, 5.900000000011162093, -90.28090023534366537 ) ) ;
#104854 = AXIS2_PLACEMENT_3D ( 'NONE', #193698, #94577, #15064 ) ;
#104855 = EDGE_CURVE ( 'NONE', #46601, #194632, #72002, .T. ) ;
#104856 = EDGE_LOOP ( 'NONE', ( #196196, #217841, #226557, #56253 ) ) ;
#104857 = ADVANCED_FACE ( 'NONE', ( #51108 ), #91554, .F. ) ;
#104858 = VERTEX_POINT ( 'NONE', #92821 ) ;
#104859 = CARTESIAN_POINT ( 'NONE',  ( -21.05000000000000071, 1.115600667400684642E-11, -134.0000000000000000 ) ) ;
#104860 = EDGE_CURVE ( 'NONE', #241306, #34161, #106606, .T. ) ;
#104861 = VERTEX_POINT ( 'NONE', #248055 ) ;
#104862 = EDGE_CURVE ( 'NONE', #5558, #223147, #206408, .T. ) ;
#104863 = CYLINDRICAL_SURFACE ( 'NONE', #97552, 0.09999999999999939493 ) ;
#104864 = CARTESIAN_POINT ( 'NONE',  ( 23.15000000000000213, -9.499999999988844479, -191.1060308773475072 ) ) ;
#104865 = TOROIDAL_SURFACE ( 'NONE', #155016, 2.100000000000002309, 0.1000000000000000056 ) ;
#104867 = ORIENTED_EDGE ( 'NONE', *, *, #114509, .T. ) ;
#104866 = CARTESIAN_POINT ( 'NONE',  ( 19.99999999999998934, 11.75000000001115907, -125.3500000000000512 ) ) ;
#104868 = DIRECTION ( 'NONE',  ( -2.940209281316621016E-16, 1.000000000000000000, -4.704334850106593625E-15 ) ) ;
#104869 = LINE ( 'NONE', #164893, #136484 ) ;
#104870 = ADVANCED_FACE ( 'NONE', ( #151556 ), #29054, .F. ) ;
#104871 = DIRECTION ( 'NONE',  ( 0.000000000000000000, 0.000000000000000000, 1.000000000000000000 ) ) ;
#104872 = DIRECTION ( 'NONE',  ( 1.000000000000000000, 0.000000000000000000, 0.000000000000000000 ) ) ;
#104873 = FACE_OUTER_BOUND ( 'NONE', #185813, .T. ) ;
#104874 = CARTESIAN_POINT ( 'NONE',  ( 22.57320508075687115, 31.85509083104287598, -238.8280249686205536 ) ) ;
#104875 = AXIS2_PLACEMENT_3D ( 'NONE', #238520, #63734, #239824 ) ;
#104876 = DIRECTION ( 'NONE',  ( -4.408576920032447355E-17, 0.3427706569149636118, -0.9394191166662962944 ) ) ;
#104877 = CARTESIAN_POINT ( 'NONE',  ( -18.59999999999999787, 102.4393534156124730, -51.38159887701667827 ) ) ;
#104879 = ORIENTED_EDGE ( 'NONE', *, *, #167891, .F. ) ;
#104878 = FACE_OUTER_BOUND ( 'NONE', #247366, .T. ) ;
#104881 = EDGE_CURVE ( 'NONE', #254577, #49571, #239734, .T. ) ;
#104880 = TOROIDAL_SURFACE ( 'NONE', #109579, 4.099999999999999645, 0.1000000000000000056 ) ;
#104882 = ORIENTED_EDGE ( 'NONE', *, *, #225858, .T. ) ;
#104883 = AXIS2_PLACEMENT_3D ( 'NONE', #43256, #203608, #224446 ) ;
#104884 = AXIS2_PLACEMENT_3D ( 'NONE', #134502, #17167, #137093 ) ;
#104885 = CARTESIAN_POINT ( 'NONE',  ( 20.97224591636398472, 65.37484658384822467, -90.77318157986078972 ) ) ;
#104886 = VECTOR ( 'NONE', #27253, 1000.000000000000000 ) ;
#104887 = CYLINDRICAL_SURFACE ( 'NONE', #217531, 0.1000000000000021844 ) ;
#104888 = CIRCLE ( 'NONE', #250663, 0.1000000000000028644 ) ;
#104889 = DIRECTION ( 'NONE',  ( 2.952720810173289112E-16, 1.000000000000000000, 6.530723674265620862E-15 ) ) ;
#104890 = EDGE_CURVE ( 'NONE', #196680, #211746, #160656, .T. ) ;
#104891 = CARTESIAN_POINT ( 'NONE',  ( 20.11144452914042802, 66.06638914889266800, -195.6328140305747070 ) ) ;
#104892 = CARTESIAN_POINT ( 'NONE',  ( -21.14999999999994174, 87.60324567546805952, -37.87437456276921210 ) ) ;
#104893 = VECTOR ( 'NONE', #31039, 1000.000000000000000 ) ;
#104894 = ORIENTED_EDGE ( 'NONE', *, *, #247672, .T. ) ;
#104895 = EDGE_CURVE ( 'NONE', #75249, #242431, #31612, .T. ) ;
#104896 = CARTESIAN_POINT ( 'NONE',  ( -22.57320508075687115, 64.25000000001165290, -69.52310748452440237 ) ) ;
#104897 = CIRCLE ( 'NONE', #117422, 0.1000000000000028644 ) ;
#104898 = CARTESIAN_POINT ( 'NONE',  ( -20.94999999999999929, 44.52640028187936849, -247.3006740988509193 ) ) ;
#104899 = ORIENTED_EDGE ( 'NONE', *, *, #197515, .F. ) ;
#104900 = CIRCLE ( 'NONE', #167337, 0.2000000000000057288 ) ;
#104901 = CARTESIAN_POINT ( 'NONE',  ( 21.15000000000005542, 65.15000000001120384, -3.123107484524795474 ) ) ;
#104902 = AXIS2_PLACEMENT_3D ( 'NONE', #169321, #14071, #229265 ) ;
#104903 = DIRECTION ( 'NONE',  ( 0.000000000000000000, -0.8700118002898357128, 0.4930308989875171188 ) ) ;
#104904 = EDGE_CURVE ( 'NONE', #136029, #139968, #69440, .T. ) ;
#104905 = EDGE_LOOP ( 'NONE', ( #191381, #108598, #97597, #136438 ) ) ;
#104906 = CARTESIAN_POINT ( 'NONE',  ( -21.09107601085569428, 6.363877975371215356, -66.96069283528275662 ) ) ;
#104907 = ORIENTED_EDGE ( 'NONE', *, *, #96388, .T. ) ;
#104909 = AXIS2_PLACEMENT_3D ( 'NONE', #89534, #244756, #28331 ) ;
#104908 = CARTESIAN_POINT ( 'NONE',  ( -20.94999999999999929, -11.64999999998884306, -130.9000000000000341 ) ) ;
#104910 = ORIENTED_EDGE ( 'NONE', *, *, #14349, .F. ) ;
#104911 = DIRECTION ( 'NONE',  ( -1.000000000000000000, -0.000000000000000000, -0.000000000000000000 ) ) ;
#104912 = CARTESIAN_POINT ( 'NONE',  ( 18.49999999999999289, 6.450000000011156587, -155.1500000000000057 ) ) ;
#104913 = ORIENTED_EDGE ( 'NONE', *, *, #104326, .T. ) ;
#104914 = DIRECTION ( 'NONE',  ( 1.000000000000000000, 0.000000000000000000, 0.000000000000000000 ) ) ;
#104916 = ORIENTED_EDGE ( 'NONE', *, *, #34998, .F. ) ;
#104915 = DIRECTION ( 'NONE',  ( -1.000000000000000000, -0.000000000000000000, -0.000000000000000000 ) ) ;
#104917 = VECTOR ( 'NONE', #68349, 1000.000000000000000 ) ;
#104918 = DIRECTION ( 'NONE',  ( -1.000000000000000000, 0.000000000000000000, -0.000000000000000000 ) ) ;
#104920 = ORIENTED_EDGE ( 'NONE', *, *, #122782, .F. ) ;
#104919 = AXIS2_PLACEMENT_3D ( 'NONE', #80422, #219972, #204250 ) ;
#104921 = CIRCLE ( 'NONE', #125801, 0.1000000000000000472 ) ;
#104922 = EDGE_CURVE ( 'NONE', #223187, #235258, #81475, .T. ) ;
#104923 = CIRCLE ( 'NONE', #9296, 0.1000000000000010186 ) ;
#104924 = ORIENTED_EDGE ( 'NONE', *, *, #228069, .T. ) ;
#104925 = DIRECTION ( 'NONE',  ( 0.000000000000000000, 0.000000000000000000, 1.000000000000000000 ) ) ;
#104926 = CARTESIAN_POINT ( 'NONE',  ( -21.44999999999999929, 68.75000000001205080, -124.1731074845243370 ) ) ;
#104928 = EDGE_CURVE ( 'NONE', #189415, #204479, #10784, .T. ) ;
#104927 =( BOUNDED_CURVE ( )  B_SPLINE_CURVE ( 3, ( #19493, #98981, #78154, #75630 ),
 .UNSPECIFIED., .F., .F. ) 
 B_SPLINE_CURVE_WITH_KNOTS ( ( 4, 4 ),
 ( 3.192897208853993085, 4.712388980384689674 ),
 .UNSPECIFIED. ) 
 CURVE ( )  GEOMETRIC_REPRESENTATION_ITEM ( )  RATIONAL_B_SPLINE_CURVE ( ( 1.000000000000000000, 0.8166740347213228279, 0.8166740347213228279, 1.000000000000000000 ) ) 
 REPRESENTATION_ITEM ( '' )  );
#104929 = DIRECTION ( 'NONE',  ( -0.000000000000000000, -1.000000000000000000, -6.982962677686266711E-15 ) ) ;
#104930 = CARTESIAN_POINT ( 'NONE',  ( -16.80939487329394666, 9.949999999999983302, -20.85000000000088249 ) ) ;
#104931 = CARTESIAN_POINT ( 'NONE',  ( -14.23072895065543619, 66.54401276639984530, -188.5115763176265489 ) ) ;
#104932 = CARTESIAN_POINT ( 'NONE',  ( -23.15000000000000213, 59.16775194334852728, -221.0793150863668473 ) ) ;
#104934 = EDGE_LOOP ( 'NONE', ( #181771, #200545, #128806 ) ) ;
#104933 = EDGE_CURVE ( 'NONE', #156652, #154626, #169034, .T. ) ;
#104936 = ADVANCED_FACE ( 'NONE', ( #152846 ), #52406, .F. ) ;
#104935 = CARTESIAN_POINT ( 'NONE',  ( -18.50000000000000000, 66.65000000001229807, -157.6731074845244223 ) ) ;
#104937 = CARTESIAN_POINT ( 'NONE',  ( -14.00000000000000178, 62.10905854918435409, -217.1108499610990918 ) ) ;
#104938 = DIRECTION ( 'NONE',  ( 1.000000000000000000, 0.000000000000000000, 0.000000000000000000 ) ) ;
#104939 = FACE_OUTER_BOUND ( 'NONE', #31015, .T. ) ;
#104940 = ORIENTED_EDGE ( 'NONE', *, *, #69470, .F. ) ;
#104942 = CARTESIAN_POINT ( 'NONE',  ( 20.88420186297724612, 68.10670728244119232, -224.1434476749765565 ) ) ;
#104941 = CIRCLE ( 'NONE', #209212, 0.09999999999998898659 ) ;
#104944 = EDGE_CURVE ( 'NONE', #168638, #50336, #189378, .T. ) ;
#104943 = ORIENTED_EDGE ( 'NONE', *, *, #14358, .F. ) ;
#104945 = CARTESIAN_POINT ( 'NONE',  ( 13.88302573338718560, 9.457410944778565920, -115.5000839737900833 ) ) ;
#104946 = ORIENTED_EDGE ( 'NONE', *, *, #50279, .F. ) ;
#104947 =( BOUNDED_SURFACE ( )  B_SPLINE_SURFACE ( 3, 2, ( 
 ( #130875, #111329, #151759 ),
 ( #193443, #14818, #167471 ),
 ( #147889, #179038, #76040 ),
 ( #255910, #219390, #59011 ),
 ( #348, #16099, #40803 ),
 ( #35669, #99436, #253394 ) ),
 .UNSPECIFIED., .F., .F., .F. ) 
 B_SPLINE_SURFACE_WITH_KNOTS ( ( 4, 2, 4 ),
 ( 3, 3 ),
 ( -1.776356839400250465E-15, 0.7853981633974468357, 1.570796326794895448 ),
 ( 0.000000000000000000, 1.000000000000000000 ),
 .UNSPECIFIED. ) 
 GEOMETRIC_REPRESENTATION_ITEM ( )  RATIONAL_B_SPLINE_SURFACE ( (
 ( 1.000000000000000000, 0.5000000000000456302, 1.000000000000000000),
 ( 1.000000000000000000, 0.4993418825340405487, 1.000000000000000000),
 ( 1.000000000000000000, 0.5278258667052666553, 1.000000000000000000),
 ( 1.000000000000000000, 0.6092287576700228247, 1.000000000000000000),
 ( 1.000000000000000000, 0.6611148371775413812, 1.000000000000000000),
 ( 1.000000000000000000, 0.7071067811865597852, 1.000000000000000000) ) ) 
 REPRESENTATION_ITEM ( '' )  SURFACE ( )  );
#104948 = CYLINDRICAL_SURFACE ( 'NONE', #101300, 0.09999999999999939493 ) ;
#104949 = LINE ( 'NONE', #158568, #97879 ) ;
#104950 = EDGE_CURVE ( 'NONE', #198415, #203294, #10737, .T. ) ;
#104951 = ORIENTED_EDGE ( 'NONE', *, *, #208918, .F. ) ;
#104953 = ORIENTED_EDGE ( 'NONE', *, *, #136102, .F. ) ;
#104952 = CARTESIAN_POINT ( 'NONE',  ( 18.49999999999999289, 8.882751598337870647, -187.0399955572217721 ) ) ;
#104954 = EDGE_LOOP ( 'NONE', ( #21918, #158916, #162210, #31276 ) ) ;
#104955 = CYLINDRICAL_SURFACE ( 'NONE', #56235, 0.5000000000000004441 ) ;
#104956 = CARTESIAN_POINT ( 'NONE',  ( -18.58222699835055280, 65.66799936921512426, -63.92993998886008455 ) ) ;
#104957 = ORIENTED_EDGE ( 'NONE', *, *, #179314, .F. ) ;
#104958 = DIRECTION ( 'NONE',  ( -0.7071067811865388020, 0.7071067811865561215, 0.000000000000000000 ) ) ;
#104959 = CARTESIAN_POINT ( 'NONE',  ( -23.15000000000000213, 73.40000000001151648, -49.24772940728643533 ) ) ;
#104960 = EDGE_LOOP ( 'NONE', ( #142191, #133995, #219719, #96678, #204706 ) ) ;
#104961 = ORIENTED_EDGE ( 'NONE', *, *, #197493, .F. ) ;
#104962 =( BOUNDED_CURVE ( )  B_SPLINE_CURVE ( 3, ( #207351, #149952, #126518, #151228 ),
 .UNSPECIFIED., .F., .F. ) 
 B_SPLINE_CURVE_WITH_KNOTS ( ( 4, 4 ),
 ( 4.712388980384689674, 6.231880751915386263 ),
 .UNSPECIFIED. ) 
 CURVE ( )  GEOMETRIC_REPRESENTATION_ITEM ( )  RATIONAL_B_SPLINE_CURVE ( ( 1.000000000000000000, 0.8166740347213228279, 0.8166740347213228279, 1.000000000000000000 ) ) 
 REPRESENTATION_ITEM ( '' )  );
#104963 = EDGE_CURVE ( 'NONE', #89621, #240969, #14610, .T. ) ;
#104964 = FACE_OUTER_BOUND ( 'NONE', #4338, .T. ) ;
#104965 = ADVANCED_FACE ( 'NONE', ( #90246 ), #169853, .F. ) ;
#104966 = EDGE_CURVE ( 'NONE', #239369, #42405, #233006, .T. ) ;
#104967 = DIRECTION ( 'NONE',  ( -1.000000000000000000, -0.000000000000000000, -0.000000000000000000 ) ) ;
#104969 = VERTEX_POINT ( 'NONE', #237486 ) ;
#104968 = CARTESIAN_POINT ( 'NONE',  ( -18.50000000000000000, 43.57568952063339651, -245.1784935019914826 ) ) ;
#104970 = DIRECTION ( 'NONE',  ( 0.000000000000000000, 0.000000000000000000, 1.000000000000000000 ) ) ;
#104971 = CARTESIAN_POINT ( 'NONE',  ( 20.05000000000002913, 7.250000000011171508, -121.3500000000000227 ) ) ;
#104972 = CARTESIAN_POINT ( 'NONE',  ( -16.89318236219975589, 9.951535257886286345, -121.3551296321058857 ) ) ;
#104974 = DIRECTION ( 'NONE',  ( 0.000000000000000000, 0.8814952561688398358, -0.4721928772777406746 ) ) ;
#104973 = DIRECTION ( 'NONE',  ( 0.000000000000000000, 6.982962677686266711E-15, -1.000000000000000000 ) ) ;
#104975 = CARTESIAN_POINT ( 'NONE',  ( 21.05000000000000071, 39.20537871576060240, -236.6597480159109921 ) ) ;
#104976 = LINE ( 'NONE', #86713, #40303 ) ;
#104977 = AXIS2_PLACEMENT_3D ( 'NONE', #48042, #31094, #127590 ) ;
#104978 = DIRECTION ( 'NONE',  ( 1.734723475976817507E-14, -6.982962677686266711E-15, 1.000000000000000000 ) ) ;
#104979 = CARTESIAN_POINT ( 'NONE',  ( -18.59999999999999787, -1.736705739456431807, -78.51742258762372728 ) ) ;
#104980 = ORIENTED_EDGE ( 'NONE', *, *, #117250, .T. ) ;
#104981 = ORIENTED_EDGE ( 'NONE', *, *, #161784, .F. ) ;
#104982 = CARTESIAN_POINT ( 'NONE',  ( 20.94999999999999929, 1.115600667400684642E-11, -134.0000000000000284 ) ) ;
#104983 = VERTEX_POINT ( 'NONE', #234923 ) ;
#104984 = DIRECTION ( 'NONE',  ( 1.000000000000000000, -7.304098846218163263E-16, 4.217023435051626718E-16 ) ) ;
#104986 = EDGE_CURVE ( 'NONE', #180491, #51613, #56257, .T. ) ;
#104985 = ORIENTED_EDGE ( 'NONE', *, *, #83882, .F. ) ;
#104987 = AXIS2_PLACEMENT_3D ( 'NONE', #171758, #196413, #752 ) ;
#104988 = CIRCLE ( 'NONE', #234606, 11.64999999999999325 ) ;
#104989 = CYLINDRICAL_SURFACE ( 'NONE', #57387, 0.1000000000000028644 ) ;
#104990 = ORIENTED_EDGE ( 'NONE', *, *, #175765, .F. ) ;
#104991 = LINE ( 'NONE', #88016, #150708 ) ;
#104992 = EDGE_LOOP ( 'NONE', ( #149200, #125609, #36268, #178683 ) ) ;
#104993 = ORIENTED_EDGE ( 'NONE', *, *, #120580, .T. ) ;
#104994 = CARTESIAN_POINT ( 'NONE',  ( 19.92426406871192412, 54.53338637621133245, -228.6684279704127505 ) ) ;
#104995 = CARTESIAN_POINT ( 'NONE',  ( -21.11927991906891577, 75.99091632053813328, -109.4716006030158155 ) ) ;
#104997 = ORIENTED_EDGE ( 'NONE', *, *, #119874, .T. ) ;
#104996 = CYLINDRICAL_SURFACE ( 'NONE', #62235, 0.1000000000000021844 ) ;
#104998 = CARTESIAN_POINT ( 'NONE',  ( 19.96984138294323685, 11.75000000001116263, -158.7245720712021750 ) ) ;
#105000 = ORIENTED_EDGE ( 'NONE', *, *, #91386, .T. ) ;
#104999 = CARTESIAN_POINT ( 'NONE',  ( -15.75000000000000355, 47.91805600923872532, -233.7139610577891631 ) ) ;
#105001 = DIRECTION ( 'NONE',  ( 0.000000000000000000, 0.8814952561688429444, -0.4721928772777349015 ) ) ;
#105002 = DIRECTION ( 'NONE',  ( 0.000000000000000000, 0.000000000000000000, 1.000000000000000000 ) ) ;
#105004 = VERTEX_POINT ( 'NONE', #19732 ) ;
#105003 = CARTESIAN_POINT ( 'NONE',  ( 21.14999999999999858, 69.74218538953655866, -203.6208977758331855 ) ) ;
#105005 = DIRECTION ( 'NONE',  ( 0.000000000000000000, 0.000000000000000000, 1.000000000000000000 ) ) ;
#105007 = ADVANCED_FACE ( 'NONE', ( #194528 ), #38025, .T. ) ;
#105006 = CARTESIAN_POINT ( 'NONE',  ( -14.77538296656415007, 27.73642831988484758, -234.0663351390819287 ) ) ;
#105008 = CIRCLE ( 'NONE', #42508, 0.6000000000000033085 ) ;
#105009 = CIRCLE ( 'NONE', #250808, 11.75000000000000533 ) ;
#105010 = DIRECTION ( 'NONE',  ( 1.000000000000000000, 0.000000000000000000, 0.000000000000000000 ) ) ;
#105011 = CIRCLE ( 'NONE', #221745, 11.64999999999999325 ) ;
#105012 = VERTEX_POINT ( 'NONE', #233642 ) ;
#105014 = CARTESIAN_POINT ( 'NONE',  ( -21.12230431290519306, 69.54243334671967602, -203.5283173362134335 ) ) ;
#105013 = CARTESIAN_POINT ( 'NONE',  ( -21.14999999999999858, 11.50215294792677057, -198.5972978622482970 ) ) ;
#105016 = EDGE_CURVE ( 'NONE', #38637, #4064, #176249, .T. ) ;
#105015 = FACE_OUTER_BOUND ( 'NONE', #43727, .T. ) ;
#105017 = CARTESIAN_POINT ( 'NONE',  ( -23.15000000000000213, 61.57587952878036219, -212.2000740415318774 ) ) ;
#105018 = DIRECTION ( 'NONE',  ( -1.000000000000000000, -0.000000000000000000, -0.000000000000000000 ) ) ;
#105019 = DIRECTION ( 'NONE',  ( -1.000000000000000000, 0.000000000000000000, 0.000000000000000000 ) ) ;
#105020 = ORIENTED_EDGE ( 'NONE', *, *, #213390, .T. ) ;
#105021 = VERTEX_POINT ( 'NONE', #118839 ) ;
#105022 = ORIENTED_EDGE ( 'NONE', *, *, #201833, .T. ) ;
#105023 = ADVANCED_FACE ( 'NONE', ( #159247 ), #223330, .T. ) ;
#105024 = DIRECTION ( 'NONE',  ( 0.000000000000000000, 1.000000000000000000, 0.000000000000000000 ) ) ;
#105025 = EDGE_CURVE ( 'NONE', #53997, #140889, #110921, .T. ) ;
#105026 = VERTEX_POINT ( 'NONE', #99229 ) ;
#105027 = DIRECTION ( 'NONE',  ( -1.000000000000000000, -0.000000000000000000, -0.000000000000000000 ) ) ;
#105028 = ORIENTED_EDGE ( 'NONE', *, *, #58861, .T. ) ;
#105029 = CARTESIAN_POINT ( 'NONE',  ( -21.93340585971646561, 7.324147022868593204, -100.5000000000000426 ) ) ;
#105030 = CARTESIAN_POINT ( 'NONE',  ( 23.14999999999999858, 70.40000000001222702, -148.9283735034374843 ) ) ;
#105031 = VECTOR ( 'NONE', #156222, 1000.000000000000000 ) ;
#105032 = VERTEX_POINT ( 'NONE', #79668 ) ;
#105033 = DIRECTION ( 'NONE',  ( 0.000000000000000000, 0.9908441862701596881, -0.1350103645451904977 ) ) ;
#105034 = SHAPE_REPRESENTATION_RELATIONSHIP ( 'NONE' , 'NONE' ,  #198303, #51500 ) ;
#105035 = AXIS2_PLACEMENT_3D ( 'NONE', #46972, #26164, #10447 ) ;
#105036 = ORIENTED_EDGE ( 'NONE', *, *, #184137, .T. ) ;
#105037 = EDGE_CURVE ( 'NONE', #7533, #159923, #54964, .T. ) ;
#105038 = ORIENTED_EDGE ( 'NONE', *, *, #171497, .F. ) ;
#105039 = EDGE_CURVE ( 'NONE', #198292, #57380, #36750, .T. ) ;
#105040 = VERTEX_POINT ( 'NONE', #154138 ) ;
#105041 = CARTESIAN_POINT ( 'NONE',  ( -23.15000000000000213, 74.00000000001254818, -182.6477294072865050 ) ) ;
#105042 = CARTESIAN_POINT ( 'NONE',  ( 21.05000000000000071, 9.374458193048763377, -220.5475659691911119 ) ) ;
#105043 = CARTESIAN_POINT ( 'NONE',  ( 18.69999999999999929, -1.212568896937008089, -8.000000000000000000 ) ) ;
#105044 = CARTESIAN_POINT ( 'NONE',  ( -33.72168855820452649, 64.52683809664961245, -127.2731074845243882 ) ) ;
#105045 = CARTESIAN_POINT ( 'NONE',  ( -20.64999999999999858, 82.57900542960499024, -215.5587758314583482 ) ) ;
#105046 = DIRECTION ( 'NONE',  ( 1.000000000000000000, 2.952720810173289112E-16, -0.000000000000000000 ) ) ;
#105047 = CIRCLE ( 'NONE', #9235, 0.09999999999998898659 ) ;
#105049 = DIRECTION ( 'NONE',  ( 0.000000000000000000, 1.000000000000000000, 0.000000000000000000 ) ) ;
#105048 = CARTESIAN_POINT ( 'NONE',  ( 18.59999999999999076, 8.433899723187009201, -209.4150263691077782 ) ) ;
#105050 = DIRECTION ( 'NONE',  ( 0.000000000000000000, -0.8814952561688430555, 0.4721928772777346239 ) ) ;
#105052 = ORIENTED_EDGE ( 'NONE', *, *, #161868, .T. ) ;
#105051 = DIRECTION ( 'NONE',  ( 1.000000000000000000, -9.458662978381124901E-16, 5.066746821047763994E-16 ) ) ;
#105054 = DIRECTION ( 'NONE',  ( -1.000000000000000000, 0.000000000000000000, 0.000000000000000000 ) ) ;
#105053 = CARTESIAN_POINT ( 'NONE',  ( -20.94999999999999574, 11.75000000001115552, -40.34160068989711334 ) ) ;
#105055 = DIRECTION ( 'NONE',  ( 4.504528286903032433E-15, 0.1298341882520054891, 0.9915357197604850459 ) ) ;
#105056 = ORIENTED_EDGE ( 'NONE', *, *, #26671, .F. ) ;
#105057 = CARTESIAN_POINT ( 'NONE',  ( 20.95132126680579887, 10.48994987015794322, -74.57032453843456210 ) ) ;
#105058 = CARTESIAN_POINT ( 'NONE',  ( -18.50000000000000000, 9.250000000011157297, -112.8500000000000369 ) ) ;
#105059 = CARTESIAN_POINT ( 'NONE',  ( 21.05000000000000071, -11.64999999998883595, -64.10000000000000853 ) ) ;
#105060 = ORIENTED_EDGE ( 'NONE', *, *, #229545, .T. ) ;
#105061 = EDGE_CURVE ( 'NONE', #38481, #144465, #134506, .T. ) ;
#105062 = CIRCLE ( 'NONE', #109179, 0.5000000000000004441 ) ;
#105064 = DIRECTION ( 'NONE',  ( -0.000000000000000000, -0.000000000000000000, -1.000000000000000000 ) ) ;
#105063 = AXIS2_PLACEMENT_3D ( 'NONE', #136908, #138171, #238575 ) ;
#105065 = EDGE_CURVE ( 'NONE', #218711, #83651, #127481, .T. ) ;
#105066 = CARTESIAN_POINT ( 'NONE',  ( 20.12500000000000355, 10.24195072709382970, -108.3602037270861587 ) ) ;
#105067 = DIRECTION ( 'NONE',  ( 1.000000000000000000, 7.136802563874199107E-16, 1.554319503706929991E-16 ) ) ;
#105068 = CIRCLE ( 'NONE', #100957, 0.5000000000000022204 ) ;
#105069 = ORIENTED_EDGE ( 'NONE', *, *, #177340, .T. ) ;
#105070 = ORIENTED_EDGE ( 'NONE', *, *, #201617, .T. ) ;
#105071 = CIRCLE ( 'NONE', #84391, 2.000000000000001776 ) ;
#105072 = DIRECTION ( 'NONE',  ( 1.000000000000000000, 0.000000000000000000, 0.000000000000000000 ) ) ;
#105073 = VERTEX_POINT ( 'NONE', #199660 ) ;
#105074 = CARTESIAN_POINT ( 'NONE',  ( 21.07094088545303734, 6.320167221927647461, -66.90110629744782500 ) ) ;
#105075 = CARTESIAN_POINT ( 'NONE',  ( -18.46919391072055561, -9.670724388266535243, -174.1738035317996491 ) ) ;
#105076 = DIRECTION ( 'NONE',  ( 0.000000000000000000, -0.8096735173027155286, 0.5868805631290314739 ) ) ;
#105078 = EDGE_CURVE ( 'NONE', #148410, #159233, #206595, .T. ) ;
#105077 = DIRECTION ( 'NONE',  ( 0.000000000000000000, 0.9910827722268049644, -0.1332476588733589318 ) ) ;
#105079 = VERTEX_POINT ( 'NONE', #116263 ) ;
#105080 = VECTOR ( 'NONE', #190079, 1000.000000000000000 ) ;
#105082 = CIRCLE ( 'NONE', #9260, 0.1000000000000001027 ) ;
#105081 = LINE ( 'NONE', #8596, #129560 ) ;
#105083 = CYLINDRICAL_SURFACE ( 'NONE', #129120, 0.09999999999998898659 ) ;
#105086 = EDGE_CURVE ( 'NONE', #71706, #83423, #156745, .T. ) ;
#105085 = DIRECTION ( 'NONE',  ( -0.000000000000000000, -0.000000000000000000, 1.000000000000000000 ) ) ;
#105084 = AXIS2_PLACEMENT_3D ( 'NONE', #46229, #21554, #219730 ) ;
#105087 = VECTOR ( 'NONE', #74304, 1000.000000000000000 ) ;
#105088 = CARTESIAN_POINT ( 'NONE',  ( 21.05000000000000071, 76.00000000001190870, -103.0231074845243029 ) ) ;
#105089 = CIRCLE ( 'NONE', #134156, 0.1000000000000062367 ) ;
#105090 = ORIENTED_EDGE ( 'NONE', *, *, #57873, .F. ) ;
#105091 = CIRCLE ( 'NONE', #250859, 0.1999999999999945155 ) ;
#105092 = AXIS2_PLACEMENT_3D ( 'NONE', #101235, #123425, #85537 ) ;
#105094 = EDGE_LOOP ( 'NONE', ( #180488, #35342, #120603, #178698, #24 ) ) ;
#105093 = DIRECTION ( 'NONE',  ( 0.000000000000000000, 0.000000000000000000, -1.000000000000000000 ) ) ;
#105095 = CARTESIAN_POINT ( 'NONE',  ( -23.15000000000000213, 2.319530388122572617, -217.8268657444419887 ) ) ;
#105096 = CARTESIAN_POINT ( 'NONE',  ( 18.51565452909312626, 78.14133456817783951, -231.3592074214313072 ) ) ;
#105097 = EDGE_CURVE ( 'NONE', #257555, #101145, #108284, .T. ) ;
#105098 = AXIS2_PLACEMENT_3D ( 'NONE', #117873, #18774, #134850 ) ;
#105099 = CARTESIAN_POINT ( 'NONE',  ( 18.59999999999999432, 1.728086936805619311, -20.38443500516777007 ) ) ;
#105100 = CARTESIAN_POINT ( 'NONE',  ( -18.59999999999999787, 1.851028230152016674, -179.1539132694224463 ) ) ;
#105101 = CARTESIAN_POINT ( 'NONE',  ( 21.14999999999999858, 10.21728496540352360, -227.9671432372868765 ) ) ;
#105102 = DIRECTION ( 'NONE',  ( 0.7071067811865474617, 0.6909108974501236844, 0.1504730267678055788 ) ) ;
#105103 = VERTEX_POINT ( 'NONE', #117532 ) ;
#105104 = DIRECTION ( 'NONE',  ( 0.000000000000000000, -0.2128009952263604232, 0.9770955615653316162 ) ) ;
#105105 = DIRECTION ( 'NONE',  ( 0.000000000000000000, 0.000000000000000000, 1.000000000000000000 ) ) ;
#105106 = CARTESIAN_POINT ( 'NONE',  ( -33.72168855820452649, 11.47316190336247388, -24.25000000000001066 ) ) ;
#105107 = CARTESIAN_POINT ( 'NONE',  ( 18.49999999999999289, 10.49142135624846439, -125.3500000000000512 ) ) ;
#105108 = AXIS2_PLACEMENT_3D ( 'NONE', #133707, #213234, #94576 ) ;
#105109 = LINE ( 'NONE', #163848, #11671 ) ;
#105110 = AXIS2_PLACEMENT_3D ( 'NONE', #109364, #53268, #93670 ) ;
#105111 = CIRCLE ( 'NONE', #246790, 7.900000000000007461 ) ;
#105112 = EDGE_LOOP ( 'NONE', ( #215090, #198232, #67796, #200619 ) ) ;
#105113 = VERTEX_POINT ( 'NONE', #97939 ) ;
#105114 = DIRECTION ( 'NONE',  ( 0.000000000000000000, 1.000000000000000000, 0.000000000000000000 ) ) ;
#105115 = CARTESIAN_POINT ( 'NONE',  ( -21.04999999999999716, 85.60000000001264198, -196.4910380878246201 ) ) ;
#105116 = CARTESIAN_POINT ( 'NONE',  ( 18.39999999999999858, 87.08727414655710675, -199.6327537731849873 ) ) ;
#105117 = CARTESIAN_POINT ( 'NONE',  ( 23.50000000000005684, 74.63923853664559260, -43.99645795275012006 ) ) ;
#105118 = FACE_OUTER_BOUND ( 'NONE', #85090, .T. ) ;
#105119 = CARTESIAN_POINT ( 'NONE',  ( 20.94999999999999574, 65.37642973952880254, -62.03116228129384524 ) ) ;
#105120 = DIRECTION ( 'NONE',  ( 0.000000000000000000, 0.9908441862701600211, -0.1350103645451876666 ) ) ;
#105121 = VECTOR ( 'NONE', #129762, 1000.000000000000000 ) ;
#105122 = ORIENTED_EDGE ( 'NONE', *, *, #153689, .F. ) ;
#105123 = FACE_OUTER_BOUND ( 'NONE', #102714, .T. ) ;
#105124 = VECTOR ( 'NONE', #81094, 1000.000000000000114 ) ;
#105125 = ORIENTED_EDGE ( 'NONE', *, *, #58822, .T. ) ;
#105126 = DIRECTION ( 'NONE',  ( -1.000000000000000000, 0.000000000000000000, -0.000000000000000000 ) ) ;
#105127 = CARTESIAN_POINT ( 'NONE',  ( -21.44999999999999929, 68.65000000001180069, -81.87310748452436826 ) ) ;
#105128 = DIRECTION ( 'NONE',  ( 1.000000000000000000, 0.000000000000000000, 0.000000000000000000 ) ) ;
#105129 = DIRECTION ( 'NONE',  ( 0.000000000000000000, -0.9394191166662962944, -0.3427706569149635563 ) ) ;
#105130 = FACE_OUTER_BOUND ( 'NONE', #126262, .T. ) ;
#105131 = CARTESIAN_POINT ( 'NONE',  ( 20.85000000000000142, -11.64999999998883595, -134.0000000000000284 ) ) ;
#105132 = CARTESIAN_POINT ( 'NONE',  ( -18.51991288638512501, -9.392436789673425324, -7.143266403958832278 ) ) ;
#105133 = CARTESIAN_POINT ( 'NONE',  ( -21.07094088545304089, 6.320167221927643020, -66.90110629744782500 ) ) ;
#105134 = CYLINDRICAL_SURFACE ( 'NONE', #4795, 0.09999999999999771572 ) ;
#105135 = ADVANCED_FACE ( 'NONE', ( #177548 ), #256989, .T. ) ;
#105136 = FACE_OUTER_BOUND ( 'NONE', #255950, .T. ) ;
#105137 = CARTESIAN_POINT ( 'NONE',  ( 18.59999999999999076, 6.550000000011156231, -88.15000000000004832 ) ) ;
#105138 = DIRECTION ( 'NONE',  ( -1.000000000000000000, 0.000000000000000000, 0.000000000000000000 ) ) ;
#105139 = CARTESIAN_POINT ( 'NONE',  ( 21.04999999999999716, 8.871279686006802834, -176.0586289951408787 ) ) ;
#105140 = CIRCLE ( 'NONE', #171681, 0.6000000000000033085 ) ;
#105141 = ORIENTED_EDGE ( 'NONE', *, *, #223667, .F. ) ;
#105142 = DIRECTION ( 'NONE',  ( 1.000000000000000000, 0.000000000000000000, 0.000000000000000000 ) ) ;
#105143 = CARTESIAN_POINT ( 'NONE',  ( -20.94999999999999929, 88.41227409416113403, -39.02310748452423894 ) ) ;
#105144 = EDGE_CURVE ( 'NONE', #154991, #61597, #181387, .T. ) ;
#105145 = ORIENTED_EDGE ( 'NONE', *, *, #250125, .F. ) ;
#105146 = DIRECTION ( 'NONE',  ( 0.000000000000000000, 0.000000000000000000, -1.000000000000000000 ) ) ;
#105147 = CARTESIAN_POINT ( 'NONE',  ( 21.10710606213542562, 67.22310597611910055, -157.7821109581250028 ) ) ;
#105148 = EDGE_CURVE ( 'NONE', #53603, #174229, #221739, .T. ) ;
#105149 = DIRECTION ( 'NONE',  ( 0.000000000000000000, -0.2128009952263603954, 0.9770955615653315052 ) ) ;
#105150 = EDGE_LOOP ( 'NONE', ( #184455, #138138, #208060, #47154 ) ) ;
#105151 = CARTESIAN_POINT ( 'NONE',  ( 20.85000000000000142, 64.25000000001146816, -42.80697314750249660 ) ) ;
#105152 = CARTESIAN_POINT ( 'NONE',  ( 18.59999999999999787, 7.476371755685457643, -241.7308184205399471 ) ) ;
#105153 = AXIS2_PLACEMENT_3D ( 'NONE', #20494, #81688, #201671 ) ;
#105154 = ORIENTED_EDGE ( 'NONE', *, *, #245461, .F. ) ;
#105155 = VECTOR ( 'NONE', #13185, 1000.000000000000000 ) ;
#105156 = LINE ( 'NONE', #47777, #235313 ) ;
#105157 = AXIS2_PLACEMENT_3D ( 'NONE', #23334, #62437, #42868 ) ;
#105158 = ADVANCED_FACE ( 'NONE', ( #223046 ), #183927, .T. ) ;
#105159 = VERTEX_POINT ( 'NONE', #125242 ) ;
#105160 = ADVANCED_FACE ( 'NONE', ( #44430 ), #214673, .T. ) ;
#105161 = LINE ( 'NONE', #206881, #37723 ) ;
#105162 = FACE_OUTER_BOUND ( 'NONE', #232593, .T. ) ;
#105163 = DIRECTION ( 'NONE',  ( 0.000000000000000000, -0.8814952561688430555, 0.4721928772777346239 ) ) ;
#105165 = CARTESIAN_POINT ( 'NONE',  ( 21.08035267497491105, 33.99482676082369892, -243.8066059240260586 ) ) ;
#105164 = PRODUCT_DEFINITION_CONTEXT ( 'detailed design', #922, 'design' ) ;
#105166 = ADVANCED_FACE ( 'NONE', ( #202213 ), #242602, .T. ) ;
#105167 = DIRECTION ( 'NONE',  ( 0.000000000000000000, 0.000000000000000000, -1.000000000000000000 ) ) ;
#105168 = CARTESIAN_POINT ( 'NONE',  ( 18.59999999999999076, 64.35000000001275566, -215.2731074845244450 ) ) ;
#105169 = CARTESIAN_POINT ( 'NONE',  ( 20.94999999999999929, 28.15345123516638282, -259.0759448016705733 ) ) ;
#105170 = VECTOR ( 'NONE', #37075, 1000.000000000000000 ) ;
#105171 = CYLINDRICAL_SURFACE ( 'NONE', #26242, 0.09999999999998898659 ) ;
#105173 = CARTESIAN_POINT ( 'NONE',  ( 20.85000000000000142, 11.75000000001115907, -127.2161343370219413 ) ) ;
#105172 = AXIS2_PLACEMENT_3D ( 'NONE', #53334, #170768, #212424 ) ;
#105175 = ORIENTED_EDGE ( 'NONE', *, *, #38472, .T. ) ;
#105174 = CARTESIAN_POINT ( 'NONE',  ( -16.89268316805465986, 14.16190809729244648, -219.2603268738197073 ) ) ;
#105176 = ORIENTED_EDGE ( 'NONE', *, *, #183522, .T. ) ;
#105178 = CARTESIAN_POINT ( 'NONE',  ( -23.15000000000000213, -9.599999999988845900, -157.6060308773475924 ) ) ;
#105177 = CARTESIAN_POINT ( 'NONE',  ( 23.14999999999999503, 64.25000000001146816, -43.03791325517834565 ) ) ;
#105180 = ORIENTED_EDGE ( 'NONE', *, *, #80419, .F. ) ;
#105179 = CARTESIAN_POINT ( 'NONE',  ( 20.94999999999999929, 0.000000000000000000, -33.50000000000000000 ) ) ;
#105181 = ORIENTED_EDGE ( 'NONE', *, *, #57794, .T. ) ;
#105182 = CARTESIAN_POINT ( 'NONE',  ( -18.59999999999999787, -9.321008403350132809, -74.23593824907793248 ) ) ;
#105183 = DIRECTION ( 'NONE',  ( -1.000000000000000000, 1.614276770400120371E-15, 3.515722686956159758E-16 ) ) ;
#105184 = EDGE_CURVE ( 'NONE', #225625, #242050, #144217, .T. ) ;
#105185 = DIRECTION ( 'NONE',  ( -1.000000000000000000, 0.000000000000000000, 0.000000000000000000 ) ) ;
#105186 = AXIS2_PLACEMENT_3D ( 'NONE', #245074, #147254, #106833 ) ;
#105187 = CARTESIAN_POINT ( 'NONE',  ( -20.88420186297724257, 10.33025634372637391, -173.0870929282638997 ) ) ;
#105188 = CARTESIAN_POINT ( 'NONE',  ( -18.55807992284872299, 67.49241595948059569, -195.4314365843280541 ) ) ;
#105189 = CARTESIAN_POINT ( 'NONE',  ( -20.85000000000000142, -1.135018845910178431, -41.21697688343231647 ) ) ;
#105190 = AXIS2_PLACEMENT_3D ( 'NONE', #746, #157319, #256318 ) ;
#105191 = AXIS2_PLACEMENT_3D ( 'NONE', #57111, #257853, #15466 ) ;
#105192 = AXIS2_PLACEMENT_3D ( 'NONE', #219345, #40756, #253335 ) ;
#105193 = B_SPLINE_CURVE_WITH_KNOTS ( 'NONE', 3,
 ( #131077, #210618, #68550, #71132 ),
 .UNSPECIFIED., .F., .F.,
 ( 4, 4 ),
 ( 0.000000000000000000, 0.0001048066582182451801 ),
 .UNSPECIFIED. ) ;
#105194 = EDGE_CURVE ( 'NONE', #189000, #46992, #146071, .T. ) ;
#105196 = VECTOR ( 'NONE', #118536, 1000.000000000000000 ) ;
#105195 = DIRECTION ( 'NONE',  ( 0.000000000000000000, 0.8814952561688431665, -0.4721928772777346794 ) ) ;
#105197 = ORIENTED_EDGE ( 'NONE', *, *, #11192, .T. ) ;
#105198 = ORIENTED_EDGE ( 'NONE', *, *, #29422, .F. ) ;
#105199 = DIRECTION ( 'NONE',  ( 0.000000000000000000, -0.4721928772777346239, -0.8814952561688430555 ) ) ;
#105200 = EDGE_LOOP ( 'NONE', ( #203511, #166980, #245327, #42859, #222233 ) ) ;
#105201 = CARTESIAN_POINT ( 'NONE',  ( 22.60000000000000142, 64.25043287652299284, -170.1239658536231616 ) ) ;
#105202 = ORIENTED_EDGE ( 'NONE', *, *, #22420, .F. ) ;
#105203 = DIRECTION ( 'NONE',  ( 0.000000000000000000, -0.01562499999996343723, -0.9998779222360104635 ) ) ;
#105204 = CARTESIAN_POINT ( 'NONE',  ( 22.39999999999999503, 7.612336166715857111, -199.3421143478784359 ) ) ;
#105205 = CARTESIAN_POINT ( 'NONE',  ( 21.05000000000000071, 76.00000000001213607, -136.5231074845243313 ) ) ;
#105206 = LINE ( 'NONE', #145652, #108192 ) ;
#105207 = EDGE_LOOP ( 'NONE', ( #212217, #837, #50240, #44080 ) ) ;
#105208 = DIRECTION ( 'NONE',  ( 1.000000000000000000, 0.000000000000000000, 0.000000000000000000 ) ) ;
#105209 = VERTEX_POINT ( 'NONE', #225590 ) ;
#105210 = CARTESIAN_POINT ( 'NONE',  ( 21.05000000000000071, -11.29603075032412995, -137.0478991596638991 ) ) ;
#105211 = CARTESIAN_POINT ( 'NONE',  ( -21.53699400388026319, 30.46440795807614776, -252.3262297579089193 ) ) ;
#105212 = CARTESIAN_POINT ( 'NONE',  ( -18.59999999999999787, -1.835859311432481045, -179.1044391687985353 ) ) ;
#105213 = DIRECTION ( 'NONE',  ( 1.186688945009009831E-16, 1.000000000000000000, 6.982962677686266711E-15 ) ) ;
#105214 = ORIENTED_EDGE ( 'NONE', *, *, #103804, .T. ) ;
#105215 = AXIS2_PLACEMENT_3D ( 'NONE', #38221, #82430, #139853 ) ;
#105216 = CARTESIAN_POINT ( 'NONE',  ( 21.00000000000000000, 43.85220609964365224, -235.6449878604632886 ) ) ;
#105217 = ORIENTED_EDGE ( 'NONE', *, *, #23162, .F. ) ;
#105220 = ORIENTED_EDGE ( 'NONE', *, *, #216132, .T. ) ;
#105219 = CARTESIAN_POINT ( 'NONE',  ( 21.13736287352038445, 67.95335762362823573, -149.1731074845244223 ) ) ;
#105218 = CARTESIAN_POINT ( 'NONE',  ( -18.59999999999999787, 7.021664781900089913, -37.33356540189728889 ) ) ;
#105221 = DIRECTION ( 'NONE',  ( -0.000000000000000000, -0.01283462868040327436, 0.9999176327611370985 ) ) ;
#105222 = EDGE_LOOP ( 'NONE', ( #64017, #202022, #129069, #70668 ) ) ;
#105223 = ADVANCED_FACE ( 'NONE', ( #46962 ), #206058, .T. ) ;
#105224 = LINE ( 'NONE', #84369, #154424 ) ;
#105225 = ORIENTED_EDGE ( 'NONE', *, *, #77797, .F. ) ;
#105227 = EDGE_CURVE ( 'NONE', #197443, #56953, #2576, .T. ) ;
#105226 = DIRECTION ( 'NONE',  ( 0.000000000000000000, 0.9126074666063753726, 0.4088369013363320481 ) ) ;
#105228 = AXIS2_PLACEMENT_3D ( 'NONE', #83815, #139958, #117840 ) ;
#105229 = CARTESIAN_POINT ( 'NONE',  ( 18.54999999999999716, 8.750000000011182166, -176.7499999999999716 ) ) ;
#105230 = EDGE_CURVE ( 'NONE', #100941, #128950, #31843, .T. ) ;
#105231 = DIRECTION ( 'NONE',  ( 0.000000000000000000, 0.000000000000000000, -1.000000000000000000 ) ) ;
#105232 = ADVANCED_FACE ( 'NONE', ( #48265 ), #28757, .F. ) ;
#105233 = DIRECTION ( 'NONE',  ( 0.000000000000000000, -6.467318590049456648E-15, 1.000000000000000000 ) ) ;
#105234 = CIRCLE ( 'NONE', #226055, 0.2000000000000057288 ) ;
#105235 = CARTESIAN_POINT ( 'NONE',  ( 23.25000000000000000, 6.550000000000000711, -12.35000000000000320 ) ) ;
#105236 = VECTOR ( 'NONE', #251514, 1000.000000000000000 ) ;
#105238 = ORIENTED_EDGE ( 'NONE', *, *, #154083, .F. ) ;
#105237 = EDGE_CURVE ( 'NONE', #152197, #115296, #132955, .T. ) ;
#105239 = AXIS2_PLACEMENT_3D ( 'NONE', #48883, #207982, #67169 ) ;
#105240 = AXIS2_PLACEMENT_3D ( 'NONE', #41868, #200916, #181379 ) ;
#105241 = CARTESIAN_POINT ( 'NONE',  ( 23.14999999999998437, -11.74999999998884448, -167.4999999999999432 ) ) ;
#105242 = LINE ( 'NONE', #226491, #232549 ) ;
#105243 = CARTESIAN_POINT ( 'NONE',  ( -15.70407651835961360, 66.64419340838212236, -153.7320049529782864 ) ) ;
#105244 = EDGE_CURVE ( 'NONE', #204139, #101473, #50807, .T. ) ;
#105245 = ORIENTED_EDGE ( 'NONE', *, *, #101116, .F. ) ;
#105246 = DIRECTION ( 'NONE',  ( 0.000000000000000000, -0.9770955615653316162, -0.2128009952263604232 ) ) ;
#105249 = EDGE_CURVE ( 'NONE', #106008, #237605, #7876, .T. ) ;
#105248 = EDGE_CURVE ( 'NONE', #162643, #71034, #131766, .T. ) ;
#105247 = ORIENTED_EDGE ( 'NONE', *, *, #96218, .T. ) ;
#105250 = CARTESIAN_POINT ( 'NONE',  ( -18.79999999999999716, 7.900000000000000355, -1.300000000000000044 ) ) ;
#105251 = AXIS2_PLACEMENT_3D ( 'NONE', #89527, #230327, #133797 ) ;
#105252 = CARTESIAN_POINT ( 'NONE',  ( -20.94999999999999929, 74.75000000001232081, -162.0231074845243597 ) ) ;
#105253 = CARTESIAN_POINT ( 'NONE',  ( 20.99551997958343108, 36.17041074700797054, -235.9598556649045520 ) ) ;
#105255 = ORIENTED_EDGE ( 'NONE', *, *, #106189, .T. ) ;
#105254 = CARTESIAN_POINT ( 'NONE',  ( -18.59999999999999787, 5.900000000011102586, -110.7190997646564483 ) ) ;
#105256 = DIRECTION ( 'NONE',  ( 1.000000000000000000, 0.000000000000000000, 0.000000000000000000 ) ) ;
#105257 = AXIS2_PLACEMENT_3D ( 'NONE', #3093, #219581, #125631 ) ;
#105258 = CARTESIAN_POINT ( 'NONE',  ( -12.48127053791144547, 62.79551507739392235, -216.3883973845401840 ) ) ;
#105259 = AXIS2_PLACEMENT_3D ( 'NONE', #254247, #148765, #49646 ) ;
#105260 = EDGE_CURVE ( 'NONE', #203548, #213770, #214967, .T. ) ;
#105261 = DIRECTION ( 'NONE',  ( 0.000000000000000000, -0.9964539953858893018, -0.08413937888704772772 ) ) ;
#105262 = ORIENTED_EDGE ( 'NONE', *, *, #165055, .T. ) ;
#105263 = AXIS2_PLACEMENT_3D ( 'NONE', #68431, #130969, #89259 ) ;
#105264 = CARTESIAN_POINT ( 'NONE',  ( -20.94999999999999929, 77.16270174995010223, -128.4231074845242802 ) ) ;
#105265 = DIRECTION ( 'NONE',  ( 1.000000000000000000, 0.000000000000000000, 0.000000000000000000 ) ) ;
#105267 = ORIENTED_EDGE ( 'NONE', *, *, #181183, .T. ) ;
#105266 = EDGE_CURVE ( 'NONE', #257620, #213934, #226899, .T. ) ;
#105269 = EDGE_CURVE ( 'NONE', #129083, #118551, #19340, .T. ) ;
#105268 = CARTESIAN_POINT ( 'NONE',  ( 22.49999999999999645, 64.35042919246758686, -170.1231074845244393 ) ) ;
#105270 = AXIS2_PLACEMENT_3D ( 'NONE', #132903, #212445, #36386 ) ;
#105271 = ORIENTED_EDGE ( 'NONE', *, *, #206818, .F. ) ;
#105272 = AXIS2_PLACEMENT_3D ( 'NONE', #81381, #85237, #205204 ) ;
#105273 = CIRCLE ( 'NONE', #26800, 0.09999999999998898659 ) ;
#105274 = EDGE_CURVE ( 'NONE', #53997, #43410, #165085, .T. ) ;
#105275 = DIRECTION ( 'NONE',  ( 0.000000000000000000, 0.2617529984165152257, 0.9651348961777124202 ) ) ;
#105276 = AXIS2_PLACEMENT_3D ( 'NONE', #42274, #63098, #181781 ) ;
#105278 = ORIENTED_EDGE ( 'NONE', *, *, #30494, .F. ) ;
#105277 = CARTESIAN_POINT ( 'NONE',  ( 23.14999999999999503, 14.05000000001115623, -128.4863049292391395 ) ) ;
#105279 = EDGE_CURVE ( 'NONE', #19019, #242320, #11731, .T. ) ;
#105282 = EDGE_LOOP ( 'NONE', ( #254975, #56672, #228712, #152880 ) ) ;
#105281 = ORIENTED_EDGE ( 'NONE', *, *, #63228, .F. ) ;
#105280 = CARTESIAN_POINT ( 'NONE',  ( 20.73486653747088937, 68.25000000001197975, -115.6731074845243654 ) ) ;
#105283 = CARTESIAN_POINT ( 'NONE',  ( 20.94999999999999929, 69.35000000001262777, -193.5060803140843859 ) ) ;
#105284 = DIRECTION ( 'NONE',  ( -1.000000000000000000, 0.000000000000000000, 0.000000000000000000 ) ) ;
#105285 = CARTESIAN_POINT ( 'NONE',  ( -23.15000000000000213, 11.65000000001115588, -54.84999999999999432 ) ) ;
#105287 = CARTESIAN_POINT ( 'NONE',  ( -12.48127053791145613, 66.62341902196760657, -51.89616123751247301 ) ) ;
#105286 = DIRECTION ( 'NONE',  ( -0.000000000000000000, -6.982962677686266711E-15, 1.000000000000000000 ) ) ;
#105288 = DIRECTION ( 'NONE',  ( -3.469446951953604722E-14, -0.9999176327611370985, -0.01283462868040260302 ) ) ;
#105289 = CIRCLE ( 'NONE', #159515, 0.09999999999998898659 ) ;
#105290 = DIRECTION ( 'NONE',  ( 1.000000000000000000, 0.000000000000000000, 0.000000000000000000 ) ) ;
#105291 = PLANE ( 'NONE',  #125703 ) ;
#105293 = DIRECTION ( 'NONE',  ( 1.000000000000000000, 0.000000000000000000, 0.000000000000000000 ) ) ;
#105292 = CIRCLE ( 'NONE', #26243, 7.720710678118663850 ) ;
#105294 = VERTEX_POINT ( 'NONE', #31310 ) ;
#105295 = ORIENTED_EDGE ( 'NONE', *, *, #200566, .T. ) ;
#105296 = LINE ( 'NONE', #182324, #29311 ) ;
#105298 = ORIENTED_EDGE ( 'NONE', *, *, #179087, .T. ) ;
#105297 = DIRECTION ( 'NONE',  ( 0.000000000000000000, -0.9908441862701596881, -0.1350103645451904977 ) ) ;
#105299 = ORIENTED_EDGE ( 'NONE', *, *, #211355, .F. ) ;
#105300 = CARTESIAN_POINT ( 'NONE',  ( 23.24999999999999289, 69.55000000001173532, -81.27310748452437394 ) ) ;
#105301 = ORIENTED_EDGE ( 'NONE', *, *, #110442, .T. ) ;
#105302 = CARTESIAN_POINT ( 'NONE',  ( -20.54999999999999716, -6.980131799343633148, -224.1659828210180194 ) ) ;
#105303 = ORIENTED_EDGE ( 'NONE', *, *, #175041, .F. ) ;
#105304 = FACE_OUTER_BOUND ( 'NONE', #118201, .T. ) ;
#105305 = DIRECTION ( 'NONE',  ( 0.000000000000000000, 1.000000000000000000, 6.982962677686266711E-15 ) ) ;
#105306 = CIRCLE ( 'NONE', #71499, 0.09999999999999939493 ) ;
#105308 = ORIENTED_EDGE ( 'NONE', *, *, #210428, .F. ) ;
#105307 = ORIENTED_EDGE ( 'NONE', *, *, #203874, .T. ) ;
#105309 = ORIENTED_EDGE ( 'NONE', *, *, #159394, .T. ) ;
#105310 = DIRECTION ( 'NONE',  ( -0.000000000000000000, 1.000000000000000000, 6.982962677686266711E-15 ) ) ;
#105311 = ORIENTED_EDGE ( 'NONE', *, *, #137893, .F. ) ;
#105312 = ORIENTED_EDGE ( 'NONE', *, *, #140202, .T. ) ;
#105313 = CARTESIAN_POINT ( 'NONE',  ( -20.54999999999999716, 2.400000000011155432, -157.6060308773475924 ) ) ;
#105314 = CARTESIAN_POINT ( 'NONE',  ( 21.14999999999999503, 76.10000000001203091, -114.6726782920691079 ) ) ;
#105315 = AXIS2_PLACEMENT_3D ( 'NONE', #257467, #239258, #154611 ) ;
#105317 = ORIENTED_EDGE ( 'NONE', *, *, #251615, .T. ) ;
#105316 = CARTESIAN_POINT ( 'NONE',  ( -23.25000000000000000, 87.65000000001246860, -173.1231074845242688 ) ) ;
#105318 = CARTESIAN_POINT ( 'NONE',  ( 23.24999999999999645, 76.00000000001165290, -69.52310748452431710 ) ) ;
#105319 = CARTESIAN_POINT ( 'NONE',  ( -23.15000000000000213, 11.43341603104965110, -245.8667934851861787 ) ) ;
#105321 = ORIENTED_EDGE ( 'NONE', *, *, #102232, .T. ) ;
#105320 = CARTESIAN_POINT ( 'NONE',  ( -18.40000000000000213, 70.35000000001201670, -115.6731074845243370 ) ) ;
#105322 = CARTESIAN_POINT ( 'NONE',  ( -18.59999999999999787, 7.021664781911246322, -137.7335654018973514 ) ) ;
#105323 = ORIENTED_EDGE ( 'NONE', *, *, #225918, .T. ) ;
#105324 = CARTESIAN_POINT ( 'NONE',  ( -23.25000000000000000, 68.18350826420393673, -222.4110246041809091 ) ) ;
#105325 = VERTEX_POINT ( 'NONE', #168262 ) ;
#105326 = CARTESIAN_POINT ( 'NONE',  ( 21.30740335185486245, 69.44334207798438285, -170.1220420103002482 ) ) ;
#105328 = ADVANCED_FACE ( 'NONE', ( #229481 ), #129093, .T. ) ;
#105327 = DIRECTION ( 'NONE',  ( 0.000000000000000000, 1.000000000000000000, 6.982962677686266711E-15 ) ) ;
#105329 = EDGE_LOOP ( 'NONE', ( #164684, #167378, #123257, #168692, #253649, #37915, #64545, #166648, #15882, #146623 ) ) ;
#105331 = DIRECTION ( 'NONE',  ( 1.000000000000000000, 0.000000000000000000, 0.000000000000000000 ) ) ;
#105330 = LINE ( 'NONE', #147050, #198775 ) ;
#105332 = EDGE_CURVE ( 'NONE', #197918, #76140, #190367, .T. ) ;
#105333 = AXIS2_PLACEMENT_3D ( 'NONE', #242754, #101943, #199817 ) ;
#105334 = CARTESIAN_POINT ( 'NONE',  ( 20.02499999999999858, 9.749999999999998224, -21.25000000000000000 ) ) ;
#105335 = CARTESIAN_POINT ( 'NONE',  ( -23.25000000000000000, -4.352039508298082282, -236.2331130063498676 ) ) ;
#105336 = ORIENTED_EDGE ( 'NONE', *, *, #181626, .F. ) ;
#105337 = ORIENTED_EDGE ( 'NONE', *, *, #21154, .T. ) ;
#105338 = EDGE_CURVE ( 'NONE', #80723, #125708, #27751, .T. ) ;
#105339 = SPHERICAL_SURFACE ( 'NONE', #246879, 0.1000000000000000056 ) ;
#105341 = ADVANCED_FACE ( 'NONE', ( #250317 ), #69138, .T. ) ;
#105340 = CYLINDRICAL_SURFACE ( 'NONE', #89979, 0.09999999999999438505 ) ;
#105342 = ORIENTED_EDGE ( 'NONE', *, *, #202051, .T. ) ;
#105343 = CARTESIAN_POINT ( 'NONE',  ( -22.39999999999999858, 0.09999999999999939493, 7.790779598373403836 ) ) ;
#105344 = VERTEX_POINT ( 'NONE', #109509 ) ;
#105345 = CARTESIAN_POINT ( 'NONE',  ( -21.64999999999999858, 68.65000000001229807, -157.7731074845244166 ) ) ;
#105346 = SPHERICAL_SURFACE ( 'NONE', #137775, 0.1000000000000000056 ) ;
#105347 = CARTESIAN_POINT ( 'NONE',  ( 19.99999999999998934, 54.53338637621133955, -228.6684279704127789 ) ) ;
#105348 = LINE ( 'NONE', #88367, #149685 ) ;
#105349 = EDGE_LOOP ( 'NONE', ( #152119, #144959, #4543, #257043 ) ) ;
#105350 = AXIS2_PLACEMENT_3D ( 'NONE', #254861, #91993, #232819 ) ;
#105351 = CARTESIAN_POINT ( 'NONE',  ( 18.50000000000000711, -9.421074344976677395, -207.8244720594301498 ) ) ;
#105352 = AXIS2_PLACEMENT_3D ( 'NONE', #225155, #81782, #45260 ) ;
#105353 = ADVANCED_FACE ( 'NONE', ( #230775 ), #194150, .F. ) ;
#105354 = ORIENTED_EDGE ( 'NONE', *, *, #94695, .T. ) ;
#105355 = ORIENTED_EDGE ( 'NONE', *, *, #253681, .T. ) ;
#105356 = EDGE_CURVE ( 'NONE', #150841, #254455, #77319, .T. ) ;
#105357 = ORIENTED_EDGE ( 'NONE', *, *, #157689, .F. ) ;
#105358 = CIRCLE ( 'NONE', #59571, 0.1000000000000124678 ) ;
#105359 = DIRECTION ( 'NONE',  ( 1.000000000000000000, 0.000000000000000000, 0.000000000000000000 ) ) ;
#105360 = DIRECTION ( 'NONE',  ( 0.000000000000000000, 0.000000000000000000, 1.000000000000000000 ) ) ;
#105361 = DIRECTION ( 'NONE',  ( -1.000000000000000000, -0.000000000000000000, -0.000000000000000000 ) ) ;
#105362 = DIRECTION ( 'NONE',  ( 0.000000000000000000, 0.000000000000000000, 1.000000000000000000 ) ) ;
#105363 = CARTESIAN_POINT ( 'NONE',  ( -21.14999999999999858, 11.65000000001115588, -100.6000000000000369 ) ) ;
#105365 = CARTESIAN_POINT ( 'NONE',  ( 21.05000000000000071, 58.88775506787933267, -225.6504858384382999 ) ) ;
#105364 = CARTESIAN_POINT ( 'NONE',  ( 22.32929514600007792, 68.42135243463518179, -69.62218316263829365 ) ) ;
#105367 = ORIENTED_EDGE ( 'NONE', *, *, #182773, .T. ) ;
#105366 = CARTESIAN_POINT ( 'NONE',  ( -16.97683809663752186, 9.950000000011138823, -80.40236401819653622 ) ) ;
#105368 = CARTESIAN_POINT ( 'NONE',  ( -22.49436431346200038, 11.64995094766461392, -100.4330964702777749 ) ) ;
#105369 = VERTEX_POINT ( 'NONE', #169545 ) ;
#105370 = DIRECTION ( 'NONE',  ( 0.000000000000000000, 1.000000000000000000, 0.000000000000000000 ) ) ;
#105371 = ORIENTED_EDGE ( 'NONE', *, *, #32646, .T. ) ;
#105372 = ORIENTED_EDGE ( 'NONE', *, *, #211857, .T. ) ;
#105373 = CARTESIAN_POINT ( 'NONE',  ( 23.14999999999999858, 76.00000000001170974, -69.52310748452431710 ) ) ;
#105375 = AXIS2_PLACEMENT_3D ( 'NONE', #224656, #86408, #50817 ) ;
#105374 = CARTESIAN_POINT ( 'NONE',  ( 23.50000000000005684, 66.40137734081807253, -35.02137779515522453 ) ) ;
#105376 = CARTESIAN_POINT ( 'NONE',  ( 21.13736287352038445, 8.046642376395153562, -176.7499999999999716 ) ) ;
#105377 = VECTOR ( 'NONE', #34773, 1000.000000000000000 ) ;
#105378 = EDGE_CURVE ( 'NONE', #227184, #82680, #123395, .T. ) ;
#105379 = DIRECTION ( 'NONE',  ( -1.000000000000000000, -0.000000000000000000, -0.000000000000000000 ) ) ;
#105380 = AXIS2_PLACEMENT_3D ( 'NONE', #109009, #92023, #152029 ) ;
#105381 = EDGE_CURVE ( 'NONE', #79682, #233201, #198578, .T. ) ;
#105382 = DIRECTION ( 'NONE',  ( 0.000000000000000000, -0.4646089985449268767, -0.8855159391400474478 ) ) ;
#105383 = ORIENTED_EDGE ( 'NONE', *, *, #212524, .T. ) ;
#105384 = EDGE_LOOP ( 'NONE', ( #85281, #28092, #115923, #106324 ) ) ;
#105385 = CIRCLE ( 'NONE', #163687, 0.1000000000000028644 ) ;
#105386 = DIRECTION ( 'NONE',  ( -0.000000000000000000, -0.9126074666063771490, -0.4088369013363281623 ) ) ;
#105387 = ORIENTED_EDGE ( 'NONE', *, *, #176478, .T. ) ;
#105388 = FACE_OUTER_BOUND ( 'NONE', #199054, .T. ) ;
#105389 = CARTESIAN_POINT ( 'NONE',  ( 23.14999999999999503, 19.68370618165487329, -225.3554403480446240 ) ) ;
#105390 = DIRECTION ( 'NONE',  ( 1.000000000000000000, 0.000000000000000000, 0.000000000000000000 ) ) ;
#105391 = CARTESIAN_POINT ( 'NONE',  ( -16.95709691156408283, 66.05000000001209060, -123.8630499220137864 ) ) ;
#105393 = EDGE_CURVE ( 'NONE', #192091, #61013, #153839, .T. ) ;
#105392 = CARTESIAN_POINT ( 'NONE',  ( 22.16821283564876666, 7.558973340791918183, -67.00000000000004263 ) ) ;
#105394 = ORIENTED_EDGE ( 'NONE', *, *, #198640, .F. ) ;
#105395 = DIRECTION ( 'NONE',  ( 0.000000000000000000, -6.982962677686266711E-15, 1.000000000000000000 ) ) ;
#105397 = CARTESIAN_POINT ( 'NONE',  ( 18.59999999999999432, 68.68284540823283635, -224.2482512540334767 ) ) ;
#105396 = CIRCLE ( 'NONE', #176189, 0.09999999999999939493 ) ;
#105399 = DIRECTION ( 'NONE',  ( -1.000000000000000000, 0.000000000000000000, 0.000000000000000000 ) ) ;
#105398 = AXIS2_PLACEMENT_3D ( 'NONE', #253027, #233495, #216468 ) ;
#105400 = EDGE_CURVE ( 'NONE', #66849, #212706, #15250, .T. ) ;
#105401 = AXIS2_PLACEMENT_3D ( 'NONE', #73737, #236623, #174142 ) ;
#105402 = DIRECTION ( 'NONE',  ( 1.000000000000000000, -7.136802563874198121E-16, -1.554319503706931717E-16 ) ) ;
#105403 = DIRECTION ( 'NONE',  ( 0.000000000000000000, 1.000000000000000000, 0.000000000000000000 ) ) ;
#105404 = EDGE_CURVE ( 'NONE', #184335, #99738, #119479, .T. ) ;
#105405 = DIRECTION ( 'NONE',  ( 0.000000000000000000, 0.000000000000000000, 1.000000000000000000 ) ) ;
#105406 = ORIENTED_EDGE ( 'NONE', *, *, #113828, .F. ) ;
#105407 = CARTESIAN_POINT ( 'NONE',  ( 23.24999999999999645, 66.37271706025207152, -233.9386508266050839 ) ) ;
#105408 = ORIENTED_EDGE ( 'NONE', *, *, #249567, .F. ) ;
#105409 = ADVANCED_FACE ( 'NONE', ( #15588 ), #215157, .T. ) ;
#105410 = DIRECTION ( 'NONE',  ( 1.000000000000000000, -1.335000415235278971E-16, 2.979993593738921214E-16 ) ) ;
#105411 = DIRECTION ( 'NONE',  ( -1.000000000000000000, 0.000000000000000000, 0.000000000000000000 ) ) ;
#105412 = EDGE_LOOP ( 'NONE', ( #12883, #15322, #41748 ) ) ;
#105413 = EDGE_CURVE ( 'NONE', #230514, #43496, #206782, .T. ) ;
#105414 = AXIS2_PLACEMENT_3D ( 'NONE', #240227, #215507, #235087 ) ;
#105415 = LINE ( 'NONE', #184996, #156591 ) ;
#105416 = FILL_AREA_STYLE_COLOUR ( '', #56367 ) ;
#105418 = TOROIDAL_SURFACE ( 'NONE', #201127, 7.800000000000000711, 0.1000000000000000056 ) ;
#105417 = CARTESIAN_POINT ( 'NONE',  ( 22.60000000000000142, 67.23127455305841238, -235.8551265064783991 ) ) ;
#105419 = CARTESIAN_POINT ( 'NONE',  ( -20.85000000000000142, 65.66751761918720831, -164.4282609406112670 ) ) ;
#105420 = CARTESIAN_POINT ( 'NONE',  ( -18.50000000000000000, 16.02417409648692725, -219.3605785455116006 ) ) ;
#105421 = ORIENTED_EDGE ( 'NONE', *, *, #202651, .T. ) ;
#105422 = VERTEX_POINT ( 'NONE', #158947 ) ;
#105423 = DIRECTION ( 'NONE',  ( -1.000000000000000000, 0.000000000000000000, -0.000000000000000000 ) ) ;
#105425 = VERTEX_POINT ( 'NONE', #213755 ) ;
#105424 = DIRECTION ( 'NONE',  ( -1.000000000000000000, 2.849773892568378313E-16, -7.728835255496647986E-17 ) ) ;
#105426 = CIRCLE ( 'NONE', #134664, 0.09999999999999967248 ) ;
#105427 = LINE ( 'NONE', #65054, #130029 ) ;
#105428 = AXIS2_PLACEMENT_3D ( 'NONE', #142537, #222052, #123002 ) ;
#105429 = CARTESIAN_POINT ( 'NONE',  ( 20.94999999999999929, -8.999999999988842703, -191.1060308773475072 ) ) ;
#105430 = VERTEX_POINT ( 'NONE', #135484 ) ;
#105431 = DIRECTION ( 'NONE',  ( -1.000000000000000000, -0.000000000000000000, -0.000000000000000000 ) ) ;
#105432 = AXIS2_PLACEMENT_3D ( 'NONE', #70537, #71805, #49653 ) ;
#105433 = ITEM_DEFINED_TRANSFORMATION ( 'NONE', 'NONE', #115215,  #2425 ) ;
#105435 = AXIS2_PLACEMENT_3D ( 'NONE', #51377, #189649, #11006 ) ;
#105434 = CARTESIAN_POINT ( 'NONE',  ( -18.50000000000000000, 11.75000000001115197, -88.75000000000004263 ) ) ;
#105436 = ORIENTED_EDGE ( 'NONE', *, *, #71200, .F. ) ;
#105437 = AXIS2_PLACEMENT_3D ( 'NONE', #91864, #102734, #227515 ) ;
#105438 = DIRECTION ( 'NONE',  ( 0.000000000000000000, 6.982962677686266711E-15, -1.000000000000000000 ) ) ;
#105439 = CIRCLE ( 'NONE', #9607, 0.1000000000000066946 ) ;
#105440 = PRODUCT_DEFINITION_SHAPE ( 'NONE', 'NONE',  #86666 ) ;
#105441 = B_SPLINE_CURVE_WITH_KNOTS ( 'NONE', 3,
 ( #83596, #61512, #78482, #163185, #242699, #64068, #216721, #141052, #178922, #220585, #38105, #117627, #197151, #198442, #18529, #158088, #79754, #159343, #87470 ),
 .UNSPECIFIED., .F., .F.,
 ( 4, 3, 3, 3, 3, 3, 4 ),
 ( 0.000000000000000000, 2.646747978908423797E-05, 5.271166642128778001E-05, 9.008788829884103923E-05, 0.0001426648776561041253, 0.0001897378458659842060, 0.0001917382627806401836 ),
 .UNSPECIFIED. ) ;
#105442 = VECTOR ( 'NONE', #196046, 1000.000000000000114 ) ;
#105443 = ORIENTED_EDGE ( 'NONE', *, *, #249582, .F. ) ;
#105444 = VERTEX_POINT ( 'NONE', #76807 ) ;
#105445 = DIRECTION ( 'NONE',  ( 1.000000000000000000, 0.000000000000000000, 0.000000000000000000 ) ) ;
#105446 = CARTESIAN_POINT ( 'NONE',  ( 16.27683809663750125, 9.350000000011137402, -76.25000000000004263 ) ) ;
#105448 = AXIS2_PLACEMENT_3D ( 'NONE', #182752, #110900, #190464 ) ;
#105447 = DIRECTION ( 'NONE',  ( -1.000000000000000000, 0.000000000000000000, 0.000000000000000000 ) ) ;
#105450 = AXIS2_PLACEMENT_3D ( 'NONE', #86930, #46529, #145632 ) ;
#105449 = LINE ( 'NONE', #67641, #194740 ) ;
#105451 = DIRECTION ( 'NONE',  ( 1.000000000000000000, 0.000000000000000000, 0.000000000000000000 ) ) ;
#105452 = FACE_OUTER_BOUND ( 'NONE', #25945, .T. ) ;
#105453 = CARTESIAN_POINT ( 'NONE',  ( -16.93339986808596720, 10.00510392856591757, -12.56599367181285487 ) ) ;
#105455 = DIRECTION ( 'NONE',  ( 0.000000000000000000, 0.000000000000000000, -1.000000000000000000 ) ) ;
#105454 = CARTESIAN_POINT ( 'NONE',  ( 21.05000000000000071, 76.00000000001267608, -203.5231074845243597 ) ) ;
#105456 = AXIS2_PLACEMENT_3D ( 'NONE', #197020, #236162, #234895 ) ;
#105457 = CARTESIAN_POINT ( 'NONE',  ( -16.89060415895971090, 9.951220762813354881, -113.1459202242704976 ) ) ;
#105458 = CARTESIAN_POINT ( 'NONE',  ( -18.39999999999999858, 85.60000000001187459, -96.42291809330220076 ) ) ;
#105459 = LINE ( 'NONE', #226717, #186294 ) ;
#105460 = VERTEX_POINT ( 'NONE', #173403 ) ;
#105461 = VERTEX_POINT ( 'NONE', #74284 ) ;
#105462 = CARTESIAN_POINT ( 'NONE',  ( 18.60000000000000142, 47.16152503674116758, -255.1462838189583238 ) ) ;
#105463 = AXIS2_PLACEMENT_3D ( 'NONE', #24518, #244812, #87005 ) ;
#105464 = LINE ( 'NONE', #84607, #166118 ) ;
#105466 = CARTESIAN_POINT ( 'NONE',  ( -12.33960340485503515, 12.83090422469975778, -215.9260128953783067 ) ) ;
#105465 = CARTESIAN_POINT ( 'NONE',  ( -18.40000000000000213, 70.35000000001187459, -90.37310748452433984 ) ) ;
#105467 = AXIS2_PLACEMENT_3D ( 'NONE', #27603, #252685, #246603 ) ;
#105468 = VECTOR ( 'NONE', #130940, 1000.000000000000000 ) ;
#105469 = AXIS2_PLACEMENT_3D ( 'NONE', #127291, #141708, #23081 ) ;
#105470 = DIRECTION ( 'NONE',  ( -0.000000000000000000, 0.000000000000000000, 1.000000000000000000 ) ) ;
#105471 = FACE_OUTER_BOUND ( 'NONE', #234592, .T. ) ;
#105473 = ADVANCED_FACE ( 'NONE', ( #75559 ), #160996, .T. ) ;
#105472 = DIRECTION ( 'NONE',  ( 1.186688945009009831E-16, -0.4721928772777346239, -0.8814952561688430555 ) ) ;
#105474 = ORIENTED_EDGE ( 'NONE', *, *, #208437, .F. ) ;
#105475 = ORIENTED_EDGE ( 'NONE', *, *, #95632, .F. ) ;
#105476 = ADVANCED_FACE ( 'NONE', ( #115952 ), #134206, .F. ) ;
#105477 = EDGE_CURVE ( 'NONE', #18436, #98928, #79361, .T. ) ;
#105478 = CARTESIAN_POINT ( 'NONE',  ( -12.42749937872396515, 9.370689921602609829, -17.52646512666106204 ) ) ;
#105479 = ORIENTED_EDGE ( 'NONE', *, *, #147841, .T. ) ;
#105480 = CARTESIAN_POINT ( 'NONE',  ( 20.94999999999999574, 87.75000000001210765, -133.6231074845242119 ) ) ;
#105481 = AXIS2_PLACEMENT_3D ( 'NONE', #211766, #111373, #162698 ) ;
#105482 = AXIS2_PLACEMENT_3D ( 'NONE', #39836, #119354, #61946 ) ;
#105483 = CIRCLE ( 'NONE', #172212, 7.899999999999995914 ) ;
#105484 = AXIS2_PLACEMENT_3D ( 'NONE', #219816, #114302, #37353 ) ;
#105485 = CARTESIAN_POINT ( 'NONE',  ( 18.50000000000000355, 85.40000000001137437, -29.14106563635156988 ) ) ;
#105486 = ORIENTED_EDGE ( 'NONE', *, *, #61995, .T. ) ;
#105487 = DIRECTION ( 'NONE',  ( 0.000000000000000000, 0.7965107556683636014, -0.6046243595031649543 ) ) ;
#105488 = EDGE_CURVE ( 'NONE', #161116, #113073, #27931, .T. ) ;
#105489 = EDGE_LOOP ( 'NONE', ( #105653, #37376, #254147, #218491 ) ) ;
#105490 = CARTESIAN_POINT ( 'NONE',  ( 20.94999999999999929, 76.00000000001145395, -40.02310748452431710 ) ) ;
#105491 = CARTESIAN_POINT ( 'NONE',  ( -21.59142135623730852, 29.47917209469435207, -236.7998429059379362 ) ) ;
#105492 = DIRECTION ( 'NONE',  ( -0.000000000000000000, -0.2617529984165031243, -0.9651348961777157509 ) ) ;
#105493 = CARTESIAN_POINT ( 'NONE',  ( 18.49999999999998579, -9.321008403350155902, -141.2359382490778899 ) ) ;
#105494 = DIRECTION ( 'NONE',  ( 0.000000000000000000, -0.1350103645451876666, 0.9908441862701600211 ) ) ;
#105495 = FACE_OUTER_BOUND ( 'NONE', #205793, .T. ) ;
#105496 = DIRECTION ( 'NONE',  ( 0.000000000000000000, -7.272083257015735086E-15, 1.000000000000000000 ) ) ;
#105497 = DIRECTION ( 'NONE',  ( 0.000000000000000000, -0.8660254037844247188, 0.5000000000000245359 ) ) ;
#105499 = ORIENTED_EDGE ( 'NONE', *, *, #247698, .F. ) ;
#105498 = CARTESIAN_POINT ( 'NONE',  ( -20.94999999999999929, 36.65892442174472876, -249.5511627012454596 ) ) ;
#105501 = CARTESIAN_POINT ( 'NONE',  ( -20.65000000000000568, 68.75000000001182343, -82.17310748452436542 ) ) ;
#105500 = CARTESIAN_POINT ( 'NONE',  ( -16.79363873026997922, 66.05114977059356818, -115.6769537030788939 ) ) ;
#105502 = ORIENTED_EDGE ( 'NONE', *, *, #178945, .T. ) ;
#105504 = ORIENTED_EDGE ( 'NONE', *, *, #115526, .T. ) ;
#105503 = CARTESIAN_POINT ( 'NONE',  ( 18.59999999999999076, 69.55000000001150795, -48.27310748452436684 ) ) ;
#105505 = ORIENTED_EDGE ( 'NONE', *, *, #191605, .T. ) ;
#105506 = CARTESIAN_POINT ( 'NONE',  ( 19.92426406871192412, 11.75000000001116085, -91.85000000000003695 ) ) ;
#105507 = DIRECTION ( 'NONE',  ( -0.000000000000000000, 0.000000000000000000, -1.000000000000000000 ) ) ;
#105508 = CIRCLE ( 'NONE', #180561, 0.09999999999999939493 ) ;
#105509 = EDGE_CURVE ( 'NONE', #109568, #84452, #240111, .T. ) ;
#105511 = ADVANCED_FACE ( 'NONE', ( #257966 ), #138053, .F. ) ;
#105510 = CARTESIAN_POINT ( 'NONE',  ( -18.50000000000000000, -1.164121893241208960, -41.21484808557161017 ) ) ;
#105512 = CARTESIAN_POINT ( 'NONE',  ( 20.12500000000000000, 66.25000000001209344, -128.4113362024100979 ) ) ;
#105513 = CARTESIAN_POINT ( 'NONE',  ( 21.05000000000000071, -11.48912529306490349, -103.4000000000000341 ) ) ;
#105514 = ORIENTED_EDGE ( 'NONE', *, *, #212514, .F. ) ;
#105515 = DIRECTION ( 'NONE',  ( 0.000000000000000000, -0.2128009952263604232, 0.9770955615653316162 ) ) ;
#105516 = EDGE_CURVE ( 'NONE', #15766, #160550, #89792, .T. ) ;
#105517 = FACE_OUTER_BOUND ( 'NONE', #241201, .T. ) ;
#105518 = VERTEX_POINT ( 'NONE', #24565 ) ;
#105519 = VERTEX_POINT ( 'NONE', #108882 ) ;
#105520 = DIRECTION ( 'NONE',  ( 0.000000000000000000, -1.000000000000000000, -6.352154140967427193E-15 ) ) ;
#105521 = AXIS2_PLACEMENT_3D ( 'NONE', #172664, #228751, #252137 ) ;
#105522 = AXIS2_PLACEMENT_3D ( 'NONE', #172267, #187941, #206214 ) ;
#105523 = ORIENTED_EDGE ( 'NONE', *, *, #242813, .F. ) ;
#105524 = CARTESIAN_POINT ( 'NONE',  ( -20.94999999999999929, 1.115650877919449575E-11, -205.0999999999999375 ) ) ;
#105525 = ORIENTED_EDGE ( 'NONE', *, *, #185533, .F. ) ;
#105526 = CARTESIAN_POINT ( 'NONE',  ( 18.39999999999999503, 11.75000000001113953, -154.8500000000000227 ) ) ;
#105527 = AXIS2_PLACEMENT_3D ( 'NONE', #56306, #154189, #14655 ) ;
#105528 = DIRECTION ( 'NONE',  ( 0.000000000000000000, -6.997203936713175802E-15, 1.000000000000000000 ) ) ;
#105529 = DIRECTION ( 'NONE',  ( 1.000000000000000000, -0.000000000000000000, 0.000000000000000000 ) ) ;
#105530 = CARTESIAN_POINT ( 'NONE',  ( 20.04142135623730070, 64.25000000001277556, -215.2731074845244450 ) ) ;
#105531 = DIRECTION ( 'NONE',  ( -1.000000000000000000, 0.000000000000000000, 0.000000000000000000 ) ) ;
#105532 = VERTEX_POINT ( 'NONE', #1098 ) ;
#105533 = EDGE_CURVE ( 'NONE', #179633, #58353, #245475, .T. ) ;
#105534 = CARTESIAN_POINT ( 'NONE',  ( -18.59999999999999787, 7.021664781911246322, -171.1335654018973003 ) ) ;
#105536 = AXIS2_PLACEMENT_3D ( 'NONE', #195957, #216775, #99377 ) ;
#105535 = CARTESIAN_POINT ( 'NONE',  ( 21.14999999999999858, 11.65000000001116298, -21.75000000000000355 ) ) ;
#105537 = CARTESIAN_POINT ( 'NONE',  ( -16.87683809663752399, 9.850000000011140955, -146.6500000000000341 ) ) ;
#105538 = PLANE ( 'NONE',  #68411 ) ;
#105539 = VERTEX_POINT ( 'NONE', #188416 ) ;
#105541 = CARTESIAN_POINT ( 'NONE',  ( -20.64999999999999858, 76.00000000001141132, -34.12310748452431852 ) ) ;
#105540 = CARTESIAN_POINT ( 'NONE',  ( -21.05000000000000071, 28.60154115857408641, -258.4512230915049713 ) ) ;
#105542 = ORIENTED_EDGE ( 'NONE', *, *, #122478, .T. ) ;
#105544 = ORIENTED_EDGE ( 'NONE', *, *, #243166, .T. ) ;
#105543 = FACE_OUTER_BOUND ( 'NONE', #224466, .T. ) ;
#105545 = VERTEX_POINT ( 'NONE', #139331 ) ;
#105546 = DIRECTION ( 'NONE',  ( 0.000000000000000000, 0.000000000000000000, -1.000000000000000000 ) ) ;
#105547 = CIRCLE ( 'NONE', #131088, 2.000000000000002665 ) ;
#105549 = FACE_OUTER_BOUND ( 'NONE', #127530, .T. ) ;
#105548 = VECTOR ( 'NONE', #136713, 1000.000000000000000 ) ;
#105550 = EDGE_CURVE ( 'NONE', #245381, #21468, #77751, .T. ) ;
#105551 = FACE_OUTER_BOUND ( 'NONE', #115255, .T. ) ;
#105552 = ORIENTED_EDGE ( 'NONE', *, *, #39357, .F. ) ;
#105553 = CARTESIAN_POINT ( 'NONE',  ( -23.25000000000000355, 50.88295650978584206, -230.3037755757580953 ) ) ;
#105554 = DIRECTION ( 'NONE',  ( 0.000000000000000000, 0.000000000000000000, 1.000000000000000000 ) ) ;
#105555 = EDGE_CURVE ( 'NONE', #45677, #27613, #119814, .T. ) ;
#105557 = DIRECTION ( 'NONE',  ( 0.000000000000000000, 6.982962677686266711E-15, -1.000000000000000000 ) ) ;
#105556 = DIRECTION ( 'NONE',  ( 0.000000000000000000, 0.000000000000000000, 1.000000000000000000 ) ) ;
#105558 = EDGE_CURVE ( 'NONE', #84692, #53603, #148018, .T. ) ;
#105560 = EDGE_LOOP ( 'NONE', ( #25264, #49733, #141464, #184084 ) ) ;
#105559 = CARTESIAN_POINT ( 'NONE',  ( -18.39999999999999858, 46.91436717984746707, -255.3877622108296634 ) ) ;
#105561 = VECTOR ( 'NONE', #16562, 1000.000000000000000 ) ;
#105562 = AXIS2_PLACEMENT_3D ( 'NONE', #219480, #142508, #61707 ) ;
#105563 = AXIS2_PLACEMENT_3D ( 'NONE', #257170, #158175, #16081 ) ;
#105564 = VERTEX_POINT ( 'NONE', #227544 ) ;
#105565 = CARTESIAN_POINT ( 'NONE',  ( -16.88560720703333473, 9.950564843760847822, -79.64811192086376934 ) ) ;
#105566 = DIRECTION ( 'NONE',  ( 0.000000000000000000, 0.2128009952263693327, -0.9770955615653295068 ) ) ;
#105567 = EDGE_CURVE ( 'NONE', #136660, #224829, #187162, .T. ) ;
#105568 = CARTESIAN_POINT ( 'NONE',  ( 20.85000000000000142, 77.13501884592227498, -128.8061306010920362 ) ) ;
#105570 = EDGE_CURVE ( 'NONE', #244761, #56847, #69427, .T. ) ;
#105569 = ORIENTED_EDGE ( 'NONE', *, *, #13775, .T. ) ;
#105571 = CARTESIAN_POINT ( 'NONE',  ( -18.40000000000000213, 11.75000000001113953, -146.6500000000000341 ) ) ;
#105572 = ORIENTED_EDGE ( 'NONE', *, *, #91490, .F. ) ;
#105574 = CIRCLE ( 'NONE', #122178, 0.1000000000000089567 ) ;
#105573 = DIRECTION ( 'NONE',  ( 0.000000000000000000, -6.982962677686266711E-15, 1.000000000000000000 ) ) ;
#105575 = CARTESIAN_POINT ( 'NONE',  ( -22.48660254037843487, 64.35000000001238618, -170.0731074845244279 ) ) ;
#105576 = CARTESIAN_POINT ( 'NONE',  ( 22.47071067811865319, 7.720074744509197728, -33.40090754529740025 ) ) ;
#105577 = EDGE_CURVE ( 'NONE', #70387, #222885, #19539, .T. ) ;
#105578 = ORIENTED_EDGE ( 'NONE', *, *, #42026, .T. ) ;
#105579 = CARTESIAN_POINT ( 'NONE',  ( -21.14999999999999858, 75.90220970870363715, -176.2809220950004487 ) ) ;
#105580 = VECTOR ( 'NONE', #2639, 1000.000000000000000 ) ;
#105581 = CIRCLE ( 'NONE', #118078, 0.1000000000000028644 ) ;
#105582 = CIRCLE ( 'NONE', #93134, 0.1000000000000013933 ) ;
#105583 = EDGE_CURVE ( 'NONE', #221732, #207854, #94517, .T. ) ;
#105584 = ORIENTED_EDGE ( 'NONE', *, *, #108329, .F. ) ;
#105585 = CARTESIAN_POINT ( 'NONE',  ( -22.50000000000000000, 11.65000000001115588, -33.50000000000000000 ) ) ;
#105586 = EDGE_CURVE ( 'NONE', #24834, #3363, #202673, .T. ) ;
#105587 = ADVANCED_FACE ( 'NONE', ( #168907 ), #101459, .F. ) ;
#105588 = VERTEX_POINT ( 'NONE', #141911 ) ;
#105589 = VERTEX_POINT ( 'NONE', #221430 ) ;
#105590 = ORIENTED_EDGE ( 'NONE', *, *, #12381, .T. ) ;
#105591 = ADVANCED_FACE ( 'NONE', ( #42826 ), #122366, .T. ) ;
#105592 = DIRECTION ( 'NONE',  ( 1.000000000000000000, 0.000000000000000000, 0.000000000000000000 ) ) ;
#105593 = ORIENTED_EDGE ( 'NONE', *, *, #229562, .F. ) ;
#105595 = ORIENTED_EDGE ( 'NONE', *, *, #230732, .T. ) ;
#105594 = CARTESIAN_POINT ( 'NONE',  ( -22.47071067811865319, 7.720074744498064412, 0.09909245470260744093 ) ) ;
#105597 = ADVANCED_FACE ( 'NONE', ( #83196 ), #150590, .F. ) ;
#105596 = ORIENTED_EDGE ( 'NONE', *, *, #207818, .T. ) ;
#105598 = ADVANCED_FACE ( 'NONE', ( #209264, #51447 ), #52750, .T. ) ;
#105600 = ORIENTED_EDGE ( 'NONE', *, *, #185221, .T. ) ;
#105599 = ORIENTED_EDGE ( 'NONE', *, *, #204267, .T. ) ;
#105601 = AXIS2_PLACEMENT_3D ( 'NONE', #235403, #230270, #155906 ) ;
#105602 = ADVANCED_FACE ( 'NONE', ( #16234 ), #94452, .F. ) ;
#105603 = CIRCLE ( 'NONE', #234636, 0.2000000000000005107 ) ;
#105604 = CARTESIAN_POINT ( 'NONE',  ( -18.44232395689904536, -9.552282557039346145, -107.3422519848068362 ) ) ;
#105605 = ORIENTED_EDGE ( 'NONE', *, *, #55155, .F. ) ;
#105606 = LINE ( 'NONE', #69095, #110575 ) ;
#105607 = AXIS2_PLACEMENT_3D ( 'NONE', #191519, #207217, #225455 ) ;
#105608 = PLANE ( 'NONE',  #17997 ) ;
#105609 = CARTESIAN_POINT ( 'NONE',  ( -18.31331870001021400, 87.00168188095352662, -199.3901562392411506 ) ) ;
#105610 = ORIENTED_EDGE ( 'NONE', *, *, #152861, .T. ) ;
#105612 = ORIENTED_EDGE ( 'NONE', *, *, #226241, .F. ) ;
#105611 = AXIS2_PLACEMENT_3D ( 'NONE', #206270, #204962, #22517 ) ;
#105613 = DIRECTION ( 'NONE',  ( -1.020425574104004196E-15, -6.982962677686266711E-15, 1.000000000000000000 ) ) ;
#105614 = CIRCLE ( 'NONE', #84757, 0.09999999999999843736 ) ;
#105616 = ORIENTED_EDGE ( 'NONE', *, *, #16963, .F. ) ;
#105615 = CARTESIAN_POINT ( 'NONE',  ( -16.93353400591626112, 65.99538760383960323, -182.5904230143190148 ) ) ;
#105617 = CARTESIAN_POINT ( 'NONE',  ( -16.81744102076749314, 9.950000000011142376, -180.1499999999999773 ) ) ;
#105619 = ORIENTED_EDGE ( 'NONE', *, *, #65457, .F. ) ;
#105618 = CARTESIAN_POINT ( 'NONE',  ( -18.59999999999999787, 14.86477715130881272, -235.7932433709592601 ) ) ;
#105620 = ADVANCED_FACE ( 'NONE', ( #74927 ), #30658, .T. ) ;
#105621 = ORIENTED_EDGE ( 'NONE', *, *, #197809, .T. ) ;
#105622 = DIRECTION ( 'NONE',  ( 0.000000000000000000, -7.086529944415894657E-15, 1.000000000000000000 ) ) ;
#105623 = AXIS2_PLACEMENT_3D ( 'NONE', #168058, #207153, #67625 ) ;
#105624 = AXIS2_PLACEMENT_3D ( 'NONE', #138622, #42145, #99501 ) ;
#105626 = ORIENTED_EDGE ( 'NONE', *, *, #167753, .F. ) ;
#105625 = AXIS2_PLACEMENT_3D ( 'NONE', #75523, #76775, #15555 ) ;
#105627 = ORIENTED_EDGE ( 'NONE', *, *, #32660, .T. ) ;
#105628 = CIRCLE ( 'NONE', #101322, 0.09999999999999939493 ) ;
#105629 = DIRECTION ( 'NONE',  ( 0.000000000000000000, 0.000000000000000000, -1.000000000000000000 ) ) ;
#105630 = CARTESIAN_POINT ( 'NONE',  ( -23.15000000000000213, 11.65000000001115588, -88.25000000000005684 ) ) ;
#105631 = CIRCLE ( 'NONE', #197411, 0.09999999999999939493 ) ;
#105633 = ORIENTED_EDGE ( 'NONE', *, *, #169322, .T. ) ;
#105632 = VERTEX_POINT ( 'NONE', #171468 ) ;
#105634 = ORIENTED_EDGE ( 'NONE', *, *, #83131, .F. ) ;
#105635 = CARTESIAN_POINT ( 'NONE',  ( -22.60000000000094289, 64.05844819680055480, -247.1686437718134925 ) ) ;
#105636 = EDGE_LOOP ( 'NONE', ( #139241, #201463 ) ) ;
#105637 = VERTEX_POINT ( 'NONE', #175314 ) ;
#105638 = CARTESIAN_POINT ( 'NONE',  ( -23.15000000000000213, 17.15380675273576472, -224.5473919504296703 ) ) ;
#105640 = ORIENTED_EDGE ( 'NONE', *, *, #216804, .T. ) ;
#105639 = DIRECTION ( 'NONE',  ( 0.000000000000000000, -0.9876197685951263461, 0.1568667991644794590 ) ) ;
#105641 = CARTESIAN_POINT ( 'NONE',  ( -18.59999999999999787, 0.6713328740235187109, -212.7808875799876205 ) ) ;
#105642 = CIRCLE ( 'NONE', #168260, 11.64999999999999325 ) ;
#105644 = CARTESIAN_POINT ( 'NONE',  ( 18.45036689428353682, -9.490184143317748067, -107.5126958274858708 ) ) ;
#105643 = CARTESIAN_POINT ( 'NONE',  ( 19.97071067811864609, 11.72071067812981404, -192.1499999999999488 ) ) ;
#105645 = DIRECTION ( 'NONE',  ( 0.000000000000000000, -6.853228547068871147E-15, 1.000000000000000000 ) ) ;
#105646 = CARTESIAN_POINT ( 'NONE',  ( -12.25000000000000711, 62.53104822794669815, -217.4650886355768762 ) ) ;
#105647 = ORIENTED_EDGE ( 'NONE', *, *, #25293, .T. ) ;
#105648 = ORIENTED_EDGE ( 'NONE', *, *, #154816, .F. ) ;
#105649 = CIRCLE ( 'NONE', #76629, 0.1000000000000028644 ) ;
#105650 = DIRECTION ( 'NONE',  ( -0.000000000000000000, 0.8660254037844411501, 0.4999999999999956701 ) ) ;
#105652 = ADVANCED_FACE ( 'NONE', ( #35794 ), #233964, .F. ) ;
#105651 = FACE_OUTER_BOUND ( 'NONE', #38620, .T. ) ;
#105653 = ORIENTED_EDGE ( 'NONE', *, *, #138895, .T. ) ;
#105654 = EDGE_CURVE ( 'NONE', #230044, #19091, #98573, .T. ) ;
#105655 = AXIS2_PLACEMENT_3D ( 'NONE', #241943, #215950, #85402 ) ;
#105656 = AXIS2_PLACEMENT_3D ( 'NONE', #81212, #121673, #224590 ) ;
#105657 = AXIS2_PLACEMENT_3D ( 'NONE', #196239, #215791, #60573 ) ;
#105658 = FACE_BOUND ( 'NONE', #149716, .T. ) ;
#105659 = ORIENTED_EDGE ( 'NONE', *, *, #250406, .F. ) ;
#105660 = ORIENTED_EDGE ( 'NONE', *, *, #201216, .T. ) ;
#105661 = EDGE_CURVE ( 'NONE', #55259, #109463, #81834, .T. ) ;
#105662 = CARTESIAN_POINT ( 'NONE',  ( -21.52071067811865746, 7.779289321892505882, -88.15000000000004832 ) ) ;
#105663 = EDGE_CURVE ( 'NONE', #61430, #74964, #210560, .T. ) ;
#105664 = ORIENTED_EDGE ( 'NONE', *, *, #43516, .T. ) ;
#105665 = CARTESIAN_POINT ( 'NONE',  ( 21.13920837816993270, 8.783247050131068434, -112.7500000000000284 ) ) ;
#105666 = ORIENTED_EDGE ( 'NONE', *, *, #128335, .F. ) ;
#105667 = CYLINDRICAL_SURFACE ( 'NONE', #243787, 11.80000000000000782 ) ;
#105668 = FACE_OUTER_BOUND ( 'NONE', #177837, .T. ) ;
#105670 = DIRECTION ( 'NONE',  ( 0.000000000000000000, -0.9651348961777157509, 0.2617529984165031243 ) ) ;
#105669 = LINE ( 'NONE', #125268, #148780 ) ;
#105671 = CARTESIAN_POINT ( 'NONE',  ( -20.85000000000000142, -1.362429037182151470, -141.8888812479212334 ) ) ;
#105672 = DIRECTION ( 'NONE',  ( 0.000000000000000000, -0.9126074666064696306, -0.4088369013361213278 ) ) ;
#105673 = AXIS2_PLACEMENT_3D ( 'NONE', #9390, #10690, #129344 ) ;
#105674 = ORIENTED_EDGE ( 'NONE', *, *, #160345, .T. ) ;
#105675 = CIRCLE ( 'NONE', #84821, 11.79999999999999005 ) ;
#105676 = CIRCLE ( 'NONE', #97475, 2.099999999999990763 ) ;
#105678 = VERTEX_POINT ( 'NONE', #95724 ) ;
#105677 = ORIENTED_EDGE ( 'NONE', *, *, #37064, .F. ) ;
#105679 = ORIENTED_EDGE ( 'NONE', *, *, #120220, .T. ) ;
#105680 = DIRECTION ( 'NONE',  ( -0.000000000000000000, -0.000000000000000000, 1.000000000000000000 ) ) ;
#105681 =( BOUNDED_SURFACE ( )  B_SPLINE_SURFACE ( 3, 2, ( 
 ( #90654, #209321, #170259 ),
 ( #153248, #30727, #110222 ),
 ( #213173, #32003, #73702 ),
 ( #249745, #71128, #111519 ),
 ( #230174, #232763, #54100 ),
 ( #133644, #15001, #247161 ) ),
 .UNSPECIFIED., .F., .F., .F. ) 
 B_SPLINE_SURFACE_WITH_KNOTS ( ( 4, 2, 4 ),
 ( 3, 3 ),
 ( 3.141592653589793116, 3.926990816987241395, 4.712388980384689674 ),
 ( 0.000000000000000000, 1.000000000000000000 ),
 .UNSPECIFIED. ) 
 GEOMETRIC_REPRESENTATION_ITEM ( )  RATIONAL_B_SPLINE_SURFACE ( (
 ( 1.000000000000000000, 0.9238795325112820755, 1.000000000000000000),
 ( 1.000000000000000000, 0.9240297172244890112, 1.000000000000000000),
 ( 1.000000000000000000, 0.9038128468037535113, 1.000000000000000000),
 ( 1.000000000000000000, 0.8282379607651170206, 1.000000000000000000),
 ( 1.000000000000000000, 0.7727932973490044821, 1.000000000000000000),
 ( 1.000000000000000000, 0.7071067811865352493, 1.000000000000000000) ) ) 
 REPRESENTATION_ITEM ( '' )  SURFACE ( )  );
#105682 = CARTESIAN_POINT ( 'NONE',  ( -20.64999999999999858, 2.000000000011154189, -154.7753780772379173 ) ) ;
#105684 = CARTESIAN_POINT ( 'NONE',  ( 20.99142135623731065, 11.60000000001116049, -194.0717967697245001 ) ) ;
#105683 = DIRECTION ( 'NONE',  ( 0.000000000000000000, 0.000000000000000000, 1.000000000000000000 ) ) ;
#105685 = CARTESIAN_POINT ( 'NONE',  ( -21.11101077989000530, 75.98471473109790963, -142.9467922192504261 ) ) ;
#105686 = ORIENTED_EDGE ( 'NONE', *, *, #178003, .F. ) ;
#105687 = FACE_OUTER_BOUND ( 'NONE', #144046, .T. ) ;
#105688 = DIRECTION ( 'NONE',  ( -0.000000000000000000, 0.9126074666063770380, 0.4088369013363281068 ) ) ;
#105689 = CARTESIAN_POINT ( 'NONE',  ( -21.05000000000000071, 1.115600667400684642E-11, -100.5000000000000284 ) ) ;
#105690 = CARTESIAN_POINT ( 'NONE',  ( -16.93301857435212909, 9.976309354746613067, -87.88577557116147432 ) ) ;
#105691 = ORIENTED_EDGE ( 'NONE', *, *, #114198, .F. ) ;
#105692 = EDGE_CURVE ( 'NONE', #202111, #129010, #110162, .T. ) ;
#105693 = CARTESIAN_POINT ( 'NONE',  ( 18.42555734704283310, -9.497158361936710591, -7.039830497734937076 ) ) ;
#105694 = AXIS2_PLACEMENT_3D ( 'NONE', #219063, #69012, #145947 ) ;
#105695 = DIRECTION ( 'NONE',  ( 1.000000000000000000, 0.000000000000000000, 0.000000000000000000 ) ) ;
#105696 = EDGE_LOOP ( 'NONE', ( #228099, #127467, #244087, #59975 ) ) ;
#105697 = ORIENTED_EDGE ( 'NONE', *, *, #199683, .F. ) ;
#105698 = CARTESIAN_POINT ( 'NONE',  ( -20.54999999999999716, 85.00000000001188027, -93.12913836187181005 ) ) ;
#105699 = DIRECTION ( 'NONE',  ( 0.000000000000000000, 0.000000000000000000, 1.000000000000000000 ) ) ;
#105700 = DIRECTION ( 'NONE',  ( 0.000000000000000000, -0.9915357197604853789, 0.1298341882520022694 ) ) ;
#105701 = CARTESIAN_POINT ( 'NONE',  ( 21.05000000000000071, 87.29603075034691528, -66.47520832486038955 ) ) ;
#105702 = CARTESIAN_POINT ( 'NONE',  ( -22.39999999999999858, 64.35000000001195986, -103.1231074845243825 ) ) ;
#105703 = CARTESIAN_POINT ( 'NONE',  ( -21.05000000000000071, 6.497017786431962705, -0.01454569056942280232 ) ) ;
#105704 = ORIENTED_EDGE ( 'NONE', *, *, #126857, .F. ) ;
#105705 = CARTESIAN_POINT ( 'NONE',  ( -20.64999999999999858, 85.00000000001251976, -179.5170766071767332 ) ) ;
#105707 = ADVANCED_FACE ( 'NONE', ( #129733 ), #69780, .T. ) ;
#105706 = DIRECTION ( 'NONE',  ( -1.000000000000000000, -0.000000000000000000, -0.000000000000000000 ) ) ;
#105708 = CARTESIAN_POINT ( 'NONE',  ( -21.07954763557493294, 0.06587591862955510802, -60.67070900996179716 ) ) ;
#105710 = DIRECTION ( 'NONE',  ( -1.000000000000000000, -0.000000000000000000, -0.000000000000000000 ) ) ;
#105709 = FACE_OUTER_BOUND ( 'NONE', #40120, .T. ) ;
#105711 = CARTESIAN_POINT ( 'NONE',  ( -23.15000000000000213, 2.000000000011154189, -87.87537807723795424 ) ) ;
#105712 = EDGE_CURVE ( 'NONE', #53966, #252130, #2756, .T. ) ;
#105713 = DIRECTION ( 'NONE',  ( -0.000000000000000000, -6.982962677686266711E-15, 1.000000000000000000 ) ) ;
#105714 = DIRECTION ( 'NONE',  ( 0.000000000000000000, -0.3738317757008748909, -0.9274965247785733613 ) ) ;
#105715 = CARTESIAN_POINT ( 'NONE',  ( 21.14999999999999503, 11.40444339177024524, -198.6185779617709670 ) ) ;
#105716 = AXIS2_PLACEMENT_3D ( 'NONE', #54912, #97875, #60055 ) ;
#105718 = ORIENTED_EDGE ( 'NONE', *, *, #3426, .F. ) ;
#105717 = CARTESIAN_POINT ( 'NONE',  ( 22.47071067811864964, 29.57301391503007792, -252.6169816238249552 ) ) ;
#105719 = VECTOR ( 'NONE', #154943, 1000.000000000000000 ) ;
#105720 = CIRCLE ( 'NONE', #5762, 0.1000000000000028644 ) ;
#105721 = EDGE_CURVE ( 'NONE', #225666, #56536, #174041, .T. ) ;
#105722 = ADVANCED_FACE ( 'NONE', ( #90590 ), #148529, .F. ) ;
#105723 = EDGE_CURVE ( 'NONE', #186771, #229354, #61219, .T. ) ;
#105724 = CARTESIAN_POINT ( 'NONE',  ( -21.65000000000000213, 7.250000000011138646, -143.2500000000000284 ) ) ;
#105726 = CARTESIAN_POINT ( 'NONE',  ( -18.51697539158857353, 65.68434038414308418, -30.48668807260655456 ) ) ;
#105725 = VECTOR ( 'NONE', #43646, 999.9999999999998863 ) ;
#105727 = ADVANCED_FACE ( 'NONE', ( #91883 ), #73714, .T. ) ;
#105728 = DIRECTION ( 'NONE',  ( 1.000000000000000000, 0.000000000000000000, 0.000000000000000000 ) ) ;
#105729 = ORIENTED_EDGE ( 'NONE', *, *, #190258, .F. ) ;
#105730 = VECTOR ( 'NONE', #117000, 1000.000000000000000 ) ;
#105731 = DIRECTION ( 'NONE',  ( 0.000000000000000000, -0.9770955615653316162, -0.2128009952263604232 ) ) ;
#105732 = CIRCLE ( 'NONE', #126611, 0.09999999999999843736 ) ;
#105733 = DIRECTION ( 'NONE',  ( 0.000000000000000000, 0.9651348961777157509, -0.2617529984165031243 ) ) ;
#105734 = LINE ( 'NONE', #226994, #223467 ) ;
#105735 = AXIS2_PLACEMENT_3D ( 'NONE', #14245, #115894, #33834 ) ;
#105736 = VERTEX_POINT ( 'NONE', #72346 ) ;
#105737 = CARTESIAN_POINT ( 'NONE',  ( -21.14999999999994174, 74.16448838626247664, -47.52760213295649550 ) ) ;
#105739 = ORIENTED_EDGE ( 'NONE', *, *, #133247, .F. ) ;
#105738 = CARTESIAN_POINT ( 'NONE',  ( -16.84793658983412712, 9.950000000011073098, -188.2663533221895591 ) ) ;
#105741 = CARTESIAN_POINT ( 'NONE',  ( 21.05000000000000071, 75.90220970870363715, -176.2809220950004772 ) ) ;
#105740 = CARTESIAN_POINT ( 'NONE',  ( 21.08479644141222664, -1.293017255164235157, -194.7878304459186722 ) ) ;
#105742 = EDGE_CURVE ( 'NONE', #120691, #61360, #173440, .T. ) ;
#105743 = DIRECTION ( 'NONE',  ( 6.484947573744954877E-15, -0.9274965247785555977, 0.3738317757009190223 ) ) ;
#105744 = EDGE_LOOP ( 'NONE', ( #100231, #221744, #186559, #109842 ) ) ;
#105745 = CARTESIAN_POINT ( 'NONE',  ( 21.14999999999999858, 81.77808381374873647, -227.1078217596952697 ) ) ;
#105746 = AXIS2_PLACEMENT_3D ( 'NONE', #221147, #182044, #162492 ) ;
#105747 = DIRECTION ( 'NONE',  ( 0.000000000000000000, 0.000000000000000000, 1.000000000000000000 ) ) ;
#105749 = FACE_OUTER_BOUND ( 'NONE', #166929, .T. ) ;
#105748 = CIRCLE ( 'NONE', #226365, 0.09999999999999938105 ) ;
#105751 = CIRCLE ( 'NONE', #114143, 0.09999999999999112377 ) ;
#105750 = CARTESIAN_POINT ( 'NONE',  ( 20.04142135623730070, 11.75000000001115907, -88.35000000000003695 ) ) ;
#105752 = CARTESIAN_POINT ( 'NONE',  ( -18.59999999999999787, 42.92545512184477730, -254.1955779480491344 ) ) ;
#105753 = ORIENTED_EDGE ( 'NONE', *, *, #190594, .F. ) ;
#105754 = CARTESIAN_POINT ( 'NONE',  ( 20.94999999999999929, -1.349153571964892606, -108.2874973355899328 ) ) ;
#105755 = CARTESIAN_POINT ( 'NONE',  ( 21.14999999999999503, 76.00000000001199396, -109.2731074845243171 ) ) ;
#105756 = AXIS2_PLACEMENT_3D ( 'NONE', #213012, #73541, #119063 ) ;
#105757 = CARTESIAN_POINT ( 'NONE',  ( -20.94999999999999929, 7.128833340093095217, -233.7327013124392749 ) ) ;
#105758 = AXIS2_PLACEMENT_3D ( 'NONE', #256928, #177482, #105573 ) ;
#105759 = LINE ( 'NONE', #184036, #249284 ) ;
#105760 = ORIENTED_EDGE ( 'NONE', *, *, #29746, .T. ) ;
#105761 = EDGE_LOOP ( 'NONE', ( #77694, #10136 ) ) ;
#105762 = CIRCLE ( 'NONE', #26709, 0.4999999999999944489 ) ;
#105763 = DIRECTION ( 'NONE',  ( 1.000000000000000000, 0.000000000000000000, 0.000000000000000000 ) ) ;
#105764 = CIRCLE ( 'NONE', #205742, 0.1000000000000028644 ) ;
#105765 = AXIS2_PLACEMENT_3D ( 'NONE', #71203, #132440, #73779 ) ;
#105766 = LINE ( 'NONE', #204877, #173739 ) ;
#105767 = CARTESIAN_POINT ( 'NONE',  ( -23.15000000000000213, 64.35000000001187459, -90.87310748452438247 ) ) ;
#105768 = CARTESIAN_POINT ( 'NONE',  ( 21.05933563467872105, 13.07370587250136040, -210.6321695627368911 ) ) ;
#105769 = CARTESIAN_POINT ( 'NONE',  ( 21.09546886439553859, 8.878553113026075749, -146.2370938505546860 ) ) ;
#105771 = DIRECTION ( 'NONE',  ( -0.000000000000000000, -6.982962677686266711E-15, 1.000000000000000000 ) ) ;
#105770 = CARTESIAN_POINT ( 'NONE',  ( -21.05000000000000071, 14.81796439977981272, -236.5325475414793743 ) ) ;
#105772 = CARTESIAN_POINT ( 'NONE',  ( 18.59999999999999432, -1.835859311432481045, -78.50443916879852679 ) ) ;
#105773 = CYLINDRICAL_SURFACE ( 'NONE', #6093, 3.999999999999994671 ) ;
#105774 = CARTESIAN_POINT ( 'NONE',  ( -22.50014994444007854, 64.25028026811983750, -136.6061876412430820 ) ) ;
#105775 = EDGE_CURVE ( 'NONE', #119358, #121523, #252928, .T. ) ;
#105777 = VERTEX_POINT ( 'NONE', #119167 ) ;
#105776 = CARTESIAN_POINT ( 'NONE',  ( 15.57250062127602419, 62.77489950700472576, -216.4869172218852214 ) ) ;
#105778 = DIRECTION ( 'NONE',  ( -0.000000000000000000, 6.982962677686266711E-15, -1.000000000000000000 ) ) ;
#105779 = CARTESIAN_POINT ( 'NONE',  ( 18.59999999999999076, 43.21392023178792385, -245.1418509714632421 ) ) ;
#105780 =( BOUNDED_CURVE ( )  B_SPLINE_CURVE ( 3, ( #246034, #225154, #122237, #102632 ),
 .UNSPECIFIED., .F., .F. ) 
 B_SPLINE_CURVE_WITH_KNOTS ( ( 4, 4 ),
 ( 0.000000000000000000, 1.570796326794891229 ),
 .UNSPECIFIED. ) 
 CURVE ( )  GEOMETRIC_REPRESENTATION_ITEM ( )  RATIONAL_B_SPLINE_CURVE ( ( 1.000000000000000000, 0.8047378541243662697, 0.8047378541243662697, 1.000000000000000000 ) ) 
 REPRESENTATION_ITEM ( '' )  );
#105781 = ORIENTED_EDGE ( 'NONE', *, *, #36188, .F. ) ;
#105782 = DIRECTION ( 'NONE',  ( 1.000000000000000000, -0.000000000000000000, -0.000000000000000000 ) ) ;
#105783 = CARTESIAN_POINT ( 'NONE',  ( -18.59999999999999787, 85.32100840337338354, -129.2871692354463562 ) ) ;
#105784 = CARTESIAN_POINT ( 'NONE',  ( 21.04999999999997584, 18.90422431703804307, -227.9828523687716313 ) ) ;
#105785 = DIRECTION ( 'NONE',  ( 0.000000000000000000, -1.000000000000000000, 0.000000000000000000 ) ) ;
#105787 = ADVANCED_FACE ( 'NONE', ( #1762 ), #18765, .T. ) ;
#105786 = DIRECTION ( 'NONE',  ( 0.000000000000000000, 1.000000000000000000, 0.000000000000000000 ) ) ;
#105788 = ORIENTED_EDGE ( 'NONE', *, *, #244793, .T. ) ;
#105789 = ORIENTED_EDGE ( 'NONE', *, *, #112784, .F. ) ;
#105790 = AXIS2_PLACEMENT_3D ( 'NONE', #255573, #160410, #54840 ) ;
#105791 = ADVANCED_FACE ( 'NONE', ( #179164 ), #60453, .T. ) ;
#105792 = EDGE_CURVE ( 'NONE', #109264, #18074, #136121, .T. ) ;
#105793 = CIRCLE ( 'NONE', #64135, 0.1000000000000026007 ) ;
#105794 = LINE ( 'NONE', #62847, #192745 ) ;
#105795 = EDGE_LOOP ( 'NONE', ( #31467, #141539 ) ) ;
#105796 = CARTESIAN_POINT ( 'NONE',  ( 18.59999999999999076, 69.35000000001222986, -148.8731074845244109 ) ) ;
#105797 = ORIENTED_EDGE ( 'NONE', *, *, #234714, .F. ) ;
#105798 = CARTESIAN_POINT ( 'NONE',  ( -16.87683809663752399, 23.65833333334447985, -50.25000000000000000 ) ) ;
#105799 = DIRECTION ( 'NONE',  ( 1.000000000000000000, -0.000000000000000000, -0.000000000000000000 ) ) ;
#105800 = AXIS2_PLACEMENT_3D ( 'NONE', #154049, #54877, #134406 ) ;
#105801 = CIRCLE ( 'NONE', #72520, 0.5000000000000004441 ) ;
#105802 = PLANE ( 'NONE',  #97202 ) ;
#105803 = EDGE_LOOP ( 'NONE', ( #153005, #156326, #165328, #35621 ) ) ;
#105804 = EDGE_CURVE ( 'NONE', #45065, #146218, #76165, .T. ) ;
#105805 = TOROIDAL_SURFACE ( 'NONE', #9968, 7.800000000000000711, 0.1000000000000000056 ) ;
#105806 = EDGE_CURVE ( 'NONE', #2285, #14789, #56582, .T. ) ;
#105807 = CYLINDRICAL_SURFACE ( 'NONE', #84170, 0.09999999999999939493 ) ;
#105809 = AXIS2_PLACEMENT_3D ( 'NONE', #8834, #128789, #66242 ) ;
#105808 = DIRECTION ( 'NONE',  ( 0.000000000000000000, 0.000000000000000000, 1.000000000000000000 ) ) ;
#105810 = DIRECTION ( 'NONE',  ( 0.000000000000000000, 0.000000000000000000, -1.000000000000000000 ) ) ;
#105812 = AXIS2_PLACEMENT_3D ( 'NONE', #7689, #208468, #209733 ) ;
#105811 = DIRECTION ( 'NONE',  ( 0.000000000000000000, 0.4999999999999088507, 0.8660254037844913322 ) ) ;
#105813 = PRODUCT_RELATED_PRODUCT_CATEGORY ( 'part', '', ( #244984 ) ) ;
#105814 = CARTESIAN_POINT ( 'NONE',  ( -20.94999999999999929, 86.27712145182582049, -209.5223386573213702 ) ) ;
#105815 = CIRCLE ( 'NONE', #251584, 0.09999999999999982514 ) ;
#105816 = CARTESIAN_POINT ( 'NONE',  ( -18.50000000000000711, 64.25000000001190870, -96.00830171387039513 ) ) ;
#105817 = ORIENTED_EDGE ( 'NONE', *, *, #97075, .F. ) ;
#105819 = CARTESIAN_POINT ( 'NONE',  ( -20.64999999999999858, 85.00000000001197975, -112.9170766071766820 ) ) ;
#105818 = DIRECTION ( 'NONE',  ( 0.000000000000000000, 0.000000000000000000, -1.000000000000000000 ) ) ;
#105820 = VERTEX_POINT ( 'NONE', #38350 ) ;
#105822 = ORIENTED_EDGE ( 'NONE', *, *, #165972, .F. ) ;
#105821 = DIRECTION ( 'NONE',  ( -0.000000000000000000, 0.2617529984165031243, 0.9651348961777157509 ) ) ;
#105823 = VECTOR ( 'NONE', #135107, 1000.000000000000000 ) ;
#105824 = ORIENTED_EDGE ( 'NONE', *, *, #208768, .T. ) ;
#105825 = CARTESIAN_POINT ( 'NONE',  ( -18.59999999999999787, 102.4393534156127572, -84.88159887701665696 ) ) ;
#105826 = CARTESIAN_POINT ( 'NONE',  ( -18.40000000000000213, 11.75000000001113953, -154.8500000000000227 ) ) ;
#105827 = DIRECTION ( 'NONE',  ( 1.000000000000000000, 0.000000000000000000, 0.000000000000000000 ) ) ;
#105828 = ADVANCED_FACE ( 'NONE', ( #257323 ), #177868, .F. ) ;
#105829 = CARTESIAN_POINT ( 'NONE',  ( 18.59999999999999076, 1.835341550224411922, -11.65515129256298010 ) ) ;
#105830 = ORIENTED_EDGE ( 'NONE', *, *, #159300, .F. ) ;
#105831 = ADVANCED_FACE ( 'NONE', ( #96980 ), #256042, .T. ) ;
#105832 = EDGE_CURVE ( 'NONE', #111084, #246341, #211248, .T. ) ;
#105833 = PLANE ( 'NONE',  #255513 ) ;
#105835 = CARTESIAN_POINT ( 'NONE',  ( -16.81930730667007268, 66.06300193113824548, -157.2963397539862171 ) ) ;
#105834 = AXIS2_PLACEMENT_3D ( 'NONE', #213202, #164161, #65046 ) ;
#105836 = ORIENTED_EDGE ( 'NONE', *, *, #172165, .F. ) ;
#105837 = CARTESIAN_POINT ( 'NONE',  ( -16.94333152882356330, 9.990342011468825945, -154.8920315311015088 ) ) ;
#105838 = CIRCLE ( 'NONE', #176610, 0.1000000000000024342 ) ;
#105839 = DIRECTION ( 'NONE',  ( -1.000000000000000000, 0.000000000000000000, -0.000000000000000000 ) ) ;
#105840 = ORIENTED_EDGE ( 'NONE', *, *, #201253, .T. ) ;
#105841 = MANIFOLD_SOLID_BREP ( 'Stock-MAS-200-1', #136645 ) ;
#105842 = CARTESIAN_POINT ( 'NONE',  ( -16.79270642812298320, 9.946244216949343908, -146.6610667214371233 ) ) ;
#105843 = CIRCLE ( 'NONE', #222349, 0.1000000000000028644 ) ;
#105844 = CIRCLE ( 'NONE', #197433, 3.900000000000000799 ) ;
#105845 = ORIENTED_EDGE ( 'NONE', *, *, #215010, .T. ) ;
#105846 = VECTOR ( 'NONE', #172588, 1000.000000000000000 ) ;
#105847 = DIRECTION ( 'NONE',  ( 0.000000000000000000, -0.5626415523513815797, 0.8267009638119623416 ) ) ;
#105848 = ORIENTED_EDGE ( 'NONE', *, *, #24902, .T. ) ;
#105849 = DIRECTION ( 'NONE',  ( 1.000000000000000000, 1.646408749285562691E-14, 1.073024830501117725E-15 ) ) ;
#105850 = CARTESIAN_POINT ( 'NONE',  ( 20.90000000000000213, 11.49641995933507843, 1.885425182446133885 ) ) ;
#105851 = DIRECTION ( 'NONE',  ( 0.000000000000000000, -7.172728831056617961E-15, 1.000000000000000000 ) ) ;
#105852 = CARTESIAN_POINT ( 'NONE',  ( -21.07016717456945898, 6.176163237836298059, -199.6548974988868679 ) ) ;
#105853 = ADVANCED_FACE ( 'NONE', ( #143843 ), #19720, .F. ) ;
#105854 = AXIS2_PLACEMENT_3D ( 'NONE', #173637, #134426, #152766 ) ;
#105855 = CARTESIAN_POINT ( 'NONE',  ( -19.89999999999999503, 4.631764625546185066, 22.00000000000000355 ) ) ;
#105856 = AXIS2_PLACEMENT_3D ( 'NONE', #155940, #213302, #195059 ) ;
#105857 = AXIS2_PLACEMENT_3D ( 'NONE', #222053, #79978, #82541 ) ;
#105858 = DIRECTION ( 'NONE',  ( 1.000000000000000000, 0.000000000000000000, 0.000000000000000000 ) ) ;
#105859 = ORIENTED_EDGE ( 'NONE', *, *, #66843, .T. ) ;
#105861 = FACE_OUTER_BOUND ( 'NONE', #188807, .T. ) ;
#105860 = CARTESIAN_POINT ( 'NONE',  ( -21.09107601085566230, 69.63612202465257894, -170.0624146492417879 ) ) ;
#105862 = CARTESIAN_POINT ( 'NONE',  ( 20.90000000000000213, -1.901609089591594470, -11.59510167572422112 ) ) ;
#105863 = CARTESIAN_POINT ( 'NONE',  ( -16.92778301347309622, 12.44710274780528181, -211.1553281274974552 ) ) ;
#105864 = ADVANCED_FACE ( 'NONE', ( #123022 ), #219600, .F. ) ;
#105865 = CARTESIAN_POINT ( 'NONE',  ( 21.05000000000000071, 76.10000000001272724, -210.0637644362255969 ) ) ;
#105867 = ORIENTED_EDGE ( 'NONE', *, *, #22013, .T. ) ;
#105866 = FACE_OUTER_BOUND ( 'NONE', #79133, .T. ) ;
#105869 = ORIENTED_EDGE ( 'NONE', *, *, #222352, .F. ) ;
#105868 = CARTESIAN_POINT ( 'NONE',  ( -23.25000000000000000, 1.115600667400684642E-11, -200.9999999999999432 ) ) ;
#105870 = FILL_AREA_STYLE_COLOUR ( '', #177035 ) ;
#105871 = LINE ( 'NONE', #45924, #188172 ) ;
#105872 = EDGE_CURVE ( 'NONE', #188675, #202242, #140490, .T. ) ;
#105874 = ORIENTED_EDGE ( 'NONE', *, *, #155138, .F. ) ;
#105873 = DIRECTION ( 'NONE',  ( 1.000000000000000000, -0.000000000000000000, -0.000000000000000000 ) ) ;
#105875 = ADVANCED_FACE ( 'NONE', ( #244224 ), #26495, .T. ) ;
#105877 = EDGE_CURVE ( 'NONE', #28001, #110479, #83836, .T. ) ;
#105876 = DIRECTION ( 'NONE',  ( 1.000000000000000000, 0.000000000000000000, 0.000000000000000000 ) ) ;
#105878 = AXIS2_PLACEMENT_3D ( 'NONE', #210455, #168797, #211740 ) ;
#105879 = CARTESIAN_POINT ( 'NONE',  ( 20.85000000000000142, 7.783179459866048866, -245.3643104511423019 ) ) ;
#105881 = EDGE_CURVE ( 'NONE', #191930, #153656, #40592, .T. ) ;
#105880 = ORIENTED_EDGE ( 'NONE', *, *, #44691, .T. ) ;
#105882 = ORIENTED_EDGE ( 'NONE', *, *, #37975, .T. ) ;
#105883 = CARTESIAN_POINT ( 'NONE',  ( -17.11825945287482753, 65.95000000001262208, -190.8731074845244393 ) ) ;
#105884 = CARTESIAN_POINT ( 'NONE',  ( 21.72449340488910607, 65.71604372252069481, -82.17310748452439384 ) ) ;
#105885 = ORIENTED_EDGE ( 'NONE', *, *, #35919, .F. ) ;
#105886 = DIRECTION ( 'NONE',  ( -1.000000000000000000, 0.000000000000000000, 0.000000000000000000 ) ) ;
#105887 = CARTESIAN_POINT ( 'NONE',  ( -16.87845715379269507, 9.957858113908169884, -180.1238006510588718 ) ) ;
#105888 = ORIENTED_EDGE ( 'NONE', *, *, #33281, .T. ) ;
#105889 = VECTOR ( 'NONE', #166906, 1000.000000000000114 ) ;
#105891 = EDGE_CURVE ( 'NONE', #240051, #95993, #215331, .T. ) ;
#105890 = CARTESIAN_POINT ( 'NONE',  ( 21.08884785362045378, 6.200991531159584902, -199.5985400833362178 ) ) ;
#105892 = CIRCLE ( 'NONE', #151750, 0.09999999999998898659 ) ;
#105893 = EDGE_CURVE ( 'NONE', #116921, #132362, #227795, .T. ) ;
#105894 = AXIS2_PLACEMENT_3D ( 'NONE', #174429, #12761, #175676 ) ;
#105895 = AXIS2_PLACEMENT_3D ( 'NONE', #29728, #229188, #130061 ) ;
#105896 = EDGE_LOOP ( 'NONE', ( #110907, #13880, #53665, #55249 ) ) ;
#105897 = ORIENTED_EDGE ( 'NONE', *, *, #172415, .T. ) ;
#105898 = CARTESIAN_POINT ( 'NONE',  ( -18.50000000000000000, -9.399999999988850163, -73.88204184817267617 ) ) ;
#105899 = ORIENTED_EDGE ( 'NONE', *, *, #102349, .F. ) ;
#105900 = EDGE_CURVE ( 'NONE', #100999, #79411, #223378, .T. ) ;
#105901 = CARTESIAN_POINT ( 'NONE',  ( -22.50000000000000000, 75.90000000001170122, -77.31388708289772183 ) ) ;
#105902 = VERTEX_POINT ( 'NONE', #87717 ) ;
#105904 = ORIENTED_EDGE ( 'NONE', *, *, #35255, .F. ) ;
#105903 = CYLINDRICAL_SURFACE ( 'NONE', #93213, 0.09999999999999939493 ) ;
#105905 = CARTESIAN_POINT ( 'NONE',  ( -21.05439746398122836, 11.75000000001115197, -73.98991648748463490 ) ) ;
#105906 = ORIENTED_EDGE ( 'NONE', *, *, #111253, .F. ) ;
#105907 = CARTESIAN_POINT ( 'NONE',  ( 18.59999999999999787, -0.5913595841389442942, -242.4574432119242999 ) ) ;
#105909 = ORIENTED_EDGE ( 'NONE', *, *, #13110, .T. ) ;
#105908 = EDGE_CURVE ( 'NONE', #203977, #14615, #202547, .T. ) ;
#105911 = VERTEX_POINT ( 'NONE', #227241 ) ;
#105910 = ORIENTED_EDGE ( 'NONE', *, *, #75615, .T. ) ;
#105913 = DIRECTION ( 'NONE',  ( 1.000000000000000000, 0.000000000000000000, 0.000000000000000000 ) ) ;
#105912 = CIRCLE ( 'NONE', #64249, 0.09999999999999971412 ) ;
#105914 = ADVANCED_FACE ( 'NONE', ( #48605 ), #105989, .F. ) ;
#105915 = LINE ( 'NONE', #164646, #35831 ) ;
#105916 = ORIENTED_EDGE ( 'NONE', *, *, #208897, .T. ) ;
#105917 = CIRCLE ( 'NONE', #89181, 0.9750000000000036415 ) ;
#105918 = CIRCLE ( 'NONE', #251694, 0.09999999999999939493 ) ;
#105919 = CIRCLE ( 'NONE', #134958, 0.1000000000000028644 ) ;
#105920 = AXIS2_PLACEMENT_3D ( 'NONE', #74432, #195648, #230920 ) ;
#105921 = EDGE_LOOP ( 'NONE', ( #150166, #232553, #213116, #20454 ) ) ;
#105922 = LINE ( 'NONE', #85066, #149553 ) ;
#105923 = DIRECTION ( 'NONE',  ( 0.000000000000000000, -0.1298341882520022694, -0.9915357197604853789 ) ) ;
#105925 = EDGE_LOOP ( 'NONE', ( #45733, #131493, #108297, #120750 ) ) ;
#105924 = DIRECTION ( 'NONE',  ( 0.000000000000000000, -0.2617529984165031243, -0.9651348961777157509 ) ) ;
#105926 = CARTESIAN_POINT ( 'NONE',  ( -23.25000000000000000, -11.64999999998884483, -137.1000000000000227 ) ) ;
#105927 = ORIENTED_EDGE ( 'NONE', *, *, #169940, .T. ) ;
#105928 = EDGE_CURVE ( 'NONE', #114955, #240778, #15447, .T. ) ;
#105929 = CARTESIAN_POINT ( 'NONE',  ( -23.15000000000000213, 4.349999999999999645, -21.25000000000000000 ) ) ;
#105930 = CARTESIAN_POINT ( 'NONE',  ( 18.49999999999999289, 65.71984138295523792, -111.7985354133230516 ) ) ;
#105931 = EDGE_CURVE ( 'NONE', #28188, #204919, #7204, .T. ) ;
#105932 = VECTOR ( 'NONE', #59173, 1000.000000000000000 ) ;
#105933 = ORIENTED_EDGE ( 'NONE', *, *, #32224, .F. ) ;
#105934 = AXIS2_PLACEMENT_3D ( 'NONE', #179319, #60612, #58035 ) ;
#105935 = CARTESIAN_POINT ( 'NONE',  ( 23.25000000000000000, -8.596261682231828516, -57.54987248284972168 ) ) ;
#105936 = DIRECTION ( 'NONE',  ( 0.000000000000000000, 0.7216758089626587047, -0.6922311945860948335 ) ) ;
#105937 = AXIS2_PLACEMENT_3D ( 'NONE', #108760, #168791, #171356 ) ;
#105938 = ORIENTED_EDGE ( 'NONE', *, *, #59048, .F. ) ;
#105939 = DIRECTION ( 'NONE',  ( 1.000000000000000000, 0.000000000000000000, 0.000000000000000000 ) ) ;
#105940 = ORIENTED_EDGE ( 'NONE', *, *, #28203, .F. ) ;
#105941 = AXIS2_PLACEMENT_3D ( 'NONE', #34117, #35399, #94038 ) ;
#105944 = VERTEX_POINT ( 'NONE', #103421 ) ;
#105943 = VERTEX_POINT ( 'NONE', #23938 ) ;
#105942 = VECTOR ( 'NONE', #90837, 1000.000000000000000 ) ;
#105945 = EDGE_LOOP ( 'NONE', ( #228120, #165357, #2337, #121881 ) ) ;
#105946 = DIRECTION ( 'NONE',  ( -1.000000000000000000, -1.476360405086644309E-16, 0.000000000000000000 ) ) ;
#105947 = ORIENTED_EDGE ( 'NONE', *, *, #217995, .T. ) ;
#105948 = DIRECTION ( 'NONE',  ( 0.000000000000000000, 0.000000000000000000, -1.000000000000000000 ) ) ;
#105949 = ORIENTED_EDGE ( 'NONE', *, *, #111502, .F. ) ;
#105950 = CARTESIAN_POINT ( 'NONE',  ( -16.89797118371577866, 66.02361927736723146, -48.58581411696576424 ) ) ;
#105951 = AXIS2_PLACEMENT_3D ( 'NONE', #217508, #98826, #83109 ) ;
#105952 = AXIS2_PLACEMENT_3D ( 'NONE', #121312, #101670, #202096 ) ;
#105953 = CARTESIAN_POINT ( 'NONE',  ( 21.05000000000000071, -8.663551401857999323, -124.4758988819327215 ) ) ;
#105954 = TOROIDAL_SURFACE ( 'NONE', #60184, 11.65000000000000036, 0.1000000000000000056 ) ;
#105955 = ORIENTED_EDGE ( 'NONE', *, *, #84103, .F. ) ;
#105956 = B_SPLINE_CURVE_WITH_KNOTS ( 'NONE', 3,
 ( #123942, #62680, #26125, #223012, #166944, #202183, #65229, #144752, #103058, #225568 ),
 .UNSPECIFIED., .F., .F.,
 ( 4, 3, 3, 4 ),
 ( 7.632826238685023174E-06, 4.756916949876414344E-05, 9.484459048151255107E-05, 0.0001435500935099816788 ),
 .UNSPECIFIED. ) ;
#105957 = VERTEX_POINT ( 'NONE', #183001 ) ;
#105958 = ORIENTED_EDGE ( 'NONE', *, *, #20925, .T. ) ;
#105959 = EDGE_CURVE ( 'NONE', #253697, #66070, #64325, .T. ) ;
#105960 = CARTESIAN_POINT ( 'NONE',  ( -20.85000000000000142, 76.00000000001170974, -69.52310748452431710 ) ) ;
#105961 = ORIENTED_EDGE ( 'NONE', *, *, #180597, .F. ) ;
#105962 = CARTESIAN_POINT ( 'NONE',  ( -21.14999999999994174, 76.00000000001119815, -36.02310748452479316 ) ) ;
#105964 = ORIENTED_EDGE ( 'NONE', *, *, #198794, .T. ) ;
#105963 = DIRECTION ( 'NONE',  ( 0.000000000000000000, 0.2617529984165152257, 0.9651348961777124202 ) ) ;
#105965 = DIRECTION ( 'NONE',  ( 0.000000000000000000, -0.5907332058517320572, 0.8068669527896995541 ) ) ;
#105966 = CARTESIAN_POINT ( 'NONE',  ( 22.10000000000000142, -11.75000000000000355, 12.09999999999999609 ) ) ;
#105967 = CARTESIAN_POINT ( 'NONE',  ( -20.85000000000000142, 68.97833521811203639, -132.8895420826271163 ) ) ;
#105968 = DIRECTION ( 'NONE',  ( 1.000000000000000000, -0.000000000000000000, -0.000000000000000000 ) ) ;
#105969 = CARTESIAN_POINT ( 'NONE',  ( -18.50000000000000000, 85.40000000001263913, -196.2258477248610120 ) ) ;
#105970 = AXIS2_PLACEMENT_3D ( 'NONE', #63848, #83376, #200793 ) ;
#105972 = CARTESIAN_POINT ( 'NONE',  ( 18.59999999999999076, 1.250000000011167511, -75.00000000000004263 ) ) ;
#105971 = CARTESIAN_POINT ( 'NONE',  ( -21.05000000000000071, -0.09999999998884338825, -60.45934304829880546 ) ) ;
#105973 = DIRECTION ( 'NONE',  ( 0.000000000000000000, 0.9908441862701596881, -0.1350103645451904977 ) ) ;
#105974 = CARTESIAN_POINT ( 'NONE',  ( 19.90000000000000924, 4.513204987021262937, 22.00000000000000355 ) ) ;
#105975 = TOROIDAL_SURFACE ( 'NONE', #172689, 7.791421356237316687, 0.1000000000000000056 ) ;
#105976 = DIRECTION ( 'NONE',  ( 1.000000000000000000, 0.000000000000000000, 0.000000000000000000 ) ) ;
#105977 = EDGE_CURVE ( 'NONE', #174669, #89497, #161168, .T. ) ;
#105979 = FACE_OUTER_BOUND ( 'NONE', #117377, .T. ) ;
#105978 = CIRCLE ( 'NONE', #131127, 0.1000000000000072220 ) ;
#105980 = ORIENTED_EDGE ( 'NONE', *, *, #54945, .T. ) ;
#105981 = AXIS2_PLACEMENT_3D ( 'NONE', #111365, #12286, #91801 ) ;
#105982 = CIRCLE ( 'NONE', #239285, 0.09999999999998898659 ) ;
#105984 = VERTEX_POINT ( 'NONE', #232412 ) ;
#105983 = DIRECTION ( 'NONE',  ( -1.186688945009010324E-16, 0.4721928772777345684, 0.8814952561688430555 ) ) ;
#105985 = ORIENTED_EDGE ( 'NONE', *, *, #168028, .F. ) ;
#105986 = FACE_OUTER_BOUND ( 'NONE', #49258, .T. ) ;
#105987 = CARTESIAN_POINT ( 'NONE',  ( 20.52683494730037239, 8.980530818312608687, -142.5052527225372216 ) ) ;
#105988 = CIRCLE ( 'NONE', #189233, 0.09999999999999939493 ) ;
#105989 = SPHERICAL_SURFACE ( 'NONE', #207159, 0.1000000000000000056 ) ;
#105990 = VERTEX_POINT ( 'NONE', #30349 ) ;
#105991 = VECTOR ( 'NONE', #250959, 1000.000000000000000 ) ;
#105992 = CIRCLE ( 'NONE', #122617, 4.049999999999998046 ) ;
#105993 = CARTESIAN_POINT ( 'NONE',  ( -22.50000000000000000, 76.00000000001165290, -69.52310748452431710 ) ) ;
#105994 = TOROIDAL_SURFACE ( 'NONE', #43485, 0.2000000000000000111, 0.1000000000000000056 ) ;
#105995 = CARTESIAN_POINT ( 'NONE',  ( -20.54999999999999716, 85.50000000001222134, -146.4170766071767389 ) ) ;
#105996 = ORIENTED_EDGE ( 'NONE', *, *, #200033, .F. ) ;
#105997 = CARTESIAN_POINT ( 'NONE',  ( -20.64999999999999858, 7.533155231024649012, -235.5891828794142384 ) ) ;
#105998 = DIRECTION ( 'NONE',  ( -1.000000000000000000, 0.000000000000000000, 0.000000000000000000 ) ) ;
#105999 = DIRECTION ( 'NONE',  ( 0.000000000000000000, 2.664535259100343354E-15, -1.000000000000000000 ) ) ;
#106000 = CARTESIAN_POINT ( 'NONE',  ( -20.64999999999999858, -9.000000000000003553, -9.893969122652444881 ) ) ;
#106002 = ORIENTED_EDGE ( 'NONE', *, *, #174492, .T. ) ;
#106001 = DIRECTION ( 'NONE',  ( 1.000000000000000000, 0.000000000000000000, 0.000000000000000000 ) ) ;
#106003 = CIRCLE ( 'NONE', #214368, 0.09999999999999939493 ) ;
#106004 = LINE ( 'NONE', #58223, #240216 ) ;
#106005 = DIRECTION ( 'NONE',  ( -1.000000000000000000, 0.000000000000000000, -0.000000000000000000 ) ) ;
#106006 = LINE ( 'NONE', #30370, #37624 ) ;
#106007 = CARTESIAN_POINT ( 'NONE',  ( 18.52165635395173027, 85.48115071129409159, -95.99826990166178575 ) ) ;
#106008 = VERTEX_POINT ( 'NONE', #129433 ) ;
#106009 = DIRECTION ( 'NONE',  ( 0.000000000000000000, -0.4999999999999994449, -0.8660254037844390407 ) ) ;
#106010 = CARTESIAN_POINT ( 'NONE',  ( 13.99999999999999822, 9.850000000011137402, -184.2499999999999716 ) ) ;
#106011 = TOROIDAL_SURFACE ( 'NONE', #14496, 1.900000000000002576, 0.1000000000000000056 ) ;
#106013 = FACE_OUTER_BOUND ( 'NONE', #157720, .T. ) ;
#106012 = DIRECTION ( 'NONE',  ( 1.734723475976817507E-14, 1.000000000000000000, 6.982962677686266711E-15 ) ) ;
#106014 = DIRECTION ( 'NONE',  ( 0.000000000000000000, -7.086529944415894657E-15, 1.000000000000000000 ) ) ;
#106016 = EDGE_CURVE ( 'NONE', #57461, #88904, #149017, .T. ) ;
#106015 = DIRECTION ( 'NONE',  ( 0.000000000000000000, 0.2617529984165032908, 0.9651348961777156399 ) ) ;
#106017 = CARTESIAN_POINT ( 'NONE',  ( -18.50211644919735576, 10.30207779524867284, -38.98955207167824000 ) ) ;
#106018 = CARTESIAN_POINT ( 'NONE',  ( 21.05000000000005400, 67.75000000001118394, -3.123107484524795474 ) ) ;
#106019 = DIRECTION ( 'NONE',  ( 0.000000000000000000, 0.000000000000000000, -1.000000000000000000 ) ) ;
#106020 = DIRECTION ( 'NONE',  ( 0.000000000000000000, 6.982962677686266711E-15, -1.000000000000000000 ) ) ;
#106021 = AXIS2_PLACEMENT_3D ( 'NONE', #59784, #19413, #178507 ) ;
#106023 = ORIENTED_EDGE ( 'NONE', *, *, #84087, .T. ) ;
#106022 = CIRCLE ( 'NONE', #26969, 0.09999999999999553690 ) ;
#106024 = DIRECTION ( 'NONE',  ( 0.000000000000000000, 0.000000000000000000, 1.000000000000000000 ) ) ;
#106025 = AXIS2_PLACEMENT_3D ( 'NONE', #60275, #21194, #61575 ) ;
#106026 = VERTEX_POINT ( 'NONE', #113721 ) ;
#106027 = ORIENTED_EDGE ( 'NONE', *, *, #99455, .T. ) ;
#106028 = EDGE_CURVE ( 'NONE', #8771, #30882, #28099, .T. ) ;
#106029 = DIRECTION ( 'NONE',  ( -1.000000000000000000, -0.000000000000000000, 0.000000000000000000 ) ) ;
#106030 = CARTESIAN_POINT ( 'NONE',  ( 20.94999999999999929, 5.399999999999998579, -12.40526601891309788 ) ) ;
#106031 = ORIENTED_EDGE ( 'NONE', *, *, #79386, .T. ) ;
#106032 = ADVANCED_FACE ( 'NONE', ( #211545 ), #132136, .F. ) ;
#106033 = EDGE_LOOP ( 'NONE', ( #28708, #61716, #224329, #201309 ) ) ;
#106034 = ADVANCED_FACE ( 'NONE', ( #248089 ), #55005, .T. ) ;
#106035 = ORIENTED_EDGE ( 'NONE', *, *, #203304, .F. ) ;
#106036 = VECTOR ( 'NONE', #243907, 1000.000000000000227 ) ;
#106037 = ORIENTED_EDGE ( 'NONE', *, *, #102132, .T. ) ;
#106038 = FACE_OUTER_BOUND ( 'NONE', #211676, .T. ) ;
#106039 = CYLINDRICAL_SURFACE ( 'NONE', #236789, 0.09999999999999939493 ) ;
#106040 = DIRECTION ( 'NONE',  ( 1.000000000000000000, 0.000000000000000000, 0.000000000000000000 ) ) ;
#106041 = FACE_OUTER_BOUND ( 'NONE', #24635, .T. ) ;
#106042 = CARTESIAN_POINT ( 'NONE',  ( -21.12757541349819590, 1.425016164502732163, -230.6714675275338777 ) ) ;
#106043 = CIRCLE ( 'NONE', #31107, 0.1000000000000028644 ) ;
#106044 = DIRECTION ( 'NONE',  ( 1.000000000000000000, 0.000000000000000000, 0.000000000000000000 ) ) ;
#106045 = LINE ( 'NONE', #241731, #249366 ) ;
#106047 = ORIENTED_EDGE ( 'NONE', *, *, #205441, .T. ) ;
#106046 = DIRECTION ( 'NONE',  ( 0.000000000000000000, 0.000000000000000000, -1.000000000000000000 ) ) ;
#106049 = CARTESIAN_POINT ( 'NONE',  ( 21.12400222705975494, 8.778511907088235589, -79.25000000000004263 ) ) ;
#106048 = CARTESIAN_POINT ( 'NONE',  ( 20.85000000000000142, 11.75000000000000355, -26.71613433702190932 ) ) ;
#106050 = ADVANCED_FACE ( 'NONE', ( #228547 ), #2939, .T. ) ;
#106051 = CYLINDRICAL_SURFACE ( 'NONE', #53241, 0.09999999999998898659 ) ;
#106052 = ORIENTED_EDGE ( 'NONE', *, *, #18515, .T. ) ;
#106053 = CARTESIAN_POINT ( 'NONE',  ( -20.85000000000000142, 7.021664781911246322, -171.3335654018973173 ) ) ;
#106054 = FACE_OUTER_BOUND ( 'NONE', #40335, .T. ) ;
#106055 = DIRECTION ( 'NONE',  ( 0.000000000000000000, -1.000000000000000000, -6.352154140967427193E-15 ) ) ;
#106056 = EDGE_LOOP ( 'NONE', ( #75672, #182301, #7972, #106207 ) ) ;
#106057 = CARTESIAN_POINT ( 'NONE',  ( 23.24999999999999645, 64.25000000001202238, -115.6731074845243938 ) ) ;
#106058 = CARTESIAN_POINT ( 'NONE',  ( 20.94999999999999929, 1.115600667400684642E-11, -200.9999999999999432 ) ) ;
#106059 = ORIENTED_EDGE ( 'NONE', *, *, #75462, .T. ) ;
#106060 = VECTOR ( 'NONE', #240654, 1000.000000000000000 ) ;
#106062 = CARTESIAN_POINT ( 'NONE',  ( 21.05000000000000071, 6.477552182504599187, -67.09999996529958821 ) ) ;
#106061 = CIRCLE ( 'NONE', #22909, 4.049999999999998046 ) ;
#106063 = DIRECTION ( 'NONE',  ( 1.000000000000000000, 0.000000000000000000, 0.000000000000000000 ) ) ;
#106064 = DIRECTION ( 'NONE',  ( 0.000000000000000000, 0.000000000000000000, 1.000000000000000000 ) ) ;
#106065 = CARTESIAN_POINT ( 'NONE',  ( -23.15000000000000213, 26.25728039895700761, -243.9792867493661106 ) ) ;
#106066 = ORIENTED_EDGE ( 'NONE', *, *, #155310, .T. ) ;
#106067 = VERTEX_POINT ( 'NONE', #74641 ) ;
#106068 = CARTESIAN_POINT ( 'NONE',  ( -17.05016517655774422, 66.05000000001255955, -182.6958054805178051 ) ) ;
#106069 = CARTESIAN_POINT ( 'NONE',  ( 21.05000000000000071, 10.72371710471867701, -41.16491356908760935 ) ) ;
#106070 = CARTESIAN_POINT ( 'NONE',  ( -21.44999999999999929, 68.85000000001228670, -157.7731074845244166 ) ) ;
#106071 = CARTESIAN_POINT ( 'NONE',  ( -23.25000000000000000, 64.25000000001203659, -114.7731074845243882 ) ) ;
#106072 = AXIS2_PLACEMENT_3D ( 'NONE', #15196, #132570, #94710 ) ;
#106073 = CARTESIAN_POINT ( 'NONE',  ( 21.10320863425824811, 6.400277386470322405, -167.4749777487728579 ) ) ;
#106074 = VECTOR ( 'NONE', #215242, 1000.000000000000114 ) ;
#106075 = DIRECTION ( 'NONE',  ( 0.7071067811865487940, -0.7071067811865462405, -4.216150419019403701E-15 ) ) ;
#106077 = ORIENTED_EDGE ( 'NONE', *, *, #19973, .F. ) ;
#106076 = AXIS2_PLACEMENT_3D ( 'NONE', #226310, #223752, #206777 ) ;
#106078 = CARTESIAN_POINT ( 'NONE',  ( -20.94983749550516450, 65.70233904877009934, -97.54874109119680270 ) ) ;
#106079 = CIRCLE ( 'NONE', #18633, 7.900000000000003908 ) ;
#106080 = EDGE_CURVE ( 'NONE', #164153, #93761, #102885, .T. ) ;
#106082 = VERTEX_POINT ( 'NONE', #111157 ) ;
#106081 = CARTESIAN_POINT ( 'NONE',  ( 18.59999999999999076, 68.92903212821303782, -99.27654326265604823 ) ) ;
#106083 = DIRECTION ( 'NONE',  ( -1.000000000000000000, 2.849773892568378313E-16, -7.728835255496647986E-17 ) ) ;
#106084 = DIRECTION ( 'NONE',  ( -1.000000000000000000, 0.000000000000000000, 0.000000000000000000 ) ) ;
#106085 = DIRECTION ( 'NONE',  ( 6.938893903907223644E-15, -0.9770955615653313941, -0.2128009952263606730 ) ) ;
#106087 = CARTESIAN_POINT ( 'NONE',  ( -16.92280123533699410, 66.05000000001207638, -123.6724751704392702 ) ) ;
#106086 = PRESENTATION_LAYER_ASSIGNMENT (  '', '', ( #97888 ) ) ;
#106088 = FACE_OUTER_BOUND ( 'NONE', #33567, .T. ) ;
#106090 = EDGE_LOOP ( 'NONE', ( #70999, #122113, #83282, #255599 ) ) ;
#106089 = DIRECTION ( 'NONE',  ( 1.000000000000000000, 0.000000000000000000, 0.000000000000000000 ) ) ;
#106091 = CYLINDRICAL_SURFACE ( 'NONE', #76032, 0.1000000000000124678 ) ;
#106092 = DIRECTION ( 'NONE',  ( -0.000000000000000000, -6.982962677686266711E-15, 1.000000000000000000 ) ) ;
#106093 = CARTESIAN_POINT ( 'NONE',  ( -22.59999999999999787, 1.148907358139439339E-11, -201.0000000000015064 ) ) ;
#106094 = CARTESIAN_POINT ( 'NONE',  ( -20.54999999999999716, 68.75000000001230660, -157.7731074845244166 ) ) ;
#106095 = EDGE_CURVE ( 'NONE', #248248, #87594, #73345, .T. ) ;
#106096 = VERTEX_POINT ( 'NONE', #190721 ) ;
#106097 = CARTESIAN_POINT ( 'NONE',  ( 18.50000000000000000, -7.631834139420993424, -210.1304494778855485 ) ) ;
#106098 = CARTESIAN_POINT ( 'NONE',  ( -16.97683810757273193, 66.05000000001201954, -116.2866841969848082 ) ) ;
#106099 = DIRECTION ( 'NONE',  ( 0.000000000000000000, -1.000000000000000000, 0.000000000000000000 ) ) ;
#106100 = EDGE_CURVE ( 'NONE', #216161, #96682, #154182, .T. ) ;
#106101 = DIRECTION ( 'NONE',  ( -1.000000000000000000, -1.652117596168391700E-15, -1.153667551319263085E-29 ) ) ;
#106102 = VECTOR ( 'NONE', #235570, 1000.000000000000114 ) ;
#106103 = VERTEX_POINT ( 'NONE', #249394 ) ;
#106104 = CYLINDRICAL_SURFACE ( 'NONE', #42647, 0.09999999999999939493 ) ;
#106105 = AXIS2_PLACEMENT_3D ( 'NONE', #219117, #20966, #177479 ) ;
#106106 = ORIENTED_EDGE ( 'NONE', *, *, #219615, .T. ) ;
#106107 = CIRCLE ( 'NONE', #6159, 0.09999999999999939493 ) ;
#106108 = DIRECTION ( 'NONE',  ( -1.000000000000000000, 0.000000000000000000, -0.000000000000000000 ) ) ;
#106110 = DIRECTION ( 'NONE',  ( 0.000000000000000000, 0.000000000000000000, 1.000000000000000000 ) ) ;
#106109 = AXIS2_PLACEMENT_3D ( 'NONE', #112254, #251744, #212633 ) ;
#106111 = ADVANCED_FACE ( 'NONE', ( #89004 ), #229812, .T. ) ;
#106112 =( NAMED_UNIT ( * ) SI_UNIT ( $, .STERADIAN. ) SOLID_ANGLE_UNIT ( ) );
#106113 = CARTESIAN_POINT ( 'NONE',  ( -23.15000000000000213, -11.74999999998884448, -164.4000000000000057 ) ) ;
#106114 = VERTEX_POINT ( 'NONE', #112455 ) ;
#106115 = AXIS2_PLACEMENT_3D ( 'NONE', #921, #80454, #117066 ) ;
#106116 = ADVANCED_FACE ( 'NONE', ( #134547 ), #90424, .T. ) ;
#106117 = AXIS2_PLACEMENT_3D ( 'NONE', #240880, #118371, #100044 ) ;
#106119 = EDGE_CURVE ( 'NONE', #170728, #218203, #160916, .T. ) ;
#106118 = DIRECTION ( 'NONE',  ( 0.000000000000000000, -0.1350103645451876666, -0.9908441862701600211 ) ) ;
#106120 = TOROIDAL_SURFACE ( 'NONE', #164422, 0.2000000000000000111, 0.1000000000000000056 ) ;
#106121 = DIRECTION ( 'NONE',  ( 0.000000000000000000, 0.7397890806274223241, 0.6728388485993012091 ) ) ;
#106122 = DIRECTION ( 'NONE',  ( -0.000000000000000000, 0.000000000000000000, 1.000000000000000000 ) ) ;
#106123 = CIRCLE ( 'NONE', #38958, 12.87499999999999822 ) ;
#106124 = FACE_OUTER_BOUND ( 'NONE', #177562, .T. ) ;
#106125 = CARTESIAN_POINT ( 'NONE',  ( 23.24999999999999289, 64.25000000001213607, -136.4231074845243938 ) ) ;
#106126 = EDGE_LOOP ( 'NONE', ( #236975, #35518, #100940, #95609 ) ) ;
#106128 = ORIENTED_EDGE ( 'NONE', *, *, #92323, .T. ) ;
#106127 = CYLINDRICAL_SURFACE ( 'NONE', #165150, 0.1000000000000028644 ) ;
#106129 = EDGE_CURVE ( 'NONE', #255042, #108803, #173754, .T. ) ;
#106130 = AXIS2_PLACEMENT_3D ( 'NONE', #706, #39897, #119412 ) ;
#106131 = ORIENTED_EDGE ( 'NONE', *, *, #93223, .F. ) ;
#106132 = DIRECTION ( 'NONE',  ( 0.000000000000000000, -0.9651348961777157509, 0.2617529984165031243 ) ) ;
#106133 = ORIENTED_EDGE ( 'NONE', *, *, #59171, .T. ) ;
#106134 = CARTESIAN_POINT ( 'NONE',  ( 21.04999999999999361, 61.12590067187060328, -234.3012893943877373 ) ) ;
#106135 = CARTESIAN_POINT ( 'NONE',  ( 22.60000000000000142, 1.115600667400684642E-11, -67.00000000000004263 ) ) ;
#106136 = DIRECTION ( 'NONE',  ( 0.000000000000000000, -0.9654727137038715545, 0.2605042016806676242 ) ) ;
#106137 = ORIENTED_EDGE ( 'NONE', *, *, #22622, .T. ) ;
#106138 = EDGE_CURVE ( 'NONE', #29211, #213820, #116308, .T. ) ;
#106139 = EDGE_CURVE ( 'NONE', #14440, #99302, #165654, .T. ) ;
#106141 = CIRCLE ( 'NONE', #64477, 2.100000000000008527 ) ;
#106140 = DIRECTION ( 'NONE',  ( 1.000000000000000000, 0.000000000000000000, 0.000000000000000000 ) ) ;
#106142 = CARTESIAN_POINT ( 'NONE',  ( -23.25000000000000355, 42.79061499530347845, -240.6131891775583824 ) ) ;
#106143 = DIRECTION ( 'NONE',  ( 1.000000000000000000, 0.000000000000000000, 0.000000000000000000 ) ) ;
#106144 = VECTOR ( 'NONE', #213637, 1000.000000000000000 ) ;
#106145 = EDGE_LOOP ( 'NONE', ( #90585, #159277, #1374, #88197 ) ) ;
#106146 = CARTESIAN_POINT ( 'NONE',  ( -15.55912972643741199, 8.490870273573719373, -146.6500000000000341 ) ) ;
#106148 = ORIENTED_EDGE ( 'NONE', *, *, #162096, .T. ) ;
#106147 = FACE_OUTER_BOUND ( 'NONE', #55712, .T. ) ;
#106149 = CARTESIAN_POINT ( 'NONE',  ( 23.15000000000000213, 84.59626168225550202, -179.4732350016745954 ) ) ;
#106150 = CARTESIAN_POINT ( 'NONE',  ( -21.05000000000000071, 87.75000000001192291, -106.1231074845242262 ) ) ;
#106151 = ORIENTED_EDGE ( 'NONE', *, *, #3047, .T. ) ;
#106152 = LINE ( 'NONE', #162313, #201776 ) ;
#106153 = CARTESIAN_POINT ( 'NONE',  ( -16.91256925476570316, 44.01351207619228489, -235.3144196755796145 ) ) ;
#106154 = CARTESIAN_POINT ( 'NONE',  ( -21.64999999999999858, 61.51843870376554690, -221.1987795346359746 ) ) ;
#106155 = VERTEX_POINT ( 'NONE', #35507 ) ;
#106156 = CARTESIAN_POINT ( 'NONE',  ( -20.64999999999999858, 76.00000000001227818, -157.0481074845243938 ) ) ;
#106157 = EDGE_CURVE ( 'NONE', #61299, #133057, #223873, .T. ) ;
#106158 = EDGE_CURVE ( 'NONE', #170879, #45677, #57284, .T. ) ;
#106159 = LINE ( 'NONE', #201422, #255548 ) ;
#106160 = VECTOR ( 'NONE', #66767, 1000.000000000000114 ) ;
#106161 = VERTEX_POINT ( 'NONE', #195855 ) ;
#106162 = AXIS2_PLACEMENT_3D ( 'NONE', #135402, #214953, #112024 ) ;
#106163 = EDGE_CURVE ( 'NONE', #208514, #187772, #115550, .T. ) ;
#106164 = AXIS2_PLACEMENT_3D ( 'NONE', #158845, #238349, #33785 ) ;
#106165 = ORIENTED_EDGE ( 'NONE', *, *, #216935, .F. ) ;
#106166 = DIRECTION ( 'NONE',  ( -1.000000000000000000, 2.952720810173289112E-16, 2.061873921506763405E-30 ) ) ;
#106167 = AXIS2_PLACEMENT_3D ( 'NONE', #139890, #18682, #60366 ) ;
#106168 = CIRCLE ( 'NONE', #251939, 0.1000000000000002554 ) ;
#106169 = ORIENTED_EDGE ( 'NONE', *, *, #243765, .F. ) ;
#106170 = DIRECTION ( 'NONE',  ( -1.836970198721029934E-16, -1.000000000000000000, -6.982962677686266711E-15 ) ) ;
#106171 = DIRECTION ( 'NONE',  ( -0.000000000000000000, 0.9969158384938637818, -0.07847809223010315804 ) ) ;
#106173 = ORIENTED_EDGE ( 'NONE', *, *, #248754, .T. ) ;
#106172 = LINE ( 'NONE', #241846, #87604 ) ;
#106174 = DIRECTION ( 'NONE',  ( 0.000000000000000000, 0.000000000000000000, -1.000000000000000000 ) ) ;
#106175 = CARTESIAN_POINT ( 'NONE',  ( 20.97224591636398472, 10.62515341617478271, -112.7499259046635984 ) ) ;
#106176 = CARTESIAN_POINT ( 'NONE',  ( 20.84999999999998721, 68.11287320386161070, -224.1382462126928488 ) ) ;
#106177 = FACE_OUTER_BOUND ( 'NONE', #247819, .T. ) ;
#106178 = DIRECTION ( 'NONE',  ( 0.000000000000000000, 0.8814952561688430555, -0.4721928772777346239 ) ) ;
#106179 = DIRECTION ( 'NONE',  ( 0.000000000000000000, 0.000000000000000000, 1.000000000000000000 ) ) ;
#106180 = AXIS2_PLACEMENT_3D ( 'NONE', #151907, #132309, #157034 ) ;
#106181 = EDGE_CURVE ( 'NONE', #162761, #59200, #132299, .T. ) ;
#106182 = DIRECTION ( 'NONE',  ( 0.000000000000000000, 0.9126074666063660468, 0.4088369013363524762 ) ) ;
#106183 = CARTESIAN_POINT ( 'NONE',  ( -20.00857864376270001, 66.85000000001200249, -115.3731074845243683 ) ) ;
#106185 = ORIENTED_EDGE ( 'NONE', *, *, #161934, .F. ) ;
#106184 = DIRECTION ( 'NONE',  ( -1.000000000000000000, 0.000000000000000000, -0.000000000000000000 ) ) ;
#106186 = CARTESIAN_POINT ( 'NONE',  ( -21.05000000000000071, 1.115600667400684642E-11, -74.90000000000004832 ) ) ;
#106187 = AXIS2_PLACEMENT_3D ( 'NONE', #143442, #106874, #166900 ) ;
#106188 = ORIENTED_EDGE ( 'NONE', *, *, #73169, .F. ) ;
#106189 = EDGE_CURVE ( 'NONE', #143318, #67614, #32396, .T. ) ;
#106190 = DIRECTION ( 'NONE',  ( -0.7071067811865475727, 0.7071067811865475727, 4.937700262164531476E-15 ) ) ;
#106192 = EDGE_CURVE ( 'NONE', #29625, #162728, #95440, .T. ) ;
#106191 = DIRECTION ( 'NONE',  ( 1.000000000000000000, 0.000000000000000000, 0.000000000000000000 ) ) ;
#106193 = CARTESIAN_POINT ( 'NONE',  ( 20.94999999999999929, 1.115650877919449413E-11, -96.40000000000003411 ) ) ;
#106194 = EDGE_CURVE ( 'NONE', #117242, #71417, #24006, .T. ) ;
#106195 = CIRCLE ( 'NONE', #127066, 0.09999999999998898659 ) ;
#106196 = CARTESIAN_POINT ( 'NONE',  ( 20.85000000000000142, 7.128833340094563376, -233.7327013124401276 ) ) ;
#106197 = DIRECTION ( 'NONE',  ( -1.000000000000000000, 0.000000000000000000, 0.000000000000000000 ) ) ;
#106198 = ADVANCED_FACE ( 'NONE', ( #99275 ), #1469, .F. ) ;
#106199 = EDGE_LOOP ( 'NONE', ( #134240, #246822, #94798, #95986 ) ) ;
#106200 = PLANE ( 'NONE',  #6382 ) ;
#106201 = DIRECTION ( 'NONE',  ( 1.000000000000000000, 0.000000000000000000, 0.000000000000000000 ) ) ;
#106202 = ORIENTED_EDGE ( 'NONE', *, *, #31392, .T. ) ;
#106204 = ADVANCED_FACE ( 'NONE', ( #57584 ), #60154, .T. ) ;
#106203 = FACE_OUTER_BOUND ( 'NONE', #257719, .T. ) ;
#106205 = EDGE_CURVE ( 'NONE', #212700, #32720, #61585, .T. ) ;
#106206 = CARTESIAN_POINT ( 'NONE',  ( -18.59999999999999787, 102.4393534156134962, -185.3815988770167280 ) ) ;
#106207 = ORIENTED_EDGE ( 'NONE', *, *, #17088, .F. ) ;
#106208 = CARTESIAN_POINT ( 'NONE',  ( -16.86578989773641624, 66.01519019875379968, -190.9877723711466615 ) ) ;
#106209 = ORIENTED_EDGE ( 'NONE', *, *, #174879, .F. ) ;
#106210 = EDGE_CURVE ( 'NONE', #230417, #212700, #3113, .T. ) ;
#106211 = CARTESIAN_POINT ( 'NONE',  ( -15.06774609480955363, 9.417651958852161442, -48.85878739244044056 ) ) ;
#106212 = ORIENTED_EDGE ( 'NONE', *, *, #64920, .T. ) ;
#106213 = DIRECTION ( 'NONE',  ( -1.000000000000000000, -2.952720810173289112E-16, 0.000000000000000000 ) ) ;
#106214 = DIRECTION ( 'NONE',  ( -1.000000000000000000, 0.000000000000000000, 0.000000000000000000 ) ) ;
#106215 = ORIENTED_EDGE ( 'NONE', *, *, #253126, .F. ) ;
#106216 = ORIENTED_EDGE ( 'NONE', *, *, #247110, .T. ) ;
#106217 = DIRECTION ( 'NONE',  ( 1.284434275755705296E-16, -0.7071067811865471286, 0.7071067811865479058 ) ) ;
#106219 = ORIENTED_EDGE ( 'NONE', *, *, #215653, .F. ) ;
#106218 = CARTESIAN_POINT ( 'NONE',  ( 14.87567385445977663, 9.430764995433474240, -48.73053739475045631 ) ) ;
#106220 = EDGE_CURVE ( 'NONE', #13368, #112033, #219779, .T. ) ;
#106221 = DIRECTION ( 'NONE',  ( 1.000000000000000000, 2.885090398161910739E-16, 6.283419270304611573E-17 ) ) ;
#106222 = AXIS2_PLACEMENT_3D ( 'NONE', #105003, #45080, #123342 ) ;
#106223 = ADVANCED_FACE ( 'NONE', ( #234963 ), #135836, .T. ) ;
#106224 = EDGE_LOOP ( 'NONE', ( #127850, #183176, #205737 ) ) ;
#106225 = EDGE_CURVE ( 'NONE', #156269, #248318, #15648, .T. ) ;
#106226 = AXIS2_PLACEMENT_3D ( 'NONE', #242428, #200749, #222867 ) ;
#106227 = VERTEX_POINT ( 'NONE', #255758 ) ;
#106228 = LINE ( 'NONE', #209198, #120174 ) ;
#106229 = FACE_OUTER_BOUND ( 'NONE', #132585, .T. ) ;
#106231 = EDGE_CURVE ( 'NONE', #176771, #185866, #186490, .T. ) ;
#106230 = FACE_OUTER_BOUND ( 'NONE', #83470, .T. ) ;
#106232 = FACE_OUTER_BOUND ( 'NONE', #211591, .T. ) ;
#106233 = LINE ( 'NONE', #5852, #256109 ) ;
#106234 = ADVANCED_FACE ( 'NONE', ( #217937 ), #53206, .T. ) ;
#106235 = LINE ( 'NONE', #3283, #171303 ) ;
#106236 = ORIENTED_EDGE ( 'NONE', *, *, #245882, .F. ) ;
#106237 = CARTESIAN_POINT ( 'NONE',  ( -16.92563707711778775, 66.03100930561575410, -182.6423491850004552 ) ) ;
#106238 = CARTESIAN_POINT ( 'NONE',  ( -20.94999999999999929, -1.261786168553869603, -75.08649896354552311 ) ) ;
#106239 = DIRECTION ( 'NONE',  ( 1.000000000000000000, 0.000000000000000000, 0.000000000000000000 ) ) ;
#106240 = CARTESIAN_POINT ( 'NONE',  ( 21.14999999999999858, 63.99342642423710714, -222.3880800784493772 ) ) ;
#106241 = EDGE_LOOP ( 'NONE', ( #2133, #222039 ) ) ;
#106242 = DIRECTION ( 'NONE',  ( 0.000000000000000000, 0.000000000000000000, -1.000000000000000000 ) ) ;
#106243 = VERTEX_POINT ( 'NONE', #97985 ) ;
#106244 = CARTESIAN_POINT ( 'NONE',  ( 13.76927104934456914, 9.455987233623899257, -115.5115311668978677 ) ) ;
#106245 = ORIENTED_EDGE ( 'NONE', *, *, #99216, .F. ) ;
#106246 = COLOUR_RGB ( '', 0.09019608, 0.27058824, 0.51372549) ;
#106247 = CIRCLE ( 'NONE', #127116, 0.09999999999998898659 ) ;
#106248 = CARTESIAN_POINT ( 'NONE',  ( -22.47071067811865319, 68.27992525551462677, -203.6221999392270448 ) ) ;
#106249 = CARTESIAN_POINT ( 'NONE',  ( -21.45000000000000284, 68.29142135624915966, -90.77310748452437394 ) ) ;
#106250 = ORIENTED_EDGE ( 'NONE', *, *, #195130, .F. ) ;
#106251 = ORIENTED_EDGE ( 'NONE', *, *, #107694, .F. ) ;
#106253 = ORIENTED_EDGE ( 'NONE', *, *, #125002, .T. ) ;
#106252 = FACE_OUTER_BOUND ( 'NONE', #37129, .T. ) ;
#106254 = EDGE_CURVE ( 'NONE', #231898, #208732, #65670, .T. ) ;
#106255 = DIRECTION ( 'NONE',  ( 1.000000000000000000, -0.000000000000000000, -0.000000000000000000 ) ) ;
#106256 = ORIENTED_EDGE ( 'NONE', *, *, #135206, .T. ) ;
#106257 = FACE_OUTER_BOUND ( 'NONE', #59253, .T. ) ;
#106258 = CARTESIAN_POINT ( 'NONE',  ( -21.05000000000000426, 11.60000000001115872, -174.4282032302755283 ) ) ;
#106260 = ORIENTED_EDGE ( 'NONE', *, *, #66953, .T. ) ;
#106259 = EDGE_CURVE ( 'NONE', #204570, #195198, #24919, .T. ) ;
#106261 = CARTESIAN_POINT ( 'NONE',  ( -18.59999999999999787, 52.81534179157634412, -244.1198638051726277 ) ) ;
#106263 = FACE_OUTER_BOUND ( 'NONE', #110551, .T. ) ;
#106262 = VECTOR ( 'NONE', #118807, 1000.000000000000000 ) ;
#106264 = TOROIDAL_SURFACE ( 'NONE', #239571, 12.77499999999999858, 0.1000000000000000056 ) ;
#106265 = VERTEX_POINT ( 'NONE', #183968 ) ;
#106266 = VECTOR ( 'NONE', #203890, 1000.000000000000000 ) ;
#106267 = AXIS2_PLACEMENT_3D ( 'NONE', #120104, #40572, #114937 ) ;
#106268 =( GEOMETRIC_REPRESENTATION_CONTEXT ( 3 ) GLOBAL_UNCERTAINTY_ASSIGNED_CONTEXT ( ( #188595 ) ) GLOBAL_UNIT_ASSIGNED_CONTEXT ( ( #156740, #238818, #89663 ) ) REPRESENTATION_CONTEXT ( 'NONE', 'WORKASPACE' ) );
#106269 = EDGE_CURVE ( 'NONE', #257620, #15539, #36518, .T. ) ;
#106270 = FACE_OUTER_BOUND ( 'NONE', #95959, .T. ) ;
#106272 = EDGE_LOOP ( 'NONE', ( #143772, #179343, #203404, #247939 ) ) ;
#106271 = CARTESIAN_POINT ( 'NONE',  ( -18.69999999999999929, -8.150000000000005684, 10.52591260281975138 ) ) ;
#106273 = CYLINDRICAL_SURFACE ( 'NONE', #95034, 3.999999999999996447 ) ;
#106274 = CARTESIAN_POINT ( 'NONE',  ( 23.25000000000000000, 87.65000000001172964, -81.27310748452423184 ) ) ;
#106275 = FACE_OUTER_BOUND ( 'NONE', #163292, .T. ) ;
#106277 = LINE ( 'NONE', #25495, #91044 ) ;
#106276 = DIRECTION ( 'NONE',  ( 1.000000000000000000, 0.000000000000000000, 0.000000000000000000 ) ) ;
#106278 = CARTESIAN_POINT ( 'NONE',  ( 21.05000000000000071, 39.17748843728426067, -236.9342652831892622 ) ) ;
#106279 = CARTESIAN_POINT ( 'NONE',  ( -16.97683809663752186, 66.15000000001261071, -190.8731074845244393 ) ) ;
#106280 = CYLINDRICAL_SURFACE ( 'NONE', #130793, 0.09999999999999939493 ) ;
#106281 = ADVANCED_FACE ( 'NONE', ( #206102 ), #223053, .T. ) ;
#106282 = DIRECTION ( 'NONE',  ( -1.836970198721029934E-16, 0.9770955615653316162, 0.2128009952263604232 ) ) ;
#106283 = CIRCLE ( 'NONE', #202174, 0.6000000000000064171 ) ;
#106284 = ORIENTED_EDGE ( 'NONE', *, *, #91717, .T. ) ;
#106285 = AXIS2_PLACEMENT_3D ( 'NONE', #153825, #132938, #115934 ) ;
#106286 = AXIS2_PLACEMENT_3D ( 'NONE', #86887, #188574, #126026 ) ;
#106287 = ORIENTED_EDGE ( 'NONE', *, *, #187807, .T. ) ;
#106288 = CARTESIAN_POINT ( 'NONE',  ( -23.49999999999994316, 76.00000000001119815, -36.02310748452479316 ) ) ;
#106289 = ORIENTED_EDGE ( 'NONE', *, *, #141402, .T. ) ;
#106290 = DIRECTION ( 'NONE',  ( 0.000000000000000000, 0.000000000000000000, 1.000000000000000000 ) ) ;
#106291 = AXIS2_PLACEMENT_3D ( 'NONE', #78584, #79850, #76023 ) ;
#106292 = CIRCLE ( 'NONE', #122912, 0.09999999999999939493 ) ;
#106293 = CIRCLE ( 'NONE', #160522, 0.09999999999999986677 ) ;
#106294 = EDGE_LOOP ( 'NONE', ( #144381, #139751, #106452, #10739 ) ) ;
#106295 = CARTESIAN_POINT ( 'NONE',  ( 20.94999027547553894, 65.70673848566998743, -131.0638252334829588 ) ) ;
#106296 = FACE_OUTER_BOUND ( 'NONE', #206754, .T. ) ;
#106297 = ORIENTED_EDGE ( 'NONE', *, *, #65380, .T. ) ;
#106298 = DIRECTION ( 'NONE',  ( 0.000000000000000000, -0.9770955615653553750, -0.2128009952262508719 ) ) ;
#106299 = VERTEX_POINT ( 'NONE', #47000 ) ;
#106300 = ORIENTED_EDGE ( 'NONE', *, *, #242456, .T. ) ;
#106302 = DIRECTION ( 'NONE',  ( -1.000000000000000000, -0.000000000000000000, -0.000000000000000000 ) ) ;
#106301 = CIRCLE ( 'NONE', #139625, 1.500000000000001332 ) ;
#106303 = CARTESIAN_POINT ( 'NONE',  ( -21.08376601933334271, 75.93622398908212290, -109.3650547558000454 ) ) ;
#106305 = ORIENTED_EDGE ( 'NONE', *, *, #199864, .F. ) ;
#106304 = CARTESIAN_POINT ( 'NONE',  ( 21.15000000000000213, 67.21339244341145047, -57.27310748452438105 ) ) ;
#106306 = DIRECTION ( 'NONE',  ( 0.000000000000000000, 0.000000000000000000, 1.000000000000000000 ) ) ;
#106308 = VERTEX_POINT ( 'NONE', #106986 ) ;
#106307 = DIRECTION ( 'NONE',  ( -1.000000000000000000, 0.000000000000000000, -0.000000000000000000 ) ) ;
#106309 = DIRECTION ( 'NONE',  ( 0.7071359030027680737, 0.7070776581709111719, 0.000000000000000000 ) ) ;
#106310 = AXIS2_PLACEMENT_3D ( 'NONE', #199625, #41837, #62668 ) ;
#106311 = CARTESIAN_POINT ( 'NONE',  ( 20.85000000000000142, 77.73670573947964613, -125.0056848969006182 ) ) ;
#106312 = AXIS2_PLACEMENT_3D ( 'NONE', #195075, #192485, #94656 ) ;
#106314 = ORIENTED_EDGE ( 'NONE', *, *, #129940, .T. ) ;
#106313 = DIRECTION ( 'NONE',  ( 1.000000000000000000, 0.000000000000000000, 0.000000000000000000 ) ) ;
#106315 = CARTESIAN_POINT ( 'NONE',  ( 18.56579813702275317, 10.33025634372637924, -173.0870929282638997 ) ) ;
#106316 = EDGE_CURVE ( 'NONE', #222282, #134996, #39471, .T. ) ;
#106317 = CARTESIAN_POINT ( 'NONE',  ( -16.97683809663753252, 9.950000000011138823, -113.7715247686699769 ) ) ;
#106319 = DIRECTION ( 'NONE',  ( 0.000000000000000000, 0.2617529984164506107, 0.9651348961777299618 ) ) ;
#106318 = CARTESIAN_POINT ( 'NONE',  ( -20.94999999999999929, 7.031312794766356511, -171.1091509382273159 ) ) ;
#106320 = CARTESIAN_POINT ( 'NONE',  ( -21.05000000000000071, 1.115600667400684642E-11, -134.0000000000000284 ) ) ;
#106321 = LINE ( 'NONE', #122067, #22658 ) ;
#106322 = DIRECTION ( 'NONE',  ( 0.000000000000000000, 1.000000000000000000, -0.000000000000000000 ) ) ;
#106323 = FACE_OUTER_BOUND ( 'NONE', #35397, .T. ) ;
#106324 = ORIENTED_EDGE ( 'NONE', *, *, #31853, .F. ) ;
#106325 = VERTEX_POINT ( 'NONE', #221779 ) ;
#106326 = ORIENTED_EDGE ( 'NONE', *, *, #150629, .F. ) ;
#106327 = DIRECTION ( 'NONE',  ( 1.000000000000000000, -0.000000000000000000, -0.000000000000000000 ) ) ;
#106328 = ORIENTED_EDGE ( 'NONE', *, *, #145019, .T. ) ;
#106329 = DIRECTION ( 'NONE',  ( 0.000000000000000000, -1.000000000000000000, -7.105427357601001859E-15 ) ) ;
#106330 = ORIENTED_EDGE ( 'NONE', *, *, #161012, .F. ) ;
#106331 = EDGE_CURVE ( 'NONE', #223322, #183920, #203536, .T. ) ;
#106332 = DIRECTION ( 'NONE',  ( 0.000000000000000000, 1.000000000000000000, 7.272083257015735086E-15 ) ) ;
#106333 = CARTESIAN_POINT ( 'NONE',  ( 18.60000000000000853, -9.364236010355613260, -40.68025440072462118 ) ) ;
#106334 = EDGE_CURVE ( 'NONE', #126780, #51098, #135953, .T. ) ;
#106335 = TOROIDAL_SURFACE ( 'NONE', #198129, 11.65000000000000036, 0.1000000000000000056 ) ;
#106336 = AXIS2_PLACEMENT_3D ( 'NONE', #187090, #42420, #142778 ) ;
#106337 = EDGE_LOOP ( 'NONE', ( #61266, #46971, #4138, #188085 ) ) ;
#106338 = CARTESIAN_POINT ( 'NONE',  ( 14.22916352759893854, 9.457410930301318075, -152.4999159087463170 ) ) ;
#106339 = TOROIDAL_SURFACE ( 'NONE', #89791, 0.2000000000000000111, 0.1000000000000000056 ) ;
#106340 = EDGE_CURVE ( 'NONE', #18611, #176425, #110848, .T. ) ;
#106341 = ORIENTED_EDGE ( 'NONE', *, *, #150074, .T. ) ;
#106342 = EDGE_LOOP ( 'NONE', ( #103787, #231276, #1893, #257711 ) ) ;
#106343 = ORIENTED_EDGE ( 'NONE', *, *, #78130, .F. ) ;
#106344 = TOROIDAL_SURFACE ( 'NONE', #93902, 0.2000000000000000111, 0.1000000000000000056 ) ;
#106345 = ADVANCED_FACE ( 'NONE', ( #190411 ), #191708, .F. ) ;
#106346 = DIRECTION ( 'NONE',  ( 1.000000000000000000, 7.304098846218134667E-16, 0.000000000000000000 ) ) ;
#106347 = DIRECTION ( 'NONE',  ( 0.000000000000000000, 0.000000000000000000, -1.000000000000000000 ) ) ;
#106348 = AXIS2_PLACEMENT_3D ( 'NONE', #47022, #126585, #27527 ) ;
#106349 = DIRECTION ( 'NONE',  ( 0.000000000000000000, 0.000000000000000000, 1.000000000000000000 ) ) ;
#106351 = ADVANCED_FACE ( 'NONE', ( #211237 ), #169774, .T. ) ;
#106350 = CARTESIAN_POINT ( 'NONE',  ( 18.52928932188134326, 65.72071067813087097, -145.3145288407617386 ) ) ;
#106352 = DIRECTION ( 'NONE',  ( 0.000000000000000000, -0.9770955615653316162, -0.2128009952263604232 ) ) ;
#106353 = CARTESIAN_POINT ( 'NONE',  ( -21.04999999999994387, 65.35000000001120668, -4.423107484524790856 ) ) ;
#106355 = DIRECTION ( 'NONE',  ( 1.000000000000000000, 0.000000000000000000, 0.000000000000000000 ) ) ;
#106354 = LINE ( 'NONE', #226300, #145550 ) ;
#106356 = DIRECTION ( 'NONE',  ( 0.000000000000000000, 0.000000000000000000, 1.000000000000000000 ) ) ;
#106358 = VERTEX_POINT ( 'NONE', #11781 ) ;
#106357 = DIRECTION ( 'NONE',  ( 1.000000000000000000, -0.000000000000000000, 0.000000000000000000 ) ) ;
#106360 = DIRECTION ( 'NONE',  ( -1.000000000000000000, 0.000000000000000000, 0.000000000000000000 ) ) ;
#106359 = CARTESIAN_POINT ( 'NONE',  ( -18.40000000000000213, 64.58541674041201475, -82.17310748452442226 ) ) ;
#106361 = EDGE_CURVE ( 'NONE', #19723, #173980, #86489, .T. ) ;
#106362 = DIRECTION ( 'NONE',  ( -1.000000000000000000, -0.000000000000000000, -0.000000000000000000 ) ) ;
#106363 = AXIS2_PLACEMENT_3D ( 'NONE', #184245, #68155, #182982 ) ;
#106364 = ORIENTED_EDGE ( 'NONE', *, *, #192329, .F. ) ;
#106365 = AXIS2_PLACEMENT_3D ( 'NONE', #195244, #156120, #174421 ) ;
#106366 = CARTESIAN_POINT ( 'NONE',  ( 23.14999999999999858, 5.900000000011162093, -56.78090023534362984 ) ) ;
#106367 = CARTESIAN_POINT ( 'NONE',  ( 20.04142135391667168, 64.25000000001148237, -44.82060061889435332 ) ) ;
#106368 = ORIENTED_EDGE ( 'NONE', *, *, #33504, .T. ) ;
#106369 = ADVANCED_FACE ( 'NONE', ( #108293 ), #73049, .F. ) ;
#106370 = AXIS2_PLACEMENT_3D ( 'NONE', #51873, #68915, #128879 ) ;
#106371 = CARTESIAN_POINT ( 'NONE',  ( -18.59999999999999787, -9.499999999988842703, -79.15000000000004832 ) ) ;
#106372 = DIRECTION ( 'NONE',  ( 0.000000000000000000, 6.982962677686266711E-15, -1.000000000000000000 ) ) ;
#106373 = DIRECTION ( 'NONE',  ( -2.827886303505249259E-16, 0.8660254037844412611, 0.4999999999999956701 ) ) ;
#106374 = ORIENTED_EDGE ( 'NONE', *, *, #84568, .T. ) ;
#106375 = VERTEX_POINT ( 'NONE', #226946 ) ;
#106376 = DIRECTION ( 'NONE',  ( 0.000000000000000000, 0.8814952561688438326, -0.4721928772777334582 ) ) ;
#106377 = ORIENTED_EDGE ( 'NONE', *, *, #39429, .F. ) ;
#106378 = CARTESIAN_POINT ( 'NONE',  ( 22.00411653962179059, 7.253442868381116959, -66.90096189419941197 ) ) ;
#106379 = FACE_OUTER_BOUND ( 'NONE', #244623, .T. ) ;
#106380 = CARTESIAN_POINT ( 'NONE',  ( 18.45139536634708932, 85.48608172029291552, -62.88259586671362911 ) ) ;
#106381 = DIRECTION ( 'NONE',  ( 1.000000000000000000, -4.851622311275599093E-17, 1.082981191754466866E-16 ) ) ;
#106382 = EDGE_LOOP ( 'NONE', ( #48257, #678, #217896, #182097 ) ) ;
#106383 = EDGE_CURVE ( 'NONE', #55100, #234093, #69786, .T. ) ;
#106384 = DIRECTION ( 'NONE',  ( -1.000000000000000000, 0.000000000000000000, -0.000000000000000000 ) ) ;
#106385 = CARTESIAN_POINT ( 'NONE',  ( -21.05000000000000071, 6.540656951712397138, -100.6000000000000369 ) ) ;
#106386 = CARTESIAN_POINT ( 'NONE',  ( 20.94999999999999929, 29.00069016757795026, -237.9048565010683376 ) ) ;
#106387 = CARTESIAN_POINT ( 'NONE',  ( 20.85000000000000142, 78.57744179526842743, -232.8011145694030972 ) ) ;
#106388 = CIRCLE ( 'NONE', #256183, 0.1000000000000028644 ) ;
#106389 = ORIENTED_EDGE ( 'NONE', *, *, #49810, .T. ) ;
#106390 = AXIS2_PLACEMENT_3D ( 'NONE', #168772, #27954, #146558 ) ;
#106391 = CARTESIAN_POINT ( 'NONE',  ( 20.86777300164945004, 10.33200063079656417, -39.09316749566428939 ) ) ;
#106392 = ADVANCED_FACE ( 'NONE', ( #152582 ), #249719, .T. ) ;
#106394 = ORIENTED_EDGE ( 'NONE', *, *, #21573, .F. ) ;
#106393 = CARTESIAN_POINT ( 'NONE',  ( 22.39999999999999503, 12.54173083476182882, -223.4160622903444562 ) ) ;
#106395 = CARTESIAN_POINT ( 'NONE',  ( 21.05000000000000071, 74.65091558138459504, -61.53660852097885225 ) ) ;
#106396 = CARTESIAN_POINT ( 'NONE',  ( 18.41789779300689744, 78.24072138699057177, -231.5548841640768671 ) ) ;
#106397 = DIRECTION ( 'NONE',  ( 0.000000000000000000, 0.2617529984165152257, 0.9651348961777124202 ) ) ;
#106398 = LINE ( 'NONE', #185963, #17241 ) ;
#106399 = DIRECTION ( 'NONE',  ( 0.000000000000000000, 0.000000000000000000, 1.000000000000000000 ) ) ;
#106400 = DIRECTION ( 'NONE',  ( -0.000000000000000000, -0.000000000000000000, 1.000000000000000000 ) ) ;
#106401 = ORIENTED_EDGE ( 'NONE', *, *, #85763, .F. ) ;
#106402 = CARTESIAN_POINT ( 'NONE',  ( -20.94999999999999929, 11.60000000001115161, -140.9282032302755852 ) ) ;
#106403 = DIRECTION ( 'NONE',  ( 0.000000000000000000, 0.4999999999999949485, -0.8660254037844415942 ) ) ;
#106404 = ADVANCED_FACE ( 'NONE', ( #9182 ), #74089, .T. ) ;
#106405 = AXIS2_PLACEMENT_3D ( 'NONE', #200004, #106005, #86435 ) ;
#106406 = DIRECTION ( 'NONE',  ( 0.000000000000000000, 0.000000000000000000, 1.000000000000000000 ) ) ;
#106407 = DIRECTION ( 'NONE',  ( 0.000000000000000000, 0.000000000000000000, 1.000000000000000000 ) ) ;
#106408 = EDGE_CURVE ( 'NONE', #8334, #53190, #44831, .T. ) ;
#106409 = ORIENTED_EDGE ( 'NONE', *, *, #176494, .F. ) ;
#106410 = EDGE_LOOP ( 'NONE', ( #110421, #229910, #177545, #216435 ) ) ;
#106411 = CARTESIAN_POINT ( 'NONE',  ( -20.54999999999999716, 7.150000000011155876, -155.1500000000000057 ) ) ;
#106413 = CARTESIAN_POINT ( 'NONE',  ( 21.93340585898238260, 1.115541036281197940E-11, -126.6758529778678763 ) ) ;
#106412 = CIRCLE ( 'NONE', #193938, 0.09999999999999530098 ) ;
#106414 = DIRECTION ( 'NONE',  ( 1.000000000000000000, 0.000000000000000000, 0.000000000000000000 ) ) ;
#106415 = ADVANCED_FACE ( 'NONE', ( #112160 ), #49596, .T. ) ;
#106416 = CARTESIAN_POINT ( 'NONE',  ( 20.95000000000005258, 66.15000000001120384, -4.623107484524796362 ) ) ;
#106417 = DIRECTION ( 'NONE',  ( -1.000000000000000000, 0.000000000000000000, -0.000000000000000000 ) ) ;
#106418 = ADVANCED_FACE ( 'NONE', ( #130405 ), #94889, .T. ) ;
#106420 = ADVANCED_FACE ( 'NONE', ( #70483 ), #240637, .T. ) ;
#106419 = DIRECTION ( 'NONE',  ( 0.000000000000000000, -0.8660254037844377084, -0.5000000000000016653 ) ) ;
#106421 = LINE ( 'NONE', #4752, #228708 ) ;
#106422 = PRESENTATION_LAYER_ASSIGNMENT (  '', '', ( #202141 ) ) ;
#106423 = AXIS2_PLACEMENT_3D ( 'NONE', #56385, #16024, #176378 ) ;
#106424 = ORIENTED_EDGE ( 'NONE', *, *, #238598, .T. ) ;
#106425 = DIRECTION ( 'NONE',  ( 0.000000000000000000, 0.1575844902526835067, 0.9875055080513738259 ) ) ;
#106426 = ADVANCED_FACE ( 'NONE', ( #31355 ), #76850, .F. ) ;
#106427 = ORIENTED_EDGE ( 'NONE', *, *, #250212, .T. ) ;
#106428 = DIRECTION ( 'NONE',  ( 0.000000000000000000, 0.8660254037844420383, -0.4999999999999943379 ) ) ;
#106429 = DIRECTION ( 'NONE',  ( -1.000000000000000000, 0.000000000000000000, -0.000000000000000000 ) ) ;
#106430 = DIRECTION ( 'NONE',  ( 0.000000000000000000, 0.000000000000000000, -1.000000000000000000 ) ) ;
#106431 = CARTESIAN_POINT ( 'NONE',  ( -16.78569801330232636, 9.947933733124651567, -46.15691290534750379 ) ) ;
#106432 = CARTESIAN_POINT ( 'NONE',  ( -18.40000000000000213, 64.52132590001160395, -45.29780070086501098 ) ) ;
#106433 = DIRECTION ( 'NONE',  ( -1.000000000000000000, 0.000000000000000000, 0.000000000000000000 ) ) ;
#106434 = DIRECTION ( 'NONE',  ( 1.000000000000000000, 0.000000000000000000, 0.000000000000000000 ) ) ;
#106435 = DIRECTION ( 'NONE',  ( 0.000000000000000000, -0.9651348961777157509, 0.2617529984165031243 ) ) ;
#106436 = DIRECTION ( 'NONE',  ( -1.000000000000000000, -0.000000000000000000, -0.000000000000000000 ) ) ;
#106437 = DIRECTION ( 'NONE',  ( -1.000000000000000000, -0.000000000000000000, -0.000000000000000000 ) ) ;
#106438 = CIRCLE ( 'NONE', #148160, 6.258578643762701788 ) ;
#106439 = VECTOR ( 'NONE', #154982, 1000.000000000000000 ) ;
#106441 = DIRECTION ( 'NONE',  ( -1.836970198721029934E-16, 1.000000000000000000, 0.000000000000000000 ) ) ;
#106440 = AXIS2_PLACEMENT_3D ( 'NONE', #43552, #147789, #162231 ) ;
#106442 = AXIS2_PLACEMENT_3D ( 'NONE', #83473, #104330, #221707 ) ;
#106443 = ORIENTED_EDGE ( 'NONE', *, *, #122007, .T. ) ;
#106444 =( GEOMETRIC_REPRESENTATION_CONTEXT ( 3 ) GLOBAL_UNCERTAINTY_ASSIGNED_CONTEXT ( ( #186040 ) ) GLOBAL_UNIT_ASSIGNED_CONTEXT ( ( #58860, #82270, #241394 ) ) REPRESENTATION_CONTEXT ( 'NONE', 'WORKASPACE' ) );
#106445 = FACE_OUTER_BOUND ( 'NONE', #84672, .T. ) ;
#106446 = ADVANCED_FACE ( 'NONE', ( #215086 ), #19462, .T. ) ;
#106447 = ADVANCED_FACE ( 'NONE', ( #195550 ), #100242, .F. ) ;
#106448 = ORIENTED_EDGE ( 'NONE', *, *, #178076, .T. ) ;
#106449 = DIRECTION ( 'NONE',  ( -1.000000000000000000, 0.000000000000000000, 0.000000000000000000 ) ) ;
#106450 = PLANE ( 'NONE',  #231564 ) ;
#106451 = LINE ( 'NONE', #244694, #134624 ) ;
#106452 = ORIENTED_EDGE ( 'NONE', *, *, #177489, .F. ) ;
#106453 = CARTESIAN_POINT ( 'NONE',  ( 18.41832399655377372, -9.682403266662264585, -174.1568436200283543 ) ) ;
#106454 = DIRECTION ( 'NONE',  ( 0.000000000000000000, 0.9994937237965569876, 0.03181660087583042945 ) ) ;
#106455 = EDGE_CURVE ( 'NONE', #243325, #79959, #36490, .T. ) ;
#106456 = ORIENTED_EDGE ( 'NONE', *, *, #100178, .T. ) ;
#106457 = CIRCLE ( 'NONE', #152320, 0.4000000000000045186 ) ;
#106458 = COLOUR_RGB ( '', 0.40784314, 0.44705882, 0.49803922) ;
#106459 = AXIS2_PLACEMENT_3D ( 'NONE', #134100, #177121, #94983 ) ;
#106460 = DIRECTION ( 'NONE',  ( 0.000000000000000000, 0.1335171055202867274, 0.9910465087640866200 ) ) ;
#106461 = ORIENTED_EDGE ( 'NONE', *, *, #53034, .T. ) ;
#106462 = AXIS2_PLACEMENT_3D ( 'NONE', #228374, #204932, #87550 ) ;
#106463 = DIRECTION ( 'NONE',  ( -1.000000000000000000, -0.000000000000000000, 0.000000000000000000 ) ) ;
#106465 =( BOUNDED_SURFACE ( )  B_SPLINE_SURFACE ( 3, 2, ( 
 ( #174949, #191918, #151504 ),
 ( #195766, #91507, #35419 ),
 ( #135749, #172372, #51051 ),
 ( #75795, #234874, #130624 ),
 ( #210179, #31565, #176196 ),
 ( #94056, #70685, #73257 ),
 ( #52351, #56205, #13260 ),
 ( #232322, #111062, #114918 ),
 ( #215296, #250565, #190624 ),
 ( #71949, #36699, #92773 ),
 ( #113631, #231037, #214024 ),
 ( #74555, #251850, #152795 ) ),
 .UNSPECIFIED., .F., .F., .F. ) 
 B_SPLINE_SURFACE_WITH_KNOTS ( ( 4, 2, 2, 2, 2, 4 ),
 ( 3, 3 ),
 ( 3.174653483277204646, 3.943930578431714018, 4.713207673586222946, 5.482484768740731873, 5.867123316317986337, 6.251761863895240801 ),
 ( 0.000000000000000000, 1.000000000000000000 ),
 .UNSPECIFIED. ) 
 GEOMETRIC_REPRESENTATION_ITEM ( )  RATIONAL_B_SPLINE_SURFACE ( (
 ( 1.000000000000000000, 0.8659465255642335713, 1.000000000000000000),
 ( 1.000000000000000000, 0.8648614068459831161, 1.000000000000000000),
 ( 1.000000000000000000, 0.8489031841361811548, 1.000000000000000000),
 ( 1.000000000000000000, 0.7927507630123762361, 1.000000000000000000),
 ( 1.000000000000000000, 0.7523013859009685111, 1.000000000000000000),
 ( 1.000000000000000000, 0.6616226951196223505, 1.000000000000000000),
 ( 1.000000000000000000, 0.6112214368956626620, 1.000000000000000000),
 ( 1.000000000000000000, 0.5507684314381751101, 1.000000000000000000),
 ( 1.000000000000000000, 0.5333267243066852625, 1.000000000000000000),
 ( 1.000000000000000000, 0.5084565446564963676, 1.000000000000000000),
 ( 1.000000000000000000, 0.5010722703387235910, 1.000000000000000000),
 ( 1.000000000000000000, 0.5001234037138085897, 1.000000000000000000) ) ) 
 REPRESENTATION_ITEM ( '' )  SURFACE ( )  );
#106464 = CARTESIAN_POINT ( 'NONE',  ( -20.64999999999999858, 4.250000000011156409, -112.8500000000000369 ) ) ;
#106466 = CARTESIAN_POINT ( 'NONE',  ( 22.50000000000000000, 0.1000000000111554016, -88.85042919245522341 ) ) ;
#106468 = VECTOR ( 'NONE', #198226, 1000.000000000000000 ) ;
#106467 = DIRECTION ( 'NONE',  ( 0.000000000000000000, 0.000000000000000000, -1.000000000000000000 ) ) ;
#106470 = FACE_OUTER_BOUND ( 'NONE', #124206, .T. ) ;
#106469 = VECTOR ( 'NONE', #97831, 1000.000000000000000 ) ;
#106471 = AXIS2_PLACEMENT_3D ( 'NONE', #180086, #155414, #54963 ) ;
#106472 = CARTESIAN_POINT ( 'NONE',  ( 21.30000000000002558, 36.65892442174472876, -249.5511627012454596 ) ) ;
#106473 = DIRECTION ( 'NONE',  ( 0.000000000000000000, 0.000000000000000000, -1.000000000000000000 ) ) ;
#106474 = DIRECTION ( 'NONE',  ( -1.000000000000000000, -0.000000000000000000, -0.000000000000000000 ) ) ;
#106475 = CARTESIAN_POINT ( 'NONE',  ( -23.15000000000000213, 74.00000000001259082, -190.7984855617622770 ) ) ;
#106477 = EDGE_LOOP ( 'NONE', ( #179558, #98842, #95615, #39748 ) ) ;
#106476 = CARTESIAN_POINT ( 'NONE',  ( 23.25000000000000000, -9.599999999988845900, -110.3939691226524786 ) ) ;
#106478 = ORIENTED_EDGE ( 'NONE', *, *, #54762, .F. ) ;
#106479 = DIRECTION ( 'NONE',  ( -0.000000000000000000, 1.000000000000000000, 6.982962677686266711E-15 ) ) ;
#106481 = ORIENTED_EDGE ( 'NONE', *, *, #232902, .F. ) ;
#106480 = LINE ( 'NONE', #9982, #139172 ) ;
#106482 = EDGE_CURVE ( 'NONE', #134658, #115551, #144952, .T. ) ;
#106483 = ORIENTED_EDGE ( 'NONE', *, *, #233274, .F. ) ;
#106484 = DIRECTION ( 'NONE',  ( 0.7071067811865474617, 0.7071067811865474617, 0.000000000000000000 ) ) ;
#106485 = DIRECTION ( 'NONE',  ( 1.000000000000000000, 0.000000000000000000, 0.000000000000000000 ) ) ;
#106486 = VECTOR ( 'NONE', #7502, 1000.000000000000000 ) ;
#106488 =( BOUNDED_SURFACE ( )  B_SPLINE_SURFACE ( 3, 2, ( 
 ( #237036, #179644, #196614 ),
 ( #100057, #19269, #220037 ),
 ( #140482, #101315, #58363 ),
 ( #97487, #20574, #120964 ) ),
 .UNSPECIFIED., .F., .F., .F. ) 
 B_SPLINE_SURFACE_WITH_KNOTS ( ( 4, 4 ),
 ( 3, 3 ),
 ( 5.204170427930421283E-18, 0.001979672783031532438 ),
 ( 0.000000000000000000, 1.000000000000000000 ),
 .UNSPECIFIED. ) 
 GEOMETRIC_REPRESENTATION_ITEM ( )  RATIONAL_B_SPLINE_SURFACE ( (
 ( 1.000000000000000000, 0.7103081912008247789, 1.000000000000000000),
 ( 1.000000000000000000, 0.7104998333562062562, 1.000000000000000000),
 ( 1.000000000000000000, 0.7107238315751961411, 1.000000000000000000),
 ( 1.000000000000000000, 0.7110073749541059307, 1.000000000000000000) ) ) 
 REPRESENTATION_ITEM ( '' )  SURFACE ( )  );
#106487 = CIRCLE ( 'NONE', #89940, 11.80000000000000604 ) ;
#106489 = DIRECTION ( 'NONE',  ( 0.7071067811865486830, -0.1504730267678052180, 0.6909108974501224631 ) ) ;
#106490 = DIRECTION ( 'NONE',  ( 0.000000000000000000, 0.2617529984165034018, 0.9651348961777157509 ) ) ;
#106491 = EDGE_CURVE ( 'NONE', #186373, #142984, #119864, .T. ) ;
#106492 = CIRCLE ( 'NONE', #35810, 0.1000000000000001860 ) ;
#106493 = DIRECTION ( 'NONE',  ( -0.000000000000000000, -0.2617529984165031243, -0.9651348961777157509 ) ) ;
#106494 = VECTOR ( 'NONE', #145335, 1000.000000000000000 ) ;
#106495 = CARTESIAN_POINT ( 'NONE',  ( 21.05000000000000071, 2.585532092011767702, -212.8717110730202933 ) ) ;
#106496 = EDGE_CURVE ( 'NONE', #209946, #188501, #199136, .T. ) ;
#106497 = DIRECTION ( 'NONE',  ( -0.000000000000000000, -0.8660254037844377084, -0.5000000000000016653 ) ) ;
#106498 = ORIENTED_EDGE ( 'NONE', *, *, #237462, .F. ) ;
#106499 = ORIENTED_EDGE ( 'NONE', *, *, #193367, .T. ) ;
#106500 = ADVANCED_FACE ( 'NONE', ( #78127 ), #45008, .F. ) ;
#106501 = DIRECTION ( 'NONE',  ( 0.000000000000000000, -0.8814952561688430555, 0.4721928772777346239 ) ) ;
#106502 = B_SPLINE_CURVE_WITH_KNOTS ( 'NONE', 3,
 ( #15710, #95212, #176064, #196872, #238571, #78207, #14422, #254266, #255514, #258085 ),
 .UNSPECIFIED., .F., .F.,
 ( 4, 3, 3, 4 ),
 ( -2.000561356210515597E-06, 0.000000000000000000, 1.787822682428821068E-05, 4.206475347089863842E-05 ),
 .UNSPECIFIED. ) ;
#106503 = ORIENTED_EDGE ( 'NONE', *, *, #96461, .F. ) ;
#106504 = CARTESIAN_POINT ( 'NONE',  ( -21.05000000000000071, 87.65000000001246860, -173.0231074845243029 ) ) ;
#106505 = ORIENTED_EDGE ( 'NONE', *, *, #111760, .F. ) ;
#106506 =( BOUNDED_SURFACE ( )  B_SPLINE_SURFACE ( 3, 2, ( 
 ( #929, #19251, #103895 ),
 ( #139168, #84291, #220015 ),
 ( #41403, #163901, #243424 ),
 ( #218712, #178349, #64785 ) ),
 .UNSPECIFIED., .F., .F., .F. ) 
 B_SPLINE_SURFACE_WITH_KNOTS ( ( 4, 4 ),
 ( 3, 3 ),
 ( 0.0006461284895273969623, 0.0007503702773985950749 ),
 ( 0.000000000000000000, 1.000000000000000000 ),
 .UNSPECIFIED. ) 
 GEOMETRIC_REPRESENTATION_ITEM ( )  RATIONAL_B_SPLINE_SURFACE ( (
 ( 1.000000000000000000, 0.7071067811865475727, 1.000000000000000000),
 ( 1.000000000000000000, 0.7076476444648585051, 1.000000000000000000),
 ( 1.000000000000000000, 0.7075727925192710766, 1.000000000000000000),
 ( 1.000000000000000000, 0.7071067811865923147, 1.000000000000000000) ) ) 
 REPRESENTATION_ITEM ( '' )  SURFACE ( )  );
#106507 = EDGE_CURVE ( 'NONE', #92572, #26497, #33476, .T. ) ;
#106509 = ADVANCED_FACE ( 'NONE', ( #237224 ), #124981, .F. ) ;
#106508 = EDGE_CURVE ( 'NONE', #71963, #87941, #153389, .T. ) ;
#106510 = CARTESIAN_POINT ( 'NONE',  ( -21.14999999999999858, 76.00000000001169553, -76.06376443622556849 ) ) ;
#106511 = DIRECTION ( 'NONE',  ( 0.000000000000000000, 6.982962677686266711E-15, -1.000000000000000000 ) ) ;
#106512 = CARTESIAN_POINT ( 'NONE',  ( -16.92570016628983609, 22.95634624765352427, -230.9134574420077968 ) ) ;
#106513 = ORIENTED_EDGE ( 'NONE', *, *, #138143, .T. ) ;
#106514 = CARTESIAN_POINT ( 'NONE',  ( -23.25000000000000355, 11.75000000001113953, -124.7500000000000284 ) ) ;
#106515 = ORIENTED_EDGE ( 'NONE', *, *, #204477, .F. ) ;
#106516 = TOROIDAL_SURFACE ( 'NONE', #27494, 4.099999999999999645, 0.1000000000000000056 ) ;
#106517 = CARTESIAN_POINT ( 'NONE',  ( 18.59999999999999076, 55.05538098155519577, -230.0782228604559805 ) ) ;
#106518 = DIRECTION ( 'NONE',  ( 0.000000000000000000, -0.8814952561688437216, 0.4721928772777334582 ) ) ;
#106519 = TOROIDAL_SURFACE ( 'NONE', #69171, 0.4000000000000009104, 0.1000000000000000056 ) ;
#106520 = DIRECTION ( 'NONE',  ( -0.7071067811865214825, -0.7071067811865735520, 0.000000000000000000 ) ) ;
#106521 = DIRECTION ( 'NONE',  ( 0.000000000000000000, 0.8814952561688476074, -0.4721928772777262417 ) ) ;
#106522 = AXIS2_PLACEMENT_3D ( 'NONE', #41567, #121111, #71718 ) ;
#106523 = AXIS2_PLACEMENT_3D ( 'NONE', #176808, #136341, #137638 ) ;
#106524 = ORIENTED_EDGE ( 'NONE', *, *, #217114, .F. ) ;
#106525 = CARTESIAN_POINT ( 'NONE',  ( -21.05000000000000071, 36.02367271998545561, -235.8812521208699309 ) ) ;
#106526 = ORIENTED_EDGE ( 'NONE', *, *, #157099, .T. ) ;
#106529 = ORIENTED_EDGE ( 'NONE', *, *, #31126, .T. ) ;
#106528 = CYLINDRICAL_SURFACE ( 'NONE', #238805, 12.87499999999999822 ) ;
#106527 = CARTESIAN_POINT ( 'NONE',  ( 18.39999999999999147, 46.96039402156218046, -255.3459641718772843 ) ) ;
#106530 = EDGE_CURVE ( 'NONE', #96909, #255325, #86669, .T. ) ;
#106531 = CARTESIAN_POINT ( 'NONE',  ( -20.54999999999999716, 76.00000000001192291, -104.9231074845242944 ) ) ;
#106532 = EDGE_CURVE ( 'NONE', #86681, #3957, #25888, .T. ) ;
#106533 = EDGE_LOOP ( 'NONE', ( #69239, #73490, #25187, #32484 ) ) ;
#106534 = VECTOR ( 'NONE', #35111, 1000.000000000000000 ) ;
#106535 = LINE ( 'NONE', #227783, #87900 ) ;
#106536 = ORIENTED_EDGE ( 'NONE', *, *, #76422, .F. ) ;
#106537 = ADVANCED_FACE ( 'NONE', ( #3736 ), #159868, .F. ) ;
#106538 = CARTESIAN_POINT ( 'NONE',  ( -23.25000000000000000, 11.65000000000000036, -21.34999999999999787 ) ) ;
#106539 = DIRECTION ( 'NONE',  ( -0.000000000000000000, 0.1350103645451974088, -0.9908441862701587999 ) ) ;
#106540 = AXIS2_PLACEMENT_3D ( 'NONE', #69461, #148999, #228529 ) ;
#106541 = CARTESIAN_POINT ( 'NONE',  ( -17.29158576265543346, 65.63525233399388981, -80.94034923973221396 ) ) ;
#106542 = VECTOR ( 'NONE', #182078, 1000.000000000000000 ) ;
#106543 = DIRECTION ( 'NONE',  ( 1.000000000000000000, 0.000000000000000000, 0.000000000000000000 ) ) ;
#106544 = EDGE_CURVE ( 'NONE', #91499, #88476, #65847, .T. ) ;
#106545 = CIRCLE ( 'NONE', #243939, 0.1000000000000028644 ) ;
#106546 = ORIENTED_EDGE ( 'NONE', *, *, #49886, .T. ) ;
#106548 = ADVANCED_FACE ( 'NONE', ( #222770 ), #203233, .T. ) ;
#106547 = CARTESIAN_POINT ( 'NONE',  ( -18.34374000495059676, 16.37079970714665933, -222.2530670965321349 ) ) ;
#106549 = CARTESIAN_POINT ( 'NONE',  ( -16.83199318825828783, 14.11404101182791493, -219.1395801100928793 ) ) ;
#106550 = CARTESIAN_POINT ( 'NONE',  ( -18.41817142474042157, -9.498703066590927335, -140.6039654876370264 ) ) ;
#106551 = ORIENTED_EDGE ( 'NONE', *, *, #238232, .T. ) ;
#106552 = FACE_BOUND ( 'NONE', #30007, .T. ) ;
#106553 = VERTEX_POINT ( 'NONE', #243631 ) ;
#106554 = DIRECTION ( 'NONE',  ( -1.000000000000000000, 1.836970198721029934E-16, 1.601412966608202925E-30 ) ) ;
#106555 = DIRECTION ( 'NONE',  ( 4.504528286903032433E-15, 0.1298341882520054891, 0.9915357197604850459 ) ) ;
#106556 = CARTESIAN_POINT ( 'NONE',  ( 21.14999999999999858, 69.35000000001186038, -90.67310748452435121 ) ) ;
#106557 = VECTOR ( 'NONE', #188707, 1000.000000000000114 ) ;
#106559 = ORIENTED_EDGE ( 'NONE', *, *, #213771, .F. ) ;
#106558 = PLANE ( 'NONE',  #73756 ) ;
#106560 = EDGE_CURVE ( 'NONE', #196725, #110507, #82396, .T. ) ;
#106561 = CARTESIAN_POINT ( 'NONE',  ( -21.44999999999999929, 44.92467540951147953, -237.7943620901849613 ) ) ;
#106562 = CARTESIAN_POINT ( 'NONE',  ( -15.75000000000001421, 62.62153588618861733, -217.1314428046943874 ) ) ;
#106563 = DIRECTION ( 'NONE',  ( 0.000000000000000000, 0.000000000000000000, -1.000000000000000000 ) ) ;
#106564 = VERTEX_POINT ( 'NONE', #205785 ) ;
#106565 = EDGE_CURVE ( 'NONE', #88561, #82161, #49098, .T. ) ;
#106566 = DIRECTION ( 'NONE',  ( 0.000000000000000000, 0.000000000000000000, 1.000000000000000000 ) ) ;
#106567 = DIRECTION ( 'NONE',  ( -0.000000000000000000, -0.000000000000000000, 1.000000000000000000 ) ) ;
#106568 = ORIENTED_EDGE ( 'NONE', *, *, #75926, .F. ) ;
#106569 = CARTESIAN_POINT ( 'NONE',  ( -21.53699400384572016, 65.45457063877245218, -242.4061840233274836 ) ) ;
#106570 = CIRCLE ( 'NONE', #135800, 0.09999999999998712696 ) ;
#106571 = VECTOR ( 'NONE', #233061, 999.9999999999998863 ) ;
#106572 = AXIS2_PLACEMENT_3D ( 'NONE', #242798, #160739, #124160 ) ;
#106573 = CIRCLE ( 'NONE', #85705, 0.1999999999999945155 ) ;
#106574 = VERTEX_POINT ( 'NONE', #27192 ) ;
#106575 = CARTESIAN_POINT ( 'NONE',  ( 20.73486653747088937, 12.00939135261245028, -219.7232347456343859 ) ) ;
#106577 = ORIENTED_EDGE ( 'NONE', *, *, #23406, .T. ) ;
#106576 = DIRECTION ( 'NONE',  ( 0.000000000000000000, 0.4088369013363281623, -0.9126074666063771490 ) ) ;
#106578 = ADVANCED_FACE ( 'NONE', ( #22037 ), #174235, .T. ) ;
#106581 = ORIENTED_EDGE ( 'NONE', *, *, #134452, .T. ) ;
#106580 = VERTEX_POINT ( 'NONE', #224056 ) ;
#106579 = LINE ( 'NONE', #123605, #222015 ) ;
#106582 = CARTESIAN_POINT ( 'NONE',  ( -21.04999999999994387, 82.72707916847673459, -26.51159310135756897 ) ) ;
#106583 = CARTESIAN_POINT ( 'NONE',  ( 20.94999999999999929, 4.850467289730772791, -45.53426740900168568 ) ) ;
#106584 = FACE_OUTER_BOUND ( 'NONE', #240020, .T. ) ;
#106586 = CARTESIAN_POINT ( 'NONE',  ( -12.60829076262179882, 66.61047060254480812, -51.70599957163072702 ) ) ;
#106585 = DIRECTION ( 'NONE',  ( 0.000000000000000000, 0.000000000000000000, -1.000000000000000000 ) ) ;
#106587 = CARTESIAN_POINT ( 'NONE',  ( 18.69999999999999929, -8.350000000000004974, 21.95857864376268864 ) ) ;
#106588 = FACE_OUTER_BOUND ( 'NONE', #228173, .T. ) ;
#106589 = CIRCLE ( 'NONE', #235785, 2.000000000000001776 ) ;
#106590 = FACE_OUTER_BOUND ( 'NONE', #252418, .T. ) ;
#106591 = DIRECTION ( 'NONE',  ( 1.186688945009009831E-16, -1.000000000000000000, 0.000000000000000000 ) ) ;
#106592 = CARTESIAN_POINT ( 'NONE',  ( 11.60000000000000142, -8.250000000000005329, 19.04142135623731136 ) ) ;
#106593 = ORIENTED_EDGE ( 'NONE', *, *, #143802, .F. ) ;
#106594 = ORIENTED_EDGE ( 'NONE', *, *, #153983, .T. ) ;
#106595 = FACE_OUTER_BOUND ( 'NONE', #68299, .T. ) ;
#106596 = CIRCLE ( 'NONE', #110903, 0.09999999999999939493 ) ;
#106598 = ORIENTED_EDGE ( 'NONE', *, *, #184834, .F. ) ;
#106597 = DIRECTION ( 'NONE',  ( 0.000000000000000000, -0.2128009952263603677, 0.9770955615653313941 ) ) ;
#106599 = ORIENTED_EDGE ( 'NONE', *, *, #23461, .F. ) ;
#106600 = CARTESIAN_POINT ( 'NONE',  ( -16.80438519320023616, 12.41397469025448785, -211.2436573308034440 ) ) ;
#106601 = ORIENTED_EDGE ( 'NONE', *, *, #139267, .F. ) ;
#106602 = DIRECTION ( 'NONE',  ( 0.000000000000000000, 0.9126074666063770380, 0.4088369013363281068 ) ) ;
#106603 = ORIENTED_EDGE ( 'NONE', *, *, #33190, .T. ) ;
#106604 = CARTESIAN_POINT ( 'NONE',  ( -16.87331047859649757, 66.05000000001224691, -149.1731074845244223 ) ) ;
#106605 = CARTESIAN_POINT ( 'NONE',  ( -18.60000000000000142, -9.523954320741635726, -174.3820170568273795 ) ) ;
#106608 = EDGE_LOOP ( 'NONE', ( #179426, #2650, #115857, #41264, #38415 ) ) ;
#106607 = ORIENTED_EDGE ( 'NONE', *, *, #89079, .T. ) ;
#106606 = CIRCLE ( 'NONE', #27575, 0.09999999999999063804 ) ;
#106609 = ORIENTED_EDGE ( 'NONE', *, *, #58498, .T. ) ;
#106610 = DIRECTION ( 'NONE',  ( 1.000000000000000000, 0.000000000000000000, 0.000000000000000000 ) ) ;
#106611 = ORIENTED_EDGE ( 'NONE', *, *, #156357, .T. ) ;
#106612 = VERTEX_POINT ( 'NONE', #45435 ) ;
#106613 = CARTESIAN_POINT ( 'NONE',  ( -16.88328101497759448, 14.15959734275620541, -219.2561499714656748 ) ) ;
#106614 = CARTESIAN_POINT ( 'NONE',  ( -18.50000000000000000, 68.97833521811179480, -99.18954208262705663 ) ) ;
#106616 = ORIENTED_EDGE ( 'NONE', *, *, #19165, .T. ) ;
#106615 = FACE_OUTER_BOUND ( 'NONE', #206662, .T. ) ;
#106617 = DIRECTION ( 'NONE',  ( 0.000000000000000000, 8.881784197002011602E-16, -1.000000000000000000 ) ) ;
#106618 = CARTESIAN_POINT ( 'NONE',  ( 19.58285714285715073, 10.38499851036257837, -108.1296846673899950 ) ) ;
#106620 = ORIENTED_EDGE ( 'NONE', *, *, #81549, .F. ) ;
#106619 = DIRECTION ( 'NONE',  ( -0.000000000000000000, -0.000000000000000000, 1.000000000000000000 ) ) ;
#106621 = CARTESIAN_POINT ( 'NONE',  ( 23.24999999999999289, 35.97645343225767789, -235.9694016464868298 ) ) ;
#106622 = ORIENTED_EDGE ( 'NONE', *, *, #95194, .F. ) ;
#106623 = LINE ( 'NONE', #222731, #253482 ) ;
#106624 = ORIENTED_EDGE ( 'NONE', *, *, #98082, .F. ) ;
#106625 = CARTESIAN_POINT ( 'NONE',  ( -21.05000000000000071, 18.60982576078065165, -226.6665746245395496 ) ) ;
#106626 = FACE_OUTER_BOUND ( 'NONE', #65412, .T. ) ;
#106627 = EDGE_CURVE ( 'NONE', #203324, #30979, #2439, .T. ) ;
#106628 = CIRCLE ( 'NONE', #219069, 0.09999999999999130418 ) ;
#106629 = ORIENTED_EDGE ( 'NONE', *, *, #115787, .F. ) ;
#106631 = DIRECTION ( 'NONE',  ( -1.000000000000000000, -0.000000000000000000, -0.000000000000000000 ) ) ;
#106630 = DIRECTION ( 'NONE',  ( -1.000000000000000000, -0.000000000000000000, 0.000000000000000000 ) ) ;
#106632 = CIRCLE ( 'NONE', #202335, 0.1999999999999987899 ) ;
#106633 = AXIS2_PLACEMENT_3D ( 'NONE', #140591, #243547, #106585 ) ;
#106634 = FACE_OUTER_BOUND ( 'NONE', #21025, .T. ) ;
#106635 = FACE_BOUND ( 'NONE', #207693, .T. ) ;
#106636 = EDGE_LOOP ( 'NONE', ( #181510, #207027, #181673 ) ) ;
#106637 = EDGE_LOOP ( 'NONE', ( #141593, #73346, #156391, #232641 ) ) ;
#106638 = CARTESIAN_POINT ( 'NONE',  ( 18.59999999999999076, 63.58402440245809828, -209.2218768284338637 ) ) ;
#106639 = CARTESIAN_POINT ( 'NONE',  ( -23.25000000000000000, 11.65000000001115588, -21.75000000000000355 ) ) ;
#106640 = ORIENTED_EDGE ( 'NONE', *, *, #228069, .F. ) ;
#106641 = DIRECTION ( 'NONE',  ( 1.186688945009010077E-16, 1.000000000000000000, 6.982962677686266711E-15 ) ) ;
#106642 = ORIENTED_EDGE ( 'NONE', *, *, #85000, .T. ) ;
#106643 = CARTESIAN_POINT ( 'NONE',  ( 20.94999999999999929, 85.50000000001179501, -79.41707660717668205 ) ) ;
#106644 = ORIENTED_EDGE ( 'NONE', *, *, #47951, .T. ) ;
#106645 = CARTESIAN_POINT ( 'NONE',  ( -18.59999999999999787, 78.48087866980282001, -232.8271061603568910 ) ) ;
#106646 = ADVANCED_FACE ( 'NONE', ( #221481 ), #41823, .F. ) ;
#106647 = EDGE_CURVE ( 'NONE', #39612, #257620, #87111, .T. ) ;
#106648 = CARTESIAN_POINT ( 'NONE',  ( 23.15000000000000213, 87.48912529308749697, -39.12310748452424747 ) ) ;
#106649 = DIRECTION ( 'NONE',  ( -1.000000000000000000, -0.000000000000000000, 0.000000000000000000 ) ) ;
#106650 = VERTEX_POINT ( 'NONE', #32319 ) ;
#106651 = DIRECTION ( 'NONE',  ( -1.836970198721029934E-16, 1.000000000000000000, 0.000000000000000000 ) ) ;
#106652 =( NAMED_UNIT ( * ) PLANE_ANGLE_UNIT ( ) SI_UNIT ( $, .RADIAN. ) );
#106653 = ORIENTED_EDGE ( 'NONE', *, *, #32149, .T. ) ;
#106654 = VERTEX_POINT ( 'NONE', #207083 ) ;
#106655 = VECTOR ( 'NONE', #127388, 1000.000000000000000 ) ;
#106656 = EDGE_LOOP ( 'NONE', ( #61449, #9965, #190846, #244191 ) ) ;
#106657 = ADVANCED_FACE ( 'NONE', ( #29758 ), #110534, .T. ) ;
#106658 = DIRECTION ( 'NONE',  ( 1.186688945009009831E-16, -1.000000000000000000, 0.000000000000000000 ) ) ;
#106659 = DIRECTION ( 'NONE',  ( 0.000000000000000000, 0.000000000000000000, 1.000000000000000000 ) ) ;
#106660 = CARTESIAN_POINT ( 'NONE',  ( -1.739115166359751801E-14, 59.19392724319018839, -220.9828015967491126 ) ) ;
#106662 = EDGE_CURVE ( 'NONE', #145162, #68945, #149086, .T. ) ;
#106661 = DIRECTION ( 'NONE',  ( -3.265361837132813093E-16, 1.000000000000000000, 0.000000000000000000 ) ) ;
#106663 = AXIS2_PLACEMENT_3D ( 'NONE', #136960, #202082, #138226 ) ;
#106664 = SPHERICAL_SURFACE ( 'NONE', #105157, 0.1000000000000000056 ) ;
#106666 = CARTESIAN_POINT ( 'NONE',  ( 18.59999999999999076, 76.00000000001142553, -36.02310748452432421 ) ) ;
#106665 = CARTESIAN_POINT ( 'NONE',  ( -18.69999999999999929, -11.65000000000000036, 5.900000000000001243 ) ) ;
#106668 = EDGE_LOOP ( 'NONE', ( #87609, #126324, #3012, #196687 ) ) ;
#106667 = DIRECTION ( 'NONE',  ( 1.000000000000000000, -3.965082230804126670E-15, 0.000000000000000000 ) ) ;
#106669 = CARTESIAN_POINT ( 'NONE',  ( -22.49231231312463208, 11.64998490368843953, -100.4389471123986652 ) ) ;
#106670 = ORIENTED_EDGE ( 'NONE', *, *, #14697, .T. ) ;
#106671 = CIRCLE ( 'NONE', #252409, 0.2000000000000057288 ) ;
#106672 = ADVANCED_FACE ( 'NONE', ( #187536 ), #166700, .T. ) ;
#106673 = CARTESIAN_POINT ( 'NONE',  ( 20.95512820512820440, 8.876151316299271343, -79.15000000000004832 ) ) ;
#106674 = TOROIDAL_SURFACE ( 'NONE', #169085, 0.4000000000000017431, 0.1000000000000000056 ) ;
#106675 = EDGE_LOOP ( 'NONE', ( #193757, #6643, #237646, #27766 ) ) ;
#106676 = ORIENTED_EDGE ( 'NONE', *, *, #108538, .F. ) ;
#106677 = CARTESIAN_POINT ( 'NONE',  ( -1.820710678118658388, -9.929289321870186313, -158.6500000000000057 ) ) ;
#106678 = DIRECTION ( 'NONE',  ( 0.000000000000000000, 1.000000000000000000, 0.000000000000000000 ) ) ;
#106679 = CARTESIAN_POINT ( 'NONE',  ( -21.05000000000253024, 75.94867256767116714, -209.8232908208007927 ) ) ;
#106680 = CARTESIAN_POINT ( 'NONE',  ( -20.64999999999999858, 76.00000000001244871, -170.0231074845243597 ) ) ;
#106681 = EDGE_CURVE ( 'NONE', #50099, #213687, #182405, .T. ) ;
#106682 = AXIS2_PLACEMENT_3D ( 'NONE', #12363, #231398, #189693 ) ;
#106683 = CARTESIAN_POINT ( 'NONE',  ( 23.14999999999999858, 5.000000000011153745, -88.09473398108696074 ) ) ;
#106685 = VERTEX_POINT ( 'NONE', #92249 ) ;
#106684 = CIRCLE ( 'NONE', #139991, 0.09999999999999939493 ) ;
#106687 = ORIENTED_EDGE ( 'NONE', *, *, #175943, .T. ) ;
#106686 = ADVANCED_FACE ( 'NONE', ( #131383 ), #11458, .T. ) ;
#106688 = AXIS2_PLACEMENT_3D ( 'NONE', #189845, #171597, #227675 ) ;
#106689 = CARTESIAN_POINT ( 'NONE',  ( -15.55912972643740488, 67.50912972644967169, -149.1731074845244223 ) ) ;
#106690 = ORIENTED_EDGE ( 'NONE', *, *, #207160, .T. ) ;
#106691 = CARTESIAN_POINT ( 'NONE',  ( -21.65000000000000213, 29.50054346320101928, -236.9717244483098568 ) ) ;
#106692 = CARTESIAN_POINT ( 'NONE',  ( 21.98333005346336577, 0.000000000000000000, 7.374075329056667627 ) ) ;
#106693 = CARTESIAN_POINT ( 'NONE',  ( 18.59999999999999787, -14.27107483842559610, -0.5438473119858301397 ) ) ;
#106694 = PLANE ( 'NONE',  #162984 ) ;
#106695 = AXIS2_PLACEMENT_3D ( 'NONE', #143123, #243526, #223950 ) ;
#106696 = DIRECTION ( 'NONE',  ( 1.000000000000000000, 0.000000000000000000, 0.000000000000000000 ) ) ;
#106697 = CARTESIAN_POINT ( 'NONE',  ( -20.54999999999999716, 76.00000000001213607, -136.5231074845243313 ) ) ;
#106698 = EDGE_LOOP ( 'NONE', ( #92414, #15460, #250126, #135575 ) ) ;
#106699 = CARTESIAN_POINT ( 'NONE',  ( -23.15000000000000213, 2.000000000011154189, -87.27537807723794572 ) ) ;
#106700 = CARTESIAN_POINT ( 'NONE',  ( -21.05000000000000071, 14.05000000001115623, -106.0136950707610310 ) ) ;
#106701 = DIRECTION ( 'NONE',  ( -1.000000000000000000, 6.938893903907270030E-14, 0.000000000000000000 ) ) ;
#106702 = ADVANCED_FACE ( 'NONE', ( #71437 ), #230495, .F. ) ;
#106703 = CARTESIAN_POINT ( 'NONE',  ( -23.15000000000000213, 73.50000000001151079, -49.24772940728643533 ) ) ;
#106704 = CARTESIAN_POINT ( 'NONE',  ( -18.43569575749025446, 85.51932773110432606, -96.05013110796488718 ) ) ;
#106705 = AXIS2_PLACEMENT_3D ( 'NONE', #180065, #87022, #148311 ) ;
#106706 = CARTESIAN_POINT ( 'NONE',  ( 21.14999999999999858, 64.35000000001237197, -169.9231074845244507 ) ) ;
#106707 = B_SPLINE_CURVE_WITH_KNOTS ( 'NONE', 3,
 ( #141354, #235311, #137482, #160938, #22721, #56644, #219594, #100896, #240457, #38406 ),
 .UNSPECIFIED., .F., .F.,
 ( 4, 2, 2, 2, 4 ),
 ( 0.000000000000000000, 3.990160268013564522E-05, 7.980320536027129044E-05, 0.0001596064107205425809, 0.0003192128214410908538 ),
 .UNSPECIFIED. ) ;
#106708 = ORIENTED_EDGE ( 'NONE', *, *, #248042, .F. ) ;
#106709 = CARTESIAN_POINT ( 'NONE',  ( -17.04295772865478398, 65.97510057475076906, -157.3731074845244109 ) ) ;
#106710 = ORIENTED_EDGE ( 'NONE', *, *, #123004, .T. ) ;
#106711 = FACE_OUTER_BOUND ( 'NONE', #238077, .T. ) ;
#106713 = VECTOR ( 'NONE', #37304, 1000.000000000000227 ) ;
#106712 = LINE ( 'NONE', #222815, #197960 ) ;
#106714 = DIRECTION ( 'NONE',  ( -1.000000000000000000, -2.952720810173289112E-16, 0.000000000000000000 ) ) ;
#106715 = CARTESIAN_POINT ( 'NONE',  ( 20.77526135991770317, 67.06799098339197940, -161.5545389417991657 ) ) ;
#106717 = VERTEX_POINT ( 'NONE', #186237 ) ;
#106716 = AXIS2_PLACEMENT_3D ( 'NONE', #182492, #144610, #5082 ) ;
#106718 = DIRECTION ( 'NONE',  ( 1.000000000000000000, -0.000000000000000000, -0.000000000000000000 ) ) ;
#106719 = DIRECTION ( 'NONE',  ( 0.000000000000000000, 0.000000000000000000, -1.000000000000000000 ) ) ;
#106720 = CIRCLE ( 'NONE', #31766, 0.1000000000000010186 ) ;
#106721 = AXIS2_PLACEMENT_3D ( 'NONE', #247017, #227457, #209184 ) ;
#106722 = PRESENTATION_STYLE_ASSIGNMENT (( #6341 ) ) ;
#106723 = CARTESIAN_POINT ( 'NONE',  ( -18.50000000000000000, -1.164121893230052995, -175.4148480855716059 ) ) ;
#106724 = FACE_OUTER_BOUND ( 'NONE', #94143, .T. ) ;
#106725 = CARTESIAN_POINT ( 'NONE',  ( -21.14999999999994174, 82.78482233730476025, -26.42994920107286916 ) ) ;
#106726 = AXIS2_PLACEMENT_3D ( 'NONE', #112398, #56242, #91544 ) ;
#106727 = EDGE_CURVE ( 'NONE', #129596, #171512, #49292, .T. ) ;
#106728 = EDGE_CURVE ( 'NONE', #56891, #89909, #171840, .T. ) ;
#106729 = ORIENTED_EDGE ( 'NONE', *, *, #156590, .T. ) ;
#106730 = ORIENTED_EDGE ( 'NONE', *, *, #76553, .T. ) ;
#106731 = CARTESIAN_POINT ( 'NONE',  ( -5.900000000000005684, -11.25000000000000000, 1.279358563532896415E-15 ) ) ;
#106732 = LINE ( 'NONE', #186301, #255087 ) ;
#106733 = DIRECTION ( 'NONE',  ( -1.000000000000000000, 0.000000000000000000, 0.000000000000000000 ) ) ;
#106734 = DIRECTION ( 'NONE',  ( 0.9880948137434723000, -0.06289798482097132271, 0.1404011487086684051 ) ) ;
#106735 = EDGE_CURVE ( 'NONE', #19733, #109777, #117015, .T. ) ;
#106737 = ADVANCED_FACE ( 'NONE', ( #149696 ), #257689, .T. ) ;
#106736 = AXIS2_PLACEMENT_3D ( 'NONE', #21683, #101153, #201583 ) ;
#106738 = VERTEX_POINT ( 'NONE', #173135 ) ;
#106739 = CARTESIAN_POINT ( 'NONE',  ( 21.05000000000000071, 28.08470566095357057, -239.2860081655328770 ) ) ;
#106740 = ITEM_DEFINED_TRANSFORMATION ( 'NONE', 'NONE', #94538,  #2425 ) ;
#106741 = AXIS2_PLACEMENT_3D ( 'NONE', #157127, #49342, #168050 ) ;
#106742 = FACE_OUTER_BOUND ( 'NONE', #89530, .T. ) ;
#106743 = AXIS2_PLACEMENT_3D ( 'NONE', #100620, #1545, #117655 ) ;
#106744 = ADVANCED_FACE ( 'NONE', ( #157410 ), #16600, .F. ) ;
#106745 = VERTEX_POINT ( 'NONE', #34890 ) ;
#106746 = CARTESIAN_POINT ( 'NONE',  ( -20.94999999999999929, -1.164121893241208960, -41.41484808557160591 ) ) ;
#106747 = B_SPLINE_CURVE_WITH_KNOTS ( 'NONE', 3,
 ( #77031, #196974, #40525, #37938, #35388, #61, #216547 ),
 .UNSPECIFIED., .F., .F.,
 ( 4, 3, 4 ),
 ( 3.469446951953614189E-18, 3.882884552234413058E-05, 5.798605692158380332E-05 ),
 .UNSPECIFIED. ) ;
#106748 = EDGE_CURVE ( 'NONE', #243244, #206950, #61757, .T. ) ;
#106749 = EDGE_CURVE ( 'NONE', #39196, #57412, #58252, .T. ) ;
#106750 = ORIENTED_EDGE ( 'NONE', *, *, #191884, .T. ) ;
#106751 = ADVANCED_FACE ( 'NONE', ( #79091 ), #233083, .T. ) ;
#106752 = AXIS2_PLACEMENT_3D ( 'NONE', #222360, #202828, #24216 ) ;
#106753 = EDGE_LOOP ( 'NONE', ( #222286, #220749, #255321, #64666 ) ) ;
#106754 = CARTESIAN_POINT ( 'NONE',  ( -22.60000000000094289, 75.89914163091351895, -114.7726746080137303 ) ) ;
#106755 = DIRECTION ( 'NONE',  ( 1.000000000000000000, 0.000000000000000000, 0.000000000000000000 ) ) ;
#106756 = DIRECTION ( 'NONE',  ( 0.000000000000000000, -0.2128009952263650861, 0.9770955615653305060 ) ) ;
#106757 = LINE ( 'NONE', #165476, #7253 ) ;
#106758 = CARTESIAN_POINT ( 'NONE',  ( -17.01473183483381035, 14.13772148853350252, -219.1573629999798811 ) ) ;
#106759 = EDGE_CURVE ( 'NONE', #220140, #143709, #120063, .T. ) ;
#106760 = DIRECTION ( 'NONE',  ( -0.000000000000000000, 0.8660254037844502539, 0.4999999999999799050 ) ) ;
#106761 = FACE_OUTER_BOUND ( 'NONE', #162839, .T. ) ;
#106763 = CARTESIAN_POINT ( 'NONE',  ( -21.64999999999999858, 68.75000000001186606, -90.77310748452435973 ) ) ;
#106762 = CARTESIAN_POINT ( 'NONE',  ( 20.95539060131842746, 65.37613784235624337, -95.36937367086818540 ) ) ;
#106764 = CARTESIAN_POINT ( 'NONE',  ( 18.59999999999999787, 77.83585931145570669, -125.0186683157258329 ) ) ;
#106766 = EDGE_CURVE ( 'NONE', #156566, #181381, #75296, .T. ) ;
#106765 = CARTESIAN_POINT ( 'NONE',  ( 22.39999999999999503, 7.790779598384535376, -133.9000000000000057 ) ) ;
#106767 = CARTESIAN_POINT ( 'NONE',  ( -20.54999999999999716, 61.88149656937975607, -248.1136133839584090 ) ) ;
#106768 = DIRECTION ( 'NONE',  ( -0.000000000000000000, -0.000000000000000000, 1.000000000000000000 ) ) ;
#106769 = AXIS2_PLACEMENT_3D ( 'NONE', #85182, #49940, #206455 ) ;
#106770 = VERTEX_POINT ( 'NONE', #97356 ) ;
#106771 = ORIENTED_EDGE ( 'NONE', *, *, #143894, .T. ) ;
#106772 = TOROIDAL_SURFACE ( 'NONE', #114973, 2.100000000000002309, 0.1000000000000000056 ) ;
#106773 = DIRECTION ( 'NONE',  ( 0.000000000000000000, -0.7397360091702802620, 0.6728971962616779878 ) ) ;
#106774 = CIRCLE ( 'NONE', #206735, 0.1000000000000001860 ) ;
#106775 = CARTESIAN_POINT ( 'NONE',  ( -23.25000000000000355, 70.35000000001261355, -190.8731074845244109 ) ) ;
#106777 = DIRECTION ( 'NONE',  ( -1.000000000000000000, -0.000000000000000000, -0.000000000000000000 ) ) ;
#106776 = DIRECTION ( 'NONE',  ( 0.000000000000000000, 0.000000000000000000, 1.000000000000000000 ) ) ;
#106778 = EDGE_CURVE ( 'NONE', #188810, #249694, #16003, .T. ) ;
#106779 = CARTESIAN_POINT ( 'NONE',  ( 20.95378194480896639, 39.25578854815272933, -236.8440500613521351 ) ) ;
#106780 = CARTESIAN_POINT ( 'NONE',  ( -21.65000000000000213, 7.250000000011139534, -87.85000000000003695 ) ) ;
#106781 = DIRECTION ( 'NONE',  ( 0.000000000000000000, 0.000000000000000000, -1.000000000000000000 ) ) ;
#106782 = EDGE_CURVE ( 'NONE', #147011, #168551, #249039, .T. ) ;
#106783 = EDGE_CURVE ( 'NONE', #952, #241619, #197773, .T. ) ;
#106784 = ORIENTED_EDGE ( 'NONE', *, *, #11742, .T. ) ;
#106785 = ORIENTED_EDGE ( 'NONE', *, *, #256861, .T. ) ;
#106786 = FACE_OUTER_BOUND ( 'NONE', #159767, .T. ) ;
#106787 = AXIS2_PLACEMENT_3D ( 'NONE', #55365, #95792, #54113 ) ;
#106788 = VERTEX_POINT ( 'NONE', #135220 ) ;
#106789 = FACE_OUTER_BOUND ( 'NONE', #62570, .T. ) ;
#106790 = TOROIDAL_SURFACE ( 'NONE', #140096, 0.2000000000000000111, 0.1000000000000000056 ) ;
#106791 = AXIS2_PLACEMENT_3D ( 'NONE', #36663, #154062, #97851 ) ;
#106792 = DIRECTION ( 'NONE',  ( 0.000000000000000000, -0.9126074666063769270, -0.4088369013363280513 ) ) ;
#106793 = AXIS2_PLACEMENT_3D ( 'NONE', #22170, #84643, #203359 ) ;
#106794 = VERTEX_POINT ( 'NONE', #14023 ) ;
#106795 = CARTESIAN_POINT ( 'NONE',  ( -18.51697539158856998, 18.38637412622487588, -236.9471295141160567 ) ) ;
#106796 = VERTEX_POINT ( 'NONE', #93539 ) ;
#106797 = CARTESIAN_POINT ( 'NONE',  ( -20.93284271247462058, 64.25000000001250555, -177.0379132551783812 ) ) ;
#106798 = PLANE ( 'NONE',  #124533 ) ;
#106799 = DIRECTION ( 'NONE',  ( 0.000000000000000000, 1.000000000000000000, 6.982962677686266711E-15 ) ) ;
#106800 = DIRECTION ( 'NONE',  ( 0.000000000000000000, 0.000000000000000000, -1.000000000000000000 ) ) ;
#106801 = LINE ( 'NONE', #67686, #151450 ) ;
#106802 = DIRECTION ( 'NONE',  ( 1.000000000000000000, 0.000000000000000000, -0.000000000000000000 ) ) ;
#106803 = DIRECTION ( 'NONE',  ( 0.000000000000000000, -1.000000000000000000, -6.982962677686265922E-15 ) ) ;
#106804 = CARTESIAN_POINT ( 'NONE',  ( -18.60000000000000142, -8.150000000000005684, -15.00000000000000000 ) ) ;
#106806 = ORIENTED_EDGE ( 'NONE', *, *, #91095, .F. ) ;
#106805 = CARTESIAN_POINT ( 'NONE',  ( 18.41832399655381991, -0.9152169696499932172, -242.2974987189348610 ) ) ;
#106808 = CARTESIAN_POINT ( 'NONE',  ( -23.25000000000000000, 76.00000000001197975, -107.1731074845243086 ) ) ;
#106807 = FACE_OUTER_BOUND ( 'NONE', #65241, .T. ) ;
#106809 = ORIENTED_EDGE ( 'NONE', *, *, #120012, .T. ) ;
#106811 = ORIENTED_EDGE ( 'NONE', *, *, #95352, .F. ) ;
#106810 = DIRECTION ( 'NONE',  ( -1.000000000000000000, -7.304098846218163263E-16, 4.217023435051627211E-16 ) ) ;
#106812 = AXIS2_PLACEMENT_3D ( 'NONE', #180088, #86074, #165670 ) ;
#106813 = EDGE_LOOP ( 'NONE', ( #57053, #147334, #19752 ) ) ;
#106814 = LINE ( 'NONE', #69010, #203160 ) ;
#106815 = CARTESIAN_POINT ( 'NONE',  ( 20.94999999999999929, 1.115600667400684642E-11, -100.5000000000000284 ) ) ;
#106816 = CYLINDRICAL_SURFACE ( 'NONE', #208822, 0.09999999999999939493 ) ;
#106817 = LINE ( 'NONE', #245059, #147423 ) ;
#106818 = CARTESIAN_POINT ( 'NONE',  ( -21.05000000000000071, 74.16465844978745281, -91.46795619196133487 ) ) ;
#106819 = DIRECTION ( 'NONE',  ( 1.000000000000000000, 1.836970198721029934E-16, 0.000000000000000000 ) ) ;
#106820 = DIRECTION ( 'NONE',  ( 0.000000000000000000, -0.4721928772777402861, -0.8814952561688399468 ) ) ;
#106821 = DIRECTION ( 'NONE',  ( -1.000000000000000000, -0.000000000000000000, -0.000000000000000000 ) ) ;
#106822 = EDGE_CURVE ( 'NONE', #160294, #77989, #139048, .T. ) ;
#106824 = AXIS2_PLACEMENT_3D ( 'NONE', #105772, #6695, #104487 ) ;
#106823 = CARTESIAN_POINT ( 'NONE',  ( -21.05000000000000071, 87.65000000001144542, -39.02310748452423894 ) ) ;
#106825 = ORIENTED_EDGE ( 'NONE', *, *, #2498, .F. ) ;
#106826 = ORIENTED_EDGE ( 'NONE', *, *, #89357, .F. ) ;
#106827 = EDGE_CURVE ( 'NONE', #110428, #18469, #78320, .T. ) ;
#106828 = DIRECTION ( 'NONE',  ( 0.000000000000000000, -0.8496786552930076786, -0.5273008465188218086 ) ) ;
#106829 = AXIS2_PLACEMENT_3D ( 'NONE', #68469, #188403, #9764 ) ;
#106830 = ORIENTED_EDGE ( 'NONE', *, *, #18418, .T. ) ;
#106831 = CARTESIAN_POINT ( 'NONE',  ( 21.00000000000000000, 30.37633856152204359, -235.1250019192171408 ) ) ;
#106832 = ORIENTED_EDGE ( 'NONE', *, *, #154252, .F. ) ;
#106833 = DIRECTION ( 'NONE',  ( 0.000000000000000000, 1.000000000000000000, 1.156482317317864980E-14 ) ) ;
#106834 =( GEOMETRIC_REPRESENTATION_CONTEXT ( 3 ) GLOBAL_UNCERTAINTY_ASSIGNED_CONTEXT ( ( #97481 ) ) GLOBAL_UNIT_ASSIGNED_CONTEXT ( ( #129485, #85172, #126914 ) ) REPRESENTATION_CONTEXT ( 'NONE', 'WORKASPACE' ) );
#106835 = EDGE_CURVE ( 'NONE', #89253, #168386, #133944, .T. ) ;
#106836 = ADVANCED_FACE ( 'NONE', ( #76539 ), #193943, .F. ) ;
#106837 = CARTESIAN_POINT ( 'NONE',  ( 19.83283456528359423, 11.75000000000000711, -24.84999999941982551 ) ) ;
#106838 = DIRECTION ( 'NONE',  ( 0.000000000000000000, -0.2128009952263900384, 0.9770955615653251769 ) ) ;
#106839 = DIRECTION ( 'NONE',  ( 0.000000000000000000, 0.000000000000000000, 1.000000000000000000 ) ) ;
#106840 = DIRECTION ( 'NONE',  ( -1.000000000000000000, 0.000000000000000000, 0.000000000000000000 ) ) ;
#106841 = ORIENTED_EDGE ( 'NONE', *, *, #49144, .T. ) ;
#106842 = SPHERICAL_SURFACE ( 'NONE', #190988, 0.1000000000000000056 ) ;
#106843 = DIRECTION ( 'NONE',  ( 0.000000000000000000, -0.9126074666063769270, -0.4088369013363280513 ) ) ;
#106844 = CARTESIAN_POINT ( 'NONE',  ( 18.50000000000000355, 85.42145614550700827, -62.28112540050488377 ) ) ;
#106845 = DIRECTION ( 'NONE',  ( -6.938893903907222067E-15, 0.4721928772777344019, 0.8814952561688432775 ) ) ;
#106846 = ORIENTED_EDGE ( 'NONE', *, *, #85293, .T. ) ;
#106848 = CARTESIAN_POINT ( 'NONE',  ( -23.25000000000000000, 87.65000000001276703, -215.2731074845242745 ) ) ;
#106847 = CARTESIAN_POINT ( 'NONE',  ( 21.11101077988997332, 61.02755128856028932, -234.1884601127081567 ) ) ;
#106849 = CIRCLE ( 'NONE', #248510, 0.09999999999998898659 ) ;
#106850 = ORIENTED_EDGE ( 'NONE', *, *, #34436, .F. ) ;
#106852 = VERTEX_POINT ( 'NONE', #156119 ) ;
#106851 =( NAMED_UNIT ( * ) PLANE_ANGLE_UNIT ( ) SI_UNIT ( $, .RADIAN. ) );
#106853 = ORIENTED_EDGE ( 'NONE', *, *, #213737, .T. ) ;
#106854 = DIRECTION ( 'NONE',  ( -6.938893903907224433E-15, 1.000000000000000000, 0.000000000000000000 ) ) ;
#106856 = EDGE_CURVE ( 'NONE', #23444, #254970, #178315, .T. ) ;
#106855 = CIRCLE ( 'NONE', #6902, 0.1000000000000105804 ) ;
#106857 = DIRECTION ( 'NONE',  ( 0.000000000000000000, -2.775557561562888827E-14, 1.000000000000000000 ) ) ;
#106858 = AXIS2_PLACEMENT_3D ( 'NONE', #123041, #141311, #125596 ) ;
#106859 = CARTESIAN_POINT ( 'NONE',  ( 21.05000000000000071, 5.400000000011154988, -57.10603087734755690 ) ) ;
#106860 = ORIENTED_EDGE ( 'NONE', *, *, #34248, .T. ) ;
#106861 = LINE ( 'NONE', #186430, #72028 ) ;
#106862 = VECTOR ( 'NONE', #132821, 1000.000000000000227 ) ;
#106863 = PLANE ( 'NONE',  #90659 ) ;
#106864 = AXIS2_PLACEMENT_3D ( 'NONE', #38544, #180621, #81478 ) ;
#106866 = CARTESIAN_POINT ( 'NONE',  ( -20.94999999999994600, 65.19115966511134275, -29.92310748452479174 ) ) ;
#106865 = CARTESIAN_POINT ( 'NONE',  ( -22.59999985501179154, 11.74986979300298806, 0.06559866979945758181 ) ) ;
#106867 = TOROIDAL_SURFACE ( 'NONE', #215020, 0.9750000000000019762, 0.1000000000000000056 ) ;
#106869 = ORIENTED_EDGE ( 'NONE', *, *, #204550, .F. ) ;
#106868 = DIRECTION ( 'NONE',  ( 0.000000000000000000, 0.000000000000000000, -1.000000000000000000 ) ) ;
#106870 = EDGE_CURVE ( 'NONE', #2364, #178867, #132499, .T. ) ;
#106871 = ORIENTED_EDGE ( 'NONE', *, *, #22389, .F. ) ;
#106873 = ADVANCED_FACE ( 'NONE', ( #37442 ), #7797, .T. ) ;
#106872 = CARTESIAN_POINT ( 'NONE',  ( 19.97071067695833690, 64.27928932305343324, -78.34685405172075434 ) ) ;
#106874 = DIRECTION ( 'NONE',  ( 1.000000000000000000, 0.000000000000000000, 0.000000000000000000 ) ) ;
#106875 = VECTOR ( 'NONE', #27779, 1000.000000000000227 ) ;
#106876 = DIRECTION ( 'NONE',  ( 0.000000000000000000, -1.000000000000000000, 0.000000000000000000 ) ) ;
#106877 = ORIENTED_EDGE ( 'NONE', *, *, #184251, .F. ) ;
#106879 = CIRCLE ( 'NONE', #52706, 0.09999999999999939493 ) ;
#106878 = CARTESIAN_POINT ( 'NONE',  ( 23.24999999999999645, 61.34848953995434329, -212.6564661897791382 ) ) ;
#106880 = AXIS2_PLACEMENT_3D ( 'NONE', #8350, #51282, #27934 ) ;
#106881 = CARTESIAN_POINT ( 'NONE',  ( -23.25000000000000000, -1.835859311432481045, -145.5044391687985694 ) ) ;
#106882 = DIRECTION ( 'NONE',  ( -1.000000000000000000, 0.000000000000000000, 0.000000000000000000 ) ) ;
#106883 = VERTEX_POINT ( 'NONE', #40025 ) ;
#106884 = EDGE_CURVE ( 'NONE', #31072, #172386, #82931, .T. ) ;
#106885 = DIRECTION ( 'NONE',  ( 0.000000000000000000, 0.000000000000000000, -1.000000000000000000 ) ) ;
#106886 = EDGE_CURVE ( 'NONE', #6487, #249282, #186860, .T. ) ;
#106887 = AXIS2_PLACEMENT_3D ( 'NONE', #106279, #144126, #202832 ) ;
#106888 = ORIENTED_EDGE ( 'NONE', *, *, #61373, .T. ) ;
#106889 = EDGE_CURVE ( 'NONE', #178019, #9008, #220169, .T. ) ;
#106890 = DIRECTION ( 'NONE',  ( 0.000000000000000000, -0.8660254037844459241, -0.4999999999999873990 ) ) ;
#106891 = LINE ( 'NONE', #147309, #102240 ) ;
#106892 = ORIENTED_EDGE ( 'NONE', *, *, #120089, .F. ) ;
#106893 = ORIENTED_EDGE ( 'NONE', *, *, #110340, .F. ) ;
#106894 = CARTESIAN_POINT ( 'NONE',  ( -20.54999999999999716, 71.65000000001182912, -86.27310748452434552 ) ) ;
#106895 = VERTEX_POINT ( 'NONE', #162527 ) ;
#106897 = ORIENTED_EDGE ( 'NONE', *, *, #151172, .T. ) ;
#106896 = CARTESIAN_POINT ( 'NONE',  ( -22.40000000000000213, 1.115488287304407678E-11, -155.7495671075413668 ) ) ;
#106898 = ADVANCED_FACE ( 'NONE', ( #828 ), #57649, .T. ) ;
#106899 = SHAPE_REPRESENTATION ( 'Injection Molded Chain Links 12', ( #2425 ), #81157 ) ;
#106900 = ORIENTED_EDGE ( 'NONE', *, *, #256781, .F. ) ;
#106901 = CIRCLE ( 'NONE', #160912, 0.5000000000000004441 ) ;
#106902 = VECTOR ( 'NONE', #137661, 1000.000000000000000 ) ;
#106904 = ORIENTED_EDGE ( 'NONE', *, *, #162978, .F. ) ;
#106903 = ORIENTED_EDGE ( 'NONE', *, *, #41242, .F. ) ;
#106905 = EDGE_CURVE ( 'NONE', #31696, #90944, #3485, .T. ) ;
#106906 = AXIS2_PLACEMENT_3D ( 'NONE', #44777, #202564, #143860 ) ;
#106907 = CIRCLE ( 'NONE', #252653, 0.09999999999999939493 ) ;
#106908 = CARTESIAN_POINT ( 'NONE',  ( -18.40000000000000213, -9.499999999988851584, -107.1001893912220879 ) ) ;
#106909 = ORIENTED_EDGE ( 'NONE', *, *, #44323, .F. ) ;
#106910 = DIRECTION ( 'NONE',  ( 0.000000000000000000, 0.4930308989875575865, 0.8700118002898125091 ) ) ;
#106911 = CYLINDRICAL_SURFACE ( 'NONE', #70085, 3.999999999999996447 ) ;
#106912 = DIRECTION ( 'NONE',  ( 0.000000000000000000, -0.9651348961777157509, 0.2617529984165031243 ) ) ;
#106913 = CARTESIAN_POINT ( 'NONE',  ( -23.15000000000000213, 64.35000000001203091, -114.7731074845243882 ) ) ;
#106914 = ORIENTED_EDGE ( 'NONE', *, *, #115178, .T. ) ;
#106915 = ORIENTED_EDGE ( 'NONE', *, *, #214869, .F. ) ;
#106916 = DIRECTION ( 'NONE',  ( 0.000000000000000000, -0.8814952561688476074, 0.4721928772777262417 ) ) ;
#106918 = ORIENTED_EDGE ( 'NONE', *, *, #225965, .F. ) ;
#106917 = CARTESIAN_POINT ( 'NONE',  ( 15.74999999999999645, 9.850000000011137402, -150.7500000000000284 ) ) ;
#106919 = CARTESIAN_POINT ( 'NONE',  ( -21.14999999999999858, 64.35000000001195986, -102.9231074845243938 ) ) ;
#106921 = ORIENTED_EDGE ( 'NONE', *, *, #150107, .T. ) ;
#106920 = DIRECTION ( 'NONE',  ( -2.978066053179067751E-16, 1.000000000000000000, 0.000000000000000000 ) ) ;
#106922 = AXIS2_PLACEMENT_3D ( 'NONE', #106010, #123042, #86440 ) ;
#106923 = ORIENTED_EDGE ( 'NONE', *, *, #197644, .F. ) ;
#106924 = FACE_OUTER_BOUND ( 'NONE', #211666, .T. ) ;
#106925 = CIRCLE ( 'NONE', #181948, 0.09999999999999602263 ) ;
#106926 = ORIENTED_EDGE ( 'NONE', *, *, #16633, .T. ) ;
#106927 = ORIENTED_EDGE ( 'NONE', *, *, #88504, .F. ) ;
#106928 = CARTESIAN_POINT ( 'NONE',  ( 20.85000000000000142, 66.90607807833499976, -235.8243394455619182 ) ) ;
#106929 = FACE_OUTER_BOUND ( 'NONE', #175258, .T. ) ;
#106931 = ORIENTED_EDGE ( 'NONE', *, *, #103425, .T. ) ;
#106930 = ORIENTED_EDGE ( 'NONE', *, *, #22280, .T. ) ;
#106932 = EDGE_LOOP ( 'NONE', ( #160242, #174039, #42045, #147524 ) ) ;
#106933 = DIRECTION ( 'NONE',  ( 1.000000000000000000, 0.000000000000000000, 0.000000000000000000 ) ) ;
#106934 = EDGE_LOOP ( 'NONE', ( #16375, #52007, #113928, #119854 ) ) ;
#106935 = ORIENTED_EDGE ( 'NONE', *, *, #81642, .F. ) ;
#106936 = FACE_OUTER_BOUND ( 'NONE', #181085, .T. ) ;
#106937 = VECTOR ( 'NONE', #138664, 1000.000000000000000 ) ;
#106939 = EDGE_LOOP ( 'NONE', ( #161522, #214367, #13179 ) ) ;
#106938 = CARTESIAN_POINT ( 'NONE',  ( 21.05000000000000071, 14.05000000000000071, -27.98630492923908619 ) ) ;
#106940 = CARTESIAN_POINT ( 'NONE',  ( 18.59999999999999787, 68.49522935589659767, -224.1230159437372436 ) ) ;
#106942 = CARTESIAN_POINT ( 'NONE',  ( -18.59999999999999787, 12.87592094156238609, -205.3750039893633073 ) ) ;
#106941 = DIRECTION ( 'NONE',  ( 0.000000000000000000, -0.2617529984164955192, -0.9651348961777178603 ) ) ;
#106943 = CARTESIAN_POINT ( 'NONE',  ( 18.40000000000000213, 85.50000000001264766, -196.5237453873441495 ) ) ;
#106944 = CARTESIAN_POINT ( 'NONE',  ( -13.54795643572458808, 62.05093865251257768, -218.8507522889722452 ) ) ;
#106945 = ORIENTED_EDGE ( 'NONE', *, *, #47341, .T. ) ;
#106946 = ORIENTED_EDGE ( 'NONE', *, *, #27608, .T. ) ;
#106947 = LINE ( 'NONE', #228205, #186132 ) ;
#106948 = CARTESIAN_POINT ( 'NONE',  ( -17.01825945287482966, 10.04999999999998295, -12.65000000000000213 ) ) ;
#106949 = EDGE_CURVE ( 'NONE', #186279, #163243, #153584, .T. ) ;
#106950 = ORIENTED_EDGE ( 'NONE', *, *, #151462, .T. ) ;
#106951 = AXIS2_PLACEMENT_3D ( 'NONE', #53801, #96746, #92912 ) ;
#106952 = VECTOR ( 'NONE', #54082, 1000.000000000000000 ) ;
#106953 = AXIS2_PLACEMENT_3D ( 'NONE', #163620, #44954, #245722 ) ;
#106954 = AXIS2_PLACEMENT_3D ( 'NONE', #63370, #240755, #123369 ) ;
#106955 = SPHERICAL_SURFACE ( 'NONE', #105035, 0.1000000000000000056 ) ;
#106956 = ORIENTED_EDGE ( 'NONE', *, *, #7992, .F. ) ;
#106957 = ORIENTED_EDGE ( 'NONE', *, *, #64019, .T. ) ;
#106958 = CARTESIAN_POINT ( 'NONE',  ( -20.94999999999999929, 77.26178616857691850, -94.93660852097882241 ) ) ;
#106959 = EDGE_CURVE ( 'NONE', #232547, #67059, #64680, .T. ) ;
#106960 = CARTESIAN_POINT ( 'NONE',  ( 20.94999999999999929, 6.550000000000000711, -12.24999999999999289 ) ) ;
#106961 = VERTEX_POINT ( 'NONE', #204183 ) ;
#106962 = DIRECTION ( 'NONE',  ( -1.000000000000000000, 2.952720810173289112E-16, 2.061873921506763405E-30 ) ) ;
#106963 = CARTESIAN_POINT ( 'NONE',  ( 21.11747605621531321, 8.778708005504054057, -112.7445631697898136 ) ) ;
#106964 = ORIENTED_EDGE ( 'NONE', *, *, #226880, .F. ) ;
#106965 = CARTESIAN_POINT ( 'NONE',  ( 20.94999999999999574, 74.83729825007431202, -161.9231074845243654 ) ) ;
#106966 = FACE_OUTER_BOUND ( 'NONE', #47481, .T. ) ;
#106968 = CARTESIAN_POINT ( 'NONE',  ( 18.49999999999999289, 64.35000000001245724, -170.0231074845244166 ) ) ;
#106967 = DIRECTION ( 'NONE',  ( 0.000000000000000000, 0.000000000000000000, 1.000000000000000000 ) ) ;
#106969 = EDGE_CURVE ( 'NONE', #217845, #155156, #159962, .T. ) ;
#106971 = ADVANCED_FACE ( 'NONE', ( #4690 ), #5977, .T. ) ;
#106970 = PLANE ( 'NONE',  #220068 ) ;
#106972 = CARTESIAN_POINT ( 'NONE',  ( -20.00857864376270001, 9.150000000011157653, -54.75000000000000000 ) ) ;
#106973 = DIRECTION ( 'NONE',  ( -1.000000000000000000, 1.836970198721029934E-16, 1.282749433769087757E-30 ) ) ;
#106974 = VECTOR ( 'NONE', #77506, 1000.000000000000000 ) ;
#106975 = AXIS2_PLACEMENT_3D ( 'NONE', #80383, #26563, #206466 ) ;
#106976 = AXIS2_PLACEMENT_3D ( 'NONE', #120882, #200391, #8304 ) ;
#106977 = ORIENTED_EDGE ( 'NONE', *, *, #163938, .F. ) ;
#106979 = EDGE_LOOP ( 'NONE', ( #122355, #176157, #249939, #145501 ) ) ;
#106978 = EDGE_LOOP ( 'NONE', ( #205723, #133577, #72384, #437 ) ) ;
#106980 = AXIS2_PLACEMENT_3D ( 'NONE', #20257, #198880, #99755 ) ;
#106981 = EDGE_LOOP ( 'NONE', ( #92908, #180888, #31831, #85870 ) ) ;
#106982 = EDGE_CURVE ( 'NONE', #84861, #256406, #190969, .T. ) ;
#106983 = CARTESIAN_POINT ( 'NONE',  ( -22.50000000000000000, 0.09999999999999939493, 0.000000000000000000 ) ) ;
#106984 = CARTESIAN_POINT ( 'NONE',  ( -16.86578989773640913, 66.01519019875300387, -82.05844259790215744 ) ) ;
#106986 = CARTESIAN_POINT ( 'NONE',  ( -20.64999999999999858, 8.653397185701672711, -220.7611668973962367 ) ) ;
#106985 = DIRECTION ( 'NONE',  ( 0.000000000000000000, 1.000000000000000000, 0.000000000000000000 ) ) ;
#106987 = CARTESIAN_POINT ( 'NONE',  ( 20.85000000000000142, 11.65000000001115943, -100.5000000000000426 ) ) ;
#106988 = ORIENTED_EDGE ( 'NONE', *, *, #215932, .F. ) ;
#106989 = CARTESIAN_POINT ( 'NONE',  ( 21.30000000000002558, 36.65892442174472876, -249.5511627012454596 ) ) ;
#106990 = DIRECTION ( 'NONE',  ( 0.000000000000000000, -0.08413937888704771384, 0.9964539953858891908 ) ) ;
#106991 = CARTESIAN_POINT ( 'NONE',  ( -23.15000000000000213, 85.00000000001222134, -146.4170766071767389 ) ) ;
#106992 = CARTESIAN_POINT ( 'NONE',  ( -21.05000000000000071, 1.434427651312520480, -230.7796976835703049 ) ) ;
#106993 = ORIENTED_EDGE ( 'NONE', *, *, #172323, .T. ) ;
#106994 = CARTESIAN_POINT ( 'NONE',  ( 23.15000000000000213, -11.64999999998883595, -88.75000000000004263 ) ) ;
#106995 = DIRECTION ( 'NONE',  ( 0.000000000000000000, 0.000000000000000000, 1.000000000000000000 ) ) ;
#106996 = ORIENTED_EDGE ( 'NONE', *, *, #46221, .T. ) ;
#106998 = VERTEX_POINT ( 'NONE', #43846 ) ;
#106997 = EDGE_CURVE ( 'NONE', #200607, #251965, #174432, .T. ) ;
#106999 = DIRECTION ( 'NONE',  ( 1.000000000000000000, 0.000000000000000000, 0.000000000000000000 ) ) ;
#107000 = LINE ( 'NONE', #164435, #64586 ) ;
#107001 = ADVANCED_FACE ( 'NONE', ( #42548 ), #141653, .F. ) ;
#107002 = CARTESIAN_POINT ( 'NONE',  ( -18.59999999999999787, 68.20313450767837082, -227.8297066677462794 ) ) ;
#107003 = FACE_OUTER_BOUND ( 'NONE', #87200, .T. ) ;
#107004 = CARTESIAN_POINT ( 'NONE',  ( -18.59999999999999787, -1.261786168565025568, -8.086498963545480478 ) ) ;
#107005 = VECTOR ( 'NONE', #109285, 1000.000000000000227 ) ;
#107006 = DIRECTION ( 'NONE',  ( 0.000000000000000000, -7.124650136758311291E-15, 1.000000000000000000 ) ) ;
#107007 = ORIENTED_EDGE ( 'NONE', *, *, #182500, .F. ) ;
#107008 = CARTESIAN_POINT ( 'NONE',  ( -23.15000000000000213, -8.999999999988844479, -157.6060308773475924 ) ) ;
#107010 = CARTESIAN_POINT ( 'NONE',  ( -20.64999999999999858, -6.688413578037177842, -212.5825622730469036 ) ) ;
#107009 = DIRECTION ( 'NONE',  ( 1.000000000000000000, 0.000000000000000000, 0.000000000000000000 ) ) ;
#107011 = DIRECTION ( 'NONE',  ( 1.000000000000000000, 0.000000000000000000, 0.000000000000000000 ) ) ;
#107012 = EDGE_CURVE ( 'NONE', #252230, #197089, #53576, .T. ) ;
#107013 = TOROIDAL_SURFACE ( 'NONE', #119502, 11.65000000000000036, 0.1000000000000000056 ) ;
#107014 = LINE ( 'NONE', #129169, #245700 ) ;
#107015 = DIRECTION ( 'NONE',  ( 0.000000000000000000, 1.000000000000000000, 0.000000000000000000 ) ) ;
#107016 = DIRECTION ( 'NONE',  ( 0.000000000000000000, -0.2128009952263604232, 0.9770955615653316162 ) ) ;
#107017 = CIRCLE ( 'NONE', #165282, 0.4999999999999990008 ) ;
#107019 = ORIENTED_EDGE ( 'NONE', *, *, #138552, .T. ) ;
#107018 = DIRECTION ( 'NONE',  ( 1.020425574104003999E-15, -0.8814952561688430555, 0.4721928772777346239 ) ) ;
#107020 =( GEOMETRIC_REPRESENTATION_CONTEXT ( 3 ) GLOBAL_UNCERTAINTY_ASSIGNED_CONTEXT ( ( #144310 ) ) GLOBAL_UNIT_ASSIGNED_CONTEXT ( ( #6955, #77749, #30417 ) ) REPRESENTATION_CONTEXT ( 'NONE', 'WORKASPACE' ) );
#107021 = AXIS2_PLACEMENT_3D ( 'NONE', #151550, #56248, #92814 ) ;
#107022 = AXIS2_PLACEMENT_3D ( 'NONE', #222471, #163820, #245921 ) ;
#107023 = CARTESIAN_POINT ( 'NONE',  ( -18.50000000000000000, 2.272311100394797556, -217.9150152700588876 ) ) ;
#107024 = DIRECTION ( 'NONE',  ( 0.000000000000000000, -0.8814952561688476074, 0.4721928772777262417 ) ) ;
#107025 = CARTESIAN_POINT ( 'NONE',  ( 13.88302573338718737, 9.457410944778565920, -149.0000839737900549 ) ) ;
#107026 = VECTOR ( 'NONE', #134324, 1000.000000000000114 ) ;
#107027 = ORIENTED_EDGE ( 'NONE', *, *, #157508, .T. ) ;
#107028 = DIRECTION ( 'NONE',  ( 0.000000000000000000, -0.1350103645451904977, -0.9908441862701596881 ) ) ;
#107029 = CIRCLE ( 'NONE', #27973, 0.1999999999999987899 ) ;
#107030 = CARTESIAN_POINT ( 'NONE',  ( -21.05000000000000071, -0.09999999998884338825, -93.95934304829879125 ) ) ;
#107031 = CARTESIAN_POINT ( 'NONE',  ( -20.85000000000000142, 70.22659352830977753, -197.9852579278363578 ) ) ;
#107032 = ADVANCED_FACE ( 'NONE', ( #65971 ), #200351, .T. ) ;
#107033 = CIRCLE ( 'NONE', #65350, 0.1000000000000056677 ) ;
#107034 = EDGE_CURVE ( 'NONE', #144450, #76379, #203426, .T. ) ;
#107035 = ORIENTED_EDGE ( 'NONE', *, *, #147076, .T. ) ;
#107036 = CARTESIAN_POINT ( 'NONE',  ( -16.97092634996638338, 65.99911103366348186, -56.89296471822659385 ) ) ;
#107039 = ORIENTED_EDGE ( 'NONE', *, *, #193069, .T. ) ;
#107038 = DIRECTION ( 'NONE',  ( -1.000000000000000000, -2.952720810173289112E-16, 0.000000000000000000 ) ) ;
#107037 = CIRCLE ( 'NONE', #236229, 0.09999999999999939493 ) ;
#107041 = CARTESIAN_POINT ( 'NONE',  ( -23.15000000000000213, 71.65000000001207070, -124.3731074845243256 ) ) ;
#107040 = CARTESIAN_POINT ( 'NONE',  ( -23.15000000000000213, 76.00000000001165290, -69.52310748452431710 ) ) ;
#107042 = AXIS2_PLACEMENT_3D ( 'NONE', #82147, #85996, #161745 ) ;
#107044 = EDGE_CURVE ( 'NONE', #3677, #33572, #70173, .T. ) ;
#107043 = CARTESIAN_POINT ( 'NONE',  ( 23.14999999999999858, 71.22429906543254674, -114.8718755885703047 ) ) ;
#107045 = EDGE_CURVE ( 'NONE', #241204, #26573, #253468, .T. ) ;
#107047 = ORIENTED_EDGE ( 'NONE', *, *, #155750, .F. ) ;
#107046 = AXIS2_PLACEMENT_3D ( 'NONE', #57580, #220536, #194572 ) ;
#107048 = CARTESIAN_POINT ( 'NONE',  ( 21.05000000000000071, 18.94619844861577462, -232.5189405348540674 ) ) ;
#107049 = DIRECTION ( 'NONE',  ( 0.000000000000000000, 0.000000000000000000, 1.000000000000000000 ) ) ;
#107050 = CARTESIAN_POINT ( 'NONE',  ( -21.04999999999999716, 69.72991413632300350, -136.5579754875374192 ) ) ;
#107051 = DIRECTION ( 'NONE',  ( -0.000000000000000000, -0.9579639084728132081, -0.2868887416116073230 ) ) ;
#107052 = DIRECTION ( 'NONE',  ( 0.000000000000000000, -1.000000000000000000, 0.000000000000000000 ) ) ;
#107053 = ADVANCED_FACE ( 'NONE', ( #247160 ), #9845, .F. ) ;
#107054 = EDGE_LOOP ( 'NONE', ( #183181, #44720, #131198, #47230, #182714 ) ) ;
#107055 = DIRECTION ( 'NONE',  ( 0.000000000000000000, -0.8814952561688516042, 0.4721928772777186922 ) ) ;
#107056 = LINE ( 'NONE', #169659, #138130 ) ;
#107057 = ADVANCED_FACE ( 'NONE', ( #110221 ), #199327, .T. ) ;
#107058 = AXIS2_PLACEMENT_3D ( 'NONE', #217912, #198373, #19758 ) ;
#107059 = SURFACE_STYLE_USAGE ( .BOTH. , #33685 ) ;
#107061 = ADVANCED_FACE ( 'NONE', ( #125927 ), #41126, .F. ) ;
#107060 = EDGE_CURVE ( 'NONE', #21668, #144797, #225970, .T. ) ;
#107062 = AXIS2_PLACEMENT_3D ( 'NONE', #27214, #106696, #224081 ) ;
#107063 = ORIENTED_EDGE ( 'NONE', *, *, #29141, .F. ) ;
#107064 = EDGE_CURVE ( 'NONE', #52702, #85372, #182590, .T. ) ;
#107065 = ORIENTED_EDGE ( 'NONE', *, *, #69577, .F. ) ;
#107066 = LINE ( 'NONE', #246577, #63211 ) ;
#107067 = DIRECTION ( 'NONE',  ( 0.000000000000000000, 0.2617529984165174461, 0.9651348961777118651 ) ) ;
#107068 = DIRECTION ( 'NONE',  ( -2.827886303505249259E-16, -0.8660254037844378194, -0.5000000000000016653 ) ) ;
#107069 = EDGE_CURVE ( 'NONE', #179078, #48863, #128586, .T. ) ;
#107070 = PLANE ( 'NONE',  #12234 ) ;
#107071 = CARTESIAN_POINT ( 'NONE',  ( 23.24999999999999645, 79.90000000001214175, -136.5231074845243029 ) ) ;
#107072 = AXIS2_PLACEMENT_3D ( 'NONE', #209251, #93153, #29381 ) ;
#107074 = CYLINDRICAL_SURFACE ( 'NONE', #245159, 7.899999999999990585 ) ;
#107073 = DIRECTION ( 'NONE',  ( 0.000000000000000000, 0.000000000000000000, -1.000000000000000000 ) ) ;
#107075 = DIRECTION ( 'NONE',  ( 0.000000000000000000, 0.000000000000000000, -1.000000000000000000 ) ) ;
#107077 = EDGE_CURVE ( 'NONE', #126171, #158135, #16181, .T. ) ;
#107076 = DIRECTION ( 'NONE',  ( 1.000000000000000000, 0.000000000000000000, 0.000000000000000000 ) ) ;
#107079 = ADVANCED_FACE ( 'NONE', ( #86795 ), #206767, .F. ) ;
#107078 = CARTESIAN_POINT ( 'NONE',  ( -23.25000000000000000, 76.00000000001165290, -69.52310748452431710 ) ) ;
#107080 = DIRECTION ( 'NONE',  ( 1.000000000000000000, 0.000000000000000000, 0.000000000000000000 ) ) ;
#107082 = ORIENTED_EDGE ( 'NONE', *, *, #20595, .T. ) ;
#107081 = DIRECTION ( 'NONE',  ( 1.000000000000000000, 0.000000000000000000, 0.000000000000000000 ) ) ;
#107083 = CARTESIAN_POINT ( 'NONE',  ( 21.09813707148777340, 69.61493789427588297, -170.0544589840539231 ) ) ;
#107084 = DIRECTION ( 'NONE',  ( 1.000000000000000000, -0.000000000000000000, 0.000000000000000000 ) ) ;
#107086 = DIRECTION ( 'NONE',  ( -1.000000000000000000, -0.000000000000000000, -0.000000000000000000 ) ) ;
#107085 = CARTESIAN_POINT ( 'NONE',  ( -23.15000000000000213, 73.40000000001185754, -89.79848556176223440 ) ) ;
#107087 = VECTOR ( 'NONE', #181999, 1000.000000000000000 ) ;
#107088 = EDGE_CURVE ( 'NONE', #232204, #41537, #185915, .T. ) ;
#107089 = ORIENTED_EDGE ( 'NONE', *, *, #198656, .F. ) ;
#107090 = DIRECTION ( 'NONE',  ( 0.000000000000000000, 0.000000000000000000, 1.000000000000000000 ) ) ;
#107091 = CARTESIAN_POINT ( 'NONE',  ( -23.15000000000000213, -11.48912529306489994, -197.8999999999999773 ) ) ;
#107092 = DIRECTION ( 'NONE',  ( -0.000000000000000000, 0.000000000000000000, 1.000000000000000000 ) ) ;
#107093 = DIRECTION ( 'NONE',  ( 1.000000000000000000, 0.000000000000000000, 0.000000000000000000 ) ) ;
#107094 = DIRECTION ( 'NONE',  ( -1.000000000000000000, 2.986185139342070877E-16, -6.665775143889692774E-16 ) ) ;
#107095 = ORIENTED_EDGE ( 'NONE', *, *, #132674, .F. ) ;
#107096 = ADVANCED_FACE ( 'NONE', ( #251000 ), #28159, .T. ) ;
#107097 = AXIS2_PLACEMENT_3D ( 'NONE', #197322, #76099, #74859 ) ;
#107098 = EDGE_LOOP ( 'NONE', ( #94909, #146162, #131552 ) ) ;
#107099 = TOROIDAL_SURFACE ( 'NONE', #102987, 11.65000000000000036, 0.1000000000000000056 ) ;
#107100 = AXIS2_PLACEMENT_3D ( 'NONE', #240117, #1484, #83566 ) ;
#107101 = CIRCLE ( 'NONE', #173802, 4.049999999999998046 ) ;
#107102 = EDGE_CURVE ( 'NONE', #43818, #83438, #11904, .T. ) ;
#107103 = DIRECTION ( 'NONE',  ( 0.000000000000000000, -1.000000000000000000, -2.891205793294679805E-16 ) ) ;
#107104 = ORIENTED_EDGE ( 'NONE', *, *, #4137, .F. ) ;
#107105 = LINE ( 'NONE', #186664, #55448 ) ;
#107106 = VERTEX_POINT ( 'NONE', #205468 ) ;
#107107 = AXIS2_PLACEMENT_3D ( 'NONE', #226553, #222710, #47927 ) ;
#107108 = DIRECTION ( 'NONE',  ( 0.000000000000000000, 0.000000000000000000, 1.000000000000000000 ) ) ;
#107109 = CYLINDRICAL_SURFACE ( 'NONE', #119158, 0.09999999999998898659 ) ;
#107110 = CARTESIAN_POINT ( 'NONE',  ( 20.94999999999999574, 44.00266445878927613, -258.8505972146074896 ) ) ;
#107111 = ORIENTED_EDGE ( 'NONE', *, *, #133935, .F. ) ;
#107112 = EDGE_CURVE ( 'NONE', #250008, #22041, #51507, .T. ) ;
#107113 = CARTESIAN_POINT ( 'NONE',  ( -23.15000000000000213, 85.00000000001197975, -112.9170766071766820 ) ) ;
#107115 = VECTOR ( 'NONE', #213778, 1000.000000000000000 ) ;
#107114 = CARTESIAN_POINT ( 'NONE',  ( -21.07954763557684430, 65.51098451068844497, -241.9465028898075047 ) ) ;
#107116 = CARTESIAN_POINT ( 'NONE',  ( -18.50000000000000000, 11.75000000001115197, -67.10000000000005116 ) ) ;
#107117 = CARTESIAN_POINT ( 'NONE',  ( 18.59999999999999076, 64.35000000001141984, -36.02310748452440237 ) ) ;
#107118 = DIRECTION ( 'NONE',  ( 0.000000000000000000, 0.000000000000000000, -1.000000000000000000 ) ) ;
#107119 = DIRECTION ( 'NONE',  ( 8.673617379884087537E-15, 6.982962677686266711E-15, -1.000000000000000000 ) ) ;
#107120 = CARTESIAN_POINT ( 'NONE',  ( 15.75000000000000000, 62.53104822794671236, -217.4650886355768478 ) ) ;
#107121 = EDGE_LOOP ( 'NONE', ( #212894, #162408, #130770, #12808 ) ) ;
#107123 = CARTESIAN_POINT ( 'NONE',  ( -22.49510344025093644, 75.93287232181852175, -215.1730775896386376 ) ) ;
#107122 = DIRECTION ( 'NONE',  ( 0.000000000000000000, -0.2617529984165031243, -0.9651348961777157509 ) ) ;
#107124 = EDGE_LOOP ( 'NONE', ( #130523, #15415, #14299, #96513 ) ) ;
#107126 = ORIENTED_EDGE ( 'NONE', *, *, #133471, .T. ) ;
#107125 = FACE_OUTER_BOUND ( 'NONE', #159201, .T. ) ;
#107127 = CIRCLE ( 'NONE', #111229, 0.09999999999999938105 ) ;
#107128 = EDGE_LOOP ( 'NONE', ( #8577, #135521, #237425, #171105 ) ) ;
#107129 = CARTESIAN_POINT ( 'NONE',  ( -20.54999999999999716, 68.85000000001156195, -57.17310748452437252 ) ) ;
#107130 = CARTESIAN_POINT ( 'NONE',  ( 18.51697539158856642, 10.31565961587946312, -72.53641941191783360 ) ) ;
#107131 = DIRECTION ( 'NONE',  ( -0.000000000000000000, 1.000000000000000000, 6.982962677686266711E-15 ) ) ;
#107132 = DIRECTION ( 'NONE',  ( 0.000000000000000000, -0.8700118002898359348, 0.4930308989875165082 ) ) ;
#107133 = ORIENTED_EDGE ( 'NONE', *, *, #73539, .T. ) ;
#107134 = DIRECTION ( 'NONE',  ( 0.000000000000000000, -0.9651348961777379554, 0.2617529984164210233 ) ) ;
#107135 = PLANE ( 'NONE',  #89747 ) ;
#107136 = EDGE_LOOP ( 'NONE', ( #27506, #200203, #51623, #142654 ) ) ;
#107137 = CARTESIAN_POINT ( 'NONE',  ( 18.41789779300690455, -9.499999999988844479, -174.5320696663606554 ) ) ;
#107138 = EDGE_CURVE ( 'NONE', #46518, #153680, #29743, .T. ) ;
#107139 = DIRECTION ( 'NONE',  ( -1.000000000000000000, 0.000000000000000000, 0.000000000000000000 ) ) ;
#107140 = ORIENTED_EDGE ( 'NONE', *, *, #129604, .F. ) ;
#107141 = VECTOR ( 'NONE', #242364, 1000.000000000000000 ) ;
#107142 = MANIFOLD_SOLID_BREP ( 'Stock-MAS-200-1', #16078 ) ;
#107143 = ADVANCED_FACE ( 'NONE', ( #13692 ), #29452, .T. ) ;
#107144 = DIRECTION ( 'NONE',  ( -0.000000000000000000, -6.982962677686266711E-15, 1.000000000000000000 ) ) ;
#107145 = TOROIDAL_SURFACE ( 'NONE', #36260, 0.2000000000000000111, 0.1000000000000000056 ) ;
#107146 = AXIS2_PLACEMENT_3D ( 'NONE', #56013, #36514, #232135 ) ;
#107147 = ORIENTED_EDGE ( 'NONE', *, *, #103325, .F. ) ;
#107148 = LINE ( 'NONE', #122881, #117356 ) ;
#107149 = ORIENTED_EDGE ( 'NONE', *, *, #6525, .F. ) ;
#107150 = EDGE_CURVE ( 'NONE', #140260, #224599, #249215, .T. ) ;
#107151 = EDGE_CURVE ( 'NONE', #217355, #151273, #66710, .T. ) ;
#107152 = CARTESIAN_POINT ( 'NONE',  ( -21.55000000000000426, 7.750000000011159074, -155.1500000000000057 ) ) ;
#107153 = CYLINDRICAL_SURFACE ( 'NONE', #5957, 4.049999999999998046 ) ;
#107154 = FACE_OUTER_BOUND ( 'NONE', #51393, .T. ) ;
#107155 = ADVANCED_FACE ( 'NONE', ( #139727 ), #160627, .T. ) ;
#107156 = AXIS2_PLACEMENT_3D ( 'NONE', #90148, #146281, #8080 ) ;
#107157 = VECTOR ( 'NONE', #152360, 1000.000000000000000 ) ;
#107158 = DIRECTION ( 'NONE',  ( 0.000000000000000000, 0.8814952561688438326, -0.4721928772777331806 ) ) ;
#107159 = LINE ( 'NONE', #6782, #89062 ) ;
#107160 = DIRECTION ( 'NONE',  ( 0.000000000000000000, 0.000000000000000000, -1.000000000000000000 ) ) ;
#107161 = ORIENTED_EDGE ( 'NONE', *, *, #248566, .T. ) ;
#107163 = DIRECTION ( 'NONE',  ( 0.000000000000000000, 0.2617529984165152257, 0.9651348961777124202 ) ) ;
#107162 = LINE ( 'NONE', #31522, #52875 ) ;
#107164 = ADVANCED_FACE ( 'NONE', ( #15000 ), #95781, .T. ) ;
#107165 = EDGE_LOOP ( 'NONE', ( #208961, #144810, #195142, #117128 ) ) ;
#107166 = AXIS2_PLACEMENT_3D ( 'NONE', #106183, #149208, #226121 ) ;
#107167 = CARTESIAN_POINT ( 'NONE',  ( 21.05000000000000071, 8.776282895303632259, -175.9880007215843136 ) ) ;
#107168 = LINE ( 'NONE', #186734, #215137 ) ;
#107169 = DIRECTION ( 'NONE',  ( -1.000000000000000000, -0.000000000000000000, -0.000000000000000000 ) ) ;
#107171 = ORIENTED_EDGE ( 'NONE', *, *, #210680, .F. ) ;
#107170 = DIRECTION ( 'NONE',  ( 1.020425574104004196E-15, 1.210927747993693964E-31, -1.000000000000000000 ) ) ;
#107173 = ORIENTED_EDGE ( 'NONE', *, *, #90028, .T. ) ;
#107172 = DIRECTION ( 'NONE',  ( -1.000000000000000000, 0.000000000000000000, 0.000000000000000000 ) ) ;
#107174 = DIRECTION ( 'NONE',  ( 0.000000000000000000, -0.6728971962617862346, 0.7397360091701815632 ) ) ;
#107175 = FACE_OUTER_BOUND ( 'NONE', #241521, .T. ) ;
#107177 = VERTEX_POINT ( 'NONE', #94506 ) ;
#107176 = CARTESIAN_POINT ( 'NONE',  ( -16.88853107394619002, 9.950878483358135185, -154.8529363468922497 ) ) ;
#107178 = VECTOR ( 'NONE', #253222, 1000.000000000000114 ) ;
#107179 = EDGE_CURVE ( 'NONE', #51868, #183416, #254119, .T. ) ;
#107180 = DIRECTION ( 'NONE',  ( 0.000000000000000000, 0.8149014228131966631, -0.5795995782408988051 ) ) ;
#107181 = DIRECTION ( 'NONE',  ( 0.000000000000000000, -0.08413937888704771384, 0.9964539953858891908 ) ) ;
#107182 = ORIENTED_EDGE ( 'NONE', *, *, #79816, .T. ) ;
#107183 = DIRECTION ( 'NONE',  ( 1.000000000000000000, 0.000000000000000000, 0.000000000000000000 ) ) ;
#107184 = ORIENTED_EDGE ( 'NONE', *, *, #154440, .F. ) ;
#107185 = CARTESIAN_POINT ( 'NONE',  ( 20.94999999999999929, 7.120270961708750512, -204.6595630418393057 ) ) ;
#107186 = CARTESIAN_POINT ( 'NONE',  ( -20.94999999999999929, 1.115600667400684642E-11, -155.7000000000000455 ) ) ;
#107187 = AXIS2_PLACEMENT_3D ( 'NONE', #205514, #223790, #66015 ) ;
#107188 = VERTEX_POINT ( 'NONE', #79747 ) ;
#107189 = EDGE_CURVE ( 'NONE', #220406, #58187, #104280, .T. ) ;
#107190 = CARTESIAN_POINT ( 'NONE',  ( 20.99999999999999645, 66.25000000001182343, -82.17310748452439384 ) ) ;
#107191 = EDGE_CURVE ( 'NONE', #6351, #154564, #150115, .T. ) ;
#107192 = DIRECTION ( 'NONE',  ( 0.000000000000000000, 0.000000000000000000, -1.000000000000000000 ) ) ;
#107193 = AXIS2_PLACEMENT_3D ( 'NONE', #96823, #193411, #229947 ) ;
#107194 = VERTEX_POINT ( 'NONE', #74984 ) ;
#107195 = CIRCLE ( 'NONE', #232134, 0.09999999999999986677 ) ;
#107196 = CIRCLE ( 'NONE', #215540, 0.1000000000000124678 ) ;
#107197 = DIRECTION ( 'NONE',  ( 0.000000000000000000, 1.000000000000000000, 0.000000000000000000 ) ) ;
#107198 = PRODUCT_DEFINITION_FORMATION_WITH_SPECIFIED_SOURCE ( 'ANY', '', #5496, .NOT_KNOWN. ) ;
#107199 = ADVANCED_FACE ( 'NONE', ( #134896 ), #154531, .F. ) ;
#107200 = ORIENTED_EDGE ( 'NONE', *, *, #223928, .T. ) ;
#107201 = ORIENTED_EDGE ( 'NONE', *, *, #237402, .T. ) ;
#107203 = PLANE ( 'NONE',  #11193 ) ;
#107202 = AXIS2_PLACEMENT_3D ( 'NONE', #113368, #11720, #75547 ) ;
#107204 = ORIENTED_EDGE ( 'NONE', *, *, #255543, .T. ) ;
#107205 = CARTESIAN_POINT ( 'NONE',  ( 18.39999999999999858, -0.9152171842607033092, -242.2974985173726452 ) ) ;
#107206 = AXIS2_PLACEMENT_3D ( 'NONE', #148085, #105055, #144209 ) ;
#107207 = ORIENTED_EDGE ( 'NONE', *, *, #84798, .T. ) ;
#107209 = ORIENTED_EDGE ( 'NONE', *, *, #108141, .F. ) ;
#107208 = DIRECTION ( 'NONE',  ( -0.000000000000000000, 0.000000000000000000, 1.000000000000000000 ) ) ;
#107210 = EDGE_CURVE ( 'NONE', #47267, #242166, #214451, .T. ) ;
#107211 = EDGE_CURVE ( 'NONE', #117904, #144564, #83422, .T. ) ;
#107212 = CARTESIAN_POINT ( 'NONE',  ( -21.00250684356852560, 11.75000000001115197, -74.01480576875988504 ) ) ;
#107213 = ORIENTED_EDGE ( 'NONE', *, *, #235997, .T. ) ;
#107214 = DIRECTION ( 'NONE',  ( 1.000000000000000000, 0.000000000000000000, 0.000000000000000000 ) ) ;
#107215 = VERTEX_POINT ( 'NONE', #220575 ) ;
#107218 = EDGE_LOOP ( 'NONE', ( #178398, #223298, #174185, #145068 ) ) ;
#107217 = ORIENTED_EDGE ( 'NONE', *, *, #120059, .F. ) ;
#107216 = DIRECTION ( 'NONE',  ( 1.000000000000000000, 0.000000000000000000, 0.000000000000000000 ) ) ;
#107219 = CARTESIAN_POINT ( 'NONE',  ( -20.00857864376270001, 66.85000000001228670, -157.7731074845244166 ) ) ;
#107220 = ADVANCED_FACE ( 'NONE', ( #101874 ), #2784, .F. ) ;
#107221 = CARTESIAN_POINT ( 'NONE',  ( 20.85000000000000142, 7.661991824395936845, -241.5144583139544636 ) ) ;
#107223 = EDGE_LOOP ( 'NONE', ( #149944, #146746 ) ) ;
#107222 = VECTOR ( 'NONE', #141727, 999.9999999999998863 ) ;
#107224 = CIRCLE ( 'NONE', #148943, 0.1000000000000028644 ) ;
#107225 = VECTOR ( 'NONE', #65258, 1000.000000000000000 ) ;
#107226 = CIRCLE ( 'NONE', #61450, 0.09999999999999939493 ) ;
#107227 = ORIENTED_EDGE ( 'NONE', *, *, #204716, .F. ) ;
#107228 = AXIS2_PLACEMENT_3D ( 'NONE', #203408, #3918, #19638 ) ;
#107229 = CARTESIAN_POINT ( 'NONE',  ( -21.14999999999999858, 69.45934304831143891, -203.5231074845243882 ) ) ;
#107230 = EDGE_CURVE ( 'NONE', #52558, #38015, #87529, .T. ) ;
#107231 = CARTESIAN_POINT ( 'NONE',  ( 20.27550659511089037, 44.43555011622476769, -235.9687455856084739 ) ) ;
#107232 =( BOUNDED_CURVE ( )  B_SPLINE_CURVE ( 3, ( #95446, #18488, #116316, #214120 ),
 .UNSPECIFIED., .F., .F. ) 
 B_SPLINE_CURVE_WITH_KNOTS ( ( 4, 4 ),
 ( 3.141592653589793116, 4.712388980384689674 ),
 .UNSPECIFIED. ) 
 CURVE ( )  GEOMETRIC_REPRESENTATION_ITEM ( )  RATIONAL_B_SPLINE_CURVE ( ( 1.000000000000000000, 0.8047378541243649375, 0.8047378541243649375, 1.000000000000000000 ) ) 
 REPRESENTATION_ITEM ( '' )  );
#107234 = ORIENTED_EDGE ( 'NONE', *, *, #163180, .T. ) ;
#107233 = FACE_OUTER_BOUND ( 'NONE', #19439, .T. ) ;
#107235 = DIRECTION ( 'NONE',  ( 0.000000000000000000, 0.000000000000000000, 1.000000000000000000 ) ) ;
#107236 = ORIENTED_EDGE ( 'NONE', *, *, #248474, .T. ) ;
#107237 = CIRCLE ( 'NONE', #240518, 12.77499999999999503 ) ;
#107238 = CARTESIAN_POINT ( 'NONE',  ( 21.05000000000000071, 86.43238724539048690, -209.5644480942280836 ) ) ;
#107239 = DIRECTION ( 'NONE',  ( 0.000000000000000000, 0.000000000000000000, 1.000000000000000000 ) ) ;
#107240 = ORIENTED_EDGE ( 'NONE', *, *, #82875, .F. ) ;
#107241 = DIRECTION ( 'NONE',  ( -1.000000000000000000, -0.000000000000000000, 0.000000000000000000 ) ) ;
#107242 = DIRECTION ( 'NONE',  ( 0.000000000000000000, 0.000000000000000000, -1.000000000000000000 ) ) ;
#107243 = VERTEX_POINT ( 'NONE', #4083 ) ;
#107244 = FACE_OUTER_BOUND ( 'NONE', #108430, .T. ) ;
#107245 = CARTESIAN_POINT ( 'NONE',  ( 20.94999999999999929, 1.115600667400684642E-11, -68.90000000000000568 ) ) ;
#107246 = AXIS2_PLACEMENT_3D ( 'NONE', #30042, #89970, #109532 ) ;
#107247 = AXIS2_PLACEMENT_3D ( 'NONE', #195942, #216759, #75976 ) ;
#107248 = CIRCLE ( 'NONE', #173946, 4.000000000000003553 ) ;
#107250 = ORIENTED_EDGE ( 'NONE', *, *, #155424, .F. ) ;
#107249 = ORIENTED_EDGE ( 'NONE', *, *, #161379, .F. ) ;
#107251 = ORIENTED_EDGE ( 'NONE', *, *, #132529, .T. ) ;
#107252 = DIRECTION ( 'NONE',  ( 0.000000000000000000, 0.000000000000000000, 1.000000000000000000 ) ) ;
#107253 = ORIENTED_EDGE ( 'NONE', *, *, #58589, .T. ) ;
#107254 = ORIENTED_EDGE ( 'NONE', *, *, #81052, .T. ) ;
#107255 = CARTESIAN_POINT ( 'NONE',  ( -20.64999999999999858, 26.29846678923107106, -241.7324770631975639 ) ) ;
#107256 = DIRECTION ( 'NONE',  ( 0.000000000000000000, 0.000000000000000000, -1.000000000000000000 ) ) ;
#107257 = EDGE_LOOP ( 'NONE', ( #150747, #225446, #169987 ) ) ;
#107258 = CIRCLE ( 'NONE', #248931, 0.1000000000000053069 ) ;
#107259 = CIRCLE ( 'NONE', #153098, 0.09999999999999939493 ) ;
#107260 = ORIENTED_EDGE ( 'NONE', *, *, #226161, .F. ) ;
#107261 = ORIENTED_EDGE ( 'NONE', *, *, #34882, .T. ) ;
#107262 = ADVANCED_FACE ( 'NONE', ( #242688 ), #79151, .T. ) ;
#107263 = AXIS2_PLACEMENT_3D ( 'NONE', #65587, #6895, #147701 ) ;
#107264 = DIRECTION ( 'NONE',  ( 0.000000000000000000, -1.000000000000000000, -6.982962677686266711E-15 ) ) ;
#107265 = ORIENTED_EDGE ( 'NONE', *, *, #59342, .F. ) ;
#107266 = DIRECTION ( 'NONE',  ( 0.000000000000000000, -7.272083257015735086E-15, 1.000000000000000000 ) ) ;
#107267 = EDGE_CURVE ( 'NONE', #137660, #210729, #108406, .T. ) ;
#107269 = ORIENTED_EDGE ( 'NONE', *, *, #152411, .T. ) ;
#107268 = FACE_OUTER_BOUND ( 'NONE', #22300, .T. ) ;
#107270 = DIRECTION ( 'NONE',  ( -1.000000000000000000, -0.000000000000000000, -0.000000000000000000 ) ) ;
#107271 = CYLINDRICAL_SURFACE ( 'NONE', #143475, 0.1000000000000028644 ) ;
#107272 = CARTESIAN_POINT ( 'NONE',  ( -17.11825945287482753, 12.51174298335651791, -211.2216088517780577 ) ) ;
#107273 = CARTESIAN_POINT ( 'NONE',  ( -21.12230431290520727, 6.457566653304159132, -133.9947901483110400 ) ) ;
#107274 = CARTESIAN_POINT ( 'NONE',  ( 18.59999999999999076, 6.450000000011156587, -110.5170271704400591 ) ) ;
#107275 = EDGE_CURVE ( 'NONE', #174631, #42715, #58475, .T. ) ;
#107277 = CYLINDRICAL_SURFACE ( 'NONE', #216112, 0.09999999999999939493 ) ;
#107276 = CARTESIAN_POINT ( 'NONE',  ( -18.34374000495060386, 40.40989152675300033, -235.2989281452919954 ) ) ;
#107280 = EDGE_CURVE ( 'NONE', #119288, #62069, #45779, .T. ) ;
#107279 = AXIS2_PLACEMENT_3D ( 'NONE', #195565, #96419, #18190 ) ;
#107278 = DIRECTION ( 'NONE',  ( 1.000000000000000000, 0.000000000000000000, 0.000000000000000000 ) ) ;
#107281 = VECTOR ( 'NONE', #206762, 1000.000000000000000 ) ;
#107282 = CARTESIAN_POINT ( 'NONE',  ( 22.59999954896768770, 76.00882823225497020, -181.7736161585923469 ) ) ;
#107284 = DIRECTION ( 'NONE',  ( 0.000000000000000000, 0.000000000000000000, -1.000000000000000000 ) ) ;
#107283 = AXIS2_PLACEMENT_3D ( 'NONE', #149505, #54217, #69965 ) ;
#107286 = ORIENTED_EDGE ( 'NONE', *, *, #79507, .T. ) ;
#107285 = AXIS2_PLACEMENT_3D ( 'NONE', #91887, #107597, #90592 ) ;
#107287 = VERTEX_POINT ( 'NONE', #204839 ) ;
#107289 = ORIENTED_EDGE ( 'NONE', *, *, #29871, .F. ) ;
#107288 = DIRECTION ( 'NONE',  ( 0.000000000000000000, -0.1350103645451974088, 0.9908441862701587999 ) ) ;
#107290 = VERTEX_POINT ( 'NONE', #221821 ) ;
#107291 = EDGE_CURVE ( 'NONE', #144467, #18904, #129487, .T. ) ;
#107292 = DIRECTION ( 'NONE',  ( 0.000000000000000000, -1.000000000000000000, -0.000000000000000000 ) ) ;
#107293 = CARTESIAN_POINT ( 'NONE',  ( 21.05000000000000071, 32.27467314984873070, -239.7646184017148698 ) ) ;
#107295 = DIRECTION ( 'NONE',  ( -0.000000000000000000, 0.000000000000000000, -1.000000000000000000 ) ) ;
#107294 = LINE ( 'NONE', #248088, #165884 ) ;
#107296 = ORIENTED_EDGE ( 'NONE', *, *, #96031, .T. ) ;
#107297 =( LENGTH_UNIT ( ) NAMED_UNIT ( * ) SI_UNIT ( .MILLI., .METRE. ) );
#107298 = FACE_OUTER_BOUND ( 'NONE', #46464, .T. ) ;
#107299 = PLANE ( 'NONE',  #224444 ) ;
#107300 = ORIENTED_EDGE ( 'NONE', *, *, #33116, .F. ) ;
#107301 = VECTOR ( 'NONE', #241514, 1000.000000000000000 ) ;
#107302 = FACE_OUTER_BOUND ( 'NONE', #96491, .T. ) ;
#107303 = CARTESIAN_POINT ( 'NONE',  ( 20.94999999999999929, 67.44464249442897597, -214.0562211244547655 ) ) ;
#107304 = LINE ( 'NONE', #129446, #174696 ) ;
#107305 = CARTESIAN_POINT ( 'NONE',  ( 21.05000000000000071, 65.43728505328265044, -62.06630537887970434 ) ) ;
#107306 = EDGE_CURVE ( 'NONE', #85514, #202898, #47045, .T. ) ;
#107307 = CYLINDRICAL_SURFACE ( 'NONE', #158025, 0.1000000000000106914 ) ;
#107309 = ORIENTED_EDGE ( 'NONE', *, *, #52184, .T. ) ;
#107308 = CARTESIAN_POINT ( 'NONE',  ( -20.64999999999999858, 68.85000000001254250, -182.2731074845244166 ) ) ;
#107310 = ADVANCED_FACE ( 'NONE', ( #186597 ), #224894, .T. ) ;
#107311 = DIRECTION ( 'NONE',  ( 0.000000000000000000, -7.116814260417668513E-15, 1.000000000000000000 ) ) ;
#107312 = DIRECTION ( 'NONE',  ( 0.000000000000000000, 7.026728003956683390E-15, -1.000000000000000000 ) ) ;
#107313 = DIRECTION ( 'NONE',  ( -1.000000000000000000, -0.000000000000000000, 0.000000000000000000 ) ) ;
#107314 = ORIENTED_EDGE ( 'NONE', *, *, #136699, .T. ) ;
#107315 = CARTESIAN_POINT ( 'NONE',  ( -18.40000000000000213, 13.88102806299823833, -210.8210490262177359 ) ) ;
#107317 = CARTESIAN_POINT ( 'NONE',  ( -23.15000000000000213, -8.663551401869161950, -9.524101118067305194 ) ) ;
#107316 = CARTESIAN_POINT ( 'NONE',  ( 23.14999999999999503, 11.75000000000000000, -21.25000000000000000 ) ) ;
#107318 = DIRECTION ( 'NONE',  ( -2.827886303505247780E-16, -0.03181660087583047802, 0.9994937237965568766 ) ) ;
#107319 = CARTESIAN_POINT ( 'NONE',  ( 20.95483826173900255, 40.82941501609197843, -237.9566743329193343 ) ) ;
#107320 = ADVANCED_FACE ( 'NONE', ( #87461 ), #166689, .T. ) ;
#107321 = DIRECTION ( 'NONE',  ( -0.7071067811865127117, -0.7071067811865821007, 0.000000000000000000 ) ) ;
#107322 = CYLINDRICAL_SURFACE ( 'NONE', #72928, 0.09999999999999939493 ) ;
#107323 = AXIS2_PLACEMENT_3D ( 'NONE', #160016, #80411, #37494 ) ;
#107324 = VECTOR ( 'NONE', #131096, 1000.000000000000000 ) ;
#107325 = CARTESIAN_POINT ( 'NONE',  ( 23.14999999999999503, 64.35000000001204512, -124.3731074845243825 ) ) ;
#107326 = DIRECTION ( 'NONE',  ( 1.000000000000000000, 0.000000000000000000, 0.000000000000000000 ) ) ;
#107327 = CIRCLE ( 'NONE', #24144, 0.09999999999999939493 ) ;
#107328 = ORIENTED_EDGE ( 'NONE', *, *, #250035, .T. ) ;
#107329 = ORIENTED_EDGE ( 'NONE', *, *, #133658, .T. ) ;
#107330 =( BOUNDED_CURVE ( )  B_SPLINE_CURVE ( 3, ( #251005, #72414, #167666, #48972 ),
 .UNSPECIFIED., .F., .T. ) 
 B_SPLINE_CURVE_WITH_KNOTS ( ( 4, 4 ),
 ( 4.712388980384690562, 6.283185307179586232 ),
 .UNSPECIFIED. ) 
 CURVE ( )  GEOMETRIC_REPRESENTATION_ITEM ( )  RATIONAL_B_SPLINE_CURVE ( ( 1.000000000000000000, 0.8047378541243652705, 0.8047378541243652705, 1.000000000000000000 ) ) 
 REPRESENTATION_ITEM ( '' )  );
#107331 = EDGE_LOOP ( 'NONE', ( #42329, #206335, #234973, #80293 ) ) ;
#107332 = CARTESIAN_POINT ( 'NONE',  ( 20.84451136049770525, 65.37985808519944442, -95.52918292499884956 ) ) ;
#107333 = DIRECTION ( 'NONE',  ( 0.000000000000000000, -0.4999999999999863998, 0.8660254037844464792 ) ) ;
#107334 = VERTEX_POINT ( 'NONE', #64059 ) ;
#107336 = ADVANCED_FACE ( 'NONE', ( #202295 ), #5342, .T. ) ;
#107335 = ORIENTED_EDGE ( 'NONE', *, *, #34875, .T. ) ;
#107337 = AXIS2_PLACEMENT_3D ( 'NONE', #4845, #201789, #106521 ) ;
#107338 = VECTOR ( 'NONE', #129574, 1000.000000000000114 ) ;
#107339 = EDGE_LOOP ( 'NONE', ( #205677, #98183, #186569, #33741 ) ) ;
#107340 = CARTESIAN_POINT ( 'NONE',  ( -23.25000000000000000, 76.00000000001189449, -100.9231074845242944 ) ) ;
#107341 = EDGE_LOOP ( 'NONE', ( #61577, #230770, #82568, #117219 ) ) ;
#107342 = FACE_OUTER_BOUND ( 'NONE', #39793, .T. ) ;
#107343 = CIRCLE ( 'NONE', #94874, 0.09999999999998898659 ) ;
#107344 = LINE ( 'NONE', #228598, #30501 ) ;
#107345 = CARTESIAN_POINT ( 'NONE',  ( -23.15000000000000213, 51.33926024308902214, -230.0993571250899379 ) ) ;
#107346 = DIRECTION ( 'NONE',  ( 1.000000000000000000, -0.000000000000000000, 0.000000000000000000 ) ) ;
#107347 = EDGE_CURVE ( 'NONE', #256436, #236070, #223126, .T. ) ;
#107348 = DIRECTION ( 'NONE',  ( 0.000000000000000000, -5.551115123125777653E-14, 1.000000000000000000 ) ) ;
#107350 = ORIENTED_EDGE ( 'NONE', *, *, #88863, .T. ) ;
#107349 = CARTESIAN_POINT ( 'NONE',  ( 21.06086055315973482, 44.20743049992722717, -236.5545395267883180 ) ) ;
#107351 = FACE_OUTER_BOUND ( 'NONE', #139001, .T. ) ;
#107352 = CARTESIAN_POINT ( 'NONE',  ( -23.25000000000000355, 11.75000000001113953, -79.65000000000004832 ) ) ;
#107353 = VERTEX_POINT ( 'NONE', #240968 ) ;
#107354 = CARTESIAN_POINT ( 'NONE',  ( -23.25000000000000000, 1.115600667400684642E-11, -67.00000000000000000 ) ) ;
#107355 = DIRECTION ( 'NONE',  ( 0.000000000000000000, 6.467318590049456648E-15, -1.000000000000000000 ) ) ;
#107357 = EDGE_CURVE ( 'NONE', #192375, #121414, #199986, .T. ) ;
#107356 = CARTESIAN_POINT ( 'NONE',  ( 18.59999999999999787, 7.882824859404637508, -245.3558965132535832 ) ) ;
#107358 = ADVANCED_FACE ( 'NONE', ( #256616 ), #137993, .T. ) ;
#107359 = EDGE_LOOP ( 'NONE', ( #92693, #76832, #116867, #237534 ) ) ;
#107360 = DIRECTION ( 'NONE',  ( 0.000000000000000000, 0.9126074666063773710, 0.4088369013363272741 ) ) ;
#107361 = AXIS2_PLACEMENT_3D ( 'NONE', #117574, #160587, #18477 ) ;
#107362 = CARTESIAN_POINT ( 'NONE',  ( -16.88783316861808359, 66.05000000001182059, -82.27537152650414498 ) ) ;
#107363 = ORIENTED_EDGE ( 'NONE', *, *, #181995, .T. ) ;
#107364 = CIRCLE ( 'NONE', #161567, 0.09999999999999939493 ) ;
#107365 = EDGE_CURVE ( 'NONE', #82173, #235258, #41789, .T. ) ;
#107366 = DIRECTION ( 'NONE',  ( -0.000000000000000000, -1.000000000000000000, 6.308085367188393199E-16 ) ) ;
#107367 = EDGE_CURVE ( 'NONE', #153790, #155470, #233316, .T. ) ;
#107368 = DIRECTION ( 'NONE',  ( -1.000000000000000000, 0.000000000000000000, 0.000000000000000000 ) ) ;
#107369 = DIRECTION ( 'NONE',  ( -1.000000000000000000, 2.952720810173289112E-16, 2.061873921506763405E-30 ) ) ;
#107370 = ORIENTED_EDGE ( 'NONE', *, *, #230854, .F. ) ;
#107371 = ORIENTED_EDGE ( 'NONE', *, *, #87429, .T. ) ;
#107372 = VECTOR ( 'NONE', #215214, 1000.000000000000000 ) ;
#107373 = CARTESIAN_POINT ( 'NONE',  ( 23.24999999999999645, 65.65271564877468791, -222.5736063831752176 ) ) ;
#107374 = EDGE_CURVE ( 'NONE', #224443, #190519, #120898, .T. ) ;
#107375 = DIRECTION ( 'NONE',  ( 0.000000000000000000, 1.000000000000000000, 0.000000000000000000 ) ) ;
#107376 = DIRECTION ( 'NONE',  ( 0.000000000000000000, 0.000000000000000000, -1.000000000000000000 ) ) ;
#107377 = CIRCLE ( 'NONE', #3127, 0.1000000000000028644 ) ;
#107378 = CARTESIAN_POINT ( 'NONE',  ( 21.08376601933332495, 6.341947271286813681, -167.4362239890699584 ) ) ;
#107379 = CARTESIAN_POINT ( 'NONE',  ( 14.45963434102923628, 9.451541661396666072, -51.95387549883057687 ) ) ;
#107381 = EDGE_CURVE ( 'NONE', #97348, #5738, #208372, .T. ) ;
#107380 = FACE_OUTER_BOUND ( 'NONE', #80159, .T. ) ;
#107382 = VECTOR ( 'NONE', #171648, 1000.000000000000000 ) ;
#107383 = ORIENTED_EDGE ( 'NONE', *, *, #162133, .T. ) ;
#107384 = CARTESIAN_POINT ( 'NONE',  ( -20.85882249326303040, 65.66751761918668251, -97.42826094061121012 ) ) ;
#107386 = ORIENTED_EDGE ( 'NONE', *, *, #196605, .F. ) ;
#107385 = FACE_OUTER_BOUND ( 'NONE', #88419, .T. ) ;
#107387 = DIRECTION ( 'NONE',  ( 0.000000000000000000, 0.000000000000000000, -1.000000000000000000 ) ) ;
#107388 = CIRCLE ( 'NONE', #211448, 0.09999999999999939493 ) ;
#107389 = CARTESIAN_POINT ( 'NONE',  ( -21.05000000000000071, 64.40000000001177227, -76.45131071479988805 ) ) ;
#107390 = CARTESIAN_POINT ( 'NONE',  ( -21.08134388332232589, 75.92418108250473097, -75.85778806504229976 ) ) ;
#107392 = CARTESIAN_POINT ( 'NONE',  ( -16.84793658983414488, 66.05000000001231797, -123.7894608067136346 ) ) ;
#107391 = B_SPLINE_CURVE_WITH_KNOTS ( 'NONE', 3,
 ( #182683, #178850, #58834, #160558, #217911, #101809, #237511, #61435 ),
 .UNSPECIFIED., .F., .F.,
 ( 4, 2, 2, 4 ),
 ( 0.000000000000000000, 0.0002181133598169243877, 0.0003271700397253575520, 0.0004362267196337907705 ),
 .UNSPECIFIED. ) ;
#107393 = ADVANCED_FACE ( 'NONE', ( #40226 ), #218816, .F. ) ;
#107394 = VECTOR ( 'NONE', #227303, 1000.000000000000114 ) ;
#107396 = ORIENTED_EDGE ( 'NONE', *, *, #117789, .T. ) ;
#107395 = FACE_OUTER_BOUND ( 'NONE', #48273, .T. ) ;
#107397 = DIRECTION ( 'NONE',  ( 0.000000000000000000, 0.000000000000000000, 1.000000000000000000 ) ) ;
#107398 = CARTESIAN_POINT ( 'NONE',  ( 21.05933563467872105, 10.72452471209247626, -179.6936477489558968 ) ) ;
#107399 = DIRECTION ( 'NONE',  ( 1.000000000000000000, 0.000000000000000000, -0.000000000000000000 ) ) ;
#107400 = CARTESIAN_POINT ( 'NONE',  ( -20.64999999999999858, 4.250000000000000000, -12.35000000000000142 ) ) ;
#107401 = EDGE_LOOP ( 'NONE', ( #30476, #224991, #249653, #47400 ) ) ;
#107402 = CARTESIAN_POINT ( 'NONE',  ( 18.59999994388910238, -7.620950066970707759, -210.0092139826364814 ) ) ;
#107403 = EDGE_CURVE ( 'NONE', #181106, #89738, #102705, .T. ) ;
#107404 = SPHERICAL_SURFACE ( 'NONE', #194165, 0.1000000000000000056 ) ;
#107405 = EDGE_CURVE ( 'NONE', #223354, #207624, #50118, .T. ) ;
#107407 = B_SPLINE_CURVE_WITH_KNOTS ( 'NONE', 3,
 ( #177953, #100920, #257413, #220900, #160962, #158413, #39745, #240480, #237907, #59227 ),
 .UNSPECIFIED., .F., .F.,
 ( 4, 2, 2, 2, 4 ),
 ( 0.000000000000000000, 3.990160268011951094E-05, 7.980320536023902188E-05, 0.0001596064107204957434, 0.0003192128214409947935 ),
 .UNSPECIFIED. ) ;
#107406 = FACE_OUTER_BOUND ( 'NONE', #38728, .T. ) ;
#107408 = EDGE_CURVE ( 'NONE', #177703, #104317, #117176, .T. ) ;
#107409 = CARTESIAN_POINT ( 'NONE',  ( 20.94999999999999929, -11.48912529306489994, -164.4000000000000057 ) ) ;
#107410 = CIRCLE ( 'NONE', #36709, 0.1000000000000008799 ) ;
#107411 = VERTEX_POINT ( 'NONE', #3621 ) ;
#107412 = DIRECTION ( 'NONE',  ( 0.000000000000000000, 1.000000000000000000, -0.000000000000000000 ) ) ;
#107413 = AXIS2_PLACEMENT_3D ( 'NONE', #232667, #37041, #133544 ) ;
#107414 = ORIENTED_EDGE ( 'NONE', *, *, #220135, .F. ) ;
#107415 = TOROIDAL_SURFACE ( 'NONE', #24227, 0.2000000000000000111, 0.1000000000000000056 ) ;
#107416 = CARTESIAN_POINT ( 'NONE',  ( -18.40000000000000213, 11.33174054713633261, -54.35000000000000142 ) ) ;
#107418 = CARTESIAN_POINT ( 'NONE',  ( 18.79999999999999716, 1.350000000000000089, 16.60000000000000142 ) ) ;
#107417 = AXIS2_PLACEMENT_3D ( 'NONE', #146354, #6860, #225873 ) ;
#107419 = DIRECTION ( 'NONE',  ( 0.000000000000000000, 0.9126074666063770380, 0.4088369013363281068 ) ) ;
#107420 = CARTESIAN_POINT ( 'NONE',  ( 21.15000000000005542, 83.80000000001119531, -37.18565239344504647 ) ) ;
#107421 = ORIENTED_EDGE ( 'NONE', *, *, #240035, .T. ) ;
#107422 = EDGE_CURVE ( 'NONE', #258105, #74301, #238393, .T. ) ;
#107423 = TOROIDAL_SURFACE ( 'NONE', #253161, 6.258578643762712446, 0.1000000000000000056 ) ;
#107424 = EDGE_CURVE ( 'NONE', #245368, #201917, #238271, .T. ) ;
#107425 = CARTESIAN_POINT ( 'NONE',  ( -23.25000000000000000, -8.596261682231832069, -57.54987248284972878 ) ) ;
#107426 = DIRECTION ( 'NONE',  ( -4.336808689942052446E-15, 0.8660254037844445918, 0.4999999999999896194 ) ) ;
#107427 = CARTESIAN_POINT ( 'NONE',  ( 15.39170923737819940, 9.389529397466734650, -17.81710791289368245 ) ) ;
#107428 = CARTESIAN_POINT ( 'NONE',  ( -16.80070461187907682, 9.949999999999985079, -20.85303617083875238 ) ) ;
#107429 = CIRCLE ( 'NONE', #219842, 0.09999999999999568956 ) ;
#107431 = CIRCLE ( 'NONE', #253170, 0.09999999999999470424 ) ;
#107430 = CARTESIAN_POINT ( 'NONE',  ( 20.99142135623731065, 64.40000000001145963, -42.95131071479990226 ) ) ;
#107432 = CIRCLE ( 'NONE', #140756, 4.000000000000003553 ) ;
#107433 = VERTEX_POINT ( 'NONE', #178453 ) ;
#107435 = ORIENTED_EDGE ( 'NONE', *, *, #66223, .T. ) ;
#107434 = CARTESIAN_POINT ( 'NONE',  ( 20.94788355080264353, 10.30207779525983014, -105.9895520716782897 ) ) ;
#107436 = ORIENTED_EDGE ( 'NONE', *, *, #25806, .T. ) ;
#107437 = DIRECTION ( 'NONE',  ( 1.000000000000000000, 0.000000000000000000, 0.000000000000000000 ) ) ;
#107438 = ORIENTED_EDGE ( 'NONE', *, *, #98305, .T. ) ;
#107439 = CARTESIAN_POINT ( 'NONE',  ( 21.14261333020286315, 65.28430735075716029, -124.2731074845241466 ) ) ;
#107440 = DIRECTION ( 'NONE',  ( 0.000000000000000000, 0.4088369013363322146, -0.9126074666063751506 ) ) ;
#107441 = FACE_OUTER_BOUND ( 'NONE', #55488, .T. ) ;
#107442 = ORIENTED_EDGE ( 'NONE', *, *, #143330, .F. ) ;
#107443 = FACE_OUTER_BOUND ( 'NONE', #23860, .T. ) ;
#107444 = CYLINDRICAL_SURFACE ( 'NONE', #43017, 0.1000000000000028644 ) ;
#107445 = LINE ( 'NONE', #33096, #114514 ) ;
#107446 = ORIENTED_EDGE ( 'NONE', *, *, #41549, .T. ) ;
#107447 = CARTESIAN_POINT ( 'NONE',  ( 21.05000000000000071, -0.09999999998884338825, -33.50000000000000000 ) ) ;
#107448 = AXIS2_PLACEMENT_3D ( 'NONE', #26867, #8566, #106347 ) ;
#107450 = ORIENTED_EDGE ( 'NONE', *, *, #53978, .T. ) ;
#107449 = CARTESIAN_POINT ( 'NONE',  ( 21.72449340488910252, 65.71604372252096482, -127.2731074845243597 ) ) ;
#107451 = DIRECTION ( 'NONE',  ( 0.000000000000000000, -6.938893903907222067E-15, 1.000000000000000000 ) ) ;
#107452 = CIRCLE ( 'NONE', #3370, 0.1000000000000028644 ) ;
#107453 = DIRECTION ( 'NONE',  ( -4.408576920032447355E-17, -0.1350103645451945777, 0.9908441862701589109 ) ) ;
#107454 = ADVANCED_FACE ( 'NONE', ( #177175 ), #33463, .T. ) ;
#107455 = CIRCLE ( 'NONE', #124214, 0.1000000000000024342 ) ;
#107456 = ADVANCED_FACE ( 'NONE', ( #121137 ), #129250, .F. ) ;
#107457 = ORIENTED_EDGE ( 'NONE', *, *, #115990, .T. ) ;
#107458 = TOROIDAL_SURFACE ( 'NONE', #65948, 11.65000000000000036, 0.1000000000000000056 ) ;
#107459 = CARTESIAN_POINT ( 'NONE',  ( -20.85000000000000142, 69.06610602788578035, -132.7374616501508342 ) ) ;
#107460 = CARTESIAN_POINT ( 'NONE',  ( -12.47155713865592119, 66.62433047358626936, -120.6553174751384176 ) ) ;
#107461 = DIRECTION ( 'NONE',  ( 0.000000000000000000, -0.8814952561688476074, 0.4721928772777262417 ) ) ;
#107462 = EDGE_LOOP ( 'NONE', ( #119080, #50333, #3273, #192331 ) ) ;
#107463 = LINE ( 'NONE', #5767, #196539 ) ;
#107464 = CARTESIAN_POINT ( 'NONE',  ( 21.14999999999999858, 64.35000000001156195, -57.37310748452439668 ) ) ;
#107465 = AXIS2_PLACEMENT_3D ( 'NONE', #110440, #170475, #249959 ) ;
#107466 = VERTEX_POINT ( 'NONE', #61122 ) ;
#107467 = AXIS2_PLACEMENT_3D ( 'NONE', #226642, #88401, #168007 ) ;
#107468 = VECTOR ( 'NONE', #27854, 1000.000000000000000 ) ;
#107469 = CIRCLE ( 'NONE', #253212, 0.09999999999998898659 ) ;
#107470 = EDGE_CURVE ( 'NONE', #233341, #97884, #40320, .T. ) ;
#107471 = AXIS2_PLACEMENT_3D ( 'NONE', #38952, #256639, #139295 ) ;
#107472 = EDGE_LOOP ( 'NONE', ( #209711, #237899, #101370, #146168 ) ) ;
#107473 = FACE_OUTER_BOUND ( 'NONE', #221079, .T. ) ;
#107474 = ORIENTED_EDGE ( 'NONE', *, *, #190594, .T. ) ;
#107475 = DIRECTION ( 'NONE',  ( -0.000000000000000000, -0.000000000000000000, 1.000000000000000000 ) ) ;
#107476 = CARTESIAN_POINT ( 'NONE',  ( -16.89935556175677078, 66.05000000001257376, -183.1627838474121575 ) ) ;
#107478 = VERTEX_POINT ( 'NONE', #160260 ) ;
#107477 = CARTESIAN_POINT ( 'NONE',  ( 12.84233041328156943, 25.17626390180108231, -232.7245615205268052 ) ) ;
#107479 = CARTESIAN_POINT ( 'NONE',  ( 18.39999999999999503, 64.52683809665012404, -190.8731074845244393 ) ) ;
#107480 = CARTESIAN_POINT ( 'NONE',  ( -18.59999999999999787, 74.13328508995425636, -57.77043223824233564 ) ) ;
#107481 = LINE ( 'NONE', #8398, #189307 ) ;
#107482 = CARTESIAN_POINT ( 'NONE',  ( 21.07946286933444568, 75.92331615675530543, -75.85214480353204181 ) ) ;
#107483 = DIRECTION ( 'NONE',  ( 0.7071067811865475727, -0.7071067811865475727, 0.000000000000000000 ) ) ;
#107484 = CIRCLE ( 'NONE', #140809, 0.09999999999998898659 ) ;
#107485 = FACE_OUTER_BOUND ( 'NONE', #254399, .T. ) ;
#107486 = DIRECTION ( 'NONE',  ( 0.000000000000000000, -0.4930308989875575865, -0.8700118002898125091 ) ) ;
#107488 = ORIENTED_EDGE ( 'NONE', *, *, #21088, .T. ) ;
#107487 = FACE_OUTER_BOUND ( 'NONE', #226173, .T. ) ;
#107489 = CARTESIAN_POINT ( 'NONE',  ( -20.54999999999999716, 1.115600667400684642E-11, -167.5000000000000284 ) ) ;
#107490 = EDGE_LOOP ( 'NONE', ( #229002, #64238, #177604, #132623 ) ) ;
#107491 = AXIS2_PLACEMENT_3D ( 'NONE', #41743, #179961, #219058 ) ;
#107492 = FACE_OUTER_BOUND ( 'NONE', #160108, .T. ) ;
#107493 = CARTESIAN_POINT ( 'NONE',  ( -18.59999999999999787, 77.83585931145600512, -158.5186683157258187 ) ) ;
#107494 = FACE_OUTER_BOUND ( 'NONE', #152561, .T. ) ;
#107495 = DIRECTION ( 'NONE',  ( 0.000000000000000000, 0.9126074666063770380, 0.4088369013363281068 ) ) ;
#107496 = EDGE_LOOP ( 'NONE', ( #67599, #200954, #119386, #225022 ) ) ;
#107497 = CARTESIAN_POINT ( 'NONE',  ( -33.72168855820452649, 11.47316190337362940, -91.25000000000005684 ) ) ;
#107498 = CYLINDRICAL_SURFACE ( 'NONE', #69080, 0.1000000000000028644 ) ;
#107499 = EDGE_CURVE ( 'NONE', #131894, #14564, #89107, .T. ) ;
#107500 = CIRCLE ( 'NONE', #157623, 0.1999999999999987899 ) ;
#107501 = CIRCLE ( 'NONE', #161708, 4.000000000000003553 ) ;
#107502 = EDGE_LOOP ( 'NONE', ( #215898, #162179, #236774, #244169 ) ) ;
#107503 = AXIS2_PLACEMENT_3D ( 'NONE', #182110, #204220, #144233 ) ;
#107504 = DIRECTION ( 'NONE',  ( 2.952720810173289112E-16, 1.000000000000000000, -6.088138035986627436E-46 ) ) ;
#107505 = DIRECTION ( 'NONE',  ( -0.000000000000000000, 6.982962677686266711E-15, -1.000000000000000000 ) ) ;
#107506 = EDGE_CURVE ( 'NONE', #250279, #103901, #116758, .T. ) ;
#107507 = ORIENTED_EDGE ( 'NONE', *, *, #198123, .F. ) ;
#107508 = DIRECTION ( 'NONE',  ( -0.5932847527679310229, -0.8049926720990042694, -4.984624513800578906E-15 ) ) ;
#107509 = ORIENTED_EDGE ( 'NONE', *, *, #232525, .T. ) ;
#107510 = CARTESIAN_POINT ( 'NONE',  ( -12.25000000000000178, 9.350000000011139178, -50.25000000000000000 ) ) ;
#107511 = ORIENTED_EDGE ( 'NONE', *, *, #18643, .F. ) ;
#107512 = EDGE_CURVE ( 'NONE', #68890, #138726, #183414, .T. ) ;
#107513 = CARTESIAN_POINT ( 'NONE',  ( 18.59999999999999076, 14.05000000001116689, -106.0136950707610168 ) ) ;
#107514 = DIRECTION ( 'NONE',  ( 0.000000000000000000, 0.000000000000000000, -1.000000000000000000 ) ) ;
#107515 = AXIS2_PLACEMENT_3D ( 'NONE', #233772, #33042, #53840 ) ;
#107516 = VERTEX_POINT ( 'NONE', #201928 ) ;
#107517 = EDGE_LOOP ( 'NONE', ( #220622, #58532, #53392, #106653 ) ) ;
#107519 = FACE_BOUND ( 'NONE', #109500, .T. ) ;
#107518 = CIRCLE ( 'NONE', #166200, 0.09999999999999939493 ) ;
#107520 = ADVANCED_FACE ( 'NONE', ( #23316 ), #166738, .T. ) ;
#107522 = ORIENTED_EDGE ( 'NONE', *, *, #155725, .T. ) ;
#107521 = CARTESIAN_POINT ( 'NONE',  ( 13.43443725621852636, 9.446557523083688679, -48.58994195434588903 ) ) ;
#107523 = FACE_OUTER_BOUND ( 'NONE', #176209, .T. ) ;
#107524 = EDGE_LOOP ( 'NONE', ( #85318, #688, #233593, #8135 ) ) ;
#107525 = VECTOR ( 'NONE', #192604, 1000.000000000000114 ) ;
#107526 = ORIENTED_EDGE ( 'NONE', *, *, #181284, .T. ) ;
#107527 = DIRECTION ( 'NONE',  ( 1.000000000000000000, 0.000000000000000000, 0.000000000000000000 ) ) ;
#107528 = EDGE_CURVE ( 'NONE', #23656, #139599, #199373, .T. ) ;
#107529 = DIRECTION ( 'NONE',  ( 0.000000000000000000, -1.000000000000000000, -7.272083257015735086E-15 ) ) ;
#107530 = CARTESIAN_POINT ( 'NONE',  ( -18.50000000000000000, 38.28679861725831302, -261.0868692510649680 ) ) ;
#107531 = DIRECTION ( 'NONE',  ( 1.000000000000000000, 0.000000000000000000, 0.000000000000000000 ) ) ;
#107532 = CARTESIAN_POINT ( 'NONE',  ( 21.05000000000000071, -9.399999999988844834, -124.1060308773475924 ) ) ;
#107533 = DIRECTION ( 'NONE',  ( -0.000000000000000000, -6.982962677686266711E-15, 1.000000000000000000 ) ) ;
#107534 = ORIENTED_EDGE ( 'NONE', *, *, #193973, .F. ) ;
#107535 = DIRECTION ( 'NONE',  ( 0.000000000000000000, 0.000000000000000000, 1.000000000000000000 ) ) ;
#107536 = DIRECTION ( 'NONE',  ( 0.000000000000000000, 1.224646799147353207E-16, 1.000000000000000000 ) ) ;
#107537 = CARTESIAN_POINT ( 'NONE',  ( 23.15000000000000213, 24.17260720300848575, -252.6908294531417027 ) ) ;
#107538 = CARTESIAN_POINT ( 'NONE',  ( 21.14999999999999858, 11.65000000001116298, -112.6500000000000341 ) ) ;
#107539 = AXIS2_PLACEMENT_3D ( 'NONE', #216362, #75604, #217625 ) ;
#107540 = VERTEX_POINT ( 'NONE', #118560 ) ;
#107541 = CARTESIAN_POINT ( 'NONE',  ( -18.59999999999999787, 77.16412189325258453, -28.10825939895270764 ) ) ;
#107542 = ORIENTED_EDGE ( 'NONE', *, *, #73227, .T. ) ;
#107543 = CIRCLE ( 'NONE', #253292, 0.09999999999999939493 ) ;
#107544 = ORIENTED_EDGE ( 'NONE', *, *, #231246, .T. ) ;
#107545 = VECTOR ( 'NONE', #2519, 1000.000000000000000 ) ;
#107546 = CARTESIAN_POINT ( 'NONE',  ( 18.59999999999999787, -11.74999999998883737, -125.3500000000000512 ) ) ;
#107547 = DIRECTION ( 'NONE',  ( 0.000000000000000000, -1.000000000000000000, 0.000000000000000000 ) ) ;
#107548 = ORIENTED_EDGE ( 'NONE', *, *, #42730, .F. ) ;
#107549 = ORIENTED_EDGE ( 'NONE', *, *, #199633, .T. ) ;
#107551 = ORIENTED_EDGE ( 'NONE', *, *, #201471, .F. ) ;
#107550 = CARTESIAN_POINT ( 'NONE',  ( -21.05000000000000071, -11.48912529307605546, -30.59999999999999432 ) ) ;
#107552 = FACE_OUTER_BOUND ( 'NONE', #14617, .T. ) ;
#107553 = ORIENTED_EDGE ( 'NONE', *, *, #79299, .F. ) ;
#107554 = FACE_OUTER_BOUND ( 'NONE', #238200, .T. ) ;
#107555 = EDGE_LOOP ( 'NONE', ( #88543, #189702, #121458 ) ) ;
#107556 = CARTESIAN_POINT ( 'NONE',  ( -22.84999999999999787, 4.776122516674678272E-16, -3.900000000000000355 ) ) ;
#107557 = DIRECTION ( 'NONE',  ( -0.000000000000000000, -0.1350103645451876666, -0.9908441862701600211 ) ) ;
#107558 = AXIS2_PLACEMENT_3D ( 'NONE', #235159, #176482, #56490 ) ;
#107560 = MANIFOLD_SOLID_BREP ( 'Stock-MAS-200-1', #111715 ) ;
#107559 = AXIS2_PLACEMENT_3D ( 'NONE', #90313, #227264, #188154 ) ;
#107562 = ORIENTED_EDGE ( 'NONE', *, *, #86271, .F. ) ;
#107561 = VECTOR ( 'NONE', #47486, 1000.000000000000000 ) ;
#107563 = ADVANCED_FACE ( 'NONE', ( #6270 ), #198066, .T. ) ;
#107565 = CARTESIAN_POINT ( 'NONE',  ( -20.85000000000000142, 77.16412189325330928, -128.6082593989527254 ) ) ;
#107564 = CIRCLE ( 'NONE', #61791, 7.900000000000003908 ) ;
#107566 = DIRECTION ( 'NONE',  ( 0.7071067811865474617, 0.7071067811865474617, 0.000000000000000000 ) ) ;
#107567 = EDGE_CURVE ( 'NONE', #60702, #5347, #143217, .T. ) ;
#107568 = DIRECTION ( 'NONE',  ( -0.000000000000000000, 0.07893460099012014619, -0.9968797965484758050 ) ) ;
#107570 = ORIENTED_EDGE ( 'NONE', *, *, #126284, .T. ) ;
#107569 = DIRECTION ( 'NONE',  ( 0.000000000000000000, 0.000000000000000000, 1.000000000000000000 ) ) ;
#107572 = AXIS2_PLACEMENT_3D ( 'NONE', #52223, #71825, #195632 ) ;
#107571 = CARTESIAN_POINT ( 'NONE',  ( -23.15000000000000213, 64.25000000001185185, -90.87310748452438247 ) ) ;
#107573 = CARTESIAN_POINT ( 'NONE',  ( -22.42253884134832020, 75.99806764887642885, -81.17271318187276563 ) ) ;
#107574 = FACE_OUTER_BOUND ( 'NONE', #91, .T. ) ;
#107575 = EDGE_CURVE ( 'NONE', #227999, #62835, #216893, .T. ) ;
#107577 = DIRECTION ( 'NONE',  ( 0.000000000000000000, -0.8814952561688476074, 0.4721928772777262417 ) ) ;
#107576 = DIRECTION ( 'NONE',  ( 0.000000000000000000, 0.2128009952263485993, -0.9770955615653341697 ) ) ;
#107579 = EDGE_CURVE ( 'NONE', #226270, #80879, #126225, .T. ) ;
#107578 = CARTESIAN_POINT ( 'NONE',  ( -20.89192007715128341, 65.67101464000555211, -164.4404391622479977 ) ) ;
#107580 = CARTESIAN_POINT ( 'NONE',  ( 23.14999999999998437, 76.00000000001213607, -136.5231074845242745 ) ) ;
#107581 = VECTOR ( 'NONE', #85930, 1000.000000000000000 ) ;
#107582 = DIRECTION ( 'NONE',  ( -1.000000000000000000, 0.000000000000000000, 0.000000000000000000 ) ) ;
#107583 = DIRECTION ( 'NONE',  ( 0.000000000000000000, 0.8814952561688437216, -0.4721928772777331806 ) ) ;
#107584 = CIRCLE ( 'NONE', #253339, 0.1000000000000028644 ) ;
#107585 = ORIENTED_EDGE ( 'NONE', *, *, #132738, .T. ) ;
#107586 = AXIS2_PLACEMENT_3D ( 'NONE', #122734, #39350, #118877 ) ;
#107587 = AXIS2_PLACEMENT_3D ( 'NONE', #77102, #118816, #156679 ) ;
#107588 = VECTOR ( 'NONE', #84816, 1000.000000000000000 ) ;
#107589 = ORIENTED_EDGE ( 'NONE', *, *, #113538, .T. ) ;
#107590 = ADVANCED_FACE ( 'NONE', ( #244893 ), #187518, .T. ) ;
#107591 = ORIENTED_EDGE ( 'NONE', *, *, #223648, .F. ) ;
#107592 = ADVANCED_FACE ( 'NONE', ( #167963 ), #58665, .T. ) ;
#107593 = VECTOR ( 'NONE', #206690, 1000.000000000000000 ) ;
#107594 = DIRECTION ( 'NONE',  ( -4.408576920032448588E-17, -0.1350103645451807832, -0.9908441862701610203 ) ) ;
#107595 = EDGE_CURVE ( 'NONE', #114637, #169963, #104078, .T. ) ;
#107596 = VERTEX_POINT ( 'NONE', #208364 ) ;
#107597 = DIRECTION ( 'NONE',  ( -1.000000000000000000, 0.000000000000000000, 0.000000000000000000 ) ) ;
#107598 = CARTESIAN_POINT ( 'NONE',  ( 21.14999999999999503, -11.74999999998883560, -21.75000000000000355 ) ) ;
#107599 = PRODUCT_DEFINITION_SHAPE ( 'NONE', 'NONE',  #222081 ) ;
#107600 = ORIENTED_EDGE ( 'NONE', *, *, #160789, .F. ) ;
#107601 = DIRECTION ( 'NONE',  ( -0.000000000000000000, 1.000000000000000000, -0.000000000000000000 ) ) ;
#107602 = ORIENTED_EDGE ( 'NONE', *, *, #251064, .F. ) ;
#107603 = CIRCLE ( 'NONE', #186746, 0.09999999999999939493 ) ;
#107604 = AXIS2_PLACEMENT_3D ( 'NONE', #43252, #81069, #44544 ) ;
#107605 = ORIENTED_EDGE ( 'NONE', *, *, #126217, .T. ) ;
#107606 = CARTESIAN_POINT ( 'NONE',  ( 11.60000000000000320, -9.650000000000002132, 12.40000000000000391 ) ) ;
#107607 = DIRECTION ( 'NONE',  ( 0.000000000000000000, -0.000000000000000000, 1.000000000000000000 ) ) ;
#107608 = EDGE_LOOP ( 'NONE', ( #36485, #151319, #99560, #31201 ) ) ;
#107609 = EDGE_CURVE ( 'NONE', #217030, #101051, #92001, .T. ) ;
#107610 = EDGE_CURVE ( 'NONE', #217530, #96043, #162817, .T. ) ;
#107611 = CARTESIAN_POINT ( 'NONE',  ( 21.40925344232283223, 0.09895018863080314031, -93.84148114060958790 ) ) ;
#107613 = EDGE_LOOP ( 'NONE', ( #35958, #192036 ) ) ;
#107612 = DIRECTION ( 'NONE',  ( -1.000000000000000000, 0.000000000000000000, 0.000000000000000000 ) ) ;
#107614 = DIRECTION ( 'NONE',  ( -0.000000000000000000, 0.2128009952263603677, -0.9770955615653313941 ) ) ;
#107615 = ADVANCED_FACE ( 'NONE', ( #242325 ), #105346, .T. ) ;
#107616 = CARTESIAN_POINT ( 'NONE',  ( -16.89268316805465986, 9.951721813253337601, -121.3557524785455826 ) ) ;
#107617 = ORIENTED_EDGE ( 'NONE', *, *, #57755, .T. ) ;
#107618 = CARTESIAN_POINT ( 'NONE',  ( -18.55121869061588669, 10.32747123227773045, -72.57740328502492844 ) ) ;
#107619 = CIRCLE ( 'NONE', #11811, 0.1000000000000000472 ) ;
#107620 = LINE ( 'NONE', #8530, #27690 ) ;
#107622 = CARTESIAN_POINT ( 'NONE',  ( 21.04999999999999716, 8.871279686006799281, -179.6499999999999488 ) ) ;
#107621 = CARTESIAN_POINT ( 'NONE',  ( -20.54999999999999716, 85.40000000001148805, -45.91707660717669626 ) ) ;
#107623 = CARTESIAN_POINT ( 'NONE',  ( 18.49999999999999289, 10.49142135624846439, -91.85000000000005116 ) ) ;
#107624 = AXIS2_PLACEMENT_3D ( 'NONE', #61243, #160373, #45531 ) ;
#107625 = CARTESIAN_POINT ( 'NONE',  ( -23.25000000000000000, 2.600000000011156054, -147.2246219227621111 ) ) ;
#107626 = CARTESIAN_POINT ( 'NONE',  ( -22.50000000000000000, 1.148907358139439339E-11, -201.0000000000015064 ) ) ;
#107627 = DIRECTION ( 'NONE',  ( -0.000000000000000000, 1.000000000000000000, -0.000000000000000000 ) ) ;
#107628 = ORIENTED_EDGE ( 'NONE', *, *, #223705, .T. ) ;
#107629 = ORIENTED_EDGE ( 'NONE', *, *, #48847, .F. ) ;
#107631 = ORIENTED_EDGE ( 'NONE', *, *, #34969, .F. ) ;
#107630 = AXIS2_PLACEMENT_3D ( 'NONE', #230806, #67852, #211219 ) ;
#107632 = LINE ( 'NONE', #88044, #88833 ) ;
#107634 = EDGE_LOOP ( 'NONE', ( #221340, #193777, #209074, #204125, #59519 ) ) ;
#107633 = EDGE_CURVE ( 'NONE', #177703, #114911, #104450, .T. ) ;
#107635 = DIRECTION ( 'NONE',  ( -0.000000000000000000, 0.000000000000000000, 1.000000000000000000 ) ) ;
#107636 = ORIENTED_EDGE ( 'NONE', *, *, #33133, .T. ) ;
#107637 = ADVANCED_FACE ( 'NONE', ( #63685 ), #21119, .T. ) ;
#107638 = DIRECTION ( 'NONE',  ( 0.000000000000000000, -0.8660254037844411501, -0.4999999999999956146 ) ) ;
#107639 = DIRECTION ( 'NONE',  ( -1.000000000000000000, 0.000000000000000000, 0.000000000000000000 ) ) ;
#107640 = CIRCLE ( 'NONE', #20174, 0.09999999999999939493 ) ;
#107641 = CIRCLE ( 'NONE', #224358, 0.09999999999999459321 ) ;
#107642 = VECTOR ( 'NONE', #251695, 1000.000000000000114 ) ;
#107644 = ADVANCED_FACE ( 'NONE', ( #164084 ), #4503, .T. ) ;
#107643 = EDGE_LOOP ( 'NONE', ( #96610, #187469, #145399, #82785 ) ) ;
#107645 = CIRCLE ( 'NONE', #253399, 0.09999999999999993616 ) ;
#107646 = CARTESIAN_POINT ( 'NONE',  ( 12.48201962039795987, 9.376659938544689155, -151.6281925482172994 ) ) ;
#107647 = SURFACE_STYLE_FILL_AREA ( #167647 ) ;
#107648 = CIRCLE ( 'NONE', #236643, 0.09999999999999939493 ) ;
#107649 = ORIENTED_EDGE ( 'NONE', *, *, #224912, .T. ) ;
#107650 = ORIENTED_EDGE ( 'NONE', *, *, #34328, .F. ) ;
#107651 = VERTEX_POINT ( 'NONE', #144490 ) ;
#107652 = DIRECTION ( 'NONE',  ( -0.000000000000000000, 1.000000000000000000, 6.982962677686267499E-15 ) ) ;
#107653 = FACE_OUTER_BOUND ( 'NONE', #256006, .T. ) ;
#107654 = CARTESIAN_POINT ( 'NONE',  ( -21.05000000000000071, 76.00000000001149658, -47.72310748452432705 ) ) ;
#107655 = CARTESIAN_POINT ( 'NONE',  ( -23.15000000000000213, 19.25956423861613231, -238.0467473098318010 ) ) ;
#107656 = DIRECTION ( 'NONE',  ( -0.000000000000000000, -0.3350715337780662550, -0.9421926911474181043 ) ) ;
#107657 = CARTESIAN_POINT ( 'NONE',  ( 18.60000000000000142, 85.32100840337392356, -196.2871692354463846 ) ) ;
#107658 = DIRECTION ( 'NONE',  ( 0.000000000000000000, 5.880418562633245778E-15, -1.000000000000000000 ) ) ;
#107660 = ORIENTED_EDGE ( 'NONE', *, *, #237921, .F. ) ;
#107659 = CARTESIAN_POINT ( 'NONE',  ( -20.94999675878240808, 10.29307482169071442, -139.4586421466940465 ) ) ;
#107662 = CARTESIAN_POINT ( 'NONE',  ( -18.50000000000000000, 77.36242903720570041, -162.1342262366031548 ) ) ;
#107661 = CARTESIAN_POINT ( 'NONE',  ( 20.21567752745019320, 10.19811410124265905, -74.88262034765169517 ) ) ;
#107663 = FACE_OUTER_BOUND ( 'NONE', #9011, .T. ) ;
#107664 = VERTEX_POINT ( 'NONE', #253868 ) ;
#107665 = CARTESIAN_POINT ( 'NONE',  ( -23.15000000000000213, 46.15118611352045974, -240.5321844900040844 ) ) ;
#107666 = AXIS2_PLACEMENT_3D ( 'NONE', #221290, #59636, #19262 ) ;
#107667 = CYLINDRICAL_SURFACE ( 'NONE', #101985, 0.09999999999999939493 ) ;
#107669 = ADVANCED_FACE ( 'NONE', ( #31022 ), #54396, .F. ) ;
#107668 = DIRECTION ( 'NONE',  ( 0.000000000000000000, 0.000000000000000000, -1.000000000000000000 ) ) ;
#107670 = EDGE_LOOP ( 'NONE', ( #101965, #170460, #200206, #162514 ) ) ;
#107671 = EDGE_CURVE ( 'NONE', #203823, #150529, #89658, .T. ) ;
#107672 = DIRECTION ( 'NONE',  ( -1.073024830501117725E-15, 0.000000000000000000, 1.000000000000000000 ) ) ;
#107673 = FACE_OUTER_BOUND ( 'NONE', #48404, .T. ) ;
#107674 = EDGE_LOOP ( 'NONE', ( #131521, #2448, #222305 ) ) ;
#107675 = ORIENTED_EDGE ( 'NONE', *, *, #25915, .F. ) ;
#107676 = ADVANCED_FACE ( 'NONE', ( #133929 ), #15296, .F. ) ;
#107678 = EDGE_CURVE ( 'NONE', #129336, #138911, #46202, .T. ) ;
#107677 = DIRECTION ( 'NONE',  ( 0.000000000000000000, 0.000000000000000000, 1.000000000000000000 ) ) ;
#107679 = ORIENTED_EDGE ( 'NONE', *, *, #37021, .F. ) ;
#107680 = CARTESIAN_POINT ( 'NONE',  ( -18.39999999999999858, 85.60000000001139142, -29.42291809330221142 ) ) ;
#107681 = DIRECTION ( 'NONE',  ( 0.7071067811865487940, 0.7071067811865462405, -7.215498431451186046E-16 ) ) ;
#107682 = DIRECTION ( 'NONE',  ( 0.000000000000000000, -6.982962677686266711E-15, 1.000000000000000000 ) ) ;
#107683 = ORIENTED_EDGE ( 'NONE', *, *, #185598, .T. ) ;
#107684 = EDGE_CURVE ( 'NONE', #26109, #188180, #37869, .T. ) ;
#107685 = CARTESIAN_POINT ( 'NONE',  ( -13.77083647240106323, 9.457410930301319851, -118.9999159087463454 ) ) ;
#107686 = DIRECTION ( 'NONE',  ( 0.000000000000000000, 0.8814952561688437216, -0.4721928772777334582 ) ) ;
#107687 = CIRCLE ( 'NONE', #232619, 0.09999999999999939493 ) ;
#107688 = DIRECTION ( 'NONE',  ( -0.000000000000000000, 0.8660254037844383745, -0.5000000000000003331 ) ) ;
#107689 = AXIS2_PLACEMENT_3D ( 'NONE', #194851, #192273, #175295 ) ;
#107690 = VECTOR ( 'NONE', #166116, 1000.000000000000000 ) ;
#107691 = EDGE_CURVE ( 'NONE', #216494, #1091, #171169, .T. ) ;
#107692 = EDGE_LOOP ( 'NONE', ( #251133, #164864, #207053, #131372, #197074, #228783, #42431, #22882 ) ) ;
#107694 = EDGE_CURVE ( 'NONE', #51580, #34297, #15147, .T. ) ;
#107693 = CARTESIAN_POINT ( 'NONE',  ( 20.84999999999998721, 10.33248238082518711, -39.09484654391314962 ) ) ;
#107696 = VERTEX_POINT ( 'NONE', #251304 ) ;
#107695 = LINE ( 'NONE', #165112, #12820 ) ;
#107697 = VECTOR ( 'NONE', #1818, 1000.000000000000000 ) ;
#107698 = DIRECTION ( 'NONE',  ( -0.000000000000000000, -0.9875102702516472819, 0.1575546449569748542 ) ) ;
#107699 = LINE ( 'NONE', #222488, #18465 ) ;
#107700 = DIRECTION ( 'NONE',  ( 0.000000000000000000, 0.000000000000000000, 1.000000000000000000 ) ) ;
#107701 = EDGE_CURVE ( 'NONE', #140050, #178561, #237752, .T. ) ;
#107702 = DIRECTION ( 'NONE',  ( 0.000000000000000000, -1.000000000000000000, 0.000000000000000000 ) ) ;
#107703 = CARTESIAN_POINT ( 'NONE',  ( 21.05000005001280172, 8.871279691770906695, -12.17794758824605239 ) ) ;
#107704 = CARTESIAN_POINT ( 'NONE',  ( 20.94999999999999929, 6.550000000011156231, -43.51702717044002355 ) ) ;
#107705 = DIRECTION ( 'NONE',  ( -2.812466655313719426E-14, -0.1350103645451835865, -0.9908441862701605762 ) ) ;
#107706 = VERTEX_POINT ( 'NONE', #33606 ) ;
#107707 = DIRECTION ( 'NONE',  ( 0.000000000000000000, 0.8814952561688471633, -0.4721928772777269634 ) ) ;
#107708 = CARTESIAN_POINT ( 'NONE',  ( -20.54999999999999716, 2.499999999999998668, -20.27537807723789953 ) ) ;
#107709 = AXIS2_PLACEMENT_3D ( 'NONE', #250891, #16174, #95673 ) ;
#107710 = AXIS2_PLACEMENT_3D ( 'NONE', #235920, #100238, #136822 ) ;
#107711 = CARTESIAN_POINT ( 'NONE',  ( -23.15000000000000213, 77.02083669383561926, -199.7590813894317989 ) ) ;
#107712 = AXIS2_PLACEMENT_3D ( 'NONE', #194084, #209779, #54545 ) ;
#107713 = EDGE_CURVE ( 'NONE', #195772, #12292, #254304, .T. ) ;
#107714 = FACE_OUTER_BOUND ( 'NONE', #186396, .T. ) ;
#107715 = DIRECTION ( 'NONE',  ( 0.000000000000000000, 0.2128009952263605065, -0.9770955615653315052 ) ) ;
#107716 = AXIS2_PLACEMENT_3D ( 'NONE', #6924, #40951, #200001 ) ;
#107717 = ORIENTED_EDGE ( 'NONE', *, *, #60547, .F. ) ;
#107718 = ORIENTED_EDGE ( 'NONE', *, *, #37037, .T. ) ;
#107719 = DIRECTION ( 'NONE',  ( 0.000000000000000000, 0.000000000000000000, -1.000000000000000000 ) ) ;
#107720 = ADVANCED_FACE ( 'NONE', ( #32298 ), #154815, .T. ) ;
#107721 = CARTESIAN_POINT ( 'NONE',  ( -23.15000000000000213, 11.65000000001115588, -179.6499999999999773 ) ) ;
#107722 = CARTESIAN_POINT ( 'NONE',  ( 21.14999999999999858, 11.75000000001116263, -167.5999999999999659 ) ) ;
#107724 = ADVANCED_FACE ( 'NONE', ( #11439 ), #87707, .F. ) ;
#107723 = DIRECTION ( 'NONE',  ( 0.000000000000000000, 0.000000000000000000, 1.000000000000000000 ) ) ;
#107725 = EDGE_CURVE ( 'NONE', #141829, #248843, #130075, .T. ) ;
#107726 = CARTESIAN_POINT ( 'NONE',  ( 21.05000000000000071, 1.115600667400684642E-11, -167.5000000000000284 ) ) ;
#107727 = DIRECTION ( 'NONE',  ( -1.000000000000000000, 0.000000000000000000, 0.000000000000000000 ) ) ;
#107728 = DIRECTION ( 'NONE',  ( -1.000000000000000000, -0.000000000000000000, -0.000000000000000000 ) ) ;
#107729 = AXIS2_PLACEMENT_3D ( 'NONE', #2130, #202910, #240768 ) ;
#107730 = AXIS2_PLACEMENT_3D ( 'NONE', #187461, #203151, #105297 ) ;
#107731 = AXIS2_PLACEMENT_3D ( 'NONE', #182155, #124748, #123459 ) ;
#107732 = ORIENTED_EDGE ( 'NONE', *, *, #80736, .T. ) ;
#107733 = CARTESIAN_POINT ( 'NONE',  ( -20.54999999999999716, 2.400000000011155432, -80.22462192276213955 ) ) ;
#107734 = ORIENTED_EDGE ( 'NONE', *, *, #197409, .F. ) ;
#107735 = EDGE_CURVE ( 'NONE', #50639, #168, #110520, .T. ) ;
#107736 = CARTESIAN_POINT ( 'NONE',  ( -20.64999999999999858, 4.250000000011156409, -45.75000000000000711 ) ) ;
#107737 = DIRECTION ( 'NONE',  ( 0.000000000000000000, 0.8660254037844424824, 0.4999999999999934497 ) ) ;
#107738 = AXIS2_PLACEMENT_3D ( 'NONE', #129239, #193072, #208782 ) ;
#107739 = CARTESIAN_POINT ( 'NONE',  ( 21.05281448260627641, 8.776010158548784190, -79.17355791181147140 ) ) ;
#107740 = DIRECTION ( 'NONE',  ( 0.000000000000000000, -0.9667078373770160438, -0.2558827019433957961 ) ) ;
#107741 = DIRECTION ( 'NONE',  ( 0.000000000000000000, 0.8814952561688434995, -0.4721928772777339023 ) ) ;
#107742 = DIRECTION ( 'NONE',  ( 1.000000000000000000, 0.000000000000000000, 0.000000000000000000 ) ) ;
#107743 = CARTESIAN_POINT ( 'NONE',  ( -17.11825945287481687, 66.05000000001182059, -82.27310748452438816 ) ) ;
#107744 = ORIENTED_EDGE ( 'NONE', *, *, #237204, .F. ) ;
#107745 = CARTESIAN_POINT ( 'NONE',  ( -21.14999999999994174, 87.51781941433023349, -34.28670414799875488 ) ) ;
#107746 = LINE ( 'NONE', #67341, #92307 ) ;
#107747 = CARTESIAN_POINT ( 'NONE',  ( -18.39999999999999858, -9.599999999988844124, -74.03206939669971121 ) ) ;
#107748 = CARTESIAN_POINT ( 'NONE',  ( -23.39999999999994529, 64.35000000001120668, -3.123107484524795474 ) ) ;
#107749 = CIRCLE ( 'NONE', #153607, 0.09999999999999939493 ) ;
#107750 = AXIS2_PLACEMENT_3D ( 'NONE', #110707, #130258, #209815 ) ;
#107751 = FACE_OUTER_BOUND ( 'NONE', #119721, .T. ) ;
#107752 = DIRECTION ( 'NONE',  ( 0.000000000000000000, 0.2128009952263403282, -0.9770955615653358350 ) ) ;
#107753 = VECTOR ( 'NONE', #56071, 1000.000000000000000 ) ;
#107754 = ORIENTED_EDGE ( 'NONE', *, *, #88844, .F. ) ;
#107755 = CARTESIAN_POINT ( 'NONE',  ( -23.25000000000000000, 66.30975017506362690, -223.0162872746489882 ) ) ;
#107756 = CARTESIAN_POINT ( 'NONE',  ( 18.39999999999999503, 64.52683809664902981, -48.67310748452440805 ) ) ;
#107757 = EDGE_CURVE ( 'NONE', #234056, #74755, #241840, .T. ) ;
#107758 = ORIENTED_EDGE ( 'NONE', *, *, #56276, .F. ) ;
#107759 = EDGE_LOOP ( 'NONE', ( #84903, #91204, #41973, #237527 ) ) ;
#107760 = CARTESIAN_POINT ( 'NONE',  ( -20.54999999999999716, 8.751106741858205140, -220.7398867978736234 ) ) ;
#107761 = CARTESIAN_POINT ( 'NONE',  ( 21.08804582317334209, 11.30290901145985138, -211.1778474225062894 ) ) ;
#107762 = CIRCLE ( 'NONE', #166636, 0.09999999999998898659 ) ;
#107763 = CIRCLE ( 'NONE', #61985, 4.049999999999999822 ) ;
#107764 = CARTESIAN_POINT ( 'NONE',  ( -21.05000000000000071, -1.835341550213255957, -78.65515129256301918 ) ) ;
#107765 = ORIENTED_EDGE ( 'NONE', *, *, #167359, .F. ) ;
#107766 = CARTESIAN_POINT ( 'NONE',  ( 18.43466021071413863, -9.494190690445385883, -174.1170615601278939 ) ) ;
#107767 = CARTESIAN_POINT ( 'NONE',  ( 23.14999999999999858, -3.999999999988843147, -67.00000000000000000 ) ) ;
#107768 = CIRCLE ( 'NONE', #220219, 0.1000000000000055844 ) ;
#107769 = EDGE_CURVE ( 'NONE', #80585, #74170, #75283, .T. ) ;
#107770 = ORIENTED_EDGE ( 'NONE', *, *, #233109, .T. ) ;
#107771 = AXIS2_PLACEMENT_3D ( 'NONE', #66597, #65301, #27511 ) ;
#107772 = VECTOR ( 'NONE', #172241, 1000.000000000000114 ) ;
#107773 = CIRCLE ( 'NONE', #28723, 0.09999999999999939493 ) ;
#107774 = AXIS2_PLACEMENT_3D ( 'NONE', #140971, #157997, #117539 ) ;
#107775 = CARTESIAN_POINT ( 'NONE',  ( -20.65000000000000568, 5.650000000011139001, -188.3499999999999659 ) ) ;
#107776 = ORIENTED_EDGE ( 'NONE', *, *, #181619, .T. ) ;
#107777 = CARTESIAN_POINT ( 'NONE',  ( 23.14999999999999858, 87.75000000001202238, -114.7731074845242318 ) ) ;
#107778 = CARTESIAN_POINT ( 'NONE',  ( -18.59999999999999787, 11.75000000001115197, -179.6499999999999773 ) ) ;
#107779 = DIRECTION ( 'NONE',  ( -2.602085213965227050E-14, 0.9126074666063771490, 0.4088369013363281623 ) ) ;
#107781 = CARTESIAN_POINT ( 'NONE',  ( -18.40000000000000213, 62.48575673152180343, -209.5207689439494345 ) ) ;
#107780 = UNCERTAINTY_MEASURE_WITH_UNIT (LENGTH_MEASURE( 1.000000000000000082E-05 ), #44766, 'distance_accuracy_value', 'NONE');
#107782 = CARTESIAN_POINT ( 'NONE',  ( -18.59999999999999787, 2.923777413779037548, -208.5507632484912222 ) ) ;
#107783 = DIRECTION ( 'NONE',  ( 0.000000000000000000, 0.000000000000000000, 1.000000000000000000 ) ) ;
#107784 = DIRECTION ( 'NONE',  ( 0.000000000000000000, 0.9126074666063768159, 0.4088369013363288285 ) ) ;
#107785 = DIRECTION ( 'NONE',  ( 0.000000000000000000, 0.9908441862701605762, -0.1350103645451835310 ) ) ;
#107786 = DIRECTION ( 'NONE',  ( -1.000000000000000000, 0.000000000000000000, 0.000000000000000000 ) ) ;
#107788 = EDGE_LOOP ( 'NONE', ( #24270, #83500, #29215, #165088 ) ) ;
#107787 = DIRECTION ( 'NONE',  ( -0.8660254037844653530, 0.000000000000000000, -0.4999999999999539257 ) ) ;
#107789 = VERTEX_POINT ( 'NONE', #230475 ) ;
#107791 = DIRECTION ( 'NONE',  ( 0.000000000000000000, 0.000000000000000000, -1.000000000000000000 ) ) ;
#107790 = DIRECTION ( 'NONE',  ( 0.000000000000000000, -7.034366652768089021E-15, 1.000000000000000000 ) ) ;
#107793 = ORIENTED_EDGE ( 'NONE', *, *, #197743, .F. ) ;
#107792 = DIRECTION ( 'NONE',  ( 1.000000000000000000, 0.000000000000000000, 0.000000000000000000 ) ) ;
#107794 = ORIENTED_EDGE ( 'NONE', *, *, #210765, .F. ) ;
#107795 = DIRECTION ( 'NONE',  ( 1.000000000000000000, -0.000000000000000000, -0.000000000000000000 ) ) ;
#107796 = AXIS2_PLACEMENT_3D ( 'NONE', #55541, #155991, #235492 ) ;
#107797 = CIRCLE ( 'NONE', #241105, 0.1999999999999987899 ) ;
#107798 = DIRECTION ( 'NONE',  ( 0.000000000000000000, -1.000000000000000000, 0.000000000000000000 ) ) ;
#107799 = CIRCLE ( 'NONE', #236986, 12.97499999999999964 ) ;
#107800 = LINE ( 'NONE', #89508, #125777 ) ;
#107801 = CARTESIAN_POINT ( 'NONE',  ( -20.89192007715128341, 10.32898536001801304, -173.0826683222764757 ) ) ;
#107802 = CYLINDRICAL_SURFACE ( 'NONE', #256648, 0.09999999999999817368 ) ;
#107803 = CARTESIAN_POINT ( 'NONE',  ( -18.40000000000000213, 5.650000000011139001, -154.8500000000000227 ) ) ;
#107804 = CIRCLE ( 'NONE', #178776, 0.4999999999999944489 ) ;
#107805 = EDGE_CURVE ( 'NONE', #68580, #145089, #191377, .T. ) ;
#107806 = AXIS2_PLACEMENT_3D ( 'NONE', #30209, #131857, #109713 ) ;
#107807 = CARTESIAN_POINT ( 'NONE',  ( -18.59999999999999787, -1.835341550213255957, -112.0551512925630107 ) ) ;
#107808 = ORIENTED_EDGE ( 'NONE', *, *, #252435, .T. ) ;
#107809 = ORIENTED_EDGE ( 'NONE', *, *, #54355, .F. ) ;
#107810 = DIRECTION ( 'NONE',  ( -1.000000000000000000, 0.000000000000000000, 0.000000000000000000 ) ) ;
#107811 = AXIS2_PLACEMENT_3D ( 'NONE', #257788, #59612, #38811 ) ;
#107812 = EDGE_LOOP ( 'NONE', ( #63072, #5683, #199893, #159847 ) ) ;
#107813 = CARTESIAN_POINT ( 'NONE',  ( 20.46382478191414833, 65.40137955871495024, -162.3452930151790099 ) ) ;
#107814 = ORIENTED_EDGE ( 'NONE', *, *, #48843, .F. ) ;
#107815 = CARTESIAN_POINT ( 'NONE',  ( -23.15000000000000213, 71.65000000001155911, -57.17310748452435121 ) ) ;
#107816 = VECTOR ( 'NONE', #60477, 999.9999999999998863 ) ;
#107817 = CARTESIAN_POINT ( 'NONE',  ( 21.07928932188134397, 0.09889514566555242248, -161.1714833436066385 ) ) ;
#107818 = EDGE_CURVE ( 'NONE', #98189, #167145, #17015, .T. ) ;
#107819 = DIRECTION ( 'NONE',  ( 1.000000000000000000, 0.000000000000000000, -0.000000000000000000 ) ) ;
#107820 = CARTESIAN_POINT ( 'NONE',  ( 23.24999999999999645, 4.775700934590591196, -189.1512318959539982 ) ) ;
#107821 = ORIENTED_EDGE ( 'NONE', *, *, #135742, .T. ) ;
#107822 = DIRECTION ( 'NONE',  ( -1.000000000000000000, 0.000000000000000000, -0.000000000000000000 ) ) ;
#107823 = VERTEX_POINT ( 'NONE', #97340 ) ;
#107824 = EDGE_CURVE ( 'NONE', #49816, #229007, #161213, .T. ) ;
#107825 = DIRECTION ( 'NONE',  ( -1.000000000000000000, 0.000000000000000000, 0.000000000000000000 ) ) ;
#107826 = VECTOR ( 'NONE', #144578, 1000.000000000000000 ) ;
#107828 = CYLINDRICAL_SURFACE ( 'NONE', #10702, 0.09999999999999609201 ) ;
#107827 = AXIS2_PLACEMENT_3D ( 'NONE', #115397, #69883, #132406 ) ;
#107829 = DIRECTION ( 'NONE',  ( 2.259780016855445309E-14, -0.9875055080513764905, 0.1575844902526679359 ) ) ;
#107830 = AXIS2_PLACEMENT_3D ( 'NONE', #124246, #158265, #119102 ) ;
#107831 = ORIENTED_EDGE ( 'NONE', *, *, #86803, .T. ) ;
#107832 = CARTESIAN_POINT ( 'NONE',  ( 21.05000000000000071, -9.399999999988846611, -177.3939691226524076 ) ) ;
#107833 = EDGE_CURVE ( 'NONE', #197727, #180754, #58230, .T. ) ;
#107834 = ORIENTED_EDGE ( 'NONE', *, *, #121390, .T. ) ;
#107837 = ORIENTED_EDGE ( 'NONE', *, *, #189678, .F. ) ;
#107836 = CARTESIAN_POINT ( 'NONE',  ( 18.59999999999999076, 6.400000000011158541, -110.4304246300616086 ) ) ;
#107835 = DIRECTION ( 'NONE',  ( -1.000000000000000000, 0.000000000000000000, 0.000000000000000000 ) ) ;
#107838 = DIRECTION ( 'NONE',  ( -1.000000000000000000, 0.000000000000000000, 0.000000000000000000 ) ) ;
#107839 = ORIENTED_EDGE ( 'NONE', *, *, #108229, .T. ) ;
#107840 = CARTESIAN_POINT ( 'NONE',  ( -22.39999999999999858, 65.59531831295525706, -241.8872196075891168 ) ) ;
#107841 = ORIENTED_EDGE ( 'NONE', *, *, #20177, .F. ) ;
#107842 = DIRECTION ( 'NONE',  ( 0.000000000000000000, -6.789366196018718420E-15, 1.000000000000000000 ) ) ;
#107843 = EDGE_CURVE ( 'NONE', #157474, #184568, #158674, .T. ) ;
#107844 = DIRECTION ( 'NONE',  ( -1.000000000000000000, -0.000000000000000000, -0.000000000000000000 ) ) ;
#107845 = FACE_OUTER_BOUND ( 'NONE', #36564, .T. ) ;
#107846 = CARTESIAN_POINT ( 'NONE',  ( -16.89268316805466341, 9.951721813242185632, -12.64424752145445296 ) ) ;
#107847 = ADVANCED_FACE ( 'NONE', ( #159941 ), #29505, .F. ) ;
#107848 = ORIENTED_EDGE ( 'NONE', *, *, #173647, .T. ) ;
#107849 = CARTESIAN_POINT ( 'NONE',  ( -16.94309007106719633, 44.07787287466445747, -235.2784698230337881 ) ) ;
#107850 = FILL_AREA_STYLE_COLOUR ( '', #220047 ) ;
#107851 = CARTESIAN_POINT ( 'NONE',  ( 20.85000000000000142, 80.78317333349157536, -192.9003134612048882 ) ) ;
#107852 = ORIENTED_EDGE ( 'NONE', *, *, #34970, .T. ) ;
#107853 = DIRECTION ( 'NONE',  ( 1.000000000000000000, -0.000000000000000000, -0.000000000000000000 ) ) ;
#107854 = ORIENTED_EDGE ( 'NONE', *, *, #177789, .F. ) ;
#107855 = CARTESIAN_POINT ( 'NONE',  ( -23.15000000000000213, 4.554494125284476169, -212.9355439031026265 ) ) ;
#107856 = CARTESIAN_POINT ( 'NONE',  ( -23.25000000000000000, 10.69888912757691024, -235.6450824654141059 ) ) ;
#107857 = CARTESIAN_POINT ( 'NONE',  ( -20.90000000000000213, -1.885425182446133885, -11.49641995933507843 ) ) ;
#107859 = ORIENTED_EDGE ( 'NONE', *, *, #190113, .T. ) ;
#107858 = CARTESIAN_POINT ( 'NONE',  ( -16.88783316861821859, 44.22880863429497111, -235.2571222925663790 ) ) ;
#107860 = CARTESIAN_POINT ( 'NONE',  ( -20.94999999999999929, 0.6171228861679354250, -203.8335771285409521 ) ) ;
#107861 = ADVANCED_FACE ( 'NONE', ( #218585 ), #115661, .T. ) ;
#107862 = FACE_OUTER_BOUND ( 'NONE', #188095, .T. ) ;
#107863 = DIRECTION ( 'NONE',  ( -1.000000000000000000, 0.000000000000000000, 0.000000000000000000 ) ) ;
#107864 = ORIENTED_EDGE ( 'NONE', *, *, #18930, .F. ) ;
#107865 = AXIS2_PLACEMENT_3D ( 'NONE', #213581, #50643, #194049 ) ;
#107867 = AXIS2_PLACEMENT_3D ( 'NONE', #156717, #112432, #236211 ) ;
#107866 = DIRECTION ( 'NONE',  ( 0.000000000000000000, 0.000000000000000000, -1.000000000000000000 ) ) ;
#107868 = DIRECTION ( 'NONE',  ( 0.000000000000000000, -1.000000000000000000, -6.982962677686266711E-15 ) ) ;
#107869 = ORIENTED_EDGE ( 'NONE', *, *, #68109, .T. ) ;
#107870 = AXIS2_PLACEMENT_3D ( 'NONE', #180865, #79168, #196558 ) ;
#107872 = DIRECTION ( 'NONE',  ( 0.000000000000000000, 1.000000000000000000, -0.000000000000000000 ) ) ;
#107871 = VECTOR ( 'NONE', #243934, 1000.000000000000000 ) ;
#107873 = ORIENTED_EDGE ( 'NONE', *, *, #31537, .T. ) ;
#107874 = EDGE_CURVE ( 'NONE', #222414, #206042, #810, .T. ) ;
#107875 = DIRECTION ( 'NONE',  ( -1.073024830501117725E-15, -0.2128009952263604232, 0.9770955615653316162 ) ) ;
#107876 = CIRCLE ( 'NONE', #178839, 0.5000000000000004441 ) ;
#107878 = ORIENTED_EDGE ( 'NONE', *, *, #101853, .T. ) ;
#107877 = DIRECTION ( 'NONE',  ( 0.000000000000000000, 0.000000000000000000, 1.000000000000000000 ) ) ;
#107879 = EDGE_CURVE ( 'NONE', #90248, #242007, #234, .T. ) ;
#107882 = ORIENTED_EDGE ( 'NONE', *, *, #111758, .F. ) ;
#107881 = ORIENTED_EDGE ( 'NONE', *, *, #87007, .T. ) ;
#107880 = DIRECTION ( 'NONE',  ( -3.265361837132812600E-16, 0.9770955615653313941, 0.2128009952263603677 ) ) ;
#107884 = AXIS2_PLACEMENT_3D ( 'NONE', #211481, #76766, #255352 ) ;
#107883 = FACE_OUTER_BOUND ( 'NONE', #180133, .T. ) ;
#107885 = AXIS2_PLACEMENT_3D ( 'NONE', #245270, #26227, #105714 ) ;
#107886 = DIRECTION ( 'NONE',  ( 1.000000000000000000, -0.000000000000000000, -0.000000000000000000 ) ) ;
#107887 = CARTESIAN_POINT ( 'NONE',  ( -18.59999999999999787, 6.846123162352588665, -37.23772626684986164 ) ) ;
#107889 = DIRECTION ( 'NONE',  ( 0.000000000000000000, 0.000000000000000000, 1.000000000000000000 ) ) ;
#107888 = CARTESIAN_POINT ( 'NONE',  ( 22.49999999999999645, 0.08880997639808875521, -88.85023708196810333 ) ) ;
#107891 = EDGE_CURVE ( 'NONE', #118478, #70808, #66881, .T. ) ;
#107890 = CARTESIAN_POINT ( 'NONE',  ( -21.44999999999999929, 68.65000000001229807, -157.6731074845243938 ) ) ;
#107892 = LINE ( 'NONE', #66208, #210764 ) ;
#107893 = CARTESIAN_POINT ( 'NONE',  ( -20.94999999999999929, 70.15000000001198543, -113.1556047088022723 ) ) ;
#107894 = ADVANCED_FACE ( 'NONE', ( #36141 ), #68457, .F. ) ;
#107895 = LINE ( 'NONE', #207002, #84128 ) ;
#107896 = AXIS2_PLACEMENT_3D ( 'NONE', #44488, #124023, #201 ) ;
#107897 = VERTEX_POINT ( 'NONE', #101178 ) ;
#107898 = VERTEX_POINT ( 'NONE', #16575 ) ;
#107899 = LINE ( 'NONE', #244835, #175075 ) ;
#107900 = ORIENTED_EDGE ( 'NONE', *, *, #181212, .T. ) ;
#107901 = ORIENTED_EDGE ( 'NONE', *, *, #55049, .T. ) ;
#107902 = CARTESIAN_POINT ( 'NONE',  ( -23.39999999999994529, 77.83551161375991967, -47.52760213295649550 ) ) ;
#107903 = ADVANCED_FACE ( 'NONE', ( #255112 ), #79069, .T. ) ;
#107904 = VERTEX_POINT ( 'NONE', #116943 ) ;
#107905 = FACE_OUTER_BOUND ( 'NONE', #159339, .T. ) ;
#107906 = EDGE_CURVE ( 'NONE', #119449, #27184, #98278, .T. ) ;
#107907 = ADVANCED_FACE ( 'NONE', ( #62110 ), #199050, .T. ) ;
#107908 = ORIENTED_EDGE ( 'NONE', *, *, #193284, .T. ) ;
#107909 = CARTESIAN_POINT ( 'NONE',  ( 23.24999999999999289, 11.65000000000000746, -0.1000000000000028644 ) ) ;
#107910 = CYLINDRICAL_SURFACE ( 'NONE', #165576, 0.09999999999999892308 ) ;
#107911 = AXIS2_PLACEMENT_3D ( 'NONE', #114819, #150122, #31469 ) ;
#107913 = ORIENTED_EDGE ( 'NONE', *, *, #152705, .F. ) ;
#107912 = ORIENTED_EDGE ( 'NONE', *, *, #43954, .T. ) ;
#107914 = ORIENTED_EDGE ( 'NONE', *, *, #111879, .F. ) ;
#107915 = DIRECTION ( 'NONE',  ( 0.000000000000000000, 0.8660254037844420383, -0.4999999999999941713 ) ) ;
#107916 = ORIENTED_EDGE ( 'NONE', *, *, #136694, .T. ) ;
#107917 = EDGE_LOOP ( 'NONE', ( #183651, #100749, #40134, #180465 ) ) ;
#107918 = EDGE_CURVE ( 'NONE', #96638, #113005, #135906, .T. ) ;
#107919 = PLANE ( 'NONE',  #26381 ) ;
#107920 = DIRECTION ( 'NONE',  ( 0.000000000000000000, -1.000000000000000000, 0.000000000000000000 ) ) ;
#107921 = CARTESIAN_POINT ( 'NONE',  ( -13.11924609551136101, 9.431689550535258704, -185.7792900322359912 ) ) ;
#107923 = ORIENTED_EDGE ( 'NONE', *, *, #133972, .F. ) ;
#107922 = CARTESIAN_POINT ( 'NONE',  ( -23.15000000000000213, 1.115600667400684642E-11, -134.0000000000000000 ) ) ;
#107924 = AXIS2_PLACEMENT_3D ( 'NONE', #29395, #228848, #108886 ) ;
#107925 = DIRECTION ( 'NONE',  ( 0.7071067811865474617, -0.6824534298470372740, 0.1850873201762209819 ) ) ;
#107926 = EDGE_CURVE ( 'NONE', #201378, #105637, #194214, .T. ) ;
#107927 = SPHERICAL_SURFACE ( 'NONE', #3473, 0.1000000000000000056 ) ;
#107929 = ORIENTED_EDGE ( 'NONE', *, *, #93950, .F. ) ;
#107928 = FACE_OUTER_BOUND ( 'NONE', #76725, .T. ) ;
#107930 = DIRECTION ( 'NONE',  ( -2.561896900575096011E-15, 0.5907332058517336115, -0.8068669527896984439 ) ) ;
#107932 = EDGE_CURVE ( 'NONE', #79795, #246557, #106684, .T. ) ;
#107931 = ORIENTED_EDGE ( 'NONE', *, *, #55574, .T. ) ;
#107933 = CARTESIAN_POINT ( 'NONE',  ( -20.64999999999999858, 2.000000000011154189, -113.7246219227621395 ) ) ;
#107934 = ORIENTED_EDGE ( 'NONE', *, *, #174805, .T. ) ;
#107935 = CARTESIAN_POINT ( 'NONE',  ( -21.05000000000000071, -11.48912529306490349, -137.0000000000000000 ) ) ;
#107936 = DIRECTION ( 'NONE',  ( -0.7071067811865487940, 0.7071067811865463515, 0.000000000000000000 ) ) ;
#107937 = ORIENTED_EDGE ( 'NONE', *, *, #106163, .T. ) ;
#107940 = CARTESIAN_POINT ( 'NONE',  ( -21.05000000000000071, -11.74999999998884448, -130.9000000000000341 ) ) ;
#107939 = CARTESIAN_POINT ( 'NONE',  ( -23.15000000000000213, 76.00000000001195133, -103.0231074845243171 ) ) ;
#107938 = AXIS2_PLACEMENT_3D ( 'NONE', #155814, #38410, #235318 ) ;
#107941 = CIRCLE ( 'NONE', #24773, 0.1000000000000028644 ) ;
#107942 = DIRECTION ( 'NONE',  ( 0.000000000000000000, -0.07893460099012014619, 0.9968797965484758050 ) ) ;
#107943 = DIRECTION ( 'NONE',  ( 0.000000000000000000, 0.000000000000000000, 1.000000000000000000 ) ) ;
#107944 = DIRECTION ( 'NONE',  ( 0.7071067811865708874, -0.3338907855511046296, -0.6233112732207185536 ) ) ;
#107945 = AXIS2_PLACEMENT_3D ( 'NONE', #96822, #238945, #60283 ) ;
#107946 = ORIENTED_EDGE ( 'NONE', *, *, #43954, .F. ) ;
#107947 = VERTEX_POINT ( 'NONE', #146739 ) ;
#107948 = CARTESIAN_POINT ( 'NONE',  ( 18.79999999999999716, 1.350000000000000089, 22.10000000000000142 ) ) ;
#107949 = CARTESIAN_POINT ( 'NONE',  ( -20.85000000000000142, 7.128833340094563376, -233.7327013124401276 ) ) ;
#107951 = ORIENTED_EDGE ( 'NONE', *, *, #113904, .F. ) ;
#107950 = EDGE_CURVE ( 'NONE', #123338, #71514, #52523, .T. ) ;
#107952 = CARTESIAN_POINT ( 'NONE',  ( -20.00857864376270001, 9.150000000011157653, -188.7499999999999716 ) ) ;
#107953 = VERTEX_POINT ( 'NONE', #7247 ) ;
#107954 = EDGE_CURVE ( 'NONE', #8827, #173018, #182129, .T. ) ;
#107955 = PLANE ( 'NONE',  #194104 ) ;
#107956 = VERTEX_POINT ( 'NONE', #205449 ) ;
#107957 = DIRECTION ( 'NONE',  ( 0.000000000000000000, -0.9651348961777379554, 0.2617529984164210233 ) ) ;
#107958 = CIRCLE ( 'NONE', #236950, 0.09999999999998898659 ) ;
#107959 = VECTOR ( 'NONE', #16679, 1000.000000000000000 ) ;
#107960 = CYLINDRICAL_SURFACE ( 'NONE', #19981, 0.1000000000000008105 ) ;
#107961 = CARTESIAN_POINT ( 'NONE',  ( -18.40000000000000213, 11.75000000001113953, -154.8500000000000227 ) ) ;
#107963 = EDGE_CURVE ( 'NONE', #10085, #174644, #244235, .T. ) ;
#107962 = ORIENTED_EDGE ( 'NONE', *, *, #15436, .T. ) ;
#107964 = CARTESIAN_POINT ( 'NONE',  ( -16.77828822459933633, 63.08606603224484388, -213.1407965249532310 ) ) ;
#107965 = PRESENTATION_STYLE_ASSIGNMENT (( #191383 ) ) ;
#107967 = ORIENTED_EDGE ( 'NONE', *, *, #62543, .T. ) ;
#107966 = AXIS2_PLACEMENT_3D ( 'NONE', #93848, #173453, #252919 ) ;
#107968 = ORIENTED_EDGE ( 'NONE', *, *, #20272, .T. ) ;
#107969 = CIRCLE ( 'NONE', #66279, 0.09999999999998898659 ) ;
#107970 = AXIS2_PLACEMENT_3D ( 'NONE', #205766, #106649, #186220 ) ;
#107971 = ORIENTED_EDGE ( 'NONE', *, *, #119685, .T. ) ;
#107972 = VECTOR ( 'NONE', #139339, 1000.000000000000000 ) ;
#107973 = LINE ( 'NONE', #148384, #196048 ) ;
#107974 = LINE ( 'NONE', #6284, #128119 ) ;
#107975 = CARTESIAN_POINT ( 'NONE',  ( 21.14999999999999858, 69.35000000001205933, -124.1731074845243370 ) ) ;
#107976 = DIRECTION ( 'NONE',  ( 0.000000000000000000, 1.776356839400199780E-15, -1.000000000000000000 ) ) ;
#107977 = AXIS2_PLACEMENT_3D ( 'NONE', #6256, #166666, #198376 ) ;
#107979 = CARTESIAN_POINT ( 'NONE',  ( 21.11747605621531321, 8.778708005492896760, -12.24456316978977988 ) ) ;
#107978 = DIRECTION ( 'NONE',  ( -1.000000000000000000, 0.000000000000000000, 0.000000000000000000 ) ) ;
#107981 = ORIENTED_EDGE ( 'NONE', *, *, #22995, .T. ) ;
#107980 = FACE_OUTER_BOUND ( 'NONE', #169409, .T. ) ;
#107982 = CARTESIAN_POINT ( 'NONE',  ( -21.78635804494510708, 10.36375008473801174, -227.4840496025197751 ) ) ;
#107983 = VERTEX_POINT ( 'NONE', #86776 ) ;
#107984 = EDGE_LOOP ( 'NONE', ( #100352, #100174, #174290, #162423 ) ) ;
#107985 = VERTEX_POINT ( 'NONE', #182058 ) ;
#107986 = DIRECTION ( 'NONE',  ( 0.000000000000000000, -0.8814952561688425003, 0.4721928772777359007 ) ) ;
#107987 = FACE_BOUND ( 'NONE', #75116, .T. ) ;
#107989 = EDGE_CURVE ( 'NONE', #113573, #146959, #60896, .T. ) ;
#107988 = CARTESIAN_POINT ( 'NONE',  ( 20.94999999999999574, 76.00000000001237765, -170.0231074845243597 ) ) ;
#107990 = FACE_OUTER_BOUND ( 'NONE', #170706, .T. ) ;
#107991 = EDGE_CURVE ( 'NONE', #196598, #169810, #65954, .T. ) ;
#107992 = VECTOR ( 'NONE', #158442, 1000.000000000000000 ) ;
#107993 = DIRECTION ( 'NONE',  ( 0.000000000000000000, -1.000000000000000000, 2.775557561562884094E-14 ) ) ;
#107994 = ORIENTED_EDGE ( 'NONE', *, *, #57751, .F. ) ;
#107995 = ORIENTED_EDGE ( 'NONE', *, *, #225315, .F. ) ;
#107997 = ADVANCED_FACE ( 'NONE', ( #124649 ), #140013, .T. ) ;
#107996 = DIRECTION ( 'NONE',  ( -4.408576920032447972E-17, -0.1350103645451946055, 0.9908441862701591329 ) ) ;
#107998 = ORIENTED_EDGE ( 'NONE', *, *, #92879, .F. ) ;
#107999 = CARTESIAN_POINT ( 'NONE',  ( 23.15000000000000213, 86.27712145182582049, -209.5223386573213702 ) ) ;
#108000 = DIRECTION ( 'NONE',  ( -0.000000000000000000, 6.982962677686266711E-15, -1.000000000000000000 ) ) ;
#108001 = ORIENTED_EDGE ( 'NONE', *, *, #255197, .F. ) ;
#108002 = DIRECTION ( 'NONE',  ( 7.304098846218134667E-16, -1.000000000000000000, -6.982962677686267499E-15 ) ) ;
#108003 = FACE_OUTER_BOUND ( 'NONE', #88932, .T. ) ;
#108004 = CARTESIAN_POINT ( 'NONE',  ( -21.05000000000000071, 35.94660524813657076, -234.4748257877825495 ) ) ;
#108005 = FACE_OUTER_BOUND ( 'NONE', #248829, .T. ) ;
#108006 = ORIENTED_EDGE ( 'NONE', *, *, #126979, .F. ) ;
#108007 = CARTESIAN_POINT ( 'NONE',  ( -22.59999999999999432, 64.25012875563564307, -136.5885370755380279 ) ) ;
#108008 = ADVANCED_FACE ( 'NONE', ( #8550 ), #2642, .T. ) ;
#108009 = DIRECTION ( 'NONE',  ( 0.000000000000000000, -7.172728831056617961E-15, 1.000000000000000000 ) ) ;
#108010 = FACE_OUTER_BOUND ( 'NONE', #157984, .T. ) ;
#108011 = AXIS2_PLACEMENT_3D ( 'NONE', #7764, #23506, #122584 ) ;
#108012 = LINE ( 'NONE', #88414, #108511 ) ;
#108014 = EDGE_CURVE ( 'NONE', #228214, #115670, #102564, .T. ) ;
#108013 = DIRECTION ( 'NONE',  ( 1.000000000000000000, 0.000000000000000000, 0.000000000000000000 ) ) ;
#108015 = TOROIDAL_SURFACE ( 'NONE', #207977, 4.099999999999999645, 0.1000000000000000056 ) ;
#108016 = DIRECTION ( 'NONE',  ( 1.000000000000000000, 0.000000000000000000, 0.000000000000000000 ) ) ;
#108017 = MANIFOLD_SOLID_BREP ( 'Stock-MAS-200-1', #74159 ) ;
#108018 = VECTOR ( 'NONE', #171205, 1000.000000000000000 ) ;
#108019 = EDGE_CURVE ( 'NONE', #116663, #107897, #131643, .T. ) ;
#108020 = EDGE_LOOP ( 'NONE', ( #211584, #3307, #148246, #76826 ) ) ;
#108022 = ADVANCED_FACE ( 'NONE', ( #230158 ), #168949, .F. ) ;
#108021 = EDGE_CURVE ( 'NONE', #239334, #107898, #119177, .T. ) ;
#108023 = CARTESIAN_POINT ( 'NONE',  ( 21.05000000000000071, 16.98881331171930498, -224.4946931418895417 ) ) ;
#108024 = VERTEX_POINT ( 'NONE', #133622 ) ;
#108025 = CARTESIAN_POINT ( 'NONE',  ( -18.40000000000000213, 11.47316190337364183, -121.3914213562373448 ) ) ;
#108026 = CARTESIAN_POINT ( 'NONE',  ( -18.59999999999999787, 18.81339837015603322, -226.7756228984618190 ) ) ;
#108027 = CYLINDRICAL_SURFACE ( 'NONE', #81290, 4.049999999999998046 ) ;
#108028 = CARTESIAN_POINT ( 'NONE',  ( 20.54374330479327426, 65.49498968578932079, -162.2974238496363171 ) ) ;
#108029 = CIRCLE ( 'NONE', #141333, 0.09999999999999609201 ) ;
#108030 = VERTEX_POINT ( 'NONE', #48946 ) ;
#108031 = DIRECTION ( 'NONE',  ( -0.000000000000000000, 1.000000000000000000, 6.982962677686267499E-15 ) ) ;
#108032 = CIRCLE ( 'NONE', #253744, 0.1000000000000010186 ) ;
#108033 = CARTESIAN_POINT ( 'NONE',  ( -18.69999999999999929, -8.250000000000005329, -7.800000000000000711 ) ) ;
#108034 = CARTESIAN_POINT ( 'NONE',  ( -21.00000000000000000, 7.973296578895943121, -1.410778198689825347 ) ) ;
#108035 = EDGE_CURVE ( 'NONE', #255259, #89722, #69311, .T. ) ;
#108037 = EDGE_CURVE ( 'NONE', #181022, #77841, #181716, .T. ) ;
#108036 = CIRCLE ( 'NONE', #228672, 0.2000000000000111688 ) ;
#108038 = CARTESIAN_POINT ( 'NONE',  ( 20.94999999999999929, 28.56975825374500388, -258.1421690862028413 ) ) ;
#108039 = EDGE_LOOP ( 'NONE', ( #252157, #107253, #137834, #35614, #139613 ) ) ;
#108040 = ORIENTED_EDGE ( 'NONE', *, *, #10208, .F. ) ;
#108041 = LINE ( 'NONE', #145861, #112546 ) ;
#108042 = CARTESIAN_POINT ( 'NONE',  ( 20.94999999999999929, 82.57900542960499024, -215.5587758314583766 ) ) ;
#108043 = DIRECTION ( 'NONE',  ( 0.000000000000000000, -1.000000000000000000, 0.000000000000000000 ) ) ;
#108045 = EDGE_CURVE ( 'NONE', #8209, #90248, #215030, .T. ) ;
#108044 = CARTESIAN_POINT ( 'NONE',  ( -23.25000000000000000, 77.83585931145526615, -57.91866831572577468 ) ) ;
#108046 = CARTESIAN_POINT ( 'NONE',  ( -20.64999999999999858, 62.04503132991428060, -248.4786563706009588 ) ) ;
#108047 =( BOUNDED_CURVE ( )  B_SPLINE_CURVE ( 3, ( #171453, #86710, #26795, #108868 ),
 .UNSPECIFIED., .F., .F. ) 
 B_SPLINE_CURVE_WITH_KNOTS ( ( 4, 4 ),
 ( 3.752122642744872394, 4.712388980384671910 ),
 .UNSPECIFIED. ) 
 CURVE ( )  GEOMETRIC_REPRESENTATION_ITEM ( )  RATIONAL_B_SPLINE_CURVE ( ( 1.000000000000000000, 0.9246222802177666011, 0.9246222802177666011, 1.000000000000000000 ) ) 
 REPRESENTATION_ITEM ( '' )  );
#108048 = EDGE_LOOP ( 'NONE', ( #32732, #229274, #200258, #1308 ) ) ;
#108050 = EDGE_CURVE ( 'NONE', #44904, #121706, #153228, .T. ) ;
#108049 = CARTESIAN_POINT ( 'NONE',  ( -22.39999999999999858, 11.40444339177023814, -198.6185779617709670 ) ) ;
#108051 = EDGE_CURVE ( 'NONE', #246673, #191026, #29432, .T. ) ;
#108052 = CARTESIAN_POINT ( 'NONE',  ( 21.00000000000000000, 12.15477401631902232, -210.9923204818763622 ) ) ;
#108053 = ORIENTED_EDGE ( 'NONE', *, *, #48345, .T. ) ;
#108054 = SPHERICAL_SURFACE ( 'NONE', #71230, 0.1000000000000000056 ) ;
#108055 = CIRCLE ( 'NONE', #149766, 0.1000000000000024342 ) ;
#108056 = ORIENTED_EDGE ( 'NONE', *, *, #30896, .F. ) ;
#108057 = ORIENTED_EDGE ( 'NONE', *, *, #185047, .T. ) ;
#108058 = ORIENTED_EDGE ( 'NONE', *, *, #2840, .F. ) ;
#108059 = ADVANCED_FACE ( 'NONE', ( #150627 ), #72391, .F. ) ;
#108060 = CARTESIAN_POINT ( 'NONE',  ( 20.95429693346636313, 10.54330487990693044, -74.56088253831309487 ) ) ;
#108061 = CARTESIAN_POINT ( 'NONE',  ( -23.25000000000000000, 76.00000000001190870, -103.0231074845243029 ) ) ;
#108062 = DIRECTION ( 'NONE',  ( 0.000000000000000000, -0.9915357197604882655, 0.1298341882519793711 ) ) ;
#108063 = FACE_OUTER_BOUND ( 'NONE', #164165, .T. ) ;
#108064 = DIRECTION ( 'NONE',  ( -1.000000000000000000, 0.000000000000000000, 0.000000000000000000 ) ) ;
#108065 = CARTESIAN_POINT ( 'NONE',  ( -23.15000000000000213, 76.00000000001267608, -203.5231074845243597 ) ) ;
#108066 = CARTESIAN_POINT ( 'NONE',  ( 23.14999999999999858, 79.90000000001244018, -170.0231074845243313 ) ) ;
#108068 = CARTESIAN_POINT ( 'NONE',  ( 18.49999999999999645, 77.63717271298298783, -191.9409541190523214 ) ) ;
#108067 = DIRECTION ( 'NONE',  ( -0.000000000000000000, 0.000000000000000000, 1.000000000000000000 ) ) ;
#108069 = EDGE_CURVE ( 'NONE', #246608, #116008, #244070, .T. ) ;
#108070 = AXIS2_PLACEMENT_3D ( 'NONE', #30801, #93308, #252366 ) ;
#108071 = CARTESIAN_POINT ( 'NONE',  ( -21.55000000000000071, 7.350000000011155166, -146.3500000000000227 ) ) ;
#108072 = AXIS2_PLACEMENT_3D ( 'NONE', #59813, #100222, #196773 ) ;
#108073 = CARTESIAN_POINT ( 'NONE',  ( -18.59999999999999787, 14.81796439977981272, -236.5325475414793743 ) ) ;
#108074 = DIRECTION ( 'NONE',  ( -0.000000000000000000, 3.469446951953635015E-14, 1.000000000000000000 ) ) ;
#108075 = TOROIDAL_SURFACE ( 'NONE', #45704, 0.6000000000000017542, 0.1000000000000000056 ) ;
#108077 = CARTESIAN_POINT ( 'NONE',  ( 20.94999999999999574, 18.75483929237739744, -228.0790484105328630 ) ) ;
#108076 = TOROIDAL_SURFACE ( 'NONE', #208038, 0.9750000000000019762, 0.1000000000000000056 ) ;
#108078 = ORIENTED_EDGE ( 'NONE', *, *, #198996, .T. ) ;
#108079 = VERTEX_POINT ( 'NONE', #108920 ) ;
#108080 = DIRECTION ( 'NONE',  ( 1.000000000000000000, 0.000000000000000000, 0.000000000000000000 ) ) ;
#108081 = FACE_OUTER_BOUND ( 'NONE', #91525, .T. ) ;
#108083 = CARTESIAN_POINT ( 'NONE',  ( -12.24999999999999822, 12.72489043187539970, -215.4897534858791914 ) ) ;
#108082 = DIRECTION ( 'NONE',  ( 0.000000000000000000, 1.000000000000000000, 6.982962677686266711E-15 ) ) ;
#108084 =( BOUNDED_SURFACE ( )  B_SPLINE_SURFACE ( 3, 2, ( 
 ( #213277, #34676, #131177 ),
 ( #135007, #12546, #175472 ),
 ( #235406, #93334, #15100 ),
 ( #56744, #92052, #152058 ) ),
 .UNSPECIFIED., .F., .F., .F. ) 
 B_SPLINE_SURFACE_WITH_KNOTS ( ( 4, 4 ),
 ( 3, 3 ),
 ( 0.0002700421466196717673, 0.0004789321604330915635 ),
 ( 0.000000000000000000, 1.000000000000000000 ),
 .UNSPECIFIED. ) 
 GEOMETRIC_REPRESENTATION_ITEM ( )  RATIONAL_B_SPLINE_SURFACE ( (
 ( 1.000000000000000000, 0.7071067811865475727, 1.000000000000000000),
 ( 1.000000000000000000, 0.7163411249511619783, 1.000000000000000000),
 ( 1.000000000000000000, 0.7221957104841967290, 1.000000000000000000),
 ( 1.000000000000000000, 0.7250110520819876836, 1.000000000000000000) ) ) 
 REPRESENTATION_ITEM ( '' )  SURFACE ( )  );
#108085 = AXIS2_PLACEMENT_3D ( 'NONE', #119930, #161616, #241145 ) ;
#108086 = CARTESIAN_POINT ( 'NONE',  ( 20.95512820512820440, 39.31056039967181448, -236.7220595557971023 ) ) ;
#108087 = EDGE_CURVE ( 'NONE', #236989, #223188, #48438, .T. ) ;
#108088 = DIRECTION ( 'NONE',  ( 0.000000000000000000, 0.000000000000000000, -1.000000000000000000 ) ) ;
#108089 = VERTEX_POINT ( 'NONE', #174085 ) ;
#108090 = ORIENTED_EDGE ( 'NONE', *, *, #45816, .F. ) ;
#108091 = CIRCLE ( 'NONE', #207489, 4.000000000000003553 ) ;
#108092 = VECTOR ( 'NONE', #111868, 1000.000000000000000 ) ;
#108094 = AXIS2_PLACEMENT_3D ( 'NONE', #124800, #25695, #66097 ) ;
#108093 = CARTESIAN_POINT ( 'NONE',  ( 21.15000000000005187, 64.35000000001120668, -36.02310748452479316 ) ) ;
#108095 = ORIENTED_EDGE ( 'NONE', *, *, #198967, .F. ) ;
#108096 = DIRECTION ( 'NONE',  ( -0.000000000000000000, -1.000000000000000000, 6.308085367188393199E-16 ) ) ;
#108097 = TOROIDAL_SURFACE ( 'NONE', #12430, 0.2000000000000000111, 0.1000000000000000056 ) ;
#108098 = CARTESIAN_POINT ( 'NONE',  ( 23.14999999999999858, 67.63082410804655353, -211.8415745842588649 ) ) ;
#108099 = ORIENTED_EDGE ( 'NONE', *, *, #14984, .F. ) ;
#108100 = CARTESIAN_POINT ( 'NONE',  ( 18.59999999999999076, 43.16354019706792400, -239.5695141926698284 ) ) ;
#108101 = ORIENTED_EDGE ( 'NONE', *, *, #126539, .F. ) ;
#108102 = CARTESIAN_POINT ( 'NONE',  ( -21.45000000000000284, 29.50054346320101928, -236.9717244483098568 ) ) ;
#108103 = DIRECTION ( 'NONE',  ( 0.000000000000000000, 0.000000000000000000, 1.000000000000000000 ) ) ;
#108104 = DIRECTION ( 'NONE',  ( -0.000000000000000000, 0.9876197685951279004, -0.1568667991644694115 ) ) ;
#108105 = CARTESIAN_POINT ( 'NONE',  ( 18.46082813848004989, -9.480749650896274972, -141.0843701027156669 ) ) ;
#108106 = CARTESIAN_POINT ( 'NONE',  ( -23.25000000000000000, 64.25000000001195133, -103.0231074845244024 ) ) ;
#108107 = DIRECTION ( 'NONE',  ( 0.000000000000000000, 1.000000000000000000, -0.000000000000000000 ) ) ;
#108108 = CARTESIAN_POINT ( 'NONE',  ( -20.64999999999999858, 7.128833340094563376, -233.7327013124401276 ) ) ;
#108109 = DIRECTION ( 'NONE',  ( 1.000000000000000000, -0.000000000000000000, -0.000000000000000000 ) ) ;
#108111 = ORIENTED_EDGE ( 'NONE', *, *, #55615, .T. ) ;
#108110 = CARTESIAN_POINT ( 'NONE',  ( -20.85000000000000142, 77.83585931145546510, -91.51866831572576189 ) ) ;
#108113 = CARTESIAN_POINT ( 'NONE',  ( 20.94999999999999929, 8.433899723187009201, -209.4150263691077782 ) ) ;
#108112 = DIRECTION ( 'NONE',  ( 0.000000000000000000, -1.000000000000000000, 0.000000000000000000 ) ) ;
#108114 = ORIENTED_EDGE ( 'NONE', *, *, #16516, .F. ) ;
#108116 = ORIENTED_EDGE ( 'NONE', *, *, #159900, .F. ) ;
#108115 = DIRECTION ( 'NONE',  ( 1.000000000000000000, 0.000000000000000000, 0.000000000000000000 ) ) ;
#108117 = ORIENTED_EDGE ( 'NONE', *, *, #148858, .T. ) ;
#108118 = CYLINDRICAL_SURFACE ( 'NONE', #257281, 2.000000000000003553 ) ;
#108119 = CARTESIAN_POINT ( 'NONE',  ( -18.59999999999999787, 9.250000000011157297, -54.65000000000000568 ) ) ;
#108120 = DIRECTION ( 'NONE',  ( 0.000000000000000000, 0.8777080977375072424, -0.4791956752371691608 ) ) ;
#108121 = CARTESIAN_POINT ( 'NONE',  ( -20.64999999999999858, 7.128833340093095217, -233.7327013124392749 ) ) ;
#108122 = AXIS2_PLACEMENT_3D ( 'NONE', #133299, #52450, #132007 ) ;
#108123 = CARTESIAN_POINT ( 'NONE',  ( -21.05000000000000071, 11.75000000001115552, -93.48519422934610645 ) ) ;
#108124 = DIRECTION ( 'NONE',  ( -1.000000000000000000, 0.000000000000000000, 0.000000000000000000 ) ) ;
#108125 = CARTESIAN_POINT ( 'NONE',  ( 20.94999999999999929, 76.00000000001213607, -136.5231074845243313 ) ) ;
#108126 = DIRECTION ( 'NONE',  ( 0.000000000000000000, 0.000000000000000000, -1.000000000000000000 ) ) ;
#108127 = ADVANCED_FACE ( 'NONE', ( #151937 ), #188460, .F. ) ;
#108128 = FACE_OUTER_BOUND ( 'NONE', #186350, .T. ) ;
#108129 = EDGE_LOOP ( 'NONE', ( #228440, #240655, #245763 ) ) ;
#108130 = VERTEX_POINT ( 'NONE', #228882 ) ;
#108131 = CARTESIAN_POINT ( 'NONE',  ( -16.91247567987037570, 9.959082683680401615, -180.1287244585373060 ) ) ;
#108132 = VECTOR ( 'NONE', #156536, 1000.000000000000000 ) ;
#108133 = EDGE_LOOP ( 'NONE', ( #227560, #236209, #6832, #39927 ) ) ;
#108134 = DIRECTION ( 'NONE',  ( 0.000000000000000000, -0.7397890806274223241, -0.6728388485993012091 ) ) ;
#108136 = ORIENTED_EDGE ( 'NONE', *, *, #181647, .F. ) ;
#108135 = VECTOR ( 'NONE', #113543, 1000.000000000000000 ) ;
#108137 = DIRECTION ( 'NONE',  ( -3.469446951953605354E-14, 1.000000000000000000, 0.000000000000000000 ) ) ;
#108138 = AXIS2_PLACEMENT_3D ( 'NONE', #257388, #215742, #254826 ) ;
#108139 = CARTESIAN_POINT ( 'NONE',  ( 19.86930884467583525, 11.68691006697099866, -24.73922263893871332 ) ) ;
#108140 = CARTESIAN_POINT ( 'NONE',  ( -0.8999999999999993561, -8.250000000000005329, 26.00000000000000355 ) ) ;
#108141 = EDGE_CURVE ( 'NONE', #248135, #93031, #56778, .T. ) ;
#108142 = DIRECTION ( 'NONE',  ( 0.000000000000000000, 0.000000000000000000, 1.000000000000000000 ) ) ;
#108143 = CARTESIAN_POINT ( 'NONE',  ( 21.22070241538126467, 75.90108096947770377, -209.9930537573939660 ) ) ;
#108144 = ORIENTED_EDGE ( 'NONE', *, *, #77830, .F. ) ;
#108145 = VECTOR ( 'NONE', #148736, 1000.000000000000000 ) ;
#108146 = AXIS2_PLACEMENT_3D ( 'NONE', #216488, #133112, #117393 ) ;
#108147 = EDGE_CURVE ( 'NONE', #165923, #156363, #209304, .T. ) ;
#108148 = DIRECTION ( 'NONE',  ( 0.000000000000000000, -1.000000000000000000, 0.000000000000000000 ) ) ;
#108149 = CARTESIAN_POINT ( 'NONE',  ( 20.94999999999999929, 85.50000000001222134, -146.4170766071767389 ) ) ;
#108150 = CARTESIAN_POINT ( 'NONE',  ( -18.59999999999999787, 64.35000000001264198, -196.5083017138704236 ) ) ;
#108151 = CARTESIAN_POINT ( 'NONE',  ( -20.64999999999999858, 84.73084112150795022, -193.9250327655399531 ) ) ;
#108152 = ORIENTED_EDGE ( 'NONE', *, *, #164491, .T. ) ;
#108154 = CARTESIAN_POINT ( 'NONE',  ( 21.14999999999999858, 8.786607556611267356, -146.2500000000000284 ) ) ;
#108153 = DIRECTION ( 'NONE',  ( 0.000000000000000000, 0.000000000000000000, 1.000000000000000000 ) ) ;
#108155 = ADVANCED_FACE ( 'NONE', ( #210596, #80033, #59180 ), #37121, .F. ) ;
#108156 = ORIENTED_EDGE ( 'NONE', *, *, #101539, .T. ) ;
#108159 = VERTEX_POINT ( 'NONE', #254800 ) ;
#108158 = CARTESIAN_POINT ( 'NONE',  ( -16.80469485234343807, 51.58553706477307799, -231.9699984979453689 ) ) ;
#108157 = DIRECTION ( 'NONE',  ( 0.000000000000000000, 0.000000000000000000, 1.000000000000000000 ) ) ;
#108160 = AXIS2_PLACEMENT_3D ( 'NONE', #206766, #170257, #247159 ) ;
#108161 = VERTEX_POINT ( 'NONE', #119210 ) ;
#108162 = LINE ( 'NONE', #166884, #239281 ) ;
#108163 = VECTOR ( 'NONE', #222540, 1000.000000000000000 ) ;
#108164 = CIRCLE ( 'NONE', #249803, 0.09999999999998898659 ) ;
#108165 = CIRCLE ( 'NONE', #241438, 2.000000000000003553 ) ;
#108166 = AXIS2_PLACEMENT_3D ( 'NONE', #20583, #136641, #218741 ) ;
#108167 = DIRECTION ( 'NONE',  ( 1.000000000000000000, -0.000000000000000000, -0.000000000000000000 ) ) ;
#108168 = EDGE_CURVE ( 'NONE', #111061, #2364, #85821, .T. ) ;
#108169 = CARTESIAN_POINT ( 'NONE',  ( 18.59999999999997655, 76.00000000001170974, -69.52310748452431710 ) ) ;
#108170 = ORIENTED_EDGE ( 'NONE', *, *, #52518, .T. ) ;
#108171 = CARTESIAN_POINT ( 'NONE',  ( 18.49999999999999289, 67.65998959290219261, -227.8609496483021530 ) ) ;
#108172 = EDGE_CURVE ( 'NONE', #194825, #216685, #76205, .T. ) ;
#108173 = AXIS2_PLACEMENT_3D ( 'NONE', #253851, #59479, #176929 ) ;
#108174 = LINE ( 'NONE', #126437, #132187 ) ;
#108175 = EDGE_CURVE ( 'NONE', #1620, #232297, #152528, .T. ) ;
#108176 = DIRECTION ( 'NONE',  ( 1.000000000000000000, 0.000000000000000000, 0.000000000000000000 ) ) ;
#108178 = VERTEX_POINT ( 'NONE', #253560 ) ;
#108177 = CARTESIAN_POINT ( 'NONE',  ( 20.94560253601876809, 11.75000000001115907, -93.51008351251552142 ) ) ;
#108179 = ADVANCED_FACE ( 'NONE', ( #155789 ), #177906, .T. ) ;
#108180 = EDGE_LOOP ( 'NONE', ( #115477, #139936, #226991, #68278 ) ) ;
#108181 = CARTESIAN_POINT ( 'NONE',  ( -18.59999999999999787, 57.84918772656043018, -226.1321410194968280 ) ) ;
#108182 = AXIS2_PLACEMENT_3D ( 'NONE', #110831, #147398, #86102 ) ;
#108183 = DIRECTION ( 'NONE',  ( 0.000000000000000000, -0.8660254037844468122, -0.4999999999999859557 ) ) ;
#108184 = FACE_OUTER_BOUND ( 'NONE', #32745, .T. ) ;
#108185 = ORIENTED_EDGE ( 'NONE', *, *, #242993, .T. ) ;
#108186 = CARTESIAN_POINT ( 'NONE',  ( -23.25000000000000000, 26.47476584046484049, -241.8269156386531051 ) ) ;
#108187 = EDGE_CURVE ( 'NONE', #90864, #182918, #73418, .T. ) ;
#108188 = LINE ( 'NONE', #32532, #218320 ) ;
#108189 = EDGE_CURVE ( 'NONE', #186109, #135540, #23717, .T. ) ;
#108190 = EDGE_LOOP ( 'NONE', ( #59777, #180019, #134180, #24731 ) ) ;
#108191 = CARTESIAN_POINT ( 'NONE',  ( 20.94999999999999929, 7.533155231024652565, -235.5891828794142384 ) ) ;
#108192 = VECTOR ( 'NONE', #103944, 1000.000000000000000 ) ;
#108193 = ADVANCED_FACE ( 'NONE', ( #56613 ), #134879, .F. ) ;
#108194 = AXIS2_PLACEMENT_3D ( 'NONE', #33395, #60295, #15085 ) ;
#108195 = ORIENTED_EDGE ( 'NONE', *, *, #216381, .T. ) ;
#108196 = DIRECTION ( 'NONE',  ( 0.000000000000000000, 0.000000000000000000, -1.000000000000000000 ) ) ;
#108197 = FACE_OUTER_BOUND ( 'NONE', #216294, .T. ) ;
#108198 = AXIS2_PLACEMENT_3D ( 'NONE', #204828, #87450, #246532 ) ;
#108199 = ORIENTED_EDGE ( 'NONE', *, *, #170464, .F. ) ;
#108200 = ORIENTED_EDGE ( 'NONE', *, *, #239759, .F. ) ;
#108201 = ADVANCED_FACE ( 'NONE', ( #214436 ), #176629, .T. ) ;
#108202 = DIRECTION ( 'NONE',  ( 0.000000000000000000, 0.000000000000000000, 1.000000000000000000 ) ) ;
#108203 = VERTEX_POINT ( 'NONE', #216997 ) ;
#108205 = ORIENTED_EDGE ( 'NONE', *, *, #206330, .T. ) ;
#108204 = CARTESIAN_POINT ( 'NONE',  ( 12.33938619321247998, 66.63927620602653690, -186.2091802899177253 ) ) ;
#108206 = ORIENTED_EDGE ( 'NONE', *, *, #51999, .T. ) ;
#108207 = AXIS2_PLACEMENT_3D ( 'NONE', #102242, #591, #158441 ) ;
#108209 = EDGE_LOOP ( 'NONE', ( #182639, #3634, #247763 ) ) ;
#108208 = ORIENTED_EDGE ( 'NONE', *, *, #226747, .F. ) ;
#108210 = AXIS2_PLACEMENT_3D ( 'NONE', #234574, #130330, #215008 ) ;
#108211 = ORIENTED_EDGE ( 'NONE', *, *, #42276, .T. ) ;
#108212 = CARTESIAN_POINT ( 'NONE',  ( 20.99999999999997868, 76.00000000001165290, -69.52310748452431710 ) ) ;
#108213 = DIRECTION ( 'NONE',  ( 1.000000000000000000, 0.000000000000000000, 0.000000000000000000 ) ) ;
#108214 = AXIS2_PLACEMENT_3D ( 'NONE', #256045, #94455, #119170 ) ;
#108215 = CARTESIAN_POINT ( 'NONE',  ( 20.95263205890715952, 67.10425989211856290, -195.0335990775828066 ) ) ;
#108216 = ADVANCED_FACE ( 'NONE', ( #115341 ), #215712, .F. ) ;
#108217 = DIRECTION ( 'NONE',  ( 0.000000000000000000, 0.000000000000000000, 1.000000000000000000 ) ) ;
#108218 = ORIENTED_EDGE ( 'NONE', *, *, #222807, .F. ) ;
#108219 = ORIENTED_EDGE ( 'NONE', *, *, #70443, .F. ) ;
#108220 = CARTESIAN_POINT ( 'NONE',  ( 18.49999999999999645, -1.135018845899022466, -141.7169768834323520 ) ) ;
#108221 = ORIENTED_EDGE ( 'NONE', *, *, #249707, .T. ) ;
#108222 = LINE ( 'NONE', #224307, #113292 ) ;
#108224 = ORIENTED_EDGE ( 'NONE', *, *, #219539, .T. ) ;
#108223 = DIRECTION ( 'NONE',  ( -1.000000000000000000, 0.000000000000000000, 0.000000000000000000 ) ) ;
#108225 = EDGE_CURVE ( 'NONE', #204905, #99384, #181903, .T. ) ;
#108226 = ORIENTED_EDGE ( 'NONE', *, *, #20762, .T. ) ;
#108227 = CARTESIAN_POINT ( 'NONE',  ( -20.94999999999999929, 74.74783850729544099, -233.7633982527047465 ) ) ;
#108228 = EDGE_CURVE ( 'NONE', #127360, #254325, #252621, .T. ) ;
#108229 = EDGE_CURVE ( 'NONE', #191700, #40380, #36174, .T. ) ;
#108230 = ORIENTED_EDGE ( 'NONE', *, *, #163057, .F. ) ;
#108231 = AXIS2_PLACEMENT_3D ( 'NONE', #174227, #193749, #22516 ) ;
#108232 = AXIS2_PLACEMENT_3D ( 'NONE', #81171, #236412, #40815 ) ;
#108233 = DIRECTION ( 'NONE',  ( 0.000000000000000000, -1.000000000000000000, -6.352154140967427193E-15 ) ) ;
#108235 = ADVANCED_FACE ( 'NONE', ( #175350 ), #15330, .T. ) ;
#108234 = LINE ( 'NONE', #183911, #223604 ) ;
#108236 = ADVANCED_FACE ( 'NONE', ( #200028 ), #21411, .T. ) ;
#108238 = ORIENTED_EDGE ( 'NONE', *, *, #93184, .F. ) ;
#108237 = ORIENTED_EDGE ( 'NONE', *, *, #138635, .T. ) ;
#108239 = ORIENTED_EDGE ( 'NONE', *, *, #118295, .T. ) ;
#108240 = CYLINDRICAL_SURFACE ( 'NONE', #224113, 12.87499999999999822 ) ;
#108241 = VERTEX_POINT ( 'NONE', #145164 ) ;
#108242 = ORIENTED_EDGE ( 'NONE', *, *, #6164, .F. ) ;
#108243 = ADVANCED_FACE ( 'NONE', ( #25255 ), #66927, .T. ) ;
#108244 = CARTESIAN_POINT ( 'NONE',  ( -21.07928932188134041, 0.09889514566555068775, -161.1714833436066669 ) ) ;
#108246 = ORIENTED_EDGE ( 'NONE', *, *, #129665, .F. ) ;
#108245 = CYLINDRICAL_SURFACE ( 'NONE', #160244, 11.75000000000000000 ) ;
#108247 = CARTESIAN_POINT ( 'NONE',  ( -20.64999999999999858, 2.000000000011154189, -154.2753780772379173 ) ) ;
#108249 = DIRECTION ( 'NONE',  ( 0.000000000000000000, 0.2128009952263604232, -0.9770955615653316162 ) ) ;
#108248 = DIRECTION ( 'NONE',  ( -1.000000000000000000, -0.000000000000000000, 0.000000000000000000 ) ) ;
#108250 = DIRECTION ( 'NONE',  ( 0.000000000000000000, -1.000000000000000000, -6.352154140967427193E-15 ) ) ;
#108251 = DIRECTION ( 'NONE',  ( 1.000000000000000000, 0.000000000000000000, 0.000000000000000000 ) ) ;
#108252 = VERTEX_POINT ( 'NONE', #1801 ) ;
#108253 = ORIENTED_EDGE ( 'NONE', *, *, #223786, .T. ) ;
#108255 = AXIS2_PLACEMENT_3D ( 'NONE', #115152, #199846, #74781 ) ;
#108254 = PLANE ( 'NONE',  #40429 ) ;
#108256 = DIRECTION ( 'NONE',  ( 1.000000000000000000, 0.000000000000000000, 0.000000000000000000 ) ) ;
#108257 = AXIS2_PLACEMENT_3D ( 'NONE', #155770, #218255, #59162 ) ;
#108258 = AXIS2_PLACEMENT_3D ( 'NONE', #216792, #98103, #179001 ) ;
#108259 = AXIS2_PLACEMENT_3D ( 'NONE', #28164, #30731, #26878 ) ;
#108260 = ORIENTED_EDGE ( 'NONE', *, *, #164510, .F. ) ;
#108261 = ADVANCED_FACE ( 'NONE', ( #141331 ), #205133, .F. ) ;
#108262 = AXIS2_PLACEMENT_3D ( 'NONE', #113166, #153633, #233146 ) ;
#108263 = DIRECTION ( 'NONE',  ( 1.000000000000000000, 0.000000000000000000, 0.000000000000000000 ) ) ;
#108264 = VERTEX_POINT ( 'NONE', #242987 ) ;
#108265 = VERTEX_POINT ( 'NONE', #163465 ) ;
#108266 = CARTESIAN_POINT ( 'NONE',  ( -23.25000000000000000, 0.000000000000000000, 0.000000000000000000 ) ) ;
#108267 = CARTESIAN_POINT ( 'NONE',  ( 20.94999999999999574, 87.39257802171833589, -200.4491579046923277 ) ) ;
#108269 = ADVANCED_FACE ( 'NONE', ( #44803 ), #27838, .F. ) ;
#108268 = VERTEX_POINT ( 'NONE', #142592 ) ;
#108270 = CARTESIAN_POINT ( 'NONE',  ( -21.14999999999999858, 11.75000000001115197, -107.2838656629781724 ) ) ;
#108271 = CARTESIAN_POINT ( 'NONE',  ( 21.05281448260627641, 8.776010158548784190, -112.6735579118114572 ) ) ;
#108272 = ORIENTED_EDGE ( 'NONE', *, *, #56353, .F. ) ;
#108273 = EDGE_CURVE ( 'NONE', #66775, #130783, #42238, .T. ) ;
#108274 = LINE ( 'NONE', #24900, #102279 ) ;
#108275 = FACE_OUTER_BOUND ( 'NONE', #19211, .T. ) ;
#108277 = CARTESIAN_POINT ( 'NONE',  ( -21.05000000000000071, 10.30543449102040476, -228.0143625250146329 ) ) ;
#108276 = CARTESIAN_POINT ( 'NONE',  ( 21.14999999999999858, 65.61575147395463148, -242.1939180743342774 ) ) ;
#108278 = DIRECTION ( 'NONE',  ( -1.000000000000000000, -0.000000000000000000, -0.000000000000000000 ) ) ;
#108280 = CARTESIAN_POINT ( 'NONE',  ( 23.14999999999999858, 64.40000000001194280, -109.9513107147998880 ) ) ;
#108279 = VECTOR ( 'NONE', #82956, 1000.000000000000000 ) ;
#108281 = CARTESIAN_POINT ( 'NONE',  ( 18.41356215285961540, -9.499999999988867572, -174.5320693966995691 ) ) ;
#108282 = AXIS2_PLACEMENT_3D ( 'NONE', #203405, #142134, #121334 ) ;
#108283 = CARTESIAN_POINT ( 'NONE',  ( -23.15000000000000213, 31.36165455396662693, -233.4973802202241302 ) ) ;
#108284 = B_SPLINE_CURVE_WITH_KNOTS ( 'NONE', 3,
 ( #137097, #195815, #17171, #96648, #236191, #255712, #77120 ),
 .UNSPECIFIED., .F., .F.,
 ( 4, 3, 4 ),
 ( 0.000000000000000000, 1.860045280646148997E-05, 5.251155757305322482E-05 ),
 .UNSPECIFIED. ) ;
#108285 = ORIENTED_EDGE ( 'NONE', *, *, #153401, .F. ) ;
#108286 = VECTOR ( 'NONE', #105050, 1000.000000000000000 ) ;
#108288 = ORIENTED_EDGE ( 'NONE', *, *, #42890, .F. ) ;
#108287 = ORIENTED_EDGE ( 'NONE', *, *, #73778, .T. ) ;
#108289 = ORIENTED_EDGE ( 'NONE', *, *, #50743, .T. ) ;
#108290 = FACE_OUTER_BOUND ( 'NONE', #44105, .T. ) ;
#108291 = CARTESIAN_POINT ( 'NONE',  ( 11.60000000000006004, 67.65000000001118963, -16.98168612828748891 ) ) ;
#108293 = FACE_OUTER_BOUND ( 'NONE', #138942, .T. ) ;
#108292 = SPHERICAL_SURFACE ( 'NONE', #3721, 0.1000000000000000056 ) ;
#108294 = DIRECTION ( 'NONE',  ( 0.000000000000000000, -1.000000000000000000, 0.000000000000000000 ) ) ;
#108295 = VERTEX_POINT ( 'NONE', #185594 ) ;
#108296 = DIRECTION ( 'NONE',  ( 0.000000000000000000, 0.5000000000000078826, -0.8660254037844340447 ) ) ;
#108297 = ORIENTED_EDGE ( 'NONE', *, *, #173304, .F. ) ;
#108298 = CARTESIAN_POINT ( 'NONE',  ( -21.11833042828136442, 0.007100509059333399813, 6.445644693855379082 ) ) ;
#108299 = DIRECTION ( 'NONE',  ( 1.000000000000000000, -0.000000000000000000, -0.000000000000000000 ) ) ;
#108300 = DIRECTION ( 'NONE',  ( 0.7071067811865487940, 8.659560562354918067E-17, 0.7071067811865463515 ) ) ;
#108301 = ORIENTED_EDGE ( 'NONE', *, *, #70252, .T. ) ;
#108302 = VECTOR ( 'NONE', #237029, 999.9999999999998863 ) ;
#108303 = CARTESIAN_POINT ( 'NONE',  ( 18.47654891039379166, -9.465274948382308651, -7.125975905194652960 ) ) ;
#108304 = DIRECTION ( 'NONE',  ( 0.000000000000000000, 0.000000000000000000, 1.000000000000000000 ) ) ;
#108305 = VERTEX_POINT ( 'NONE', #222118 ) ;
#108306 = ORIENTED_EDGE ( 'NONE', *, *, #36675, .T. ) ;
#108307 = CARTESIAN_POINT ( 'NONE',  ( -20.94999999999999929, -1.249999999988843369, -175.4999999999999716 ) ) ;
#108308 = CARTESIAN_POINT ( 'NONE',  ( -21.53551880898957904, 1.194799103070417035, -230.4417267841993464 ) ) ;
#108309 = AXIS2_PLACEMENT_3D ( 'NONE', #200677, #222780, #242356 ) ;
#108310 = DIRECTION ( 'NONE',  ( 1.000000000000000000, -0.000000000000000000, -0.000000000000000000 ) ) ;
#108311 = FACE_OUTER_BOUND ( 'NONE', #66164, .T. ) ;
#108312 = LINE ( 'NONE', #186575, #144191 ) ;
#108313 = DIRECTION ( 'NONE',  ( 1.020425574104004196E-15, 1.210927747993693964E-31, 1.000000000000000000 ) ) ;
#108314 = ORIENTED_EDGE ( 'NONE', *, *, #257599, .F. ) ;
#108315 = CARTESIAN_POINT ( 'NONE',  ( 23.14999999999999503, 69.35000000001259934, -191.2731074845243882 ) ) ;
#108316 = CARTESIAN_POINT ( 'NONE',  ( 23.24999999999999645, 64.25000000001190870, -93.77310748452438816 ) ) ;
#108317 = EDGE_CURVE ( 'NONE', #54351, #14295, #224704, .T. ) ;
#108319 = DIRECTION ( 'NONE',  ( -0.7071067811865389130, 4.937700262164590641E-15, -0.7071067811865561215 ) ) ;
#108318 = DIRECTION ( 'NONE',  ( 0.000000000000000000, 0.2128009952263603677, -0.9770955615653313941 ) ) ;
#108320 = LINE ( 'NONE', #153913, #4130 ) ;
#108321 = DIRECTION ( 'NONE',  ( -1.000000000000000000, 7.049440681616512959E-16, -1.911869773728117674E-16 ) ) ;
#108323 = EDGE_CURVE ( 'NONE', #9118, #28771, #82600, .T. ) ;
#108322 = DIRECTION ( 'NONE',  ( 0.000000000000000000, 0.000000000000000000, 1.000000000000000000 ) ) ;
#108324 = CARTESIAN_POINT ( 'NONE',  ( 18.59999999999999076, 10.49142135624846439, -158.7500000000000284 ) ) ;
#108325 = CIRCLE ( 'NONE', #150034, 0.1000000000000028644 ) ;
#108327 = ORIENTED_EDGE ( 'NONE', *, *, #156572, .T. ) ;
#108326 = CARTESIAN_POINT ( 'NONE',  ( -21.05000000000000071, 1.115600667400684642E-11, -100.5000000000000284 ) ) ;
#108328 = AXIS2_PLACEMENT_3D ( 'NONE', #105169, #140480, #183481 ) ;
#108329 = EDGE_CURVE ( 'NONE', #14291, #103697, #32078, .T. ) ;
#108330 = ADVANCED_FACE ( 'NONE', ( #81320 ), #65639, .T. ) ;
#108331 = STYLED_ITEM ( 'NONE', ( #82629 ), #193366 ) ;
#108332 = CIRCLE ( 'NONE', #150039, 0.09999999999999939493 ) ;
#108333 = CIRCLE ( 'NONE', #254055, 0.1999999999999987899 ) ;
#108334 = CARTESIAN_POINT ( 'NONE',  ( -20.94999999999999929, 76.00000000001216449, -140.5231074845243597 ) ) ;
#108335 = DIRECTION ( 'NONE',  ( 0.000000000000000000, -0.4999999999999949485, 0.8660254037844415942 ) ) ;
#108336 = ORIENTED_EDGE ( 'NONE', *, *, #216147, .F. ) ;
#108337 = VECTOR ( 'NONE', #94200, 1000.000000000000000 ) ;
#108338 = EDGE_CURVE ( 'NONE', #171037, #188779, #98650, .T. ) ;
#108339 = DIRECTION ( 'NONE',  ( 1.476360405086644309E-16, 1.000000000000000000, 0.000000000000000000 ) ) ;
#108341 = EDGE_CURVE ( 'NONE', #182454, #212829, #106879, .T. ) ;
#108340 = CIRCLE ( 'NONE', #79079, 0.1000000000000028644 ) ;
#108342 = TOROIDAL_SURFACE ( 'NONE', #66826, 0.2000000000000000111, 0.1000000000000000056 ) ;
#108343 = DIRECTION ( 'NONE',  ( 1.000000000000000000, 0.000000000000000000, 0.000000000000000000 ) ) ;
#108344 = CARTESIAN_POINT ( 'NONE',  ( -20.54999999999999716, 7.128833340094563376, -233.7327013124401276 ) ) ;
#108345 = AXIS2_PLACEMENT_3D ( 'NONE', #108601, #228566, #6930 ) ;
#108346 = CIRCLE ( 'NONE', #29273, 0.09999999999999939493 ) ;
#108347 = ORIENTED_EDGE ( 'NONE', *, *, #223582, .F. ) ;
#108348 = CYLINDRICAL_SURFACE ( 'NONE', #232988, 0.1000000000000028644 ) ;
#108350 = VERTEX_POINT ( 'NONE', #106030 ) ;
#108349 = CARTESIAN_POINT ( 'NONE',  ( -16.77431908686106610, 9.945805754529134290, -188.3358392176502036 ) ) ;
#108351 = CARTESIAN_POINT ( 'NONE',  ( 18.59999999999999076, 65.79142135624984178, -182.1731074845244223 ) ) ;
#108352 = CIRCLE ( 'NONE', #174465, 11.65000000000000036 ) ;
#108353 = DIRECTION ( 'NONE',  ( 0.000000000000000000, 0.2617529984165033463, 0.9651348961777157509 ) ) ;
#108354 = ORIENTED_EDGE ( 'NONE', *, *, #67476, .T. ) ;
#108355 = CARTESIAN_POINT ( 'NONE',  ( -16.87333278164153683, 66.11739021543377248, -190.3899396783708085 ) ) ;
#108356 = CARTESIAN_POINT ( 'NONE',  ( 0.000000000000000000, 0.000000000000000000, 0.000000000000000000 ) ) ;
#108357 = CARTESIAN_POINT ( 'NONE',  ( -21.45000000000000284, 7.708578643773852157, -146.2500000000000284 ) ) ;
#108358 = EDGE_CURVE ( 'NONE', #97478, #183016, #90298, .T. ) ;
#108359 = CARTESIAN_POINT ( 'NONE',  ( -18.59999999999999787, 22.19492904189240079, -246.0046379724989549 ) ) ;
#108360 = DIRECTION ( 'NONE',  ( 0.000000000000000000, 0.9651348961777157509, -0.2617529984165031243 ) ) ;
#108361 = ORIENTED_EDGE ( 'NONE', *, *, #16367, .F. ) ;
#108362 = CARTESIAN_POINT ( 'NONE',  ( -22.39999999999999858, 7.790779598384560245, -167.3999999999999773 ) ) ;
#108363 = CARTESIAN_POINT ( 'NONE',  ( 20.85000000000000142, 87.65000000001214175, -136.5231074845242745 ) ) ;
#108364 = ADVANCED_FACE ( 'NONE', ( #6949 ), #102167, .T. ) ;
#108365 = DIRECTION ( 'NONE',  ( 1.000000000000000000, 0.000000000000000000, 0.000000000000000000 ) ) ;
#108366 = ORIENTED_EDGE ( 'NONE', *, *, #27844, .F. ) ;
#108367 = ORIENTED_EDGE ( 'NONE', *, *, #117433, .F. ) ;
#108368 = ADVANCED_FACE ( 'NONE', ( #64370 ), #47346, .F. ) ;
#108369 = CARTESIAN_POINT ( 'NONE',  ( 22.49999999999999645, 75.90000000001172964, -81.17267829206913632 ) ) ;
#108370 = AXIS2_PLACEMENT_3D ( 'NONE', #66793, #126763, #64223 ) ;
#108371 = CARTESIAN_POINT ( 'NONE',  ( -18.50000000000000000, 11.75000000001115197, -155.3500000000000227 ) ) ;
#108372 = DIRECTION ( 'NONE',  ( 1.000000000000000000, 0.000000000000000000, 0.000000000000000000 ) ) ;
#108373 = CARTESIAN_POINT ( 'NONE',  ( -21.05000000000000071, 64.40000000001147384, -42.95131071479990936 ) ) ;
#108374 = DIRECTION ( 'NONE',  ( 0.000000000000000000, 0.9126074666063770380, 0.4088369013363282178 ) ) ;
#108375 = CIRCLE ( 'NONE', #25004, 0.5000000000000051070 ) ;
#108377 = DIRECTION ( 'NONE',  ( 0.000000000000000000, -0.9770955615653316162, -0.2128009952263604232 ) ) ;
#108376 = DIRECTION ( 'NONE',  ( 0.000000000000000000, -0.000000000000000000, -1.000000000000000000 ) ) ;
#108378 = EDGE_CURVE ( 'NONE', #5127, #155241, #206441, .T. ) ;
#108379 = CARTESIAN_POINT ( 'NONE',  ( -16.91256925476570672, 66.01426884188381905, -115.5554649955190882 ) ) ;
#108380 = CARTESIAN_POINT ( 'NONE',  ( -20.64999999999999858, 7.150000000011155876, -188.6499999999999488 ) ) ;
#108381 = AXIS2_PLACEMENT_3D ( 'NONE', #101548, #242370, #2469 ) ;
#108383 = ORIENTED_EDGE ( 'NONE', *, *, #29301, .T. ) ;
#108382 = DIRECTION ( 'NONE',  ( -0.000000000000000000, -6.982962677686266711E-15, 1.000000000000000000 ) ) ;
#108384 = CARTESIAN_POINT ( 'NONE',  ( -20.64999999999999858, 7.150000000011155876, -155.1500000000000057 ) ) ;
#108385 = DIRECTION ( 'NONE',  ( 0.000000000000000000, 0.000000000000000000, 1.000000000000000000 ) ) ;
#108387 = CARTESIAN_POINT ( 'NONE',  ( -20.94999999999999929, 1.115600667400684642E-11, -100.5000000000000426 ) ) ;
#108386 = LINE ( 'NONE', #210063, #101023 ) ;
#108388 = ORIENTED_EDGE ( 'NONE', *, *, #135039, .F. ) ;
#108389 = DIRECTION ( 'NONE',  ( 0.000000000000000000, -0.1350103645451945777, 0.9908441862701590219 ) ) ;
#108390 = DIRECTION ( 'NONE',  ( 0.000000000000000000, 0.9908441862701596881, 0.1350103645451904977 ) ) ;
#108391 = ADVANCED_FACE ( 'NONE', ( #151636 ), #188169, .F. ) ;
#108392 = FACE_OUTER_BOUND ( 'NONE', #168533, .T. ) ;
#108393 = FACE_OUTER_BOUND ( 'NONE', #205743, .T. ) ;
#108394 = CARTESIAN_POINT ( 'NONE',  ( -14.00000000000000178, 66.15000000001204228, -119.7731074845243739 ) ) ;
#108395 = ORIENTED_EDGE ( 'NONE', *, *, #225096, .T. ) ;
#108397 = EDGE_LOOP ( 'NONE', ( #92184, #47199, #134497, #31956 ) ) ;
#108396 = AXIS2_PLACEMENT_3D ( 'NONE', #188245, #5725, #50015 ) ;
#108398 = ADVANCED_FACE ( 'NONE', ( #229860 ), #51187, .F. ) ;
#108399 = AXIS2_PLACEMENT_3D ( 'NONE', #253816, #70091, #203801 ) ;
#108400 = LINE ( 'NONE', #208787, #217656 ) ;
#108401 = EDGE_LOOP ( 'NONE', ( #78683, #88436, #134524, #100232 ) ) ;
#108402 = CARTESIAN_POINT ( 'NONE',  ( -18.50000000000000000, 67.85909929089923764, -227.8797997985275856 ) ) ;
#108403 = VECTOR ( 'NONE', #125579, 1000.000000000000000 ) ;
#108404 = VERTEX_POINT ( 'NONE', #231168 ) ;
#108405 =( BOUNDED_CURVE ( )  B_SPLINE_CURVE ( 3, ( #84660, #44308, #100387, #22 ),
 .UNSPECIFIED., .F., .T. ) 
 B_SPLINE_CURVE_WITH_KNOTS ( ( 4, 4 ),
 ( 4.712388980384690562, 6.283185307179586232 ),
 .UNSPECIFIED. ) 
 CURVE ( )  GEOMETRIC_REPRESENTATION_ITEM ( )  RATIONAL_B_SPLINE_CURVE ( ( 1.000000000000000000, 0.8047378541243652705, 0.8047378541243652705, 1.000000000000000000 ) ) 
 REPRESENTATION_ITEM ( '' )  );
#108406 = CIRCLE ( 'NONE', #245767, 11.74999999999999645 ) ;
#108407 = FACE_OUTER_BOUND ( 'NONE', #95582, .T. ) ;
#108408 = CYLINDRICAL_SURFACE ( 'NONE', #185784, 0.1000000000000002554 ) ;
#108409 = FACE_OUTER_BOUND ( 'NONE', #122750, .T. ) ;
#108410 = ORIENTED_EDGE ( 'NONE', *, *, #207947, .F. ) ;
#108411 = CARTESIAN_POINT ( 'NONE',  ( 20.85000000000000142, -1.736705739456431807, -145.5174225876237699 ) ) ;
#108412 = CARTESIAN_POINT ( 'NONE',  ( -18.50596464788227635, 68.04082873524789932, -224.1991862745062178 ) ) ;
#108413 = CARTESIAN_POINT ( 'NONE',  ( -20.94999999999999929, 76.00000000001170974, -69.52310748452431710 ) ) ;
#108414 = DIRECTION ( 'NONE',  ( -0.000000000000000000, 1.000000000000000000, 2.891205793294679805E-16 ) ) ;
#108416 = AXIS2_PLACEMENT_3D ( 'NONE', #141598, #257633, #79032 ) ;
#108415 = DIRECTION ( 'NONE',  ( 1.000000000000000000, 0.000000000000000000, 0.000000000000000000 ) ) ;
#108417 = CIRCLE ( 'NONE', #254136, 11.74999999999999289 ) ;
#108418 = CARTESIAN_POINT ( 'NONE',  ( 21.12802099929860944, 11.18586598252357867, -211.0991417416504419 ) ) ;
#108419 = ORIENTED_EDGE ( 'NONE', *, *, #142174, .T. ) ;
#108421 = CARTESIAN_POINT ( 'NONE',  ( -23.25000000000000000, -11.64999999998884483, -130.9000000000000341 ) ) ;
#108420 = CARTESIAN_POINT ( 'NONE',  ( -16.90137573187934095, 66.05000000001210481, -123.7346900604274964 ) ) ;
#108422 = ORIENTED_EDGE ( 'NONE', *, *, #56948, .T. ) ;
#108424 = ORIENTED_EDGE ( 'NONE', *, *, #113262, .T. ) ;
#108423 = CARTESIAN_POINT ( 'NONE',  ( -23.15000000000000213, 1.115600667400684642E-11, -100.5000000000000284 ) ) ;
#108425 = ORIENTED_EDGE ( 'NONE', *, *, #219331, .T. ) ;
#108426 = CARTESIAN_POINT ( 'NONE',  ( -18.34374000495060386, 64.52683809664983983, -160.7731074845244450 ) ) ;
#108427 = CARTESIAN_POINT ( 'NONE',  ( 13.54577453029516398, 66.54939790392371890, -151.5792115214277942 ) ) ;
#108428 = DIRECTION ( 'NONE',  ( -0.000000000000000000, 0.2617529984165031243, 0.9651348961777157509 ) ) ;
#108429 = CARTESIAN_POINT ( 'NONE',  ( -22.24259225415828212, 59.97461308214577969, -233.9897012460487247 ) ) ;
#108430 = EDGE_LOOP ( 'NONE', ( #32645, #133459, #125616, #211150, #34815 ) ) ;
#108431 = FACE_OUTER_BOUND ( 'NONE', #116160, .T. ) ;
#108432 = DIRECTION ( 'NONE',  ( 0.000000000000000000, 0.000000000000000000, -1.000000000000000000 ) ) ;
#108433 = EDGE_LOOP ( 'NONE', ( #254824, #182582, #171171 ) ) ;
#108434 = CARTESIAN_POINT ( 'NONE',  ( -16.94389599337536012, 9.991197989767877985, -154.8923551982016420 ) ) ;
#108435 = AXIS2_PLACEMENT_3D ( 'NONE', #233525, #195692, #54848 ) ;
#108436 = EDGE_CURVE ( 'NONE', #8900, #78944, #185990, .T. ) ;
#108438 = CIRCLE ( 'NONE', #250263, 0.1000000000000028644 ) ;
#108437 = FACE_OUTER_BOUND ( 'NONE', #213665, .T. ) ;
#108439 = ORIENTED_EDGE ( 'NONE', *, *, #134347, .F. ) ;
#108440 = DIRECTION ( 'NONE',  ( -1.000000000000000000, 0.000000000000000000, 0.000000000000000000 ) ) ;
#108441 = ORIENTED_EDGE ( 'NONE', *, *, #167570, .T. ) ;
#108442 = CIRCLE ( 'NONE', #100211, 0.09999999999998898659 ) ;
#108443 = CARTESIAN_POINT ( 'NONE',  ( 18.54148534481893762, 65.67467670974414773, -97.45317318268841689 ) ) ;
#108444 = ORIENTED_EDGE ( 'NONE', *, *, #31748, .F. ) ;
#108445 = DIRECTION ( 'NONE',  ( 0.000000000000000000, 0.2617529984165032908, 0.9651348961777156399 ) ) ;
#108446 = EDGE_CURVE ( 'NONE', #53024, #253379, #249434, .T. ) ;
#108447 = CARTESIAN_POINT ( 'NONE',  ( -17.29158576265544056, 42.84089317668978936, -235.4244268507395645 ) ) ;
#108448 = DIRECTION ( 'NONE',  ( 0.000000000000000000, 0.000000000000000000, 1.000000000000000000 ) ) ;
#108449 = SHAPE_REPRESENTATION ( 'Injection Molded Chain Links 4', ( #2425 ), #119141 ) ;
#108450 = CARTESIAN_POINT ( 'NONE',  ( -21.53699400381544748, 6.632243066309741586, -199.5555681750817314 ) ) ;
#108452 = ADVANCED_FACE ( 'NONE', ( #211586 ), #91632, .T. ) ;
#108451 = CIRCLE ( 'NONE', #154296, 11.80000000000000071 ) ;
#108453 = CARTESIAN_POINT ( 'NONE',  ( 23.14999999999998437, 71.95000000001195417, -103.0231074845243455 ) ) ;
#108454 = CYLINDRICAL_SURFACE ( 'NONE', #30652, 0.09999999999998898659 ) ;
#108455 = VERTEX_POINT ( 'NONE', #32991 ) ;
#108456 = CARTESIAN_POINT ( 'NONE',  ( -11.60000000000000320, -11.65000000000000036, 17.70000000000000639 ) ) ;
#108457 = ORIENTED_EDGE ( 'NONE', *, *, #49953, .F. ) ;
#108459 = PLANE ( 'NONE',  #42085 ) ;
#108458 = CARTESIAN_POINT ( 'NONE',  ( -22.94999999999999929, 8.000000000000000000, -1.212568896937008089 ) ) ;
#108460 = ORIENTED_EDGE ( 'NONE', *, *, #17254, .F. ) ;
#108461 = CARTESIAN_POINT ( 'NONE',  ( -5.899999999999938183, 64.35000000001120668, -26.12310748452479103 ) ) ;
#108462 = DIRECTION ( 'NONE',  ( -1.000000000000000000, 0.000000000000000000, 0.000000000000000000 ) ) ;
#108463 = EDGE_CURVE ( 'NONE', #218126, #64641, #223570, .T. ) ;
#108464 = DIRECTION ( 'NONE',  ( 1.000000000000000000, 0.000000000000000000, 0.000000000000000000 ) ) ;
#108465 = EDGE_LOOP ( 'NONE', ( #181721, #229124, #153203, #147544, #98193 ) ) ;
#108467 = EDGE_LOOP ( 'NONE', ( #136690, #60377, #115117, #91155 ) ) ;
#108466 = CARTESIAN_POINT ( 'NONE',  ( 18.59999999999999076, 69.45000000001199680, -115.2731074845243455 ) ) ;
#108468 = EDGE_CURVE ( 'NONE', #221002, #42291, #12122, .T. ) ;
#108469 = PLANE ( 'NONE',  #29804 ) ;
#108471 = CARTESIAN_POINT ( 'NONE',  ( 18.49999999999998934, 15.26077403838592161, -222.9041953915167937 ) ) ;
#108470 = CARTESIAN_POINT ( 'NONE',  ( -18.40000000000000213, 51.02008725058737326, -230.6098793974720422 ) ) ;
#108473 = ORIENTED_EDGE ( 'NONE', *, *, #206539, .F. ) ;
#108472 = LINE ( 'NONE', #88886, #194668 ) ;
#108474 = ORIENTED_EDGE ( 'NONE', *, *, #87597, .T. ) ;
#108475 = AXIS2_PLACEMENT_3D ( 'NONE', #167481, #226112, #111340 ) ;
#108476 = DIRECTION ( 'NONE',  ( 0.000000000000000000, 1.000000000000000000, 0.000000000000000000 ) ) ;
#108477 = ORIENTED_EDGE ( 'NONE', *, *, #115220, .F. ) ;
#108478 = CARTESIAN_POINT ( 'NONE',  ( -23.49999999999994316, 87.50449464844290048, -34.18759587077607165 ) ) ;
#108479 = ADVANCED_FACE ( 'NONE', ( #227282 ), #136078, .T. ) ;
#108480 = VERTEX_POINT ( 'NONE', #210307 ) ;
#108481 = AXIS2_PLACEMENT_3D ( 'NONE', #242997, #224711, #124351 ) ;
#108482 = DIRECTION ( 'NONE',  ( 0.000000000000000000, 0.000000000000000000, 1.000000000000000000 ) ) ;
#108483 = DIRECTION ( 'NONE',  ( -0.000000000000000000, 0.4721928772777345684, 0.8814952561688429444 ) ) ;
#108484 = VERTEX_POINT ( 'NONE', #13388 ) ;
#108485 = DIRECTION ( 'NONE',  ( 0.000000000000000000, 0.9126074666063774821, 0.4088369013363270521 ) ) ;
#108486 = ADVANCED_FACE ( 'NONE', ( #68216 ), #251984, .T. ) ;
#108487 = ORIENTED_EDGE ( 'NONE', *, *, #239867, .T. ) ;
#108488 = AXIS2_PLACEMENT_3D ( 'NONE', #134043, #55763, #214872 ) ;
#108489 = CARTESIAN_POINT ( 'NONE',  ( 21.13498764882293557, 6.346487175175731466, -199.6161075385196852 ) ) ;
#108490 = AXIS2_PLACEMENT_3D ( 'NONE', #252414, #116771, #133762 ) ;
#108491 = ORIENTED_EDGE ( 'NONE', *, *, #58742, .F. ) ;
#108492 = ORIENTED_EDGE ( 'NONE', *, *, #185338, .T. ) ;
#108493 = CARTESIAN_POINT ( 'NONE',  ( -21.07954640115303135, 61.10538041441509449, -234.2621228157806001 ) ) ;
#108494 = AXIS2_PLACEMENT_3D ( 'NONE', #56357, #216730, #77214 ) ;
#108495 = VERTEX_POINT ( 'NONE', #167343 ) ;
#108496 = CARTESIAN_POINT ( 'NONE',  ( -16.84421487269769102, 9.950000000011137047, -46.16950212244496043 ) ) ;
#108497 = EDGE_LOOP ( 'NONE', ( #100757, #7271, #7757, #203973 ) ) ;
#108499 = VERTEX_POINT ( 'NONE', #90330 ) ;
#108498 = DIRECTION ( 'NONE',  ( 1.000000000000000000, 0.000000000000000000, 0.000000000000000000 ) ) ;
#108500 = CARTESIAN_POINT ( 'NONE',  ( 18.39999999999999503, 11.75000000001113953, -57.75000000000000711 ) ) ;
#108501 = ORIENTED_EDGE ( 'NONE', *, *, #103165, .T. ) ;
#108502 = CARTESIAN_POINT ( 'NONE',  ( 23.25000000000000000, -11.64999999998884483, -134.0000000000000000 ) ) ;
#108503 = VERTEX_POINT ( 'NONE', #49929 ) ;
#108506 = VERTEX_POINT ( 'NONE', #152922 ) ;
#108505 = ORIENTED_EDGE ( 'NONE', *, *, #219723, .T. ) ;
#108504 = DIRECTION ( 'NONE',  ( 0.000000000000000000, 5.329070518200764016E-15, -1.000000000000000000 ) ) ;
#108507 = CARTESIAN_POINT ( 'NONE',  ( -18.59999999999999787, 76.00000000001239187, -162.1231074845243825 ) ) ;
#108508 = DIRECTION ( 'NONE',  ( 2.952720810173289112E-16, -1.000000000000000000, -0.000000000000000000 ) ) ;
#108509 = ORIENTED_EDGE ( 'NONE', *, *, #180539, .F. ) ;
#108510 = TOROIDAL_SURFACE ( 'NONE', #70950, 11.90000000000000391, 0.1000000000000000056 ) ;
#108511 = VECTOR ( 'NONE', #209678, 1000.000000000000000 ) ;
#108512 = CIRCLE ( 'NONE', #37813, 1.900000000000000799 ) ;
#108513 = TOROIDAL_SURFACE ( 'NONE', #112797, 0.2000000000000000111, 0.1000000000000000056 ) ;
#108514 = EDGE_CURVE ( 'NONE', #33376, #158009, #87759, .T. ) ;
#108515 = EDGE_CURVE ( 'NONE', #135260, #124226, #127751, .T. ) ;
#108516 = ORIENTED_EDGE ( 'NONE', *, *, #111742, .F. ) ;
#108517 = CARTESIAN_POINT ( 'NONE',  ( -21.05000000000000071, 69.52192177891770086, -203.4231075492199352 ) ) ;
#108518 = FACE_OUTER_BOUND ( 'NONE', #241567, .T. ) ;
#108520 = ORIENTED_EDGE ( 'NONE', *, *, #14360, .F. ) ;
#108519 = CYLINDRICAL_SURFACE ( 'NONE', #240642, 2.000000000000001776 ) ;
#108521 = CARTESIAN_POINT ( 'NONE',  ( -23.25000000000000000, 1.148907358139439339E-11, -201.0000000000015064 ) ) ;
#108522 = ORIENTED_EDGE ( 'NONE', *, *, #151628, .T. ) ;
#108523 = EDGE_CURVE ( 'NONE', #102291, #75479, #133331, .T. ) ;
#108525 = EDGE_CURVE ( 'NONE', #133332, #39283, #215224, .T. ) ;
#108524 = DIRECTION ( 'NONE',  ( 0.000000000000000000, -1.000000000000000000, 0.000000000000000000 ) ) ;
#108526 = DIRECTION ( 'NONE',  ( 0.000000000000000000, 0.9876197685951252359, -0.1568667991644863424 ) ) ;
#108527 = ORIENTED_EDGE ( 'NONE', *, *, #108468, .T. ) ;
#108528 = CARTESIAN_POINT ( 'NONE',  ( 20.94999999999999574, 6.400000000011158541, -177.4304246300615375 ) ) ;
#108529 = AXIS2_PLACEMENT_3D ( 'NONE', #187775, #21331, #27444 ) ;
#108530 = DIRECTION ( 'NONE',  ( 0.000000000000000000, 0.000000000000000000, -1.000000000000000000 ) ) ;
#108531 = EDGE_CURVE ( 'NONE', #3198, #20715, #248134, .T. ) ;
#108532 = ORIENTED_EDGE ( 'NONE', *, *, #66330, .F. ) ;
#108534 = ORIENTED_EDGE ( 'NONE', *, *, #140601, .F. ) ;
#108533 = CARTESIAN_POINT ( 'NONE',  ( 23.24999999999999645, 70.40000000001276703, -215.2731074845243882 ) ) ;
#108536 = ADVANCED_FACE ( 'NONE', ( #149058 ), #109892, .T. ) ;
#108535 = DIRECTION ( 'NONE',  ( 0.000000000000000000, -7.086529944415894657E-15, 1.000000000000000000 ) ) ;
#108538 = EDGE_CURVE ( 'NONE', #165339, #157651, #248528, .T. ) ;
#108537 = EDGE_CURVE ( 'NONE', #122271, #14565, #132012, .T. ) ;
#108540 = ORIENTED_EDGE ( 'NONE', *, *, #32133, .F. ) ;
#108539 = ORIENTED_EDGE ( 'NONE', *, *, #172828, .T. ) ;
#108541 = ORIENTED_EDGE ( 'NONE', *, *, #237600, .T. ) ;
#108542 = DIRECTION ( 'NONE',  ( 1.000000000000000000, 0.000000000000000000, 0.000000000000000000 ) ) ;
#108543 = ORIENTED_EDGE ( 'NONE', *, *, #67104, .T. ) ;
#108544 = FACE_OUTER_BOUND ( 'NONE', #202165, .T. ) ;
#108545 = ORIENTED_EDGE ( 'NONE', *, *, #11489, .T. ) ;
#108546 = DIRECTION ( 'NONE',  ( 0.7071067811865487940, 0.000000000000000000, -0.7071067811865463515 ) ) ;
#108547 = DIRECTION ( 'NONE',  ( -1.000000000000000000, 0.000000000000000000, 0.000000000000000000 ) ) ;
#108548 = AXIS2_PLACEMENT_3D ( 'NONE', #154082, #134445, #36690 ) ;
#108549 = ORIENTED_EDGE ( 'NONE', *, *, #46958, .T. ) ;
#108550 = EDGE_CURVE ( 'NONE', #197017, #51917, #3764, .T. ) ;
#108551 = CIRCLE ( 'NONE', #162556, 0.2000000000000057288 ) ;
#108552 = EDGE_LOOP ( 'NONE', ( #233632, #58499 ) ) ;
#108553 = EDGE_CURVE ( 'NONE', #155438, #186897, #185158, .T. ) ;
#108554 = EDGE_CURVE ( 'NONE', #102565, #55232, #161252, .T. ) ;
#108555 = ORIENTED_EDGE ( 'NONE', *, *, #42418, .T. ) ;
#108556 = CIRCLE ( 'NONE', #254282, 0.1000000000000124678 ) ;
#108557 = ADVANCED_FACE ( 'NONE', ( #63733 ), #241114, .F. ) ;
#108558 = VECTOR ( 'NONE', #253884, 1000.000000000000000 ) ;
#108559 = DIRECTION ( 'NONE',  ( 0.000000000000000000, 0.000000000000000000, -1.000000000000000000 ) ) ;
#108560 = VERTEX_POINT ( 'NONE', #100270 ) ;
#108561 = FACE_OUTER_BOUND ( 'NONE', #249468, .T. ) ;
#108563 = ORIENTED_EDGE ( 'NONE', *, *, #53876, .T. ) ;
#108562 = CARTESIAN_POINT ( 'NONE',  ( 21.14999999999999858, 10.71339244341104013, -179.8499999999999943 ) ) ;
#108564 = CARTESIAN_POINT ( 'NONE',  ( 20.94999999999999929, 76.00000000001190870, -103.0231074845243029 ) ) ;
#108565 = CARTESIAN_POINT ( 'NONE',  ( -16.27683809663750480, 63.69098859062252416, -213.1881598963609576 ) ) ;
#108566 = ADVANCED_FACE ( 'NONE', ( #58582 ), #14694, .T. ) ;
#108567 = DIRECTION ( 'NONE',  ( 0.000000000000000000, 0.000000000000000000, 1.000000000000000000 ) ) ;
#108568 = DIRECTION ( 'NONE',  ( 0.000000000000000000, 6.982962677686266711E-15, -1.000000000000000000 ) ) ;
#108569 = CARTESIAN_POINT ( 'NONE',  ( -16.87383368123029825, 66.05000000001230376, -157.3731074845244393 ) ) ;
#108571 = DIRECTION ( 'NONE',  ( 0.000000000000000000, 0.000000000000000000, -1.000000000000000000 ) ) ;
#108570 = DIRECTION ( 'NONE',  ( -1.000000000000000000, 1.772924042024179943E-16, -4.808324575169860901E-17 ) ) ;
#108572 = DIRECTION ( 'NONE',  ( 1.000000000000000000, 0.000000000000000000, 0.000000000000000000 ) ) ;
#108573 = DIRECTION ( 'NONE',  ( 0.000000000000000000, 0.2617529984165035128, 0.9651348961777155289 ) ) ;
#108574 = LINE ( 'NONE', #12068, #22292 ) ;
#108575 = VECTOR ( 'NONE', #234656, 1000.000000000000227 ) ;
#108576 = VERTEX_POINT ( 'NONE', #220261 ) ;
#108577 = AXIS2_PLACEMENT_3D ( 'NONE', #80347, #59497, #200331 ) ;
#108578 = AXIS2_PLACEMENT_3D ( 'NONE', #154759, #109169, #233012 ) ;
#108579 = ORIENTED_EDGE ( 'NONE', *, *, #113984, .F. ) ;
#108581 = ORIENTED_EDGE ( 'NONE', *, *, #124467, .F. ) ;
#108580 = DIRECTION ( 'NONE',  ( 0.000000000000000000, -0.9908441862701605762, -0.1350103645451835310 ) ) ;
#108582 = VERTEX_POINT ( 'NONE', #139401 ) ;
#108583 = CYLINDRICAL_SURFACE ( 'NONE', #224163, 0.1000000000000028644 ) ;
#108584 = DIRECTION ( 'NONE',  ( 0.000000000000000000, -1.000000000000000000, -6.982962677686265922E-15 ) ) ;
#108585 = CARTESIAN_POINT ( 'NONE',  ( 23.14999999999999858, 67.23127455305835554, -235.8551265064784559 ) ) ;
#108586 = ORIENTED_EDGE ( 'NONE', *, *, #8106, .F. ) ;
#108587 = ORIENTED_EDGE ( 'NONE', *, *, #5710, .T. ) ;
#108588 = PRESENTATION_STYLE_ASSIGNMENT (( #46036 ) ) ;
#108589 = CARTESIAN_POINT ( 'NONE',  ( 18.43579564894474387, -9.519327535281304264, -40.47297664386042726 ) ) ;
#108590 = CIRCLE ( 'NONE', #175270, 0.09999999999999954758 ) ;
#108591 = CARTESIAN_POINT ( 'NONE',  ( -18.59999999999999787, 11.65000000001115232, -188.7499999999999716 ) ) ;
#108592 = ORIENTED_EDGE ( 'NONE', *, *, #136699, .F. ) ;
#108593 = CARTESIAN_POINT ( 'NONE',  ( 18.54999999999999716, 66.05000000001180638, -82.17310748452433700 ) ) ;
#108594 = CARTESIAN_POINT ( 'NONE',  ( 20.94999999999999929, 8.776282895303632259, -121.7500000000000426 ) ) ;
#108595 = DIRECTION ( 'NONE',  ( 1.000000000000000000, -0.000000000000000000, -0.000000000000000000 ) ) ;
#108596 = DIRECTION ( 'NONE',  ( 0.000000000000000000, -0.2128009952263601734, 0.9770955615653315052 ) ) ;
#108598 = ORIENTED_EDGE ( 'NONE', *, *, #117958, .T. ) ;
#108597 = DIRECTION ( 'NONE',  ( 0.000000000000000000, 0.000000000000000000, 1.000000000000000000 ) ) ;
#108599 = CARTESIAN_POINT ( 'NONE',  ( 18.57071067811864040, 65.82071067813119214, -182.2731074845244450 ) ) ;
#108600 = DIRECTION ( 'NONE',  ( 0.000000000000000000, -0.9908441862701420355, -0.1350103645453197554 ) ) ;
#108601 = CARTESIAN_POINT ( 'NONE',  ( -23.15000000000000213, 1.115600667400684642E-11, -134.0000000000000284 ) ) ;
#108602 = DIRECTION ( 'NONE',  ( -1.000000000000000000, -1.794895427898103559E-16, -3.909090864890002444E-17 ) ) ;
#108603 = ORIENTED_EDGE ( 'NONE', *, *, #210341, .T. ) ;
#108604 = LINE ( 'NONE', #250675, #173744 ) ;
#108605 = DIRECTION ( 'NONE',  ( 0.000000000000000000, -1.000000000000000000, 0.000000000000000000 ) ) ;
#108606 = TOROIDAL_SURFACE ( 'NONE', #175285, 0.2000000000000000111, 0.1000000000000000056 ) ;
#108607 = EDGE_CURVE ( 'NONE', #167773, #11322, #144659, .T. ) ;
#108610 = CYLINDRICAL_SURFACE ( 'NONE', #124527, 0.09999999999999939493 ) ;
#108609 = CIRCLE ( 'NONE', #62817, 0.09999999999999967248 ) ;
#108608 = DIRECTION ( 'NONE',  ( 0.000000000000000000, -1.000000000000000000, 0.000000000000000000 ) ) ;
#108611 = DIRECTION ( 'NONE',  ( 1.000000000000000000, 0.000000000000000000, 0.000000000000000000 ) ) ;
#108612 = DIRECTION ( 'NONE',  ( 0.000000000000000000, 0.9915357197604971473, -0.1298341882519111479 ) ) ;
#108613 = VECTOR ( 'NONE', #133353, 1000.000000000000000 ) ;
#108614 = LINE ( 'NONE', #9505, #16588 ) ;
#108615 = DIRECTION ( 'NONE',  ( 0.000000000000000000, 0.000000000000000000, -1.000000000000000000 ) ) ;
#108617 = ADVANCED_FACE ( 'NONE', ( #201973 ), #78149, .F. ) ;
#108616 = CARTESIAN_POINT ( 'NONE',  ( 23.24999999999999645, 61.13752757784637026, -224.6182967272386009 ) ) ;
#108618 = CARTESIAN_POINT ( 'NONE',  ( 18.59999999999999076, 65.79142135624984178, -182.1731074845244223 ) ) ;
#108619 = EDGE_LOOP ( 'NONE', ( #74684, #139586, #28856, #78684 ) ) ;
#108620 = TOROIDAL_SURFACE ( 'NONE', #254344, 0.2000000000000000111, 0.1000000000000000056 ) ;
#108621 = EDGE_LOOP ( 'NONE', ( #169595, #7891, #158712, #19926 ) ) ;
#108622 = EDGE_LOOP ( 'NONE', ( #204019, #245123, #74591, #65932 ) ) ;
#108623 = EDGE_CURVE ( 'NONE', #109264, #62684, #252805, .T. ) ;
#108624 = DIRECTION ( 'NONE',  ( -1.000000000000000000, 0.000000000000000000, 0.000000000000000000 ) ) ;
#108625 = EDGE_CURVE ( 'NONE', #169627, #26411, #48800, .T. ) ;
#108626 = CARTESIAN_POINT ( 'NONE',  ( -21.05000000000000071, 76.00000000001210765, -133.6231074845243256 ) ) ;
#108627 = ORIENTED_EDGE ( 'NONE', *, *, #14115, .T. ) ;
#108628 = TOROIDAL_SURFACE ( 'NONE', #62843, 11.89999999999999858, 0.1000000000000000056 ) ;
#108629 = VERTEX_POINT ( 'NONE', #237245 ) ;
#108630 = ORIENTED_EDGE ( 'NONE', *, *, #103004, .T. ) ;
#108631 = CARTESIAN_POINT ( 'NONE',  ( 21.04999999999987992, 76.01759718701998736, -109.4638783781862656 ) ) ;
#108632 = EDGE_LOOP ( 'NONE', ( #80, #250536, #130346, #178658 ) ) ;
#108633 = ADVANCED_FACE ( 'NONE', ( #98977 ), #236245, .F. ) ;
#108634 = CARTESIAN_POINT ( 'NONE',  ( 13.40000000000005898, 64.35000000001120668, -18.42310748452479530 ) ) ;
#108635 = CARTESIAN_POINT ( 'NONE',  ( -16.78805706634180339, 66.05174750694062880, -82.17895427649251872 ) ) ;
#108636 = EDGE_CURVE ( 'NONE', #161055, #203545, #27996, .T. ) ;
#108637 = DIRECTION ( 'NONE',  ( 0.000000000000000000, -0.4999999999999689138, 0.8660254037844565822 ) ) ;
#108638 = DIRECTION ( 'NONE',  ( 0.7071359030028288029, 0.000000000000000000, 0.7070776581708504427 ) ) ;
#108639 = CARTESIAN_POINT ( 'NONE',  ( -16.97683809663752896, 29.65845354706183201, -234.5135633587022426 ) ) ;
#108640 = CARTESIAN_POINT ( 'NONE',  ( 20.94999999999999929, 74.16465844978745281, -91.46795619196133487 ) ) ;
#108642 = ORIENTED_EDGE ( 'NONE', *, *, #195691, .T. ) ;
#108641 = DIRECTION ( 'NONE',  ( 1.000000000000000000, 0.000000000000000000, 0.000000000000000000 ) ) ;
#108644 = DIRECTION ( 'NONE',  ( -0.000000000000000000, 1.000000000000000000, 6.982962677686266711E-15 ) ) ;
#108643 = FACE_BOUND ( 'NONE', #1102, .T. ) ;
#108646 = LINE ( 'NONE', #61519, #136021 ) ;
#108645 = AXIS2_PLACEMENT_3D ( 'NONE', #42304, #103540, #100934 ) ;
#108647 = ORIENTED_EDGE ( 'NONE', *, *, #85586, .T. ) ;
#108648 = DIRECTION ( 'NONE',  ( 1.000000000000000000, -0.000000000000000000, -0.000000000000000000 ) ) ;
#108649 = DIRECTION ( 'NONE',  ( 0.000000000000000000, -0.8660254037844468122, -0.4999999999999859557 ) ) ;
#108650 = DIRECTION ( 'NONE',  ( 0.000000000000000000, 1.000000000000000000, 3.469446951953515108E-14 ) ) ;
#108651 = EDGE_LOOP ( 'NONE', ( #94041, #159866, #178187, #236872 ) ) ;
#108652 = CARTESIAN_POINT ( 'NONE',  ( 18.59999999999999076, 77.83585931145600512, -158.4186683157258244 ) ) ;
#108653 = ADVANCED_FACE ( 'NONE', ( #119888 ), #193373, .T. ) ;
#108654 = VECTOR ( 'NONE', #107170, 1000.000000000000000 ) ;
#108655 = DIRECTION ( 'NONE',  ( 0.000000000000000000, 1.000000000000000000, 0.000000000000000000 ) ) ;
#108656 = EDGE_CURVE ( 'NONE', #191930, #190621, #190490, .T. ) ;
#108657 = ORIENTED_EDGE ( 'NONE', *, *, #255365, .F. ) ;
#108658 = DIRECTION ( 'NONE',  ( 0.000000000000000000, 0.000000000000000000, -1.000000000000000000 ) ) ;
#108659 = DIRECTION ( 'NONE',  ( 0.000000000000000000, 0.000000000000000000, 1.000000000000000000 ) ) ;
#108661 = DIRECTION ( 'NONE',  ( -0.000000000000000000, 0.2617529984165031243, 0.9651348961777157509 ) ) ;
#108660 = TOROIDAL_SURFACE ( 'NONE', #87789, 7.791421356237316687, 0.1000000000000000056 ) ;
#108662 = CARTESIAN_POINT ( 'NONE',  ( 18.59999999999999076, 15.22030141505243961, -222.9130098973476777 ) ) ;
#108663 = ORIENTED_EDGE ( 'NONE', *, *, #255178, .T. ) ;
#108664 = ORIENTED_EDGE ( 'NONE', *, *, #188289, .T. ) ;
#108665 = EDGE_CURVE ( 'NONE', #208340, #195188, #183697, .T. ) ;
#108666 = ADVANCED_FACE ( 'NONE', ( #66311 ), #87136, .F. ) ;
#108667 = LINE ( 'NONE', #192076, #65160 ) ;
#108668 = DIRECTION ( 'NONE',  ( 1.000000000000000000, 0.000000000000000000, -0.000000000000000000 ) ) ;
#108669 = CARTESIAN_POINT ( 'NONE',  ( 20.95512820512820440, 65.37615131630012399, -115.2731074845243739 ) ) ;
#108670 = DIRECTION ( 'NONE',  ( 0.000000000000000000, 0.000000000000000000, -1.000000000000000000 ) ) ;
#108671 = DIRECTION ( 'NONE',  ( 0.000000000000000000, 0.000000000000000000, -1.000000000000000000 ) ) ;
#108673 = EDGE_CURVE ( 'NONE', #13347, #78551, #145827, .T. ) ;
#108672 = CIRCLE ( 'NONE', #192082, 0.5000000000000022204 ) ;
#108674 = CYLINDRICAL_SURFACE ( 'NONE', #57628, 0.09999999999999939493 ) ;
#108675 = PLANE ( 'NONE',  #35752 ) ;
#108677 = DIRECTION ( 'NONE',  ( -0.7071067811865388020, 0.7071067811865561215, 0.000000000000000000 ) ) ;
#108676 = AXIS2_PLACEMENT_3D ( 'NONE', #37924, #178732, #77015 ) ;
#108678 = ORIENTED_EDGE ( 'NONE', *, *, #154865, .F. ) ;
#108679 = CARTESIAN_POINT ( 'NONE',  ( -20.89192007715127986, 65.67101464000501210, -97.44043916224792667 ) ) ;
#108680 = AXIS2_PLACEMENT_3D ( 'NONE', #48460, #184116, #144983 ) ;
#108682 = EDGE_LOOP ( 'NONE', ( #13678, #233125, #102780, #121100 ) ) ;
#108681 = CARTESIAN_POINT ( 'NONE',  ( 21.10710606213542206, 8.776894023904366904, -179.7409965263994138 ) ) ;
#108683 = DIRECTION ( 'NONE',  ( 0.000000000000000000, 0.000000000000000000, -1.000000000000000000 ) ) ;
#108684 = DIRECTION ( 'NONE',  ( 1.836970198721029934E-16, -1.000000000000000000, -0.000000000000000000 ) ) ;
#108685 = DIRECTION ( 'NONE',  ( -1.000000000000000000, -0.000000000000000000, -0.000000000000000000 ) ) ;
#108686 = DIRECTION ( 'NONE',  ( 1.000000000000000000, 0.000000000000000000, 0.000000000000000000 ) ) ;
#108687 = FACE_OUTER_BOUND ( 'NONE', #143618, .T. ) ;
#108689 = ORIENTED_EDGE ( 'NONE', *, *, #185164, .F. ) ;
#108688 = CARTESIAN_POINT ( 'NONE',  ( -22.10000000000000497, 6.223900101154156594, 12.00000000000000000 ) ) ;
#108690 = SPHERICAL_SURFACE ( 'NONE', #209119, 0.1000000000000000056 ) ;
#108691 = CARTESIAN_POINT ( 'NONE',  ( -18.58222699835055280, 65.66799936921584901, -164.4299399888601272 ) ) ;
#108692 = AXIS2_PLACEMENT_3D ( 'NONE', #144889, #163198, #86186 ) ;
#108693 = EDGE_CURVE ( 'NONE', #100962, #119332, #222793, .T. ) ;
#108694 = LINE ( 'NONE', #129550, #172003 ) ;
#108695 = DIRECTION ( 'NONE',  ( 0.000000000000000000, 0.9673461469267252699, -0.2534589355813257061 ) ) ;
#108696 = CIRCLE ( 'NONE', #171096, 7.800000000000001599 ) ;
#108697 = ORIENTED_EDGE ( 'NONE', *, *, #161702, .F. ) ;
#108698 = FACE_OUTER_BOUND ( 'NONE', #216692, .T. ) ;
#108699 = ORIENTED_EDGE ( 'NONE', *, *, #242190, .T. ) ;
#108700 = EDGE_CURVE ( 'NONE', #170795, #43436, #173766, .T. ) ;
#108701 = CARTESIAN_POINT ( 'NONE',  ( -23.15000000000000213, 74.00000000001156764, -56.29848556176223440 ) ) ;
#108702 = ORIENTED_EDGE ( 'NONE', *, *, #141937, .T. ) ;
#108704 = CARTESIAN_POINT ( 'NONE',  ( 18.52928932188133970, 10.27928932189250411, -88.35000000000003695 ) ) ;
#108703 = AXIS2_PLACEMENT_3D ( 'NONE', #227643, #129826, #114113 ) ;
#108705 = AXIS2_PLACEMENT_3D ( 'NONE', #34096, #152754, #148881 ) ;
#108706 = CIRCLE ( 'NONE', #146287, 0.09999999999999939493 ) ;
#108707 = ORIENTED_EDGE ( 'NONE', *, *, #158958, .T. ) ;
#108708 = AXIS2_PLACEMENT_3D ( 'NONE', #189782, #69855, #47680 ) ;
#108709 = AXIS2_PLACEMENT_3D ( 'NONE', #110629, #231885, #188887 ) ;
#108710 = CARTESIAN_POINT ( 'NONE',  ( 18.69999999999999929, -10.64999999999999325, 31.59999999999999787 ) ) ;
#108711 = FACE_OUTER_BOUND ( 'NONE', #27335, .T. ) ;
#108712 = EDGE_CURVE ( 'NONE', #86349, #158859, #119563, .T. ) ;
#108713 = PLANE ( 'NONE',  #10171 ) ;
#108714 = ORIENTED_EDGE ( 'NONE', *, *, #3047, .F. ) ;
#108715 = FACE_OUTER_BOUND ( 'NONE', #138886, .T. ) ;
#108716 = VECTOR ( 'NONE', #38970, 1000.000000000000000 ) ;
#108717 = CARTESIAN_POINT ( 'NONE',  ( 21.06089410995820899, 13.07631742462289282, -210.6405384895012958 ) ) ;
#108718 = CARTESIAN_POINT ( 'NONE',  ( 15.07585980824112859, 9.417632963106287391, -18.14894846573225706 ) ) ;
#108719 = DIRECTION ( 'NONE',  ( -1.000000000000000000, -0.000000000000000000, -0.000000000000000000 ) ) ;
#108720 = CARTESIAN_POINT ( 'NONE',  ( -20.64999999999999858, 4.350000000011156054, -88.15000000000004832 ) ) ;
#108721 = ORIENTED_EDGE ( 'NONE', *, *, #132664, .F. ) ;
#108723 = VERTEX_POINT ( 'NONE', #123721 ) ;
#108722 = DIRECTION ( 'NONE',  ( 0.000000000000000000, -1.000000000000000000, -6.982962677686266711E-15 ) ) ;
#108724 = ORIENTED_EDGE ( 'NONE', *, *, #14382, .T. ) ;
#108725 = FACE_OUTER_BOUND ( 'NONE', #97560, .T. ) ;
#108726 = ORIENTED_EDGE ( 'NONE', *, *, #137615, .T. ) ;
#108727 = DIRECTION ( 'NONE',  ( 1.000000000000000000, 0.000000000000000000, 0.000000000000000000 ) ) ;
#108728 = FACE_OUTER_BOUND ( 'NONE', #198447, .T. ) ;
#108729 = PLANE ( 'NONE',  #95744 ) ;
#108730 = EDGE_LOOP ( 'NONE', ( #240037, #143730, #1168, #14931 ) ) ;
#108731 = DIRECTION ( 'NONE',  ( 1.000000000000000000, 0.000000000000000000, 0.000000000000000000 ) ) ;
#108732 = DIRECTION ( 'NONE',  ( 0.000000000000000000, 0.8814952561688476074, -0.4721928772777262417 ) ) ;
#108733 = CARTESIAN_POINT ( 'NONE',  ( -23.25000000000000000, -1.164121893230052995, -74.91484808557160591 ) ) ;
#108735 = ORIENTED_EDGE ( 'NONE', *, *, #204584, .T. ) ;
#108734 = TOROIDAL_SURFACE ( 'NONE', #250385, 0.2000000000000000111, 0.1000000000000000056 ) ;
#108736 = LINE ( 'NONE', #106146, #133280 ) ;
#108738 = ORIENTED_EDGE ( 'NONE', *, *, #51891, .F. ) ;
#108737 = CARTESIAN_POINT ( 'NONE',  ( 13.99999999999999822, 66.15000000001204228, -119.7731074845243739 ) ) ;
#108739 = DIRECTION ( 'NONE',  ( -1.020425574104004196E-15, 0.000000000000000000, -1.000000000000000000 ) ) ;
#108740 = B_SPLINE_CURVE_WITH_KNOTS ( 'NONE', 3,
 ( #31331, #132977, #95117, #211212, #130381, #170861, #190388, #33914, #30037, #74307 ),
 .UNSPECIFIED., .F., .F.,
 ( 4, 2, 2, 2, 4 ),
 ( 0.000000000000000000, 3.990160268013856579E-05, 7.980320536027713158E-05, 0.0001596064107205558895, 0.0003192128214411109116 ),
 .UNSPECIFIED. ) ;
#108741 = DIRECTION ( 'NONE',  ( -1.000000000000000000, -0.000000000000000000, 0.000000000000000000 ) ) ;
#108742 = ORIENTED_EDGE ( 'NONE', *, *, #52617, .F. ) ;
#108743 = CARTESIAN_POINT ( 'NONE',  ( -21.05000000000000071, 1.115653327213047955E-11, -163.2000000000000171 ) ) ;
#108744 = FACE_OUTER_BOUND ( 'NONE', #56161, .T. ) ;
#108745 = VECTOR ( 'NONE', #45117, 1000.000000000000000 ) ;
#108746 = DIRECTION ( 'NONE',  ( 0.000000000000000000, -0.9770955615653316162, -0.2128009952263604232 ) ) ;
#108747 = VERTEX_POINT ( 'NONE', #205812 ) ;
#108748 = CARTESIAN_POINT ( 'NONE',  ( 21.05000000000005400, 64.35000000001119247, -6.023107484524794941 ) ) ;
#108749 = ADVANCED_FACE ( 'NONE', ( #203246 ), #194587, .T. ) ;
#108750 = CARTESIAN_POINT ( 'NONE',  ( -22.50000000000092371, -2.401771312553021342, -189.4980873520049443 ) ) ;
#108751 = EDGE_CURVE ( 'NONE', #139562, #231379, #136256, .T. ) ;
#108752 = VERTEX_POINT ( 'NONE', #28512 ) ;
#108753 = ADVANCED_FACE ( 'NONE', ( #49306, #109267 ), #144543, .T. ) ;
#108754 = TOROIDAL_SURFACE ( 'NONE', #121277, 7.800000000000000711, 0.1000000000000000056 ) ;
#108755 = AXIS2_PLACEMENT_3D ( 'NONE', #772, #99872, #221123 ) ;
#108757 = ORIENTED_EDGE ( 'NONE', *, *, #58711, .F. ) ;
#108756 = AXIS2_PLACEMENT_3D ( 'NONE', #208943, #207676, #29063 ) ;
#108758 = CARTESIAN_POINT ( 'NONE',  ( 21.30740335185486245, 69.44334207798469549, -203.6220420103002766 ) ) ;
#108759 = ORIENTED_EDGE ( 'NONE', *, *, #149604, .F. ) ;
#108760 = CARTESIAN_POINT ( 'NONE',  ( -22.39999999999999858, 11.36188319272496727, -198.4231588494578773 ) ) ;
#108761 = ADVANCED_FACE ( 'NONE', ( #184970 ), #165416, .T. ) ;
#108762 = CARTESIAN_POINT ( 'NONE',  ( 18.49999999999999289, 65.79142135624934440, -114.7731074845243739 ) ) ;
#108765 = ORIENTED_EDGE ( 'NONE', *, *, #34464, .T. ) ;
#108764 = CARTESIAN_POINT ( 'NONE',  ( 14.56326696814970845, 24.89049957252425216, -232.5305204729232571 ) ) ;
#108763 =( BOUNDED_SURFACE ( )  B_SPLINE_SURFACE ( 3, 2, ( 
 ( #257771, #96168, #54486 ),
 ( #136579, #174501, #117038 ),
 ( #94891, #216122, #214843 ),
 ( #252678, #218681, #119618 ),
 ( #134020, #157482, #75370 ),
 ( #173210, #40099, #37513 ) ),
 .UNSPECIFIED., .F., .F., .F. ) 
 B_SPLINE_SURFACE_WITH_KNOTS ( ( 4, 2, 4 ),
 ( 3, 3 ),
 ( 1.570796326794895448, 2.356194490192343505, 3.141592653589791784 ),
 ( 0.000000000000000000, 1.000000000000000000 ),
 .UNSPECIFIED. ) 
 GEOMETRIC_REPRESENTATION_ITEM ( )  RATIONAL_B_SPLINE_SURFACE ( (
 ( 1.000000000000000000, 0.7071067811865355823, 1.000000000000000000),
 ( 1.000000000000000000, 0.6611148371776521815, 1.000000000000000000),
 ( 1.000000000000000000, 0.6092287576699784157, 1.000000000000000000),
 ( 1.000000000000000000, 0.5278258667053503661, 1.000000000000000000),
 ( 1.000000000000000000, 0.4993418825337702094, 1.000000000000000000),
 ( 1.000000000000000000, 0.4999999999997460920, 1.000000000000000000) ) ) 
 REPRESENTATION_ITEM ( '' )  SURFACE ( )  );
#108766 = DIRECTION ( 'NONE',  ( 0.000000000000000000, 0.000000000000000000, -1.000000000000000000 ) ) ;
#108767 = FACE_OUTER_BOUND ( 'NONE', #112735, .T. ) ;
#108768 = DIRECTION ( 'NONE',  ( 0.000000000000000000, 0.2617529984165152257, 0.9651348961777124202 ) ) ;
#108769 = DIRECTION ( 'NONE',  ( -1.000000000000000000, 0.000000000000000000, 0.000000000000000000 ) ) ;
#108770 = DIRECTION ( 'NONE',  ( -1.000000000000000000, 0.000000000000000000, 0.000000000000000000 ) ) ;
#108771 = CYLINDRICAL_SURFACE ( 'NONE', #3092, 0.1000000000000028644 ) ;
#108773 = ORIENTED_EDGE ( 'NONE', *, *, #240960, .F. ) ;
#108772 = CARTESIAN_POINT ( 'NONE',  ( -22.47886152344871036, 75.96249906115033923, -114.6730961275722507 ) ) ;
#108774 = CARTESIAN_POINT ( 'NONE',  ( 20.84999999999999787, 17.13730476842946970, -224.4716215546872036 ) ) ;
#108775 = AXIS2_PLACEMENT_3D ( 'NONE', #180339, #219437, #42127 ) ;
#108776 = DIRECTION ( 'NONE',  ( 1.000000000000000000, 0.000000000000000000, 0.000000000000000000 ) ) ;
#108777 = CARTESIAN_POINT ( 'NONE',  ( 22.48660254037844197, 11.65000000001116298, -66.95000000000004547 ) ) ;
#108778 = EDGE_CURVE ( 'NONE', #221154, #186763, #11400, .T. ) ;
#108779 = EDGE_CURVE ( 'NONE', #107433, #78394, #89704, .T. ) ;
#108780 = DIRECTION ( 'NONE',  ( 0.000000000000000000, 0.4930308989875324399, 0.8700118002898268310 ) ) ;
#108781 = ORIENTED_EDGE ( 'NONE', *, *, #170342, .F. ) ;
#108782 = DIRECTION ( 'NONE',  ( -0.000000000000000000, 0.9126074666063770380, 0.4088369013363281068 ) ) ;
#108783 = CIRCLE ( 'NONE', #237962, 0.2000000000000057288 ) ;
#108784 = DIRECTION ( 'NONE',  ( 0.000000000000000000, 0.000000000000000000, 1.000000000000000000 ) ) ;
#108785 = EDGE_CURVE ( 'NONE', #168244, #99187, #198646, .T. ) ;
#108786 = CIRCLE ( 'NONE', #179724, 11.90000000000000746 ) ;
#108787 = ORIENTED_EDGE ( 'NONE', *, *, #161133, .T. ) ;
#108788 = DIRECTION ( 'NONE',  ( -1.000000000000000000, -0.000000000000000000, -0.000000000000000000 ) ) ;
#108789 = CARTESIAN_POINT ( 'NONE',  ( -16.93339986808596720, 10.00510392857707664, -79.56599367181290461 ) ) ;
#108790 = ORIENTED_EDGE ( 'NONE', *, *, #40903, .F. ) ;
#108791 = DIRECTION ( 'NONE',  ( -0.000000000000000000, -0.2617529984165031243, -0.9651348961777157509 ) ) ;
#108792 = ORIENTED_EDGE ( 'NONE', *, *, #14134, .F. ) ;
#108793 = DIRECTION ( 'NONE',  ( -0.000000000000000000, -1.265107689135680095E-16, 1.000000000000000000 ) ) ;
#108794 = ORIENTED_EDGE ( 'NONE', *, *, #214807, .F. ) ;
#108795 = AXIS2_PLACEMENT_3D ( 'NONE', #180862, #3483, #23087 ) ;
#108796 = CARTESIAN_POINT ( 'NONE',  ( 21.13736287352038445, 67.95335762362860521, -190.8731074845244109 ) ) ;
#108797 = ADVANCED_FACE ( 'NONE', ( #90999 ), #170597, .T. ) ;
#108798 = DIRECTION ( 'NONE',  ( 1.186688945009010077E-16, -1.000000000000000000, -0.000000000000000000 ) ) ;
#108799 = ORIENTED_EDGE ( 'NONE', *, *, #169041, .F. ) ;
#108800 = ORIENTED_EDGE ( 'NONE', *, *, #226547, .F. ) ;
#108801 = DIRECTION ( 'NONE',  ( 0.000000000000000000, 0.000000000000000000, 1.000000000000000000 ) ) ;
#108803 = VERTEX_POINT ( 'NONE', #33649 ) ;
#108802 = CARTESIAN_POINT ( 'NONE',  ( 23.14999999999999503, 15.92646454033040371, -219.3818586450342423 ) ) ;
#108804 = CARTESIAN_POINT ( 'NONE',  ( 20.84999999999998721, 65.66751761918648356, -63.92826094061123143 ) ) ;
#108805 = ORIENTED_EDGE ( 'NONE', *, *, #95778, .F. ) ;
#108806 = EDGE_CURVE ( 'NONE', #208696, #206404, #34920, .T. ) ;
#108807 = ORIENTED_EDGE ( 'NONE', *, *, #32043, .F. ) ;
#108808 = FACE_OUTER_BOUND ( 'NONE', #21622, .T. ) ;
#108810 = CARTESIAN_POINT ( 'NONE',  ( 22.39999999999999858, 75.90000000001219860, -144.3138870828976792 ) ) ;
#108809 = AXIS2_PLACEMENT_3D ( 'NONE', #106767, #143332, #204586 ) ;
#108811 = DIRECTION ( 'NONE',  ( 1.734723475976817507E-14, -6.982962677686266711E-15, 1.000000000000000000 ) ) ;
#108812 = ADVANCED_FACE ( 'NONE', ( #191422 ), #165332, .T. ) ;
#108814 = EDGE_CURVE ( 'NONE', #114401, #213950, #60365, .T. ) ;
#108813 = LINE ( 'NONE', #188363, #13127 ) ;
#108815 = CARTESIAN_POINT ( 'NONE',  ( 21.09551895715237535, 65.37856267284283263, -57.28598281862489472 ) ) ;
#108816 = DIRECTION ( 'NONE',  ( -0.000000000000000000, 1.000000000000000000, -0.000000000000000000 ) ) ;
#108817 = CIRCLE ( 'NONE', #25452, 11.70000000000000462 ) ;
#108818 = EDGE_LOOP ( 'NONE', ( #194680, #234437, #194212, #16542 ) ) ;
#108819 = DIRECTION ( 'NONE',  ( -0.000000000000000000, -0.000000000000000000, -1.000000000000000000 ) ) ;
#108820 = LINE ( 'NONE', #226168, #232015 ) ;
#108821 = CARTESIAN_POINT ( 'NONE',  ( 20.85000000000000142, -11.64999999998883595, -164.6000000000000227 ) ) ;
#108822 = CARTESIAN_POINT ( 'NONE',  ( 20.90000000000000213, 3.362550747017865493, 28.82623795144604983 ) ) ;
#108823 = CIRCLE ( 'NONE', #17274, 0.09999999999999982514 ) ;
#108824 = VERTEX_POINT ( 'NONE', #153599 ) ;
#108825 = DIRECTION ( 'NONE',  ( -1.000000000000000000, 0.000000000000000000, -0.000000000000000000 ) ) ;
#108826 = ORIENTED_EDGE ( 'NONE', *, *, #75336, .T. ) ;
#108827 = DIRECTION ( 'NONE',  ( -1.000000000000000000, -0.000000000000000000, -0.000000000000000000 ) ) ;
#108828 = ORIENTED_EDGE ( 'NONE', *, *, #209922, .T. ) ;
#108829 = EDGE_CURVE ( 'NONE', #145161, #47017, #230524, .T. ) ;
#108831 = EDGE_CURVE ( 'NONE', #85045, #71888, #29482, .T. ) ;
#108830 = AXIS2_PLACEMENT_3D ( 'NONE', #228608, #30408, #205155 ) ;
#108832 = CARTESIAN_POINT ( 'NONE',  ( -14.56556274378147542, 24.89114276590144925, -232.5309687781013395 ) ) ;
#108833 = DIRECTION ( 'NONE',  ( -1.000000000000000000, -0.000000000000000000, -0.000000000000000000 ) ) ;
#108834 = ORIENTED_EDGE ( 'NONE', *, *, #257479, .T. ) ;
#108835 = VECTOR ( 'NONE', #130145, 1000.000000000000114 ) ;
#108836 = ORIENTED_EDGE ( 'NONE', *, *, #148277, .F. ) ;
#108838 = ORIENTED_EDGE ( 'NONE', *, *, #181686, .F. ) ;
#108837 = CARTESIAN_POINT ( 'NONE',  ( 13.40000000000005898, 67.75000000001118394, -23.62310748452479103 ) ) ;
#108839 = CARTESIAN_POINT ( 'NONE',  ( -17.11825945287481332, 66.05000000001153637, -48.77310748452439526 ) ) ;
#108840 = EDGE_LOOP ( 'NONE', ( #54649, #12039, #187606, #53748 ) ) ;
#108841 = EDGE_CURVE ( 'NONE', #161481, #222763, #190115, .T. ) ;
#108842 = DIRECTION ( 'NONE',  ( 1.000000000000000000, -0.000000000000000000, -0.000000000000000000 ) ) ;
#108843 = AXIS2_PLACEMENT_3D ( 'NONE', #108594, #9486, #89017 ) ;
#108844 = CARTESIAN_POINT ( 'NONE',  ( 20.94999999999999929, 0.000000000000000000, -33.50000000000000000 ) ) ;
#108845 = ORIENTED_EDGE ( 'NONE', *, *, #204047, .F. ) ;
#108846 = EDGE_CURVE ( 'NONE', #103509, #245289, #51852, .T. ) ;
#108847 = CARTESIAN_POINT ( 'NONE',  ( -23.25000000000000000, 69.06610602788535402, -65.73746165015079157 ) ) ;
#108848 = DIRECTION ( 'NONE',  ( 0.000000000000000000, 0.2617529984165022361, 0.9651348961777160840 ) ) ;
#108849 = CIRCLE ( 'NONE', #71474, 0.1000000000000013933 ) ;
#108850 = ADVANCED_FACE ( 'NONE', ( #54436 ), #195266, .T. ) ;
#108852 = EDGE_CURVE ( 'NONE', #245185, #115670, #202926, .T. ) ;
#108851 = AXIS2_PLACEMENT_3D ( 'NONE', #226800, #48160, #93712 ) ;
#108853 = ORIENTED_EDGE ( 'NONE', *, *, #65061, .T. ) ;
#108854 = CARTESIAN_POINT ( 'NONE',  ( 20.04999999999999716, 67.25000000001206502, -127.2731074845243597 ) ) ;
#108856 =( BOUNDED_SURFACE ( )  B_SPLINE_SURFACE ( 3, 2, ( 
 ( #159067, #22119, #217707 ),
 ( #121242, #118655, #211658 ),
 ( #36567, #195627, #165472 ),
 ( #7682, #88458, #106754 ) ),
 .UNSPECIFIED., .F., .F., .F. ) 
 B_SPLINE_SURFACE_WITH_KNOTS ( ( 4, 4 ),
 ( 3, 3 ),
 ( -5.827586677109586333E-19, 0.0003124336117481331431 ),
 ( 0.000000000000000000, 1.000000000000000000 ),
 .UNSPECIFIED. ) 
 GEOMETRIC_REPRESENTATION_ITEM ( )  RATIONAL_B_SPLINE_SURFACE ( (
 ( 1.000000000000000000, 0.7040654476015839602, 1.000000000000000000),
 ( 1.000000000000000000, 0.7039193538781365334, 1.000000000000000000),
 ( 1.000000000000000000, 0.7089171279145672910, 1.000000000000000000),
 ( 1.000000000000000000, 0.7071067811865509034, 1.000000000000000000) ) ) 
 REPRESENTATION_ITEM ( '' )  SURFACE ( )  );
#108855 = VECTOR ( 'NONE', #212799, 1000.000000000000000 ) ;
#108857 = EDGE_CURVE ( 'NONE', #102466, #43391, #73774, .T. ) ;
#108858 = CARTESIAN_POINT ( 'NONE',  ( 18.59999999999998366, 7.021664781900089913, -37.33356540189728889 ) ) ;
#108859 = CIRCLE ( 'NONE', #241948, 0.1000000000000028644 ) ;
#108860 = CARTESIAN_POINT ( 'NONE',  ( -21.10257677756356642, 6.398381742543891804, -66.97504925043209312 ) ) ;
#108862 = ORIENTED_EDGE ( 'NONE', *, *, #226884, .T. ) ;
#108861 = FACE_OUTER_BOUND ( 'NONE', #97291, .T. ) ;
#108863 = EDGE_CURVE ( 'NONE', #210898, #203112, #133970, .T. ) ;
#108864 = DIRECTION ( 'NONE',  ( -1.020425574104004196E-15, 0.000000000000000000, 1.000000000000000000 ) ) ;
#108865 = DIRECTION ( 'NONE',  ( 1.713247197920696616E-14, 0.9876197685951252359, -0.1568667991644863424 ) ) ;
#108866 = EDGE_CURVE ( 'NONE', #114396, #137793, #38679, .T. ) ;
#108867 = CARTESIAN_POINT ( 'NONE',  ( 21.05000000000000071, 60.99662849158838895, -205.1669373764474642 ) ) ;
#108869 = CARTESIAN_POINT ( 'NONE',  ( -21.55000000000000071, 9.788464569039593499, -211.4053333142630891 ) ) ;
#108868 = CARTESIAN_POINT ( 'NONE',  ( -17.11825945287481332, 10.05000000001113847, -154.8500000000000227 ) ) ;
#108870 = CARTESIAN_POINT ( 'NONE',  ( 21.05000000000000071, 10.68429367439823352, -108.0266739386370887 ) ) ;
#108872 = EDGE_CURVE ( 'NONE', #19091, #121961, #119508, .T. ) ;
#108871 = DIRECTION ( 'NONE',  ( 0.000000000000000000, -1.000000000000000000, 0.000000000000000000 ) ) ;
#108873 = DIRECTION ( 'NONE',  ( 0.000000000000000000, -6.982962677686266711E-15, 1.000000000000000000 ) ) ;
#108874 = DIRECTION ( 'NONE',  ( 0.000000000000000000, -0.000000000000000000, -1.000000000000000000 ) ) ;
#108875 = AXIS2_PLACEMENT_3D ( 'NONE', #177137, #157593, #254066 ) ;
#108876 = VECTOR ( 'NONE', #183736, 1000.000000000000000 ) ;
#108877 = ORIENTED_EDGE ( 'NONE', *, *, #57104, .F. ) ;
#108878 = ORIENTED_EDGE ( 'NONE', *, *, #13720, .T. ) ;
#108879 = ORIENTED_EDGE ( 'NONE', *, *, #41535, .F. ) ;
#108880 = EDGE_CURVE ( 'NONE', #185475, #254207, #19789, .T. ) ;
#108881 = CARTESIAN_POINT ( 'NONE',  ( -21.05000000000000071, 64.25000000001220712, -143.3647081744215086 ) ) ;
#108882 = CARTESIAN_POINT ( 'NONE',  ( -20.64999999999999858, 71.75000000001253397, -182.3731074845244109 ) ) ;
#108883 = ORIENTED_EDGE ( 'NONE', *, *, #38809, .F. ) ;
#108884 = LINE ( 'NONE', #226232, #236466 ) ;
#108885 = CARTESIAN_POINT ( 'NONE',  ( -18.79999999999999716, 1.885425182446133663, -11.49641995933507665 ) ) ;
#108886 = DIRECTION ( 'NONE',  ( 0.000000000000000000, 0.4999999999999478195, 0.8660254037844686836 ) ) ;
#108887 = ORIENTED_EDGE ( 'NONE', *, *, #161900, .F. ) ;
#108888 = EDGE_LOOP ( 'NONE', ( #63837, #193221, #223059, #3880 ) ) ;
#108889 = FACE_OUTER_BOUND ( 'NONE', #70485, .T. ) ;
#108890 = CARTESIAN_POINT ( 'NONE',  ( -23.25000000000000000, -1.835859311432481045, -179.0044391687985410 ) ) ;
#108891 = ORIENTED_EDGE ( 'NONE', *, *, #70934, .F. ) ;
#108892 = PLANE ( 'NONE',  #112023 ) ;
#108894 = ORIENTED_EDGE ( 'NONE', *, *, #92240, .T. ) ;
#108893 = CARTESIAN_POINT ( 'NONE',  ( -20.54999999999999716, 74.00000000001223555, -149.7477294072864709 ) ) ;
#108895 = CARTESIAN_POINT ( 'NONE',  ( -23.15000000000000213, 76.00000000001213607, -136.5231074845243313 ) ) ;
#108896 = CARTESIAN_POINT ( 'NONE',  ( -5.900000000000002132, -11.25000000000000000, 13.90000000000000213 ) ) ;
#108897 = CIRCLE ( 'NONE', #208872, 0.1000000000000028644 ) ;
#108899 = VERTEX_POINT ( 'NONE', #40047 ) ;
#108898 = LINE ( 'NONE', #170219, #47978 ) ;
#108900 = DIRECTION ( 'NONE',  ( 0.000000000000000000, -0.1455152366551721865, -0.9893560106964475187 ) ) ;
#108901 = CARTESIAN_POINT ( 'NONE',  ( 20.96428641294248862, 64.25000000001219291, -143.3482143065823777 ) ) ;
#108902 = CARTESIAN_POINT ( 'NONE',  ( -21.05000000000000071, 5.021051876504147385E-16, -37.60000000000000142 ) ) ;
#108903 = CARTESIAN_POINT ( 'NONE',  ( -16.92989143108097494, 12.46350622712228429, -211.4700479134609736 ) ) ;
#108904 = ADVANCED_FACE ( 'NONE', ( #116986 ), #90490, .F. ) ;
#108906 = CARTESIAN_POINT ( 'NONE',  ( 20.19326291201235790, 10.15606098791279877, -108.2618618076038786 ) ) ;
#108905 = CARTESIAN_POINT ( 'NONE',  ( -16.87683809663752399, 9.850000000011139178, -154.0976359818037054 ) ) ;
#108907 = DIRECTION ( 'NONE',  ( 0.000000000000000000, 0.000000000000000000, 1.000000000000000000 ) ) ;
#108908 = CARTESIAN_POINT ( 'NONE',  ( -18.50000000000000000, 85.40000000001241176, -163.1410656363516125 ) ) ;
#108909 = EDGE_CURVE ( 'NONE', #242555, #135846, #157435, .T. ) ;
#108910 = DIRECTION ( 'NONE',  ( -1.000000000000000000, 0.000000000000000000, 0.000000000000000000 ) ) ;
#108911 = CARTESIAN_POINT ( 'NONE',  ( -20.00857864376270001, 66.65000000001150227, -48.27310748452438816 ) ) ;
#108912 = ORIENTED_EDGE ( 'NONE', *, *, #163781, .T. ) ;
#108913 = ORIENTED_EDGE ( 'NONE', *, *, #100972, .T. ) ;
#108915 = CIRCLE ( 'NONE', #33970, 0.1000000000000028644 ) ;
#108914 = CARTESIAN_POINT ( 'NONE',  ( 23.15000000000000213, 28.58935552370083144, -258.2621935127861548 ) ) ;
#108916 = VERTEX_POINT ( 'NONE', #236929 ) ;
#108917 = DIRECTION ( 'NONE',  ( 0.000000000000000000, 8.673617379884087537E-15, -1.000000000000000000 ) ) ;
#108918 = ORIENTED_EDGE ( 'NONE', *, *, #62307, .F. ) ;
#108919 = DIRECTION ( 'NONE',  ( 0.000000000000000000, 1.000000000000000000, 0.000000000000000000 ) ) ;
#108920 = CARTESIAN_POINT ( 'NONE',  ( 18.54999999999999716, 44.62608598762253109, -236.3940605665350745 ) ) ;
#108921 = EDGE_LOOP ( 'NONE', ( #200148, #14698, #224732, #38964 ) ) ;
#108922 = DIRECTION ( 'NONE',  ( 1.000000000000000000, 0.000000000000000000, 0.000000000000000000 ) ) ;
#108923 = ADVANCED_FACE ( 'NONE', ( #196511 ), #178272, .F. ) ;
#108924 = TOROIDAL_SURFACE ( 'NONE', #188058, 4.900000000000000355, 0.1000000000000000056 ) ;
#108926 = ORIENTED_EDGE ( 'NONE', *, *, #72317, .T. ) ;
#108925 = AXIS2_PLACEMENT_3D ( 'NONE', #245548, #149027, #75599 ) ;
#108927 = EDGE_LOOP ( 'NONE', ( #35568, #188381, #26144, #30879 ) ) ;
#108928 = ORIENTED_EDGE ( 'NONE', *, *, #247005, .T. ) ;
#108929 = TOROIDAL_SURFACE ( 'NONE', #83951, 11.65000000000000036, 0.1000000000000000056 ) ;
#108930 = DIRECTION ( 'NONE',  ( 0.000000000000000000, 0.000000000000000000, -1.000000000000000000 ) ) ;
#108931 = DIRECTION ( 'NONE',  ( -0.000000000000000000, 0.9770955615653313941, 0.2128009952263603954 ) ) ;
#108932 = LINE ( 'NONE', #188473, #134323 ) ;
#108933 = CARTESIAN_POINT ( 'NONE',  ( -23.15000000000000213, 11.65000000001115588, -88.35000000000003695 ) ) ;
#108934 = DIRECTION ( 'NONE',  ( 0.000000000000000000, 3.552713678800407449E-15, -1.000000000000000000 ) ) ;
#108936 = DIRECTION ( 'NONE',  ( -1.000000000000000000, -0.000000000000000000, -0.000000000000000000 ) ) ;
#108935 = DIRECTION ( 'NONE',  ( -1.000000000000000000, -0.000000000000000000, -0.000000000000000000 ) ) ;
#108937 = CARTESIAN_POINT ( 'NONE',  ( -13.43673303185028978, 9.446648990640015953, -82.08916329592322825 ) ) ;
#108939 = ORIENTED_EDGE ( 'NONE', *, *, #208248, .T. ) ;
#108938 = PLANE ( 'NONE',  #39956 ) ;
#108941 = DIRECTION ( 'NONE',  ( 0.000000000000000000, 0.000000000000000000, -1.000000000000000000 ) ) ;
#108940 = CARTESIAN_POINT ( 'NONE',  ( 20.30466543256828160, 9.304236939266628426, -75.25366265139203392 ) ) ;
#108942 = DIRECTION ( 'NONE',  ( -0.000000000000000000, 1.000000000000000000, 6.982962677686266711E-15 ) ) ;
#108943 = ORIENTED_EDGE ( 'NONE', *, *, #144705, .F. ) ;
#108944 = CARTESIAN_POINT ( 'NONE',  ( 19.58285714285715073, 9.015001489648581057, -8.420652816081712899 ) ) ;
#108945 = CARTESIAN_POINT ( 'NONE',  ( 22.57320508075688892, 64.25000000001193712, -103.0231074845244024 ) ) ;
#108946 = DIRECTION ( 'NONE',  ( 1.000000000000000000, 0.000000000000000000, 0.000000000000000000 ) ) ;
#108947 = VERTEX_POINT ( 'NONE', #257717 ) ;
#108948 = AXIS2_PLACEMENT_3D ( 'NONE', #154912, #212306, #230580 ) ;
#108949 = DIRECTION ( 'NONE',  ( 0.000000000000000000, -1.000000000000000000, -0.000000000000000000 ) ) ;
#108950 = FACE_OUTER_BOUND ( 'NONE', #232966, .T. ) ;
#108951 = DIRECTION ( 'NONE',  ( 0.000000000000000000, 0.9910827722268055195, -0.1332476588733540468 ) ) ;
#108952 = ORIENTED_EDGE ( 'NONE', *, *, #152690, .T. ) ;
#108953 = EDGE_LOOP ( 'NONE', ( #152847, #76207, #36025, #244921 ) ) ;
#108954 = LINE ( 'NONE', #226319, #74189 ) ;
#108955 = DIRECTION ( 'NONE',  ( 0.000000000000000000, 0.000000000000000000, -1.000000000000000000 ) ) ;
#108956 = CARTESIAN_POINT ( 'NONE',  ( 23.14999999999999858, 76.00000000001126921, -203.5231074845248997 ) ) ;
#108957 = CARTESIAN_POINT ( 'NONE',  ( -18.50000000000000000, 76.00000000001190870, -103.0231074845243029 ) ) ;
#108958 = VERTEX_POINT ( 'NONE', #119572 ) ;
#108959 = EDGE_CURVE ( 'NONE', #192900, #141175, #40480, .T. ) ;
#108960 = DIRECTION ( 'NONE',  ( 0.000000000000000000, 0.000000000000000000, -1.000000000000000000 ) ) ;
#108961 = CIRCLE ( 'NONE', #113076, 0.6000000000000064171 ) ;
#108963 = CARTESIAN_POINT ( 'NONE',  ( -20.85000000000000142, 76.00000000001190870, -103.0231074845243029 ) ) ;
#108962 = VECTOR ( 'NONE', #146824, 1000.000000000000000 ) ;
#108964 = ADVANCED_FACE ( 'NONE', ( #17872 ), #21747, .T. ) ;
#108965 = AXIS2_PLACEMENT_3D ( 'NONE', #57981, #234065, #116688 ) ;
#108966 = CARTESIAN_POINT ( 'NONE',  ( -13.40000000000000213, -8.250000000000007105, 15.00000000000000355 ) ) ;
#108967 = DIRECTION ( 'NONE',  ( -4.239556034732056743E-17, 0.1298341882520022694, 0.9915357197604853789 ) ) ;
#108968 = EDGE_LOOP ( 'NONE', ( #27722, #17831, #169936, #147025 ) ) ;
#108969 = DIRECTION ( 'NONE',  ( -0.000000000000000000, -0.9887567792719339499, -0.1495327102803676589 ) ) ;
#108970 = EDGE_CURVE ( 'NONE', #6716, #25976, #252994, .T. ) ;
#108972 = ORIENTED_EDGE ( 'NONE', *, *, #204974, .T. ) ;
#108971 = CARTESIAN_POINT ( 'NONE',  ( 19.99999999999998934, 11.65000000001115943, -155.2500000000000284 ) ) ;
#108973 = CARTESIAN_POINT ( 'NONE',  ( -16.93353400591625757, 10.00461239618409515, -121.4326844702054444 ) ) ;
#108974 = FACE_OUTER_BOUND ( 'NONE', #238464, .T. ) ;
#108975 = CARTESIAN_POINT ( 'NONE',  ( -20.64999999999999858, 68.75000000001205080, -124.1731074845243370 ) ) ;
#108976 = CARTESIAN_POINT ( 'NONE',  ( 20.04142135623731136, 62.37381720523315209, -208.8758809977715032 ) ) ;
#108977 = EDGE_CURVE ( 'NONE', #89516, #238120, #58274, .T. ) ;
#108978 = DIRECTION ( 'NONE',  ( 0.000000000000000000, -1.000000000000000000, 0.000000000000000000 ) ) ;
#108979 = EDGE_CURVE ( 'NONE', #180643, #19042, #99031, .T. ) ;
#108980 = CARTESIAN_POINT ( 'NONE',  ( -18.59999999999999787, 11.64999999999999680, -7.014805770653998351 ) ) ;
#108981 = AXIS2_PLACEMENT_3D ( 'NONE', #157475, #236981, #68613 ) ;
#108982 = ORIENTED_EDGE ( 'NONE', *, *, #75123, .F. ) ;
#108983 = CARTESIAN_POINT ( 'NONE',  ( 23.15000000000000213, 84.66355140188093742, -79.04720860259155302 ) ) ;
#108984 = CARTESIAN_POINT ( 'NONE',  ( -21.14999999999999858, 75.90220970870393558, -209.7809220950004772 ) ) ;
#108985 = FACE_OUTER_BOUND ( 'NONE', #114368, .T. ) ;
#108986 = CARTESIAN_POINT ( 'NONE',  ( -18.40000000000000213, 11.47316190337364183, -188.3914213562372311 ) ) ;
#108987 = EDGE_CURVE ( 'NONE', #189246, #201514, #136437, .T. ) ;
#108988 = FACE_OUTER_BOUND ( 'NONE', #78397, .T. ) ;
#108989 = CARTESIAN_POINT ( 'NONE',  ( -18.59999999999999787, 9.350000000011156942, -188.6499999999999488 ) ) ;
#108990 = ORIENTED_EDGE ( 'NONE', *, *, #40549, .F. ) ;
#108991 = ORIENTED_EDGE ( 'NONE', *, *, #18185, .T. ) ;
#108992 = LINE ( 'NONE', #9900, #22574 ) ;
#108993 = DIRECTION ( 'NONE',  ( -1.000000000000000000, 1.335000415235278971E-16, -2.979993593738921214E-16 ) ) ;
#108994 = CARTESIAN_POINT ( 'NONE',  ( 20.99999999999999645, 66.25000000001202238, -115.6731074845243796 ) ) ;
#108995 = EDGE_CURVE ( 'NONE', #75474, #78587, #238202, .T. ) ;
#108996 = CIRCLE ( 'NONE', #46453, 0.1000000000000003109 ) ;
#108997 = DIRECTION ( 'NONE',  ( -1.000000000000000000, 0.000000000000000000, -0.000000000000000000 ) ) ;
#108998 = DIRECTION ( 'NONE',  ( 0.000000000000000000, 0.000000000000000000, -1.000000000000000000 ) ) ;
#108999 = AXIS2_PLACEMENT_3D ( 'NONE', #163160, #24945, #183990 ) ;
#109000 = CARTESIAN_POINT ( 'NONE',  ( 18.59999999999999432, 1.728086936805619311, -120.8844350051678020 ) ) ;
#109001 = CARTESIAN_POINT ( 'NONE',  ( -23.24999999999999645, -9.599999999988845900, -207.6001893912220169 ) ) ;
#109002 = CIRCLE ( 'NONE', #159118, 0.09999999999998898659 ) ;
#109003 = DIRECTION ( 'NONE',  ( -0.000000000000000000, -0.9868171638914230437, 0.1618390714546045217 ) ) ;
#109004 = AXIS2_PLACEMENT_3D ( 'NONE', #176045, #151344, #252979 ) ;
#109005 = VERTEX_POINT ( 'NONE', #81666 ) ;
#109006 = CARTESIAN_POINT ( 'NONE',  ( 20.94999999999999574, 77.26178616857662007, -61.43660852097883662 ) ) ;
#109007 = CIRCLE ( 'NONE', #67326, 0.09999999999999939493 ) ;
#109008 = ORIENTED_EDGE ( 'NONE', *, *, #178113, .F. ) ;
#109009 = CARTESIAN_POINT ( 'NONE',  ( 20.85000000000000142, 76.00000000001142553, -36.02310748452432421 ) ) ;
#109010 = DIRECTION ( 'NONE',  ( 1.000000000000000000, 0.000000000000000000, 0.000000000000000000 ) ) ;
#109011 = FACE_OUTER_BOUND ( 'NONE', #66538, .T. ) ;
#109012 = CARTESIAN_POINT ( 'NONE',  ( -21.00857864376268935, 64.40000000001263913, -196.5949042542488598 ) ) ;
#109013 = DIRECTION ( 'NONE',  ( -1.000000000000000000, -1.394253735153569469E-16, -2.602809386958778209E-16 ) ) ;
#109015 = CARTESIAN_POINT ( 'NONE',  ( -18.50000000000001066, -9.421308209739168049, -7.242363214050910436 ) ) ;
#109014 = CIRCLE ( 'NONE', #100796, 0.09999999999998898659 ) ;
#109016 = CARTESIAN_POINT ( 'NONE',  ( -20.94999999999999929, 0.6869237119019839799, -212.7787591058053067 ) ) ;
#109017 = ORIENTED_EDGE ( 'NONE', *, *, #27587, .T. ) ;
#109018 = CARTESIAN_POINT ( 'NONE',  ( -20.94999999999999929, -11.74999999998884448, -97.40000000000004832 ) ) ;
#109019 = AXIS2_PLACEMENT_3D ( 'NONE', #143907, #64387, #5658 ) ;
#109020 = DIRECTION ( 'NONE',  ( -1.000000000000000000, 7.304098846218134667E-16, 5.100424963727255829E-30 ) ) ;
#109021 = DIRECTION ( 'NONE',  ( 1.000000000000000000, 0.000000000000000000, 0.000000000000000000 ) ) ;
#109022 = DIRECTION ( 'NONE',  ( 2.840903330521632269E-16, 0.7106264324241464703, -0.7035695228903323661 ) ) ;
#109023 = AXIS2_PLACEMENT_3D ( 'NONE', #90792, #192479, #169102 ) ;
#109024 = AXIS2_PLACEMENT_3D ( 'NONE', #175532, #78941, #154690 ) ;
#109025 = CARTESIAN_POINT ( 'NONE',  ( -22.48660254037843131, 11.65000000001115588, -167.4499999999999886 ) ) ;
#109026 = ADVANCED_FACE ( 'NONE', ( #80386 ), #60847, .T. ) ;
#109027 = ORIENTED_EDGE ( 'NONE', *, *, #83181, .F. ) ;
#109028 = VECTOR ( 'NONE', #217366, 1000.000000000000000 ) ;
#109029 = DIRECTION ( 'NONE',  ( -1.652117596168391700E-15, -1.000000000000000000, 0.000000000000000000 ) ) ;
#109030 = DIRECTION ( 'NONE',  ( -0.000000000000000000, 6.982962677686266711E-15, -1.000000000000000000 ) ) ;
#109031 = VERTEX_POINT ( 'NONE', #159988 ) ;
#109033 = EDGE_CURVE ( 'NONE', #55246, #96147, #178656, .T. ) ;
#109032 = VECTOR ( 'NONE', #202434, 1000.000000000000114 ) ;
#109034 = VERTEX_POINT ( 'NONE', #146791 ) ;
#109035 = CARTESIAN_POINT ( 'NONE',  ( 18.59999999999999076, 65.79142135624951493, -145.2731074845244450 ) ) ;
#109036 = DIRECTION ( 'NONE',  ( -0.000000000000000000, -0.01283462868040327436, 0.9999176327611370985 ) ) ;
#109037 = CARTESIAN_POINT ( 'NONE',  ( 21.03675099975492202, 44.27880510233411826, -236.4124706813595083 ) ) ;
#109038 = EDGE_CURVE ( 'NONE', #96287, #58661, #186383, .T. ) ;
#109039 = VERTEX_POINT ( 'NONE', #3438 ) ;
#109041 = ADVANCED_FACE ( 'NONE', ( #225043 ), #84211, .F. ) ;
#109040 = CARTESIAN_POINT ( 'NONE',  ( 21.05315837417574443, 64.25000000264165578, -42.86475148229496313 ) ) ;
#109042 = DIRECTION ( 'NONE',  ( 1.000000000000000000, -2.849773892568378313E-16, 7.728835255496647986E-17 ) ) ;
#109043 = AXIS2_PLACEMENT_3D ( 'NONE', #188281, #245693, #206566 ) ;
#109044 = VERTEX_POINT ( 'NONE', #163822 ) ;
#109045 = AXIS2_PLACEMENT_3D ( 'NONE', #29825, #92322, #51894 ) ;
#109046 = CIRCLE ( 'NONE', #254758, 0.09999999999999939493 ) ;
#109047 = VECTOR ( 'NONE', #124997, 1000.000000000000000 ) ;
#109048 = CARTESIAN_POINT ( 'NONE',  ( 20.94999999999999929, 10.72371710471868056, -112.6500000000000341 ) ) ;
#109049 = ORIENTED_EDGE ( 'NONE', *, *, #162954, .T. ) ;
#109050 = DIRECTION ( 'NONE',  ( 0.000000000000000000, 0.000000000000000000, -1.000000000000000000 ) ) ;
#109051 = EDGE_CURVE ( 'NONE', #226810, #59020, #144226, .T. ) ;
#109052 = LINE ( 'NONE', #247276, #96122 ) ;
#109054 = ORIENTED_EDGE ( 'NONE', *, *, #136614, .F. ) ;
#109053 = DIRECTION ( 'NONE',  ( 0.000000000000000000, -1.000000000000000000, -0.000000000000000000 ) ) ;
#109055 = DIRECTION ( 'NONE',  ( 1.000000000000000000, 0.000000000000000000, 0.000000000000000000 ) ) ;
#109056 = CARTESIAN_POINT ( 'NONE',  ( -18.40000000000000213, 64.52683809664972614, -145.8490535513323891 ) ) ;
#109057 = ADVANCED_FACE ( 'NONE', ( #47697 ), #28185, .F. ) ;
#109058 = DIRECTION ( 'NONE',  ( 0.000000000000000000, -0.8814952561688429444, 0.4721928772777349015 ) ) ;
#109059 = CARTESIAN_POINT ( 'NONE',  ( -16.82055514392384410, 66.05000000001228955, -157.3463094099821546 ) ) ;
#109060 = DIRECTION ( 'NONE',  ( 0.000000000000000000, 0.000000000000000000, -1.000000000000000000 ) ) ;
#109061 = CARTESIAN_POINT ( 'NONE',  ( 21.05000000000000071, 1.115600667400684642E-11, -134.0000000000000000 ) ) ;
#109062 = FACE_OUTER_BOUND ( 'NONE', #164727, .T. ) ;
#109064 = ORIENTED_EDGE ( 'NONE', *, *, #56844, .T. ) ;
#109063 = CARTESIAN_POINT ( 'NONE',  ( -20.85000000000000142, -1.851617760457748618, -212.6031897196036198 ) ) ;
#109066 = VERTEX_POINT ( 'NONE', #4713 ) ;
#109065 = PRODUCT_RELATED_PRODUCT_CATEGORY ( 'part', '', ( #68063 ) ) ;
#109068 = LINE ( 'NONE', #146898, #231287 ) ;
#109067 = DIRECTION ( 'NONE',  ( 0.000000000000000000, 0.5000000000000004441, 0.8660254037844384856 ) ) ;
#109070 = VERTEX_POINT ( 'NONE', #162549 ) ;
#109069 = DIRECTION ( 'NONE',  ( 0.000000000000000000, 0.2617529984165059553, 0.9651348961777148627 ) ) ;
#109071 = VERTEX_POINT ( 'NONE', #82951 ) ;
#109072 = CARTESIAN_POINT ( 'NONE',  ( -16.77828822459933633, 66.05377062495608698, -182.6857357354433589 ) ) ;
#109073 = VECTOR ( 'NONE', #189112, 1000.000000000000000 ) ;
#109074 = FACE_OUTER_BOUND ( 'NONE', #167614, .T. ) ;
#109076 = ADVANCED_FACE ( 'NONE', ( #6003 ), #187246, .F. ) ;
#109075 = CARTESIAN_POINT ( 'NONE',  ( 23.14999999999999503, 15.92646454033040371, -219.3818586450342423 ) ) ;
#109077 = FACE_OUTER_BOUND ( 'NONE', #1136, .T. ) ;
#109078 = ADVANCED_FACE ( 'NONE', ( #145520 ), #88089, .F. ) ;
#109079 = EDGE_CURVE ( 'NONE', #135406, #58809, #115620, .T. ) ;
#109080 = CARTESIAN_POINT ( 'NONE',  ( -20.54999999999999716, 66.65000000001150227, -48.27310748452438816 ) ) ;
#109081 = DIRECTION ( 'NONE',  ( -2.978066053179067751E-16, 1.000000000000000000, 0.000000000000000000 ) ) ;
#109082 = PLANE ( 'NONE',  #177108 ) ;
#109083 = VERTEX_POINT ( 'NONE', #48991 ) ;
#109084 = ORIENTED_EDGE ( 'NONE', *, *, #166976, .F. ) ;
#109085 = DIRECTION ( 'NONE',  ( -1.000000000000000000, -0.000000000000000000, 0.000000000000000000 ) ) ;
#109086 = ORIENTED_EDGE ( 'NONE', *, *, #187727, .F. ) ;
#109087 = PLANE ( 'NONE',  #21861 ) ;
#109088 = ORIENTED_EDGE ( 'NONE', *, *, #159619, .T. ) ;
#109089 = DIRECTION ( 'NONE',  ( 0.000000000000000000, 0.000000000000000000, -1.000000000000000000 ) ) ;
#109090 = AXIS2_PLACEMENT_3D ( 'NONE', #251715, #215156, #135605 ) ;
#109091 = CARTESIAN_POINT ( 'NONE',  ( -20.64999999999999858, 61.88149656937975607, -248.1136133839584090 ) ) ;
#109092 = DIRECTION ( 'NONE',  ( 0.000000000000000000, -6.982962677686266711E-15, 1.000000000000000000 ) ) ;
#109093 = ORIENTED_EDGE ( 'NONE', *, *, #9935, .T. ) ;
#109094 =( REPRESENTATION_RELATIONSHIP ('NONE','NONE', #36900, #26974 ) REPRESENTATION_RELATIONSHIP_WITH_TRANSFORMATION ( #202011 )SHAPE_REPRESENTATION_RELATIONSHIP( ) );
#109095 = CARTESIAN_POINT ( 'NONE',  ( 21.14999999999999858, 1.115600667400684642E-11, -93.95934304829877703 ) ) ;
#109096 = VERTEX_POINT ( 'NONE', #166413 ) ;
#109097 = CARTESIAN_POINT ( 'NONE',  ( -16.94226253665225457, 66.05000000001155058, -48.96984208014017526 ) ) ;
#109098 = CARTESIAN_POINT ( 'NONE',  ( -23.25000000000000000, 67.85909929089923764, -227.8797997985275856 ) ) ;
#109099 = EDGE_CURVE ( 'NONE', #76926, #224952, #3176, .T. ) ;
#109100 = CARTESIAN_POINT ( 'NONE',  ( -21.14999999999999858, 26.02743912001966464, -254.3139371321002216 ) ) ;
#109101 = ORIENTED_EDGE ( 'NONE', *, *, #53062, .F. ) ;
#109103 = CARTESIAN_POINT ( 'NONE',  ( 21.30000000000002558, 76.00000000001168132, -73.57310748452432847 ) ) ;
#109102 = CIRCLE ( 'NONE', #34150, 0.09999999999999939493 ) ;
#109104 = ORIENTED_EDGE ( 'NONE', *, *, #129343, .F. ) ;
#109107 = ORIENTED_EDGE ( 'NONE', *, *, #19582, .T. ) ;
#109106 = CARTESIAN_POINT ( 'NONE',  ( -18.40000000000000213, 64.52683809664974035, -149.0731074845244279 ) ) ;
#109105 = CARTESIAN_POINT ( 'NONE',  ( -23.25000000000000000, -11.74999999998884448, -36.60000000000000853 ) ) ;
#109108 = CARTESIAN_POINT ( 'NONE',  ( -20.85000000000000142, 64.25000000001148237, -42.80697314750249660 ) ) ;
#109109 = ORIENTED_EDGE ( 'NONE', *, *, #134453, .T. ) ;
#109110 = CIRCLE ( 'NONE', #13277, 2.000000000000002665 ) ;
#109111 = ORIENTED_EDGE ( 'NONE', *, *, #134739, .F. ) ;
#109112 = EDGE_CURVE ( 'NONE', #99842, #107651, #169841, .T. ) ;
#109113 = DIRECTION ( 'NONE',  ( -1.284434275755705789E-16, 0.7071067811865472397, -0.7071067811865479058 ) ) ;
#109114 = FACE_OUTER_BOUND ( 'NONE', #157305, .T. ) ;
#109115 = FACE_OUTER_BOUND ( 'NONE', #124988, .T. ) ;
#109116 = ADVANCED_FACE ( 'NONE', ( #29473 ), #86369, .T. ) ;
#109117 = CARTESIAN_POINT ( 'NONE',  ( -23.15000000000000213, 69.16514130714681130, -247.7543978865853660 ) ) ;
#109118 = AXIS2_PLACEMENT_3D ( 'NONE', #219827, #178168, #38635 ) ;
#109119 = EDGE_LOOP ( 'NONE', ( #917, #204766, #134376 ) ) ;
#109120 = ADVANCED_FACE ( 'NONE', ( #123404 ), #202933, .F. ) ;
#109121 = FACE_OUTER_BOUND ( 'NONE', #140549, .T. ) ;
#109122 = DIRECTION ( 'NONE',  ( 1.000000000000000000, 0.000000000000000000, 0.000000000000000000 ) ) ;
#109123 = CARTESIAN_POINT ( 'NONE',  ( 18.50211644919734866, 10.30207779525984435, -139.4895520716783039 ) ) ;
#109124 = ORIENTED_EDGE ( 'NONE', *, *, #141869, .T. ) ;
#109125 = PLANE ( 'NONE',  #163674 ) ;
#109126 = ORIENTED_EDGE ( 'NONE', *, *, #216804, .F. ) ;
#109127 = DIRECTION ( 'NONE',  ( -1.000000000000000000, 2.952720810173289112E-16, 2.061873921506763405E-30 ) ) ;
#109128 = B_SPLINE_CURVE_WITH_KNOTS ( 'NONE', 3,
 ( #189863, #86883, #171618, #209415, #8657, #47760, #169055, #12532 ),
 .UNSPECIFIED., .F., .F.,
 ( 4, 2, 2, 4 ),
 ( 0.000000000000000000, 0.0002181133598168873079, 0.0003271700397253444331, 0.0004362267196338015583 ),
 .UNSPECIFIED. ) ;
#109129 = VERTEX_POINT ( 'NONE', #184648 ) ;
#109130 = EDGE_CURVE ( 'NONE', #180750, #188642, #32466, .T. ) ;
#109131 = EDGE_CURVE ( 'NONE', #58292, #236311, #203109, .T. ) ;
#109132 = DIRECTION ( 'NONE',  ( -0.000000000000000000, -0.2128009952263604787, 0.9770955615653313941 ) ) ;
#109133 = CARTESIAN_POINT ( 'NONE',  ( -22.59999970745345976, 76.00935637733996941, -181.7736206921935889 ) ) ;
#109135 = ORIENTED_EDGE ( 'NONE', *, *, #79604, .F. ) ;
#109134 = DIRECTION ( 'NONE',  ( 0.000000000000000000, -1.000000000000000000, 0.000000000000000000 ) ) ;
#109136 = DIRECTION ( 'NONE',  ( 1.000000000000000000, 0.000000000000000000, 0.000000000000000000 ) ) ;
#109137 = CARTESIAN_POINT ( 'NONE',  ( -15.15564720441981805, 62.87834062276081681, -215.9526216959265810 ) ) ;
#109138 = AXIS2_PLACEMENT_3D ( 'NONE', #42306, #160982, #181815 ) ;
#109139 = LINE ( 'NONE', #49177, #214405 ) ;
#109140 = ORIENTED_EDGE ( 'NONE', *, *, #229983, .F. ) ;
#109141 = CARTESIAN_POINT ( 'NONE',  ( -18.40000000000000213, 5.650000000011139001, -87.85000000000003695 ) ) ;
#109142 = DIRECTION ( 'NONE',  ( 0.000000000000000000, 0.000000000000000000, 1.000000000000000000 ) ) ;
#109143 = ORIENTED_EDGE ( 'NONE', *, *, #54050, .F. ) ;
#109144 = CARTESIAN_POINT ( 'NONE',  ( -16.93970660449832977, 10.01284139164673270, -146.5522817357944803 ) ) ;
#109145 = ADVANCED_FACE ( 'NONE', ( #112823 ), #213190, .F. ) ;
#109146 = ADVANCED_FACE ( 'NONE', ( #12457 ), #94525, .T. ) ;
#109147 = ORIENTED_EDGE ( 'NONE', *, *, #254102, .F. ) ;
#109148 = CARTESIAN_POINT ( 'NONE',  ( -16.83794237512075398, 44.28527064927406087, -235.2577326575541576 ) ) ;
#109149 = LINE ( 'NONE', #128740, #151320 ) ;
#109150 = EDGE_CURVE ( 'NONE', #5409, #28990, #252313, .T. ) ;
#109151 = AXIS2_PLACEMENT_3D ( 'NONE', #253352, #190855, #232541 ) ;
#109154 = ORIENTED_EDGE ( 'NONE', *, *, #110923, .T. ) ;
#109153 = ORIENTED_EDGE ( 'NONE', *, *, #169118, .T. ) ;
#109152 = DIRECTION ( 'NONE',  ( 0.000000000000000000, 0.2617529984165031243, 0.9651348961777157509 ) ) ;
#109155 = CARTESIAN_POINT ( 'NONE',  ( -23.25000000000000000, 67.23127455305841238, -235.8551265064783991 ) ) ;
#109156 = CARTESIAN_POINT ( 'NONE',  ( -22.47120815636973745, 0.02890382191504724946, -155.8500680112464920 ) ) ;
#109157 = ADVANCED_FACE ( 'NONE', ( #228924 ), #82278, .T. ) ;
#109158 = CARTESIAN_POINT ( 'NONE',  ( -20.94999999999999929, 18.62343931468261360, -223.9512205031617498 ) ) ;
#109160 = CARTESIAN_POINT ( 'NONE',  ( 20.85000000000000142, 68.92903212821327941, -132.7765432626560766 ) ) ;
#109159 = CARTESIAN_POINT ( 'NONE',  ( 21.04999999999998650, 6.650000000011155876, -79.25000000000004263 ) ) ;
#109162 = ADVANCED_FACE ( 'NONE', ( #174125 ), #198824, .T. ) ;
#109161 = DIRECTION ( 'NONE',  ( 0.000000000000000000, -6.454785026890385471E-15, 1.000000000000000000 ) ) ;
#109163 = CARTESIAN_POINT ( 'NONE',  ( 20.94999999999999929, -11.48912529306489994, -63.89999999999999858 ) ) ;
#109164 = AXIS2_PLACEMENT_3D ( 'NONE', #105960, #156705, #35474 ) ;
#109165 = ORIENTED_EDGE ( 'NONE', *, *, #200438, .F. ) ;
#109166 = ORIENTED_EDGE ( 'NONE', *, *, #161250, .T. ) ;
#109167 = ADVANCED_FACE ( 'NONE', ( #69867 ), #72432, .F. ) ;
#109168 = DIRECTION ( 'NONE',  ( 1.000000000000000000, 3.265361837132813093E-16, -0.000000000000000000 ) ) ;
#109170 = ORIENTED_EDGE ( 'NONE', *, *, #128919, .F. ) ;
#109169 = DIRECTION ( 'NONE',  ( 0.000000000000000000, 1.000000000000000000, -0.000000000000000000 ) ) ;
#109171 = ORIENTED_EDGE ( 'NONE', *, *, #207720, .T. ) ;
#109173 = CARTESIAN_POINT ( 'NONE',  ( 20.05000000000002913, 68.75000000001203659, -123.8731074845243540 ) ) ;
#109172 = VECTOR ( 'NONE', #95066, 1000.000000000000000 ) ;
#109174 = VERTEX_POINT ( 'NONE', #34588 ) ;
#109175 = CARTESIAN_POINT ( 'NONE',  ( 21.14999999999999858, 43.45833571831321507, -234.7657887233444001 ) ) ;
#109176 = ADVANCED_FACE ( 'NONE', ( #149406 ), #134917, .F. ) ;
#109177 = AXIS2_PLACEMENT_3D ( 'NONE', #258039, #59860, #141982 ) ;
#109178 = VERTEX_POINT ( 'NONE', #50261 ) ;
#109179 = AXIS2_PLACEMENT_3D ( 'NONE', #213998, #20956, #194454 ) ;
#109180 = CIRCLE ( 'NONE', #171774, 0.09999999999999939493 ) ;
#109181 = DIRECTION ( 'NONE',  ( -1.000000000000000000, -0.000000000000000000, 0.000000000000000000 ) ) ;
#109183 = ORIENTED_EDGE ( 'NONE', *, *, #62009, .F. ) ;
#109182 = ORIENTED_EDGE ( 'NONE', *, *, #202746, .F. ) ;
#109184 = ORIENTED_EDGE ( 'NONE', *, *, #222553, .F. ) ;
#109186 = DIRECTION ( 'NONE',  ( 0.000000000000000000, 0.8814952561688444987, -0.4721928772777320149 ) ) ;
#109185 = AXIS2_PLACEMENT_3D ( 'NONE', #63769, #28552, #7663 ) ;
#109187 = EDGE_LOOP ( 'NONE', ( #137024, #75298, #171450, #243197 ) ) ;
#109188 = VERTEX_POINT ( 'NONE', #35873 ) ;
#109189 = CARTESIAN_POINT ( 'NONE',  ( -16.87331047859649757, 14.15900158805613884, -219.2550725561364118 ) ) ;
#109190 = DIRECTION ( 'NONE',  ( 0.000000000000000000, -0.008583690987162452199, 0.9999631594459053030 ) ) ;
#109191 = CARTESIAN_POINT ( 'NONE',  ( -15.06720934482786234, 9.417690691074259490, -185.6416006967645274 ) ) ;
#109193 = ORIENTED_EDGE ( 'NONE', *, *, #102143, .T. ) ;
#109192 = DIRECTION ( 'NONE',  ( 0.000000000000000000, -1.000000000000000000, -6.982962677686266711E-15 ) ) ;
#109194 = CARTESIAN_POINT ( 'NONE',  ( -23.15000000000000213, -4.831324760611774849, -150.9696969421987660 ) ) ;
#109195 = LINE ( 'NONE', #111788, #45175 ) ;
#109197 = ORIENTED_EDGE ( 'NONE', *, *, #212768, .T. ) ;
#109196 = CARTESIAN_POINT ( 'NONE',  ( 21.30000000000002558, 40.35498466150055918, -247.8953732508333587 ) ) ;
#109199 = CARTESIAN_POINT ( 'NONE',  ( 20.94999999999999929, 8.629318835500072282, -209.3724661700624949 ) ) ;
#109198 = B_SPLINE_CURVE_WITH_KNOTS ( 'NONE', 3,
 ( #88722, #206131, #189133, #69211, #247822, #66621, #127881, #144855, #47030, #87448, #30086, #150027, #228270, #126591, #226975, #49618 ),
 .UNSPECIFIED., .F., .F.,
 ( 4, 3, 3, 3, 3, 4 ),
 ( 0.000000000000000000, 1.810570668009715449E-05, 2.740575833571675123E-05, 4.256816319436012815E-05, 5.213463471024871391E-05, 6.641585710718335726E-05 ),
 .UNSPECIFIED. ) ;
#109200 = ORIENTED_EDGE ( 'NONE', *, *, #226859, .F. ) ;
#109201 = DIRECTION ( 'NONE',  ( -1.073024830501117725E-15, 0.2617529984165031243, 0.9651348961777157509 ) ) ;
#109202 = AXIS2_PLACEMENT_3D ( 'NONE', #55655, #174415, #218599 ) ;
#109203 = ORIENTED_EDGE ( 'NONE', *, *, #247845, .F. ) ;
#109204 = VECTOR ( 'NONE', #121510, 1000.000000000000000 ) ;
#109205 = CARTESIAN_POINT ( 'NONE',  ( -21.05439746398122836, 18.83867787284056305, -226.6757208306117946 ) ) ;
#109206 = CARTESIAN_POINT ( 'NONE',  ( -16.86445178670663481, 30.24803992267471742, -234.8155353274968604 ) ) ;
#109208 = ORIENTED_EDGE ( 'NONE', *, *, #201488, .T. ) ;
#109207 = AXIS2_PLACEMENT_3D ( 'NONE', #85335, #222273, #223572 ) ;
#109209 = AXIS2_PLACEMENT_3D ( 'NONE', #235892, #54699, #136795 ) ;
#109211 = CARTESIAN_POINT ( 'NONE',  ( 20.85000000000000142, 69.15387683765952431, -132.7853812176745407 ) ) ;
#109210 = CARTESIAN_POINT ( 'NONE',  ( -21.53699400384058293, 75.99999999999440092, -210.3108192777700367 ) ) ;
#109212 = CIRCLE ( 'NONE', #196699, 0.09999999999999642508 ) ;
#109213 = LINE ( 'NONE', #188758, #222326 ) ;
#109214 = EDGE_CURVE ( 'NONE', #225193, #140280, #194764, .T. ) ;
#109215 = CYLINDRICAL_SURFACE ( 'NONE', #55474, 0.1000000000000028644 ) ;
#109216 = DIRECTION ( 'NONE',  ( -1.000000000000000000, 0.000000000000000000, 0.000000000000000000 ) ) ;
#109217 = ORIENTED_EDGE ( 'NONE', *, *, #227097, .F. ) ;
#109218 = ORIENTED_EDGE ( 'NONE', *, *, #72936, .T. ) ;
#109219 = AXIS2_PLACEMENT_3D ( 'NONE', #187267, #112846, #192384 ) ;
#109220 = DIRECTION ( 'NONE',  ( 1.000000000000000000, 0.000000000000000000, 0.000000000000000000 ) ) ;
#109221 = CYLINDRICAL_SURFACE ( 'NONE', #169128, 12.87499999999999822 ) ;
#109222 = VERTEX_POINT ( 'NONE', #9867 ) ;
#109223 = CARTESIAN_POINT ( 'NONE',  ( 21.05000000000000071, -8.730841121484171907, -177.0980747189843214 ) ) ;
#109224 = VERTEX_POINT ( 'NONE', #90678 ) ;
#109225 = DIRECTION ( 'NONE',  ( 0.000000000000000000, 0.000000000000000000, -1.000000000000000000 ) ) ;
#109226 = AXIS2_PLACEMENT_3D ( 'NONE', #80078, #141371, #220896 ) ;
#109227 = CARTESIAN_POINT ( 'NONE',  ( -21.05000000000000071, 56.16603649944111254, -228.1013850343386764 ) ) ;
#109228 = CYLINDRICAL_SURFACE ( 'NONE', #15900, 0.1000000000000028644 ) ;
#109229 = ORIENTED_EDGE ( 'NONE', *, *, #173040, .F. ) ;
#109230 = FACE_OUTER_BOUND ( 'NONE', #42783, .T. ) ;
#109231 = EDGE_CURVE ( 'NONE', #52358, #218161, #124019, .T. ) ;
#109232 = AXIS2_PLACEMENT_3D ( 'NONE', #208139, #86857, #89438 ) ;
#109233 = AXIS2_PLACEMENT_3D ( 'NONE', #237675, #166830, #246331 ) ;
#109234 = VERTEX_POINT ( 'NONE', #93249 ) ;
#109236 = ORIENTED_EDGE ( 'NONE', *, *, #115294, .T. ) ;
#109235 = TOROIDAL_SURFACE ( 'NONE', #188357, 0.2000000000000000111, 0.1000000000000000056 ) ;
#109237 = ORIENTED_EDGE ( 'NONE', *, *, #176025, .T. ) ;
#109238 = CARTESIAN_POINT ( 'NONE',  ( 22.49999999999999645, 64.35012909624795441, -136.6056273753972903 ) ) ;
#109239 = CARTESIAN_POINT ( 'NONE',  ( 18.69999999999999929, 0.000000000000000000, 0.000000000000000000 ) ) ;
#109240 = CARTESIAN_POINT ( 'NONE',  ( -16.87683809663752399, 66.15000000001225544, -149.9254715027207396 ) ) ;
#109241 = DIRECTION ( 'NONE',  ( 0.000000000000000000, 0.000000000000000000, -1.000000000000000000 ) ) ;
#109242 = FACE_OUTER_BOUND ( 'NONE', #39313, .T. ) ;
#109244 = CARTESIAN_POINT ( 'NONE',  ( -23.25000000000000000, 36.65892442174472876, -249.5511627012454596 ) ) ;
#109243 = DIRECTION ( 'NONE',  ( 1.000000000000000000, -0.000000000000000000, -0.000000000000000000 ) ) ;
#109246 = VERTEX_POINT ( 'NONE', #172847 ) ;
#109245 = DIRECTION ( 'NONE',  ( 0.000000000000000000, 0.000000000000000000, -1.000000000000000000 ) ) ;
#109247 = FACE_OUTER_BOUND ( 'NONE', #41167, .T. ) ;
#109248 = ORIENTED_EDGE ( 'NONE', *, *, #255694, .T. ) ;
#109249 = DIRECTION ( 'NONE',  ( 0.000000000000000000, 0.9887567792719341719, -0.1495327102803664099 ) ) ;
#109250 = EDGE_LOOP ( 'NONE', ( #91921, #234729, #246807, #250704 ) ) ;
#109251 = EDGE_LOOP ( 'NONE', ( #117403, #61433, #189357, #10933 ) ) ;
#109252 = CARTESIAN_POINT ( 'NONE',  ( -21.05000000000000071, 43.51422117117169108, -240.0698702536254530 ) ) ;
#109253 = DIRECTION ( 'NONE',  ( 1.000000000000000000, 0.000000000000000000, 0.000000000000000000 ) ) ;
#109254 = CARTESIAN_POINT ( 'NONE',  ( 18.49999999999999289, 10.25000000001115552, -121.8500000000000369 ) ) ;
#109255 = DIRECTION ( 'NONE',  ( 0.000000000000000000, 0.9274965247785529332, -0.3738317757009255171 ) ) ;
#109256 = VECTOR ( 'NONE', #247489, 1000.000000000000000 ) ;
#109257 = CARTESIAN_POINT ( 'NONE',  ( 0.9000000000000547562, 66.35000000001119247, -10.02310748452479139 ) ) ;
#109258 = ORIENTED_EDGE ( 'NONE', *, *, #196761, .T. ) ;
#109259 = ORIENTED_EDGE ( 'NONE', *, *, #46650, .T. ) ;
#109260 = DIRECTION ( 'NONE',  ( 0.000000000000000000, 0.000000000000000000, 1.000000000000000000 ) ) ;
#109261 = VERTEX_POINT ( 'NONE', #71149 ) ;
#109262 = DIRECTION ( 'NONE',  ( -1.000000000000000000, 0.000000000000000000, 0.000000000000000000 ) ) ;
#109263 = FACE_OUTER_BOUND ( 'NONE', #250603, .T. ) ;
#109264 = VERTEX_POINT ( 'NONE', #230198 ) ;
#109265 = CARTESIAN_POINT ( 'NONE',  ( 20.99999999999999645, 51.70063031245850027, -232.1289905089708441 ) ) ;
#109266 = LINE ( 'NONE', #7618, #229420 ) ;
#109267 = FACE_OUTER_BOUND ( 'NONE', #52156, .T. ) ;
#109268 = CARTESIAN_POINT ( 'NONE',  ( 18.39999999999999858, -9.599999999988845900, -140.6001893912220737 ) ) ;
#109269 = ORIENTED_EDGE ( 'NONE', *, *, #131571, .T. ) ;
#109270 = DIRECTION ( 'NONE',  ( 0.000000000000000000, 0.4999999999999956701, -0.8660254037844411501 ) ) ;
#109271 = DIRECTION ( 'NONE',  ( 0.000000000000000000, 0.1350103645451904977, -0.9908441862701596881 ) ) ;
#109272 = CARTESIAN_POINT ( 'NONE',  ( 18.59999999999999076, 28.91254064196106910, -237.8576372133405528 ) ) ;
#109273 = CARTESIAN_POINT ( 'NONE',  ( 20.94999999999999574, 4.459011116736869340, -245.2267018908137857 ) ) ;
#109274 = EDGE_CURVE ( 'NONE', #68660, #178487, #151978, .T. ) ;
#109275 = DIRECTION ( 'NONE',  ( 1.000000000000000000, 0.000000000000000000, 0.000000000000000000 ) ) ;
#109277 = VERTEX_POINT ( 'NONE', #111539 ) ;
#109276 = AXIS2_PLACEMENT_3D ( 'NONE', #84579, #122489, #123767 ) ;
#109278 = ADVANCED_FACE ( 'NONE', ( #191100 ), #91967, .F. ) ;
#109279 = CARTESIAN_POINT ( 'NONE',  ( 21.05000012384952868, 10.62872029887554604, -12.17797733003523497 ) ) ;
#109280 = ORIENTED_EDGE ( 'NONE', *, *, #201847, .T. ) ;
#109281 = CARTESIAN_POINT ( 'NONE',  ( 20.94999999999999929, 8.776282895303632259, -155.2500000000000284 ) ) ;
#109282 = ADVANCED_FACE ( 'NONE', ( #158402 ), #175394, .F. ) ;
#109283 = DIRECTION ( 'NONE',  ( 0.000000000000000000, -0.2128009952263403282, 0.9770955615653358350 ) ) ;
#109284 = DIRECTION ( 'NONE',  ( 0.000000000000000000, 0.000000000000000000, 1.000000000000000000 ) ) ;
#109285 = DIRECTION ( 'NONE',  ( 0.000000000000000000, 0.9770955615653313941, 0.2128009952263603677 ) ) ;
#109286 = VERTEX_POINT ( 'NONE', #237897 ) ;
#109287 = DIRECTION ( 'NONE',  ( 1.000000000000000000, 0.000000000000000000, 0.000000000000000000 ) ) ;
#109288 = CARTESIAN_POINT ( 'NONE',  ( -18.50000000000000000, 9.150000000000002132, 11.75000000000000000 ) ) ;
#109289 = DIRECTION ( 'NONE',  ( 0.000000000000000000, 0.000000000000000000, 1.000000000000000000 ) ) ;
#109290 = DIRECTION ( 'NONE',  ( 1.000000000000000000, 0.000000000000000000, 0.000000000000000000 ) ) ;
#109291 = TOROIDAL_SURFACE ( 'NONE', #254976, 0.2000000000000000111, 0.1000000000000000056 ) ;
#109292 = EDGE_CURVE ( 'NONE', #250592, #173747, #77513, .T. ) ;
#109294 = DIRECTION ( 'NONE',  ( 1.000000000000000000, 0.000000000000000000, 0.000000000000000000 ) ) ;
#109293 = AXIS2_PLACEMENT_3D ( 'NONE', #95275, #99101, #219059 ) ;
#109295 = ORIENTED_EDGE ( 'NONE', *, *, #31957, .T. ) ;
#109296 = ORIENTED_EDGE ( 'NONE', *, *, #228972, .T. ) ;
#109297 = LINE ( 'NONE', #106731, #170854 ) ;
#109299 = CARTESIAN_POINT ( 'NONE',  ( 22.10000000000000497, -11.65000000000000036, -15.00000000000000000 ) ) ;
#109298 = CIRCLE ( 'NONE', #71918, 0.09999999999999939493 ) ;
#109300 = DIRECTION ( 'NONE',  ( 1.000000000000000000, 2.952720810173289112E-16, -0.000000000000000000 ) ) ;
#109301 = CARTESIAN_POINT ( 'NONE',  ( -16.88495309932519817, 44.11948899812239233, -235.3010259908169814 ) ) ;
#109302 = ADVANCED_FACE ( 'NONE', ( #220891 ), #59217, .F. ) ;
#109303 = EDGE_LOOP ( 'NONE', ( #93459, #244449, #140939, #63191 ) ) ;
#109304 = CARTESIAN_POINT ( 'NONE',  ( 22.49533356619861379, 11.65000000631534149, -33.43487741967727800 ) ) ;
#109305 = ITEM_DEFINED_TRANSFORMATION ( 'NONE', 'NONE', #69450,  #2425 ) ;
#109306 = LINE ( 'NONE', #28559, #171636 ) ;
#109307 = CIRCLE ( 'NONE', #5238, 0.1000000000000028644 ) ;
#109308 = ORIENTED_EDGE ( 'NONE', *, *, #150235, .F. ) ;
#109309 = AXIS2_PLACEMENT_3D ( 'NONE', #188999, #213686, #209852 ) ;
#109310 = ORIENTED_EDGE ( 'NONE', *, *, #172636, .T. ) ;
#109311 = ORIENTED_EDGE ( 'NONE', *, *, #33415, .T. ) ;
#109312 = AXIS2_PLACEMENT_3D ( 'NONE', #104258, #246365, #145964 ) ;
#109313 = ORIENTED_EDGE ( 'NONE', *, *, #17126, .F. ) ;
#109314 = DIRECTION ( 'NONE',  ( -1.000000000000000000, 0.000000000000000000, 0.000000000000000000 ) ) ;
#109315 = FACE_OUTER_BOUND ( 'NONE', #62022, .T. ) ;
#109316 = CARTESIAN_POINT ( 'NONE',  ( -21.05000000000000071, 74.16465844978787914, -158.3679561919613832 ) ) ;
#109317 = EDGE_CURVE ( 'NONE', #81658, #212844, #194945, .T. ) ;
#109318 = DIRECTION ( 'NONE',  ( 1.000000000000000000, 0.000000000000000000, 0.000000000000000000 ) ) ;
#109320 = AXIS2_PLACEMENT_3D ( 'NONE', #232803, #35885, #77526 ) ;
#109319 = CARTESIAN_POINT ( 'NONE',  ( 18.59999999999999076, 63.62814136979439184, -224.4990371885399441 ) ) ;
#109322 = FACE_OUTER_BOUND ( 'NONE', #101518, .T. ) ;
#109321 = AXIS2_PLACEMENT_3D ( 'NONE', #128678, #152105, #249898 ) ;
#109325 = FACE_OUTER_BOUND ( 'NONE', #86007, .T. ) ;
#109324 = TOROIDAL_SURFACE ( 'NONE', #25970, 0.2000000000000000111, 0.1000000000000000056 ) ;
#109323 = DIRECTION ( 'NONE',  ( 1.000000000000000000, -0.000000000000000000, -0.000000000000000000 ) ) ;
#109326 = CARTESIAN_POINT ( 'NONE',  ( 18.59999999999999432, 77.29973367124354411, -213.4949779616549392 ) ) ;
#109327 = CARTESIAN_POINT ( 'NONE',  ( -18.40000000000000213, 64.52683809664949877, -112.2731074845243739 ) ) ;
#109328 = CARTESIAN_POINT ( 'NONE',  ( -18.40000000000000213, 11.47316190337364183, -91.17405393319209850 ) ) ;
#109329 = DIRECTION ( 'NONE',  ( 0.000000000000000000, 6.982962677686266711E-15, -1.000000000000000000 ) ) ;
#109330 = ORIENTED_EDGE ( 'NONE', *, *, #509, .F. ) ;
#109331 = EDGE_LOOP ( 'NONE', ( #185922, #44732, #200455, #8460, #157378, #219839 ) ) ;
#109332 = CARTESIAN_POINT ( 'NONE',  ( -20.99749315643149217, 11.75000000001115197, -93.48519423124027128 ) ) ;
#109333 = DIRECTION ( 'NONE',  ( 1.000000000000000000, 0.000000000000000000, 0.000000000000000000 ) ) ;
#109335 = FACE_OUTER_BOUND ( 'NONE', #91936, .T. ) ;
#109334 = DIRECTION ( 'NONE',  ( -2.940209281316621016E-16, 1.000000000000000000, 0.000000000000000000 ) ) ;
#109336 = EDGE_CURVE ( 'NONE', #243465, #148976, #28178, .T. ) ;
#109337 = DIRECTION ( 'NONE',  ( 0.000000000000000000, -6.982962677686266711E-15, 1.000000000000000000 ) ) ;
#109338 = CARTESIAN_POINT ( 'NONE',  ( 23.14999999999999503, 11.65000000001116298, -54.85000000000000142 ) ) ;
#109339 = DIRECTION ( 'NONE',  ( 0.000000000000000000, -0.1298341882520022694, -0.9915357197604853789 ) ) ;
#109340 = ORIENTED_EDGE ( 'NONE', *, *, #247380, .F. ) ;
#109341 = EDGE_CURVE ( 'NONE', #163056, #226489, #165724, .T. ) ;
#109342 = ORIENTED_EDGE ( 'NONE', *, *, #247463, .F. ) ;
#109343 = CARTESIAN_POINT ( 'NONE',  ( -15.06720934482788365, 9.417690691063098640, -18.14160069676458420 ) ) ;
#109344 = ORIENTED_EDGE ( 'NONE', *, *, #145562, .T. ) ;
#109345 = EDGE_CURVE ( 'NONE', #30986, #25213, #199009, .T. ) ;
#109346 = CARTESIAN_POINT ( 'NONE',  ( -20.94999999999999929, 16.98881331171929787, -224.4946931418895417 ) ) ;
#109347 = VECTOR ( 'NONE', #74807, 999.9999999999998863 ) ;
#109348 = AXIS2_PLACEMENT_3D ( 'NONE', #134219, #135499, #215055 ) ;
#109349 = CARTESIAN_POINT ( 'NONE',  ( 18.39999999999999503, 64.52683809664901560, -45.27310748452439526 ) ) ;
#109350 = ORIENTED_EDGE ( 'NONE', *, *, #57069, .F. ) ;
#109351 = CARTESIAN_POINT ( 'NONE',  ( 21.14999999999999858, 10.71339244341104013, -146.3500000000000227 ) ) ;
#109352 = EDGE_CURVE ( 'NONE', #153125, #253128, #76248, .T. ) ;
#109353 = EDGE_LOOP ( 'NONE', ( #125576, #233217, #6463, #248161 ) ) ;
#109354 = CYLINDRICAL_SURFACE ( 'NONE', #24756, 0.1000000000000002554 ) ;
#109355 = DIRECTION ( 'NONE',  ( 0.000000000000000000, 1.000000000000000000, 0.000000000000000000 ) ) ;
#109357 = AXIS2_PLACEMENT_3D ( 'NONE', #45146, #105077, #184649 ) ;
#109356 = CARTESIAN_POINT ( 'NONE',  ( -23.25000000000000000, 6.268811756569107274, -220.3853799378769622 ) ) ;
#109358 = EDGE_CURVE ( 'NONE', #235470, #98958, #153089, .T. ) ;
#109359 = CARTESIAN_POINT ( 'NONE',  ( -21.05000000000000071, 1.115600667400684642E-11, -167.4999999999999716 ) ) ;
#109360 = EDGE_CURVE ( 'NONE', #98329, #85452, #107248, .T. ) ;
#109361 = FACE_OUTER_BOUND ( 'NONE', #198611, .T. ) ;
#109362 = DIRECTION ( 'NONE',  ( 0.000000000000000000, 0.000000000000000000, 1.000000000000000000 ) ) ;
#109363 = CIRCLE ( 'NONE', #1012, 0.09999999999998898659 ) ;
#109364 = CARTESIAN_POINT ( 'NONE',  ( 11.60000000000006004, 67.75000000001118394, -21.02310748452479316 ) ) ;
#109366 = DIRECTION ( 'NONE',  ( 1.000000000000000000, 0.000000000000000000, 0.000000000000000000 ) ) ;
#109365 = AXIS2_PLACEMENT_3D ( 'NONE', #186470, #83475, #24855 ) ;
#109367 = VECTOR ( 'NONE', #31305, 1000.000000000000000 ) ;
#109369 = ORIENTED_EDGE ( 'NONE', *, *, #89389, .T. ) ;
#109368 = DIRECTION ( 'NONE',  ( 0.000000000000000000, 0.000000000000000000, -1.000000000000000000 ) ) ;
#109371 = DIRECTION ( 'NONE',  ( -1.000000000000000000, 0.000000000000000000, 0.000000000000000000 ) ) ;
#109370 = DIRECTION ( 'NONE',  ( 0.000000000000000000, -0.2128009952263361926, 0.9770955615653368342 ) ) ;
#109372 = VERTEX_POINT ( 'NONE', #41014 ) ;
#109374 = ORIENTED_EDGE ( 'NONE', *, *, #76677, .F. ) ;
#109373 = DIRECTION ( 'NONE',  ( 0.000000000000000000, 0.000000000000000000, 1.000000000000000000 ) ) ;
#109375 = VERTEX_POINT ( 'NONE', #119253 ) ;
#109376 = LINE ( 'NONE', #188937, #237339 ) ;
#109377 = TOROIDAL_SURFACE ( 'NONE', #55188, 4.149999999999999467, 0.1000000000000000056 ) ;
#109378 = DIRECTION ( 'NONE',  ( -0.000000000000000000, -0.1350103645451945777, 0.9908441862701590219 ) ) ;
#109379 = AXIS2_PLACEMENT_3D ( 'NONE', #190251, #93701, #195399 ) ;
#109380 = EDGE_CURVE ( 'NONE', #212264, #61003, #120548, .T. ) ;
#109381 = CARTESIAN_POINT ( 'NONE',  ( 22.49436431346199683, 75.93309647028948461, -81.17305843217778261 ) ) ;
#109382 = PLANE ( 'NONE',  #143314 ) ;
#109383 = DIRECTION ( 'NONE',  ( 1.000000000000000000, 0.000000000000000000, 0.000000000000000000 ) ) ;
#109384 = EDGE_CURVE ( 'NONE', #51363, #247233, #78382, .T. ) ;
#109385 = EDGE_CURVE ( 'NONE', #138314, #7281, #21450, .T. ) ;
#109386 = CYLINDRICAL_SURFACE ( 'NONE', #95338, 0.09999999999999982514 ) ;
#109387 = AXIS2_PLACEMENT_3D ( 'NONE', #110215, #93220, #230168 ) ;
#109388 = CARTESIAN_POINT ( 'NONE',  ( 20.94999999999999929, -3.770473190032740174, -225.9805569534692324 ) ) ;
#109389 = VECTOR ( 'NONE', #6354, 1000.000000000000000 ) ;
#109390 = CYLINDRICAL_SURFACE ( 'NONE', #93499, 0.09999999999999781286 ) ;
#109391 = AXIS2_PLACEMENT_3D ( 'NONE', #25458, #71019, #9724 ) ;
#109392 = ORIENTED_EDGE ( 'NONE', *, *, #88169, .T. ) ;
#109393 = VERTEX_POINT ( 'NONE', #180505 ) ;
#109394 = FACE_OUTER_BOUND ( 'NONE', #84657, .T. ) ;
#109395 = ORIENTED_EDGE ( 'NONE', *, *, #36449, .F. ) ;
#109396 = CARTESIAN_POINT ( 'NONE',  ( -23.15000000000000213, 87.75000000001216449, -139.6231074845242688 ) ) ;
#109397 = ORIENTED_EDGE ( 'NONE', *, *, #150679, .F. ) ;
#109399 = CIRCLE ( 'NONE', #255101, 0.1000000000000033362 ) ;
#109398 = DIRECTION ( 'NONE',  ( 1.000000000000000000, 0.000000000000000000, 0.000000000000000000 ) ) ;
#109400 = CIRCLE ( 'NONE', #67908, 0.1000000000000016709 ) ;
#109401 = EDGE_CURVE ( 'NONE', #189304, #77283, #186565, .T. ) ;
#109402 = CARTESIAN_POINT ( 'NONE',  ( 19.90621891164687440, 11.75000000000000711, -24.82844527787753464 ) ) ;
#109403 = LINE ( 'NONE', #48154, #155491 ) ;
#109404 = ADVANCED_FACE ( 'NONE', ( #236604 ), #20147, .F. ) ;
#109405 = DIRECTION ( 'NONE',  ( 1.000000000000000000, 0.000000000000000000, 0.000000000000000000 ) ) ;
#109406 = CARTESIAN_POINT ( 'NONE',  ( 21.17356465864818915, 75.90108875899885277, -209.9459106107660489 ) ) ;
#109407 = ORIENTED_EDGE ( 'NONE', *, *, #118426, .F. ) ;
#109408 = DIRECTION ( 'NONE',  ( 0.000000000000000000, 7.116814260417668513E-15, -1.000000000000000000 ) ) ;
#109409 = DIRECTION ( 'NONE',  ( 0.000000000000000000, -1.084202172485473353E-14, 1.000000000000000000 ) ) ;
#109410 = EDGE_CURVE ( 'NONE', #125186, #89024, #244986, .T. ) ;
#109411 = CARTESIAN_POINT ( 'NONE',  ( -14.00000000000000178, 66.15000000001204228, -119.7731074845243739 ) ) ;
#109412 = CARTESIAN_POINT ( 'NONE',  ( -21.13498764882296044, 0.001656394742485969677, -27.00438185652605938 ) ) ;
#109413 = DIRECTION ( 'NONE',  ( 1.000000000000000000, 0.000000000000000000, 0.000000000000000000 ) ) ;
#109414 = ORIENTED_EDGE ( 'NONE', *, *, #166607, .T. ) ;
#109415 = DIRECTION ( 'NONE',  ( 0.000000000000000000, -1.000000000000000000, 0.000000000000000000 ) ) ;
#109416 = VERTEX_POINT ( 'NONE', #157101 ) ;
#109419 = ORIENTED_EDGE ( 'NONE', *, *, #90443, .T. ) ;
#109418 = CARTESIAN_POINT ( 'NONE',  ( 20.95346350065193519, 67.11282275083783588, -161.5113755374890445 ) ) ;
#109417 = CARTESIAN_POINT ( 'NONE',  ( -5.899999999999938183, 64.35000000001120668, -22.12310748452479103 ) ) ;
#109420 = CIRCLE ( 'NONE', #255117, 4.000000000000003553 ) ;
#109421 = CARTESIAN_POINT ( 'NONE',  ( 18.49999999999999645, 77.36242903720540198, -128.6342262366031548 ) ) ;
#109422 = AXIS2_PLACEMENT_3D ( 'NONE', #17859, #218622, #846 ) ;
#109423 = CARTESIAN_POINT ( 'NONE',  ( 21.05000000000000071, 71.00000000001223555, -148.9283735034374843 ) ) ;
#109424 = DIRECTION ( 'NONE',  ( -0.000000000000000000, 0.9876197685951276783, 0.1568667991644721316 ) ) ;
#109425 = ORIENTED_EDGE ( 'NONE', *, *, #14446, .T. ) ;
#109426 = DIRECTION ( 'NONE',  ( 1.000000000000000000, 0.000000000000000000, 0.000000000000000000 ) ) ;
#109427 = DIRECTION ( 'NONE',  ( -1.000000000000000000, 0.000000000000000000, 0.000000000000000000 ) ) ;
#109429 = FACE_OUTER_BOUND ( 'NONE', #81133, .T. ) ;
#109428 = DIRECTION ( 'NONE',  ( 1.000000000000000000, 0.000000000000000000, 0.000000000000000000 ) ) ;
#109431 = EDGE_LOOP ( 'NONE', ( #82221, #82709, #122685, #38126 ) ) ;
#109430 = CARTESIAN_POINT ( 'NONE',  ( -21.14999999999999858, 1.627786319807483340, -244.0021210468063089 ) ) ;
#109432 = ADVANCED_FACE ( 'NONE', ( #98343 ), #177942, .T. ) ;
#109433 = ORIENTED_EDGE ( 'NONE', *, *, #176292, .T. ) ;
#109434 = EDGE_CURVE ( 'NONE', #137392, #25096, #132566, .T. ) ;
#109435 = CARTESIAN_POINT ( 'NONE',  ( -18.41431012584569160, 11.48747202921932242, -109.7267639868983480 ) ) ;
#109436 = CIRCLE ( 'NONE', #1085, 0.1000000000000028644 ) ;
#109437 = DIRECTION ( 'NONE',  ( 0.000000000000000000, -1.000000000000000000, -1.734723475976807292E-15 ) ) ;
#109438 = CARTESIAN_POINT ( 'NONE',  ( 18.59999999999999787, -1.835341550213255957, -145.6551512925629766 ) ) ;
#109439 = ORIENTED_EDGE ( 'NONE', *, *, #234546, .F. ) ;
#109440 = CARTESIAN_POINT ( 'NONE',  ( 21.05000000000000071, 44.10931966560507789, -259.0886734199950183 ) ) ;
#109441 = AXIS2_PLACEMENT_3D ( 'NONE', #39458, #198488, #117669 ) ;
#109442 = ADVANCED_FACE ( 'NONE', ( #65677 ), #190862, .F. ) ;
#109443 = DIRECTION ( 'NONE',  ( -0.000000000000000000, -0.1332476588733589318, 0.9910827722268049644 ) ) ;
#109444 = CARTESIAN_POINT ( 'NONE',  ( -23.24999999999999645, 37.94390843806124991, -261.1300795796834109 ) ) ;
#109445 = ORIENTED_EDGE ( 'NONE', *, *, #114435, .T. ) ;
#109446 = CARTESIAN_POINT ( 'NONE',  ( 20.19326291201597812, 59.46099628735877474, -225.7055034009678991 ) ) ;
#109447 = EDGE_CURVE ( 'NONE', #158778, #35933, #170028, .T. ) ;
#109448 = EDGE_CURVE ( 'NONE', #69009, #9522, #6989, .T. ) ;
#109449 = ORIENTED_EDGE ( 'NONE', *, *, #88207, .T. ) ;
#109450 = DIRECTION ( 'NONE',  ( 0.000000000000000000, -0.3488585713686463974, -0.9371753822965191993 ) ) ;
#109451 = DIRECTION ( 'NONE',  ( 0.000000000000000000, 0.4088369013363281623, -0.9126074666063771490 ) ) ;
#109452 = ADVANCED_FACE ( 'NONE', ( #25294, #202625 ), #224741, .F. ) ;
#109454 = VERTEX_POINT ( 'NONE', #103507 ) ;
#109453 = CIRCLE ( 'NONE', #205306, 11.89999999999999858 ) ;
#109455 = ORIENTED_EDGE ( 'NONE', *, *, #35578, .T. ) ;
#109457 = ADVANCED_FACE ( 'NONE', ( #201342 ), #220000, .T. ) ;
#109456 = EDGE_CURVE ( 'NONE', #17161, #35963, #167383, .T. ) ;
#109458 = CARTESIAN_POINT ( 'NONE',  ( 21.05000000000000071, 4.813084112160680661, -179.4415177565237798 ) ) ;
#109459 = ORIENTED_EDGE ( 'NONE', *, *, #182872, .F. ) ;
#109461 = ORIENTED_EDGE ( 'NONE', *, *, #16228, .F. ) ;
#109460 = CARTESIAN_POINT ( 'NONE',  ( 22.49999999999999645, 26.00793465928167691, -254.2726825744909718 ) ) ;
#109462 = EDGE_CURVE ( 'NONE', #9387, #25250, #236597, .T. ) ;
#109463 = VERTEX_POINT ( 'NONE', #43561 ) ;
#109466 = ORIENTED_EDGE ( 'NONE', *, *, #192718, .F. ) ;
#109465 = ORIENTED_EDGE ( 'NONE', *, *, #208248, .F. ) ;
#109464 = CARTESIAN_POINT ( 'NONE',  ( 22.39999999999999503, 59.71212129423884818, -233.8158665866020272 ) ) ;
#109467 = CARTESIAN_POINT ( 'NONE',  ( -18.50000000000000000, -9.399999999988850163, -107.3820418481727046 ) ) ;
#109468 = VECTOR ( 'NONE', #235348, 1000.000000000000000 ) ;
#109469 = VERTEX_POINT ( 'NONE', #184334 ) ;
#109470 = DIRECTION ( 'NONE',  ( 1.000000000000000000, 0.000000000000000000, -0.000000000000000000 ) ) ;
#109471 = EDGE_CURVE ( 'NONE', #165951, #256132, #65919, .T. ) ;
#109472 = ADVANCED_FACE ( 'NONE', ( #163503 ), #5680, .F. ) ;
#109473 = CARTESIAN_POINT ( 'NONE',  ( -20.64999999999999858, 2.400000000011155432, -87.27537807723794572 ) ) ;
#109474 = AXIS2_PLACEMENT_3D ( 'NONE', #170710, #113246, #130229 ) ;
#109475 = LINE ( 'NONE', #80604, #134314 ) ;
#109476 = EDGE_LOOP ( 'NONE', ( #63851, #120796, #54627, #6113 ) ) ;
#109477 = VERTEX_POINT ( 'NONE', #106065 ) ;
#109478 = CIRCLE ( 'NONE', #5415, 0.09999999999999605038 ) ;
#109479 = EDGE_CURVE ( 'NONE', #6436, #14418, #244308, .T. ) ;
#109480 = FACE_OUTER_BOUND ( 'NONE', #48113, .T. ) ;
#109481 =( BOUNDED_CURVE ( )  B_SPLINE_CURVE ( 3, ( #105643, #147368, #7875, #207356 ),
 .UNSPECIFIED., .F., .F. ) 
 B_SPLINE_CURVE_WITH_KNOTS ( ( 4, 4 ),
 ( 0.000000000000000000, 1.570796326794916320 ),
 .UNSPECIFIED. ) 
 CURVE ( )  GEOMETRIC_REPRESENTATION_ITEM ( )  RATIONAL_B_SPLINE_CURVE ( ( 1.000000000000000000, 0.8047378541243603856, 0.8047378541243603856, 1.000000000000000000 ) ) 
 REPRESENTATION_ITEM ( '' )  );
#109483 = ORIENTED_EDGE ( 'NONE', *, *, #15830, .F. ) ;
#109482 = DIRECTION ( 'NONE',  ( 0.000000000000000000, -0.01283462868042125823, -0.9999176327611367654 ) ) ;
#109484 = DIRECTION ( 'NONE',  ( 0.000000000000000000, 6.982962677686266711E-15, -1.000000000000000000 ) ) ;
#109486 = EDGE_LOOP ( 'NONE', ( #176093, #254913, #244494, #46449 ) ) ;
#109485 = LINE ( 'NONE', #230749, #198230 ) ;
#109487 = VERTEX_POINT ( 'NONE', #143928 ) ;
#109488 = EDGE_CURVE ( 'NONE', #180800, #224095, #53460, .T. ) ;
#109489 = CARTESIAN_POINT ( 'NONE',  ( 21.13736287352038445, 8.046642376395153562, -180.1499999999999773 ) ) ;
#109490 = ADVANCED_FACE ( 'NONE', ( #104773 ), #149151, .T. ) ;
#109491 = AXIS2_PLACEMENT_3D ( 'NONE', #113393, #75574, #233366 ) ;
#109492 = ORIENTED_EDGE ( 'NONE', *, *, #199839, .T. ) ;
#109493 = B_SPLINE_CURVE_WITH_KNOTS ( 'NONE', 3,
 ( #23858, #241588, #147623, #188045, #126777, #165930, #9388, #203749, #221996, #145045, #164628, #146326, #206322, #48520 ),
 .UNSPECIFIED., .F., .F.,
 ( 4, 2, 2, 2, 2, 2, 4 ),
 ( 0.000000000000000000, 2.389617747646909451E-05, 4.779235495293818902E-05, 9.558470990583940675E-05, 0.0001911694198115973086, 0.0003823388396230649466, 0.0007646776792459603241 ),
 .UNSPECIFIED. ) ;
#109494 = CARTESIAN_POINT ( 'NONE',  ( -16.92973740335358457, 66.00749618554368681, -149.1170484493211177 ) ) ;
#109495 = DIRECTION ( 'NONE',  ( 0.000000000000000000, 0.9126074666063773710, 0.4088369013363274962 ) ) ;
#109497 = EDGE_LOOP ( 'NONE', ( #128602, #11852, #3943, #241907, #193414, #242574, #37709, #194133, #135034, #80185, #183073, #135329, #146840, #187089, #55990, #118127, #18739, #188019, #83082, #223916, #113322, #32244, #197752, #85174, #192878 ) ) ;
#109496 = ORIENTED_EDGE ( 'NONE', *, *, #70742, .F. ) ;
#109498 = VERTEX_POINT ( 'NONE', #166107 ) ;
#109499 = CARTESIAN_POINT ( 'NONE',  ( 21.05000000000000426, 6.258817194692626984, -33.46636726466636702 ) ) ;
#109500 = EDGE_LOOP ( 'NONE', ( #194688, #223049 ) ) ;
#109501 = ORIENTED_EDGE ( 'NONE', *, *, #145090, .F. ) ;
#109503 = DIRECTION ( 'NONE',  ( -0.000000000000000000, 0.4088369013363281623, -0.9126074666063771490 ) ) ;
#109502 = AXIS2_PLACEMENT_3D ( 'NONE', #107948, #66260, #87078 ) ;
#109505 = VERTEX_POINT ( 'NONE', #12157 ) ;
#109504 = DIRECTION ( 'NONE',  ( -1.000000000000000000, -0.000000000000000000, 0.000000000000000000 ) ) ;
#109506 = ADVANCED_FACE ( 'NONE', ( #250733 ), #252018, .F. ) ;
#109507 = CARTESIAN_POINT ( 'NONE',  ( -23.15000000000000213, 66.14499960962992020, -239.8604363256158933 ) ) ;
#109509 = CARTESIAN_POINT ( 'NONE',  ( -23.15000000000000213, 19.98118924431957311, -235.6825596947570602 ) ) ;
#109508 = DIRECTION ( 'NONE',  ( 9.044546369203336152E-15, 0.2438576117979363023, -0.9698110461157920525 ) ) ;
#109510 = CARTESIAN_POINT ( 'NONE',  ( 23.24999999999999645, 28.46934351190515855, -239.7465010792843714 ) ) ;
#109511 = CARTESIAN_POINT ( 'NONE',  ( -18.38817693311004575, 11.48149151591092476, -191.7499999999999716 ) ) ;
#109512 = ORIENTED_EDGE ( 'NONE', *, *, #196255, .F. ) ;
#109513 = AXIS2_PLACEMENT_3D ( 'NONE', #176379, #133386, #36883 ) ;
#109514 = CIRCLE ( 'NONE', #22065, 4.000000000000003553 ) ;
#109515 = VECTOR ( 'NONE', #100351, 1000.000000000000000 ) ;
#109516 = EDGE_LOOP ( 'NONE', ( #111473, #225707, #9957, #145773 ) ) ;
#109517 = VECTOR ( 'NONE', #128791, 1000.000000000000000 ) ;
#109518 = ADVANCED_FACE ( 'NONE', ( #31732 ), #151676, .T. ) ;
#109519 = CARTESIAN_POINT ( 'NONE',  ( -18.59999999999999787, 0.000000000000000000, 0.000000000000000000 ) ) ;
#109520 = CARTESIAN_POINT ( 'NONE',  ( 21.05000000000000071, 62.04148992963929032, -247.7470044306132024 ) ) ;
#109521 = ORIENTED_EDGE ( 'NONE', *, *, #152456, .T. ) ;
#109522 = ORIENTED_EDGE ( 'NONE', *, *, #40444, .F. ) ;
#109523 = ORIENTED_EDGE ( 'NONE', *, *, #158614, .T. ) ;
#109524 = LINE ( 'NONE', #70456, #225895 ) ;
#109525 = ADVANCED_FACE ( 'NONE', ( #73421 ), #212904, .T. ) ;
#109526 = CARTESIAN_POINT ( 'NONE',  ( -20.94999999999999929, -1.835341550224411922, -11.65515129256298010 ) ) ;
#109527 = EDGE_LOOP ( 'NONE', ( #858, #87480, #211487, #147389 ) ) ;
#109528 = FACE_OUTER_BOUND ( 'NONE', #69550, .T. ) ;
#109529 = ORIENTED_EDGE ( 'NONE', *, *, #194905, .T. ) ;
#109530 = FACE_OUTER_BOUND ( 'NONE', #212534, .T. ) ;
#109531 = CARTESIAN_POINT ( 'NONE',  ( -16.94107738177414291, 65.98576071487538286, -115.5731074845243711 ) ) ;
#109533 = CARTESIAN_POINT ( 'NONE',  ( -23.25000000000000000, 1.115600667400684642E-11, -69.10000000000000853 ) ) ;
#109532 = DIRECTION ( 'NONE',  ( -1.000000000000000000, 0.000000000000000000, 0.000000000000000000 ) ) ;
#109534 = CARTESIAN_POINT ( 'NONE',  ( 19.96984138294287092, 11.75000000001137934, -91.72457207120136502 ) ) ;
#109535 = CARTESIAN_POINT ( 'NONE',  ( 20.85000000000000142, -1.835859311443637010, -45.10443916879852821 ) ) ;
#109536 = DIRECTION ( 'NONE',  ( 0.7071067811865388020, -0.7071067811865561215, 0.000000000000000000 ) ) ;
#109537 = DIRECTION ( 'NONE',  ( 1.000000000000000000, -0.000000000000000000, 0.000000000000000000 ) ) ;
#109538 = AXIS2_PLACEMENT_3D ( 'NONE', #85140, #90300, #184273 ) ;
#109539 = ORIENTED_EDGE ( 'NONE', *, *, #178742, .F. ) ;
#109540 = EDGE_CURVE ( 'NONE', #87224, #191212, #70043, .T. ) ;
#109542 = ORIENTED_EDGE ( 'NONE', *, *, #157491, .T. ) ;
#109541 = ORIENTED_EDGE ( 'NONE', *, *, #227138, .T. ) ;
#109543 = ORIENTED_EDGE ( 'NONE', *, *, #218099, .F. ) ;
#109544 = CIRCLE ( 'NONE', #218242, 0.1000000000000008937 ) ;
#109545 = CYLINDRICAL_SURFACE ( 'NONE', #57750, 7.900000000000003908 ) ;
#109546 = CIRCLE ( 'NONE', #146952, 0.1999999999999987899 ) ;
#109547 = DIRECTION ( 'NONE',  ( 1.000000000000000000, 0.000000000000000000, 0.000000000000000000 ) ) ;
#109548 =( BOUNDED_SURFACE ( )  B_SPLINE_SURFACE ( 3, 2, ( 
 ( #244101, #167178, #65467 ),
 ( #101996, #45909, #246665 ),
 ( #68037, #125455, #26357 ),
 ( #181590, #105855, #86291 ) ),
 .UNSPECIFIED., .F., .F., .F. ) 
 B_SPLINE_SURFACE_WITH_KNOTS ( ( 4, 4 ),
 ( 3, 3 ),
 ( 1.570796326794896558, 3.141592653589793116 ),
 ( 0.000000000000000000, 1.000000000000000000 ),
 .UNSPECIFIED. ) 
 GEOMETRIC_REPRESENTATION_ITEM ( )  RATIONAL_B_SPLINE_SURFACE ( (
 ( 1.000000000000000000, 0.7071067811865475727, 1.000000000000000000),
 ( 1.000000000000000000, 0.6753870962079413509, 1.000000000000000000),
 ( 1.000000000000000000, 0.6438648806865591157, 1.000000000000000000),
 ( 1.000000000000000000, 0.6447402616204922499, 1.000000000000000000) ) ) 
 REPRESENTATION_ITEM ( '' )  SURFACE ( )  );
#109550 = DIRECTION ( 'NONE',  ( 0.000000000000000000, -0.9126074666063769270, -0.4088369013363280513 ) ) ;
#109549 = CARTESIAN_POINT ( 'NONE',  ( -21.05000000000000071, 1.115600667400684642E-11, -104.7999999999999972 ) ) ;
#109551 = DIRECTION ( 'NONE',  ( 0.000000000000000000, 0.9994937237965558774, 0.03181660087586650476 ) ) ;
#109552 = ORIENTED_EDGE ( 'NONE', *, *, #108172, .F. ) ;
#109553 = AXIS2_PLACEMENT_3D ( 'NONE', #176051, #76913, #237289 ) ;
#109554 = DIRECTION ( 'NONE',  ( 1.000000000000000000, 0.000000000000000000, 0.000000000000000000 ) ) ;
#109555 = ORIENTED_EDGE ( 'NONE', *, *, #218833, .T. ) ;
#109556 = DIRECTION ( 'NONE',  ( 0.000000000000000000, 0.000000000000000000, 1.000000000000000000 ) ) ;
#109557 = TOROIDAL_SURFACE ( 'NONE', #176228, 0.2000000000000000111, 0.1000000000000000056 ) ;
#109558 = DIRECTION ( 'NONE',  ( 1.000000000000000000, 0.000000000000000000, 0.000000000000000000 ) ) ;
#109559 = AXIS2_PLACEMENT_3D ( 'NONE', #190992, #228822, #23259 ) ;
#109560 = CIRCLE ( 'NONE', #138751, 0.09999999999999939493 ) ;
#109561 = CARTESIAN_POINT ( 'NONE',  ( -21.05000000000000071, 1.626685360119048074, -230.7493234433891018 ) ) ;
#109562 = EDGE_LOOP ( 'NONE', ( #113655, #164775, #134728, #121056, #241642, #53645, #107082, #235034, #46994 ) ) ;
#109563 = FACE_OUTER_BOUND ( 'NONE', #89354, .T. ) ;
#109564 = VECTOR ( 'NONE', #210770, 999.9999999999998863 ) ;
#109565 = B_SPLINE_CURVE_WITH_KNOTS ( 'NONE', 3,
 ( #124597, #46315, #47596, #67181, #187151, #244521, #7185, #64598, #222363, #247081, #68471, #148004, #128438, #107578, #86712, #188405, #125851, #85414, #223665 ),
 .UNSPECIFIED., .F., .F.,
 ( 4, 3, 3, 3, 3, 3, 4 ),
 ( -2.000416914646550933E-06, 4.235164736271501695E-22, 4.714008503745888536E-05, 9.979203887778544059E-05, 0.0001372215519229606556, 0.0001635031576221011721, 0.0001900083748504231092 ),
 .UNSPECIFIED. ) ;
#109566 = CARTESIAN_POINT ( 'NONE',  ( -21.00000000000000000, 11.49641995933507843, 1.885425182446133885 ) ) ;
#109567 = EDGE_LOOP ( 'NONE', ( #38021, #149863, #152932, #181167 ) ) ;
#109568 = VERTEX_POINT ( 'NONE', #69554 ) ;
#109569 = FACE_OUTER_BOUND ( 'NONE', #231950, .T. ) ;
#109570 = DIRECTION ( 'NONE',  ( -0.7071067811865487940, 0.7071067811865463515, -7.215498431451184074E-16 ) ) ;
#109571 = DIRECTION ( 'NONE',  ( -0.000000000000000000, 0.4721928772777346239, 0.8814952561688430555 ) ) ;
#109572 = DIRECTION ( 'NONE',  ( 0.000000000000000000, 0.000000000000000000, -1.000000000000000000 ) ) ;
#109573 = DIRECTION ( 'NONE',  ( 0.000000000000000000, -6.467318590049456648E-15, 1.000000000000000000 ) ) ;
#109575 = AXIS2_PLACEMENT_3D ( 'NONE', #117625, #233733, #36840 ) ;
#109574 = DIRECTION ( 'NONE',  ( 0.000000000000000000, 0.000000000000000000, -1.000000000000000000 ) ) ;
#109576 = ORIENTED_EDGE ( 'NONE', *, *, #9369, .T. ) ;
#109577 = DIRECTION ( 'NONE',  ( -0.000000000000000000, -0.1350103645451835865, -0.9908441862701606873 ) ) ;
#109578 = CARTESIAN_POINT ( 'NONE',  ( -13.40000000000000213, -8.250000000000005329, 19.04142135623731491 ) ) ;
#109579 = AXIS2_PLACEMENT_3D ( 'NONE', #32147, #176786, #114225 ) ;
#109581 = CARTESIAN_POINT ( 'NONE',  ( 20.94999999999999929, 53.33306769324366314, -234.7945388949160872 ) ) ;
#109580 = CARTESIAN_POINT ( 'NONE',  ( -21.05000000000000071, -4.871452838297995136, -233.3782557782877518 ) ) ;
#109583 = EDGE_CURVE ( 'NONE', #185772, #184179, #178381, .T. ) ;
#109582 = DIRECTION ( 'NONE',  ( 0.000000000000000000, 0.000000000000000000, -1.000000000000000000 ) ) ;
#109584 = DIRECTION ( 'NONE',  ( 1.000000000000000000, 2.952720810173289112E-16, -0.000000000000000000 ) ) ;
#109585 = CIRCLE ( 'NONE', #59669, 12.87499999999999467 ) ;
#109586 = CARTESIAN_POINT ( 'NONE',  ( 18.49999999999999289, 10.20857864377385127, -121.8500000000000369 ) ) ;
#109587 = CARTESIAN_POINT ( 'NONE',  ( 21.97500000000000497, 66.25000000001253397, -182.3731074845244393 ) ) ;
#109589 = ORIENTED_EDGE ( 'NONE', *, *, #203920, .T. ) ;
#109588 = CARTESIAN_POINT ( 'NONE',  ( -22.10000000000000142, -3.262756495241484158E-15, 32.89999999999999858 ) ) ;
#109590 = AXIS2_PLACEMENT_3D ( 'NONE', #197987, #158897, #157632 ) ;
#109592 =( BOUNDED_SURFACE ( )  B_SPLINE_SURFACE ( 3, 2, ( 
 ( #238270, #239576, #161334 ),
 ( #60917, #240860, #59613 ),
 ( #122198, #100023, #3510 ),
 ( #62219, #141741, #235706 ),
 ( #57049, #17943, #40119 ),
 ( #136599, #139152, #216142 ) ),
 .UNSPECIFIED., .F., .F., .F. ) 
 B_SPLINE_SURFACE_WITH_KNOTS ( ( 4, 2, 4 ),
 ( 3, 3 ),
 ( -1.776356839400250465E-15, 0.7853981633974468357, 1.570796326794895448 ),
 ( 0.000000000000000000, 1.000000000000000000 ),
 .UNSPECIFIED. ) 
 GEOMETRIC_REPRESENTATION_ITEM ( )  RATIONAL_B_SPLINE_SURFACE ( (
 ( 1.000000000000000000, 0.4999999999999926170, 1.000000000000000000),
 ( 1.000000000000000000, 0.4993418825367712532, 1.000000000000000000),
 ( 1.000000000000000000, 0.5278258667012460936, 1.000000000000000000),
 ( 1.000000000000000000, 0.6092287576740391675, 1.000000000000000000),
 ( 1.000000000000000000, 0.6611148371745850794, 1.000000000000000000),
 ( 1.000000000000000000, 0.7071067811865597852, 1.000000000000000000) ) ) 
 REPRESENTATION_ITEM ( '' )  SURFACE ( )  );
#109591 = AXIS2_PLACEMENT_3D ( 'NONE', #220636, #42014, #4142 ) ;
#109593 = TOROIDAL_SURFACE ( 'NONE', #117965, 0.2000000000000000111, 0.1000000000000000056 ) ;
#109594 = CIRCLE ( 'NONE', #126145, 0.1000000000000054040 ) ;
#109595 = EDGE_CURVE ( 'NONE', #175634, #170209, #231201, .T. ) ;
#109596 = EDGE_CURVE ( 'NONE', #251611, #149929, #111713, .T. ) ;
#109597 = DIRECTION ( 'NONE',  ( 0.000000000000000000, 1.000000000000000000, 6.982962677686266711E-15 ) ) ;
#109598 = LINE ( 'NONE', #108334, #749 ) ;
#109599 = CARTESIAN_POINT ( 'NONE',  ( 20.10000000000000853, 4.645987002755569861, 21.91686199900910736 ) ) ;
#109601 = EDGE_CURVE ( 'NONE', #208658, #222829, #211647, .T. ) ;
#109600 = VECTOR ( 'NONE', #85673, 1000.000000000000000 ) ;
#109602 = ORIENTED_EDGE ( 'NONE', *, *, #114393, .F. ) ;
#109603 = CIRCLE ( 'NONE', #88742, 0.5000000000000004441 ) ;
#109604 = AXIS2_PLACEMENT_3D ( 'NONE', #38898, #118433, #257875 ) ;
#109606 = CARTESIAN_POINT ( 'NONE',  ( 18.59999999999999076, 19.00443933019177223, -232.7770257915295531 ) ) ;
#109605 = AXIS2_PLACEMENT_3D ( 'NONE', #175387, #179233, #237893 ) ;
#109607 = DIRECTION ( 'NONE',  ( 0.000000000000000000, -0.7397360091702823714, 0.6728971962616756564 ) ) ;
#109608 = DIRECTION ( 'NONE',  ( 1.000000000000000000, 0.000000000000000000, 0.000000000000000000 ) ) ;
#109609 = EDGE_CURVE ( 'NONE', #4179, #189559, #86738, .T. ) ;
#109611 = ORIENTED_EDGE ( 'NONE', *, *, #53433, .F. ) ;
#109610 = ADVANCED_FACE ( 'NONE', ( #193354 ), #74156, .F. ) ;
#109612 = DIRECTION ( 'NONE',  ( 0.000000000000000000, -6.938893903907222067E-15, 1.000000000000000000 ) ) ;
#109614 = ORIENTED_EDGE ( 'NONE', *, *, #122329, .F. ) ;
#109613 = CARTESIAN_POINT ( 'NONE',  ( 21.93642651522410603, 68.67283376068658640, -170.0231074845243882 ) ) ;
#109615 = DIRECTION ( 'NONE',  ( 0.000000000000000000, -0.9525900758537706459, 0.3042567129660534997 ) ) ;
#109616 = EDGE_CURVE ( 'NONE', #231419, #127836, #153264, .T. ) ;
#109617 = CARTESIAN_POINT ( 'NONE',  ( 21.05000000000000071, 87.75000000001173817, -72.62310748452422615 ) ) ;
#109618 = ORIENTED_EDGE ( 'NONE', *, *, #114140, .T. ) ;
#109619 = CARTESIAN_POINT ( 'NONE',  ( -20.54999999999999716, 54.27339256631721298, -236.8935360681107625 ) ) ;
#109620 = SHAPE_DEFINITION_REPRESENTATION ( #145016, #108449 ) ;
#109621 = CARTESIAN_POINT ( 'NONE',  ( -20.88420186297724257, 65.66974365629646115, -63.93601455626049557 ) ) ;
#109622 = CARTESIAN_POINT ( 'NONE',  ( -22.50000000000000000, 1.115600667400684642E-11, -33.39999999999999858 ) ) ;
#109624 = EDGE_CURVE ( 'NONE', #141624, #19886, #107432, .T. ) ;
#109623 = DIRECTION ( 'NONE',  ( 0.000000000000000000, 0.000000000000000000, -1.000000000000000000 ) ) ;
#109625 = ORIENTED_EDGE ( 'NONE', *, *, #9550, .T. ) ;
#109626 = DIRECTION ( 'NONE',  ( 1.000000000000000000, 0.000000000000000000, 0.000000000000000000 ) ) ;
#109627 = DIRECTION ( 'NONE',  ( -4.239556034732056743E-17, 0.1298341882520022694, 0.9915357197604853789 ) ) ;
#109628 = CIRCLE ( 'NONE', #255329, 0.1000000000000013933 ) ;
#109629 = FACE_OUTER_BOUND ( 'NONE', #129614, .T. ) ;
#109630 = EDGE_LOOP ( 'NONE', ( #172096, #119, #127384, #92239, #62154 ) ) ;
#109631 = VERTEX_POINT ( 'NONE', #253297 ) ;
#109632 = CARTESIAN_POINT ( 'NONE',  ( -18.40000000000000213, 70.35000000001201670, -115.6731074845243370 ) ) ;
#109633 = EDGE_CURVE ( 'NONE', #93167, #87114, #74718, .T. ) ;
#109634 = DIRECTION ( 'NONE',  ( -1.000000000000000000, 0.000000000000000000, 0.000000000000000000 ) ) ;
#109635 = DIRECTION ( 'NONE',  ( 0.000000000000000000, 0.000000000000000000, -1.000000000000000000 ) ) ;
#109636 = CARTESIAN_POINT ( 'NONE',  ( 20.94999999999999574, -1.261786168565025568, -8.086498963545480478 ) ) ;
#109638 = CARTESIAN_POINT ( 'NONE',  ( -18.59999999999999787, 74.25000000001259082, -191.8535959266227451 ) ) ;
#109637 = CARTESIAN_POINT ( 'NONE',  ( 23.14999999999999503, 64.35000000001173248, -81.27310748452440237 ) ) ;
#109639 = CARTESIAN_POINT ( 'NONE',  ( -21.14999999999999858, 76.00000000001242029, -176.5637644362255969 ) ) ;
#109640 = CARTESIAN_POINT ( 'NONE',  ( -18.41431012584569515, 64.51252797080381640, -112.2498714714227219 ) ) ;
#109642 = CARTESIAN_POINT ( 'NONE',  ( -18.52186455168912360, 46.94619712998765948, -255.3315249897759145 ) ) ;
#109641 = AXIS2_PLACEMENT_3D ( 'NONE', #100407, #222934, #160441 ) ;
#109643 = CIRCLE ( 'NONE', #59737, 0.09999999999998898659 ) ;
#109645 = ORIENTED_EDGE ( 'NONE', *, *, #85190, .T. ) ;
#109644 = CARTESIAN_POINT ( 'NONE',  ( -16.87851181299898684, 12.41404482784453656, -211.2427395888011006 ) ) ;
#109646 = CARTESIAN_POINT ( 'NONE',  ( -18.59999999999999787, -9.499999999988849808, -175.5999999999999659 ) ) ;
#109647 = DIRECTION ( 'NONE',  ( -1.000000000000000000, 0.000000000000000000, 0.000000000000000000 ) ) ;
#109648 = DIRECTION ( 'NONE',  ( 0.000000000000000000, -0.8814952561688476074, 0.4721928772777262417 ) ) ;
#109649 = ADVANCED_FACE ( 'NONE', ( #168691 ), #149093, .F. ) ;
#109650 = ORIENTED_EDGE ( 'NONE', *, *, #101479, .T. ) ;
#109651 = DIRECTION ( 'NONE',  ( 0.000000000000000000, 0.000000000000000000, 1.000000000000000000 ) ) ;
#109652 = DIRECTION ( 'NONE',  ( 0.000000000000000000, -7.056502275159890043E-15, 1.000000000000000000 ) ) ;
#109653 = DIRECTION ( 'NONE',  ( 1.000000000000000000, 0.000000000000000000, 0.000000000000000000 ) ) ;
#109654 = CARTESIAN_POINT ( 'NONE',  ( 23.14999999999998792, 64.35000000001268461, -203.5231074845244166 ) ) ;
#109655 = EDGE_LOOP ( 'NONE', ( #238638, #18322, #135167, #19717 ) ) ;
#109656 = B_SPLINE_CURVE_WITH_KNOTS ( 'NONE', 3,
 ( #112466, #214125, #190735, #53759, #51158, #75894, #232424, #35521 ),
 .UNSPECIFIED., .F., .F.,
 ( 4, 2, 2, 4 ),
 ( 0.000000000000000000, 0.0002114466876442058806, 0.0003171700314663111926, 0.0004228933752884164775 ),
 .UNSPECIFIED. ) ;
#109657 = VERTEX_POINT ( 'NONE', #189494 ) ;
#109659 = CIRCLE ( 'NONE', #251308, 0.09999999999998304689 ) ;
#109658 = CARTESIAN_POINT ( 'NONE',  ( -23.15000000000000213, 1.115600667400684642E-11, -98.50000000000004263 ) ) ;
#109660 = ORIENTED_EDGE ( 'NONE', *, *, #194135, .T. ) ;
#109661 = DIRECTION ( 'NONE',  ( 4.239556034732056743E-17, -0.1298341882520022694, -0.9915357197604852679 ) ) ;
#109662 = ORIENTED_EDGE ( 'NONE', *, *, #87750, .T. ) ;
#109663 = AXIS2_PLACEMENT_3D ( 'NONE', #186058, #174239, #95924 ) ;
#109664 = ADVANCED_FACE ( 'NONE', ( #10855 ), #130787, .F. ) ;
#109665 = PLANE ( 'NONE',  #197805 ) ;
#109666 = PLANE ( 'NONE',  #115057 ) ;
#109667 = AXIS2_PLACEMENT_3D ( 'NONE', #160626, #255796, #56337 ) ;
#109668 = DIRECTION ( 'NONE',  ( 1.000000000000000000, 0.000000000000000000, 0.000000000000000000 ) ) ;
#109669 = ORIENTED_EDGE ( 'NONE', *, *, #124949, .F. ) ;
#109670 = ADVANCED_FACE ( 'NONE', ( #77225 ), #237604, .T. ) ;
#109671 = DIRECTION ( 'NONE',  ( -1.000000000000000000, -0.000000000000000000, -0.000000000000000000 ) ) ;
#109672 = DIRECTION ( 'NONE',  ( -1.073024830501117923E-15, -0.9126074666063771490, -0.4088369013363281623 ) ) ;
#109673 = CIRCLE ( 'NONE', #9717, 0.1000000000000008799 ) ;
#109674 = ADVANCED_FACE ( 'NONE', ( #198467 ), #49167, .F. ) ;
#109676 = DIRECTION ( 'NONE',  ( 0.000000000000000000, 0.000000000000000000, -1.000000000000000000 ) ) ;
#109675 = CIRCLE ( 'NONE', #172279, 1.749999999999998002 ) ;
#109677 = EDGE_CURVE ( 'NONE', #182088, #60637, #36738, .T. ) ;
#109678 = DIRECTION ( 'NONE',  ( 0.000000000000000000, -1.000000000000000000, 0.000000000000000000 ) ) ;
#109679 = FACE_OUTER_BOUND ( 'NONE', #24878, .T. ) ;
#109680 = LINE ( 'NONE', #30180, #73915 ) ;
#109681 = ORIENTED_EDGE ( 'NONE', *, *, #118208, .F. ) ;
#109683 = FACE_OUTER_BOUND ( 'NONE', #157831, .T. ) ;
#109682 = DIRECTION ( 'NONE',  ( 0.000000000000000000, 6.982962677686266711E-15, -1.000000000000000000 ) ) ;
#109684 = VERTEX_POINT ( 'NONE', #1538 ) ;
#109686 = ORIENTED_EDGE ( 'NONE', *, *, #26163, .F. ) ;
#109685 = CARTESIAN_POINT ( 'NONE',  ( 20.94999999999999929, -5.637547571910522137, -233.4427589080015650 ) ) ;
#109687 = ORIENTED_EDGE ( 'NONE', *, *, #163832, .T. ) ;
#109688 = DIRECTION ( 'NONE',  ( 0.000000000000000000, 0.000000000000000000, 1.000000000000000000 ) ) ;
#109689 = CARTESIAN_POINT ( 'NONE',  ( 15.48841904831874849, 67.43841904833030299, -48.67310748452437963 ) ) ;
#109690 = FACE_OUTER_BOUND ( 'NONE', #83852, .T. ) ;
#109691 = EDGE_CURVE ( 'NONE', #161130, #92943, #215749, .T. ) ;
#109692 = CIRCLE ( 'NONE', #118070, 0.1000000000000075273 ) ;
#109693 = CARTESIAN_POINT ( 'NONE',  ( 18.59999999999999787, -1.835859311432481045, -179.0044391687985410 ) ) ;
#109694 = ORIENTED_EDGE ( 'NONE', *, *, #186639, .T. ) ;
#109695 = DIRECTION ( 'NONE',  ( 0.000000000000000000, 0.2617529984165029577, 0.9651348961777157509 ) ) ;
#109696 = AXIS2_PLACEMENT_3D ( 'NONE', #241469, #78523, #177672 ) ;
#109697 = VERTEX_POINT ( 'NONE', #199778 ) ;
#109698 = AXIS2_PLACEMENT_3D ( 'NONE', #226833, #45639, #185143 ) ;
#109699 = CIRCLE ( 'NONE', #176368, 0.09999999999999939493 ) ;
#109700 = CARTESIAN_POINT ( 'NONE',  ( 23.14999999999999858, 1.115600667400684642E-11, -67.00000000000004263 ) ) ;
#109701 = CIRCLE ( 'NONE', #238710, 11.80000000000000426 ) ;
#109702 = CARTESIAN_POINT ( 'NONE',  ( -21.05000000000000071, 74.16465844978715438, -57.96795619196134908 ) ) ;
#109703 = ORIENTED_EDGE ( 'NONE', *, *, #173598, .F. ) ;
#109704 = DIRECTION ( 'NONE',  ( 1.000000000000000000, 0.000000000000000000, 0.000000000000000000 ) ) ;
#109705 = EDGE_LOOP ( 'NONE', ( #131271, #142112, #195531, #207742, #239718 ) ) ;
#109706 = CARTESIAN_POINT ( 'NONE',  ( 18.55807992284871588, 65.67101464000501210, -97.44043916224792667 ) ) ;
#109707 = EDGE_LOOP ( 'NONE', ( #224351, #106853, #246113, #31802 ) ) ;
#109708 = LINE ( 'NONE', #228404, #233588 ) ;
#109709 = EDGE_CURVE ( 'NONE', #231654, #51680, #154258, .T. ) ;
#109710 = LINE ( 'NONE', #107152, #152335 ) ;
#109711 = FACE_OUTER_BOUND ( 'NONE', #181654, .T. ) ;
#109712 = EDGE_CURVE ( 'NONE', #158579, #195135, #36866, .T. ) ;
#109713 = DIRECTION ( 'NONE',  ( 0.000000000000000000, -7.056502275159890832E-15, 1.000000000000000000 ) ) ;
#109714 = AXIS2_PLACEMENT_3D ( 'NONE', #58972, #138509, #118992 ) ;
#109715 = VECTOR ( 'NONE', #122747, 1000.000000000000000 ) ;
#109716 = DIRECTION ( 'NONE',  ( -1.073024830501117725E-15, 6.982962677686266711E-15, -1.000000000000000000 ) ) ;
#109717 = CARTESIAN_POINT ( 'NONE',  ( -20.54999999999999716, 71.75000000001205080, -124.1731074845243228 ) ) ;
#109718 = AXIS2_PLACEMENT_3D ( 'NONE', #83369, #144644, #121288 ) ;
#109719 = EDGE_LOOP ( 'NONE', ( #160496, #175924, #29641, #11402 ) ) ;
#109720 = CARTESIAN_POINT ( 'NONE',  ( 18.39999999999999503, 64.25000000001222134, -145.7731074845244450 ) ) ;
#109721 = EDGE_LOOP ( 'NONE', ( #69832, #211388, #224825, #207971 ) ) ;
#109723 = CARTESIAN_POINT ( 'NONE',  ( 23.25000000000000000, -9.599999999988849453, -55.25000000000004974 ) ) ;
#109722 = DIRECTION ( 'NONE',  ( 1.000000000000000000, 0.000000000000000000, 0.000000000000000000 ) ) ;
#109724 = VERTEX_POINT ( 'NONE', #175109 ) ;
#109725 = DIRECTION ( 'NONE',  ( 1.000000000000000000, 0.000000000000000000, 0.000000000000000000 ) ) ;
#109726 = CIRCLE ( 'NONE', #117917, 11.74999999999999645 ) ;
#109727 = DIRECTION ( 'NONE',  ( 1.000000000000000000, 0.000000000000000000, 0.000000000000000000 ) ) ;
#109728 = CARTESIAN_POINT ( 'NONE',  ( -21.05000000000000071, 48.04585786805223080, -246.4610531646956417 ) ) ;
#109729 = AXIS2_PLACEMENT_3D ( 'NONE', #177566, #257010, #82238 ) ;
#109730 = ORIENTED_EDGE ( 'NONE', *, *, #39055, .F. ) ;
#109732 = ORIENTED_EDGE ( 'NONE', *, *, #61772, .F. ) ;
#109731 = CYLINDRICAL_SURFACE ( 'NONE', #241314, 0.09999999999999939493 ) ;
#109733 = CARTESIAN_POINT ( 'NONE',  ( -18.43707690579160641, 85.68240343348780641, -29.36626410711147273 ) ) ;
#109734 = CIRCLE ( 'NONE', #30657, 0.1000000000000008937 ) ;
#109736 = CARTESIAN_POINT ( 'NONE',  ( -16.89797118371619078, 66.02361927736880887, -190.9604008520841489 ) ) ;
#109735 = CARTESIAN_POINT ( 'NONE',  ( -23.25000000000000000, 30.38404434817536526, -239.4399867032565794 ) ) ;
#109738 = ORIENTED_EDGE ( 'NONE', *, *, #162795, .T. ) ;
#109737 = CARTESIAN_POINT ( 'NONE',  ( -20.64999999999999858, 7.150000000011155876, -112.8500000000000369 ) ) ;
#109739 = VECTOR ( 'NONE', #115242, 1000.000000000000000 ) ;
#109740 = CIRCLE ( 'NONE', #247097, 0.1000000000000028644 ) ;
#109741 = AXIS2_PLACEMENT_3D ( 'NONE', #213721, #35130, #232028 ) ;
#109742 = PRODUCT_DEFINITION_SHAPE ( 'NONE', 'NONE',  #228620 ) ;
#109743 = ORIENTED_EDGE ( 'NONE', *, *, #114815, .F. ) ;
#109744 = ADVANCED_FACE ( 'NONE', ( #233759 ), #17282, .F. ) ;
#109745 = CIRCLE ( 'NONE', #55549, 0.1000000000000132172 ) ;
#109746 = CARTESIAN_POINT ( 'NONE',  ( 23.15000000000000213, -11.48912529306489994, -131.0000000000000284 ) ) ;
#109747 = CARTESIAN_POINT ( 'NONE',  ( 21.05000000000000071, 67.07338541492478612, -94.55142446530125255 ) ) ;
#109748 = ORIENTED_EDGE ( 'NONE', *, *, #50257, .T. ) ;
#109749 = FACE_OUTER_BOUND ( 'NONE', #211296, .T. ) ;
#109750 = ORIENTED_EDGE ( 'NONE', *, *, #226100, .F. ) ;
#109751 = EDGE_CURVE ( 'NONE', #127544, #222677, #20334, .T. ) ;
#109752 = CARTESIAN_POINT ( 'NONE',  ( 21.05000000000000071, 12.71802988599559470, -223.5105008658000258 ) ) ;
#109753 = DIRECTION ( 'NONE',  ( 1.000000000000000000, 0.000000000000000000, 0.000000000000000000 ) ) ;
#109754 = AXIS2_PLACEMENT_3D ( 'NONE', #195599, #133048, #156486 ) ;
#109755 = EDGE_LOOP ( 'NONE', ( #211842, #206665, #239037, #110123, #251738 ) ) ;
#109756 = CARTESIAN_POINT ( 'NONE',  ( -18.59999999999999787, -11.75000000000000000, 30.09999999999999787 ) ) ;
#109757 = EDGE_CURVE ( 'NONE', #142016, #87394, #35576, .T. ) ;
#109758 = AXIS2_PLACEMENT_3D ( 'NONE', #209569, #169188, #70084 ) ;
#109759 = EDGE_CURVE ( 'NONE', #81489, #173014, #79779, .T. ) ;
#109760 = ORIENTED_EDGE ( 'NONE', *, *, #26455, .F. ) ;
#109761 = DIRECTION ( 'NONE',  ( 0.000000000000000000, -0.9910827722268055195, -0.1332476588733540468 ) ) ;
#109762 = VECTOR ( 'NONE', #218508, 1000.000000000000000 ) ;
#109763 = AXIS2_PLACEMENT_3D ( 'NONE', #240325, #82488, #139905 ) ;
#109764 = ADVANCED_FACE ( 'NONE', ( #218008 ), #74344, .T. ) ;
#109765 = EDGE_LOOP ( 'NONE', ( #207630, #40285 ) ) ;
#109766 = AXIS2_PLACEMENT_3D ( 'NONE', #242715, #199776, #21144 ) ;
#109767 = ORIENTED_EDGE ( 'NONE', *, *, #62432, .T. ) ;
#109769 = EDGE_CURVE ( 'NONE', #124376, #4366, #197175, .T. ) ;
#109768 = CARTESIAN_POINT ( 'NONE',  ( -18.59999994787167310, -9.523637689750295010, -73.88244953477273214 ) ) ;
#109770 = ORIENTED_EDGE ( 'NONE', *, *, #1581, .F. ) ;
#109771 = DIRECTION ( 'NONE',  ( 1.000000000000000000, 0.000000000000000000, 0.000000000000000000 ) ) ;
#109772 = EDGE_LOOP ( 'NONE', ( #201766, #256167, #250502, #234180 ) ) ;
#109774 = ORIENTED_EDGE ( 'NONE', *, *, #113080, .T. ) ;
#109773 = CARTESIAN_POINT ( 'NONE',  ( -21.65000000000000213, 7.250000000011139534, -154.8500000000000227 ) ) ;
#109775 = VERTEX_POINT ( 'NONE', #39430 ) ;
#109776 = DIRECTION ( 'NONE',  ( 0.000000000000000000, -0.000000000000000000, -1.000000000000000000 ) ) ;
#109777 = VERTEX_POINT ( 'NONE', #238887 ) ;
#109779 = ORIENTED_EDGE ( 'NONE', *, *, #114504, .T. ) ;
#109778 = ORIENTED_EDGE ( 'NONE', *, *, #257453, .F. ) ;
#109780 = CYLINDRICAL_SURFACE ( 'NONE', #94610, 0.5000000000000004441 ) ;
#109781 = DIRECTION ( 'NONE',  ( 0.000000000000000000, 0.2128009952263403282, -0.9770955615653358350 ) ) ;
#109783 = ORIENTED_EDGE ( 'NONE', *, *, #207836, .F. ) ;
#109782 = CIRCLE ( 'NONE', #247145, 0.9000000000000014655 ) ;
#109785 = EDGE_CURVE ( 'NONE', #136054, #79014, #16010, .T. ) ;
#109784 = CIRCLE ( 'NONE', #159886, 0.1000000000000028644 ) ;
#109786 = VECTOR ( 'NONE', #196400, 999.9999999999998863 ) ;
#109787 = EDGE_CURVE ( 'NONE', #256245, #45832, #82637, .T. ) ;
#109788 = ORIENTED_EDGE ( 'NONE', *, *, #189571, .T. ) ;
#109789 = ADVANCED_FACE ( 'NONE', ( #116379 ), #235040, .T. ) ;
#109790 = CARTESIAN_POINT ( 'NONE',  ( -21.05000000000282512, 69.50298221358175965, -203.5085617939581653 ) ) ;
#109792 = EDGE_LOOP ( 'NONE', ( #55483, #171119, #171996, #27709 ) ) ;
#109791 = LINE ( 'NONE', #207642, #174050 ) ;
#109793 = DIRECTION ( 'NONE',  ( 1.000000000000000000, 0.000000000000000000, 0.000000000000000000 ) ) ;
#109794 = VERTEX_POINT ( 'NONE', #56371 ) ;
#109795 = DIRECTION ( 'NONE',  ( 0.000000000000000000, 6.938893903907222067E-15, -1.000000000000000000 ) ) ;
#109796 = DIRECTION ( 'NONE',  ( -1.000000000000000000, 0.000000000000000000, 0.000000000000000000 ) ) ;
#109797 = VERTEX_POINT ( 'NONE', #96768 ) ;
#109799 = EDGE_CURVE ( 'NONE', #24108, #87934, #255827, .T. ) ;
#109798 = SPHERICAL_SURFACE ( 'NONE', #152548, 0.1000000000000000056 ) ;
#109800 = DIRECTION ( 'NONE',  ( 0.000000000000000000, 0.1495327102803792052, -0.9887567792719320625 ) ) ;
#109801 = ORIENTED_EDGE ( 'NONE', *, *, #9935, .F. ) ;
#109802 = ADVANCED_FACE ( 'NONE', ( #62809 ), #161810, .T. ) ;
#109804 = ORIENTED_EDGE ( 'NONE', *, *, #42594, .T. ) ;
#109803 = DIRECTION ( 'NONE',  ( 0.000000000000000000, -6.938893903907222067E-15, 1.000000000000000000 ) ) ;
#109805 = DIRECTION ( 'NONE',  ( 0.000000000000000000, 0.000000000000000000, 1.000000000000000000 ) ) ;
#109807 = ORIENTED_EDGE ( 'NONE', *, *, #21357, .T. ) ;
#109806 = EDGE_LOOP ( 'NONE', ( #247802, #79193, #121629, #161705 ) ) ;
#109808 = CIRCLE ( 'NONE', #163818, 1.749999999999999778 ) ;
#109809 = ORIENTED_EDGE ( 'NONE', *, *, #189737, .F. ) ;
#109810 = CARTESIAN_POINT ( 'NONE',  ( -23.15000000000000213, 64.35000000001258513, -191.3731074845244393 ) ) ;
#109811 = ORIENTED_EDGE ( 'NONE', *, *, #144735, .T. ) ;
#109812 = ORIENTED_EDGE ( 'NONE', *, *, #6986, .T. ) ;
#109813 = DIRECTION ( 'NONE',  ( 0.000000000000000000, 0.000000000000000000, -1.000000000000000000 ) ) ;
#109814 = ORIENTED_EDGE ( 'NONE', *, *, #189997, .F. ) ;
#109815 = EDGE_CURVE ( 'NONE', #83134, #70064, #105759, .T. ) ;
#109816 = CYLINDRICAL_SURFACE ( 'NONE', #152336, 0.09999999999999939493 ) ;
#109817 = DIRECTION ( 'NONE',  ( -1.000000000000000000, 0.000000000000000000, 0.000000000000000000 ) ) ;
#109818 = ORIENTED_EDGE ( 'NONE', *, *, #187097, .F. ) ;
#109819 = VERTEX_POINT ( 'NONE', #47078 ) ;
#109820 = EDGE_CURVE ( 'NONE', #232658, #113969, #153651, .T. ) ;
#109821 = DIRECTION ( 'NONE',  ( 0.000000000000000000, 0.8660254037844420383, -0.4999999999999943379 ) ) ;
#109822 = ORIENTED_EDGE ( 'NONE', *, *, #156571, .F. ) ;
#109823 = VECTOR ( 'NONE', #79514, 1000.000000000000000 ) ;
#109824 = AXIS2_PLACEMENT_3D ( 'NONE', #63344, #144161, #91599 ) ;
#109825 = CARTESIAN_POINT ( 'NONE',  ( 22.57320508075688537, 64.35000000001166143, -69.52310748452440237 ) ) ;
#109826 = ORIENTED_EDGE ( 'NONE', *, *, #139046, .F. ) ;
#109827 = CARTESIAN_POINT ( 'NONE',  ( 22.59999999999999787, 0.04781839071596408891, -122.2499775809528160 ) ) ;
#109828 = EDGE_CURVE ( 'NONE', #177518, #213781, #166101, .T. ) ;
#109830 = VERTEX_POINT ( 'NONE', #121534 ) ;
#109829 = DIRECTION ( 'NONE',  ( 2.952720810173289112E-16, 1.000000000000000000, -6.088138035986627436E-46 ) ) ;
#109831 = CARTESIAN_POINT ( 'NONE',  ( 18.59999999999999787, -9.399999999988843058, -207.8820418481726620 ) ) ;
#109832 = DIRECTION ( 'NONE',  ( -4.801466763864314121E-15, 0.2605042016806606298, 0.9654727137038736640 ) ) ;
#109833 = DIRECTION ( 'NONE',  ( 0.000000000000000000, -3.339342691255721203E-13, 1.000000000000000000 ) ) ;
#109834 = DIRECTION ( 'NONE',  ( 1.000000000000000000, 0.000000000000000000, 0.000000000000000000 ) ) ;
#109835 = CARTESIAN_POINT ( 'NONE',  ( -16.88560720703333473, 66.04943515626260364, -157.3749955636607183 ) ) ;
#109836 = CARTESIAN_POINT ( 'NONE',  ( -23.25000000000000000, 87.65000000001215597, -139.5231074845243029 ) ) ;
#109837 = DIRECTION ( 'NONE',  ( -1.000000000000000000, -2.952720810173289112E-16, 0.000000000000000000 ) ) ;
#109838 = DIRECTION ( 'NONE',  ( -0.000000000000000000, 0.000000000000000000, 1.000000000000000000 ) ) ;
#109839 = AXIS2_PLACEMENT_3D ( 'NONE', #16389, #136285, #60617 ) ;
#109840 = CARTESIAN_POINT ( 'NONE',  ( 23.15000000000000213, -8.663551401857999323, -157.9758988819327215 ) ) ;
#109841 = AXIS2_PLACEMENT_3D ( 'NONE', #108461, #238006, #47174 ) ;
#109842 = ORIENTED_EDGE ( 'NONE', *, *, #236076, .F. ) ;
#109843 = CIRCLE ( 'NONE', #134955, 0.5999999999999872102 ) ;
#109844 = AXIS2_PLACEMENT_3D ( 'NONE', #57168, #78033, #237120 ) ;
#109845 = ORIENTED_EDGE ( 'NONE', *, *, #33141, .T. ) ;
#109847 = ORIENTED_EDGE ( 'NONE', *, *, #40766, .T. ) ;
#109846 = DIRECTION ( 'NONE',  ( 0.000000000000000000, -1.000000000000000000, 0.000000000000000000 ) ) ;
#109848 = VERTEX_POINT ( 'NONE', #185327 ) ;
#109849 = CARTESIAN_POINT ( 'NONE',  ( -17.78241384941283343, 65.14442424720841984, -92.77406981203996850 ) ) ;
#109850 = CARTESIAN_POINT ( 'NONE',  ( 18.39999999999999503, 70.35000000001187459, -90.37310748452433984 ) ) ;
#109852 = DIRECTION ( 'NONE',  ( -1.000000000000000000, -0.000000000000000000, -0.000000000000000000 ) ) ;
#109851 = CARTESIAN_POINT ( 'NONE',  ( 20.72390388899080804, 39.18426925412079953, -236.8157669261957494 ) ) ;
#109853 = ORIENTED_EDGE ( 'NONE', *, *, #19151, .T. ) ;
#109854 = VERTEX_POINT ( 'NONE', #5373 ) ;
#109855 = VECTOR ( 'NONE', #69813, 1000.000000000000227 ) ;
#109856 = AXIS2_PLACEMENT_3D ( 'NONE', #86365, #130656, #248038 ) ;
#109858 = AXIS2_PLACEMENT_3D ( 'NONE', #130545, #87556, #27644 ) ;
#109857 = CYLINDRICAL_SURFACE ( 'NONE', #29321, 0.1000000000000013656 ) ;
#109859 = CYLINDRICAL_SURFACE ( 'NONE', #124692, 11.74999999999999645 ) ;
#109860 = VERTEX_POINT ( 'NONE', #204872 ) ;
#109861 = ORIENTED_EDGE ( 'NONE', *, *, #257859, .F. ) ;
#109862 = CARTESIAN_POINT ( 'NONE',  ( -16.77683809663752257, 9.945835743215301505, -180.1639490191041943 ) ) ;
#109863 = CARTESIAN_POINT ( 'NONE',  ( 21.00000000000000000, 66.25000000001199396, -115.2731074845243597 ) ) ;
#109864 = CARTESIAN_POINT ( 'NONE',  ( 21.05000000000000071, 65.27628318601533408, -61.92870824864008483 ) ) ;
#109865 = CIRCLE ( 'NONE', #72482, 0.1000000000000028644 ) ;
#109866 = CARTESIAN_POINT ( 'NONE',  ( -18.59999999999999787, 78.12133356376091342, -231.3112718935514636 ) ) ;
#109868 = ORIENTED_EDGE ( 'NONE', *, *, #163624, .F. ) ;
#109867 = DIRECTION ( 'NONE',  ( 0.000000000000000000, -0.9999176327611369874, 0.01283462868041987913 ) ) ;
#109869 = DIRECTION ( 'NONE',  ( 1.000000000000000000, 0.000000000000000000, 0.000000000000000000 ) ) ;
#109870 = CARTESIAN_POINT ( 'NONE',  ( 22.88900146558018989, 67.29609520889906094, -93.77310748452437394 ) ) ;
#109871 = CIRCLE ( 'NONE', #55876, 0.1000000000000001305 ) ;
#109872 = CARTESIAN_POINT ( 'NONE',  ( -21.05000000000000071, -1.835341550213257733, -78.55515129256303908 ) ) ;
#109873 = CARTESIAN_POINT ( 'NONE',  ( -16.89268316805465986, 9.951721813253337601, -54.35575247854554704 ) ) ;
#109875 = VERTEX_POINT ( 'NONE', #6682 ) ;
#109874 = AXIS2_PLACEMENT_3D ( 'NONE', #182865, #26340, #42061 ) ;
#109876 = CARTESIAN_POINT ( 'NONE',  ( -18.40000000000000213, 11.47316190337310893, -124.7001707515342872 ) ) ;
#109877 = CARTESIAN_POINT ( 'NONE',  ( 18.49999999999999289, 6.450000000011156587, -121.6500000000000341 ) ) ;
#109878 = CIRCLE ( 'NONE', #176553, 4.149999999999999467 ) ;
#109880 = DIRECTION ( 'NONE',  ( -1.000000000000000000, 0.000000000000000000, 0.000000000000000000 ) ) ;
#109879 = FACE_OUTER_BOUND ( 'NONE', #100845, .T. ) ;
#109882 = EDGE_CURVE ( 'NONE', #153561, #24271, #193844, .T. ) ;
#109881 = FACE_OUTER_BOUND ( 'NONE', #91725, .T. ) ;
#109883 = CARTESIAN_POINT ( 'NONE',  ( -16.83233564386402037, 9.930221796595782635, -54.22452066347574373 ) ) ;
#109884 = LINE ( 'NONE', #70803, #208129 ) ;
#109885 = DIRECTION ( 'NONE',  ( 0.000000000000000000, -0.000000000000000000, -1.000000000000000000 ) ) ;
#109886 = CYLINDRICAL_SURFACE ( 'NONE', #29898, 0.1000000000000028644 ) ;
#109887 = CARTESIAN_POINT ( 'NONE',  ( -21.08479644141223019, 69.65496134228024516, -136.5816619270885326 ) ) ;
#109888 = EDGE_LOOP ( 'NONE', ( #237773, #128065, #85866, #34894 ) ) ;
#109889 = ORIENTED_EDGE ( 'NONE', *, *, #180856, .F. ) ;
#109890 = VERTEX_POINT ( 'NONE', #245308 ) ;
#109891 = PLANE ( 'NONE',  #6998 ) ;
#109892 = CYLINDRICAL_SURFACE ( 'NONE', #148599, 7.899999999999990585 ) ;
#109893 = ORIENTED_EDGE ( 'NONE', *, *, #190569, .T. ) ;
#109894 = EDGE_CURVE ( 'NONE', #202583, #245309, #66104, .T. ) ;
#109895 = VERTEX_POINT ( 'NONE', #164494 ) ;
#109896 = VECTOR ( 'NONE', #140150, 1000.000000000000000 ) ;
#109897 =( NAMED_UNIT ( * ) SI_UNIT ( $, .STERADIAN. ) SOLID_ANGLE_UNIT ( ) );
#109898 = AXIS2_PLACEMENT_3D ( 'NONE', #26701, #144036, #243150 ) ;
#109899 = ORIENTED_EDGE ( 'NONE', *, *, #95841, .T. ) ;
#109900 = VECTOR ( 'NONE', #105494, 1000.000000000000114 ) ;
#109901 = DIRECTION ( 'NONE',  ( 0.000000000000000000, -1.000000000000000000, -1.734723475976807292E-15 ) ) ;
#109902 = ORIENTED_EDGE ( 'NONE', *, *, #78408, .T. ) ;
#109903 =( BOUNDED_CURVE ( )  B_SPLINE_CURVE ( 3, ( #11154, #127249, #28182, #167684 ),
 .UNSPECIFIED., .F., .T. ) 
 B_SPLINE_CURVE_WITH_KNOTS ( ( 4, 4 ),
 ( 1.570796326794908992, 2.617993877991514395 ),
 .UNSPECIFIED. ) 
 CURVE ( )  GEOMETRIC_REPRESENTATION_ITEM ( )  RATIONAL_B_SPLINE_CURVE ( ( 1.000000000000000000, 0.9106836025229576581, 0.9106836025229576581, 1.000000000000000000 ) ) 
 REPRESENTATION_ITEM ( '' )  );
#109904 = CARTESIAN_POINT ( 'NONE',  ( 21.00000000000000000, 9.750000000011153745, -54.75000000000000000 ) ) ;
#109905 = CARTESIAN_POINT ( 'NONE',  ( -16.83199318825829849, 30.08928172373351728, -234.7663019489722842 ) ) ;
#109906 = LINE ( 'NONE', #249450, #115165 ) ;
#109907 = VECTOR ( 'NONE', #44633, 1000.000000000000000 ) ;
#109908 = ADVANCED_FACE ( 'NONE', ( #244002 ), #53642, .F. ) ;
#109909 = AXIS2_PLACEMENT_3D ( 'NONE', #50519, #212206, #73998 ) ;
#109910 = SPHERICAL_SURFACE ( 'NONE', #154170, 0.1000000000000000056 ) ;
#109911 = ADVANCED_FACE ( 'NONE', ( #240179 ), #61534, .T. ) ;
#109912 = CARTESIAN_POINT ( 'NONE',  ( -21.05000000000000071, 1.835341550235567887, -112.1551512925630192 ) ) ;
#109914 = VERTEX_POINT ( 'NONE', #182774 ) ;
#109913 = CARTESIAN_POINT ( 'NONE',  ( -16.87683809663752399, 29.49590395944697363, -234.5399335999045718 ) ) ;
#109916 = FACE_OUTER_BOUND ( 'NONE', #250944, .T. ) ;
#109915 = CARTESIAN_POINT ( 'NONE',  ( 21.05000000000000071, 11.60000000000000497, -26.57179676972450366 ) ) ;
#109917 = FACE_OUTER_BOUND ( 'NONE', #239032, .T. ) ;
#109918 = ORIENTED_EDGE ( 'NONE', *, *, #222171, .F. ) ;
#109919 = DIRECTION ( 'NONE',  ( 0.000000000000000000, 0.000000000000000000, 1.000000000000000000 ) ) ;
#109920 = AXIS2_PLACEMENT_3D ( 'NONE', #45183, #128580, #188547 ) ;
#109922 = ADVANCED_FACE ( 'NONE', ( #65375, #22424 ), #101906, .T. ) ;
#109921 = CARTESIAN_POINT ( 'NONE',  ( -16.94226253665225457, 66.05000000001183480, -82.46984208014016815 ) ) ;
#109923 = CARTESIAN_POINT ( 'NONE',  ( 20.94999999999999929, 43.47002849391839874, -245.0086825852825143 ) ) ;
#109924 = EDGE_LOOP ( 'NONE', ( #20034, #42063, #11373 ) ) ;
#109925 = AXIS2_PLACEMENT_3D ( 'NONE', #219028, #61253, #45540 ) ;
#109926 = CARTESIAN_POINT ( 'NONE',  ( 21.05000000000000071, 67.23127455305841238, -235.8551265064783991 ) ) ;
#109927 = VECTOR ( 'NONE', #204581, 1000.000000000000227 ) ;
#109928 = ADVANCED_FACE ( 'NONE', ( #241456 ), #124084, .T. ) ;
#109929 = AXIS2_PLACEMENT_3D ( 'NONE', #88350, #182693, #180119 ) ;
#109930 = DIRECTION ( 'NONE',  ( 0.000000000000000000, -0.4088369013363276072, 0.9126074666063773710 ) ) ;
#109931 = EDGE_LOOP ( 'NONE', ( #224309, #127110, #101292, #187754 ) ) ;
#109932 = AXIS2_PLACEMENT_3D ( 'NONE', #233285, #92451, #214972 ) ;
#109933 = DIRECTION ( 'NONE',  ( 2.952720810173288619E-16, -1.000000000000000000, 0.000000000000000000 ) ) ;
#109934 = ADVANCED_FACE ( 'NONE', ( #251718 ), #73119, .F. ) ;
#109935 = DIRECTION ( 'NONE',  ( 1.000000000000000000, 0.000000000000000000, 0.000000000000000000 ) ) ;
#109936 = DIRECTION ( 'NONE',  ( 0.000000000000000000, 0.5868805631290315850, 0.8096735173027156396 ) ) ;
#109937 = ORIENTED_EDGE ( 'NONE', *, *, #158346, .F. ) ;
#109938 = VECTOR ( 'NONE', #165448, 1000.000000000000114 ) ;
#109939 = ORIENTED_EDGE ( 'NONE', *, *, #210130, .F. ) ;
#109940 = ADVANCED_FACE ( 'NONE', ( #109629 ), #124381, .T. ) ;
#109941 = DIRECTION ( 'NONE',  ( -2.252264143451594314E-15, 0.1298341882520054891, 0.9915357197604850459 ) ) ;
#109943 = AXIS2_PLACEMENT_3D ( 'NONE', #85417, #244524, #65897 ) ;
#109942 = DIRECTION ( 'NONE',  ( 0.000000000000000000, 0.9968797965484755830, 0.07893460099012303277 ) ) ;
#109944 = CARTESIAN_POINT ( 'NONE',  ( -20.94999999999999929, 70.15000000001266756, -193.3906102602464330 ) ) ;
#109945 = CARTESIAN_POINT ( 'NONE',  ( 21.05000000000000071, 1.115600667400684642E-11, -67.00000000000000000 ) ) ;
#109947 = DIRECTION ( 'NONE',  ( 0.000000000000000000, -0.8814952561688430555, 0.4721928772777346239 ) ) ;
#109946 = CARTESIAN_POINT ( 'NONE',  ( -20.64999999999999858, 45.00644278977874535, -237.9768835835062077 ) ) ;
#109948 = CARTESIAN_POINT ( 'NONE',  ( 20.94999999999999929, 7.128833340094563376, -233.7327013124401276 ) ) ;
#109949 = DIRECTION ( 'NONE',  ( 0.000000000000000000, -1.000000000000000000, -6.982962677686265922E-15 ) ) ;
#109950 = CARTESIAN_POINT ( 'NONE',  ( -21.29999999999995808, 1.115600667400684642E-11, -171.5499999999999829 ) ) ;
#109951 = CIRCLE ( 'NONE', #1793, 0.09999999999999939493 ) ;
#109952 = ORIENTED_EDGE ( 'NONE', *, *, #10489, .T. ) ;
#109953 = CARTESIAN_POINT ( 'NONE',  ( -20.86777300164945004, 65.66799936921530900, -97.42993998886008455 ) ) ;
#109954 = CIRCLE ( 'NONE', #234870, 11.89999999999999325 ) ;
#109956 = VERTEX_POINT ( 'NONE', #110924 ) ;
#109955 = LINE ( 'NONE', #14748, #246216 ) ;
#109957 = CIRCLE ( 'NONE', #197437, 0.09999999999999939493 ) ;
#109958 = CARTESIAN_POINT ( 'NONE',  ( 18.49999999999999289, 65.79142135624982757, -178.7559501969990663 ) ) ;
#109959 = CARTESIAN_POINT ( 'NONE',  ( -18.50000000000000000, 9.350000000011156942, -112.8500000000000369 ) ) ;
#109960 = CARTESIAN_POINT ( 'NONE',  ( -21.14999999999999858, 64.25000000001263345, -196.7969768484652491 ) ) ;
#109961 = DIRECTION ( 'NONE',  ( 0.000000000000000000, 0.9126074666063773710, 0.4088369013363274962 ) ) ;
#109963 = VERTEX_POINT ( 'NONE', #212605 ) ;
#109962 = CARTESIAN_POINT ( 'NONE',  ( 23.14999999999999858, 64.35000000001176090, -76.53791325517833855 ) ) ;
#109964 = DIRECTION ( 'NONE',  ( 0.000000000000000000, 0.000000000000000000, -1.000000000000000000 ) ) ;
#109965 = CYLINDRICAL_SURFACE ( 'NONE', #124702, 0.09999999999999939493 ) ;
#109966 = DIRECTION ( 'NONE',  ( -0.000000000000000000, -0.2128009952263603677, 0.9770955615653313941 ) ) ;
#109967 =( BOUNDED_CURVE ( )  B_SPLINE_CURVE ( 3, ( #141586, #162456, #102426, #2059 ),
 .UNSPECIFIED., .F., .F. ) 
 B_SPLINE_CURVE_WITH_KNOTS ( ( 4, 4 ),
 ( 3.141592653589793116, 4.712388980384689674 ),
 .UNSPECIFIED. ) 
 CURVE ( )  GEOMETRIC_REPRESENTATION_ITEM ( )  RATIONAL_B_SPLINE_CURVE ( ( 1.000000000000000000, 0.8047378541243649375, 0.8047378541243649375, 1.000000000000000000 ) ) 
 REPRESENTATION_ITEM ( '' )  );
#109968 = ORIENTED_EDGE ( 'NONE', *, *, #55544, .T. ) ;
#109969 = DIRECTION ( 'NONE',  ( 0.000000000000000000, 0.9910827722268049644, 0.1332476588733589318 ) ) ;
#109970 = VERTEX_POINT ( 'NONE', #87490 ) ;
#109971 = FACE_OUTER_BOUND ( 'NONE', #151704, .T. ) ;
#109973 = ORIENTED_EDGE ( 'NONE', *, *, #45197, .T. ) ;
#109972 = CIRCLE ( 'NONE', #93214, 0.5000000000000013323 ) ;
#109974 = DIRECTION ( 'NONE',  ( 0.000000000000000000, 0.000000000000000000, -1.000000000000000000 ) ) ;
#109975 = TOROIDAL_SURFACE ( 'NONE', #214039, 0.2000000000000000111, 0.1000000000000000056 ) ;
#109976 = AXIS2_PLACEMENT_3D ( 'NONE', #216937, #194849, #54022 ) ;
#109977 = ORIENTED_EDGE ( 'NONE', *, *, #23992, .F. ) ;
#109978 = ADVANCED_FACE ( 'NONE', ( #247866 ), #249166, .F. ) ;
#109979 = DIRECTION ( 'NONE',  ( 1.000000000000000000, -0.000000000000000000, 0.000000000000000000 ) ) ;
#109981 = EDGE_CURVE ( 'NONE', #193307, #151638, #147485, .T. ) ;
#109980 = DIRECTION ( 'NONE',  ( 0.000000000000000000, 2.891205793294679805E-16, -1.000000000000000000 ) ) ;
#109982 = DIRECTION ( 'NONE',  ( 1.000000000000000000, 0.000000000000000000, 0.000000000000000000 ) ) ;
#109983 = EDGE_LOOP ( 'NONE', ( #214144, #123674, #68292, #153530 ) ) ;
#109984 = EDGE_CURVE ( 'NONE', #13111, #64755, #48375, .T. ) ;
#109985 = ADVANCED_FACE ( 'NONE', ( #227012 ), #152652, .F. ) ;
#109986 = DIRECTION ( 'NONE',  ( -1.652117596168391700E-15, 1.000000000000000000, 6.982962677686266711E-15 ) ) ;
#109987 = CARTESIAN_POINT ( 'NONE',  ( 22.39999999999999503, 11.48087284840413425, -198.4995883060917947 ) ) ;
#109988 = EDGE_CURVE ( 'NONE', #51264, #216196, #178572, .T. ) ;
#109989 = CARTESIAN_POINT ( 'NONE',  ( -21.05000000000000071, 5.900000000011102586, -43.71909976465641989 ) ) ;
#109990 = CARTESIAN_POINT ( 'NONE',  ( 22.14074124539698829, 7.199733713072927088, -199.3305999336096761 ) ) ;
#109991 = DIRECTION ( 'NONE',  ( 1.073024830501117725E-15, 0.000000000000000000, 1.000000000000000000 ) ) ;
#109992 = ADVANCED_FACE ( 'NONE', ( #53520 ), #220048, .F. ) ;
#109994 = EDGE_CURVE ( 'NONE', #169487, #160579, #57719, .T. ) ;
#109993 = DIRECTION ( 'NONE',  ( 1.000000000000000000, 0.000000000000000000, 0.000000000000000000 ) ) ;
#109995 = ORIENTED_EDGE ( 'NONE', *, *, #163935, .T. ) ;
#109997 = ORIENTED_EDGE ( 'NONE', *, *, #133355, .T. ) ;
#109996 = CARTESIAN_POINT ( 'NONE',  ( -22.39999999999999858, 7.790779598384559357, -167.4999999999999432 ) ) ;
#109998 = ORIENTED_EDGE ( 'NONE', *, *, #204603, .T. ) ;
#109999 = AXIS2_PLACEMENT_3D ( 'NONE', #76996, #157870, #133129 ) ;
#110000 = DIRECTION ( 'NONE',  ( -1.000000000000000000, 1.186688945009010077E-16, 8.286604613020808509E-31 ) ) ;
#110001 = EDGE_LOOP ( 'NONE', ( #249704, #246719, #121596, #72983 ) ) ;
#110002 = CARTESIAN_POINT ( 'NONE',  ( 20.12500000000000000, 66.25000000001209344, -128.4113362024100979 ) ) ;
#110003 = CARTESIAN_POINT ( 'NONE',  ( 22.39999999999999503, 1.115541036281197940E-11, -25.70922040162662370 ) ) ;
#110004 = EDGE_CURVE ( 'NONE', #150814, #178668, #207475, .T. ) ;
#110005 = DIRECTION ( 'NONE',  ( 0.000000000000000000, -0.9126074666063770380, -0.4088369013363281068 ) ) ;
#110006 = ORIENTED_EDGE ( 'NONE', *, *, #153557, .T. ) ;
#110007 = CARTESIAN_POINT ( 'NONE',  ( 18.69999999999999929, -2.105948478070175156, -13.13328020565119125 ) ) ;
#110008 = FACE_OUTER_BOUND ( 'NONE', #233450, .T. ) ;
#110009 = DIRECTION ( 'NONE',  ( 0.000000000000000000, 7.147358527629766941E-15, -1.000000000000000000 ) ) ;
#110010 = ORIENTED_EDGE ( 'NONE', *, *, #208662, .T. ) ;
#110011 = EDGE_CURVE ( 'NONE', #206437, #116798, #168384, .T. ) ;
#110013 = ORIENTED_EDGE ( 'NONE', *, *, #129643, .F. ) ;
#110012 = CARTESIAN_POINT ( 'NONE',  ( 18.50000000000000000, 85.40000000001208491, -129.5238218066853904 ) ) ;
#110014 = DIRECTION ( 'NONE',  ( -3.265361837132813093E-16, -1.000000000000000000, -6.982962677686266711E-15 ) ) ;
#110015 = CARTESIAN_POINT ( 'NONE',  ( -18.59999999999999787, 1.162701749938009677, -8.099999999999999645 ) ) ;
#110016 = EDGE_CURVE ( 'NONE', #47140, #256719, #174306, .T. ) ;
#110018 = ADVANCED_FACE ( 'NONE', ( #113489 ), #30127, .T. ) ;
#110017 = VECTOR ( 'NONE', #228449, 1000.000000000000000 ) ;
#110019 = AXIS2_PLACEMENT_3D ( 'NONE', #156223, #153693, #234435 ) ;
#110020 = EDGE_LOOP ( 'NONE', ( #84878, #166337, #221249, #211824 ) ) ;
#110021 = VECTOR ( 'NONE', #196802, 1000.000000000000000 ) ;
#110023 = CARTESIAN_POINT ( 'NONE',  ( 18.50000000000000000, -9.499999999999998224, -40.10018939122205239 ) ) ;
#110022 = AXIS2_PLACEMENT_3D ( 'NONE', #50511, #131355, #110506 ) ;
#110025 = EDGE_CURVE ( 'NONE', #205524, #231927, #130479, .T. ) ;
#110024 = DIRECTION ( 'NONE',  ( 1.000000000000000000, 0.000000000000000000, 0.000000000000000000 ) ) ;
#110026 = DIRECTION ( 'NONE',  ( 1.734723475976817507E-14, 0.2617529984165031243, 0.9651348961777157509 ) ) ;
#110027 = ORIENTED_EDGE ( 'NONE', *, *, #256458, .T. ) ;
#110028 = CARTESIAN_POINT ( 'NONE',  ( -23.25000000000000000, 11.65000000000000036, 11.75000000000000000 ) ) ;
#110029 = EDGE_CURVE ( 'NONE', #17724, #27168, #212324, .T. ) ;
#110030 = CARTESIAN_POINT ( 'NONE',  ( -23.15000000000000213, 64.25000000001151079, -48.17310748452440805 ) ) ;
#110031 = ADVANCED_FACE ( 'NONE', ( #178634 ), #139457, .T. ) ;
#110032 = DIRECTION ( 'NONE',  ( 0.000000000000000000, 0.000000000000000000, 1.000000000000000000 ) ) ;
#110033 = ORIENTED_EDGE ( 'NONE', *, *, #220336, .T. ) ;
#110034 = VECTOR ( 'NONE', #128018, 1000.000000000000000 ) ;
#110035 = VECTOR ( 'NONE', #66009, 1000.000000000000000 ) ;
#110036 = AXIS2_PLACEMENT_3D ( 'NONE', #210161, #169778, #190605 ) ;
#110037 = ORIENTED_EDGE ( 'NONE', *, *, #57895, .F. ) ;
#110038 = PLANE ( 'NONE',  #190280 ) ;
#110039 = AXIS2_PLACEMENT_3D ( 'NONE', #51720, #192556, #131286 ) ;
#110040 = VECTOR ( 'NONE', #150103, 1000.000000000000000 ) ;
#110041 = EDGE_LOOP ( 'NONE', ( #186663, #292, #108474, #189121, #107286, #166148, #42149, #23934, #29031, #71996, #91335, #145749, #199082, #124499 ) ) ;
#110042 = FACE_OUTER_BOUND ( 'NONE', #66834, .T. ) ;
#110043 = DIRECTION ( 'NONE',  ( 0.000000000000000000, -0.4088369013363276072, 0.9126074666063772600 ) ) ;
#110045 = ORIENTED_EDGE ( 'NONE', *, *, #14067, .F. ) ;
#110044 = CARTESIAN_POINT ( 'NONE',  ( 18.59999999999999076, -1.149570369564537842, -208.8159124845019221 ) ) ;
#110046 = DIRECTION ( 'NONE',  ( -1.000000000000000000, 0.000000000000000000, 0.000000000000000000 ) ) ;
#110047 = CARTESIAN_POINT ( 'NONE',  ( 20.94999999999999929, 10.72371710471867701, -108.1649135690876449 ) ) ;
#110048 = DIRECTION ( 'NONE',  ( 1.000000000000000000, 0.000000000000000000, 0.000000000000000000 ) ) ;
#110049 = CARTESIAN_POINT ( 'NONE',  ( -18.39999999999999858, 85.60000000001166143, -62.82291809330219223 ) ) ;
#110050 = CARTESIAN_POINT ( 'NONE',  ( 21.05000000000000071, 7.081614052365321932, -233.8208508380561454 ) ) ;
#110051 = VECTOR ( 'NONE', #167336, 1000.000000000000114 ) ;
#110052 = CARTESIAN_POINT ( 'NONE',  ( -16.97092634996705485, 10.00088896636034264, -79.63014276629733956 ) ) ;
#110053 = AXIS2_PLACEMENT_3D ( 'NONE', #240555, #220973, #59303 ) ;
#110054 = CARTESIAN_POINT ( 'NONE',  ( -20.54999999999999716, -9.399999999988846611, -124.1060308773475924 ) ) ;
#110056 = VERTEX_POINT ( 'NONE', #252995 ) ;
#110055 = DIRECTION ( 'NONE',  ( -1.000000000000000000, 0.000000000000000000, 0.000000000000000000 ) ) ;
#110057 = AXIS2_PLACEMENT_3D ( 'NONE', #179332, #37248, #197575 ) ;
#110058 = CIRCLE ( 'NONE', #184881, 0.09999999999999939493 ) ;
#110059 = DIRECTION ( 'NONE',  ( -1.000000000000000000, 0.000000000000000000, 0.000000000000000000 ) ) ;
#110060 = DIRECTION ( 'NONE',  ( -0.8191520442889921316, 0.5735764363510457153, 0.000000000000000000 ) ) ;
#110061 = DIRECTION ( 'NONE',  ( 0.000000000000000000, -0.9908441862701605762, -0.1350103645451835310 ) ) ;
#110062 = AXIS2_PLACEMENT_3D ( 'NONE', #152135, #170444, #12624 ) ;
#110064 = ORIENTED_EDGE ( 'NONE', *, *, #218621, .F. ) ;
#110063 = VECTOR ( 'NONE', #254338, 1000.000000000000000 ) ;
#110066 = CIRCLE ( 'NONE', #139081, 0.09999999999999939493 ) ;
#110065 = DIRECTION ( 'NONE',  ( 1.000000000000000000, -0.000000000000000000, -0.000000000000000000 ) ) ;
#110067 = EDGE_CURVE ( 'NONE', #107540, #241350, #103502, .T. ) ;
#110068 = DIRECTION ( 'NONE',  ( 0.000000000000000000, -0.1568667991644863147, 0.9876197685951252359 ) ) ;
#110069 = DIRECTION ( 'NONE',  ( 1.000000000000000000, -0.000000000000000000, -0.000000000000000000 ) ) ;
#110070 = ADVANCED_FACE ( 'NONE', ( #235999 ), #157747, .T. ) ;
#110071 = ORIENTED_EDGE ( 'NONE', *, *, #135621, .T. ) ;
#110072 = CARTESIAN_POINT ( 'NONE',  ( -23.25000000000000000, 7.128833340094563376, -233.7327013124401276 ) ) ;
#110073 = DIRECTION ( 'NONE',  ( 0.000000000000000000, 0.000000000000000000, -1.000000000000000000 ) ) ;
#110074 = EDGE_CURVE ( 'NONE', #121991, #88576, #74406, .T. ) ;
#110075 = ORIENTED_EDGE ( 'NONE', *, *, #17769, .F. ) ;
#110077 = EDGE_CURVE ( 'NONE', #247484, #145626, #237298, .T. ) ;
#110076 = FACE_OUTER_BOUND ( 'NONE', #88913, .T. ) ;
#110078 = ORIENTED_EDGE ( 'NONE', *, *, #17351, .T. ) ;
#110079 = DIRECTION ( 'NONE',  ( -1.000000000000000000, -0.000000000000000000, -0.000000000000000000 ) ) ;
#110081 = ORIENTED_EDGE ( 'NONE', *, *, #213288, .T. ) ;
#110080 = CARTESIAN_POINT ( 'NONE',  ( 22.39999999999999503, 76.00000000001219291, -144.3138870828976792 ) ) ;
#110082 = DIRECTION ( 'NONE',  ( 0.000000000000000000, 0.000000000000000000, -1.000000000000000000 ) ) ;
#110083 = ORIENTED_EDGE ( 'NONE', *, *, #20975, .F. ) ;
#110084 = AXIS2_PLACEMENT_3D ( 'NONE', #195873, #112476, #194597 ) ;
#110085 = CARTESIAN_POINT ( 'NONE',  ( 23.24999999999999645, 67.17743825834614313, -182.6731074845244223 ) ) ;
#110086 = ORIENTED_EDGE ( 'NONE', *, *, #18745, .T. ) ;
#110087 = AXIS2_PLACEMENT_3D ( 'NONE', #180006, #216544, #37935 ) ;
#110088 = VERTEX_POINT ( 'NONE', #114778 ) ;
#110089 = CARTESIAN_POINT ( 'NONE',  ( 18.58703555225034876, 85.40633674080100946, -129.3981628432775892 ) ) ;
#110091 = ORIENTED_EDGE ( 'NONE', *, *, #104198, .T. ) ;
#110090 = FILL_AREA_STYLE ('',( #68406 ) ) ;
#110092 = AXIS2_PLACEMENT_3D ( 'NONE', #146887, #166507, #85614 ) ;
#110093 = CARTESIAN_POINT ( 'NONE',  ( 20.91682497891422798, 65.67736539654923433, -63.96251168765719797 ) ) ;
#110094 = VERTEX_POINT ( 'NONE', #216434 ) ;
#110095 = EDGE_CURVE ( 'NONE', #94180, #120362, #213874, .T. ) ;
#110096 = VECTOR ( 'NONE', #10346, 1000.000000000000000 ) ;
#110097 = CIRCLE ( 'NONE', #255806, 0.1000000000000024342 ) ;
#110098 = VERTEX_POINT ( 'NONE', #256792 ) ;
#110099 = CARTESIAN_POINT ( 'NONE',  ( 20.85000000000000142, 68.97833521811179480, -99.18954208262705663 ) ) ;
#110100 = CARTESIAN_POINT ( 'NONE',  ( 23.14999999999999858, 1.115600667400684642E-11, -134.0000000000000284 ) ) ;
#110101 = EDGE_LOOP ( 'NONE', ( #249396, #20474, #241931, #17179, #208860 ) ) ;
#110102 = AXIS2_PLACEMENT_3D ( 'NONE', #48725, #128283, #5728 ) ;
#110103 = DIRECTION ( 'NONE',  ( 0.000000000000000000, 1.000000000000000000, 0.000000000000000000 ) ) ;
#110104 = FACE_OUTER_BOUND ( 'NONE', #77559, .T. ) ;
#110105 = DIRECTION ( 'NONE',  ( 1.000000000000000000, -7.049440681616513945E-16, 1.911869773728117674E-16 ) ) ;
#110106 = CIRCLE ( 'NONE', #43483, 0.1999999999999996503 ) ;
#110107 = ORIENTED_EDGE ( 'NONE', *, *, #131432, .F. ) ;
#110108 = DIRECTION ( 'NONE',  ( -1.000000000000000000, 0.000000000000000000, 0.000000000000000000 ) ) ;
#110109 = AXIS2_PLACEMENT_3D ( 'NONE', #139819, #58980, #72492 ) ;
#110111 = EDGE_CURVE ( 'NONE', #121961, #78857, #106502, .T. ) ;
#110110 = CYLINDRICAL_SURFACE ( 'NONE', #198673, 0.5000000000000004441 ) ;
#110112 = CARTESIAN_POINT ( 'NONE',  ( -17.78043020864320667, 10.85359211200568375, -10.33695083427979178 ) ) ;
#110114 = DIRECTION ( 'NONE',  ( 0.000000000000000000, 0.9856811345164803173, 0.1686199900910455851 ) ) ;
#110113 = TOROIDAL_SURFACE ( 'NONE', #160217, 0.6000000000000015321, 0.1000000000000000056 ) ;
#110115 = ORIENTED_EDGE ( 'NONE', *, *, #249812, .T. ) ;
#110116 = EDGE_CURVE ( 'NONE', #124309, #152443, #153458, .T. ) ;
#110117 = CARTESIAN_POINT ( 'NONE',  ( 18.51697539158856642, 10.31565961587946134, -106.0364194119178904 ) ) ;
#110118 = ORIENTED_EDGE ( 'NONE', *, *, #50279, .T. ) ;
#110119 = CARTESIAN_POINT ( 'NONE',  ( -18.41799967126737059, -7.785976380097459071, -209.8926136578000126 ) ) ;
#110120 = ORIENTED_EDGE ( 'NONE', *, *, #19918, .T. ) ;
#110121 = CARTESIAN_POINT ( 'NONE',  ( 21.05000000000005400, 64.35000000001120668, -3.123107484524795474 ) ) ;
#110122 = DIRECTION ( 'NONE',  ( 1.000000000000000000, 0.000000000000000000, 0.000000000000000000 ) ) ;
#110123 = ORIENTED_EDGE ( 'NONE', *, *, #71140, .T. ) ;
#110124 = ORIENTED_EDGE ( 'NONE', *, *, #205007, .T. ) ;
#110125 = DIRECTION ( 'NONE',  ( 1.000000000000000000, -0.000000000000000000, -0.000000000000000000 ) ) ;
#110126 = DIRECTION ( 'NONE',  ( 0.000000000000000000, 0.9908441862701596881, -0.1350103645451904977 ) ) ;
#110127 = ORIENTED_EDGE ( 'NONE', *, *, #226404, .F. ) ;
#110128 = AXIS2_PLACEMENT_3D ( 'NONE', #190509, #206196, #27597 ) ;
#110129 = ADVANCED_FACE ( 'NONE', ( #40412 ), #174801, .T. ) ;
#110130 = CARTESIAN_POINT ( 'NONE',  ( -1.739115166359751170E-14, 11.65000000001114699, -91.85000000000003695 ) ) ;
#110131 = CARTESIAN_POINT ( 'NONE',  ( -18.50016250449483479, 65.70233904876991460, -64.04874109119681691 ) ) ;
#110132 = EDGE_CURVE ( 'NONE', #182847, #234718, #57884, .T. ) ;
#110133 = EDGE_LOOP ( 'NONE', ( #150702, #229036, #149838, #212484 ) ) ;
#110134 = DIRECTION ( 'NONE',  ( 1.000000000000000000, 0.000000000000000000, 0.000000000000000000 ) ) ;
#110135 = EDGE_CURVE ( 'NONE', #175804, #206030, #215158, .T. ) ;
#110136 = MANIFOLD_SOLID_BREP ( 'Stock-MAS-200-1', #36934 ) ;
#110138 = VERTEX_POINT ( 'NONE', #239871 ) ;
#110137 = TOROIDAL_SURFACE ( 'NONE', #35360, 11.65000000000000036, 0.1000000000000000056 ) ;
#110139 = VECTOR ( 'NONE', #144937, 1000.000000000000227 ) ;
#110140 = DIRECTION ( 'NONE',  ( 7.304098846218134667E-16, 1.000000000000000000, 6.982962677686266711E-15 ) ) ;
#110141 = DIRECTION ( 'NONE',  ( 1.000000000000000000, 0.000000000000000000, 0.000000000000000000 ) ) ;
#110142 = ADVANCED_FACE ( 'NONE', ( #101589 ), #135609, .T. ) ;
#110143 = DIRECTION ( 'NONE',  ( 0.000000000000000000, 0.000000000000000000, -1.000000000000000000 ) ) ;
#110145 = VERTEX_POINT ( 'NONE', #199468 ) ;
#110144 = PLANE ( 'NONE',  #201550 ) ;
#110146 = DIRECTION ( 'NONE',  ( 0.000000000000000000, 6.982962677686266711E-15, -1.000000000000000000 ) ) ;
#110147 = DIRECTION ( 'NONE',  ( 0.000000000000000000, 0.9126074666063632712, 0.4088369013363589710 ) ) ;
#110148 = DIRECTION ( 'NONE',  ( -1.000000000000000000, 0.000000000000000000, 0.000000000000000000 ) ) ;
#110149 = EDGE_CURVE ( 'NONE', #161732, #144437, #84583, .T. ) ;
#110151 = DIRECTION ( 'NONE',  ( 0.000000000000000000, 6.982962677686266711E-15, -1.000000000000000000 ) ) ;
#110150 = FACE_OUTER_BOUND ( 'NONE', #95533, .T. ) ;
#110152 = DIRECTION ( 'NONE',  ( -1.000000000000000000, 0.000000000000000000, 0.000000000000000000 ) ) ;
#110153 = DIRECTION ( 'NONE',  ( 0.000000000000000000, 1.000000000000000000, 0.000000000000000000 ) ) ;
#110154 = CARTESIAN_POINT ( 'NONE',  ( -18.59999999999999787, 74.36282728704149747, -91.44095411905230719 ) ) ;
#110155 = CARTESIAN_POINT ( 'NONE',  ( -21.05000000000000071, 28.60154115857408641, -258.4512230915049713 ) ) ;
#110156 = AXIS2_PLACEMENT_3D ( 'NONE', #150274, #126842, #31628 ) ;
#110157 = ORIENTED_EDGE ( 'NONE', *, *, #189487, .F. ) ;
#110158 = ORIENTED_EDGE ( 'NONE', *, *, #14714, .F. ) ;
#110159 = AXIS2_PLACEMENT_3D ( 'NONE', #13135, #172244, #19553 ) ;
#110160 = VERTEX_POINT ( 'NONE', #63788 ) ;
#110161 = FACE_OUTER_BOUND ( 'NONE', #132138, .T. ) ;
#110162 = LINE ( 'NONE', #93166, #136017 ) ;
#110163 = ORIENTED_EDGE ( 'NONE', *, *, #183077, .T. ) ;
#110164 = CARTESIAN_POINT ( 'NONE',  ( -23.25000000000000355, 11.74999999999998224, -20.85000000000000142 ) ) ;
#110165 = CARTESIAN_POINT ( 'NONE',  ( 20.91682497891423154, 10.32263460347359185, -206.5605957968671476 ) ) ;
#110166 = DIRECTION ( 'NONE',  ( 0.000000000000000000, -1.000000000000000000, 0.000000000000000000 ) ) ;
#110167 = VERTEX_POINT ( 'NONE', #144588 ) ;
#110168 = ORIENTED_EDGE ( 'NONE', *, *, #126178, .F. ) ;
#110170 = CYLINDRICAL_SURFACE ( 'NONE', #175427, 0.1000000000000055844 ) ;
#110169 = MECHANICAL_DESIGN_GEOMETRIC_PRESENTATION_REPRESENTATION (  '', ( #118587 ), #64402 ) ;
#110171 = AXIS2_PLACEMENT_3D ( 'NONE', #209144, #110048, #207898 ) ;
#110172 = DIRECTION ( 'NONE',  ( 0.000000000000000000, -0.9908441862701600211, -0.1350103645451876666 ) ) ;
#110173 = EDGE_LOOP ( 'NONE', ( #99204, #254089, #26387, #164173 ) ) ;
#110174 = CARTESIAN_POINT ( 'NONE',  ( 18.49999999999999645, 76.00000000001213607, -136.5231074845243313 ) ) ;
#110176 = EDGE_LOOP ( 'NONE', ( #159237, #235396, #187255, #134700 ) ) ;
#110175 = CARTESIAN_POINT ( 'NONE',  ( -23.25000000000000000, 71.65000000001199965, -115.1731074845243370 ) ) ;
#110177 = CARTESIAN_POINT ( 'NONE',  ( -23.15000000000000213, 23.38726701055792745, -229.1122755113798348 ) ) ;
#110178 = CARTESIAN_POINT ( 'NONE',  ( 23.14999999999999858, 0.000000000000000000, -33.50000000000000000 ) ) ;
#110180 = ORIENTED_EDGE ( 'NONE', *, *, #89537, .F. ) ;
#110179 = FACE_OUTER_BOUND ( 'NONE', #242314, .T. ) ;
#110181 = CARTESIAN_POINT ( 'NONE',  ( -18.79999999999999716, 0.000000000000000000, 0.000000000000000000 ) ) ;
#110182 = CARTESIAN_POINT ( 'NONE',  ( 20.85000000000000142, 64.25000000001219291, -143.3069731475025037 ) ) ;
#110183 = DIRECTION ( 'NONE',  ( 0.000000000000000000, -0.2617529984164856383, -0.9651348961777204138 ) ) ;
#110184 = DIRECTION ( 'NONE',  ( 1.000000000000000000, 0.000000000000000000, 0.000000000000000000 ) ) ;
#110186 = FACE_OUTER_BOUND ( 'NONE', #184463, .T. ) ;
#110185 = CARTESIAN_POINT ( 'NONE',  ( 21.72449340488909897, 65.71604372252039639, -48.67310748452440095 ) ) ;
#110187 = DIRECTION ( 'NONE',  ( 0.000000000000000000, -0.000000000000000000, 1.000000000000000000 ) ) ;
#110188 = CARTESIAN_POINT ( 'NONE',  ( -18.44232395689961734, 85.55228255706272478, -163.1808554997175520 ) ) ;
#110189 = AXIS2_PLACEMENT_3D ( 'NONE', #155909, #195034, #136290 ) ;
#110190 = DIRECTION ( 'NONE',  ( 0.000000000000000000, -0.2617529984165152257, -0.9651348961777124202 ) ) ;
#110191 = CYLINDRICAL_SURFACE ( 'NONE', #146839, 0.1000000000000028644 ) ;
#110192 = ORIENTED_EDGE ( 'NONE', *, *, #171023, .T. ) ;
#110193 = CIRCLE ( 'NONE', #185224, 0.09999999999999939493 ) ;
#110194 = CARTESIAN_POINT ( 'NONE',  ( 23.15000000000000213, -8.999999999988842703, -157.6060308773475640 ) ) ;
#110195 = VERTEX_POINT ( 'NONE', #104178 ) ;
#110196 = CARTESIAN_POINT ( 'NONE',  ( 19.58285714285715073, 9.015001489659738354, -75.42065281608175553 ) ) ;
#110197 = VERTEX_POINT ( 'NONE', #61220 ) ;
#110198 = FACE_OUTER_BOUND ( 'NONE', #113942, .T. ) ;
#110199 = EDGE_CURVE ( 'NONE', #185811, #250368, #124562, .T. ) ;
#110200 = CARTESIAN_POINT ( 'NONE',  ( -21.05000000000000071, 70.10000000001213039, -126.3040077198679398 ) ) ;
#110201 = ADVANCED_FACE ( 'NONE', ( #100319 ), #179902, .F. ) ;
#110202 = EDGE_CURVE ( 'NONE', #219374, #252440, #66301, .T. ) ;
#110203 = ORIENTED_EDGE ( 'NONE', *, *, #55209, .T. ) ;
#110204 = TOROIDAL_SURFACE ( 'NONE', #1306, 11.70000000000000462, 0.1000000000000000056 ) ;
#110205 = CARTESIAN_POINT ( 'NONE',  ( 18.59999999999999076, 11.65000000000000391, -33.50000000000000000 ) ) ;
#110206 = SURFACE_SIDE_STYLE ('',( #128503 ) ) ;
#110207 = AXIS2_PLACEMENT_3D ( 'NONE', #51792, #131345, #210886 ) ;
#110208 = ORIENTED_EDGE ( 'NONE', *, *, #201604, .F. ) ;
#110209 = ORIENTED_EDGE ( 'NONE', *, *, #241272, .F. ) ;
#110210 = CIRCLE ( 'NONE', #77083, 0.09999999999999939493 ) ;
#110211 = EDGE_LOOP ( 'NONE', ( #223379, #73004, #176261 ) ) ;
#110212 = AXIS2_PLACEMENT_3D ( 'NONE', #107556, #189677, #25479 ) ;
#110213 = CARTESIAN_POINT ( 'NONE',  ( -5.900000000000003020, -11.65000000000000036, 10.10000000000000142 ) ) ;
#110214 = CARTESIAN_POINT ( 'NONE',  ( -16.79814274880124358, 66.05072745733427553, -56.87067444747639655 ) ) ;
#110215 = CARTESIAN_POINT ( 'NONE',  ( 20.94999999999999929, 8.776282895303632259, -112.6500000000000341 ) ) ;
#110216 = VECTOR ( 'NONE', #100345, 1000.000000000000000 ) ;
#110217 = CARTESIAN_POINT ( 'NONE',  ( 13.43663047529820176, 27.81851053932208728, -234.0989799278904115 ) ) ;
#110218 = DIRECTION ( 'NONE',  ( 0.000000000000000000, 0.9126074666063844765, 0.4088369013363113980 ) ) ;
#110219 = EDGE_CURVE ( 'NONE', #21500, #201700, #164184, .T. ) ;
#110221 = FACE_OUTER_BOUND ( 'NONE', #189343, .T. ) ;
#110220 = CARTESIAN_POINT ( 'NONE',  ( -20.85000000000000142, -11.64999999998884306, -67.00000000000000000 ) ) ;
#110222 = CARTESIAN_POINT ( 'NONE',  ( 18.49999999999999289, 10.20857864609425825, -58.20250686563007037 ) ) ;
#110224 = EDGE_LOOP ( 'NONE', ( #238121, #156894, #22347, #169910 ) ) ;
#110223 = CARTESIAN_POINT ( 'NONE',  ( -20.94403535211772294, 10.30632246271647467, -139.5041836778896140 ) ) ;
#110226 = DIRECTION ( 'NONE',  ( 0.000000000000000000, 0.000000000000000000, -1.000000000000000000 ) ) ;
#110225 = CARTESIAN_POINT ( 'NONE',  ( 20.58091095332318332, 9.018470153363605135, -75.41865018215861483 ) ) ;
#110227 = ORIENTED_EDGE ( 'NONE', *, *, #15779, .T. ) ;
#110228 = DIRECTION ( 'NONE',  ( 1.000000000000000000, 0.000000000000000000, 0.000000000000000000 ) ) ;
#110229 = VECTOR ( 'NONE', #12850, 1000.000000000000000 ) ;
#110230 = DIRECTION ( 'NONE',  ( -0.000000000000000000, -6.982962677686266711E-15, 1.000000000000000000 ) ) ;
#110231 = DIRECTION ( 'NONE',  ( -0.000000000000000000, 0.1350103645451945777, -0.9908441862701590219 ) ) ;
#110232 = AXIS2_PLACEMENT_3D ( 'NONE', #75414, #131499, #251450 ) ;
#110233 = ORIENTED_EDGE ( 'NONE', *, *, #29611, .F. ) ;
#110234 = VECTOR ( 'NONE', #124189, 1000.000000000000227 ) ;
#110235 = DIRECTION ( 'NONE',  ( 1.000000000000000000, 0.000000000000000000, 0.000000000000000000 ) ) ;
#110236 = AXIS2_PLACEMENT_3D ( 'NONE', #135730, #14538, #193169 ) ;
#110237 = DIRECTION ( 'NONE',  ( 1.000000000000000000, -1.875376730785737719E-16, -1.309568571767809260E-30 ) ) ;
#110238 = CARTESIAN_POINT ( 'NONE',  ( 15.39793903038207823, 66.61031399435617573, -87.35026397817307497 ) ) ;
#110239 = VERTEX_POINT ( 'NONE', #1223 ) ;
#110240 = ORIENTED_EDGE ( 'NONE', *, *, #116945, .F. ) ;
#110241 = TOROIDAL_SURFACE ( 'NONE', #255943, 11.90000000000000213, 0.1000000000000000056 ) ;
#110242 = DIRECTION ( 'NONE',  ( 0.000000000000000000, 0.000000000000000000, -1.000000000000000000 ) ) ;
#110243 = EDGE_CURVE ( 'NONE', #78723, #74229, #24692, .T. ) ;
#110244 = ADVANCED_FACE ( 'NONE', ( #243707 ), #80760, .T. ) ;
#110245 = CARTESIAN_POINT ( 'NONE',  ( -18.50000972452446035, 10.29326151435326508, -172.9592822510415147 ) ) ;
#110246 = DIRECTION ( 'NONE',  ( 0.000000000000000000, -0.1298341882520022694, -0.9915357197604853789 ) ) ;
#110247 = CARTESIAN_POINT ( 'NONE',  ( -20.90851465518105812, 10.32532329027886320, -206.5699343018359002 ) ) ;
#110248 = ORIENTED_EDGE ( 'NONE', *, *, #256308, .T. ) ;
#110249 = AXIS2_PLACEMENT_3D ( 'NONE', #30272, #211461, #107216 ) ;
#110250 = TOROIDAL_SURFACE ( 'NONE', #143580, 0.2000000000000000111, 0.1000000000000000056 ) ;
#110251 = LINE ( 'NONE', #50265, #192116 ) ;
#110252 = DIRECTION ( 'NONE',  ( 0.000000000000000000, 0.2617529984165036239, 0.9651348961777156399 ) ) ;
#110253 = ADVANCED_FACE ( 'NONE', ( #165468 ), #45506, .T. ) ;
#110254 = CARTESIAN_POINT ( 'NONE',  ( 22.47071067811865319, 0.09909245471376171288, -126.2799252555019649 ) ) ;
#110255 = DIRECTION ( 'NONE',  ( -1.000000000000000000, -2.952720810173289112E-16, 0.000000000000000000 ) ) ;
#110256 = EDGE_LOOP ( 'NONE', ( #243318, #190320, #127440, #203907 ) ) ;
#110257 = DIRECTION ( 'NONE',  ( 1.000000000000000000, 0.000000000000000000, 0.000000000000000000 ) ) ;
#110259 = ORIENTED_EDGE ( 'NONE', *, *, #209568, .F. ) ;
#110258 = CARTESIAN_POINT ( 'NONE',  ( -17.22767730084084192, 65.65075578754407104, -192.1655361750986515 ) ) ;
#110260 = CARTESIAN_POINT ( 'NONE',  ( -22.50000000000000000, 12.67709964810648238, -223.3751320524553705 ) ) ;
#110261 = DIRECTION ( 'NONE',  ( 0.000000000000000000, 0.000000000000000000, -1.000000000000000000 ) ) ;
#110262 = DIRECTION ( 'NONE',  ( 1.000000000000000000, 0.000000000000000000, 0.000000000000000000 ) ) ;
#110263 = LINE ( 'NONE', #133685, #21245 ) ;
#110264 = EDGE_LOOP ( 'NONE', ( #168623, #163968, #179771 ) ) ;
#110265 = DIRECTION ( 'NONE',  ( -0.7071067811865389130, 0.000000000000000000, 0.7071067811865561215 ) ) ;
#110266 = CYLINDRICAL_SURFACE ( 'NONE', #230027, 0.4999999999999944489 ) ;
#110267 = DIRECTION ( 'NONE',  ( 1.000000000000000000, 0.000000000000000000, 0.000000000000000000 ) ) ;
#110268 = ORIENTED_EDGE ( 'NONE', *, *, #246560, .F. ) ;
#110269 = FACE_OUTER_BOUND ( 'NONE', #92210, .T. ) ;
#110270 = FACE_OUTER_BOUND ( 'NONE', #123437, .T. ) ;
#110271 = DIRECTION ( 'NONE',  ( 0.000000000000000000, -0.01283462868041947667, -0.9999176327611367654 ) ) ;
#110273 = AXIS2_PLACEMENT_3D ( 'NONE', #61004, #118435, #177139 ) ;
#110272 = DIRECTION ( 'NONE',  ( 1.000000000000000000, 0.000000000000000000, 0.000000000000000000 ) ) ;
#110274 = CIRCLE ( 'NONE', #1925, 0.09999999999998898659 ) ;
#110275 = CARTESIAN_POINT ( 'NONE',  ( 21.04999999999953886, 6.441084688482137111, -167.5177194333097646 ) ) ;
#110276 = CARTESIAN_POINT ( 'NONE',  ( 23.24999999999999645, 76.00000000001170974, -69.52310748452431710 ) ) ;
#110277 = ORIENTED_EDGE ( 'NONE', *, *, #29868, .T. ) ;
#110278 = EDGE_LOOP ( 'NONE', ( #9613, #97651, #161826 ) ) ;
#110279 = AXIS2_PLACEMENT_3D ( 'NONE', #232623, #34427, #129642 ) ;
#110280 = PLANE ( 'NONE',  #5971 ) ;
#110281 = ADVANCED_FACE ( 'NONE', ( #204572 ), #37091, .T. ) ;
#110282 = DIRECTION ( 'NONE',  ( 1.000000000000000000, 0.000000000000000000, 0.000000000000000000 ) ) ;
#110283 = CIRCLE ( 'NONE', #243560, 0.09999999999999939493 ) ;
#110285 = EDGE_CURVE ( 'NONE', #148530, #93424, #207783, .T. ) ;
#110284 = DIRECTION ( 'NONE',  ( 0.000000000000000000, 0.000000000000000000, 1.000000000000000000 ) ) ;
#110286 =( BOUNDED_CURVE ( )  B_SPLINE_CURVE ( 3, ( #241546, #139860, #122896, #164587 ),
 .UNSPECIFIED., .F., .F. ) 
 B_SPLINE_CURVE_WITH_KNOTS ( ( 4, 4 ),
 ( 3.432212674861196966, 3.693332928900581624 ),
 .UNSPECIFIED. ) 
 CURVE ( )  GEOMETRIC_REPRESENTATION_ITEM ( )  RATIONAL_B_SPLINE_CURVE ( ( 1.000000000000000000, 0.9943260843901261525, 0.9943260843901261525, 1.000000000000000000 ) ) 
 REPRESENTATION_ITEM ( '' )  );
#110287 = CYLINDRICAL_SURFACE ( 'NONE', #99570, 0.1000000000000028644 ) ;
#110288 = CARTESIAN_POINT ( 'NONE',  ( -20.54999999999999716, 85.50000000001159606, -59.62913836187181005 ) ) ;
#110289 = EDGE_CURVE ( 'NONE', #256663, #240042, #107797, .T. ) ;
#110290 = EDGE_CURVE ( 'NONE', #141516, #61931, #183740, .T. ) ;
#110292 = AXIS2_PLACEMENT_3D ( 'NONE', #212848, #189430, #49903 ) ;
#110291 = CARTESIAN_POINT ( 'NONE',  ( 20.85000000000000142, 11.65000000001115943, -194.2161343370218560 ) ) ;
#110293 = CARTESIAN_POINT ( 'NONE',  ( 23.14999999999999858, -11.74999999999999112, 11.75000000000000000 ) ) ;
#110294 = VECTOR ( 'NONE', #43513, 1000.000000000000000 ) ;
#110295 = CARTESIAN_POINT ( 'NONE',  ( -18.39999999999999858, 11.47316190337362762, -109.7998292484660539 ) ) ;
#110297 = AXIS2_PLACEMENT_3D ( 'NONE', #234470, #137931, #212373 ) ;
#110296 = CARTESIAN_POINT ( 'NONE',  ( -18.59999999999999787, 14.05000000000000071, -5.513695070760990191 ) ) ;
#110298 = EDGE_CURVE ( 'NONE', #8118, #116802, #193693, .T. ) ;
#110300 = EDGE_CURVE ( 'NONE', #144523, #166838, #70425, .T. ) ;
#110299 = ADVANCED_FACE ( 'NONE', ( #171584 ), #110287, .T. ) ;
#110301 = ORIENTED_EDGE ( 'NONE', *, *, #50388, .F. ) ;
#110302 = CARTESIAN_POINT ( 'NONE',  ( -18.60000000000001563, 85.36424052760251868, -62.34285890268348140 ) ) ;
#110303 = ORIENTED_EDGE ( 'NONE', *, *, #6665, .T. ) ;
#110304 = DIRECTION ( 'NONE',  ( 0.000000000000000000, 0.000000000000000000, -1.000000000000000000 ) ) ;
#110305 = FACE_OUTER_BOUND ( 'NONE', #224953, .T. ) ;
#110308 = ADVANCED_FACE ( 'NONE', ( #155867 ), #234082, .T. ) ;
#110307 = CIRCLE ( 'NONE', #26955, 0.09999999999999939493 ) ;
#110306 = CARTESIAN_POINT ( 'NONE',  ( 23.25000000000000000, 85.60000000001252829, -179.9170766071767389 ) ) ;
#110309 = FACE_OUTER_BOUND ( 'NONE', #148060, .T. ) ;
#110310 = CARTESIAN_POINT ( 'NONE',  ( 21.05000000000000071, 21.98309897467606433, -231.7335930323676791 ) ) ;
#110311 = CARTESIAN_POINT ( 'NONE',  ( 23.04999999999999716, 41.49355468354239207, -237.7178856438439141 ) ) ;
#110312 = DIRECTION ( 'NONE',  ( 0.000000000000000000, -6.982962677686266711E-15, 1.000000000000000000 ) ) ;
#110313 = ORIENTED_EDGE ( 'NONE', *, *, #116006, .F. ) ;
#110314 = LINE ( 'NONE', #189855, #45621 ) ;
#110315 = ADVANCED_FACE ( 'NONE', ( #73765 ), #246651, .T. ) ;
#110316 = DIRECTION ( 'NONE',  ( -1.000000000000000000, -0.000000000000000000, -0.000000000000000000 ) ) ;
#110317 = DIRECTION ( 'NONE',  ( 1.000000000000000000, -1.646408749285562060E-14, -1.073024830501232702E-15 ) ) ;
#110318 = EDGE_CURVE ( 'NONE', #178265, #106770, #8045, .T. ) ;
#110319 = EDGE_CURVE ( 'NONE', #72948, #134440, #131138, .T. ) ;
#110320 = CARTESIAN_POINT ( 'NONE',  ( -18.40000000000000213, 64.25000000001230660, -157.3731074845244393 ) ) ;
#110321 = AXIS2_PLACEMENT_3D ( 'NONE', #80975, #161843, #160557 ) ;
#110322 = AXIS2_PLACEMENT_3D ( 'NONE', #96507, #213910, #253034 ) ;
#110323 = ORIENTED_EDGE ( 'NONE', *, *, #58026, .T. ) ;
#110324 = DIRECTION ( 'NONE',  ( -1.000000000000000000, -0.000000000000000000, -0.000000000000000000 ) ) ;
#110326 = ADVANCED_FACE ( 'NONE', ( #35917 ), #153827, .F. ) ;
#110325 = CARTESIAN_POINT ( 'NONE',  ( -21.05000000000000071, 1.162701749949165642, -141.9000000000000341 ) ) ;
#110327 = ORIENTED_EDGE ( 'NONE', *, *, #30565, .T. ) ;
#110328 = EDGE_LOOP ( 'NONE', ( #224099, #141190, #229890, #75427 ) ) ;
#110329 = DIRECTION ( 'NONE',  ( -0.000000000000000000, 0.9876013379310886187, 0.1569827930593787890 ) ) ;
#110330 = CYLINDRICAL_SURFACE ( 'NONE', #10803, 0.09999999999999939493 ) ;
#110331 = EDGE_CURVE ( 'NONE', #7145, #143246, #91242, .T. ) ;
#110332 = ORIENTED_EDGE ( 'NONE', *, *, #198586, .F. ) ;
#110333 = DIRECTION ( 'NONE',  ( -0.000000000000000000, 1.000000000000000000, 6.982962677686267499E-15 ) ) ;
#110334 = EDGE_CURVE ( 'NONE', #89902, #88287, #152021, .T. ) ;
#110335 = EDGE_LOOP ( 'NONE', ( #156218, #61727, #84524, #241615, #132567, #51774, #162089 ) ) ;
#110336 = AXIS2_PLACEMENT_3D ( 'NONE', #62718, #1443, #44451 ) ;
#110337 = CARTESIAN_POINT ( 'NONE',  ( 18.59999999999999432, 16.56538529403860238, -240.6448716151659823 ) ) ;
#110338 = ORIENTED_EDGE ( 'NONE', *, *, #135727, .T. ) ;
#110339 = CARTESIAN_POINT ( 'NONE',  ( 20.95512820512820795, 10.62384868372303615, -79.20016201942446799 ) ) ;
#110340 = EDGE_CURVE ( 'NONE', #17245, #130685, #230786, .T. ) ;
#110341 = CYLINDRICAL_SURFACE ( 'NONE', #67094, 0.1000000000000028644 ) ;
#110343 = ORIENTED_EDGE ( 'NONE', *, *, #134694, .T. ) ;
#110342 = PLANE ( 'NONE',  #195801 ) ;
#110344 = DIRECTION ( 'NONE',  ( 0.000000000000000000, 3.528251137579945416E-15, -1.000000000000000000 ) ) ;
#110346 = DIRECTION ( 'NONE',  ( 0.000000000000000000, -1.000000000000000000, 0.000000000000000000 ) ) ;
#110345 = UNCERTAINTY_MEASURE_WITH_UNIT (LENGTH_MEASURE( 1.000000000000000082E-05 ), #71424, 'distance_accuracy_value', 'NONE');
#110347 = DIRECTION ( 'NONE',  ( -1.000000000000000000, 0.000000000000000000, 0.000000000000000000 ) ) ;
#110348 = DIRECTION ( 'NONE',  ( -0.000000000000000000, -0.4791956752371546169, -0.8777080977375152360 ) ) ;
#110349 = DIRECTION ( 'NONE',  ( 1.000000000000000000, -0.000000000000000000, 0.000000000000000000 ) ) ;
#110350 = DIRECTION ( 'NONE',  ( 0.000000000000000000, 0.000000000000000000, -1.000000000000000000 ) ) ;
#110351 = CARTESIAN_POINT ( 'NONE',  ( -21.05000000000000071, 76.00000000001195133, -103.0231074845243171 ) ) ;
#110353 = EDGE_LOOP ( 'NONE', ( #208324, #118310, #249697, #196588 ) ) ;
#110352 = LINE ( 'NONE', #49090, #27737 ) ;
#110354 = ORIENTED_EDGE ( 'NONE', *, *, #59423, .F. ) ;
#110356 = DIRECTION ( 'NONE',  ( 1.000000000000000000, 0.000000000000000000, 0.000000000000000000 ) ) ;
#110355 = LINE ( 'NONE', #129911, #187209 ) ;
#110357 = B_SPLINE_CURVE_WITH_KNOTS ( 'NONE', 3,
 ( #210838, #115580, #92166, #189992 ),
 .UNSPECIFIED., .F., .F.,
 ( 4, 4 ),
 ( 0.000000000000000000, 0.0001048066582182725969 ),
 .UNSPECIFIED. ) ;
#110358 = ORIENTED_EDGE ( 'NONE', *, *, #66852, .F. ) ;
#110359 = ORIENTED_EDGE ( 'NONE', *, *, #132167, .T. ) ;
#110360 = DIRECTION ( 'NONE',  ( -0.000000000000000000, 0.2605042016806385363, 0.9654727137038795481 ) ) ;
#110361 = DIRECTION ( 'NONE',  ( 0.000000000000000000, 0.4999999999999608646, -0.8660254037844612451 ) ) ;
#110362 =( GEOMETRIC_REPRESENTATION_CONTEXT ( 3 ) GLOBAL_UNCERTAINTY_ASSIGNED_CONTEXT ( ( #149506 ) ) GLOBAL_UNIT_ASSIGNED_CONTEXT ( ( #59879, #136871, #139420 ) ) REPRESENTATION_CONTEXT ( 'NONE', 'WORKASPACE' ) );
#110363 = DIRECTION ( 'NONE',  ( 0.7071359030027680737, 0.7070776581709111719, 0.000000000000000000 ) ) ;
#110364 = PLANE ( 'NONE',  #56956 ) ;
#110365 = CARTESIAN_POINT ( 'NONE',  ( -21.04999999999994387, 87.50449464844290048, -37.85861909827351468 ) ) ;
#110366 = CARTESIAN_POINT ( 'NONE',  ( 18.54999999999999716, 12.98648691417778167, -219.5104337504080263 ) ) ;
#110367 = DIRECTION ( 'NONE',  ( 0.000000000000000000, 0.4088369013363281623, -0.9126074666063771490 ) ) ;
#110369 = VERTEX_POINT ( 'NONE', #201381 ) ;
#110368 = ADVANCED_FACE ( 'NONE', ( #129845 ), #41056, .F. ) ;
#110370 = ORIENTED_EDGE ( 'NONE', *, *, #481, .T. ) ;
#110371 = CARTESIAN_POINT ( 'NONE',  ( 18.69999999999999929, -11.65000000000000036, 30.09999999999999787 ) ) ;
#110372 = AXIS2_PLACEMENT_3D ( 'NONE', #206966, #171723, #10045 ) ;
#110373 = EDGE_CURVE ( 'NONE', #119503, #30937, #217074, .T. ) ;
#110374 = AXIS2_PLACEMENT_3D ( 'NONE', #251477, #211080, #250206 ) ;
#110375 = ORIENTED_EDGE ( 'NONE', *, *, #99174, .F. ) ;
#110376 = DIRECTION ( 'NONE',  ( 0.7071067811865474617, 0.7071067811865474617, -0.000000000000000000 ) ) ;
#110377 = ORIENTED_EDGE ( 'NONE', *, *, #140023, .F. ) ;
#110378 = CARTESIAN_POINT ( 'NONE',  ( -20.94999999999999929, 1.162701749938009677, -7.900000000000000355 ) ) ;
#110379 = AXIS2_PLACEMENT_3D ( 'NONE', #67260, #84195, #166399 ) ;
#110380 = CIRCLE ( 'NONE', #210360, 0.9000000000000014655 ) ;
#110381 =( BOUNDED_SURFACE ( )  B_SPLINE_SURFACE ( 3, 2, ( 
 ( #40827, #61642, #244119 ),
 ( #82455, #145013, #43371 ),
 ( #241561, #163320, #204978 ),
 ( #141185, #224555, #45928 ),
 ( #223269, #25110, #44653 ),
 ( #26377, #185446, #42105 ) ),
 .UNSPECIFIED., .F., .F., .T. ) 
 B_SPLINE_SURFACE_WITH_KNOTS ( ( 4, 2, 4 ),
 ( 3, 3 ),
 ( 0.0001381104793128061785, 0.0002947094729387477754, 0.0004513084665646893722 ),
 ( 0.000000000000000000, 1.000000000000000000 ),
 .UNSPECIFIED. ) 
 GEOMETRIC_REPRESENTATION_ITEM ( )  RATIONAL_B_SPLINE_SURFACE ( (
 ( 1.000000000000000000, 0.7071067811865494601, 1.000000000000000000),
 ( 1.000000000000000000, 0.6919563088097517856, 1.000000000000000000),
 ( 1.000000000000000000, 0.6959445945719651139, 1.000000000000000000),
 ( 1.000000000000000000, 0.7137882985310910477, 1.000000000000000000),
 ( 1.000000000000000000, 0.7257496306098256689, 1.000000000000000000),
 ( 1.000000000000000000, 0.7250110520819876836, 1.000000000000000000) ) ) 
 REPRESENTATION_ITEM ( '' )  SURFACE ( )  );
#110382 = DIRECTION ( 'NONE',  ( -1.000000000000000000, -0.000000000000000000, -0.000000000000000000 ) ) ;
#110383 = PRESENTATION_LAYER_ASSIGNMENT (  '', '', ( #206075 ) ) ;
#110384 = EDGE_CURVE ( 'NONE', #242360, #71456, #82814, .T. ) ;
#110386 = EDGE_CURVE ( 'NONE', #92871, #156136, #116203, .T. ) ;
#110385 = DIRECTION ( 'NONE',  ( 0.000000000000000000, -1.000000000000000000, 0.000000000000000000 ) ) ;
#110387 = EDGE_LOOP ( 'NONE', ( #171246, #157220, #201391, #230082 ) ) ;
#110388 = DIRECTION ( 'NONE',  ( -4.391705002472929091E-16, 1.000000000000000000, 0.000000000000000000 ) ) ;
#110389 = VERTEX_POINT ( 'NONE', #239228 ) ;
#110390 = PLANE ( 'NONE',  #123134 ) ;
#110391 = CARTESIAN_POINT ( 'NONE',  ( 23.14999999999998437, 12.67709964810647882, -223.3751320524553705 ) ) ;
#110392 = EDGE_LOOP ( 'NONE', ( #187517, #118106, #207609 ) ) ;
#110393 = DIRECTION ( 'NONE',  ( -1.000000000000000000, 0.000000000000000000, 0.000000000000000000 ) ) ;
#110394 = ORIENTED_EDGE ( 'NONE', *, *, #45803, .F. ) ;
#110397 = EDGE_LOOP ( 'NONE', ( #32211, #7882, #108419, #76558 ) ) ;
#110396 = CARTESIAN_POINT ( 'NONE',  ( 18.56579813702275317, 46.46179379974390855, -243.0832762246653260 ) ) ;
#110395 = CARTESIAN_POINT ( 'NONE',  ( -20.94999999999994600, 64.25000000001119815, -29.92310748452479174 ) ) ;
#110398 = CARTESIAN_POINT ( 'NONE',  ( 23.14999999999998437, 1.115650265596050101E-11, -96.45000000000003126 ) ) ;
#110400 = ORIENTED_EDGE ( 'NONE', *, *, #216467, .F. ) ;
#110399 = CIRCLE ( 'NONE', #131249, 0.1999999999999996503 ) ;
#110401 = CIRCLE ( 'NONE', #93840, 0.1000000000000028644 ) ;
#110402 = DIRECTION ( 'NONE',  ( 0.000000000000000000, -0.8814952561688438326, 0.4721928772777330696 ) ) ;
#110403 = EDGE_LOOP ( 'NONE', ( #130774, #190371, #106904, #22617 ) ) ;
#110404 = AXIS2_PLACEMENT_3D ( 'NONE', #163892, #222551, #28262 ) ;
#110405 = CARTESIAN_POINT ( 'NONE',  ( -18.50000000000000000, 61.63293978347611812, -221.5406706031726003 ) ) ;
#110406 = ORIENTED_EDGE ( 'NONE', *, *, #226891, .T. ) ;
#110407 = CARTESIAN_POINT ( 'NONE',  ( 20.85000000000000142, 14.73746888278882849, -235.8584165281851028 ) ) ;
#110408 = CARTESIAN_POINT ( 'NONE',  ( 18.59999999999999432, 74.36282728704190959, -158.4409541190523498 ) ) ;
#110409 = DIRECTION ( 'NONE',  ( 1.000000000000000000, 0.000000000000000000, 0.000000000000000000 ) ) ;
#110410 = AXIS2_PLACEMENT_3D ( 'NONE', #173894, #215530, #253375 ) ;
#110411 = CIRCLE ( 'NONE', #2061, 11.80000000000000426 ) ;
#110412 = VECTOR ( 'NONE', #61718, 1000.000000000000114 ) ;
#110413 = CARTESIAN_POINT ( 'NONE',  ( 20.95000000000005258, 64.35000000001120668, -30.12310748452479103 ) ) ;
#110414 = EDGE_LOOP ( 'NONE', ( #196741, #49111, #128881, #133925 ) ) ;
#110415 = DIRECTION ( 'NONE',  ( 0.000000000000000000, -0.1686199900910313187, 0.9856811345164828708 ) ) ;
#110416 = CARTESIAN_POINT ( 'NONE',  ( 20.94999999999999929, 70.50000000001223555, -148.9283735034374843 ) ) ;
#110417 = CARTESIAN_POINT ( 'NONE',  ( 18.52643265882457868, 10.31973158071402885, -139.5505334713354841 ) ) ;
#110418 = ORIENTED_EDGE ( 'NONE', *, *, #225831, .T. ) ;
#110419 = ADVANCED_FACE ( 'NONE', ( #218357 ), #3751, .F. ) ;
#110420 = DIRECTION ( 'NONE',  ( 0.000000000000000000, 0.000000000000000000, 1.000000000000000000 ) ) ;
#110421 = ORIENTED_EDGE ( 'NONE', *, *, #83553, .F. ) ;
#110422 = ORIENTED_EDGE ( 'NONE', *, *, #12355, .T. ) ;
#110423 = VECTOR ( 'NONE', #241617, 1000.000000000000000 ) ;
#110424 = AXIS2_PLACEMENT_3D ( 'NONE', #4764, #86871, #127310 ) ;
#110425 = DIRECTION ( 'NONE',  ( 0.000000000000000000, -0.000000000000000000, 1.000000000000000000 ) ) ;
#110426 = CARTESIAN_POINT ( 'NONE',  ( -22.39999999999999858, 76.10085836911117951, -181.7726746080137445 ) ) ;
#110428 = VERTEX_POINT ( 'NONE', #179285 ) ;
#110427 = CARTESIAN_POINT ( 'NONE',  ( 18.55857864376267941, 10.36715728753653565, -58.25000000000000711 ) ) ;
#110429 = FACE_OUTER_BOUND ( 'NONE', #154000, .T. ) ;
#110430 = ORIENTED_EDGE ( 'NONE', *, *, #209876, .T. ) ;
#110431 = AXIS2_PLACEMENT_3D ( 'NONE', #234165, #35992, #235442 ) ;
#110432 = ADVANCED_FACE ( 'NONE', ( #59259 ), #56700, .F. ) ;
#110433 = CARTESIAN_POINT ( 'NONE',  ( -20.94999999999999929, 36.18002604163306302, -236.0784499204090991 ) ) ;
#110434 = LINE ( 'NONE', #129981, #14539 ) ;
#110435 = EDGE_CURVE ( 'NONE', #176502, #248551, #137028, .T. ) ;
#110436 = ORIENTED_EDGE ( 'NONE', *, *, #26997, .T. ) ;
#110437 = CARTESIAN_POINT ( 'NONE',  ( 22.47071067811864609, 68.27992525551464098, -203.6221999392270448 ) ) ;
#110438 = DIRECTION ( 'NONE',  ( 1.000000000000000000, 0.000000000000000000, 0.000000000000000000 ) ) ;
#110439 = VERTEX_POINT ( 'NONE', #82685 ) ;
#110440 = CARTESIAN_POINT ( 'NONE',  ( 21.05000000000000071, -1.162701749926853712, -108.6000000000000227 ) ) ;
#110441 = ORIENTED_EDGE ( 'NONE', *, *, #207451, .T. ) ;
#110442 = EDGE_CURVE ( 'NONE', #154587, #112394, #99686, .T. ) ;
#110443 = DIRECTION ( 'NONE',  ( 0.000000000000000000, -0.8700118002898354908, 0.4930308989875170078 ) ) ;
#110444 = CARTESIAN_POINT ( 'NONE',  ( -21.05000000000000071, 12.71802988599559292, -223.5105008658000258 ) ) ;
#110445 = EDGE_CURVE ( 'NONE', #46944, #215317, #236985, .T. ) ;
#110446 = EDGE_CURVE ( 'NONE', #18666, #108495, #141299, .T. ) ;
#110448 = ORIENTED_EDGE ( 'NONE', *, *, #238420, .T. ) ;
#110447 = VERTEX_POINT ( 'NONE', #180550 ) ;
#110449 = AXIS2_PLACEMENT_3D ( 'NONE', #128657, #148202, #227734 ) ;
#110450 = CARTESIAN_POINT ( 'NONE',  ( -22.50000000000000000, 11.75000000000000000, -3.469446951953614189E-15 ) ) ;
#110451 = CARTESIAN_POINT ( 'NONE',  ( -22.49917693094574389, 0.08522996423282774847, -155.8502042154692901 ) ) ;
#110452 = CIRCLE ( 'NONE', #118863, 0.1000000000000054040 ) ;
#110453 = PLANE ( 'NONE',  #210817 ) ;
#110454 = EDGE_CURVE ( 'NONE', #195444, #14366, #240515, .T. ) ;
#110456 = CARTESIAN_POINT ( 'NONE',  ( 20.94999999999999929, 69.45000000001186891, -90.87310748452435405 ) ) ;
#110455 = CARTESIAN_POINT ( 'NONE',  ( -22.50000000000000000, 68.20922040163854660, -103.1231074845243540 ) ) ;
#110457 = FACE_OUTER_BOUND ( 'NONE', #78193, .T. ) ;
#110458 = DIRECTION ( 'NONE',  ( 1.000000000000000000, 0.000000000000000000, -0.000000000000000000 ) ) ;
#110459 = DIRECTION ( 'NONE',  ( 1.000000000000000000, 0.000000000000000000, 0.000000000000000000 ) ) ;
#110460 = CARTESIAN_POINT ( 'NONE',  ( -22.39999999999999858, 68.20922040163873135, -136.5231074845243313 ) ) ;
#110461 = ORIENTED_EDGE ( 'NONE', *, *, #170464, .T. ) ;
#110463 = VERTEX_POINT ( 'NONE', #121861 ) ;
#110462 = CIRCLE ( 'NONE', #251936, 11.70000000000000284 ) ;
#110464 = CARTESIAN_POINT ( 'NONE',  ( -20.64999999999999858, 46.10080905699345521, -240.6643289267983334 ) ) ;
#110465 = AXIS2_PLACEMENT_3D ( 'NONE', #102834, #100267, #2460 ) ;
#110467 = ORIENTED_EDGE ( 'NONE', *, *, #55179, .T. ) ;
#110466 = DIRECTION ( 'NONE',  ( 0.000000000000000000, -1.000000000000000000, 0.000000000000000000 ) ) ;
#110468 = VERTEX_POINT ( 'NONE', #116712 ) ;
#110469 = EDGE_CURVE ( 'NONE', #85685, #165864, #257445, .T. ) ;
#110470 = DIRECTION ( 'NONE',  ( 1.000000000000000000, 0.000000000000000000, 0.000000000000000000 ) ) ;
#110471 = EDGE_LOOP ( 'NONE', ( #68052, #29426, #146866, #179212, #252915, #129084, #117205 ) ) ;
#110472 = CARTESIAN_POINT ( 'NONE',  ( 21.07094088545304800, 33.98475570745946328, -243.8237622992367051 ) ) ;
#110473 = B_SPLINE_CURVE_WITH_KNOTS ( 'NONE', 3,
 ( #125094, #122526, #204601, #25989, #1259, #105478, #185048, #6408, #119981, #142062, #199503, #221585, #80790, #160386, #161665, #42983, #202054, #23445, #102925, #109343, #169385, #67668, #190200, #10281, #229327, #187640, #250166, #228032, #147206, #186349 ),
 .UNSPECIFIED., .F., .F.,
 ( 4, 2, 2, 2, 2, 2, 2, 2, 2, 2, 2, 2, 2, 2, 4 ),
 ( 0.000000000000000000, 0.0003422764154113400658, 0.0006845528308226801317, 0.001026829246234020306, 0.001369105661645360263, 0.002053658492468029336, 0.002738211323290697975, 0.003080487738702029476, 0.003422764154113361410, 0.003765040569524692477, 0.004107316984936024845, 0.004449593400347355912, 0.004791869815758687846, 0.005134146231170023250, 0.005476422646581358654 ),
 .UNSPECIFIED. ) ;
#110474 = ORIENTED_EDGE ( 'NONE', *, *, #242859, .F. ) ;
#110475 = VECTOR ( 'NONE', #226670, 1000.000000000000000 ) ;
#110476 = DIRECTION ( 'NONE',  ( 1.000000000000000000, -0.000000000000000000, 0.000000000000000000 ) ) ;
#110478 = EDGE_LOOP ( 'NONE', ( #164936, #191556, #215508, #133547 ) ) ;
#110477 = ORIENTED_EDGE ( 'NONE', *, *, #12072, .F. ) ;
#110479 = VERTEX_POINT ( 'NONE', #22776 ) ;
#110480 = ORIENTED_EDGE ( 'NONE', *, *, #77895, .F. ) ;
#110481 = ORIENTED_EDGE ( 'NONE', *, *, #67024, .T. ) ;
#110482 = DIRECTION ( 'NONE',  ( 1.000000000000000000, -2.952720810173289112E-16, -2.061873921506763405E-30 ) ) ;
#110483 = DIRECTION ( 'NONE',  ( 1.000000000000000000, 1.836970198721029934E-16, 0.000000000000000000 ) ) ;
#110484 = CARTESIAN_POINT ( 'NONE',  ( -12.25000000000000000, 9.350000000011132073, -184.3657431672738767 ) ) ;
#110486 = ORIENTED_EDGE ( 'NONE', *, *, #223417, .F. ) ;
#110485 = DIRECTION ( 'NONE',  ( -1.000000000000000000, -0.000000000000000000, -0.000000000000000000 ) ) ;
#110487 = AXIS2_PLACEMENT_3D ( 'NONE', #133527, #228791, #154419 ) ;
#110488 = DIRECTION ( 'NONE',  ( -6.938893903907222856E-15, 1.000000000000000000, 2.891205793294679805E-16 ) ) ;
#110489 = CARTESIAN_POINT ( 'NONE',  ( -22.59999999999999787, 11.74956712350054744, -167.3991416309012550 ) ) ;
#110491 = ORIENTED_EDGE ( 'NONE', *, *, #178765, .F. ) ;
#110490 = DIRECTION ( 'NONE',  ( 0.000000000000000000, 0.000000000000000000, 1.000000000000000000 ) ) ;
#110492 = DIRECTION ( 'NONE',  ( 1.000000000000000000, 0.000000000000000000, 0.000000000000000000 ) ) ;
#110493 = EDGE_LOOP ( 'NONE', ( #89496, #114494, #106598, #166808 ) ) ;
#110494 = CARTESIAN_POINT ( 'NONE',  ( 18.59999999999999787, -1.249999999988843369, -208.8004807544150481 ) ) ;
#110495 = VERTEX_POINT ( 'NONE', #102244 ) ;
#110496 = DIRECTION ( 'NONE',  ( -1.020425574104004196E-15, -0.000000000000000000, -1.000000000000000000 ) ) ;
#110497 = CARTESIAN_POINT ( 'NONE',  ( 21.14999999999999858, 10.71339244339988461, -12.25000000000000000 ) ) ;
#110498 = ORIENTED_EDGE ( 'NONE', *, *, #212387, .T. ) ;
#110500 = DIRECTION ( 'NONE',  ( 0.000000000000000000, -1.000000000000000000, -6.982962677686265922E-15 ) ) ;
#110499 = FACE_OUTER_BOUND ( 'NONE', #221467, .T. ) ;
#110501 = CARTESIAN_POINT ( 'NONE',  ( -18.50000000000000000, 66.65000000001229807, -157.8731074845244393 ) ) ;
#110502 = CIRCLE ( 'NONE', #143814, 12.97499999999998721 ) ;
#110503 = EDGE_CURVE ( 'NONE', #157637, #199601, #39778, .T. ) ;
#110504 = FACE_OUTER_BOUND ( 'NONE', #185146, .T. ) ;
#110505 = AXIS2_PLACEMENT_3D ( 'NONE', #110015, #7062, #207868 ) ;
#110506 = DIRECTION ( 'NONE',  ( 1.000000000000000000, 0.000000000000000000, 0.000000000000000000 ) ) ;
#110507 = VERTEX_POINT ( 'NONE', #117997 ) ;
#110508 = EDGE_LOOP ( 'NONE', ( #40735, #63359, #188259, #137379 ) ) ;
#110509 = CARTESIAN_POINT ( 'NONE',  ( 21.05000000000000071, 8.776282648971246658, -8.487592378520258052 ) ) ;
#110510 = DIRECTION ( 'NONE',  ( 1.000000000000000000, -0.000000000000000000, -0.000000000000000000 ) ) ;
#110511 = ORIENTED_EDGE ( 'NONE', *, *, #238472, .T. ) ;
#110512 = DIRECTION ( 'NONE',  ( 0.000000000000000000, -0.9651348961777157509, 0.2617529984165031243 ) ) ;
#110513 = ORIENTED_EDGE ( 'NONE', *, *, #189173, .F. ) ;
#110514 = FACE_OUTER_BOUND ( 'NONE', #15293, .T. ) ;
#110515 = EDGE_CURVE ( 'NONE', #117707, #67207, #158104, .T. ) ;
#110516 = DIRECTION ( 'NONE',  ( -1.000000000000000000, -0.000000000000000000, -0.000000000000000000 ) ) ;
#110517 = EDGE_CURVE ( 'NONE', #91491, #134169, #87308, .T. ) ;
#110518 = EDGE_CURVE ( 'NONE', #124526, #7935, #177988, .T. ) ;
#110519 = ORIENTED_EDGE ( 'NONE', *, *, #66839, .F. ) ;
#110520 = B_SPLINE_CURVE_WITH_KNOTS ( 'NONE', 3,
 ( #132662, #192638, #173117, #29739, #252588, #171821 ),
 .UNSPECIFIED., .F., .F.,
 ( 4, 2, 4 ),
 ( 0.000000000000000000, 0.0001497467027049069303, 0.0002994934054098138607 ),
 .UNSPECIFIED. ) ;
#110521 = LINE ( 'NONE', #229204, #119266 ) ;
#110522 = VECTOR ( 'NONE', #149341, 1000.000000000000000 ) ;
#110523 = ORIENTED_EDGE ( 'NONE', *, *, #108806, .F. ) ;
#110524 = EDGE_LOOP ( 'NONE', ( #244124, #215610 ) ) ;
#110525 = EDGE_LOOP ( 'NONE', ( #78374, #225188, #29681, #177298 ) ) ;
#110526 = CARTESIAN_POINT ( 'NONE',  ( -21.05000000000000071, 1.115600667400684642E-11, -171.7999999999999545 ) ) ;
#110527 = CARTESIAN_POINT ( 'NONE',  ( 14.22821877134046176, 66.54397173950364675, -54.51190944945866335 ) ) ;
#110528 = CIRCLE ( 'NONE', #106226, 0.09999999999999939493 ) ;
#110529 = DIRECTION ( 'NONE',  ( 1.000000000000000000, -7.304098846218135653E-16, -5.100424963727256530E-30 ) ) ;
#110530 = FACE_OUTER_BOUND ( 'NONE', #21710, .T. ) ;
#110531 = FACE_OUTER_BOUND ( 'NONE', #177599, .T. ) ;
#110532 = EDGE_CURVE ( 'NONE', #92460, #166897, #138800, .T. ) ;
#110534 = SPHERICAL_SURFACE ( 'NONE', #36677, 0.1000000000000000056 ) ;
#110533 = CARTESIAN_POINT ( 'NONE',  ( -21.53752568617687047, 10.24627015979678291, -227.7034273308914578 ) ) ;
#110536 = ORIENTED_EDGE ( 'NONE', *, *, #130062, .T. ) ;
#110535 = DIRECTION ( 'NONE',  ( 1.073024830501117725E-15, 0.000000000000000000, 1.000000000000000000 ) ) ;
#110537 = DIRECTION ( 'NONE',  ( 1.284434275755705296E-16, -0.7071067811865471286, 0.7071067811865479058 ) ) ;
#110538 = VERTEX_POINT ( 'NONE', #163546 ) ;
#110539 = ADVANCED_FACE ( 'NONE', ( #86544 ), #126986, .T. ) ;
#110540 = CARTESIAN_POINT ( 'NONE',  ( -16.87845715379269507, 22.95868340314714118, -230.9157653750406496 ) ) ;
#110541 = ORIENTED_EDGE ( 'NONE', *, *, #68486, .F. ) ;
#110542 = VERTEX_POINT ( 'NONE', #65729 ) ;
#110543 = CARTESIAN_POINT ( 'NONE',  ( -18.50000000000000000, 4.064367954407505756, -211.9684786640956418 ) ) ;
#110544 = CARTESIAN_POINT ( 'NONE',  ( -23.25000000000000000, 43.35377423437995503, -245.1717807829448930 ) ) ;
#110545 = DIRECTION ( 'NONE',  ( 1.000000000000000000, 0.000000000000000000, 0.000000000000000000 ) ) ;
#110546 = CARTESIAN_POINT ( 'NONE',  ( -20.94999999999999929, 74.83729825007408465, -128.6231074845242972 ) ) ;
#110547 = CIRCLE ( 'NONE', #102135, 0.1000000000000028644 ) ;
#110548 = AXIS2_PLACEMENT_3D ( 'NONE', #168035, #186286, #7642 ) ;
#110549 = DIRECTION ( 'NONE',  ( 0.000000000000000000, -0.9908441862701610203, 0.1350103645451807555 ) ) ;
#110550 = VERTEX_POINT ( 'NONE', #244352 ) ;
#110551 = EDGE_LOOP ( 'NONE', ( #171066, #218241, #84213, #194242 ) ) ;
#110552 = EDGE_CURVE ( 'NONE', #86798, #61130, #228801, .T. ) ;
#110553 = LINE ( 'NONE', #87129, #223971 ) ;
#110555 = ORIENTED_EDGE ( 'NONE', *, *, #183393, .F. ) ;
#110554 = ADVANCED_FACE ( 'NONE', ( #104815 ), #166154, .T. ) ;
#110556 = CARTESIAN_POINT ( 'NONE',  ( 19.99999999999998934, 11.75000000000000355, -24.85000000000000142 ) ) ;
#110557 = DIRECTION ( 'NONE',  ( 0.000000000000000000, -1.000000000000000000, 0.000000000000000000 ) ) ;
#110558 = ORIENTED_EDGE ( 'NONE', *, *, #60262, .T. ) ;
#110559 = ADVANCED_FACE ( 'NONE', ( #145250 ), #26627, .T. ) ;
#110560 = DIRECTION ( 'NONE',  ( 0.000000000000000000, -0.2128009952263606175, 0.9770955615653315052 ) ) ;
#110561 = DIRECTION ( 'NONE',  ( 0.000000000000000000, -0.1335171055202867274, -0.9910465087640866200 ) ) ;
#110562 = DIRECTION ( 'NONE',  ( 0.000000000000000000, 0.9126074666063771490, 0.4088369013363278293 ) ) ;
#110563 = DIRECTION ( 'NONE',  ( 1.000000000000000000, 0.000000000000000000, 0.000000000000000000 ) ) ;
#110564 = VERTEX_POINT ( 'NONE', #226051 ) ;
#110565 = CARTESIAN_POINT ( 'NONE',  ( -5.900000000000003020, -11.34999999999999964, 10.10000000000000142 ) ) ;
#110566 = CARTESIAN_POINT ( 'NONE',  ( 20.94999999999999929, 85.40000000001221281, -146.4170766071767389 ) ) ;
#110567 = DIRECTION ( 'NONE',  ( 1.000000000000000000, -0.000000000000000000, -0.000000000000000000 ) ) ;
#110568 = DIRECTION ( 'NONE',  ( -0.000000000000000000, 0.000000000000000000, 1.000000000000000000 ) ) ;
#110569 = CARTESIAN_POINT ( 'NONE',  ( -20.00857864376270001, 66.85000000001254250, -182.3731074845244393 ) ) ;
#110570 = EDGE_CURVE ( 'NONE', #256994, #129211, #202666, .T. ) ;
#110571 = CARTESIAN_POINT ( 'NONE',  ( 23.24999999999999645, 76.00000000001213607, -136.5231074845243313 ) ) ;
#110572 = MANIFOLD_SOLID_BREP ( 'Stock-MAS-200-1', #28367 ) ;
#110573 = AXIS2_PLACEMENT_3D ( 'NONE', #183502, #240912, #162663 ) ;
#110574 = AXIS2_PLACEMENT_3D ( 'NONE', #205840, #148448, #71491 ) ;
#110575 = VECTOR ( 'NONE', #93764, 1000.000000000000000 ) ;
#110576 = VERTEX_POINT ( 'NONE', #4459 ) ;
#110577 = DIRECTION ( 'NONE',  ( 1.000000000000000000, 0.000000000000000000, 0.000000000000000000 ) ) ;
#110578 = ORIENTED_EDGE ( 'NONE', *, *, #116209, .T. ) ;
#110579 = LINE ( 'NONE', #33666, #126609 ) ;
#110580 = DIRECTION ( 'NONE',  ( -0.000000000000000000, -0.000000000000000000, 1.000000000000000000 ) ) ;
#110581 = CARTESIAN_POINT ( 'NONE',  ( -23.15000000000000213, 84.59626168225560150, -194.0729799673740104 ) ) ;
#110582 = FACE_OUTER_BOUND ( 'NONE', #133575, .T. ) ;
#110583 = CARTESIAN_POINT ( 'NONE',  ( 21.07928932188134397, 65.47931918658503037, -241.9371126717015841 ) ) ;
#110584 = ORIENTED_EDGE ( 'NONE', *, *, #125044, .F. ) ;
#110585 = ADVANCED_FACE ( 'NONE', ( #83955 ), #243075, .T. ) ;
#110586 = CARTESIAN_POINT ( 'NONE',  ( -18.50000000000000000, -1.736257131586239844, -78.56865232901753870 ) ) ;
#110587 = CARTESIAN_POINT ( 'NONE',  ( -20.85000000000000142, -1.249999999988843369, -141.8004807544151333 ) ) ;
#110588 = CARTESIAN_POINT ( 'NONE',  ( -18.50000000000000355, 77.26327546522934142, -128.6212428177779543 ) ) ;
#110589 = FACE_OUTER_BOUND ( 'NONE', #203223, .T. ) ;
#110590 = AXIS2_PLACEMENT_3D ( 'NONE', #71325, #53011, #150836 ) ;
#110591 = DIRECTION ( 'NONE',  ( 0.000000000000000000, 0.000000000000000000, -1.000000000000000000 ) ) ;
#110592 = AXIS2_PLACEMENT_3D ( 'NONE', #211091, #49450, #32490 ) ;
#110593 = ORIENTED_EDGE ( 'NONE', *, *, #37285, .F. ) ;
#110594 = ORIENTED_EDGE ( 'NONE', *, *, #56886, .T. ) ;
#110595 = CARTESIAN_POINT ( 'NONE',  ( 18.49999999999998934, 63.62814136979439184, -224.4990371885399441 ) ) ;
#110596 = DIRECTION ( 'NONE',  ( -0.7071067811865463515, -0.7071067811865487940, -4.937700262164540154E-15 ) ) ;
#110598 = ADVANCED_FACE ( 'NONE', ( #44887 ), #203951, .F. ) ;
#110597 = CYLINDRICAL_SURFACE ( 'NONE', #130907, 0.1000000000000000472 ) ;
#110599 = LINE ( 'NONE', #8941, #257800 ) ;
#110600 = AXIS2_PLACEMENT_3D ( 'NONE', #232552, #233816, #197246 ) ;
#110601 = EDGE_LOOP ( 'NONE', ( #127811, #41601, #161770, #68530 ) ) ;
#110602 = DIRECTION ( 'NONE',  ( 1.000000000000000000, 0.000000000000000000, 0.000000000000000000 ) ) ;
#110603 = CIRCLE ( 'NONE', #256269, 0.1000000000000027117 ) ;
#110604 = EDGE_CURVE ( 'NONE', #191967, #91362, #128848, .T. ) ;
#110605 = CONTEXT_DEPENDENT_SHAPE_REPRESENTATION ( #215714, #195313 ) ;
#110606 = AXIS2_PLACEMENT_3D ( 'NONE', #122886, #42074, #81159 ) ;
#110607 = AXIS2_PLACEMENT_3D ( 'NONE', #29053, #147677, #148977 ) ;
#110608 = DIRECTION ( 'NONE',  ( 1.000000000000000000, 2.952720810173289112E-16, -0.000000000000000000 ) ) ;
#110609 = ORIENTED_EDGE ( 'NONE', *, *, #216957, .T. ) ;
#110610 = DIRECTION ( 'NONE',  ( -1.000000000000000000, 0.000000000000000000, 0.000000000000000000 ) ) ;
#110611 = ADVANCED_FACE ( 'NONE', ( #18456 ), #241370, .F. ) ;
#110612 = AXIS2_PLACEMENT_3D ( 'NONE', #240991, #220148, #118489 ) ;
#110613 = EDGE_CURVE ( 'NONE', #126714, #140417, #83000, .T. ) ;
#110614 = ORIENTED_EDGE ( 'NONE', *, *, #62969, .F. ) ;
#110616 = ORIENTED_EDGE ( 'NONE', *, *, #12507, .F. ) ;
#110615 = TOROIDAL_SURFACE ( 'NONE', #243708, 0.6000000000000009770, 0.1000000000000000056 ) ;
#110617 = ORIENTED_EDGE ( 'NONE', *, *, #181233, .T. ) ;
#110618 = CARTESIAN_POINT ( 'NONE',  ( 20.99999999999999645, 66.25000000001188027, -90.37310748452436826 ) ) ;
#110619 = CARTESIAN_POINT ( 'NONE',  ( 20.94999999999999929, 0.000000000000000000, -33.50000000000000000 ) ) ;
#110620 = CARTESIAN_POINT ( 'NONE',  ( -20.64999999999999858, 2.399999999999999467, -13.22462192276210224 ) ) ;
#110621 = AXIS2_PLACEMENT_3D ( 'NONE', #167074, #207466, #210034 ) ;
#110622 = CARTESIAN_POINT ( 'NONE',  ( -23.25000000000000000, 77.25000000001209344, -128.7226267301092548 ) ) ;
#110623 = LINE ( 'NONE', #74101, #40536 ) ;
#110624 = DIRECTION ( 'NONE',  ( 0.000000000000000000, -0.000000000000000000, 1.000000000000000000 ) ) ;
#110625 = CARTESIAN_POINT ( 'NONE',  ( -16.94037747912386394, 10.01353938248632858, -12.55113095797549327 ) ) ;
#110627 = DIRECTION ( 'NONE',  ( 0.000000000000000000, 0.9126074666063773710, 0.4088369013363274962 ) ) ;
#110626 = DIRECTION ( 'NONE',  ( -1.000000000000000000, 0.000000000000000000, -3.469446951953635015E-14 ) ) ;
#110628 = EDGE_CURVE ( 'NONE', #40042, #166959, #78417, .T. ) ;
#110629 = CARTESIAN_POINT ( 'NONE',  ( -18.69999999999999929, 0.000000000000000000, 0.000000000000000000 ) ) ;
#110630 = LINE ( 'NONE', #229307, #251998 ) ;
#110631 = DIRECTION ( 'NONE',  ( 0.000000000000000000, 0.000000000000000000, 1.000000000000000000 ) ) ;
#110632 = CARTESIAN_POINT ( 'NONE',  ( -23.15000000000000213, 13.96869538424788360, -210.3925794786332233 ) ) ;
#110633 = ORIENTED_EDGE ( 'NONE', *, *, #83187, .T. ) ;
#110634 = VERTEX_POINT ( 'NONE', #140988 ) ;
#110635 = DIRECTION ( 'NONE',  ( 0.000000000000000000, 0.000000000000000000, 1.000000000000000000 ) ) ;
#110636 = EDGE_CURVE ( 'NONE', #238440, #99338, #16426, .T. ) ;
#110637 = CARTESIAN_POINT ( 'NONE',  ( -18.59999999999999787, -9.399999999988851940, -207.8820418481726335 ) ) ;
#110638 = PLANE ( 'NONE',  #53529 ) ;
#110639 = LINE ( 'NONE', #151061, #35256 ) ;
#110641 = ADVANCED_FACE ( 'NONE', ( #2725 ), #142250, .T. ) ;
#110640 = DIRECTION ( 'NONE',  ( 0.000000000000000000, 0.000000000000000000, 1.000000000000000000 ) ) ;
#110642 = LINE ( 'NONE', #149798, #2462 ) ;
#110643 =( REPRESENTATION_RELATIONSHIP ('NONE','NONE', #36900, #18588 ) REPRESENTATION_RELATIONSHIP_WITH_TRANSFORMATION ( #25947 )SHAPE_REPRESENTATION_RELATIONSHIP( ) );
#110644 = EDGE_LOOP ( 'NONE', ( #240123, #254965, #257647, #90745 ) ) ;
#110645 = ORIENTED_EDGE ( 'NONE', *, *, #132398, .T. ) ;
#110646 = AXIS2_PLACEMENT_3D ( 'NONE', #91466, #52306, #15806 ) ;
#110647 = ADVANCED_FACE ( 'NONE', ( #216653 ), #60063, .F. ) ;
#110648 = AXIS2_PLACEMENT_3D ( 'NONE', #111077, #186786, #189342 ) ;
#110649 = CARTESIAN_POINT ( 'NONE',  ( 20.04142135623730070, 11.65000000000000391, -24.65000000000000213 ) ) ;
#110650 = ORIENTED_EDGE ( 'NONE', *, *, #212973, .F. ) ;
#110651 = FACE_OUTER_BOUND ( 'NONE', #207318, .T. ) ;
#110652 = VECTOR ( 'NONE', #253742, 1000.000000000000000 ) ;
#110653 = EDGE_CURVE ( 'NONE', #118654, #200940, #199687, .T. ) ;
#110654 = AXIS2_PLACEMENT_3D ( 'NONE', #251540, #93751, #209867 ) ;
#110655 = ORIENTED_EDGE ( 'NONE', *, *, #132375, .F. ) ;
#110656 = DIRECTION ( 'NONE',  ( 1.000000000000000000, -0.000000000000000000, -0.000000000000000000 ) ) ;
#110657 = ORIENTED_EDGE ( 'NONE', *, *, #75332, .T. ) ;
#110658 = EDGE_CURVE ( 'NONE', #250043, #140759, #69146, .T. ) ;
#110660 = CIRCLE ( 'NONE', #94084, 0.1000000000000028644 ) ;
#110659 = DIRECTION ( 'NONE',  ( 0.000000000000000000, 0.8814952561688428334, -0.4721928772777349570 ) ) ;
#110661 = EDGE_CURVE ( 'NONE', #175518, #95323, #149710, .T. ) ;
#110663 = CIRCLE ( 'NONE', #185685, 0.09999999999999939493 ) ;
#110662 = LINE ( 'NONE', #11583, #228593 ) ;
#110664 = DIRECTION ( 'NONE',  ( 1.000000000000000000, 0.000000000000000000, 0.000000000000000000 ) ) ;
#110665 = CARTESIAN_POINT ( 'NONE',  ( 18.47073956224757296, -9.471729412460623720, -141.1086857528176779 ) ) ;
#110666 = CARTESIAN_POINT ( 'NONE',  ( -21.45000000000000284, 7.708578643762696636, -21.25000000000000000 ) ) ;
#110667 = CARTESIAN_POINT ( 'NONE',  ( -21.53752568622136820, 0.09897446127752260181, -60.21319212545143529 ) ) ;
#110668 = AXIS2_PLACEMENT_3D ( 'NONE', #8300, #224746, #69559 ) ;
#110669 = CARTESIAN_POINT ( 'NONE',  ( -23.39999999999994529, 64.35000000001120668, -3.123107484524795474 ) ) ;
#110670 = LINE ( 'NONE', #54541, #232962 ) ;
#110672 = ORIENTED_EDGE ( 'NONE', *, *, #26855, .T. ) ;
#110671 = CARTESIAN_POINT ( 'NONE',  ( 18.40000000000000213, -0.6805341177324860658, -242.5179126613615495 ) ) ;
#110674 = CARTESIAN_POINT ( 'NONE',  ( -18.39999999999999858, 64.52683809664912928, -60.19716141771643692 ) ) ;
#110673 = CARTESIAN_POINT ( 'NONE',  ( -21.05000000000000071, 6.540656951701240729, -0.09999999999999939493 ) ) ;
#110675 = ORIENTED_EDGE ( 'NONE', *, *, #74926, .T. ) ;
#110677 = ORIENTED_EDGE ( 'NONE', *, *, #170066, .T. ) ;
#110676 = SURFACE_STYLE_FILL_AREA ( #111977 ) ;
#110678 = VERTEX_POINT ( 'NONE', #207383 ) ;
#110679 = CARTESIAN_POINT ( 'NONE',  ( -20.54999999999999716, -8.999999999988846255, -109.8939691226524786 ) ) ;
#110680 = CARTESIAN_POINT ( 'NONE',  ( -20.54999999999999716, 73.60000000001177511, -79.41707660717676731 ) ) ;
#110681 = CARTESIAN_POINT ( 'NONE',  ( 20.94560253601876809, 62.83003337064300808, -207.1937220765705376 ) ) ;
#110682 = CARTESIAN_POINT ( 'NONE',  ( -23.25000000000000000, -5.011722593499800205, -233.2041167654973322 ) ) ;
#110684 = CARTESIAN_POINT ( 'NONE',  ( 20.04999999999999716, 8.750000000011173285, -54.35000000000000142 ) ) ;
#110683 = CIRCLE ( 'NONE', #164673, 11.75000000000001066 ) ;
#110685 = CARTESIAN_POINT ( 'NONE',  ( -18.59999999999999787, 79.11538813396778380, -196.3722783875038544 ) ) ;
#110686 = CARTESIAN_POINT ( 'NONE',  ( -20.54999999999999716, 76.00000000001246292, -172.0231074845243597 ) ) ;
#110687 = DIRECTION ( 'NONE',  ( 1.000000000000000000, 0.000000000000000000, 0.000000000000000000 ) ) ;
#110688 = DIRECTION ( 'NONE',  ( 0.000000000000000000, 0.1350103645451904977, 0.9908441862701596881 ) ) ;
#110689 = VERTEX_POINT ( 'NONE', #108277 ) ;
#110690 = ORIENTED_EDGE ( 'NONE', *, *, #46532, .F. ) ;
#110691 = B_SPLINE_CURVE_WITH_KNOTS ( 'NONE', 3,
 ( #137021, #216552, #11963, #71924 ),
 .UNSPECIFIED., .F., .F.,
 ( 4, 4 ),
 ( 0.000000000000000000, 0.001767853679387115145 ),
 .UNSPECIFIED. ) ;
#110692 = CARTESIAN_POINT ( 'NONE',  ( -16.94389599338512298, 9.991197989766199328, -180.1076448018102099 ) ) ;
#110693 = AXIS2_PLACEMENT_3D ( 'NONE', #47665, #148078, #28154 ) ;
#110694 = TOROIDAL_SURFACE ( 'NONE', #185716, 0.2000000000000000111, 0.1000000000000000056 ) ;
#110695 = EDGE_CURVE ( 'NONE', #170246, #165391, #245546, .T. ) ;
#110696 = EDGE_LOOP ( 'NONE', ( #189458, #3612, #153813, #157749, #63295 ) ) ;
#110697 = TOROIDAL_SURFACE ( 'NONE', #206378, 0.2000000000000000111, 0.1000000000000000056 ) ;
#110699 = CARTESIAN_POINT ( 'NONE',  ( 21.05000000000000071, 1.115600667400684642E-11, -46.37500000000000000 ) ) ;
#110698 = TOROIDAL_SURFACE ( 'NONE', #144569, 0.2000000000000000111, 0.1000000000000000056 ) ;
#110700 = VERTEX_POINT ( 'NONE', #28781 ) ;
#110701 = CARTESIAN_POINT ( 'NONE',  ( 5.900000000000055422, 64.75000000001119815, -36.02310748452479316 ) ) ;
#110702 = CARTESIAN_POINT ( 'NONE',  ( -20.00857864376270001, 66.65000000001259650, -191.2731074845244166 ) ) ;
#110703 = CARTESIAN_POINT ( 'NONE',  ( -22.45372860728439690, -2.464509553302064671, -189.6138598038565419 ) ) ;
#110704 = DIRECTION ( 'NONE',  ( 0.000000000000000000, 0.000000000000000000, 1.000000000000000000 ) ) ;
#110705 = DIRECTION ( 'NONE',  ( -4.391705002472928105E-16, 0.9770955615653315052, 0.2128009952263601179 ) ) ;
#110706 = ORIENTED_EDGE ( 'NONE', *, *, #213915, .F. ) ;
#110707 = CARTESIAN_POINT ( 'NONE',  ( 23.14999999999999503, 17.01923898301590654, -224.3994341343041867 ) ) ;
#110708 = CARTESIAN_POINT ( 'NONE',  ( -17.01473183483382812, 9.950000000011137047, -180.2499999999999716 ) ) ;
#110709 = DIRECTION ( 'NONE',  ( 0.7071359030028113724, 0.000000000000000000, -0.7070776581708677622 ) ) ;
#110710 = DIRECTION ( 'NONE',  ( 0.000000000000000000, 0.4088369013363281068, -0.9126074666063770380 ) ) ;
#110712 = EDGE_CURVE ( 'NONE', #200905, #200766, #8221, .T. ) ;
#110711 = DIRECTION ( 'NONE',  ( 0.000000000000000000, 1.000000000000000000, 0.000000000000000000 ) ) ;
#110713 = ORIENTED_EDGE ( 'NONE', *, *, #228054, .T. ) ;
#110714 = VECTOR ( 'NONE', #5616, 1000.000000000000114 ) ;
#110716 = CARTESIAN_POINT ( 'NONE',  ( -23.15000000000000213, 28.00279607545604676, -239.9795148779844283 ) ) ;
#110715 = CARTESIAN_POINT ( 'NONE',  ( -21.53752568617681007, 6.786807874514923178, -133.9010255387155723 ) ) ;
#110717 = ORIENTED_EDGE ( 'NONE', *, *, #110016, .T. ) ;
#110720 = ORIENTED_EDGE ( 'NONE', *, *, #211524, .T. ) ;
#110719 = CARTESIAN_POINT ( 'NONE',  ( -16.85939681242906474, 51.35418898951247968, -232.1141021923019707 ) ) ;
#110718 = DIRECTION ( 'NONE',  ( -1.000000000000000000, 0.000000000000000000, 0.000000000000000000 ) ) ;
#110721 = DIRECTION ( 'NONE',  ( 0.000000000000000000, 1.000000000000000000, 0.000000000000000000 ) ) ;
#110722 = CARTESIAN_POINT ( 'NONE',  ( -21.05000000000000071, 34.10170768283902021, -243.5983364837296392 ) ) ;
#110723 = DIRECTION ( 'NONE',  ( 0.000000000000000000, 0.9999631594459055250, 0.008583690987131395445 ) ) ;
#110724 = CIRCLE ( 'NONE', #73158, 0.1000000000000118433 ) ;
#110725 = ORIENTED_EDGE ( 'NONE', *, *, #221183, .T. ) ;
#110726 = FACE_OUTER_BOUND ( 'NONE', #163371, .T. ) ;
#110728 = DIRECTION ( 'NONE',  ( 1.000000000000000000, 7.492892343619937423E-30, -1.073024830501117725E-15 ) ) ;
#110727 = FACE_OUTER_BOUND ( 'NONE', #228422, .T. ) ;
#110730 = ORIENTED_EDGE ( 'NONE', *, *, #177385, .F. ) ;
#110729 = DIRECTION ( 'NONE',  ( 1.000000000000000000, 0.000000000000000000, 0.000000000000000000 ) ) ;
#110731 = VERTEX_POINT ( 'NONE', #46984 ) ;
#110732 = LINE ( 'NONE', #190291, #57543 ) ;
#110733 = DIRECTION ( 'NONE',  ( 0.000000000000000000, -0.9371753822965314118, 0.3488585713686133682 ) ) ;
#110734 = LINE ( 'NONE', #149890, #25952 ) ;
#110735 = VERTEX_POINT ( 'NONE', #203518 ) ;
#110736 = CARTESIAN_POINT ( 'NONE',  ( -23.15000000000000213, 64.35000000001156195, -57.27310748452440237 ) ) ;
#110737 = CARTESIAN_POINT ( 'NONE',  ( 23.24999999999999289, 64.35000000001221565, -148.2731074845243882 ) ) ;
#110738 = CARTESIAN_POINT ( 'NONE',  ( 21.05000000000000071, 71.00000000001186606, -90.61784146561124942 ) ) ;
#110739 = EDGE_LOOP ( 'NONE', ( #207585, #103094, #54208, #217085 ) ) ;
#110740 = CARTESIAN_POINT ( 'NONE',  ( 20.11144452913859837, 59.70930804554667759, -225.6397765276010716 ) ) ;
#110741 = DIRECTION ( 'NONE',  ( 0.000000000000000000, 0.1568667991644863147, -0.9876197685951252359 ) ) ;
#110742 = ADVANCED_FACE ( 'NONE', ( #223068 ), #129118, .T. ) ;
#110743 = ORIENTED_EDGE ( 'NONE', *, *, #229460, .T. ) ;
#110744 = CIRCLE ( 'NONE', #256428, 3.999999999999999112 ) ;
#110745 = DIRECTION ( 'NONE',  ( -0.000000000000000000, 1.000000000000000000, 0.000000000000000000 ) ) ;
#110746 = DIRECTION ( 'NONE',  ( 1.000000000000000000, 0.000000000000000000, 0.000000000000000000 ) ) ;
#110747 = AXIS2_PLACEMENT_3D ( 'NONE', #50091, #244440, #65807 ) ;
#110748 = CIRCLE ( 'NONE', #81492, 12.87499999999999822 ) ;
#110749 = AXIS2_PLACEMENT_3D ( 'NONE', #249020, #52059, #149922 ) ;
#110750 = ORIENTED_EDGE ( 'NONE', *, *, #199970, .T. ) ;
#110751 = VERTEX_POINT ( 'NONE', #147393 ) ;
#110752 = ADVANCED_FACE ( 'NONE', ( #166997 ), #66582, .T. ) ;
#110753 = DIRECTION ( 'NONE',  ( -0.000000000000000000, -6.982962677686266711E-15, 1.000000000000000000 ) ) ;
#110754 = VERTEX_POINT ( 'NONE', #106968 ) ;
#110756 = ORIENTED_EDGE ( 'NONE', *, *, #200873, .F. ) ;
#110755 = CARTESIAN_POINT ( 'NONE',  ( 12.25000000000000000, 66.65000000001258229, -186.7731074845244166 ) ) ;
#110757 = ADVANCED_FACE ( 'NONE', ( #45721 ), #183950, .T. ) ;
#110758 = ORIENTED_EDGE ( 'NONE', *, *, #111779, .F. ) ;
#110761 = ORIENTED_EDGE ( 'NONE', *, *, #194341, .T. ) ;
#110760 = ORIENTED_EDGE ( 'NONE', *, *, #55565, .F. ) ;
#110759 = DIRECTION ( 'NONE',  ( 0.000000000000000000, 6.982962677686266711E-15, -1.000000000000000000 ) ) ;
#110762 = CARTESIAN_POINT ( 'NONE',  ( -18.33682934331516279, -9.511185591082426782, -107.4056547686733580 ) ) ;
#110764 = ADVANCED_FACE ( 'NONE', ( #5280 ), #228225, .T. ) ;
#110763 = ORIENTED_EDGE ( 'NONE', *, *, #183604, .F. ) ;
#110765 = CARTESIAN_POINT ( 'NONE',  ( -23.15000000000000213, 87.65000000001172964, -72.62310748452422615 ) ) ;
#110766 = CARTESIAN_POINT ( 'NONE',  ( -23.15000000000000213, -8.999999999988846255, -76.89396912265249284 ) ) ;
#110767 = CIRCLE ( 'NONE', #206630, 0.2000000000000057288 ) ;
#110768 = DIRECTION ( 'NONE',  ( 1.000000000000000000, 0.000000000000000000, 0.000000000000000000 ) ) ;
#110769 = DIRECTION ( 'NONE',  ( 0.000000000000000000, 0.000000000000000000, -1.000000000000000000 ) ) ;
#110771 = VERTEX_POINT ( 'NONE', #125269 ) ;
#110770 = TOROIDAL_SURFACE ( 'NONE', #94196, 3.899999999999999467, 0.1000000000000000056 ) ;
#110772 = ORIENTED_EDGE ( 'NONE', *, *, #77516, .T. ) ;
#110773 = ORIENTED_EDGE ( 'NONE', *, *, #144522, .F. ) ;
#110774 = CARTESIAN_POINT ( 'NONE',  ( 21.03675099975492202, 8.875180032795963569, -146.3255421367780968 ) ) ;
#110776 = ORIENTED_EDGE ( 'NONE', *, *, #97919, .F. ) ;
#110775 = DIRECTION ( 'NONE',  ( 0.000000000000000000, 0.000000000000000000, 1.000000000000000000 ) ) ;
#110778 = DIRECTION ( 'NONE',  ( -1.000000000000000000, 0.000000000000000000, 0.000000000000000000 ) ) ;
#110777 = CIRCLE ( 'NONE', #6729, 3.900000000000002132 ) ;
#110780 = ORIENTED_EDGE ( 'NONE', *, *, #173663, .T. ) ;
#110779 = FACE_OUTER_BOUND ( 'NONE', #207838, .T. ) ;
#110781 = EDGE_CURVE ( 'NONE', #157888, #203753, #137204, .T. ) ;
#110782 = ORIENTED_EDGE ( 'NONE', *, *, #10208, .T. ) ;
#110783 = DIRECTION ( 'NONE',  ( -0.000000000000000000, -1.000000000000000000, -0.000000000000000000 ) ) ;
#110784 = CIRCLE ( 'NONE', #35968, 4.049999999999995381 ) ;
#110785 = ORIENTED_EDGE ( 'NONE', *, *, #73845, .F. ) ;
#110786 = CARTESIAN_POINT ( 'NONE',  ( -16.79270642812298320, 9.946244216949343908, -180.1610667214370665 ) ) ;
#110787 = DIRECTION ( 'NONE',  ( 1.000000000000000000, 0.000000000000000000, 0.000000000000000000 ) ) ;
#110790 = ORIENTED_EDGE ( 'NONE', *, *, #178888, .F. ) ;
#110789 = ORIENTED_EDGE ( 'NONE', *, *, #202074, .T. ) ;
#110788 = AXIS2_PLACEMENT_3D ( 'NONE', #72637, #230405, #51738 ) ;
#110791 = EDGE_LOOP ( 'NONE', ( #207311, #160295, #199007, #205560 ) ) ;
#110792 = FACE_OUTER_BOUND ( 'NONE', #29352, .T. ) ;
#110793 = EDGE_LOOP ( 'NONE', ( #21550, #222784 ) ) ;
#110794 = VECTOR ( 'NONE', #199795, 1000.000000000000000 ) ;
#110795 = ORIENTED_EDGE ( 'NONE', *, *, #54190, .F. ) ;
#110796 = FACE_OUTER_BOUND ( 'NONE', #123622, .T. ) ;
#110798 = ORIENTED_EDGE ( 'NONE', *, *, #2422, .F. ) ;
#110797 = DIRECTION ( 'NONE',  ( 0.000000000000000000, 0.01562500000001058528, 0.9998779222360095753 ) ) ;
#110799 = FACE_OUTER_BOUND ( 'NONE', #194934, .T. ) ;
#110800 = AXIS2_PLACEMENT_3D ( 'NONE', #136381, #727, #80256 ) ;
#110802 = DIRECTION ( 'NONE',  ( 1.000000000000000000, -1.836970198721029934E-16, -1.282749433769087582E-30 ) ) ;
#110801 = CARTESIAN_POINT ( 'NONE',  ( 18.59999999999998366, 14.80545736607782814, -235.9842437978701639 ) ) ;
#110803 = CARTESIAN_POINT ( 'NONE',  ( 21.14999999999999858, 45.02833974712562792, -238.5149546970766892 ) ) ;
#110804 = CARTESIAN_POINT ( 'NONE',  ( -14.56556274378147009, 62.06390979127200325, -218.8186321886648784 ) ) ;
#110805 = EDGE_LOOP ( 'NONE', ( #134847, #62108, #68168, #124317 ) ) ;
#110806 = ORIENTED_EDGE ( 'NONE', *, *, #75951, .F. ) ;
#110807 = CARTESIAN_POINT ( 'NONE',  ( 23.15000000000000213, -4.914013037343258894, -233.1828366659746905 ) ) ;
#110808 = CARTESIAN_POINT ( 'NONE',  ( -20.85000000000000142, 80.78317333349157536, -192.9003134612048882 ) ) ;
#110809 = AXIS2_PLACEMENT_3D ( 'NONE', #139619, #118815, #238747 ) ;
#110810 = ORIENTED_EDGE ( 'NONE', *, *, #180597, .T. ) ;
#110811 = EDGE_CURVE ( 'NONE', #102162, #239427, #27492, .T. ) ;
#110812 = CARTESIAN_POINT ( 'NONE',  ( -20.64999999999999858, 71.65000000001199965, -115.3731074845243256 ) ) ;
#110813 = DIRECTION ( 'NONE',  ( -0.000000000000000000, -0.000000000000000000, -1.000000000000000000 ) ) ;
#110814 = EDGE_LOOP ( 'NONE', ( #73888, #9509, #242748, #40538 ) ) ;
#110815 = VERTEX_POINT ( 'NONE', #204780 ) ;
#110816 = DIRECTION ( 'NONE',  ( 0.000000000000000000, 0.000000000000000000, -1.000000000000000000 ) ) ;
#110817 = CARTESIAN_POINT ( 'NONE',  ( -18.37160782347004329, 64.52438358520969075, -127.2731074845243882 ) ) ;
#110818 = VERTEX_POINT ( 'NONE', #109533 ) ;
#110819 = CARTESIAN_POINT ( 'NONE',  ( 20.94999999999999574, -1.162701749926853712, -41.60000000000000142 ) ) ;
#110820 = VERTEX_POINT ( 'NONE', #48290 ) ;
#110821 = CARTESIAN_POINT ( 'NONE',  ( -21.05000000000000071, 6.540656951712397138, -100.6000000000000369 ) ) ;
#110823 = ADVANCED_FACE ( 'NONE', ( #86098 ), #189091, .T. ) ;
#110822 = DIRECTION ( 'NONE',  ( 0.000000000000000000, 0.4930308989875575865, 0.8700118002898125091 ) ) ;
#110825 = CARTESIAN_POINT ( 'NONE',  ( -21.13422380239141773, -1.381786344668824107, -194.6553994825906102 ) ) ;
#110824 = CARTESIAN_POINT ( 'NONE',  ( -18.40000000000000213, 64.25000000001182343, -82.17310748452439384 ) ) ;
#110826 = CARTESIAN_POINT ( 'NONE',  ( -21.14999999999999858, -11.38316329222462464, -203.4791315943886048 ) ) ;
#110827 = AXIS2_PLACEMENT_3D ( 'NONE', #7440, #242202, #63561 ) ;
#110828 = DIRECTION ( 'NONE',  ( 1.186688945009009831E-16, 1.000000000000000000, 6.982962677686266711E-15 ) ) ;
#110829 = DIRECTION ( 'NONE',  ( 0.000000000000000000, 1.000000000000000000, 2.891205793294679805E-16 ) ) ;
#110830 = VECTOR ( 'NONE', #62529, 1000.000000000000000 ) ;
#110831 = CARTESIAN_POINT ( 'NONE',  ( 20.94999999999999574, 0.6656436123793491033, -212.6810495496487476 ) ) ;
#110832 = EDGE_CURVE ( 'NONE', #176630, #245188, #186530, .T. ) ;
#110834 = EDGE_CURVE ( 'NONE', #79923, #137338, #166461, .T. ) ;
#110833 = CIRCLE ( 'NONE', #56622, 7.899999999999991473 ) ;
#110835 = AXIS2_PLACEMENT_3D ( 'NONE', #151808, #17410, #171392 ) ;
#110837 = ORIENTED_EDGE ( 'NONE', *, *, #96995, .F. ) ;
#110836 = CARTESIAN_POINT ( 'NONE',  ( -18.59999999999999787, 85.50000000001229239, -157.8731074845242972 ) ) ;
#110838 = AXIS2_PLACEMENT_3D ( 'NONE', #141857, #84405, #186129 ) ;
#110840 = ORIENTED_EDGE ( 'NONE', *, *, #71376, .T. ) ;
#110839 = EDGE_LOOP ( 'NONE', ( #207461, #220981, #217576, #92279 ) ) ;
#110841 = ORIENTED_EDGE ( 'NONE', *, *, #195152, .T. ) ;
#110842 = CARTESIAN_POINT ( 'NONE',  ( -20.85000000000000142, 77.26327546522911405, -95.12124281777788326 ) ) ;
#110843 = EDGE_CURVE ( 'NONE', #139949, #99525, #78913, .T. ) ;
#110844 = PLANE ( 'NONE',  #211773 ) ;
#110845 = EDGE_CURVE ( 'NONE', #37720, #109129, #224672, .T. ) ;
#110846 = AXIS2_PLACEMENT_3D ( 'NONE', #82888, #140316, #41267 ) ;
#110848 = LINE ( 'NONE', #187844, #232299 ) ;
#110847 = CARTESIAN_POINT ( 'NONE',  ( 21.05000000000000071, -1.849084418615859926, -112.1560105214471577 ) ) ;
#110849 = CARTESIAN_POINT ( 'NONE',  ( 20.94999999999999929, 6.450000000011156587, -77.01702717044007329 ) ) ;
#110850 = EDGE_LOOP ( 'NONE', ( #131384, #215246, #50222, #7679 ) ) ;
#110851 = EDGE_CURVE ( 'NONE', #2789, #48342, #173432, .T. ) ;
#110852 = CARTESIAN_POINT ( 'NONE',  ( -22.50000000000000000, 11.64987090377453960, -100.4174801091271121 ) ) ;
#110853 = TOROIDAL_SURFACE ( 'NONE', #181775, 0.2000000000000000111, 0.1000000000000000056 ) ;
#110854 = ORIENTED_EDGE ( 'NONE', *, *, #236578, .F. ) ;
#110855 = EDGE_LOOP ( 'NONE', ( #11083, #228880, #14520, #241495 ) ) ;
#110856 = DIRECTION ( 'NONE',  ( 1.000000000000000000, 0.000000000000000000, -0.000000000000000000 ) ) ;
#110857 = AXIS2_PLACEMENT_3D ( 'NONE', #220613, #221861, #241461 ) ;
#110858 = SPHERICAL_SURFACE ( 'NONE', #197491, 0.1000000000000000056 ) ;
#110859 = CARTESIAN_POINT ( 'NONE',  ( 23.24999999999999645, 7.128833340093095217, -233.7327013124392749 ) ) ;
#110860 = ORIENTED_EDGE ( 'NONE', *, *, #225296, .F. ) ;
#110861 = CARTESIAN_POINT ( 'NONE',  ( 23.14999999999999858, -11.74999999998883560, -88.75000000000004263 ) ) ;
#110862 = ADVANCED_FACE ( 'NONE', ( #92540 ), #6768, .T. ) ;
#110863 = CARTESIAN_POINT ( 'NONE',  ( 18.59999999999999076, 4.252251777740764460, -211.8999245327126744 ) ) ;
#110864 = VERTEX_POINT ( 'NONE', #75588 ) ;
#110865 = ORIENTED_EDGE ( 'NONE', *, *, #88815, .F. ) ;
#110866 = DIRECTION ( 'NONE',  ( 1.000000000000000000, 0.000000000000000000, -0.000000000000000000 ) ) ;
#110867 = CARTESIAN_POINT ( 'NONE',  ( 18.49999999999999645, 7.783179459866045313, -245.3643104511423303 ) ) ;
#110868 = ADVANCED_FACE ( 'NONE', ( #15620 ), #212523, .T. ) ;
#110869 = CIRCLE ( 'NONE', #35872, 0.09999999999999939493 ) ;
#110870 = DIRECTION ( 'NONE',  ( -6.938893903907222067E-15, -1.000000000000000000, -6.982962677686266711E-15 ) ) ;
#110871 = EDGE_CURVE ( 'NONE', #243577, #214271, #113391, .T. ) ;
#110872 = DIRECTION ( 'NONE',  ( 1.186688945009010077E-16, -1.000000000000000000, -0.000000000000000000 ) ) ;
#110873 = DIRECTION ( 'NONE',  ( 1.000000000000000000, -0.000000000000000000, -0.000000000000000000 ) ) ;
#110874 = ADVANCED_FACE ( 'NONE', ( #36464 ), #209952, .F. ) ;
#110875 = CARTESIAN_POINT ( 'NONE',  ( -21.05000000000000071, 6.300179817914679070, 0.05148288188165942719 ) ) ;
#110876 = ORIENTED_EDGE ( 'NONE', *, *, #134126, .F. ) ;
#110877 = DIRECTION ( 'NONE',  ( 1.000000000000000000, 0.000000000000000000, 0.000000000000000000 ) ) ;
#110878 = CARTESIAN_POINT ( 'NONE',  ( 20.04142135623730070, 64.25000000001220712, -145.3731074845244393 ) ) ;
#110880 = CYLINDRICAL_SURFACE ( 'NONE', #33162, 0.1000000000000101918 ) ;
#110879 = CARTESIAN_POINT ( 'NONE',  ( 20.85000000000000142, -1.135018845899022466, -175.2169768834323520 ) ) ;
#110881 = CARTESIAN_POINT ( 'NONE',  ( 21.98333005346336577, 1.115600667400684642E-11, -26.12592467094333415 ) ) ;
#110882 = CARTESIAN_POINT ( 'NONE',  ( -17.11825945287481332, 30.25354784785470486, -234.7188954791831748 ) ) ;
#110883 = LINE ( 'NONE', #250392, #3850 ) ;
#110884 = CARTESIAN_POINT ( 'NONE',  ( 20.94999027547553894, 10.29326151435327219, -139.4592822510415147 ) ) ;
#110887 = ORIENTED_EDGE ( 'NONE', *, *, #43593, .F. ) ;
#110886 = CIRCLE ( 'NONE', #131733, 0.09999999999999543976 ) ;
#110885 = LINE ( 'NONE', #176022, #40556 ) ;
#110888 = CIRCLE ( 'NONE', #240066, 0.09999999999999939493 ) ;
#110889 = CIRCLE ( 'NONE', #256374, 0.1999999999999996503 ) ;
#110890 = ADVANCED_FACE ( 'NONE', ( #195535 ), #153868, .F. ) ;
#110891 = EDGE_CURVE ( 'NONE', #54225, #86886, #120110, .T. ) ;
#110892 = CARTESIAN_POINT ( 'NONE',  ( 20.85000000000000142, -1.835859311432481045, -212.5044391687984842 ) ) ;
#110893 = CARTESIAN_POINT ( 'NONE',  ( -22.59999999999999787, 64.25043287652255231, -103.1239658536231047 ) ) ;
#110894 = EDGE_CURVE ( 'NONE', #199629, #184760, #73032, .T. ) ;
#110895 = CARTESIAN_POINT ( 'NONE',  ( -20.05000000000000426, 63.83985267992358104, -213.0213082169670145 ) ) ;
#110896 = VECTOR ( 'NONE', #7947, 1000.000000000000000 ) ;
#110897 = CARTESIAN_POINT ( 'NONE',  ( -23.25000000000000000, 6.982009704867601307, -204.6961521182562649 ) ) ;
#110898 = VECTOR ( 'NONE', #86138, 1000.000000000000000 ) ;
#110899 = ORIENTED_EDGE ( 'NONE', *, *, #138318, .T. ) ;
#110900 = DIRECTION ( 'NONE',  ( 1.000000000000000000, 1.541880601228652843E-16, 2.878400969107353907E-16 ) ) ;
#110901 = DIRECTION ( 'NONE',  ( 0.000000000000000000, 1.000000000000000000, -1.224646799147353207E-16 ) ) ;
#110902 = CARTESIAN_POINT ( 'NONE',  ( -20.94999999999999929, 55.11435547888748232, -226.8560373590520101 ) ) ;
#110903 = AXIS2_PLACEMENT_3D ( 'NONE', #215817, #179312, #257473 ) ;
#110904 = ORIENTED_EDGE ( 'NONE', *, *, #222967, .T. ) ;
#110905 = CARTESIAN_POINT ( 'NONE',  ( -23.15000000000000213, 87.39257802171813694, -173.0970570643562212 ) ) ;
#110907 = ORIENTED_EDGE ( 'NONE', *, *, #250772, .T. ) ;
#110906 = CARTESIAN_POINT ( 'NONE',  ( 22.39999999999999503, 68.20922040163900135, -170.0231074845243882 ) ) ;
#110908 = CARTESIAN_POINT ( 'NONE',  ( 22.88900146558018989, 8.703904791123973084, -176.7499999999999716 ) ) ;
#110909 = DIRECTION ( 'NONE',  ( 1.000000000000000000, 0.000000000000000000, 0.000000000000000000 ) ) ;
#110910 = VERTEX_POINT ( 'NONE', #149987 ) ;
#110911 = DIRECTION ( 'NONE',  ( -1.000000000000000000, -1.652117596168391700E-15, -1.153667551319263085E-29 ) ) ;
#110912 = EDGE_CURVE ( 'NONE', #39343, #192913, #103476, .T. ) ;
#110913 = APPLICATION_PROTOCOL_DEFINITION ( 'draft international standard', 'automotive_design', 1998, #55765 ) ;
#110914 = CARTESIAN_POINT ( 'NONE',  ( -21.05000000000000426, 69.52295361822230291, -136.4231074845243938 ) ) ;
#110915 = DIRECTION ( 'NONE',  ( 1.000000000000000000, -0.000000000000000000, 0.000000000000000000 ) ) ;
#110916 = CARTESIAN_POINT ( 'NONE',  ( -18.43473496883406426, 85.49495241101126908, -95.97723591229602391 ) ) ;
#110917 = ORIENTED_EDGE ( 'NONE', *, *, #169747, .F. ) ;
#110919 = EDGE_CURVE ( 'NONE', #141245, #45367, #128447, .T. ) ;
#110918 = CARTESIAN_POINT ( 'NONE',  ( -21.05000000000000071, -10.38870553492056104, -206.3818953267866902 ) ) ;
#110920 = CARTESIAN_POINT ( 'NONE',  ( -20.05000000000000426, 9.250000000011157297, -88.25000000000005684 ) ) ;
#110921 = CIRCLE ( 'NONE', #65125, 11.64999999999999325 ) ;
#110922 = EDGE_CURVE ( 'NONE', #231520, #82701, #228424, .T. ) ;
#110923 = EDGE_CURVE ( 'NONE', #231063, #222258, #49337, .T. ) ;
#110924 = CARTESIAN_POINT ( 'NONE',  ( -22.50000000000000000, 0.1000000000111554016, -88.85042919245522341 ) ) ;
#110925 = VERTEX_POINT ( 'NONE', #236219 ) ;
#110926 = VERTEX_POINT ( 'NONE', #191989 ) ;
#110927 = EDGE_CURVE ( 'NONE', #149634, #144636, #257372, .T. ) ;
#110928 = DIRECTION ( 'NONE',  ( 0.000000000000000000, -1.000000000000000000, -1.734723475976807292E-15 ) ) ;
#110929 = CARTESIAN_POINT ( 'NONE',  ( -23.15000000000000213, 1.115626384983466744E-11, -131.9000000000000341 ) ) ;
#110930 = CARTESIAN_POINT ( 'NONE',  ( 18.59999999999999432, 74.83729825007360148, -61.42310748452432989 ) ) ;
#110931 = DIRECTION ( 'NONE',  ( -0.000000000000000000, 0.000000000000000000, 1.000000000000000000 ) ) ;
#110934 = CARTESIAN_POINT ( 'NONE',  ( 22.45301702632625762, -2.464224896439110690, -189.6138028341777897 ) ) ;
#110933 = CIRCLE ( 'NONE', #219261, 11.80000000000000426 ) ;
#110932 = CARTESIAN_POINT ( 'NONE',  ( 22.59999999999999787, 64.35042919246788529, -203.6231074845244393 ) ) ;
#110935 = CARTESIAN_POINT ( 'NONE',  ( -18.59999999999999787, 72.08710075277812734, -58.04128451151338197 ) ) ;
#110936 = CARTESIAN_POINT ( 'NONE',  ( -16.87036670365548474, 66.01058118071034642, -115.5435473672223168 ) ) ;
#110937 = CARTESIAN_POINT ( 'NONE',  ( -18.34374000495060386, 13.17878477875124688, -207.5966336730521391 ) ) ;
#110938 = AXIS2_PLACEMENT_3D ( 'NONE', #42303, #120576, #81386 ) ;
#110939 = VERTEX_POINT ( 'NONE', #34206 ) ;
#110940 = VECTOR ( 'NONE', #238095, 1000.000000000000000 ) ;
#110941 = EDGE_CURVE ( 'NONE', #170896, #105294, #149969, .T. ) ;
#110943 = VERTEX_POINT ( 'NONE', #197084 ) ;
#110942 = CARTESIAN_POINT ( 'NONE',  ( 21.05000000000000071, 8.001317420522640944, -237.7387931148579980 ) ) ;
#110944 = CARTESIAN_POINT ( 'NONE',  ( -18.59999999999999787, 1.162701749949165642, -142.1000000000000227 ) ) ;
#110945 = EDGE_CURVE ( 'NONE', #71883, #64464, #53443, .T. ) ;
#110946 = DIRECTION ( 'NONE',  ( -0.000000000000000000, 1.000000000000000000, 7.525063763929033127E-15 ) ) ;
#110948 = FACE_OUTER_BOUND ( 'NONE', #187127, .T. ) ;
#110947 = DIRECTION ( 'NONE',  ( 0.000000000000000000, -0.8700118002898354908, 0.4930308989875170078 ) ) ;
#110949 =( GEOMETRIC_REPRESENTATION_CONTEXT ( 3 ) GLOBAL_UNCERTAINTY_ASSIGNED_CONTEXT ( ( #233204 ) ) GLOBAL_UNIT_ASSIGNED_CONTEXT ( ( #178182, #191020, #59146 ) ) REPRESENTATION_CONTEXT ( 'NONE', 'WORKASPACE' ) );
#110950 = ORIENTED_EDGE ( 'NONE', *, *, #73468, .F. ) ;
#110951 = CARTESIAN_POINT ( 'NONE',  ( -18.50000000000000000, 64.02438395623025258, -266.2629958759080182 ) ) ;
#110953 = EDGE_CURVE ( 'NONE', #241599, #237434, #25246, .T. ) ;
#110952 = DIRECTION ( 'NONE',  ( 0.000000000000000000, 0.000000000000000000, -1.000000000000000000 ) ) ;
#110954 = CARTESIAN_POINT ( 'NONE',  ( 22.48660254037844197, 11.65000000001116298, -133.9500000000000171 ) ) ;
#110955 = LINE ( 'NONE', #190518, #64819 ) ;
#110956 = ORIENTED_EDGE ( 'NONE', *, *, #91834, .F. ) ;
#110957 = VERTEX_POINT ( 'NONE', #95431 ) ;
#110958 = DIRECTION ( 'NONE',  ( 0.000000000000000000, 0.8660254037844309360, -0.5000000000000134337 ) ) ;
#110959 = ORIENTED_EDGE ( 'NONE', *, *, #134930, .T. ) ;
#110960 = CARTESIAN_POINT ( 'NONE',  ( -18.59999999999999787, 85.50000000001185185, -90.87310748452424036 ) ) ;
#110961 = EDGE_CURVE ( 'NONE', #87552, #67930, #65873, .T. ) ;
#110962 = AXIS2_PLACEMENT_3D ( 'NONE', #51231, #33034, #27884 ) ;
#110963 = CARTESIAN_POINT ( 'NONE',  ( -20.85000000000000142, 64.35000000001176090, -76.30697314750248950 ) ) ;
#110964 = VECTOR ( 'NONE', #115217, 1000.000000000000000 ) ;
#110965 = CARTESIAN_POINT ( 'NONE',  ( 21.05000000000000071, 8.776282895303630482, -142.5586289951409640 ) ) ;
#110966 = EDGE_CURVE ( 'NONE', #214701, #208046, #249265, .T. ) ;
#110967 = CARTESIAN_POINT ( 'NONE',  ( 20.99105743725315776, 6.322468215188231433, 12.11686199560448252 ) ) ;
#110969 = ORIENTED_EDGE ( 'NONE', *, *, #240057, .T. ) ;
#110968 = AXIS2_PLACEMENT_3D ( 'NONE', #48778, #167476, #207890 ) ;
#110970 = CYLINDRICAL_SURFACE ( 'NONE', #238931, 0.1000000000000048767 ) ;
#110971 = ADVANCED_FACE ( 'NONE', ( #94137 ), #173737, .T. ) ;
#110972 = TOROIDAL_SURFACE ( 'NONE', #106864, 11.65000000000000036, 0.1000000000000000056 ) ;
#110973 = DIRECTION ( 'NONE',  ( 1.000000000000000000, 0.000000000000000000, 0.000000000000000000 ) ) ;
#110974 = AXIS2_PLACEMENT_3D ( 'NONE', #223679, #26812, #106290 ) ;
#110975 = EDGE_CURVE ( 'NONE', #127685, #65499, #186731, .T. ) ;
#110976 = CARTESIAN_POINT ( 'NONE',  ( -18.56579813702275672, 68.10670728244119232, -224.1434476749765565 ) ) ;
#110977 = FACE_OUTER_BOUND ( 'NONE', #55221, .T. ) ;
#110978 = DIRECTION ( 'NONE',  ( 2.952720810173289112E-16, 1.000000000000000000, 6.530723674265620862E-15 ) ) ;
#110979 = DIRECTION ( 'NONE',  ( 0.000000000000000000, 0.000000000000000000, -1.000000000000000000 ) ) ;
#110980 = CARTESIAN_POINT ( 'NONE',  ( -16.79270642812263858, 66.05375578307364037, -149.1841742059602041 ) ) ;
#110981 = ORIENTED_EDGE ( 'NONE', *, *, #148049, .T. ) ;
#110983 = DIRECTION ( 'NONE',  ( 1.000000000000000000, 0.000000000000000000, 0.000000000000000000 ) ) ;
#110982 = DIRECTION ( 'NONE',  ( 1.000000000000000000, 0.000000000000000000, 0.000000000000000000 ) ) ;
#110984 = ORIENTED_EDGE ( 'NONE', *, *, #120153, .F. ) ;
#110986 = ORIENTED_EDGE ( 'NONE', *, *, #175310, .T. ) ;
#110985 = CARTESIAN_POINT ( 'NONE',  ( 18.59999999999999076, 6.450000000011156587, -188.7499999999999716 ) ) ;
#110987 = CIRCLE ( 'NONE', #173583, 0.5000000000000013323 ) ;
#110988 = ORIENTED_EDGE ( 'NONE', *, *, #173026, .F. ) ;
#110989 = DIRECTION ( 'NONE',  ( 0.000000000000000000, -6.938893903907222067E-15, 1.000000000000000000 ) ) ;
#110990 = AXIS2_PLACEMENT_3D ( 'NONE', #189750, #69826, #34549 ) ;
#110991 = CARTESIAN_POINT ( 'NONE',  ( -23.15000000000000213, 1.148907358139439339E-11, -201.0000000000015064 ) ) ;
#110992 = AXIS2_PLACEMENT_3D ( 'NONE', #144267, #244667, #100001 ) ;
#110993 = CARTESIAN_POINT ( 'NONE',  ( 18.52928932304161691, 65.72071067697012836, -78.34685405172071171 ) ) ;
#110994 = CARTESIAN_POINT ( 'NONE',  ( -22.47071067811865319, 59.75442326890419764, -233.9300113800878762 ) ) ;
#110995 = ORIENTED_EDGE ( 'NONE', *, *, #187693, .T. ) ;
#110996 = EDGE_CURVE ( 'NONE', #109463, #56926, #233669, .T. ) ;
#110997 = CARTESIAN_POINT ( 'NONE',  ( 21.05000000000000426, 69.58617371119972006, -203.4373665474910240 ) ) ;
#110998 = DIRECTION ( 'NONE',  ( -0.000000000000000000, 0.000000000000000000, -1.000000000000000000 ) ) ;
#110999 = AXIS2_PLACEMENT_3D ( 'NONE', #72310, #193537, #211816 ) ;
#111000 = ORIENTED_EDGE ( 'NONE', *, *, #245112, .T. ) ;
#111001 = CARTESIAN_POINT ( 'NONE',  ( -16.89268316805465986, 9.951721813253337601, -154.8557524785455541 ) ) ;
#111002 = CIRCLE ( 'NONE', #169310, 0.1000000000000098310 ) ;
#111003 = DIRECTION ( 'NONE',  ( 1.000000000000000000, 0.000000000000000000, 0.000000000000000000 ) ) ;
#111004 = VERTEX_POINT ( 'NONE', #155447 ) ;
#111005 = CYLINDRICAL_SURFACE ( 'NONE', #31141, 0.09999999999998898659 ) ;
#111006 = VERTEX_POINT ( 'NONE', #135823 ) ;
#111007 = CARTESIAN_POINT ( 'NONE',  ( -23.25000000000000355, 70.35000000001230092, -157.3731074845244109 ) ) ;
#111008 = ORIENTED_EDGE ( 'NONE', *, *, #142467, .T. ) ;
#111009 = CARTESIAN_POINT ( 'NONE',  ( 15.74999999999999645, 66.65000000001228386, -153.2731074845244166 ) ) ;
#111010 = EDGE_CURVE ( 'NONE', #207631, #63258, #137450, .T. ) ;
#111011 = CARTESIAN_POINT ( 'NONE',  ( -17.78043020864320667, 41.65515396761067279, -235.4199665519760458 ) ) ;
#111012 = CARTESIAN_POINT ( 'NONE',  ( 21.04999999999999716, 75.93429838968962997, -75.78142354185638396 ) ) ;
#111013 = TOROIDAL_SURFACE ( 'NONE', #115119, 1.900000000000002576, 0.1000000000000000056 ) ;
#111014 = AXIS2_PLACEMENT_3D ( 'NONE', #138927, #114270, #253762 ) ;
#111015 = CIRCLE ( 'NONE', #44392, 14.30833333333333890 ) ;
#111016 = CIRCLE ( 'NONE', #131861, 0.1000000000000028644 ) ;
#111017 = DIRECTION ( 'NONE',  ( 0.000000000000000000, 1.000000000000000000, 0.000000000000000000 ) ) ;
#111018 = CARTESIAN_POINT ( 'NONE',  ( 21.14999999999999858, 76.00000000001200817, -109.5637644362255685 ) ) ;
#111020 = EDGE_CURVE ( 'NONE', #40483, #232204, #165887, .T. ) ;
#111019 = CARTESIAN_POINT ( 'NONE',  ( 21.14999999999999503, -0.09999999998884338825, -55.35042919245524473 ) ) ;
#111021 = ORIENTED_EDGE ( 'NONE', *, *, #2894, .F. ) ;
#111022 = DIRECTION ( 'NONE',  ( 0.000000000000000000, 0.8814952561688437216, -0.4721928772777334582 ) ) ;
#111023 = ORIENTED_EDGE ( 'NONE', *, *, #87007, .F. ) ;
#111025 = LINE ( 'NONE', #88869, #17141 ) ;
#111024 = DIRECTION ( 'NONE',  ( -1.000000000000000000, 0.000000000000000000, 0.000000000000000000 ) ) ;
#111026 = AXIS2_PLACEMENT_3D ( 'NONE', #147666, #128103, #108535 ) ;
#111027 = ORIENTED_EDGE ( 'NONE', *, *, #134984, .T. ) ;
#111028 = DIRECTION ( 'NONE',  ( 1.000000000000000000, 0.000000000000000000, -0.000000000000000000 ) ) ;
#111029 = CARTESIAN_POINT ( 'NONE',  ( -21.13614978966382196, 6.499104701833789299, 1.201516235680224439E-15 ) ) ;
#111030 = CARTESIAN_POINT ( 'NONE',  ( 23.24999999999999289, 11.65000000000000746, -12.15000000000000036 ) ) ;
#111032 = ORIENTED_EDGE ( 'NONE', *, *, #115469, .F. ) ;
#111031 =( BOUNDED_SURFACE ( )  B_SPLINE_SURFACE ( 3, 2, ( 
 ( #159613, #116625, #141326 ),
 ( #196160, #81315, #177901 ),
 ( #158361, #78762, #59175 ),
 ( #17512, #97018, #138713 ),
 ( #218270, #99598, #39689 ),
 ( #20106, #239145, #140016 ) ),
 .UNSPECIFIED., .F., .F., .F. ) 
 B_SPLINE_SURFACE_WITH_KNOTS ( ( 4, 2, 4 ),
 ( 3, 3 ),
 ( 0.0001300404313046571046, 0.0003183318589266614972, 0.0005066232865486658627 ),
 ( 0.000000000000000000, 1.000000000000000000 ),
 .UNSPECIFIED. ) 
 GEOMETRIC_REPRESENTATION_ITEM ( )  RATIONAL_B_SPLINE_SURFACE ( (
 ( 1.000000000000000000, 0.7071067811865475727, 1.000000000000000000),
 ( 1.000000000000000000, 0.7625113560542592372, 1.000000000000000000),
 ( 1.000000000000000000, 0.8126073484685066850, 1.000000000000000000),
 ( 1.000000000000000000, 0.8923049332735827344, 1.000000000000000000),
 ( 1.000000000000000000, 0.9231914937766932949, 1.000000000000000000),
 ( 1.000000000000000000, 0.9238795325112901802, 1.000000000000000000) ) ) 
 REPRESENTATION_ITEM ( '' )  SURFACE ( )  );
#111034 = ORIENTED_EDGE ( 'NONE', *, *, #153315, .T. ) ;
#111033 = DIRECTION ( 'NONE',  ( 1.000000000000000000, 0.000000000000000000, 0.000000000000000000 ) ) ;
#111035 = AXIS2_PLACEMENT_3D ( 'NONE', #239131, #117887, #98291 ) ;
#111037 = DIRECTION ( 'NONE',  ( -1.000000000000000000, 0.000000000000000000, 0.000000000000000000 ) ) ;
#111036 = LINE ( 'NONE', #90167, #1249 ) ;
#111038 = CIRCLE ( 'NONE', #194455, 0.09999999999999481526 ) ;
#111040 = ORIENTED_EDGE ( 'NONE', *, *, #166310, .T. ) ;
#111039 = CARTESIAN_POINT ( 'NONE',  ( -21.05000000000000071, 5.204170427930421283E-15, -2.899999999999982592 ) ) ;
#111041 = AXIS2_PLACEMENT_3D ( 'NONE', #44243, #162921, #45516 ) ;
#111042 = ORIENTED_EDGE ( 'NONE', *, *, #136565, .T. ) ;
#111043 = LINE ( 'NONE', #228443, #35280 ) ;
#111044 = DIRECTION ( 'NONE',  ( 1.000000000000000000, 0.000000000000000000, -0.000000000000000000 ) ) ;
#111045 = ORIENTED_EDGE ( 'NONE', *, *, #185462, .F. ) ;
#111046 = CARTESIAN_POINT ( 'NONE',  ( -22.39999999999999858, 12.54173083476182526, -223.4160622903444846 ) ) ;
#111047 = ORIENTED_EDGE ( 'NONE', *, *, #186666, .F. ) ;
#111048 = AXIS2_PLACEMENT_3D ( 'NONE', #240672, #122014, #140266 ) ;
#111049 = CARTESIAN_POINT ( 'NONE',  ( -18.46907102845854354, -9.473727364752953406, -107.1760347387365897 ) ) ;
#111050 = CARTESIAN_POINT ( 'NONE',  ( 20.04142135623731136, 34.40595771266846725, -235.0146864773515176 ) ) ;
#111051 = ORIENTED_EDGE ( 'NONE', *, *, #57280, .T. ) ;
#111052 = LINE ( 'NONE', #233583, #237368 ) ;
#111053 = EDGE_CURVE ( 'NONE', #132890, #169820, #101816, .T. ) ;
#111054 = EDGE_LOOP ( 'NONE', ( #86410, #31566, #141797, #184359 ) ) ;
#111055 = VECTOR ( 'NONE', #230873, 1000.000000000000000 ) ;
#111056 = AXIS2_PLACEMENT_3D ( 'NONE', #179504, #809, #80346 ) ;
#111057 = CARTESIAN_POINT ( 'NONE',  ( 21.15000000000005542, 78.47315729244128590, -52.27034697567518862 ) ) ;
#111058 = VECTOR ( 'NONE', #215855, 1000.000000000000227 ) ;
#111059 = AXIS2_PLACEMENT_3D ( 'NONE', #97344, #116949, #236889 ) ;
#111060 = EDGE_LOOP ( 'NONE', ( #124797, #169226, #118188, #198739 ) ) ;
#111061 = VERTEX_POINT ( 'NONE', #44460 ) ;
#111062 = CARTESIAN_POINT ( 'NONE',  ( 20.41140022480129446, 18.75715215813852765, -228.1517052862273829 ) ) ;
#111063 = VERTEX_POINT ( 'NONE', #1453 ) ;
#111064 = EDGE_CURVE ( 'NONE', #147103, #205939, #65289, .T. ) ;
#111065 = LINE ( 'NONE', #92775, #113051 ) ;
#111066 = ORIENTED_EDGE ( 'NONE', *, *, #138832, .F. ) ;
#111068 = ORIENTED_EDGE ( 'NONE', *, *, #100621, .F. ) ;
#111067 = DIRECTION ( 'NONE',  ( 0.000000000000000000, -1.000000000000000000, -6.982962677686266711E-15 ) ) ;
#111069 = EDGE_CURVE ( 'NONE', #227928, #107106, #220021, .T. ) ;
#111070 = ORIENTED_EDGE ( 'NONE', *, *, #138586, .F. ) ;
#111071 = CARTESIAN_POINT ( 'NONE',  ( 23.24999999999999289, 55.98745301258800566, -232.8057040749261262 ) ) ;
#111072 = ORIENTED_EDGE ( 'NONE', *, *, #1185, .F. ) ;
#111075 = ORIENTED_EDGE ( 'NONE', *, *, #181322, .F. ) ;
#111074 = ORIENTED_EDGE ( 'NONE', *, *, #198958, .F. ) ;
#111073 = SPHERICAL_SURFACE ( 'NONE', #110249, 0.1000000000000000056 ) ;
#111076 = AXIS2_PLACEMENT_3D ( 'NONE', #25587, #206783, #47688 ) ;
#111077 = CARTESIAN_POINT ( 'NONE',  ( 21.14999999999999858, 11.65000000001115943, -167.5999999999999659 ) ) ;
#111078 = AXIS2_PLACEMENT_3D ( 'NONE', #225356, #46724, #227945 ) ;
#111079 = AXIS2_PLACEMENT_3D ( 'NONE', #103003, #26067, #44345 ) ;
#111081 = EDGE_CURVE ( 'NONE', #126038, #6193, #24415, .T. ) ;
#111080 = VERTEX_POINT ( 'NONE', #139667 ) ;
#111082 = EDGE_CURVE ( 'NONE', #58852, #136758, #211680, .T. ) ;
#111083 = LINE ( 'NONE', #249328, #196675 ) ;
#111084 = VERTEX_POINT ( 'NONE', #83536 ) ;
#111085 = DIRECTION ( 'NONE',  ( 0.000000000000000000, -6.454785026890406770E-15, 1.000000000000000000 ) ) ;
#111087 = ORIENTED_EDGE ( 'NONE', *, *, #25337, .T. ) ;
#111086 = DIRECTION ( 'NONE',  ( 1.000000000000000000, 0.000000000000000000, 0.000000000000000000 ) ) ;
#111088 = CARTESIAN_POINT ( 'NONE',  ( 23.24999999999999645, 52.07980129617636322, -232.9753775883424964 ) ) ;
#111089 = ORIENTED_EDGE ( 'NONE', *, *, #246995, .T. ) ;
#111090 = EDGE_CURVE ( 'NONE', #72671, #101771, #115996, .T. ) ;
#111092 = CARTESIAN_POINT ( 'NONE',  ( 21.05000000000000071, 65.37049252075090067, -95.39512808452764148 ) ) ;
#111091 =( BOUNDED_CURVE ( )  B_SPLINE_CURVE ( 3, ( #12399, #52768, #89327, #68506 ),
 .UNSPECIFIED., .F., .F. ) 
 B_SPLINE_CURVE_WITH_KNOTS ( ( 4, 4 ),
 ( 0.5235987755983128045, 1.570796326794896558 ),
 .UNSPECIFIED. ) 
 CURVE ( )  GEOMETRIC_REPRESENTATION_ITEM ( )  RATIONAL_B_SPLINE_CURVE ( ( 1.000000000000000000, 0.9106836025229614329, 0.9106836025229614329, 1.000000000000000000 ) ) 
 REPRESENTATION_ITEM ( '' )  );
#111093 = DIRECTION ( 'NONE',  ( 0.000000000000000000, 0.000000000000000000, -1.000000000000000000 ) ) ;
#111094 = EDGE_LOOP ( 'NONE', ( #81131, #216073, #77449, #163594 ) ) ;
#111095 = CARTESIAN_POINT ( 'NONE',  ( 18.46858270002953262, 85.47420267472219280, -62.42108554982039692 ) ) ;
#111096 = CARTESIAN_POINT ( 'NONE',  ( 18.52643265882457868, 18.39335631088233569, -236.9600537807593241 ) ) ;
#111097 = ADVANCED_FACE ( 'NONE', ( #123995 ), #243918, .T. ) ;
#111098 = ORIENTED_EDGE ( 'NONE', *, *, #253371, .F. ) ;
#111100 = ORIENTED_EDGE ( 'NONE', *, *, #202167, .T. ) ;
#111099 = CARTESIAN_POINT ( 'NONE',  ( -21.14999999999994174, 76.00000000001119815, -40.07310748452479032 ) ) ;
#111101 = FACE_OUTER_BOUND ( 'NONE', #54697, .T. ) ;
#111102 = VECTOR ( 'NONE', #121109, 1000.000000000000000 ) ;
#111104 = ORIENTED_EDGE ( 'NONE', *, *, #18207, .F. ) ;
#111103 = ORIENTED_EDGE ( 'NONE', *, *, #234676, .T. ) ;
#111105 = ORIENTED_EDGE ( 'NONE', *, *, #6773, .F. ) ;
#111106 = LINE ( 'NONE', #169846, #103293 ) ;
#111107 = VERTEX_POINT ( 'NONE', #240085 ) ;
#111108 = ORIENTED_EDGE ( 'NONE', *, *, #224821, .T. ) ;
#111109 = FACE_OUTER_BOUND ( 'NONE', #119514, .T. ) ;
#111110 = ORIENTED_EDGE ( 'NONE', *, *, #143253, .F. ) ;
#111111 = FACE_OUTER_BOUND ( 'NONE', #88219, .T. ) ;
#111112 = CIRCLE ( 'NONE', #177773, 0.2000000000000057288 ) ;
#111113 = DIRECTION ( 'NONE',  ( 0.000000000000000000, 0.000000000000000000, -1.000000000000000000 ) ) ;
#111114 = EDGE_CURVE ( 'NONE', #159251, #12445, #140928, .T. ) ;
#111115 = VERTEX_POINT ( 'NONE', #79697 ) ;
#111116 = ORIENTED_EDGE ( 'NONE', *, *, #240079, .T. ) ;
#111117 = VECTOR ( 'NONE', #23424, 1000.000000000000000 ) ;
#111118 = DIRECTION ( 'NONE',  ( 0.000000000000000000, -0.9910465087640866200, -0.1335171055202867274 ) ) ;
#111119 = ORIENTED_EDGE ( 'NONE', *, *, #72087, .T. ) ;
#111120 = TOROIDAL_SURFACE ( 'NONE', #136030, 11.90000000000000213, 0.1000000000000000056 ) ;
#111121 = AXIS2_PLACEMENT_3D ( 'NONE', #63010, #4313, #222058 ) ;
#111122 =( BOUNDED_SURFACE ( )  B_SPLINE_SURFACE ( 3, 2, ( 
 ( #145151, #224693, #46062 ),
 ( #205121, #185578, #6938 ),
 ( #10802, #210296, #129466 ),
 ( #128181, #29126, #90317 ),
 ( #72071, #68207, #31678 ),
 ( #109883, #208996, #147747 ),
 ( #169921, #30379, #48628 ),
 ( #189445, #249420, #168644 ),
 ( #9504, #248118, #89039 ),
 ( #49918, #151625, #211575 ) ),
 .UNSPECIFIED., .F., .F., .F. ) 
 B_SPLINE_SURFACE_WITH_KNOTS ( ( 4, 2, 2, 2, 4 ),
 ( 3, 3 ),
 ( 0.002161241639767248670, 0.002579950749615824400, 0.002789305304540112482, 0.002893982582002256523, 0.002998659859464400564 ),
 ( 0.000000000000000000, 1.000000000000000000 ),
 .UNSPECIFIED. ) 
 GEOMETRIC_REPRESENTATION_ITEM ( )  RATIONAL_B_SPLINE_SURFACE ( (
 ( 1.000000000000000000, 0.7071067811865536790, 1.000000000000000000),
 ( 1.000000000000000000, 0.7632447400664059689, 1.000000000000000000),
 ( 1.000000000000000000, 0.8158073005110477727, 1.000000000000000000),
 ( 1.000000000000000000, 0.8906973462395736396, 1.000000000000000000),
 ( 1.000000000000000000, 0.9149408947800440339, 1.000000000000000000),
 ( 1.000000000000000000, 0.9493368785275709820, 1.000000000000000000),
 ( 1.000000000000000000, 0.9605194247156193521, 1.000000000000000000),
 ( 1.000000000000000000, 0.9803630264781763026, 1.000000000000000000),
 ( 1.000000000000000000, 0.9900844824270708111, 1.000000000000000000),
 ( 1.000000000000000000, 0.9894588281429294030, 1.000000000000000000) ) ) 
 REPRESENTATION_ITEM ( '' )  SURFACE ( )  );
#111123 = AXIS2_PLACEMENT_3D ( 'NONE', #141061, #77216, #56360 ) ;
#111124 = EDGE_CURVE ( 'NONE', #51212, #176240, #86699, .T. ) ;
#111125 = LINE ( 'NONE', #173720, #150873 ) ;
#111126 = ORIENTED_EDGE ( 'NONE', *, *, #11424, .T. ) ;
#111127 = DIRECTION ( 'NONE',  ( -7.304098846218134667E-16, 0.9651348961777158619, -0.2617529984165031243 ) ) ;
#111128 = CIRCLE ( 'NONE', #40440, 0.09999999999998898659 ) ;
#111130 = EDGE_LOOP ( 'NONE', ( #93096, #105578, #14719, #146230 ) ) ;
#111129 = CARTESIAN_POINT ( 'NONE',  ( -21.70464131381649509, 68.90464198104452009, -170.0231074845243882 ) ) ;
#111131 = CARTESIAN_POINT ( 'NONE',  ( 23.14999999999999503, 6.650000000011155876, -88.25000000000005684 ) ) ;
#111132 = DIRECTION ( 'NONE',  ( -1.000000000000000000, 0.000000000000000000, -0.000000000000000000 ) ) ;
#111133 = CARTESIAN_POINT ( 'NONE',  ( 20.95496329884391784, 65.43256679391905095, -128.9487975522395402 ) ) ;
#111134 = FACE_OUTER_BOUND ( 'NONE', #114218, .T. ) ;
#111135 = CARTESIAN_POINT ( 'NONE',  ( -21.09610168723073542, 6.378955715235934854, -133.9664104931085546 ) ) ;
#111136 = CARTESIAN_POINT ( 'NONE',  ( 19.88284271247461987, 11.69142135624847256, -58.25000000000000000 ) ) ;
#111137 = CARTESIAN_POINT ( 'NONE',  ( -18.59999999999999787, 74.83729825007462466, -195.4231074845243654 ) ) ;
#111138 = CARTESIAN_POINT ( 'NONE',  ( -21.05000000000000071, -12.41227409413852811, -131.1000000000000227 ) ) ;
#111139 = CARTESIAN_POINT ( 'NONE',  ( 18.31325810956315792, 38.21040716756283473, -261.2006724472523160 ) ) ;
#111140 = CARTESIAN_POINT ( 'NONE',  ( -21.59142135623730852, 52.75120266497943078, -233.7402936251220638 ) ) ;
#111141 = EDGE_CURVE ( 'NONE', #32289, #188196, #174286, .T. ) ;
#111142 = AXIS2_PLACEMENT_3D ( 'NONE', #82343, #64104, #199784 ) ;
#111143 = ORIENTED_EDGE ( 'NONE', *, *, #169202, .F. ) ;
#111144 = EDGE_CURVE ( 'NONE', #231702, #70035, #65902, .T. ) ;
#111145 = AXIS2_PLACEMENT_3D ( 'NONE', #86987, #186119, #7476 ) ;
#111147 = ORIENTED_EDGE ( 'NONE', *, *, #243850, .T. ) ;
#111146 = CIRCLE ( 'NONE', #98625, 0.1999999999999996503 ) ;
#111148 = ORIENTED_EDGE ( 'NONE', *, *, #243834, .F. ) ;
#111149 = TOROIDAL_SURFACE ( 'NONE', #211114, 12.97499999999999609, 0.1000000000000000056 ) ;
#111150 = ORIENTED_EDGE ( 'NONE', *, *, #40837, .F. ) ;
#111151 = CARTESIAN_POINT ( 'NONE',  ( -18.37013991200266005, 64.50025238379991777, -93.81613049504150581 ) ) ;
#111152 = ADVANCED_FACE ( 'NONE', ( #4030 ), #161792, .T. ) ;
#111153 = CARTESIAN_POINT ( 'NONE',  ( -23.25000000000000355, 11.75000000001113953, -76.25000000000004263 ) ) ;
#111154 = TOROIDAL_SURFACE ( 'NONE', #69662, 11.65000000000000036, 0.1000000000000000056 ) ;
#111155 = CIRCLE ( 'NONE', #161242, 0.1000000000000000472 ) ;
#111157 = CARTESIAN_POINT ( 'NONE',  ( -18.50000000000000000, 74.13328508995498112, -158.2704322382423641 ) ) ;
#111156 = DIRECTION ( 'NONE',  ( -0.5735764363510466035, -0.8191520442889914655, 0.000000000000000000 ) ) ;
#111158 = ORIENTED_EDGE ( 'NONE', *, *, #12227, .F. ) ;
#111159 = EDGE_LOOP ( 'NONE', ( #217109, #243522, #205193, #23690 ) ) ;
#111160 = EDGE_CURVE ( 'NONE', #243832, #172933, #244968, .T. ) ;
#111161 = EDGE_CURVE ( 'NONE', #183191, #36016, #140994, .T. ) ;
#111162 = CARTESIAN_POINT ( 'NONE',  ( 21.14999999999999858, -2.479040261793999722, -189.6172560698084624 ) ) ;
#111163 = CARTESIAN_POINT ( 'NONE',  ( 18.54148534481893407, 10.32532329027886675, -173.0699343018359855 ) ) ;
#111164 = CARTESIAN_POINT ( 'NONE',  ( -20.54999999999999716, 0.000000000000000000, -33.50000000000000000 ) ) ;
#111165 = ORIENTED_EDGE ( 'NONE', *, *, #204096, .T. ) ;
#111166 = VERTEX_POINT ( 'NONE', #220527 ) ;
#111167 = CIRCLE ( 'NONE', #27995, 0.09999999999999942268 ) ;
#111168 = DIRECTION ( 'NONE',  ( 0.000000000000000000, -1.000000000000000000, 0.000000000000000000 ) ) ;
#111169 = AXIS2_PLACEMENT_3D ( 'NONE', #130753, #169934, #9514 ) ;
#111170 = CARTESIAN_POINT ( 'NONE',  ( 23.14999999999998437, 76.00000000001162448, -65.47310748452431994 ) ) ;
#111171 = LINE ( 'NONE', #250662, #43101 ) ;
#111172 = CIRCLE ( 'NONE', #214634, 0.2000000000000057288 ) ;
#111173 = ADVANCED_FACE ( 'NONE', ( #181412 ), #247779, .F. ) ;
#111174 = CARTESIAN_POINT ( 'NONE',  ( 23.14999999999999858, 5.000000000011153745, -88.59473398108696074 ) ) ;
#111176 = EDGE_LOOP ( 'NONE', ( #180334, #34652, #84456, #185546 ) ) ;
#111175 = CARTESIAN_POINT ( 'NONE',  ( 20.95000000000005258, 65.25000000001119815, -4.523107484524794053 ) ) ;
#111177 = LINE ( 'NONE', #92880, #31932 ) ;
#111178 = CARTESIAN_POINT ( 'NONE',  ( -18.50000000000000000, 46.32970330538243786, -243.0551226933711746 ) ) ;
#111179 = CARTESIAN_POINT ( 'NONE',  ( -22.50000000000000000, 11.64976291804307884, -167.4111900236130452 ) ) ;
#111180 = FACE_OUTER_BOUND ( 'NONE', #145351, .T. ) ;
#111181 = ORIENTED_EDGE ( 'NONE', *, *, #130925, .T. ) ;
#111182 = DIRECTION ( 'NONE',  ( -1.000000000000000000, 2.952720810173289112E-16, 2.061873921506763405E-30 ) ) ;
#111184 = FACE_OUTER_BOUND ( 'NONE', #132083, .T. ) ;
#111183 = DIRECTION ( 'NONE',  ( -1.000000000000000000, 0.000000000000000000, 0.000000000000000000 ) ) ;
#111185 = CARTESIAN_POINT ( 'NONE',  ( -20.54999999999999716, -4.161311414658873886, -226.0656773515597706 ) ) ;
#111186 = CARTESIAN_POINT ( 'NONE',  ( -23.39999999999994529, 83.98667523412385094, -34.76145429838185663 ) ) ;
#111187 = VECTOR ( 'NONE', #153181, 1000.000000000000000 ) ;
#111188 = CARTESIAN_POINT ( 'NONE',  ( -16.94389599337535657, 9.991197989767881538, -121.3923551982016420 ) ) ;
#111189 = CARTESIAN_POINT ( 'NONE',  ( -18.50000000000000000, -1.362429037182155023, -108.3888812479212476 ) ) ;
#111190 = DIRECTION ( 'NONE',  ( 1.000000000000000000, -0.000000000000000000, -0.000000000000000000 ) ) ;
#111191 = CARTESIAN_POINT ( 'NONE',  ( 20.73486653747088937, 7.750000000011182166, -121.3500000000000227 ) ) ;
#111192 = EDGE_LOOP ( 'NONE', ( #196784, #109445, #20610, #138306 ) ) ;
#111193 = VERTEX_POINT ( 'NONE', #87410 ) ;
#111194 = EDGE_LOOP ( 'NONE', ( #159772, #211379, #6481, #230151, #3002 ) ) ;
#111195 = CARTESIAN_POINT ( 'NONE',  ( 20.94999999999999929, -8.999999999988842703, -57.10603087734755690 ) ) ;
#111196 = CARTESIAN_POINT ( 'NONE',  ( -20.54999999999999716, 1.115600667400684642E-11, -67.00000000000000000 ) ) ;
#111197 = EDGE_CURVE ( 'NONE', #176651, #223292, #246493, .T. ) ;
#111198 = ORIENTED_EDGE ( 'NONE', *, *, #147656, .T. ) ;
#111199 = ADVANCED_FACE ( 'NONE', ( #127845 ), #132547, .T. ) ;
#111200 = TOROIDAL_SURFACE ( 'NONE', #81933, 12.77500000000000036, 0.1000000000000000056 ) ;
#111201 = ORIENTED_EDGE ( 'NONE', *, *, #199696, .F. ) ;
#111202 = AXIS2_PLACEMENT_3D ( 'NONE', #23662, #121477, #181438 ) ;
#111203 = AXIS2_PLACEMENT_3D ( 'NONE', #3732, #57266, #102809 ) ;
#111204 = EDGE_CURVE ( 'NONE', #157067, #215622, #236758, .T. ) ;
#111205 = ORIENTED_EDGE ( 'NONE', *, *, #10243, .T. ) ;
#111206 = DIRECTION ( 'NONE',  ( 0.000000000000000000, 0.000000000000000000, 1.000000000000000000 ) ) ;
#111207 = ORIENTED_EDGE ( 'NONE', *, *, #203750, .F. ) ;
#111208 = AXIS2_PLACEMENT_3D ( 'NONE', #10420, #228182, #31297 ) ;
#111209 = LINE ( 'NONE', #72094, #213826 ) ;
#111210 = CARTESIAN_POINT ( 'NONE',  ( 22.48660254037844197, 31.85034414784619017, -238.9397275603479898 ) ) ;
#111211 = CARTESIAN_POINT ( 'NONE',  ( 22.88900146558018989, 8.703904791112817563, -12.65000000000000746 ) ) ;
#111213 = EDGE_LOOP ( 'NONE', ( #78263, #224290, #34545, #29901 ) ) ;
#111212 = FACE_OUTER_BOUND ( 'NONE', #209387, .T. ) ;
#111215 = CARTESIAN_POINT ( 'NONE',  ( 21.11345278033261508, 8.882122073382229033, -79.24602217075594979 ) ) ;
#111214 = CARTESIAN_POINT ( 'NONE',  ( 20.94999999999999929, 11.74999999999999822, -26.71613433702190932 ) ) ;
#111216 = CARTESIAN_POINT ( 'NONE',  ( -16.87786941232801396, 9.958154714156124854, -154.8771857997940060 ) ) ;
#111217 = ORIENTED_EDGE ( 'NONE', *, *, #32806, .T. ) ;
#111218 = CARTESIAN_POINT ( 'NONE',  ( 20.94999999999999929, 71.99422445362657186, -246.4870034924427671 ) ) ;
#111219 = CARTESIAN_POINT ( 'NONE',  ( -16.97683809663752186, 66.05000000001183480, -82.92547150272069700 ) ) ;
#111220 = FACE_OUTER_BOUND ( 'NONE', #225075, .T. ) ;
#111222 = EDGE_LOOP ( 'NONE', ( #108287, #66250, #223328, #24640 ) ) ;
#111221 = CIRCLE ( 'NONE', #82150, 0.09999999999998898659 ) ;
#111223 = AXIS2_PLACEMENT_3D ( 'NONE', #58321, #234407, #199148 ) ;
#111224 = SURFACE_SIDE_STYLE ('',( #72111 ) ) ;
#111225 = CARTESIAN_POINT ( 'NONE',  ( 20.85000000000000142, 76.00000000001126921, -203.5231074845248997 ) ) ;
#111226 = EDGE_CURVE ( 'NONE', #6238, #64945, #27498, .T. ) ;
#111227 = DIRECTION ( 'NONE',  ( 0.000000000000000000, 0.2128009952263485993, -0.9770955615653341697 ) ) ;
#111228 = ORIENTED_EDGE ( 'NONE', *, *, #121748, .T. ) ;
#111229 = AXIS2_PLACEMENT_3D ( 'NONE', #163567, #60590, #140122 ) ;
#111230 = DIRECTION ( 'NONE',  ( 0.000000000000000000, -2.775557561562888827E-14, 1.000000000000000000 ) ) ;
#111231 = CARTESIAN_POINT ( 'NONE',  ( -23.15000000000000213, 11.75000000001115552, -146.2500000000000284 ) ) ;
#111232 = ADVANCED_FACE ( 'NONE', ( #228229 ), #157723, .T. ) ;
#111233 = CARTESIAN_POINT ( 'NONE',  ( -20.94999999999999929, 64.40000000001234071, -163.0949042542488883 ) ) ;
#111234 = VERTEX_POINT ( 'NONE', #129124 ) ;
#111235 = EDGE_LOOP ( 'NONE', ( #91663, #250856, #158935, #231166 ) ) ;
#111236 = EDGE_CURVE ( 'NONE', #188929, #240745, #206091, .T. ) ;
#111237 = B_SPLINE_CURVE_WITH_KNOTS ( 'NONE', 3,
 ( #174124, #155821, #157100, #60534, #239185, #116667 ),
 .UNSPECIFIED., .F., .F.,
 ( 4, 2, 4 ),
 ( 0.000000000000000000, 0.0001568709654583421050, 0.0003137419309166841557 ),
 .UNSPECIFIED. ) ;
#111238 = DIRECTION ( 'NONE',  ( 0.000000000000000000, 0.000000000000000000, 1.000000000000000000 ) ) ;
#111239 = CARTESIAN_POINT ( 'NONE',  ( 23.14999999999999503, 6.650000000011155876, -155.2500000000000284 ) ) ;
#111240 = CARTESIAN_POINT ( 'NONE',  ( 20.94983749550516450, 65.70233904877071041, -164.5487410911968595 ) ) ;
#111241 = DIRECTION ( 'NONE',  ( -1.000000000000000000, -0.000000000000000000, 0.000000000000000000 ) ) ;
#111242 = EDGE_CURVE ( 'NONE', #257696, #256658, #186534, .T. ) ;
#111244 = DIRECTION ( 'NONE',  ( 0.000000000000000000, 0.9126074666063772600, 0.4088369013363277737 ) ) ;
#111243 = CARTESIAN_POINT ( 'NONE',  ( 18.59999999999999076, 67.23127455305835554, -235.8551265064784559 ) ) ;
#111245 = TOROIDAL_SURFACE ( 'NONE', #128005, 11.65000000000000036, 0.1000000000000000056 ) ;
#111246 = AXIS2_PLACEMENT_3D ( 'NONE', #116345, #134583, #158076 ) ;
#111247 = DIRECTION ( 'NONE',  ( -1.000000000000000000, -0.000000000000000000, -0.000000000000000000 ) ) ;
#111249 = VECTOR ( 'NONE', #76064, 1000.000000000000000 ) ;
#111248 = DIRECTION ( 'NONE',  ( 0.000000000000000000, 0.000000000000000000, -1.000000000000000000 ) ) ;
#111250 = VECTOR ( 'NONE', #62773, 1000.000000000000000 ) ;
#111251 = ORIENTED_EDGE ( 'NONE', *, *, #167386, .F. ) ;
#111252 = DIRECTION ( 'NONE',  ( 0.5932847527679299127, -0.8049926720990051576, 6.366092712777055223E-16 ) ) ;
#111253 = EDGE_CURVE ( 'NONE', #212172, #75051, #111899, .T. ) ;
#111255 = ORIENTED_EDGE ( 'NONE', *, *, #197393, .F. ) ;
#111254 = DIRECTION ( 'NONE',  ( 1.000000000000000000, 0.000000000000000000, 0.000000000000000000 ) ) ;
#111256 = CARTESIAN_POINT ( 'NONE',  ( 21.53699400380727269, 69.21228820682173932, -170.0231074845244166 ) ) ;
#111258 = EDGE_CURVE ( 'NONE', #128012, #121012, #124543, .T. ) ;
#111257 = EDGE_CURVE ( 'NONE', #243888, #225036, #32635, .T. ) ;
#111259 = DIRECTION ( 'NONE',  ( 0.000000000000000000, -0.9908441862701644620, 0.1350103645451558587 ) ) ;
#111260 = CARTESIAN_POINT ( 'NONE',  ( 23.14999999999999858, -1.999999999988846699, -100.5000000000000426 ) ) ;
#111261 = DIRECTION ( 'NONE',  ( 0.000000000000000000, 0.9126074666063660468, 0.4088369013363524762 ) ) ;
#111262 = CARTESIAN_POINT ( 'NONE',  ( 23.14999999999998437, 5.216452187118270523, -237.3027570999230988 ) ) ;
#111264 = ORIENTED_EDGE ( 'NONE', *, *, #63348, .F. ) ;
#111263 = CARTESIAN_POINT ( 'NONE',  ( 22.00411653962156677, 68.74655713164199256, -136.6221455902929733 ) ) ;
#111265 = CARTESIAN_POINT ( 'NONE',  ( -21.05000000000000071, 1.115600667400684642E-11, -134.0000000000000000 ) ) ;
#111266 = CARTESIAN_POINT ( 'NONE',  ( -16.81744102076748959, 51.61886293219124155, -231.9464690156495692 ) ) ;
#111267 = CARTESIAN_POINT ( 'NONE',  ( -18.59999999999999787, 77.83585931145546510, -91.51866831572576189 ) ) ;
#111268 = FACE_OUTER_BOUND ( 'NONE', #51638, .T. ) ;
#111269 = EDGE_LOOP ( 'NONE', ( #55196, #49397, #164548 ) ) ;
#111270 = DIRECTION ( 'NONE',  ( 0.000000000000000000, -0.2128009952263485993, 0.9770955615653341697 ) ) ;
#111271 = VERTEX_POINT ( 'NONE', #208677 ) ;
#111272 = AXIS2_PLACEMENT_3D ( 'NONE', #253082, #171048, #250518 ) ;
#111273 = AXIS2_PLACEMENT_3D ( 'NONE', #151659, #12146, #91656 ) ;
#111275 = AXIS2_PLACEMENT_3D ( 'NONE', #28674, #229401, #166886 ) ;
#111274 = FACE_OUTER_BOUND ( 'NONE', #204787, .T. ) ;
#111276 = EDGE_LOOP ( 'NONE', ( #172445, #145795, #106536, #44359 ) ) ;
#111277 = CARTESIAN_POINT ( 'NONE',  ( 20.84999999999998721, 87.75000000001246292, -170.0231074845242745 ) ) ;
#111278 = EDGE_CURVE ( 'NONE', #230992, #134353, #228600, .T. ) ;
#111279 = EDGE_CURVE ( 'NONE', #5875, #34079, #257750, .T. ) ;
#111280 = EDGE_LOOP ( 'NONE', ( #256670, #233786, #67223, #246211 ) ) ;
#111282 = DIRECTION ( 'NONE',  ( 0.000000000000000000, 0.000000000000000000, -1.000000000000000000 ) ) ;
#111281 = AXIS2_PLACEMENT_3D ( 'NONE', #75113, #232901, #34697 ) ;
#111283 = DIRECTION ( 'NONE',  ( 0.000000000000000000, 0.4999999999999689138, 0.8660254037844565822 ) ) ;
#111284 = EDGE_CURVE ( 'NONE', #71686, #199332, #186919, .T. ) ;
#111285 = CARTESIAN_POINT ( 'NONE',  ( -18.59999999999999787, 63.74333919030581086, -212.9951329171253747 ) ) ;
#111286 = VERTEX_POINT ( 'NONE', #108283 ) ;
#111287 = CARTESIAN_POINT ( 'NONE',  ( -16.80891096016323516, 9.949999999999983302, -12.63233719273114275 ) ) ;
#111288 = EDGE_CURVE ( 'NONE', #92871, #177284, #116184, .T. ) ;
#111289 = DIRECTION ( 'NONE',  ( -1.000000000000000000, 2.952720810173289112E-16, 2.061873921506763405E-30 ) ) ;
#111290 = CARTESIAN_POINT ( 'NONE',  ( 21.14999999999999858, 76.10000000001198828, -109.5637644362255543 ) ) ;
#111291 = ADVANCED_FACE ( 'NONE', ( #209956 ), #149495, .T. ) ;
#111292 = CARTESIAN_POINT ( 'NONE',  ( 12.48201962039795987, 9.376659938533533634, -17.62819254821727100 ) ) ;
#111293 = PLANE ( 'NONE',  #15459 ) ;
#111294 = AXIS2_PLACEMENT_3D ( 'NONE', #52444, #210269, #70776 ) ;
#111295 = ORIENTED_EDGE ( 'NONE', *, *, #94478, .F. ) ;
#111296 = CYLINDRICAL_SURFACE ( 'NONE', #203206, 0.09999999999999939493 ) ;
#111297 = ORIENTED_EDGE ( 'NONE', *, *, #197979, .F. ) ;
#111299 = ORIENTED_EDGE ( 'NONE', *, *, #191536, .F. ) ;
#111298 = CARTESIAN_POINT ( 'NONE',  ( 20.87600722750343252, 10.33112638556969465, -106.0901228926975080 ) ) ;
#111300 = ORIENTED_EDGE ( 'NONE', *, *, #249521, .F. ) ;
#111301 = CARTESIAN_POINT ( 'NONE',  ( -21.04999999999994387, 64.35000000001120668, -51.02310748452479316 ) ) ;
#111302 = ORIENTED_EDGE ( 'NONE', *, *, #130757, .F. ) ;
#111303 = CARTESIAN_POINT ( 'NONE',  ( 22.59999999999999787, 31.80488924422933295, -238.9605610896540213 ) ) ;
#111304 = CARTESIAN_POINT ( 'NONE',  ( 21.05000000000000071, 87.65000000001268177, -203.5231074845243029 ) ) ;
#111305 = CARTESIAN_POINT ( 'NONE',  ( -20.54999999999999716, 0.000000000000000000, -33.50000000000000000 ) ) ;
#111306 = ORIENTED_EDGE ( 'NONE', *, *, #29312, .T. ) ;
#111307 = EDGE_CURVE ( 'NONE', #59389, #77760, #89978, .T. ) ;
#111308 = TOROIDAL_SURFACE ( 'NONE', #15658, 4.149999999999999467, 0.1000000000000000056 ) ;
#111309 = CARTESIAN_POINT ( 'NONE',  ( 18.59999999999999076, 64.35000000001220144, -145.1731074845244507 ) ) ;
#111310 = ORIENTED_EDGE ( 'NONE', *, *, #91939, .F. ) ;
#111312 = ORIENTED_EDGE ( 'NONE', *, *, #43296, .T. ) ;
#111311 = CYLINDRICAL_SURFACE ( 'NONE', #55230, 11.80000000000000604 ) ;
#111313 = DIRECTION ( 'NONE',  ( 0.000000000000000000, 6.982962677686266711E-15, -1.000000000000000000 ) ) ;
#111314 = DIRECTION ( 'NONE',  ( 1.000000000000000000, 0.000000000000000000, 0.000000000000000000 ) ) ;
#111315 = AXIS2_PLACEMENT_3D ( 'NONE', #228684, #129572, #125706 ) ;
#111316 = EDGE_CURVE ( 'NONE', #175328, #114775, #12134, .T. ) ;
#111317 = VECTOR ( 'NONE', #191227, 1000.000000000000000 ) ;
#111318 = CIRCLE ( 'NONE', #82229, 0.1000000000000028644 ) ;
#111319 = EDGE_LOOP ( 'NONE', ( #35928, #172370, #152679, #252548, #69906 ) ) ;
#111320 = AXIS2_PLACEMENT_3D ( 'NONE', #241730, #63083, #142609 ) ;
#111321 = CARTESIAN_POINT ( 'NONE',  ( -16.92507428761699018, 9.950000000011140600, -87.78660254037849597 ) ) ;
#111322 = CYLINDRICAL_SURFACE ( 'NONE', #503, 11.80000000000000426 ) ;
#111323 = CARTESIAN_POINT ( 'NONE',  ( -20.90851465518105812, 18.40294846151842023, -236.9778203247716419 ) ) ;
#111325 = ORIENTED_EDGE ( 'NONE', *, *, #57581, .T. ) ;
#111324 = CIRCLE ( 'NONE', #15673, 11.74999999999999645 ) ;
#111326 = DIRECTION ( 'NONE',  ( 0.000000000000000000, -0.7397890806274222131, -0.6728388485993010981 ) ) ;
#111327 = EDGE_CURVE ( 'NONE', #104663, #185781, #112147, .T. ) ;
#111328 = AXIS2_PLACEMENT_3D ( 'NONE', #204190, #248469, #127237 ) ;
#111329 = CARTESIAN_POINT ( 'NONE',  ( 21.05000000000000071, 64.25000000001249134, -176.8647081744215370 ) ) ;
#111330 = DIRECTION ( 'NONE',  ( 1.000000000000000000, 0.000000000000000000, 0.000000000000000000 ) ) ;
#111331 = AXIS2_PLACEMENT_3D ( 'NONE', #90065, #169668, #7993 ) ;
#111332 = TOROIDAL_SURFACE ( 'NONE', #198804, 0.2000000000000000111, 0.1000000000000000056 ) ;
#111333 = VERTEX_POINT ( 'NONE', #76838 ) ;
#111334 = CARTESIAN_POINT ( 'NONE',  ( 21.12230431290519661, 0.005209851700161530035, -94.04243334670701415 ) ) ;
#111335 = CIRCLE ( 'NONE', #198990, 0.1000000000000028644 ) ;
#111336 = ORIENTED_EDGE ( 'NONE', *, *, #176082, .F. ) ;
#111337 = AXIS2_PLACEMENT_3D ( 'NONE', #108458, #111024, #190583 ) ;
#111338 = DIRECTION ( 'NONE',  ( 0.000000000000000000, 0.000000000000000000, 1.000000000000000000 ) ) ;
#111339 = DIRECTION ( 'NONE',  ( 1.000000000000000000, 3.265361837132813093E-16, -0.000000000000000000 ) ) ;
#111341 = ORIENTED_EDGE ( 'NONE', *, *, #123918, .F. ) ;
#111340 = DIRECTION ( 'NONE',  ( 1.000000000000000000, 0.000000000000000000, 0.000000000000000000 ) ) ;
#111342 = DIRECTION ( 'NONE',  ( 1.000000000000000000, 0.000000000000000000, 0.000000000000000000 ) ) ;
#111344 = TOROIDAL_SURFACE ( 'NONE', #3168, 11.70000000000000639, 0.1000000000000000056 ) ;
#111343 = CARTESIAN_POINT ( 'NONE',  ( 21.08750232978087524, 65.27513661400141132, -57.29424931152482259 ) ) ;
#111345 = CARTESIAN_POINT ( 'NONE',  ( 20.94999999999999929, 0.000000000000000000, -33.50000000000000000 ) ) ;
#111346 = CARTESIAN_POINT ( 'NONE',  ( 20.94999999999999574, -1.162701749926853712, -175.4999999999999716 ) ) ;
#111347 = DIRECTION ( 'NONE',  ( 0.000000000000000000, -0.4721928772777346239, -0.8814952561688430555 ) ) ;
#111348 = CARTESIAN_POINT ( 'NONE',  ( 21.09813707148777340, 6.385062105747657313, -66.96864850047053608 ) ) ;
#111350 = EDGE_LOOP ( 'NONE', ( #220474, #139600, #206309 ) ) ;
#111349 = CYLINDRICAL_SURFACE ( 'NONE', #211026, 0.09999999999999939493 ) ;
#111351 = CIRCLE ( 'NONE', #65372, 7.800000000000001599 ) ;
#111352 = AXIS2_PLACEMENT_3D ( 'NONE', #210059, #232196, #31443 ) ;
#111353 = AXIS2_PLACEMENT_3D ( 'NONE', #160301, #102837, #23363 ) ;
#111354 = DIRECTION ( 'NONE',  ( -1.000000000000000000, -0.000000000000000000, -0.000000000000000000 ) ) ;
#111355 = DIRECTION ( 'NONE',  ( 0.5735764363510457153, 0.8191520442889921316, -0.000000000000000000 ) ) ;
#111356 = CARTESIAN_POINT ( 'NONE',  ( -18.59999999999999787, 38.30077178631846380, -261.1858881914067751 ) ) ;
#111357 = LINE ( 'NONE', #34417, #43214 ) ;
#111358 = VERTEX_POINT ( 'NONE', #74316 ) ;
#111359 = AXIS2_PLACEMENT_3D ( 'NONE', #120183, #79707, #159285 ) ;
#111360 = EDGE_CURVE ( 'NONE', #244742, #220385, #57871, .T. ) ;
#111361 = DIRECTION ( 'NONE',  ( 0.000000000000000000, -0.4930308989874729320, -0.8700118002898605818 ) ) ;
#111362 = CIRCLE ( 'NONE', #3194, 12.77500000000000036 ) ;
#111363 = LINE ( 'NONE', #168815, #178354 ) ;
#111364 = ORIENTED_EDGE ( 'NONE', *, *, #135592, .F. ) ;
#111365 = CARTESIAN_POINT ( 'NONE',  ( -2.995603634470891112E-16, 69.35000000001200249, -115.3731074845243398 ) ) ;
#111367 = CARTESIAN_POINT ( 'NONE',  ( -16.94309007106719989, 9.992226192581140864, -79.60579128255554338 ) ) ;
#111366 = AXIS2_PLACEMENT_3D ( 'NONE', #179440, #218519, #20373 ) ;
#111368 = ORIENTED_EDGE ( 'NONE', *, *, #191441, .T. ) ;
#111369 = CARTESIAN_POINT ( 'NONE',  ( 23.14999999999999858, 76.00000000001216449, -140.5231074845243597 ) ) ;
#111370 = EDGE_LOOP ( 'NONE', ( #215076, #224016, #121094, #208388 ) ) ;
#111371 = EDGE_CURVE ( 'NONE', #15317, #213246, #145180, .T. ) ;
#111372 = DIRECTION ( 'NONE',  ( 0.000000000000000000, 0.000000000000000000, 1.000000000000000000 ) ) ;
#111374 = ORIENTED_EDGE ( 'NONE', *, *, #146552, .F. ) ;
#111373 = DIRECTION ( 'NONE',  ( -1.000000000000000000, 0.000000000000000000, 0.000000000000000000 ) ) ;
#111375 = CIRCLE ( 'NONE', #32299, 0.09999999999999939493 ) ;
#111377 = EDGE_CURVE ( 'NONE', #194138, #248733, #183913, .T. ) ;
#111376 = FACE_OUTER_BOUND ( 'NONE', #213878, .T. ) ;
#111378 = CIRCLE ( 'NONE', #177490, 0.09999999999999939493 ) ;
#111379 = ORIENTED_EDGE ( 'NONE', *, *, #194000, .F. ) ;
#111380 = DIRECTION ( 'NONE',  ( 1.000000000000000000, 2.952720810173289112E-16, -0.000000000000000000 ) ) ;
#111381 = CIRCLE ( 'NONE', #157199, 11.90000000000000746 ) ;
#111382 = CIRCLE ( 'NONE', #119780, 0.09999999999999939493 ) ;
#111383 = EDGE_LOOP ( 'NONE', ( #199470, #213794, #177731, #223251 ) ) ;
#111385 = VERTEX_POINT ( 'NONE', #152568 ) ;
#111384 = ORIENTED_EDGE ( 'NONE', *, *, #242263, .F. ) ;
#111386 = CARTESIAN_POINT ( 'NONE',  ( 18.51565452909259690, 85.35285933884755138, -129.3281981632919440 ) ) ;
#111387 = AXIS2_PLACEMENT_3D ( 'NONE', #254932, #178049, #235417 ) ;
#111389 = EDGE_LOOP ( 'NONE', ( #60106, #148342, #69033, #141459 ) ) ;
#111388 = DIRECTION ( 'NONE',  ( 0.000000000000000000, 0.000000000000000000, -1.000000000000000000 ) ) ;
#111390 = DIRECTION ( 'NONE',  ( 1.000000000000000000, 0.000000000000000000, 0.000000000000000000 ) ) ;
#111391 = ORIENTED_EDGE ( 'NONE', *, *, #16732, .T. ) ;
#111392 = TOROIDAL_SURFACE ( 'NONE', #157203, 0.2000000000000000111, 0.1000000000000000056 ) ;
#111393 = ADVANCED_FACE ( 'NONE', ( #52131 ), #175973, .F. ) ;
#111394 = EDGE_CURVE ( 'NONE', #69020, #25903, #155137, .T. ) ;
#111395 = ORIENTED_EDGE ( 'NONE', *, *, #132292, .F. ) ;
#111396 = CARTESIAN_POINT ( 'NONE',  ( 18.59999999999999076, 11.75000000001115907, -155.7499999999999716 ) ) ;
#111397 = DIRECTION ( 'NONE',  ( -1.000000000000000000, 0.000000000000000000, 0.000000000000000000 ) ) ;
#111398 = DIRECTION ( 'NONE',  ( 1.000000000000000000, 0.000000000000000000, 0.000000000000000000 ) ) ;
#111399 = ORIENTED_EDGE ( 'NONE', *, *, #23240, .F. ) ;
#111400 = EDGE_CURVE ( 'NONE', #182617, #193318, #55972, .T. ) ;
#111401 = DIRECTION ( 'NONE',  ( 0.000000000000000000, -0.8814952561688430555, 0.4721928772777346239 ) ) ;
#111402 = CARTESIAN_POINT ( 'NONE',  ( 21.12400247839512701, 65.27851195598117329, -57.27310748452440237 ) ) ;
#111403 = DIRECTION ( 'NONE',  ( 0.000000000000000000, -0.9915357197604882655, 0.1298341882519793711 ) ) ;
#111404 = ORIENTED_EDGE ( 'NONE', *, *, #30093, .F. ) ;
#111405 = CARTESIAN_POINT ( 'NONE',  ( -23.25000000000000000, 85.60000000001178933, -79.41707660717668205 ) ) ;
#111406 = CARTESIAN_POINT ( 'NONE',  ( -17.29158576265544056, 10.36474766601791409, -11.41724175520783113 ) ) ;
#111407 = EDGE_CURVE ( 'NONE', #130629, #158029, #117262, .T. ) ;
#111408 = LINE ( 'NONE', #171418, #26226 ) ;
#111409 = EDGE_LOOP ( 'NONE', ( #65784, #243609, #174591, #42967 ) ) ;
#111410 = FACE_OUTER_BOUND ( 'NONE', #10814, .T. ) ;
#111411 = EDGE_LOOP ( 'NONE', ( #116687, #250255, #193453, #45062, #141755, #127221, #129743, #194190 ) ) ;
#111412 = CARTESIAN_POINT ( 'NONE',  ( -21.05000000000000071, 87.48912529308871910, -200.4231074845242802 ) ) ;
#111414 = ORIENTED_EDGE ( 'NONE', *, *, #45538, .T. ) ;
#111413 = AXIS2_PLACEMENT_3D ( 'NONE', #227073, #247922, #47135 ) ;
#111415 = ADVANCED_FACE ( 'NONE', ( #33922 ), #54711, .F. ) ;
#111416 = CARTESIAN_POINT ( 'NONE',  ( -23.15000000000000213, 21.17283678855157802, -243.7231193059830332 ) ) ;
#111417 = CARTESIAN_POINT ( 'NONE',  ( -18.50000000000000000, 5.341242990002803559, -90.69334979351201298 ) ) ;
#111418 = VERTEX_POINT ( 'NONE', #97665 ) ;
#111419 = ORIENTED_EDGE ( 'NONE', *, *, #221705, .T. ) ;
#111420 = LINE ( 'NONE', #108837, #211289 ) ;
#111421 = DIRECTION ( 'NONE',  ( -0.000000000000000000, -0.000000000000000000, -1.000000000000000000 ) ) ;
#111422 = ORIENTED_EDGE ( 'NONE', *, *, #168542, .T. ) ;
#111423 = CARTESIAN_POINT ( 'NONE',  ( 20.94999999999999574, -1.851028230140860487, -11.65391326942249250 ) ) ;
#111424 = FACE_OUTER_BOUND ( 'NONE', #42845, .T. ) ;
#111425 = EDGE_CURVE ( 'NONE', #163009, #224530, #256713, .T. ) ;
#111426 = VERTEX_POINT ( 'NONE', #131685 ) ;
#111427 = VECTOR ( 'NONE', #14400, 1000.000000000000000 ) ;
#111428 = TOROIDAL_SURFACE ( 'NONE', #257119, 0.2000000000000000111, 0.1000000000000000056 ) ;
#111429 = AXIS2_PLACEMENT_3D ( 'NONE', #32680, #74367, #152613 ) ;
#111430 = ORIENTED_EDGE ( 'NONE', *, *, #130877, .F. ) ;
#111431 = DIRECTION ( 'NONE',  ( 0.000000000000000000, -1.000000000000000000, -6.982962677686266711E-15 ) ) ;
#111432 = DIRECTION ( 'NONE',  ( 0.000000000000000000, 0.9126074666063753726, 0.4088369013363320481 ) ) ;
#111433 = DIRECTION ( 'NONE',  ( 1.000000000000000000, 0.000000000000000000, 0.000000000000000000 ) ) ;
#111434 = VERTEX_POINT ( 'NONE', #132987 ) ;
#111435 = FACE_OUTER_BOUND ( 'NONE', #137940, .T. ) ;
#111436 = CARTESIAN_POINT ( 'NONE',  ( -22.50000000000000000, 12.54152817314150248, -223.4164406214577241 ) ) ;
#111437 = DIRECTION ( 'NONE',  ( 0.000000000000000000, -0.7071067811865479058, -0.7071067811865472397 ) ) ;
#111440 = DIRECTION ( 'NONE',  ( 1.000000000000000000, -0.000000000000000000, -0.000000000000000000 ) ) ;
#111439 = CIRCLE ( 'NONE', #257142, 6.258578643762719551 ) ;
#111438 = CARTESIAN_POINT ( 'NONE',  ( -17.01825945287482966, 23.02528674727019364, -230.8469138855057281 ) ) ;
#111441 = CARTESIAN_POINT ( 'NONE',  ( -18.50000000000000000, 64.35000000001259934, -191.3731074845244393 ) ) ;
#111442 = CARTESIAN_POINT ( 'NONE',  ( 18.45068634130097252, -9.486506073331604227, -107.5687784311681412 ) ) ;
#111443 = AXIS2_PLACEMENT_3D ( 'NONE', #204587, #202037, #25974 ) ;
#111444 = CARTESIAN_POINT ( 'NONE',  ( 23.24999999999999645, 2.100000000011158274, -67.00000000000000000 ) ) ;
#111445 =( BOUNDED_SURFACE ( )  B_SPLINE_SURFACE ( 3, 2, ( 
 ( #221339, #244762, #102672 ),
 ( #186094, #124841, #161410 ),
 ( #165242, #140527, #143090 ),
 ( #184797, #204354, #2296 ),
 ( #121013, #3593, #144363 ),
 ( #222620, #162683, #203077 ) ),
 .UNSPECIFIED., .F., .F., .T. ) 
 B_SPLINE_SURFACE_WITH_KNOTS ( ( 4, 2, 4 ),
 ( 3, 3 ),
 ( 1.570796326794895448, 2.356194490192343505, 3.141592653589791784 ),
 ( 0.000000000000000000, 1.000000000000000000 ),
 .UNSPECIFIED. ) 
 GEOMETRIC_REPRESENTATION_ITEM ( )  RATIONAL_B_SPLINE_SURFACE ( (
 ( 1.000000000000000000, 0.7071067811865475727, 1.000000000000000000),
 ( 1.000000000000000000, 0.6611148371776656152, 1.000000000000000000),
 ( 1.000000000000000000, 0.6092287576699577656, 1.000000000000000000),
 ( 1.000000000000000000, 0.5278258667053233877, 1.000000000000000000),
 ( 1.000000000000000000, 0.4993418825337002098, 1.000000000000000000),
 ( 1.000000000000000000, 0.5000000000000154321, 1.000000000000000000) ) ) 
 REPRESENTATION_ITEM ( '' )  SURFACE ( )  );
#111446 = ORIENTED_EDGE ( 'NONE', *, *, #194896, .T. ) ;
#111447 = ADVANCED_FACE ( 'NONE', ( #211221 ), #128633, .F. ) ;
#111448 = VECTOR ( 'NONE', #69670, 1000.000000000000000 ) ;
#111449 = VERTEX_POINT ( 'NONE', #92545 ) ;
#111450 = EDGE_CURVE ( 'NONE', #206017, #35453, #74517, .T. ) ;
#111451 = EDGE_CURVE ( 'NONE', #149939, #13384, #213787, .T. ) ;
#111452 = CARTESIAN_POINT ( 'NONE',  ( -23.25000000000000000, -0.09999999998884338825, -88.85042919245522341 ) ) ;
#111453 = DIRECTION ( 'NONE',  ( 1.000000000000000000, 0.000000000000000000, 0.000000000000000000 ) ) ;
#111454 = ORIENTED_EDGE ( 'NONE', *, *, #193127, .F. ) ;
#111455 = EDGE_CURVE ( 'NONE', #254522, #215662, #211846, .T. ) ;
#111457 = ADVANCED_FACE ( 'NONE', ( #100227 ), #112079, .F. ) ;
#111456 = CARTESIAN_POINT ( 'NONE',  ( 20.94999999999999929, 7.120270961708750512, -70.65956304183931991 ) ) ;
#111458 = DIRECTION ( 'NONE',  ( 1.000000000000000000, 0.000000000000000000, 0.000000000000000000 ) ) ;
#111459 = EDGE_CURVE ( 'NONE', #80949, #56502, #107773, .T. ) ;
#111460 = AXIS2_PLACEMENT_3D ( 'NONE', #236235, #176290, #198396 ) ;
#111461 = CARTESIAN_POINT ( 'NONE',  ( 23.14999999999999503, 35.97645343225767789, -235.9694016464868298 ) ) ;
#111462 = ORIENTED_EDGE ( 'NONE', *, *, #159256, .T. ) ;
#111463 = EDGE_CURVE ( 'NONE', #65265, #224530, #253514, .T. ) ;
#111464 = VERTEX_POINT ( 'NONE', #59818 ) ;
#111465 = AXIS2_PLACEMENT_3D ( 'NONE', #85368, #120710, #161107 ) ;
#111466 = LINE ( 'NONE', #193575, #75475 ) ;
#111467 = DIRECTION ( 'NONE',  ( 1.000000000000000000, -0.000000000000000000, -0.000000000000000000 ) ) ;
#111468 = ORIENTED_EDGE ( 'NONE', *, *, #16643, .F. ) ;
#111469 = EDGE_CURVE ( 'NONE', #231259, #256518, #199388, .T. ) ;
#111470 = B_SPLINE_CURVE_WITH_KNOTS ( 'NONE', 3,
 ( #79853, #83687, #223228, #336, #163285, #159438, #181572, #244082, #184108, #139842, #141151, #203684, #25071, #42059, #220682, #104545, #82416, #5453, #84981 ),
 .UNSPECIFIED., .F., .F.,
 ( 4, 3, 3, 3, 3, 3, 4 ),
 ( -2.000416914658901521E-06, 0.000000000000000000, 4.714008503744565809E-05, 9.979203887777271477E-05, 0.0001372215519229478891, 0.0001635031576220937453, 0.0001900083748504128364 ),
 .UNSPECIFIED. ) ;
#111471 = CARTESIAN_POINT ( 'NONE',  ( -23.25000000000000000, 69.06610602788607878, -166.2374616501508342 ) ) ;
#111473 = ORIENTED_EDGE ( 'NONE', *, *, #12906, .T. ) ;
#111472 = CARTESIAN_POINT ( 'NONE',  ( 20.02499999999999858, 66.25000000001179501, -81.77310748452437394 ) ) ;
#111474 = CARTESIAN_POINT ( 'NONE',  ( 18.59999999999999076, 62.39550153362034735, -208.7959266050682459 ) ) ;
#111475 = CIRCLE ( 'NONE', #144774, 0.1000000000000054040 ) ;
#111477 = VERTEX_POINT ( 'NONE', #198070 ) ;
#111476 = CARTESIAN_POINT ( 'NONE',  ( -23.25000000000000000, 1.115600667400684642E-11, -67.00000000000004263 ) ) ;
#111478 = CARTESIAN_POINT ( 'NONE',  ( 21.05000000000000071, 64.25000000001219291, -143.3647081744214802 ) ) ;
#111479 = FACE_OUTER_BOUND ( 'NONE', #116650, .T. ) ;
#111480 = CARTESIAN_POINT ( 'NONE',  ( -18.59999999999999787, -11.65000000000000036, 30.00000000000000000 ) ) ;
#111481 = AXIS2_PLACEMENT_3D ( 'NONE', #219048, #18295, #161682 ) ;
#111483 = DIRECTION ( 'NONE',  ( 0.000000000000000000, 0.000000000000000000, 1.000000000000000000 ) ) ;
#111482 = LINE ( 'NONE', #150614, #98989 ) ;
#111484 = DIRECTION ( 'NONE',  ( 0.000000000000000000, -6.938893903907222067E-15, 1.000000000000000000 ) ) ;
#111485 = CARTESIAN_POINT ( 'NONE',  ( -18.47130263965431141, 85.47115558597647578, -163.3397027190475512 ) ) ;
#111486 = VECTOR ( 'NONE', #239314, 1000.000000000000114 ) ;
#111487 = AXIS2_PLACEMENT_3D ( 'NONE', #48930, #247125, #68509 ) ;
#111488 = CARTESIAN_POINT ( 'NONE',  ( 21.05000000000000071, 1.560941917020248759, -230.7743948584411839 ) ) ;
#111489 = CARTESIAN_POINT ( 'NONE',  ( -21.05000000000000071, 1.835341550235567887, -179.0551512925629538 ) ) ;
#111490 = CIRCLE ( 'NONE', #32422, 0.09999999999999939493 ) ;
#111491 = ORIENTED_EDGE ( 'NONE', *, *, #187401, .T. ) ;
#111492 = EDGE_CURVE ( 'NONE', #107664, #214613, #143219, .T. ) ;
#111493 = DIRECTION ( 'NONE',  ( 1.000000000000000000, -3.265361837132813093E-16, -2.280189983783949500E-30 ) ) ;
#111494 = VECTOR ( 'NONE', #54038, 1000.000000000000000 ) ;
#111495 = VERTEX_POINT ( 'NONE', #83228 ) ;
#111496 = LINE ( 'NONE', #96710, #189405 ) ;
#111497 = ORIENTED_EDGE ( 'NONE', *, *, #160759, .T. ) ;
#111499 = FACE_OUTER_BOUND ( 'NONE', #41005, .T. ) ;
#111498 = VECTOR ( 'NONE', #212890, 1000.000000000000114 ) ;
#111500 =( LENGTH_UNIT ( ) NAMED_UNIT ( * ) SI_UNIT ( .MILLI., .METRE. ) );
#111501 = EDGE_CURVE ( 'NONE', #20561, #36642, #91224, .T. ) ;
#111502 = EDGE_CURVE ( 'NONE', #244178, #128108, #70407, .T. ) ;
#111503 =( BOUNDED_CURVE ( )  B_SPLINE_CURVE ( 3, ( #80173, #99748, #180601, #178048 ),
 .UNSPECIFIED., .F., .F. ) 
 B_SPLINE_CURVE_WITH_KNOTS ( ( 4, 4 ),
 ( 0.000000000000000000, 1.570796326794908992 ),
 .UNSPECIFIED. ) 
 CURVE ( )  GEOMETRIC_REPRESENTATION_ITEM ( )  RATIONAL_B_SPLINE_CURVE ( ( 1.000000000000000000, 0.8047378541243619399, 0.8047378541243619399, 1.000000000000000000 ) ) 
 REPRESENTATION_ITEM ( '' )  );
#111504 = ORIENTED_EDGE ( 'NONE', *, *, #87413, .F. ) ;
#111505 =( LENGTH_UNIT ( ) NAMED_UNIT ( * ) SI_UNIT ( .MILLI., .METRE. ) );
#111506 = AXIS2_PLACEMENT_3D ( 'NONE', #157488, #236994, #131471 ) ;
#111507 = ORIENTED_EDGE ( 'NONE', *, *, #170924, .F. ) ;
#111508 = CIRCLE ( 'NONE', #194915, 1.749999999999999778 ) ;
#111509 = ORIENTED_EDGE ( 'NONE', *, *, #207870, .T. ) ;
#111511 = SPHERICAL_SURFACE ( 'NONE', #208876, 0.1000000000000000056 ) ;
#111510 = AXIS2_PLACEMENT_3D ( 'NONE', #247431, #71390, #131336 ) ;
#111512 = CARTESIAN_POINT ( 'NONE',  ( -20.54999999999999716, 71.65000000001253966, -182.3731074845244109 ) ) ;
#111513 = CARTESIAN_POINT ( 'NONE',  ( 22.60000000000000142, 31.76322370622491320, -238.8696546380523671 ) ) ;
#111514 = SPHERICAL_SURFACE ( 'NONE', #186413, 0.1000000000000000056 ) ;
#111515 = LINE ( 'NONE', #91944, #214923 ) ;
#111516 = AXIS2_PLACEMENT_3D ( 'NONE', #234505, #212403, #170749 ) ;
#111518 = CARTESIAN_POINT ( 'NONE',  ( -18.34374000495059676, 11.47316190337362940, -57.75000000000000711 ) ) ;
#111517 = CARTESIAN_POINT ( 'NONE',  ( -20.54999999999999716, 85.50000000001251976, -179.9170766071767389 ) ) ;
#111519 = CARTESIAN_POINT ( 'NONE',  ( 18.49999999999999289, 10.34378108836433263, -58.32844527787764832 ) ) ;
#111521 = ORIENTED_EDGE ( 'NONE', *, *, #30392, .T. ) ;
#111520 = DIRECTION ( 'NONE',  ( 0.000000000000000000, 6.997203936713175802E-15, -1.000000000000000000 ) ) ;
#111522 = CARTESIAN_POINT ( 'NONE',  ( -18.40000000000000213, 64.52683809664931402, -82.07310748452439952 ) ) ;
#111523 = AXIS2_PLACEMENT_3D ( 'NONE', #236342, #95545, #112560 ) ;
#111524 = CARTESIAN_POINT ( 'NONE',  ( 23.15000000000000213, -11.64999999998883595, -55.25000000000004974 ) ) ;
#111525 = VERTEX_POINT ( 'NONE', #44144 ) ;
#111526 = CARTESIAN_POINT ( 'NONE',  ( -21.05000000000000071, 1.162701749949165642, -142.0000000000000284 ) ) ;
#111527 = CARTESIAN_POINT ( 'NONE',  ( 23.24999999999999645, 79.90000000001171543, -69.52310748452428868 ) ) ;
#111528 = CARTESIAN_POINT ( 'NONE',  ( -20.94999999999999929, 74.25000000001205080, -124.8535959266226598 ) ) ;
#111529 = VERTEX_POINT ( 'NONE', #217610 ) ;
#111530 = VECTOR ( 'NONE', #195534, 1000.000000000000114 ) ;
#111531 = CARTESIAN_POINT ( 'NONE',  ( 18.59999999999999076, 6.550000000011156231, -54.75000000000000000 ) ) ;
#111532 = CARTESIAN_POINT ( 'NONE',  ( -18.46856557590793457, 78.23413713284891458, -231.4806561747373053 ) ) ;
#111534 = ORIENTED_EDGE ( 'NONE', *, *, #28481, .F. ) ;
#111533 = AXIS2_PLACEMENT_3D ( 'NONE', #171544, #231500, #52833 ) ;
#111535 = ORIENTED_EDGE ( 'NONE', *, *, #197010, .F. ) ;
#111536 = CLOSED_SHELL ( 'NONE', ( #100286, #14906, #129888, #181256, #84914, #135319, #56711, #183070, #137682, #234681, #166949, #204848, #128016, #196548, #33204, #42802, #158369, #52037, #133613, #31016, #192852, #218237, #61406, #91446, #73254, #50395, #161515, #21760, #54273, #193356, #42976, #184845, #114744, #224182, #26983, #117011, #248405, #71902, #135763, #10985, #14642, #251438, #148738, #191594, #5932, #243493, #134155, #105158, #167507, #30219, #250415, #236431, #30894 ) ) ;
#111537 = CARTESIAN_POINT ( 'NONE',  ( -20.64999999999999858, 7.150000000000000355, -12.34999999999999964 ) ) ;
#111538 = CARTESIAN_POINT ( 'NONE',  ( -18.50596464788227635, 10.30632246271647112, -173.0041836778896140 ) ) ;
#111539 = CARTESIAN_POINT ( 'NONE',  ( 12.25000000000000000, 9.850000000011137402, -50.24999999999999289 ) ) ;
#111540 = CARTESIAN_POINT ( 'NONE',  ( 23.14999999999999503, 6.650000000011155876, -79.15000000000004832 ) ) ;
#111541 = ORIENTED_EDGE ( 'NONE', *, *, #177394, .T. ) ;
#111542 = CARTESIAN_POINT ( 'NONE',  ( -23.15000000000000213, 11.65000000001115588, -79.15000000000003411 ) ) ;
#111543 = AXIS2_PLACEMENT_3D ( 'NONE', #15634, #52141, #95136 ) ;
#111544 = ADVANCED_FACE ( 'NONE', ( #2420 ), #41169, .T. ) ;
#111545 = DIRECTION ( 'NONE',  ( 2.557131231893037478E-16, -0.1022405907414165593, -0.9947597004326453884 ) ) ;
#111546 = AXIS2_PLACEMENT_3D ( 'NONE', #20740, #19445, #200647 ) ;
#111547 = CARTESIAN_POINT ( 'NONE',  ( 21.00000000000000000, 52.06567329910104291, -231.9654557484363409 ) ) ;
#111548 = CARTESIAN_POINT ( 'NONE',  ( -21.65000000000000213, 65.32753222054176945, -213.4247798787853867 ) ) ;
#111549 = EDGE_CURVE ( 'NONE', #231640, #181320, #238482, .T. ) ;
#111550 = AXIS2_PLACEMENT_3D ( 'NONE', #226026, #48698, #64425 ) ;
#111551 = VERTEX_POINT ( 'NONE', #19447 ) ;
#111552 = LINE ( 'NONE', #191113, #255014 ) ;
#111553 = AXIS2_PLACEMENT_3D ( 'NONE', #123009, #185541, #163416 ) ;
#111554 = EDGE_CURVE ( 'NONE', #7639, #199740, #174479, .T. ) ;
#111556 = ORIENTED_EDGE ( 'NONE', *, *, #47488, .T. ) ;
#111555 = CARTESIAN_POINT ( 'NONE',  ( -16.94107738177415357, 65.98576071487597972, -190.9731074845244621 ) ) ;
#111557 = CARTESIAN_POINT ( 'NONE',  ( -20.54999999999999716, -9.000000000000003553, -9.893969122652444881 ) ) ;
#111558 = EDGE_CURVE ( 'NONE', #154355, #169627, #178550, .T. ) ;
#111559 = CARTESIAN_POINT ( 'NONE',  ( -20.94999999999999929, 76.00000000001142553, -36.02310748452432421 ) ) ;
#111560 = DIRECTION ( 'NONE',  ( -3.469446951953995998E-14, 0.000000000000000000, -1.000000000000000000 ) ) ;
#111561 = DIRECTION ( 'NONE',  ( -0.000000000000000000, 1.000000000000000000, 6.982962677686266711E-15 ) ) ;
#111562 = DIRECTION ( 'NONE',  ( 0.000000000000000000, 0.1350103645451876666, -0.9908441862701600211 ) ) ;
#111563 = EDGE_LOOP ( 'NONE', ( #182184, #66858 ) ) ;
#111564 = FACE_OUTER_BOUND ( 'NONE', #150605, .T. ) ;
#111565 = CIRCLE ( 'NONE', #223966, 0.2000000000000101419 ) ;
#111566 = LINE ( 'NONE', #131116, #188334 ) ;
#111567 = LINE ( 'NONE', #71172, #198767 ) ;
#111568 = ORIENTED_EDGE ( 'NONE', *, *, #100537, .T. ) ;
#111569 = CARTESIAN_POINT ( 'NONE',  ( 18.39999999999999858, 85.51932773110404185, -62.55013110796492271 ) ) ;
#111570 = DIRECTION ( 'NONE',  ( 0.000000000000000000, 0.000000000000000000, -1.000000000000000000 ) ) ;
#111571 = PLANE ( 'NONE',  #167169 ) ;
#111572 = AXIS2_PLACEMENT_3D ( 'NONE', #195260, #94837, #152280 ) ;
#111573 = AXIS2_PLACEMENT_3D ( 'NONE', #241728, #61814, #141344 ) ;
#111574 = CARTESIAN_POINT ( 'NONE',  ( -16.89268316805465986, 51.62340874627276577, -231.9425458505251072 ) ) ;
#111575 = VECTOR ( 'NONE', #147908, 1000.000000000000000 ) ;
#111576 = DIRECTION ( 'NONE',  ( 0.000000000000000000, -1.000000000000000000, -6.982962677686265922E-15 ) ) ;
#111577 = CIRCLE ( 'NONE', #136486, 0.09999999999999939493 ) ;
#111578 = CARTESIAN_POINT ( 'NONE',  ( 13.12229106158772751, 9.430637101707896264, -185.7682606180609639 ) ) ;
#111579 = EDGE_CURVE ( 'NONE', #168032, #217337, #58544, .T. ) ;
#111580 = ADVANCED_FACE ( 'NONE', ( #1129 ), #158980, .T. ) ;
#111581 = ORIENTED_EDGE ( 'NONE', *, *, #11084, .T. ) ;
#111582 = ORIENTED_EDGE ( 'NONE', *, *, #170197, .F. ) ;
#111583 = DIRECTION ( 'NONE',  ( -2.952720810173289112E-16, -0.9651348961777159730, 0.2617529984165024026 ) ) ;
#111584 = LINE ( 'NONE', #11200, #162207 ) ;
#111585 = CARTESIAN_POINT ( 'NONE',  ( -20.94999999999999929, 38.09878670418233781, -236.0309261423825262 ) ) ;
#111586 = DIRECTION ( 'NONE',  ( 0.000000000000000000, 7.026728003956683390E-15, -1.000000000000000000 ) ) ;
#111587 = DIRECTION ( 'NONE',  ( 0.000000000000000000, 0.000000000000000000, -1.000000000000000000 ) ) ;
#111588 = AXIS2_PLACEMENT_3D ( 'NONE', #69928, #149463, #228984 ) ;
#111589 = CARTESIAN_POINT ( 'NONE',  ( 20.94999999999999929, 76.00000000001190870, -103.0231074845243029 ) ) ;
#111590 = EDGE_CURVE ( 'NONE', #236175, #232261, #211820, .T. ) ;
#111591 = CARTESIAN_POINT ( 'NONE',  ( -16.93302609847409457, 9.996682520814371031, -113.0863884953625842 ) ) ;
#111592 = EDGE_CURVE ( 'NONE', #228170, #168895, #166079, .T. ) ;
#111593 = DIRECTION ( 'NONE',  ( 0.000000000000000000, -1.000000000000000000, 0.000000000000000000 ) ) ;
#111594 = ORIENTED_EDGE ( 'NONE', *, *, #154179, .F. ) ;
#111595 = CARTESIAN_POINT ( 'NONE',  ( -18.59999999999999787, 11.65000000001115232, -155.3500000000000227 ) ) ;
#111596 = ORIENTED_EDGE ( 'NONE', *, *, #80169, .F. ) ;
#111597 = LINE ( 'NONE', #32082, #151217 ) ;
#111598 = CARTESIAN_POINT ( 'NONE',  ( 20.94999999999999929, 10.47338541491290265, -7.578654464248539391 ) ) ;
#111599 = DIRECTION ( 'NONE',  ( -1.000000000000000000, 0.000000000000000000, 0.000000000000000000 ) ) ;
#111600 = EDGE_CURVE ( 'NONE', #71592, #81073, #66077, .T. ) ;
#111601 = CARTESIAN_POINT ( 'NONE',  ( 20.94999999999999929, 1.115600667400684642E-11, -167.5000000000000284 ) ) ;
#111602 =( NAMED_UNIT ( * ) SI_UNIT ( $, .STERADIAN. ) SOLID_ANGLE_UNIT ( ) );
#111603 = DIRECTION ( 'NONE',  ( 1.000000000000000000, 0.000000000000000000, 0.000000000000000000 ) ) ;
#111604 = CARTESIAN_POINT ( 'NONE',  ( 21.05000000000000071, 28.58935552370083144, -258.2621935127861548 ) ) ;
#111605 = ADVANCED_FACE ( 'NONE', ( #211888 ), #49524, .T. ) ;
#111606 = ORIENTED_EDGE ( 'NONE', *, *, #95875, .T. ) ;
#111607 = CARTESIAN_POINT ( 'NONE',  ( -16.94037747912386394, 22.92091771185253535, -230.8323684894537848 ) ) ;
#111608 = DIRECTION ( 'NONE',  ( 1.734723475976817507E-14, -1.000000000000000000, 0.000000000000000000 ) ) ;
#111609 = CARTESIAN_POINT ( 'NONE',  ( 20.94999999999999929, 62.08591502004790641, -248.5699171172615820 ) ) ;
#111610 = DIRECTION ( 'NONE',  ( 0.000000000000000000, 0.000000000000000000, 1.000000000000000000 ) ) ;
#111611 = EDGE_CURVE ( 'NONE', #79726, #86816, #116356, .T. ) ;
#111612 = AXIS2_PLACEMENT_3D ( 'NONE', #79116, #159987, #137808 ) ;
#111613 = CIRCLE ( 'NONE', #65813, 12.77500000000002522 ) ;
#111614 = DIRECTION ( 'NONE',  ( -1.000000000000000000, -0.000000000000000000, -0.000000000000000000 ) ) ;
#111615 = ORIENTED_EDGE ( 'NONE', *, *, #255216, .T. ) ;
#111616 = CARTESIAN_POINT ( 'NONE',  ( -23.15000000000000213, 4.150000000011156764, -146.3500000000000227 ) ) ;
#111617 = LINE ( 'NONE', #51600, #21034 ) ;
#111618 = VERTEX_POINT ( 'NONE', #84491 ) ;
#111619 = EDGE_CURVE ( 'NONE', #221938, #207052, #112772, .T. ) ;
#111620 = EDGE_LOOP ( 'NONE', ( #146051, #179201, #89538, #159525 ) ) ;
#111621 = LINE ( 'NONE', #33402, #147321 ) ;
#111622 = CARTESIAN_POINT ( 'NONE',  ( 18.49505816908823519, -9.437872553199978753, -174.2776572016709054 ) ) ;
#111623 = ADVANCED_FACE ( 'NONE', ( #224039 ), #34539, .T. ) ;
#111624 = VERTEX_POINT ( 'NONE', #28465 ) ;
#111625 = CARTESIAN_POINT ( 'NONE',  ( 20.85000000000000142, 77.83585931145570669, -125.0186683157258329 ) ) ;
#111626 = DIRECTION ( 'NONE',  ( -1.000000000000000000, -7.304098846218134667E-16, 0.000000000000000000 ) ) ;
#111627 = AXIS2_PLACEMENT_3D ( 'NONE', #206535, #70909, #9611 ) ;
#111628 = EDGE_LOOP ( 'NONE', ( #252112, #52086, #79618, #205190 ) ) ;
#111629 = EDGE_LOOP ( 'NONE', ( #63675, #238649, #125710, #212758 ) ) ;
#111630 = DIRECTION ( 'NONE',  ( -1.836970198721029934E-16, -1.000000000000000000, -6.982962677686266711E-15 ) ) ;
#111631 = DIRECTION ( 'NONE',  ( 1.000000000000000000, 0.000000000000000000, 0.000000000000000000 ) ) ;
#111633 = ORIENTED_EDGE ( 'NONE', *, *, #240741, .T. ) ;
#111632 = CARTESIAN_POINT ( 'NONE',  ( 21.05000000000000071, 8.629318835500072282, -209.3724661700624949 ) ) ;
#111634 = DIRECTION ( 'NONE',  ( -0.000000000000000000, -0.000000000000000000, 1.000000000000000000 ) ) ;
#111635 = FACE_OUTER_BOUND ( 'NONE', #24113, .T. ) ;
#111636 = CARTESIAN_POINT ( 'NONE',  ( -20.88420186297724612, 65.66974365629688748, -130.9360145562605169 ) ) ;
#111637 = CARTESIAN_POINT ( 'NONE',  ( 20.85000000000000142, -1.749999999988843813, -145.6189500386223017 ) ) ;
#111638 = DIRECTION ( 'NONE',  ( 1.296989514748957725E-15, 0.9151430362303984989, -0.4031292884906871321 ) ) ;
#111639 = CARTESIAN_POINT ( 'NONE',  ( -20.94999999999999929, 68.87972903831409610, -65.86354444268503983 ) ) ;
#111640 = CARTESIAN_POINT ( 'NONE',  ( -16.77902162784673479, 66.05358074280444214, -157.3611162404550896 ) ) ;
#111642 = ORIENTED_EDGE ( 'NONE', *, *, #16280, .F. ) ;
#111641 = CARTESIAN_POINT ( 'NONE',  ( 23.15000000000000213, -5.011722593499792211, -233.2041167654973322 ) ) ;
#111643 = ORIENTED_EDGE ( 'NONE', *, *, #165632, .F. ) ;
#111644 = CARTESIAN_POINT ( 'NONE',  ( -14.22969084473440304, 9.456007326080463571, -85.48863349414676804 ) ) ;
#111646 = EDGE_LOOP ( 'NONE', ( #98784, #46151, #237102, #223301 ) ) ;
#111645 = CARTESIAN_POINT ( 'NONE',  ( 21.05000000000000071, 8.776282648982402179, -75.48759237851896842 ) ) ;
#111647 = VECTOR ( 'NONE', #114395, 1000.000000000000000 ) ;
#111648 = ORIENTED_EDGE ( 'NONE', *, *, #25012, .F. ) ;
#111649 = CARTESIAN_POINT ( 'NONE',  ( -20.65000000000000568, 21.70314669089253812, -233.3151006027785286 ) ) ;
#111651 = CARTESIAN_POINT ( 'NONE',  ( -20.85000000000000142, 11.65000000001115232, -167.5000000000000284 ) ) ;
#111650 = TOROIDAL_SURFACE ( 'NONE', #15832, 12.97499999999999787, 0.1000000000000000056 ) ;
#111652 = AXIS2_PLACEMENT_3D ( 'NONE', #23416, #226703, #122497 ) ;
#111653 = DIRECTION ( 'NONE',  ( 0.7070776581709139474, -0.7071359030027652981, -2.453168425935592377E-14 ) ) ;
#111654 = CARTESIAN_POINT ( 'NONE',  ( 20.94999999999999929, 1.115600667400684642E-11, -67.00000000000000000 ) ) ;
#111656 = CARTESIAN_POINT ( 'NONE',  ( -23.15000000000000213, -11.74999999998884448, -155.7499999999999716 ) ) ;
#111655 = AXIS2_PLACEMENT_3D ( 'NONE', #90404, #14761, #91698 ) ;
#111657 = CARTESIAN_POINT ( 'NONE',  ( -20.64999999999999858, 7.250000000011155521, -54.75000000000000000 ) ) ;
#111658 = CARTESIAN_POINT ( 'NONE',  ( 23.24999999999999645, 71.22429906543317202, -191.6743393804784148 ) ) ;
#111659 = VERTEX_POINT ( 'NONE', #54072 ) ;
#111660 = ORIENTED_EDGE ( 'NONE', *, *, #230109, .T. ) ;
#111661 = ADVANCED_FACE ( 'NONE', ( #8864 ), #133607, .T. ) ;
#111662 = DIRECTION ( 'NONE',  ( -0.000000000000000000, -1.000000000000000000, -0.000000000000000000 ) ) ;
#111663 = AXIS2_PLACEMENT_3D ( 'NONE', #104592, #88900, #167207 ) ;
#111664 = VECTOR ( 'NONE', #217959, 1000.000000000000227 ) ;
#111665 = ORIENTED_EDGE ( 'NONE', *, *, #247536, .F. ) ;
#111666 = DIRECTION ( 'NONE',  ( 0.000000000000000000, 0.9126074666063769270, 0.4088369013363280513 ) ) ;
#111667 = ORIENTED_EDGE ( 'NONE', *, *, #40894, .T. ) ;
#111669 = DIRECTION ( 'NONE',  ( 1.000000000000000000, 0.000000000000000000, 0.000000000000000000 ) ) ;
#111668 = VECTOR ( 'NONE', #101684, 1000.000000000000000 ) ;
#111670 = AXIS2_PLACEMENT_3D ( 'NONE', #44553, #7996, #47085 ) ;
#111671 = CARTESIAN_POINT ( 'NONE',  ( -20.85000000000000142, 76.30149234032609229, -203.6488173052385946 ) ) ;
#111672 = ADVANCED_FACE ( 'NONE', ( #213146 ), #12313, .F. ) ;
#111673 = CARTESIAN_POINT ( 'NONE',  ( -23.49999999999994316, 64.35000000001120668, -18.32310748452479388 ) ) ;
#111674 = ORIENTED_EDGE ( 'NONE', *, *, #114300, .F. ) ;
#111675 = DIRECTION ( 'NONE',  ( -0.000000000000000000, 6.982962677686266711E-15, -1.000000000000000000 ) ) ;
#111676 = EDGE_LOOP ( 'NONE', ( #19421, #70608, #228752, #242432 ) ) ;
#111677 = EDGE_CURVE ( 'NONE', #244526, #34172, #49709, .T. ) ;
#111678 = EDGE_CURVE ( 'NONE', #226855, #2981, #105348, .T. ) ;
#111679 = DIRECTION ( 'NONE',  ( 1.000000000000000000, 0.000000000000000000, 0.000000000000000000 ) ) ;
#111680 = CARTESIAN_POINT ( 'NONE',  ( 18.49351773456764292, 9.003734232116954672, -245.4495432009024114 ) ) ;
#111681 = ORIENTED_EDGE ( 'NONE', *, *, #133605, .F. ) ;
#111682 = CARTESIAN_POINT ( 'NONE',  ( 21.05000000000000071, -11.64999999998883595, -69.90000000000004832 ) ) ;
#111683 = CIRCLE ( 'NONE', #144987, 12.87500000000000178 ) ;
#111684 = VERTEX_POINT ( 'NONE', #93195 ) ;
#111687 = ORIENTED_EDGE ( 'NONE', *, *, #239585, .F. ) ;
#111686 = CARTESIAN_POINT ( 'NONE',  ( -16.87036670365548474, 9.989418819301645769, -20.97956011730205006 ) ) ;
#111685 = CARTESIAN_POINT ( 'NONE',  ( -18.59999999999999787, -10.84999999999999076, 32.89999999999999858 ) ) ;
#111688 = CARTESIAN_POINT ( 'NONE',  ( -21.05000000000000071, 0.09779029131994770863, -27.24218538952388613 ) ) ;
#111689 = AXIS2_PLACEMENT_3D ( 'NONE', #255704, #34174, #171130 ) ;
#111690 = ORIENTED_EDGE ( 'NONE', *, *, #137107, .F. ) ;
#111691 = VECTOR ( 'NONE', #112454, 1000.000000000000114 ) ;
#111692 = VERTEX_POINT ( 'NONE', #148373 ) ;
#111693 = VECTOR ( 'NONE', #52653, 1000.000000000000000 ) ;
#111694 = AXIS2_PLACEMENT_3D ( 'NONE', #84693, #67742, #147274 ) ;
#111695 = ADVANCED_FACE ( 'NONE', ( #33272 ), #220413, .F. ) ;
#111696 = DIRECTION ( 'NONE',  ( 0.000000000000000000, 0.000000000000000000, -1.000000000000000000 ) ) ;
#111697 = ORIENTED_EDGE ( 'NONE', *, *, #205331, .T. ) ;
#111699 = CIRCLE ( 'NONE', #236763, 12.87499999999999822 ) ;
#111698 = LINE ( 'NONE', #15178, #185085 ) ;
#111700 = LINE ( 'NONE', #210799, #13541 ) ;
#111701 = CARTESIAN_POINT ( 'NONE',  ( -22.48970261584618058, 64.35000000001238618, -170.0784769727418393 ) ) ;
#111702 = LINE ( 'NONE', #75169, #197546 ) ;
#111703 = DIRECTION ( 'NONE',  ( 0.000000000000000000, 0.000000000000000000, -1.000000000000000000 ) ) ;
#111704 = EDGE_LOOP ( 'NONE', ( #71299, #242854, #176066 ) ) ;
#111705 = CARTESIAN_POINT ( 'NONE',  ( -17.11825945287481332, 9.950000000011138823, -154.7500000000000284 ) ) ;
#111706 = CARTESIAN_POINT ( 'NONE',  ( -20.94999999999999929, 64.35000000001195986, -109.8069731475024753 ) ) ;
#111707 = CARTESIAN_POINT ( 'NONE',  ( 21.10320863425824811, 6.400277386470322405, -33.47497774877286503 ) ) ;
#111708 = VERTEX_POINT ( 'NONE', #47974 ) ;
#111709 = CARTESIAN_POINT ( 'NONE',  ( -22.37643362114956957, 0.09908137368138361656, 7.625789993958400181 ) ) ;
#111711 = ORIENTED_EDGE ( 'NONE', *, *, #139496, .F. ) ;
#111710 = CIRCLE ( 'NONE', #11792, 4.150000000000001243 ) ;
#111713 = CIRCLE ( 'NONE', #228255, 0.09999999999998898659 ) ;
#111712 = DIRECTION ( 'NONE',  ( -0.000000000000000000, 1.000000000000000000, -0.000000000000000000 ) ) ;
#111714 = ORIENTED_EDGE ( 'NONE', *, *, #171773, .F. ) ;
#111715 = CLOSED_SHELL ( 'NONE', ( #233123, #95937, #202520, #135911, #101707, #86553, #148733, #167086, #59882, #191811, #149768, #138124, #205431, #46625, #174183, #82501, #250160, #38493, #163363, #230972, #131071, #194549, #38180, #76720, #129065, #129649, #66964, #43278, #120560, #235760, #108391, #238642, #257314, #85477, #224906, #197222, #136556, #185392, #97600, #52904, #110647, #97662, #104191, #245431, #118848, #74332, #191844, #256533, #69644, #238099, #57439, #159997, #146677 ) ) ;
#111716 = ADVANCED_FACE ( 'NONE', ( #67545 ), #246191, .T. ) ;
#111717 = DIRECTION ( 'NONE',  ( 1.000000000000000000, 0.000000000000000000, 0.000000000000000000 ) ) ;
#111718 = FACE_OUTER_BOUND ( 'NONE', #123659, .T. ) ;
#111720 = EDGE_LOOP ( 'NONE', ( #36771, #219724, #195123, #226903, #75140 ) ) ;
#111719 = DIRECTION ( 'NONE',  ( -1.000000000000000000, 0.000000000000000000, 0.000000000000000000 ) ) ;
#111721 = CARTESIAN_POINT ( 'NONE',  ( 18.59999999999999076, 63.58402440245809828, -209.2218768284338637 ) ) ;
#111722 = ORIENTED_EDGE ( 'NONE', *, *, #90291, .T. ) ;
#111723 = DIRECTION ( 'NONE',  ( -0.000000000000000000, 1.000000000000000000, 6.982962677686266711E-15 ) ) ;
#111724 = CIRCLE ( 'NONE', #199218, 0.09999999999998900047 ) ;
#111725 = DIRECTION ( 'NONE',  ( -1.000000000000000000, 0.000000000000000000, 0.000000000000000000 ) ) ;
#111726 = AXIS2_PLACEMENT_3D ( 'NONE', #183855, #221675, #65185 ) ;
#111728 = ADVANCED_FACE ( 'NONE', ( #144494 ), #126227, .T. ) ;
#111727 = EDGE_LOOP ( 'NONE', ( #149388, #252158, #17518, #67590 ) ) ;
#111729 = DIRECTION ( 'NONE',  ( -2.342056488767301376E-15, 0.1350103645451974088, -0.9908441862701587999 ) ) ;
#111730 = DIRECTION ( 'NONE',  ( 0.000000000000000000, 0.9770955615653257320, 0.2128009952263869853 ) ) ;
#111731 = AXIS2_PLACEMENT_3D ( 'NONE', #246594, #92659, #10575 ) ;
#111732 = VERTEX_POINT ( 'NONE', #87090 ) ;
#111733 = DIRECTION ( 'NONE',  ( -1.000000000000000000, -0.000000000000000000, -0.000000000000000000 ) ) ;
#111734 = EDGE_LOOP ( 'NONE', ( #129241, #125176, #33321, #87818 ) ) ;
#111735 = CIRCLE ( 'NONE', #40846, 0.09999999999999939493 ) ;
#111736 = LINE ( 'NONE', #92165, #191787 ) ;
#111737 = CARTESIAN_POINT ( 'NONE',  ( -18.50000000000000000, -9.399999999988850163, -73.88204184817267617 ) ) ;
#111738 = CIRCLE ( 'NONE', #240750, 0.5000000000000004441 ) ;
#111741 = VERTEX_POINT ( 'NONE', #226603 ) ;
#111740 = ORIENTED_EDGE ( 'NONE', *, *, #115390, .F. ) ;
#111739 = CARTESIAN_POINT ( 'NONE',  ( -21.05000000000000071, 74.14897176987174987, -191.8691942151018850 ) ) ;
#111742 = EDGE_CURVE ( 'NONE', #246153, #155941, #37109, .T. ) ;
#111743 = PLANE ( 'NONE',  #191314 ) ;
#111744 = AXIS2_PLACEMENT_3D ( 'NONE', #214475, #133663, #191099 ) ;
#111745 = CARTESIAN_POINT ( 'NONE',  ( -22.47886152344871036, 0.03750093887284929733, -155.8500113569520238 ) ) ;
#111746 = AXIS2_PLACEMENT_3D ( 'NONE', #116357, #238859, #77202 ) ;
#111747 = DIRECTION ( 'NONE',  ( 0.000000000000000000, -1.000000000000000000, -6.982962677686266711E-15 ) ) ;
#111748 = VECTOR ( 'NONE', #124545, 1000.000000000000000 ) ;
#111750 = DIRECTION ( 'NONE',  ( 0.000000000000000000, 0.9910827722268042983, 0.1332476588733650935 ) ) ;
#111749 = DIRECTION ( 'NONE',  ( 1.000000000000000000, -7.304098846218134667E-16, -0.000000000000000000 ) ) ;
#111751 = SPHERICAL_SURFACE ( 'NONE', #136278, 0.1000000000000000056 ) ;
#111752 = CARTESIAN_POINT ( 'NONE',  ( 22.39999999999999858, 0.1000000000111554016, -92.70922040162665212 ) ) ;
#111753 = DIRECTION ( 'NONE',  ( -7.304098846218134667E-16, 1.000000000000000000, 6.982962677686266711E-15 ) ) ;
#111754 = TOROIDAL_SURFACE ( 'NONE', #28404, 0.6000000000000004219, 0.1000000000000000056 ) ;
#111755 = LINE ( 'NONE', #192576, #150827 ) ;
#111756 = ORIENTED_EDGE ( 'NONE', *, *, #3196, .F. ) ;
#111757 = ORIENTED_EDGE ( 'NONE', *, *, #133862, .F. ) ;
#111758 = EDGE_CURVE ( 'NONE', #150585, #119824, #70588, .T. ) ;
#111759 = DIRECTION ( 'NONE',  ( 1.000000000000000000, -0.000000000000000000, 0.000000000000000000 ) ) ;
#111760 = EDGE_CURVE ( 'NONE', #149556, #174107, #78757, .T. ) ;
#111762 = ORIENTED_EDGE ( 'NONE', *, *, #101390, .F. ) ;
#111761 = DIRECTION ( 'NONE',  ( 0.000000000000000000, 0.000000000000000000, 1.000000000000000000 ) ) ;
#111763 = ORIENTED_EDGE ( 'NONE', *, *, #13753, .F. ) ;
#111764 = SPHERICAL_SURFACE ( 'NONE', #97646, 0.1000000000000000056 ) ;
#111765 = ORIENTED_EDGE ( 'NONE', *, *, #128614, .T. ) ;
#111766 = CARTESIAN_POINT ( 'NONE',  ( 21.09551895715256009, 43.48418023705998792, -234.8549715607070709 ) ) ;
#111767 = ADVANCED_FACE ( 'NONE', ( #256066 ), #196154, .F. ) ;
#111768 = EDGE_CURVE ( 'NONE', #131787, #71547, #245352, .T. ) ;
#111769 = AXIS2_PLACEMENT_3D ( 'NONE', #65113, #28617, #123818 ) ;
#111770 = VERTEX_POINT ( 'NONE', #119198 ) ;
#111771 = ADVANCED_FACE ( 'NONE', ( #174069 ), #224660, .T. ) ;
#111772 = CARTESIAN_POINT ( 'NONE',  ( -16.90128866880176162, 66.04620422280885350, -82.16043130113574477 ) ) ;
#111773 = LINE ( 'NONE', #229158, #15554 ) ;
#111774 = ADVANCED_FACE ( 'NONE', ( #253548 ), #38373, .T. ) ;
#111776 = EDGE_LOOP ( 'NONE', ( #197610, #108492, #99825, #16756 ) ) ;
#111775 = ORIENTED_EDGE ( 'NONE', *, *, #113879, .F. ) ;
#111777 = ORIENTED_EDGE ( 'NONE', *, *, #25227, .T. ) ;
#111779 = EDGE_CURVE ( 'NONE', #198491, #13912, #60480, .T. ) ;
#111778 = EDGE_CURVE ( 'NONE', #221237, #215945, #228781, .T. ) ;
#111780 = ORIENTED_EDGE ( 'NONE', *, *, #139903, .F. ) ;
#111781 = EDGE_LOOP ( 'NONE', ( #85054, #188431, #83878, #180545 ) ) ;
#111782 = PLANE ( 'NONE',  #192784 ) ;
#111783 = CARTESIAN_POINT ( 'NONE',  ( 21.10642757222115407, 43.44585438861653159, -234.7606813603525779 ) ) ;
#111784 = CARTESIAN_POINT ( 'NONE',  ( -12.92414019175886786, 9.417632963117448242, -185.6489484657322464 ) ) ;
#111786 = ORIENTED_EDGE ( 'NONE', *, *, #244732, .F. ) ;
#111785 = CARTESIAN_POINT ( 'NONE',  ( -18.50000000000000000, 9.150000000011157653, -88.75000000000004263 ) ) ;
#111787 = DIRECTION ( 'NONE',  ( 1.000000000000000000, -0.000000000000000000, -0.000000000000000000 ) ) ;
#111788 = CARTESIAN_POINT ( 'NONE',  ( -18.50000000000000000, -9.499999999988849808, -75.10000000000003695 ) ) ;
#111790 = VERTEX_POINT ( 'NONE', #57909 ) ;
#111789 = CARTESIAN_POINT ( 'NONE',  ( -16.93658623642897609, 60.90006327965645028, -221.0705442474995266 ) ) ;
#111791 = CARTESIAN_POINT ( 'NONE',  ( 20.94999999999999574, -11.64999999998883595, -170.5999999999999659 ) ) ;
#111792 = ORIENTED_EDGE ( 'NONE', *, *, #119051, .F. ) ;
#111793 = CARTESIAN_POINT ( 'NONE',  ( -22.39999999999999858, 7.790779598384560245, -66.90000000000004832 ) ) ;
#111794 = ORIENTED_EDGE ( 'NONE', *, *, #152054, .T. ) ;
#111795 = LINE ( 'NONE', #33583, #122724 ) ;
#111797 = ADVANCED_FACE ( 'NONE', ( #117894 ), #197430, .F. ) ;
#111796 = CARTESIAN_POINT ( 'NONE',  ( 23.15000000000000213, -11.74999999998883737, -179.7499999999999716 ) ) ;
#111798 = ORIENTED_EDGE ( 'NONE', *, *, #24520, .F. ) ;
#111799 = AXIS2_PLACEMENT_3D ( 'NONE', #87512, #208777, #206199 ) ;
#111802 = CARTESIAN_POINT ( 'NONE',  ( -18.46907102845854354, -9.473727364752946301, -140.6760347387365471 ) ) ;
#111801 = TOROIDAL_SURFACE ( 'NONE', #207668, 2.100000000000002309, 0.1000000000000000056 ) ;
#111800 = PLANE ( 'NONE',  #44675 ) ;
#111803 = EDGE_CURVE ( 'NONE', #44449, #140474, #66280, .T. ) ;
#111804 = AXIS2_PLACEMENT_3D ( 'NONE', #237905, #21454, #197485 ) ;
#111805 = EDGE_CURVE ( 'NONE', #72719, #54282, #56604, .T. ) ;
#111806 = CARTESIAN_POINT ( 'NONE',  ( 20.94999999999999929, 42.92545512184477730, -254.1955779480491344 ) ) ;
#111807 = DIRECTION ( 'NONE',  ( 1.000000000000000000, 0.000000000000000000, 0.000000000000000000 ) ) ;
#111808 = CARTESIAN_POINT ( 'NONE',  ( -18.50000000000000355, -1.263275465206102233, -208.9018646667463770 ) ) ;
#111809 = ORIENTED_EDGE ( 'NONE', *, *, #236125, .T. ) ;
#111810 = VERTEX_POINT ( 'NONE', #99592 ) ;
#111811 = ADVANCED_FACE ( 'NONE', ( #14968 ), #97013, .T. ) ;
#111812 = DIRECTION ( 'NONE',  ( 0.000000000000000000, 0.000000000000000000, 1.000000000000000000 ) ) ;
#111813 = DIRECTION ( 'NONE',  ( 1.000000000000000000, -0.000000000000000000, -0.000000000000000000 ) ) ;
#111814 = EDGE_LOOP ( 'NONE', ( #190357, #109750, #32839, #131114 ) ) ;
#111815 = CARTESIAN_POINT ( 'NONE',  ( 20.90000000000000213, 6.258114003436814343, 11.90000000000000036 ) ) ;
#111816 = ORIENTED_EDGE ( 'NONE', *, *, #71056, .T. ) ;
#111817 = CARTESIAN_POINT ( 'NONE',  ( -21.04999999999994387, 65.19115966511134275, -29.92310748452479174 ) ) ;
#111818 = CARTESIAN_POINT ( 'NONE',  ( -22.94999999999999929, 0.000000000000000000, 0.000000000000000000 ) ) ;
#111819 = ADVANCED_FACE ( 'NONE', ( #219555 ), #96592, .T. ) ;
#111820 = DIRECTION ( 'NONE',  ( 0.000000000000000000, 0.2617529984165180013, 0.9651348961777117541 ) ) ;
#111821 = AXIS2_PLACEMENT_3D ( 'NONE', #197488, #43569, #99654 ) ;
#111822 = ORIENTED_EDGE ( 'NONE', *, *, #184120, .F. ) ;
#111823 = AXIS2_PLACEMENT_3D ( 'NONE', #211374, #133118, #213932 ) ;
#111824 = PLANE ( 'NONE',  #44442 ) ;
#111825 = ORIENTED_EDGE ( 'NONE', *, *, #211593, .T. ) ;
#111826 = CIRCLE ( 'NONE', #145116, 11.90000000000000746 ) ;
#111827 = ORIENTED_EDGE ( 'NONE', *, *, #124742, .T. ) ;
#111828 = ORIENTED_EDGE ( 'NONE', *, *, #222090, .T. ) ;
#111829 = DIRECTION ( 'NONE',  ( 4.026293107431335996E-15, -0.8700118002898359348, 0.4930308989875165082 ) ) ;
#111830 = CARTESIAN_POINT ( 'NONE',  ( 14.77516762759921853, 66.56332574816869396, -54.34624555352518627 ) ) ;
#111831 = CARTESIAN_POINT ( 'NONE',  ( -16.27683809663751191, 9.350000000011132073, -46.04999999999999716 ) ) ;
#111832 = DIRECTION ( 'NONE',  ( 0.000000000000000000, 2.664535259100430523E-15, -1.000000000000000000 ) ) ;
#111833 = CARTESIAN_POINT ( 'NONE',  ( -16.86733706339143524, 9.965990529639665141, -20.90311530199869949 ) ) ;
#111834 =( BOUNDED_CURVE ( )  B_SPLINE_CURVE ( 3, ( #146040, #66523, #207329, #28721 ),
 .UNSPECIFIED., .F., .F. ) 
 B_SPLINE_CURVE_WITH_KNOTS ( ( 4, 4 ),
 ( 1.570796326794885012, 3.141592653589794448 ),
 .UNSPECIFIED. ) 
 CURVE ( )  GEOMETRIC_REPRESENTATION_ITEM ( )  RATIONAL_B_SPLINE_CURVE ( ( 1.000000000000000000, 0.8047378541243619399, 0.8047378541243619399, 1.000000000000000000 ) ) 
 REPRESENTATION_ITEM ( '' )  );
#111836 = CARTESIAN_POINT ( 'NONE',  ( -21.07094088545368749, 0.09889370256337755294, -161.1798327780828402 ) ) ;
#111835 = CARTESIAN_POINT ( 'NONE',  ( -21.07094088545303379, 10.02599695582151007, -228.1148069861733063 ) ) ;
#111838 = ORIENTED_EDGE ( 'NONE', *, *, #62711, .F. ) ;
#111837 = DIRECTION ( 'NONE',  ( 1.000000000000000000, -0.000000000000000000, 0.000000000000000000 ) ) ;
#111839 = CARTESIAN_POINT ( 'NONE',  ( 23.14999999999999858, 72.10000000001141984, -36.02310748452435263 ) ) ;
#111840 = ORIENTED_EDGE ( 'NONE', *, *, #9375, .F. ) ;
#111841 = CARTESIAN_POINT ( 'NONE',  ( -13.88555196119803625, 9.457431528860070102, -148.9999169378996555 ) ) ;
#111842 = ORIENTED_EDGE ( 'NONE', *, *, #6491, .T. ) ;
#111843 = ORIENTED_EDGE ( 'NONE', *, *, #213764, .F. ) ;
#111844 = CARTESIAN_POINT ( 'NONE',  ( -23.15000000000000213, 70.05000000001177796, -79.82880978955917328 ) ) ;
#111845 = CARTESIAN_POINT ( 'NONE',  ( -21.14999999999999858, 6.540656951712399803, -134.0000000000000284 ) ) ;
#111846 = FACE_OUTER_BOUND ( 'NONE', #151270, .T. ) ;
#111847 = VECTOR ( 'NONE', #62678, 1000.000000000000000 ) ;
#111848 = VECTOR ( 'NONE', #81119, 1000.000000000000000 ) ;
#111849 = DIRECTION ( 'NONE',  ( 0.000000000000000000, 0.9651348961777157509, -0.2617529984165031243 ) ) ;
#111850 = VERTEX_POINT ( 'NONE', #65625 ) ;
#111851 = VERTEX_POINT ( 'NONE', #141320 ) ;
#111852 = DIRECTION ( 'NONE',  ( 2.952720810173289112E-16, -1.000000000000000000, 0.000000000000000000 ) ) ;
#111853 = VERTEX_POINT ( 'NONE', #21400 ) ;
#111854 = FACE_OUTER_BOUND ( 'NONE', #128765, .T. ) ;
#111855 = CARTESIAN_POINT ( 'NONE',  ( 23.14999999999999858, 1.115600667400684642E-11, -146.8750000000000000 ) ) ;
#111856 = ORIENTED_EDGE ( 'NONE', *, *, #90668, .T. ) ;
#111858 = DIRECTION ( 'NONE',  ( -1.000000000000000000, -0.000000000000000000, -0.000000000000000000 ) ) ;
#111857 = VECTOR ( 'NONE', #246604, 1000.000000000000000 ) ;
#111859 = CARTESIAN_POINT ( 'NONE',  ( 20.85000000000000142, 76.00000000001190870, -103.0231074845243029 ) ) ;
#111860 = DIRECTION ( 'NONE',  ( 1.000000000000000000, 0.000000000000000000, 0.000000000000000000 ) ) ;
#111861 = LINE ( 'NONE', #133971, #242459 ) ;
#111862 = ORIENTED_EDGE ( 'NONE', *, *, #232993, .F. ) ;
#111863 = CARTESIAN_POINT ( 'NONE',  ( 20.85000000000000142, 7.021664781900089913, -37.33356540189728889 ) ) ;
#111864 = FACE_OUTER_BOUND ( 'NONE', #211595, .T. ) ;
#111865 = CYLINDRICAL_SURFACE ( 'NONE', #70983, 0.1000000000000028644 ) ;
#111866 = DIRECTION ( 'NONE',  ( -1.000000000000000000, 3.265361837132813093E-16, 2.280189983783949500E-30 ) ) ;
#111867 = EDGE_CURVE ( 'NONE', #185056, #146767, #230261, .T. ) ;
#111868 = DIRECTION ( 'NONE',  ( -0.000000000000000000, 1.000000000000000000, 1.445602896647339410E-16 ) ) ;
#111869 = AXIS2_PLACEMENT_3D ( 'NONE', #212100, #178112, #55534 ) ;
#111870 = DIRECTION ( 'NONE',  ( 0.7071359030027419834, 0.000000000000000000, 0.7070776581709371511 ) ) ;
#111872 = MANIFOLD_SOLID_BREP ( 'Stock-MAS-200-1', #249288 ) ;
#111871 = AXIS2_PLACEMENT_3D ( 'NONE', #155176, #232127, #52174 ) ;
#111873 = ADVANCED_FACE ( 'NONE', ( #23963 ), #99556, .T. ) ;
#111874 = AXIS2_PLACEMENT_3D ( 'NONE', #242063, #102519, #42585 ) ;
#111875 = EDGE_LOOP ( 'NONE', ( #65519, #192418, #109170, #3298 ) ) ;
#111876 = AXIS2_PLACEMENT_3D ( 'NONE', #236009, #196882, #157811 ) ;
#111877 = EDGE_CURVE ( 'NONE', #135886, #23667, #124511, .T. ) ;
#111878 = CARTESIAN_POINT ( 'NONE',  ( 21.05000000000000426, 0.06570161033324604938, -161.2416839426679758 ) ) ;
#111879 = EDGE_CURVE ( 'NONE', #186245, #27421, #137184, .T. ) ;
#111880 = ORIENTED_EDGE ( 'NONE', *, *, #247256, .F. ) ;
#111881 = DIRECTION ( 'NONE',  ( 0.000000000000000000, -1.000000000000000000, -7.272083257015735086E-15 ) ) ;
#111882 = LINE ( 'NONE', #233127, #91932 ) ;
#111883 = CARTESIAN_POINT ( 'NONE',  ( 20.85000000000000142, 77.83585931145600512, -158.5186683157258187 ) ) ;
#111884 = CARTESIAN_POINT ( 'NONE',  ( 22.39999999999999503, 11.40444339177024524, -198.6185779617709670 ) ) ;
#111885 = DIRECTION ( 'NONE',  ( 1.000000000000000000, 0.000000000000000000, 0.000000000000000000 ) ) ;
#111886 = DIRECTION ( 'NONE',  ( 0.000000000000000000, 0.000000000000000000, -1.000000000000000000 ) ) ;
#111887 = CIRCLE ( 'NONE', #149303, 0.09999999999999820144 ) ;
#111888 = VERTEX_POINT ( 'NONE', #47334 ) ;
#111889 = CYLINDRICAL_SURFACE ( 'NONE', #192507, 0.09999999999999609201 ) ;
#111890 = CARTESIAN_POINT ( 'NONE',  ( 21.05543885634738643, 67.22422895316451275, -124.3387230138096697 ) ) ;
#111891 = CARTESIAN_POINT ( 'NONE',  ( -20.64999999999999858, 76.00000000001170974, -69.52310748452431710 ) ) ;
#111892 = CARTESIAN_POINT ( 'NONE',  ( -15.75000000000000355, 62.10905854918435409, -217.1108499610990918 ) ) ;
#111893 = CIRCLE ( 'NONE', #32805, 0.1999999999999987899 ) ;
#111894 = DIRECTION ( 'NONE',  ( 1.000000000000000000, 0.000000000000000000, 0.000000000000000000 ) ) ;
#111895 = EDGE_CURVE ( 'NONE', #81634, #9164, #58048, .T. ) ;
#111896 = CIRCLE ( 'NONE', #66075, 0.5000000000000004441 ) ;
#111898 = EDGE_CURVE ( 'NONE', #257429, #132941, #248120, .T. ) ;
#111897 = CIRCLE ( 'NONE', #257557, 0.1000000000000055844 ) ;
#111900 = EDGE_LOOP ( 'NONE', ( #82502, #98740, #79312, #53699 ) ) ;
#111899 = CIRCLE ( 'NONE', #108182, 0.1000000000000055844 ) ;
#111901 = ORIENTED_EDGE ( 'NONE', *, *, #68173, .T. ) ;
#111902 = DIRECTION ( 'NONE',  ( -1.000000000000000000, -1.394253735153569469E-16, -2.602809386958778209E-16 ) ) ;
#111903 = CIRCLE ( 'NONE', #32821, 0.1000000000000028644 ) ;
#111904 = DIRECTION ( 'NONE',  ( -1.000000000000000000, 1.646408749285562691E-14, 1.149681084847720908E-28 ) ) ;
#111905 = CARTESIAN_POINT ( 'NONE',  ( -23.25000000000000000, 0.000000000000000000, -33.50000000000000000 ) ) ;
#111906 = LINE ( 'NONE', #191463, #213840 ) ;
#111907 = CARTESIAN_POINT ( 'NONE',  ( -16.86422026484316916, 44.06525935397618099, -235.3079849271810531 ) ) ;
#111908 = TOROIDAL_SURFACE ( 'NONE', #86906, 7.800000000000000711, 0.1000000000000000056 ) ;
#111909 = VERTEX_POINT ( 'NONE', #249422 ) ;
#111910 = CARTESIAN_POINT ( 'NONE',  ( 21.05000000000000071, 69.45934304831071415, -102.9231074845243512 ) ) ;
#111911 = CARTESIAN_POINT ( 'NONE',  ( -20.54999999999999716, -8.999999999988846255, -177.3939691226524076 ) ) ;
#111912 = VERTEX_POINT ( 'NONE', #8243 ) ;
#111913 = CARTESIAN_POINT ( 'NONE',  ( -23.25000000000000000, 85.00000000001261924, -193.6291383618718385 ) ) ;
#111914 = ADVANCED_FACE ( 'NONE', ( #68208 ), #126898, .T. ) ;
#111915 = PRODUCT_DEFINITION_SHAPE ( 'NONE', 'NONE',  #42271 ) ;
#111916 = EDGE_CURVE ( 'NONE', #249154, #1901, #237149, .T. ) ;
#111917 = VECTOR ( 'NONE', #129678, 1000.000000000000000 ) ;
#111918 = AXIS2_PLACEMENT_3D ( 'NONE', #210043, #28871, #33998 ) ;
#111919 = VERTEX_POINT ( 'NONE', #87749 ) ;
#111920 = VERTEX_POINT ( 'NONE', #30380 ) ;
#111921 = VERTEX_POINT ( 'NONE', #69512 ) ;
#111922 = CARTESIAN_POINT ( 'NONE',  ( -20.65000000000000568, 70.35000000001160458, -60.27310748452436684 ) ) ;
#111923 = DIRECTION ( 'NONE',  ( 0.000000000000000000, 0.000000000000000000, -1.000000000000000000 ) ) ;
#111924 = DIRECTION ( 'NONE',  ( 0.000000000000000000, 0.000000000000000000, -1.000000000000000000 ) ) ;
#111925 = EDGE_CURVE ( 'NONE', #58429, #61278, #87100, .T. ) ;
#111926 = CARTESIAN_POINT ( 'NONE',  ( 21.07928932188134397, 75.90110485435802445, -176.3516241409176644 ) ) ;
#111928 = VECTOR ( 'NONE', #18819, 1000.000000000000000 ) ;
#111927 = DIRECTION ( 'NONE',  ( -1.000000000000000000, 0.000000000000000000, 0.000000000000000000 ) ) ;
#111929 = DIRECTION ( 'NONE',  ( -2.940209281316621016E-16, -1.000000000000000000, -7.056502275159890832E-15 ) ) ;
#111930 = CARTESIAN_POINT ( 'NONE',  ( 20.85000000000000142, 76.00000000001142553, -36.02310748452432421 ) ) ;
#111931 = EDGE_CURVE ( 'NONE', #116410, #63242, #124723, .T. ) ;
#111932 = CIRCLE ( 'NONE', #57737, 2.599999999999998312 ) ;
#111934 = DIRECTION ( 'NONE',  ( 0.000000000000000000, 0.000000000000000000, 1.000000000000000000 ) ) ;
#111933 = CARTESIAN_POINT ( 'NONE',  ( 20.95420533658165141, 65.45413552525231182, -95.45560146383114386 ) ) ;
#111935 = CARTESIAN_POINT ( 'NONE',  ( 18.60000000000000142, -9.321008403350125704, -107.7359382490779325 ) ) ;
#111936 = CIRCLE ( 'NONE', #107624, 0.1000000000000028644 ) ;
#111937 = CARTESIAN_POINT ( 'NONE',  ( 21.09787244211736379, 22.06134468089375744, -231.7765419340705648 ) ) ;
#111938 = DIRECTION ( 'NONE',  ( 0.000000000000000000, -1.000000000000000000, 6.938893903907228378E-14 ) ) ;
#111939 = CARTESIAN_POINT ( 'NONE',  ( 21.14999999999999858, 69.45934304831041572, -69.42310748452437963 ) ) ;
#111940 = ORIENTED_EDGE ( 'NONE', *, *, #83353, .T. ) ;
#111941 = DIRECTION ( 'NONE',  ( -0.000000000000000000, 0.1332476588733642331, -0.9910827722268044093 ) ) ;
#111942 = LINE ( 'NONE', #149793, #145402 ) ;
#111943 = CARTESIAN_POINT ( 'NONE',  ( -21.55000000000000426, 7.750000000000000000, -12.34999999999999964 ) ) ;
#111944 = AXIS2_PLACEMENT_3D ( 'NONE', #106320, #125897, #108907 ) ;
#111945 = EDGE_CURVE ( 'NONE', #65006, #139626, #45622, .T. ) ;
#111946 = CARTESIAN_POINT ( 'NONE',  ( 20.85000000000000142, 69.15387683765929694, -99.28538121767448388 ) ) ;
#111947 = FACE_OUTER_BOUND ( 'NONE', #215287, .T. ) ;
#111948 = CARTESIAN_POINT ( 'NONE',  ( 21.04999999999998650, 6.650000000011155876, -45.75000000000000711 ) ) ;
#111949 = EDGE_CURVE ( 'NONE', #166644, #60084, #153812, .T. ) ;
#111950 = VERTEX_POINT ( 'NONE', #228574 ) ;
#111951 = EDGE_LOOP ( 'NONE', ( #4228, #36278, #206714, #67666 ) ) ;
#111952 = VECTOR ( 'NONE', #102876, 1000.000000000000000 ) ;
#111953 = TOROIDAL_SURFACE ( 'NONE', #32866, 0.2000000000000000111, 0.1000000000000000056 ) ;
#111954 = DIRECTION ( 'NONE',  ( 1.000000000000000000, 0.000000000000000000, 0.000000000000000000 ) ) ;
#111955 = EDGE_CURVE ( 'NONE', #131621, #91807, #108614, .T. ) ;
#111956 = ORIENTED_EDGE ( 'NONE', *, *, #49713, .F. ) ;
#111957 = DIRECTION ( 'NONE',  ( -0.9880948137434723000, -0.06289798482097130883, 0.1404011487086683774 ) ) ;
#111958 = CYLINDRICAL_SURFACE ( 'NONE', #76506, 0.09999999999999939493 ) ;
#111959 = ORIENTED_EDGE ( 'NONE', *, *, #82807, .T. ) ;
#111960 = CARTESIAN_POINT ( 'NONE',  ( 23.14999999999999858, 71.00000000001158185, -57.11784146561126363 ) ) ;
#111961 = EDGE_CURVE ( 'NONE', #116304, #226817, #109884, .T. ) ;
#111962 = VERTEX_POINT ( 'NONE', #211576 ) ;
#111963 = FACE_OUTER_BOUND ( 'NONE', #201584, .T. ) ;
#111964 = DIRECTION ( 'NONE',  ( -1.000000000000000000, 0.000000000000000000, 0.000000000000000000 ) ) ;
#111966 = CARTESIAN_POINT ( 'NONE',  ( -22.39999999999999858, 76.10085836911075319, -114.7726746080137019 ) ) ;
#111965 = AXIS2_PLACEMENT_3D ( 'NONE', #255248, #76660, #177080 ) ;
#111967 = CARTESIAN_POINT ( 'NONE',  ( 20.94999999999999929, 6.703231349641842307, -231.7785101893094577 ) ) ;
#111968 = CARTESIAN_POINT ( 'NONE',  ( -23.15000000000000213, 71.75000000001180922, -81.77310748452433131 ) ) ;
#111969 = CARTESIAN_POINT ( 'NONE',  ( -21.00023020733502932, 1.115542391533913547E-11, -60.60913075473169442 ) ) ;
#111970 = CARTESIAN_POINT ( 'NONE',  ( 18.59999999999999432, 85.48068669529105534, -129.5819923157664562 ) ) ;
#111971 = FACE_OUTER_BOUND ( 'NONE', #248916, .T. ) ;
#111973 = EDGE_LOOP ( 'NONE', ( #186699, #170784, #36082, #113646 ) ) ;
#111972 = CYLINDRICAL_SURFACE ( 'NONE', #244158, 0.09999999999999939493 ) ;
#111975 = DIRECTION ( 'NONE',  ( 0.000000000000000000, 0.000000000000000000, -1.000000000000000000 ) ) ;
#111974 = LINE ( 'NONE', #169407, #157835 ) ;
#111976 = ORIENTED_EDGE ( 'NONE', *, *, #112928, .T. ) ;
#111978 = VERTEX_POINT ( 'NONE', #149046 ) ;
#111977 = FILL_AREA_STYLE ('',( #191528 ) ) ;
#111979 = ORIENTED_EDGE ( 'NONE', *, *, #171225, .T. ) ;
#111980 = DIRECTION ( 'NONE',  ( 1.000000000000000000, -0.000000000000000000, -0.000000000000000000 ) ) ;
#111981 = FACE_OUTER_BOUND ( 'NONE', #99463, .T. ) ;
#111982 = DIRECTION ( 'NONE',  ( 0.000000000000000000, 0.8814952561688476074, -0.4721928772777262417 ) ) ;
#111983 = DIRECTION ( 'NONE',  ( 0.000000000000000000, 0.2128009952263403282, -0.9770955615653358350 ) ) ;
#111984 = CARTESIAN_POINT ( 'NONE',  ( -15.75000000000000355, 66.15000000001204228, -119.7731074845243739 ) ) ;
#111985 = DIRECTION ( 'NONE',  ( 0.000000000000000000, 0.000000000000000000, 1.000000000000000000 ) ) ;
#111986 = CARTESIAN_POINT ( 'NONE',  ( 21.00000000000000000, 66.25000000001253397, -182.2731074845244450 ) ) ;
#111987 = DIRECTION ( 'NONE',  ( 1.000000000000000000, -3.265361837132813093E-16, -2.280189983783949500E-30 ) ) ;
#111988 = AXIS2_PLACEMENT_3D ( 'NONE', #26285, #86217, #114802 ) ;
#111989 = ORIENTED_EDGE ( 'NONE', *, *, #195657, .F. ) ;
#111990 = ORIENTED_EDGE ( 'NONE', *, *, #239559, .F. ) ;
#111991 = AXIS2_PLACEMENT_3D ( 'NONE', #169570, #89969, #203516 ) ;
#111992 = CARTESIAN_POINT ( 'NONE',  ( -21.45000000000000284, 68.29142135624960019, -157.6731074845243938 ) ) ;
#111993 = TOROIDAL_SURFACE ( 'NONE', #103577, 6.258578643762700899, 0.1000000000000000056 ) ;
#111994 = AXIS2_PLACEMENT_3D ( 'NONE', #205418, #247114, #106309 ) ;
#111995 = ADVANCED_FACE ( 'NONE', ( #150326 ), #179102, .F. ) ;
#111996 = ORIENTED_EDGE ( 'NONE', *, *, #56733, .F. ) ;
#111997 = DIRECTION ( 'NONE',  ( 1.000000000000000000, -0.000000000000000000, 0.000000000000000000 ) ) ;
#111998 = ORIENTED_EDGE ( 'NONE', *, *, #216028, .T. ) ;
#111999 = CARTESIAN_POINT ( 'NONE',  ( 22.49231231312462853, 11.64998490368843953, -33.43894711239862261 ) ) ;
#112000 = AXIS2_PLACEMENT_3D ( 'NONE', #149073, #210324, #207766 ) ;
#112001 = PLANE ( 'NONE',  #159304 ) ;
#112002 = CARTESIAN_POINT ( 'NONE',  ( -22.48479450179659977, -2.433215998327764140, -189.6068383706822260 ) ) ;
#112003 = EDGE_CURVE ( 'NONE', #227104, #190290, #112445, .T. ) ;
#112004 = CARTESIAN_POINT ( 'NONE',  ( -21.05000000000000071, 1.658775325997247752, -230.6916041481598540 ) ) ;
#112005 = DIRECTION ( 'NONE',  ( 0.000000000000000000, -0.000000000000000000, -1.000000000000000000 ) ) ;
#112006 = EDGE_LOOP ( 'NONE', ( #238034, #221388, #245469, #136768 ) ) ;
#112007 = FACE_OUTER_BOUND ( 'NONE', #210139, .T. ) ;
#112008 = DIRECTION ( 'NONE',  ( -1.000000000000000000, 0.000000000000000000, -0.000000000000000000 ) ) ;
#112009 = ADVANCED_FACE ( 'NONE', ( #172496 ), #251973, .T. ) ;
#112011 = ADVANCED_FACE ( 'NONE', ( #186888 ), #83161, .F. ) ;
#112010 = CIRCLE ( 'NONE', #232635, 0.1000000000000028644 ) ;
#112012 = CARTESIAN_POINT ( 'NONE',  ( -20.64999999999999858, 1.115600667400684642E-11, -67.00000000000000000 ) ) ;
#112014 = AXIS2_PLACEMENT_3D ( 'NONE', #104232, #108112, #126383 ) ;
#112013 = DIRECTION ( 'NONE',  ( 1.000000000000000000, 0.000000000000000000, 0.000000000000000000 ) ) ;
#112015 = CARTESIAN_POINT ( 'NONE',  ( -23.25000000000000355, 40.29670989715187090, -235.0462836312595130 ) ) ;
#112016 = ORIENTED_EDGE ( 'NONE', *, *, #145991, .F. ) ;
#112018 = CARTESIAN_POINT ( 'NONE',  ( -18.59999999999999787, 85.48068669529035901, -29.08199231576641353 ) ) ;
#112017 = CARTESIAN_POINT ( 'NONE',  ( -16.91049119928363353, 60.93105485803026511, -221.0723421939750324 ) ) ;
#112019 = ORIENTED_EDGE ( 'NONE', *, *, #20362, .F. ) ;
#112022 = EDGE_LOOP ( 'NONE', ( #15534, #135239, #254019, #30129 ) ) ;
#112021 = CARTESIAN_POINT ( 'NONE',  ( 21.05000000000000071, 11.36448785225375424, -246.7787679937655980 ) ) ;
#112020 = DIRECTION ( 'NONE',  ( 0.000000000000000000, 0.2128009952263403282, -0.9770955615653358350 ) ) ;
#112023 = AXIS2_PLACEMENT_3D ( 'NONE', #187176, #151906, #52761 ) ;
#112024 = DIRECTION ( 'NONE',  ( 0.000000000000000000, 0.000000000000000000, -1.000000000000000000 ) ) ;
#112025 = DIRECTION ( 'NONE',  ( -0.000000000000000000, -0.2617529984165031243, -0.9651348961777157509 ) ) ;
#112026 = ORIENTED_EDGE ( 'NONE', *, *, #27624, .T. ) ;
#112027 = CARTESIAN_POINT ( 'NONE',  ( -18.59999999999999787, 66.65000000001205649, -124.1731074845243654 ) ) ;
#112028 = EDGE_CURVE ( 'NONE', #81962, #238821, #229847, .T. ) ;
#112029 = DIRECTION ( 'NONE',  ( -4.632305147810306538E-15, 0.1335171055202867274, -0.9910465087640865089 ) ) ;
#112030 = DIRECTION ( 'NONE',  ( 0.000000000000000000, -1.000000000000000000, 0.000000000000000000 ) ) ;
#112032 = ORIENTED_EDGE ( 'NONE', *, *, #135238, .F. ) ;
#112031 = DIRECTION ( 'NONE',  ( 1.000000000000000000, -0.000000000000000000, -0.000000000000000000 ) ) ;
#112033 = VERTEX_POINT ( 'NONE', #90319 ) ;
#112034 = FACE_OUTER_BOUND ( 'NONE', #156538, .T. ) ;
#112035 = CARTESIAN_POINT ( 'NONE',  ( 18.39999999999999858, -9.499999999988844479, -74.03206939669972542 ) ) ;
#112036 = DIRECTION ( 'NONE',  ( 0.000000000000000000, 0.000000000000000000, -1.000000000000000000 ) ) ;
#112037 = CIRCLE ( 'NONE', #145324, 4.150000000000009237 ) ;
#112038 = VECTOR ( 'NONE', #178684, 1000.000000000000000 ) ;
#112039 = CARTESIAN_POINT ( 'NONE',  ( 21.05000000000000071, 79.13126459505528487, -235.8705213229730191 ) ) ;
#112040 = ORIENTED_EDGE ( 'NONE', *, *, #216492, .F. ) ;
#112041 = DIRECTION ( 'NONE',  ( 1.000000000000000000, 0.000000000000000000, 0.000000000000000000 ) ) ;
#112042 = EDGE_CURVE ( 'NONE', #159653, #29906, #169922, .T. ) ;
#112043 = DIRECTION ( 'NONE',  ( -0.000000000000000000, 1.000000000000000000, -0.000000000000000000 ) ) ;
#112044 = DIRECTION ( 'NONE',  ( 2.827886303505249259E-16, 0.8103668758649578141, -0.5859227990963212784 ) ) ;
#112045 = EDGE_CURVE ( 'NONE', #38363, #49384, #87361, .T. ) ;
#112046 = VECTOR ( 'NONE', #65605, 1000.000000000000000 ) ;
#112047 = ORIENTED_EDGE ( 'NONE', *, *, #255705, .T. ) ;
#112048 = DIRECTION ( 'NONE',  ( -1.000000000000000000, -0.000000000000000000, 0.000000000000000000 ) ) ;
#112049 = PLANE ( 'NONE',  #130519 ) ;
#112051 = EDGE_CURVE ( 'NONE', #33915, #228115, #4092, .T. ) ;
#112050 = ORIENTED_EDGE ( 'NONE', *, *, #97199, .T. ) ;
#112053 = VECTOR ( 'NONE', #246528, 1000.000000000000000 ) ;
#112052 = CARTESIAN_POINT ( 'NONE',  ( -18.59999999999999787, 74.83729825007360148, -61.42310748452432989 ) ) ;
#112054 = CYLINDRICAL_SURFACE ( 'NONE', #39774, 0.09999999999999939493 ) ;
#112055 = ORIENTED_EDGE ( 'NONE', *, *, #4249, .T. ) ;
#112056 = ORIENTED_EDGE ( 'NONE', *, *, #60257, .T. ) ;
#112057 = VECTOR ( 'NONE', #22786, 1000.000000000000000 ) ;
#112058 = DIRECTION ( 'NONE',  ( 0.000000000000000000, 0.000000000000000000, 1.000000000000000000 ) ) ;
#112059 = ORIENTED_EDGE ( 'NONE', *, *, #28504, .T. ) ;
#112061 = ORIENTED_EDGE ( 'NONE', *, *, #14309, .F. ) ;
#112060 = LINE ( 'NONE', #214988, #142714 ) ;
#112062 = ORIENTED_EDGE ( 'NONE', *, *, #187011, .T. ) ;
#112063 = AXIS2_PLACEMENT_3D ( 'NONE', #178642, #59920, #20846 ) ;
#112067 = EDGE_CURVE ( 'NONE', #117549, #21472, #57113, .T. ) ;
#112066 = ORIENTED_EDGE ( 'NONE', *, *, #172255, .T. ) ;
#112065 = ORIENTED_EDGE ( 'NONE', *, *, #150400, .T. ) ;
#112064 = CARTESIAN_POINT ( 'NONE',  ( 18.49999999999999289, 6.846123162363745074, -137.7377262668498759 ) ) ;
#112068 = DIRECTION ( 'NONE',  ( 0.000000000000000000, -0.000000000000000000, -1.000000000000000000 ) ) ;
#112070 = ORIENTED_EDGE ( 'NONE', *, *, #99079, .F. ) ;
#112069 = VECTOR ( 'NONE', #70286, 1000.000000000000000 ) ;
#112071 = DIRECTION ( 'NONE',  ( 0.000000000000000000, 0.000000000000000000, -1.000000000000000000 ) ) ;
#112072 = CYLINDRICAL_SURFACE ( 'NONE', #161669, 0.09999999999999543976 ) ;
#112073 = CARTESIAN_POINT ( 'NONE',  ( -20.94999999999999929, 14.77103648604101060, -236.4083752604501001 ) ) ;
#112074 = AXIS2_PLACEMENT_3D ( 'NONE', #29757, #32318, #72730 ) ;
#112075 = CARTESIAN_POINT ( 'NONE',  ( 18.60000000000000142, 85.32100840337318459, -95.78716923544635620 ) ) ;
#112076 = CARTESIAN_POINT ( 'NONE',  ( 23.24999999999999645, 44.59642007000408626, -236.3278401793003809 ) ) ;
#112078 = EDGE_LOOP ( 'NONE', ( #70769, #39690, #86734, #21022, #134422, #50594 ) ) ;
#112077 = CIRCLE ( 'NONE', #41356, 0.1999999999999987899 ) ;
#112079 = TOROIDAL_SURFACE ( 'NONE', #170368, 0.2000000000000000111, 0.1000000000000000056 ) ;
#112080 = ORIENTED_EDGE ( 'NONE', *, *, #206924, .F. ) ;
#112081 = VECTOR ( 'NONE', #152547, 1000.000000000000000 ) ;
#112082 = ORIENTED_EDGE ( 'NONE', *, *, #94487, .F. ) ;
#112083 = EDGE_CURVE ( 'NONE', #2625, #126778, #162327, .T. ) ;
#112084 = CARTESIAN_POINT ( 'NONE',  ( -23.15000000000000213, 1.115649653272650466E-11, -204.9999999999999716 ) ) ;
#112086 = VERTEX_POINT ( 'NONE', #78463 ) ;
#112085 = DIRECTION ( 'NONE',  ( 3.469446951953728416E-14, -0.8660254037844309360, 0.5000000000000134337 ) ) ;
#112087 = SPHERICAL_SURFACE ( 'NONE', #146578, 0.1000000000000000056 ) ;
#112089 = ORIENTED_EDGE ( 'NONE', *, *, #193794, .F. ) ;
#112088 = CARTESIAN_POINT ( 'NONE',  ( 21.05000000000000071, 76.00000000001165290, -69.52310748452431710 ) ) ;
#112090 = CIRCLE ( 'NONE', #241273, 0.09999999999999810429 ) ;
#112091 = ORIENTED_EDGE ( 'NONE', *, *, #137390, .T. ) ;
#112092 = LINE ( 'NONE', #35144, #58432 ) ;
#112093 = EDGE_CURVE ( 'NONE', #34727, #93310, #253249, .T. ) ;
#112094 = EDGE_CURVE ( 'NONE', #251500, #238447, #79736, .T. ) ;
#112095 = B_SPLINE_CURVE_WITH_KNOTS ( 'NONE', 3,
 ( #132315, #94466, #232725, #153204, #256058, #54061, #73662, #155769 ),
 .UNSPECIFIED., .F., .F.,
 ( 4, 2, 2, 4 ),
 ( 0.000000000000000000, 9.550056980123548204E-05, 0.0001910011396024709641, 0.0003820022792049855131 ),
 .UNSPECIFIED. ) ;
#112096 = ORIENTED_EDGE ( 'NONE', *, *, #248543, .F. ) ;
#112097 = CARTESIAN_POINT ( 'NONE',  ( -16.87998658237742333, 9.950000000011138823, -180.3636395677385167 ) ) ;
#112098 = DIRECTION ( 'NONE',  ( 0.000000000000000000, 0.2128009952263485993, -0.9770955615653341697 ) ) ;
#112099 = VECTOR ( 'NONE', #37834, 1000.000000000000114 ) ;
#112100 = EDGE_CURVE ( 'NONE', #23864, #90327, #215416, .T. ) ;
#112102 = ORIENTED_EDGE ( 'NONE', *, *, #62005, .F. ) ;
#112101 = ORIENTED_EDGE ( 'NONE', *, *, #163982, .F. ) ;
#112103 = EDGE_LOOP ( 'NONE', ( #221699, #25554, #97669, #7299 ) ) ;
#112105 = EDGE_CURVE ( 'NONE', #256577, #245252, #220583, .T. ) ;
#112104 = CARTESIAN_POINT ( 'NONE',  ( 23.14999999999998437, 41.46275801244657799, -260.2743004338703940 ) ) ;
#112106 = EDGE_LOOP ( 'NONE', ( #183649, #253325, #57554, #162465 ) ) ;
#112107 = ORIENTED_EDGE ( 'NONE', *, *, #185816, .F. ) ;
#112108 = CARTESIAN_POINT ( 'NONE',  ( -23.25000000000000355, 11.75000000001113953, -87.85000000000003695 ) ) ;
#112110 = EDGE_LOOP ( 'NONE', ( #118187, #130655, #80593, #211874 ) ) ;
#112109 = CARTESIAN_POINT ( 'NONE',  ( -20.54999999999999716, 2.000000000011154189, -154.2753780772379173 ) ) ;
#112111 = DIRECTION ( 'NONE',  ( 2.940209281316621016E-16, 1.000000000000000000, 7.056502275159890832E-15 ) ) ;
#112112 = ADVANCED_FACE ( 'NONE', ( #217962 ), #170754, .F. ) ;
#112114 = CARTESIAN_POINT ( 'NONE',  ( -20.85000000000000142, 64.35000000001171827, -69.52310748452438816 ) ) ;
#112113 = DIRECTION ( 'NONE',  ( 1.000000000000000000, 7.304098846218135653E-16, 5.100424963727256530E-30 ) ) ;
#112115 = DIRECTION ( 'NONE',  ( -0.000000000000000000, -0.000000000000000000, -1.000000000000000000 ) ) ;
#112116 = DIRECTION ( 'NONE',  ( 1.000000000000000000, 0.000000000000000000, 0.000000000000000000 ) ) ;
#112117 = ORIENTED_EDGE ( 'NONE', *, *, #158015, .T. ) ;
#112118 = CIRCLE ( 'NONE', #245384, 0.1000000000000002554 ) ;
#112119 = AXIS2_PLACEMENT_3D ( 'NONE', #255292, #79251, #136668 ) ;
#112120 = ORIENTED_EDGE ( 'NONE', *, *, #238980, .T. ) ;
#112121 = CARTESIAN_POINT ( 'NONE',  ( 18.36493879433201570, 85.50000080620250742, -96.10095882417341784 ) ) ;
#112123 = EDGE_CURVE ( 'NONE', #170589, #169023, #133322, .T. ) ;
#112122 = DIRECTION ( 'NONE',  ( -0.000000000000000000, 1.265107689135680095E-16, -1.000000000000000000 ) ) ;
#112124 = CIRCLE ( 'NONE', #182864, 0.4000000000000045186 ) ;
#112125 = VERTEX_POINT ( 'NONE', #17242 ) ;
#112126 = EDGE_CURVE ( 'NONE', #226768, #67483, #249040, .T. ) ;
#112127 = EDGE_CURVE ( 'NONE', #157651, #67356, #212409, .T. ) ;
#112128 = AXIS2_PLACEMENT_3D ( 'NONE', #83864, #248116, #68206 ) ;
#112129 = CARTESIAN_POINT ( 'NONE',  ( -16.93860193097147970, 51.64699553454050829, -231.8866301305883439 ) ) ;
#112130 = DIRECTION ( 'NONE',  ( 1.000000000000000000, 0.000000000000000000, 0.000000000000000000 ) ) ;
#112131 = ORIENTED_EDGE ( 'NONE', *, *, #19986, .F. ) ;
#112132 = EDGE_LOOP ( 'NONE', ( #179046, #58104, #78346, #192160, #188541 ) ) ;
#112133 = EDGE_CURVE ( 'NONE', #154304, #76954, #153996, .T. ) ;
#112134 = DIRECTION ( 'NONE',  ( 0.000000000000000000, 0.08413937888704771384, -0.9964539953858891908 ) ) ;
#112135 = DIRECTION ( 'NONE',  ( 0.000000000000000000, 0.000000000000000000, 1.000000000000000000 ) ) ;
#112136 = ORIENTED_EDGE ( 'NONE', *, *, #36196, .F. ) ;
#112137 = ORIENTED_EDGE ( 'NONE', *, *, #108087, .F. ) ;
#112138 = DIRECTION ( 'NONE',  ( 0.000000000000000000, 0.000000000000000000, 1.000000000000000000 ) ) ;
#112139 = CARTESIAN_POINT ( 'NONE',  ( -16.78805706634180339, 9.948252493082335945, -154.8441532080318837 ) ) ;
#112141 = DIRECTION ( 'NONE',  ( 0.000000000000000000, -0.4088369013363297166, 0.9126074666063763718 ) ) ;
#112140 = DIRECTION ( 'NONE',  ( -1.000000000000000000, -0.000000000000000000, -0.000000000000000000 ) ) ;
#112142 = EDGE_CURVE ( 'NONE', #198388, #236713, #241435, .T. ) ;
#112144 = VECTOR ( 'NONE', #197833, 1000.000000000000000 ) ;
#112143 = CARTESIAN_POINT ( 'NONE',  ( 23.14999999999999503, 52.81534179157632991, -244.1198638051726277 ) ) ;
#112146 = EDGE_CURVE ( 'NONE', #46658, #47300, #141455, .T. ) ;
#112145 = CARTESIAN_POINT ( 'NONE',  ( 18.42555734704282600, -9.497158361925556846, -174.5398304977348971 ) ) ;
#112147 = LINE ( 'NONE', #156420, #24610 ) ;
#112148 = AXIS2_PLACEMENT_3D ( 'NONE', #101755, #256963, #78367 ) ;
#112149 = EDGE_CURVE ( 'NONE', #118789, #35199, #99919, .T. ) ;
#112151 = EDGE_LOOP ( 'NONE', ( #38132, #100080, #29308 ) ) ;
#112150 = DIRECTION ( 'NONE',  ( -0.000000000000000000, -1.000000000000000000, 0.000000000000000000 ) ) ;
#112152 = CIRCLE ( 'NONE', #37128, 0.1000000000000075273 ) ;
#112154 = ORIENTED_EDGE ( 'NONE', *, *, #171652, .F. ) ;
#112153 = ORIENTED_EDGE ( 'NONE', *, *, #49755, .T. ) ;
#112155 = EDGE_LOOP ( 'NONE', ( #80872, #27916, #218861, #40571, #6575 ) ) ;
#112156 = CARTESIAN_POINT ( 'NONE',  ( 18.52928932188133970, 65.72071067813119782, -182.1731074845244223 ) ) ;
#112157 = FACE_OUTER_BOUND ( 'NONE', #111213, .T. ) ;
#112158 = EDGE_CURVE ( 'NONE', #137948, #236913, #104432, .T. ) ;
#112160 = FACE_OUTER_BOUND ( 'NONE', #213340, .T. ) ;
#112159 = DIRECTION ( 'NONE',  ( 0.000000000000000000, 1.000000000000000000, -1.224646799147353207E-16 ) ) ;
#112161 = EDGE_CURVE ( 'NONE', #240937, #218845, #183172, .T. ) ;
#112162 = FACE_OUTER_BOUND ( 'NONE', #238729, .T. ) ;
#112163 = VERTEX_POINT ( 'NONE', #24950 ) ;
#112164 = CARTESIAN_POINT ( 'NONE',  ( 11.60000000000000142, -8.250000000000005329, 19.04142135623731136 ) ) ;
#112165 = ORIENTED_EDGE ( 'NONE', *, *, #181332, .F. ) ;
#112166 = ORIENTED_EDGE ( 'NONE', *, *, #47966, .T. ) ;
#112167 = DIRECTION ( 'NONE',  ( 0.7071067811865474617, 0.7071067811865474617, 0.000000000000000000 ) ) ;
#112168 = LINE ( 'NONE', #173465, #110021 ) ;
#112169 = CARTESIAN_POINT ( 'NONE',  ( -23.25000000000000000, 87.65000000001222702, -148.2731074845242176 ) ) ;
#112170 = AXIS2_PLACEMENT_3D ( 'NONE', #33750, #71570, #114522 ) ;
#112171 = CARTESIAN_POINT ( 'NONE',  ( 23.14999999999998792, 11.38316329224760359, -198.5208684056144079 ) ) ;
#112172 = CARTESIAN_POINT ( 'NONE',  ( 23.24999999999999289, 69.45000000001149942, -48.17310748452436542 ) ) ;
#112173 = ORIENTED_EDGE ( 'NONE', *, *, #5820, .F. ) ;
#112174 = EDGE_LOOP ( 'NONE', ( #90656, #27136, #150635, #73120 ) ) ;
#112175 = CARTESIAN_POINT ( 'NONE',  ( 22.39999999999999503, 64.25000000001195133, -103.1231074845243825 ) ) ;
#112176 = CARTESIAN_POINT ( 'NONE',  ( -16.90202395485831133, 9.965944544561704532, -54.40301372126067037 ) ) ;
#112177 = DIRECTION ( 'NONE',  ( -1.000000000000000000, 7.304098846218134667E-16, 5.100424963727255829E-30 ) ) ;
#112178 = CARTESIAN_POINT ( 'NONE',  ( 20.94999999999999574, 87.65000000001266756, -200.6231074845242688 ) ) ;
#112179 = CARTESIAN_POINT ( 'NONE',  ( -22.39999999999999503, 59.68594599439717285, -233.9123800762197902 ) ) ;
#112180 = DIRECTION ( 'NONE',  ( 0.000000000000000000, 0.000000000000000000, -1.000000000000000000 ) ) ;
#112181 = EDGE_LOOP ( 'NONE', ( #138674, #3987 ) ) ;
#112182 = DIRECTION ( 'NONE',  ( 1.000000000000000000, 0.000000000000000000, 0.000000000000000000 ) ) ;
#112183 = DIRECTION ( 'NONE',  ( -1.000000000000000000, -0.000000000000000000, -0.000000000000000000 ) ) ;
#112185 = FACE_OUTER_BOUND ( 'NONE', #73885, .T. ) ;
#112184 = CARTESIAN_POINT ( 'NONE',  ( -18.47140463609786210, 85.67147468523300802, -129.8503470262502049 ) ) ;
#112186 = PLANE ( 'NONE',  #133325 ) ;
#112187 = CARTESIAN_POINT ( 'NONE',  ( 23.15000000000000213, -8.999999999988844479, -177.3939691226524076 ) ) ;
#112188 = VECTOR ( 'NONE', #140455, 1000.000000000000000 ) ;
#112189 = EDGE_CURVE ( 'NONE', #87130, #156098, #108164, .T. ) ;
#112190 = AXIS2_PLACEMENT_3D ( 'NONE', #46982, #168286, #6587 ) ;
#112191 = CARTESIAN_POINT ( 'NONE',  ( -23.15000000000000213, -9.000000000000003553, -9.893969122652444881 ) ) ;
#112192 = CARTESIAN_POINT ( 'NONE',  ( -20.94999999999999929, 76.00000000001213607, -136.5231074845242745 ) ) ;
#112193 = AXIS2_PLACEMENT_3D ( 'NONE', #248524, #7348, #45187 ) ;
#112194 = AXIS2_PLACEMENT_3D ( 'NONE', #186552, #64024, #225632 ) ;
#112196 = ORIENTED_EDGE ( 'NONE', *, *, #37502, .T. ) ;
#112195 = CARTESIAN_POINT ( 'NONE',  ( 23.24999999999999645, 70.35000000001187459, -90.37310748452433984 ) ) ;
#112197 = B_SPLINE_CURVE_WITH_KNOTS ( 'NONE', 3,
 ( #230141, #252258, #231445, #235265, #155772, #56600, #131038 ),
 .UNSPECIFIED., .F., .F.,
 ( 4, 3, 4 ),
 ( 0.000000000000000000, 1.860045280647521529E-05, 5.251155757304300621E-05 ),
 .UNSPECIFIED. ) ;
#112198 = EDGE_CURVE ( 'NONE', #85212, #105589, #100573, .T. ) ;
#112199 = AXIS2_PLACEMENT_3D ( 'NONE', #180186, #5354, #143608 ) ;
#112200 = CARTESIAN_POINT ( 'NONE',  ( 21.05000000000000071, 87.65000000001246860, -173.1231074845242688 ) ) ;
#112201 = DIRECTION ( 'NONE',  ( 0.000000000000000000, -1.000000000000000000, 0.000000000000000000 ) ) ;
#112202 = AXIS2_PLACEMENT_3D ( 'NONE', #218834, #37673, #131938 ) ;
#112203 = CIRCLE ( 'NONE', #87014, 0.09999999999999939493 ) ;
#112205 = CIRCLE ( 'NONE', #29021, 4.099999999999992539 ) ;
#112204 = PLANE ( 'NONE',  #54932 ) ;
#112206 = EDGE_CURVE ( 'NONE', #72701, #223936, #29081, .T. ) ;
#112207 = CARTESIAN_POINT ( 'NONE',  ( 15.73863059295127798, 9.351403174152808973, -83.97953043683850183 ) ) ;
#112208 = DIRECTION ( 'NONE',  ( -2.827886303505249259E-16, 0.8660254037844412611, 0.4999999999999956701 ) ) ;
#112209 = CIRCLE ( 'NONE', #62117, 0.1000000000000076938 ) ;
#112210 = DIRECTION ( 'NONE',  ( 0.000000000000000000, 0.2617529984164915779, 0.9651348961777187485 ) ) ;
#112211 = DIRECTION ( 'NONE',  ( 0.000000000000000000, 1.224646799142015331E-16, 1.000000000000000000 ) ) ;
#112212 = CARTESIAN_POINT ( 'NONE',  ( 23.15000000000000213, -11.64999999998883595, -64.00000000000000000 ) ) ;
#112213 = ORIENTED_EDGE ( 'NONE', *, *, #254764, .T. ) ;
#112214 = CARTESIAN_POINT ( 'NONE',  ( 18.59999999999997655, 76.00000000001170974, -69.52310748452431710 ) ) ;
#112216 = VERTEX_POINT ( 'NONE', #243966 ) ;
#112215 = DIRECTION ( 'NONE',  ( 0.000000000000000000, 0.000000000000000000, -1.000000000000000000 ) ) ;
#112217 = CARTESIAN_POINT ( 'NONE',  ( -16.94445028196808778, 44.07934375239701552, -235.2779890399608576 ) ) ;
#112218 = CARTESIAN_POINT ( 'NONE',  ( 20.94999999999999929, 76.00000000001170974, -69.52310748452431710 ) ) ;
#112219 = ORIENTED_EDGE ( 'NONE', *, *, #132391, .F. ) ;
#112220 = CARTESIAN_POINT ( 'NONE',  ( 23.14999999999999503, 11.65000000001116298, -54.75000000000000000 ) ) ;
#112221 = PRODUCT_CONTEXT ( 'NONE', #52359, 'mechanical' ) ;
#112222 = CARTESIAN_POINT ( 'NONE',  ( 21.14999999999999858, 69.35000000001259934, -191.1731074845243938 ) ) ;
#112223 = CARTESIAN_POINT ( 'NONE',  ( 22.49999999999999645, 64.35023708197972780, -69.61191746091132870 ) ) ;
#112224 = ORIENTED_EDGE ( 'NONE', *, *, #148810, .T. ) ;
#112225 = CARTESIAN_POINT ( 'NONE',  ( 20.94999999999999929, 85.00000000001207923, -126.6291383618717816 ) ) ;
#112226 = DIRECTION ( 'NONE',  ( 1.000000000000000000, 2.952720810173289112E-16, -0.000000000000000000 ) ) ;
#112227 = AXIS2_PLACEMENT_3D ( 'NONE', #36606, #116119, #195671 ) ;
#112228 = DIRECTION ( 'NONE',  ( 0.000000000000000000, -0.4088369013363280513, 0.9126074666063769270 ) ) ;
#112229 = ORIENTED_EDGE ( 'NONE', *, *, #183122, .F. ) ;
#112230 = AXIS2_PLACEMENT_3D ( 'NONE', #245247, #2754, #62751 ) ;
#112231 = VERTEX_POINT ( 'NONE', #199733 ) ;
#112232 = DIRECTION ( 'NONE',  ( -0.000000000000000000, -0.000000000000000000, -1.000000000000000000 ) ) ;
#112233 = EDGE_CURVE ( 'NONE', #235869, #246507, #145729, .T. ) ;
#112234 = DIRECTION ( 'NONE',  ( 1.000000000000000000, 0.000000000000000000, 0.000000000000000000 ) ) ;
#112235 = DIRECTION ( 'NONE',  ( -2.812466655313719426E-14, 0.1350103645451904977, 0.9908441862701596881 ) ) ;
#112236 = CARTESIAN_POINT ( 'NONE',  ( -16.92209698673484297, 30.15287859541585291, -234.7784133219286105 ) ) ;
#112237 = EDGE_CURVE ( 'NONE', #31671, #30979, #245532, .T. ) ;
#112239 = CARTESIAN_POINT ( 'NONE',  ( 21.97500000000000497, 66.25000000001186606, -90.67310748452437963 ) ) ;
#112238 = CYLINDRICAL_SURFACE ( 'NONE', #78345, 0.09999999999999939493 ) ;
#112240 = FACE_OUTER_BOUND ( 'NONE', #157705, .T. ) ;
#112241 = CARTESIAN_POINT ( 'NONE',  ( -21.05000000000000071, 87.39257802171739797, -72.59705706435616435 ) ) ;
#112242 = FACE_OUTER_BOUND ( 'NONE', #251449, .T. ) ;
#112243 = AXIS2_PLACEMENT_3D ( 'NONE', #107091, #167110, #246601 ) ;
#112244 = ORIENTED_EDGE ( 'NONE', *, *, #24736, .T. ) ;
#112246 = VERTEX_POINT ( 'NONE', #240131 ) ;
#112245 = CARTESIAN_POINT ( 'NONE',  ( 12.68104795156994591, 62.84928511903725479, -216.1139082291015256 ) ) ;
#112247 = CARTESIAN_POINT ( 'NONE',  ( 21.08134388332232234, 69.66531941949442341, -170.0989264020314522 ) ) ;
#112248 = AXIS2_PLACEMENT_3D ( 'NONE', #204925, #124139, #125417 ) ;
#112249 = CARTESIAN_POINT ( 'NONE',  ( -21.08078803292166725, -1.270299185012213394, -194.7951902842391405 ) ) ;
#112251 = DIRECTION ( 'NONE',  ( 0.000000000000000000, 1.734723475976998188E-13, 1.000000000000000000 ) ) ;
#112250 = CARTESIAN_POINT ( 'NONE',  ( -18.50000000000000000, 64.35000000001161879, -62.50830171387039513 ) ) ;
#112252 = EDGE_CURVE ( 'NONE', #14224, #222470, #121492, .T. ) ;
#112253 = ORIENTED_EDGE ( 'NONE', *, *, #196204, .F. ) ;
#112254 = CARTESIAN_POINT ( 'NONE',  ( -23.25000000000000000, 76.10000000001174669, -81.17267829206912211 ) ) ;
#112255 = CARTESIAN_POINT ( 'NONE',  ( 18.59999999999999432, 13.71992543034163958, -238.5823796952984992 ) ) ;
#112256 = CARTESIAN_POINT ( 'NONE',  ( -18.59999999999999787, 43.92448011351754644, -236.0509145372394357 ) ) ;
#112257 = ADVANCED_FACE ( 'NONE', ( #161892 ), #120213, .F. ) ;
#112258 = ORIENTED_EDGE ( 'NONE', *, *, #164978, .F. ) ;
#112259 = AXIS2_PLACEMENT_3D ( 'NONE', #16927, #96428, #155178 ) ;
#112260 = CIRCLE ( 'NONE', #195464, 0.1000000000000009492 ) ;
#112261 = ORIENTED_EDGE ( 'NONE', *, *, #153022, .T. ) ;
#112262 = CARTESIAN_POINT ( 'NONE',  ( -21.65000000000000213, 7.250000000011138646, -109.7500000000000426 ) ) ;
#112263 = EDGE_CURVE ( 'NONE', #150811, #63552, #233071, .T. ) ;
#112264 = ORIENTED_EDGE ( 'NONE', *, *, #158843, .T. ) ;
#112265 = CARTESIAN_POINT ( 'NONE',  ( 18.49999999999999645, 5.699452464321595357, 12.54227395656983290 ) ) ;
#112266 = DIRECTION ( 'NONE',  ( 1.000000000000000000, 0.000000000000000000, 0.000000000000000000 ) ) ;
#112267 = VECTOR ( 'NONE', #120926, 1000.000000000000000 ) ;
#112269 = VECTOR ( 'NONE', #94474, 1000.000000000000000 ) ;
#112268 = CARTESIAN_POINT ( 'NONE',  ( -21.08198257630413508, 65.50254075141489807, -241.9517825296665023 ) ) ;
#112270 = CIRCLE ( 'NONE', #203818, 0.1000000000000043771 ) ;
#112271 = ORIENTED_EDGE ( 'NONE', *, *, #27868, .T. ) ;
#112272 = CARTESIAN_POINT ( 'NONE',  ( -21.65000000000000213, 63.54522198573874192, -221.7484608313106378 ) ) ;
#112273 = AXIS2_PLACEMENT_3D ( 'NONE', #199690, #25849, #138379 ) ;
#112274 = EDGE_CURVE ( 'NONE', #110468, #147247, #79080, .T. ) ;
#112275 = CARTESIAN_POINT ( 'NONE',  ( -16.27683809663751191, 19.69766786220167631, -229.8585047820796490 ) ) ;
#112276 = CARTESIAN_POINT ( 'NONE',  ( 18.59999999999999432, 70.47363787294415260, -228.3418745167492432 ) ) ;
#112277 = DIRECTION ( 'NONE',  ( 1.000000000000000000, 0.000000000000000000, 0.000000000000000000 ) ) ;
#112278 = CARTESIAN_POINT ( 'NONE',  ( -23.15000000000000213, -8.999999999988844479, -158.2060308773475867 ) ) ;
#112279 = DIRECTION ( 'NONE',  ( 0.000000000000000000, 0.9126074666064696306, 0.4088369013361213278 ) ) ;
#112280 = DIRECTION ( 'NONE',  ( -1.000000000000000000, 0.000000000000000000, -0.000000000000000000 ) ) ;
#112281 = ORIENTED_EDGE ( 'NONE', *, *, #116796, .F. ) ;
#112283 = DIRECTION ( 'NONE',  ( 0.000000000000000000, -1.000000000000000000, 0.000000000000000000 ) ) ;
#112282 = DIRECTION ( 'NONE',  ( -2.952720810173288619E-16, 0.4721928772777346239, 0.8814952561688430555 ) ) ;
#112284 = ORIENTED_EDGE ( 'NONE', *, *, #234052, .F. ) ;
#112286 = VERTEX_POINT ( 'NONE', #5329 ) ;
#112285 = CARTESIAN_POINT ( 'NONE',  ( -18.59999999999999787, -1.835859311443637010, -45.00443916879852679 ) ) ;
#112287 = ORIENTED_EDGE ( 'NONE', *, *, #101550, .T. ) ;
#112288 = CARTESIAN_POINT ( 'NONE',  ( -21.05000000000000071, 18.67052684763574533, -226.7323173977782460 ) ) ;
#112289 = CARTESIAN_POINT ( 'NONE',  ( 18.58222699835054570, 10.33200063080772324, -72.59316749566428939 ) ) ;
#112290 = CARTESIAN_POINT ( 'NONE',  ( -20.85000000000000142, -0.3238857010591806307, -200.9575895893139545 ) ) ;
#112291 = CARTESIAN_POINT ( 'NONE',  ( 21.05000000000000071, 65.37127968600773897, -128.8581939154367717 ) ) ;
#112292 = ORIENTED_EDGE ( 'NONE', *, *, #38577, .T. ) ;
#112293 = CARTESIAN_POINT ( 'NONE',  ( 21.05000000000000071, 69.74218538953655866, -203.6208977758331855 ) ) ;
#112294 = CARTESIAN_POINT ( 'NONE',  ( 21.05000000000000071, -11.64999999998883595, -103.4000000000000341 ) ) ;
#112295 = VERTEX_POINT ( 'NONE', #122765 ) ;
#112296 = AXIS2_PLACEMENT_3D ( 'NONE', #47826, #208225, #93066 ) ;
#112297 = DIRECTION ( 'NONE',  ( 1.000000000000000000, 0.000000000000000000, 0.000000000000000000 ) ) ;
#112298 = CARTESIAN_POINT ( 'NONE',  ( -21.05000000000000071, 6.300000000011169554, -67.10000000000005116 ) ) ;
#112299 = ORIENTED_EDGE ( 'NONE', *, *, #129445, .T. ) ;
#112300 = MANIFOLD_SOLID_BREP ( 'Stock-MAS-200-1', #199013 ) ;
#112301 = FACE_OUTER_BOUND ( 'NONE', #11235, .T. ) ;
#112302 = CIRCLE ( 'NONE', #241299, 0.2000000000000057288 ) ;
#112303 = ADVANCED_FACE ( 'NONE', ( #185288 ), #2775, .T. ) ;
#112304 = ORIENTED_EDGE ( 'NONE', *, *, #209904, .F. ) ;
#112305 = LINE ( 'NONE', #70631, #138175 ) ;
#112306 = ORIENTED_EDGE ( 'NONE', *, *, #150359, .T. ) ;
#112307 = CARTESIAN_POINT ( 'NONE',  ( -18.59999999999999787, 1.162701749949165642, -175.4999999999999716 ) ) ;
#112308 = DIRECTION ( 'NONE',  ( -1.000000000000000000, 0.000000000000000000, 0.000000000000000000 ) ) ;
#112309 = CARTESIAN_POINT ( 'NONE',  ( 18.49999999999999289, 10.25000000001115552, -188.8499999999999659 ) ) ;
#112310 = EDGE_CURVE ( 'NONE', #224010, #101170, #34291, .T. ) ;
#112311 = CARTESIAN_POINT ( 'NONE',  ( 20.85000000000000142, 70.15623657602074559, -198.0563205710787713 ) ) ;
#112312 = AXIS2_PLACEMENT_3D ( 'NONE', #215792, #157146, #52873 ) ;
#112313 = CIRCLE ( 'NONE', #95712, 0.1999999999999987899 ) ;
#112314 = EDGE_CURVE ( 'NONE', #81173, #26209, #24970, .T. ) ;
#112315 = ADVANCED_FACE ( 'NONE', ( #131728 ), #245266, .F. ) ;
#112316 = CARTESIAN_POINT ( 'NONE',  ( -22.37643362114956957, 0.09908137369253962323, -25.87421000604160426 ) ) ;
#112317 = CARTESIAN_POINT ( 'NONE',  ( -20.54999999999999716, -8.999999999988844479, -57.50603087734755547 ) ) ;
#112318 = CARTESIAN_POINT ( 'NONE',  ( -20.94999999999999929, -11.75000000000000000, -3.100000000000001865 ) ) ;
#112319 = ORIENTED_EDGE ( 'NONE', *, *, #20549, .T. ) ;
#112320 = CARTESIAN_POINT ( 'NONE',  ( -21.64999999999999858, 66.65000000001201386, -115.6731074845243654 ) ) ;
#112321 = VERTEX_POINT ( 'NONE', #165743 ) ;
#112324 = ORIENTED_EDGE ( 'NONE', *, *, #152117, .F. ) ;
#112323 = FACE_OUTER_BOUND ( 'NONE', #140746, .T. ) ;
#112322 = CARTESIAN_POINT ( 'NONE',  ( 20.94999999999999929, 67.23127455305835554, -235.8551265064784559 ) ) ;
#112325 = ORIENTED_EDGE ( 'NONE', *, *, #115650, .T. ) ;
#112326 = FACE_OUTER_BOUND ( 'NONE', #195403, .T. ) ;
#112327 = CARTESIAN_POINT ( 'NONE',  ( -21.12230431290520016, 6.457566653293005388, 0.005209851689006794913 ) ) ;
#112330 = B_SPLINE_CURVE_WITH_KNOTS ( 'NONE', 3,
 ( #40445, #84616, #221582, #83349 ),
 .UNSPECIFIED., .F., .F.,
 ( 4, 4 ),
 ( 3.469446951953614189E-18, 0.0001058379652594581074 ),
 .UNSPECIFIED. ) ;
#112329 = CYLINDRICAL_SURFACE ( 'NONE', #147854, 0.09999999999999939493 ) ;
#112328 = B_SPLINE_CURVE_WITH_KNOTS ( 'NONE', 3,
 ( #119959, #220321, #256806, #99048, #135619, #254277, #136917, #117362, #75682, #155237, #217718, #37845, #19552, #39126, #22131, #101601, #234736, #215170, #96485 ),
 .UNSPECIFIED., .F., .F.,
 ( 4, 3, 3, 3, 3, 3, 4 ),
 ( 1.430489624538199204E-17, 2.646747978908941165E-05, 5.271166642128824757E-05, 9.008788829885143402E-05, 0.0001426648776561019298, 0.0001897378458659829863, 0.0001917382627806356299 ),
 .UNSPECIFIED. ) ;
#112331 = CARTESIAN_POINT ( 'NONE',  ( 20.95052659398289308, 59.09967180796918029, -225.8008737851698982 ) ) ;
#112332 = VERTEX_POINT ( 'NONE', #110882 ) ;
#112334 = EDGE_LOOP ( 'NONE', ( #174115, #253440, #147338, #205376 ) ) ;
#112333 = CARTESIAN_POINT ( 'NONE',  ( 20.95483826173899899, 67.12383379524264626, -194.9768319316249006 ) ) ;
#112335 = EDGE_CURVE ( 'NONE', #187772, #104099, #150049, .T. ) ;
#112336 = EDGE_CURVE ( 'NONE', #242990, #181475, #48336, .T. ) ;
#112337 = DIRECTION ( 'NONE',  ( 1.000000000000000000, -0.000000000000000000, -0.000000000000000000 ) ) ;
#112339 = EDGE_LOOP ( 'NONE', ( #153471, #11647, #28454, #186216, #48666 ) ) ;
#112338 = CARTESIAN_POINT ( 'NONE',  ( -16.89081410710458542, 9.951318529858268036, -154.8544059198364096 ) ) ;
#112340 = TOROIDAL_SURFACE ( 'NONE', #49957, 0.2000000000000000111, 0.1000000000000000056 ) ;
#112341 = AXIS2_PLACEMENT_3D ( 'NONE', #103305, #27684, #184133 ) ;
#112342 = ORIENTED_EDGE ( 'NONE', *, *, #167359, .T. ) ;
#112343 = CARTESIAN_POINT ( 'NONE',  ( 20.95539060131842746, 12.00925073368239282, -206.2176608984306938 ) ) ;
#112344 = DIRECTION ( 'NONE',  ( 0.000000000000000000, 0.8490545835447252943, 0.5283051335749948674 ) ) ;
#112345 = ORIENTED_EDGE ( 'NONE', *, *, #133374, .T. ) ;
#112346 = DIRECTION ( 'NONE',  ( 0.000000000000000000, -1.000000000000000000, 0.000000000000000000 ) ) ;
#112347 = ORIENTED_EDGE ( 'NONE', *, *, #36276, .F. ) ;
#112348 = EDGE_CURVE ( 'NONE', #87859, #172414, #50063, .T. ) ;
#112350 = EDGE_CURVE ( 'NONE', #77589, #6871, #245890, .T. ) ;
#112349 = DIRECTION ( 'NONE',  ( 1.000000000000000000, 0.000000000000000000, 0.000000000000000000 ) ) ;
#112351 = FACE_OUTER_BOUND ( 'NONE', #201174, .T. ) ;
#112352 = ADVANCED_FACE ( 'NONE', ( #190443 ), #31387, .F. ) ;
#112353 = ORIENTED_EDGE ( 'NONE', *, *, #237420, .T. ) ;
#112354 = DIRECTION ( 'NONE',  ( 0.000000000000000000, 0.000000000000000000, 1.000000000000000000 ) ) ;
#112355 = TOROIDAL_SURFACE ( 'NONE', #179023, 4.099999999999999645, 0.1000000000000000056 ) ;
#112356 = CIRCLE ( 'NONE', #83, 0.09999999999999609201 ) ;
#112357 = CIRCLE ( 'NONE', #78986, 0.1000000000000028644 ) ;
#112358 = AXIS2_PLACEMENT_3D ( 'NONE', #41613, #24623, #2442 ) ;
#112359 = FACE_OUTER_BOUND ( 'NONE', #40765, .T. ) ;
#112360 = ORIENTED_EDGE ( 'NONE', *, *, #132845, .F. ) ;
#112361 = AXIS2_PLACEMENT_3D ( 'NONE', #216419, #54772, #97728 ) ;
#112362 = EDGE_LOOP ( 'NONE', ( #96359, #171385, #169568, #108579 ) ) ;
#112363 = CARTESIAN_POINT ( 'NONE',  ( 18.58685178364169843, -9.406733083793096029, -107.6244204690877524 ) ) ;
#112364 = ORIENTED_EDGE ( 'NONE', *, *, #114650, .F. ) ;
#112365 = CARTESIAN_POINT ( 'NONE',  ( 20.85000000000000142, 76.00000000001239187, -162.1231074845243825 ) ) ;
#112366 = ORIENTED_EDGE ( 'NONE', *, *, #25986, .F. ) ;
#112368 = ORIENTED_EDGE ( 'NONE', *, *, #117106, .T. ) ;
#112367 = CARTESIAN_POINT ( 'NONE',  ( 21.17356465864818915, 75.90108875899811380, -109.4459106107660489 ) ) ;
#112369 = VERTEX_POINT ( 'NONE', #47033 ) ;
#112370 = DIRECTION ( 'NONE',  ( 1.000000000000000000, 0.000000000000000000, 0.000000000000000000 ) ) ;
#112371 = AXIS2_PLACEMENT_3D ( 'NONE', #256426, #21754, #179554 ) ;
#112372 = EDGE_LOOP ( 'NONE', ( #150343, #85504, #6991, #60537 ) ) ;
#112376 = EDGE_CURVE ( 'NONE', #168251, #226785, #107014, .T. ) ;
#112375 = EDGE_LOOP ( 'NONE', ( #215840, #29823, #40217, #206699 ) ) ;
#112374 = ORIENTED_EDGE ( 'NONE', *, *, #250416, .F. ) ;
#112373 = FACE_OUTER_BOUND ( 'NONE', #16894, .T. ) ;
#112377 = CIRCLE ( 'NONE', #16513, 0.1000000000000028644 ) ;
#112378 = DIRECTION ( 'NONE',  ( 0.000000000000000000, 1.000000000000000000, 0.000000000000000000 ) ) ;
#112379 = ORIENTED_EDGE ( 'NONE', *, *, #214107, .F. ) ;
#112380 = DIRECTION ( 'NONE',  ( -0.000000000000000000, -0.000000000000000000, 1.000000000000000000 ) ) ;
#112381 = ORIENTED_EDGE ( 'NONE', *, *, #47341, .F. ) ;
#112382 = EDGE_CURVE ( 'NONE', #16536, #232010, #133281, .T. ) ;
#112383 = CARTESIAN_POINT ( 'NONE',  ( 20.94999999999999574, 87.65000000001235492, -167.1231074845242688 ) ) ;
#112385 = ORIENTED_EDGE ( 'NONE', *, *, #124755, .F. ) ;
#112384 = DIRECTION ( 'NONE',  ( -1.000000000000000000, 1.207181226542539700E-16, -2.694675058168174199E-16 ) ) ;
#112386 = LINE ( 'NONE', #114944, #639 ) ;
#112387 = ORIENTED_EDGE ( 'NONE', *, *, #238079, .F. ) ;
#112388 = LINE ( 'NONE', #246738, #27453 ) ;
#112390 = ORIENTED_EDGE ( 'NONE', *, *, #252188, .F. ) ;
#112389 = EDGE_CURVE ( 'NONE', #40580, #159384, #66625, .T. ) ;
#112391 = DIRECTION ( 'NONE',  ( 1.000000000000000000, -3.448943450116723075E-16, -6.438528483529606658E-16 ) ) ;
#112392 = DIRECTION ( 'NONE',  ( 0.000000000000000000, 1.000000000000000000, 0.000000000000000000 ) ) ;
#112393 = ADVANCED_FACE ( 'NONE', ( #146147 ), #41714, .T. ) ;
#112394 = VERTEX_POINT ( 'NONE', #246533 ) ;
#112396 = ORIENTED_EDGE ( 'NONE', *, *, #96712, .F. ) ;
#112395 = CARTESIAN_POINT ( 'NONE',  ( -22.39999999999999858, 76.10085836911093793, -148.2726746080136877 ) ) ;
#112397 = VECTOR ( 'NONE', #163911, 1000.000000000000000 ) ;
#112398 = CARTESIAN_POINT ( 'NONE',  ( 18.59999999999999076, 64.35000000001197407, -111.6731074845243796 ) ) ;
#112399 = EDGE_CURVE ( 'NONE', #14463, #61798, #169621, .T. ) ;
#112401 = ORIENTED_EDGE ( 'NONE', *, *, #189115, .F. ) ;
#112400 = ORIENTED_EDGE ( 'NONE', *, *, #59987, .F. ) ;
#112402 = ORIENTED_EDGE ( 'NONE', *, *, #185928, .T. ) ;
#112404 = EDGE_CURVE ( 'NONE', #129578, #96147, #175025, .T. ) ;
#112403 = CARTESIAN_POINT ( 'NONE',  ( -18.69999999999999929, -8.150000000000005684, 10.50000000000000178 ) ) ;
#112405 = ORIENTED_EDGE ( 'NONE', *, *, #175980, .F. ) ;
#112406 = ORIENTED_EDGE ( 'NONE', *, *, #43702, .T. ) ;
#112407 = DIRECTION ( 'NONE',  ( -0.000000000000000000, 0.4721928772777345684, 0.8814952561688429444 ) ) ;
#112408 = CIRCLE ( 'NONE', #166586, 0.09999999999999939493 ) ;
#112409 = ORIENTED_EDGE ( 'NONE', *, *, #244413, .T. ) ;
#112410 = DIRECTION ( 'NONE',  ( 0.000000000000000000, -0.8660254037844411501, -0.4999999999999956701 ) ) ;
#112411 = CARTESIAN_POINT ( 'NONE',  ( 20.94999999999999929, 1.115600667400684642E-11, -134.0000000000000284 ) ) ;
#112412 = EDGE_LOOP ( 'NONE', ( #126722, #253262, #95065, #2996 ) ) ;
#112413 = EDGE_LOOP ( 'NONE', ( #69415, #206807, #185151, #239424, #235911 ) ) ;
#112414 = LINE ( 'NONE', #191969, #129707 ) ;
#112416 = ORIENTED_EDGE ( 'NONE', *, *, #185215, .T. ) ;
#112415 = AXIS2_PLACEMENT_3D ( 'NONE', #29853, #11563, #151062 ) ;
#112417 = EDGE_CURVE ( 'NONE', #178867, #143316, #241606, .T. ) ;
#112419 = ADVANCED_FACE ( 'NONE', ( #150031 ), #74363, .T. ) ;
#112418 = AXIS2_PLACEMENT_3D ( 'NONE', #160402, #61274, #140813 ) ;
#112420 = DIRECTION ( 'NONE',  ( 0.000000000000000000, -1.000000000000000000, -0.000000000000000000 ) ) ;
#112421 = ORIENTED_EDGE ( 'NONE', *, *, #17747, .T. ) ;
#112422 = ORIENTED_EDGE ( 'NONE', *, *, #246622, .F. ) ;
#112423 = AXIS2_PLACEMENT_3D ( 'NONE', #244296, #202615, #102192 ) ;
#112424 = EDGE_CURVE ( 'NONE', #73797, #85875, #179278, .T. ) ;
#112425 = DIRECTION ( 'NONE',  ( 1.000000000000000000, 0.000000000000000000, 0.000000000000000000 ) ) ;
#112427 = ORIENTED_EDGE ( 'NONE', *, *, #39142, .T. ) ;
#112426 = CARTESIAN_POINT ( 'NONE',  ( 18.40000000000000213, 85.50000000001236344, -163.0237453873441780 ) ) ;
#112428 = DIRECTION ( 'NONE',  ( 0.000000000000000000, -8.673617379883787770E-15, 1.000000000000000000 ) ) ;
#112429 = CARTESIAN_POINT ( 'NONE',  ( -20.94999999999999929, 38.23914636435922176, -236.1324109481172968 ) ) ;
#112430 = VECTOR ( 'NONE', #83906, 1000.000000000000114 ) ;
#112431 = CARTESIAN_POINT ( 'NONE',  ( 20.95420533658165141, 65.45413552525251077, -128.9556014638311296 ) ) ;
#112433 = AXIS2_PLACEMENT_3D ( 'NONE', #204923, #26314, #105810 ) ;
#112432 = DIRECTION ( 'NONE',  ( 0.000000000000000000, 0.8660254037844482555, 0.4999999999999837907 ) ) ;
#112434 = DIRECTION ( 'NONE',  ( -0.000000000000000000, 6.982962677686266711E-15, -1.000000000000000000 ) ) ;
#112435 = CARTESIAN_POINT ( 'NONE',  ( -16.88219499860498374, 66.04979357458471156, -157.3737977944171291 ) ) ;
#112436 = DIRECTION ( 'NONE',  ( 0.000000000000000000, 0.9651348961777379554, -0.2617529984164210233 ) ) ;
#112437 = DIRECTION ( 'NONE',  ( 1.040834085586049673E-13, 0.7899159663865300551, 0.6132151058540831201 ) ) ;
#112439 = EDGE_CURVE ( 'NONE', #164969, #17339, #213832, .T. ) ;
#112438 = CARTESIAN_POINT ( 'NONE',  ( 18.50000000000000355, 38.28679861725832012, -261.0868692510649680 ) ) ;
#112440 = CARTESIAN_POINT ( 'NONE',  ( 18.49999999999999289, 13.20456090973765662, -206.4140623547709765 ) ) ;
#112441 = EDGE_CURVE ( 'NONE', #75472, #149751, #218069, .T. ) ;
#112442 = EDGE_LOOP ( 'NONE', ( #112244, #236526, #90978 ) ) ;
#112443 = VECTOR ( 'NONE', #90348, 1000.000000000000114 ) ;
#112444 = CIRCLE ( 'NONE', #149870, 0.6000000000000005329 ) ;
#112445 = CIRCLE ( 'NONE', #120639, 0.1000000000000028644 ) ;
#112446 = TOROIDAL_SURFACE ( 'NONE', #79082, 11.65000000000000036, 0.1000000000000000056 ) ;
#112447 = EDGE_CURVE ( 'NONE', #189298, #232474, #171, .T. ) ;
#112449 = VERTEX_POINT ( 'NONE', #152610 ) ;
#112448 = VERTEX_POINT ( 'NONE', #78157 ) ;
#112450 = EDGE_LOOP ( 'NONE', ( #58670, #232843, #37972, #133051 ) ) ;
#112451 = CIRCLE ( 'NONE', #29090, 0.1000000000000028644 ) ;
#112452 = CARTESIAN_POINT ( 'NONE',  ( 21.13614978966381841, 76.00000000001270450, -210.0222121863581037 ) ) ;
#112453 = CARTESIAN_POINT ( 'NONE',  ( 20.86036036209916134, 10.62104277658212048, -141.6663484185077664 ) ) ;
#112455 = CARTESIAN_POINT ( 'NONE',  ( 21.05000000000000071, 1.115600667400684642E-11, -113.3750000000000284 ) ) ;
#112454 = DIRECTION ( 'NONE',  ( -0.7071067811865474617, -0.7071067811865474617, -2.044391222244499837E-16 ) ) ;
#112456 = EDGE_CURVE ( 'NONE', #230504, #73243, #254222, .T. ) ;
#112457 = VERTEX_POINT ( 'NONE', #18200 ) ;
#112458 = ORIENTED_EDGE ( 'NONE', *, *, #185047, .F. ) ;
#112459 = SURFACE_STYLE_USAGE ( .BOTH. , #214115 ) ;
#112460 = CARTESIAN_POINT ( 'NONE',  ( -22.50000000000000000, 0.000000000000000000, 0.000000000000000000 ) ) ;
#112461 = CARTESIAN_POINT ( 'NONE',  ( -22.59080734064477625, 64.25000000001195133, -103.0538571926214217 ) ) ;
#112462 = CARTESIAN_POINT ( 'NONE',  ( -20.85000000000000142, 77.16412189325305349, -95.30825939895268561 ) ) ;
#112463 = EDGE_LOOP ( 'NONE', ( #57834, #216742, #238722, #209870 ) ) ;
#112464 = ORIENTED_EDGE ( 'NONE', *, *, #110941, .F. ) ;
#112465 = DIRECTION ( 'NONE',  ( 0.7071067811865474617, 0.7071067811865474617, 0.000000000000000000 ) ) ;
#112466 = CARTESIAN_POINT ( 'NONE',  ( 18.60000000000000142, 9.105964803472835101, -245.3658845043482586 ) ) ;
#112467 = CARTESIAN_POINT ( 'NONE',  ( 18.49999999999999645, 1.637172712981537659, -145.5821533654720383 ) ) ;
#112469 = ORIENTED_EDGE ( 'NONE', *, *, #66503, .F. ) ;
#112468 = DIRECTION ( 'NONE',  ( 1.000000000000000000, -0.000000000000000000, -0.000000000000000000 ) ) ;
#112470 = CARTESIAN_POINT ( 'NONE',  ( 20.94999999999999929, 31.15787740146373608, -259.8205824356103903 ) ) ;
#112471 = CARTESIAN_POINT ( 'NONE',  ( -11.60000000000000320, -8.250000000000005329, 19.04142135623731491 ) ) ;
#112472 = DIRECTION ( 'NONE',  ( 0.000000000000000000, 0.000000000000000000, -1.000000000000000000 ) ) ;
#112473 = DIRECTION ( 'NONE',  ( -0.000000000000000000, -0.000000000000000000, 1.000000000000000000 ) ) ;
#112474 = EDGE_LOOP ( 'NONE', ( #45730, #16862, #10769, #63232 ) ) ;
#112475 = CARTESIAN_POINT ( 'NONE',  ( 12.84435279558020149, 66.58929125296475604, -84.95389907868030832 ) ) ;
#112476 = DIRECTION ( 'NONE',  ( 0.000000000000000000, 1.000000000000000000, 0.000000000000000000 ) ) ;
#112477 = CIRCLE ( 'NONE', #220790, 0.1999999999999987899 ) ;
#112478 = FACE_OUTER_BOUND ( 'NONE', #17715, .T. ) ;
#112480 = CARTESIAN_POINT ( 'NONE',  ( -21.05000000000000071, 74.16465844978819177, -191.9679561919613775 ) ) ;
#112479 = DIRECTION ( 'NONE',  ( 0.000000000000000000, -6.982962677686266711E-15, 1.000000000000000000 ) ) ;
#112481 = LINE ( 'NONE', #134573, #158126 ) ;
#112482 = AXIS2_PLACEMENT_3D ( 'NONE', #32544, #172054, #251544 ) ;
#112483 = CARTESIAN_POINT ( 'NONE',  ( -20.64999999999999858, 6.659649981195239654, -220.3002595397864241 ) ) ;
#112484 = DIRECTION ( 'NONE',  ( 0.000000000000000000, 0.9915357197604792727, -0.1298341882520475943 ) ) ;
#112485 = DIRECTION ( 'NONE',  ( -0.000000000000000000, 1.000000000000000000, 6.352154140967427193E-15 ) ) ;
#112486 = CARTESIAN_POINT ( 'NONE',  ( 15.48841904831874849, 8.561580951692381092, -87.85000000000005116 ) ) ;
#112488 = EDGE_LOOP ( 'NONE', ( #51765, #214372, #156358, #76065 ) ) ;
#112487 = VECTOR ( 'NONE', #192995, 999.9999999999998863 ) ;
#112489 = ORIENTED_EDGE ( 'NONE', *, *, #245032, .T. ) ;
#112490 = ORIENTED_EDGE ( 'NONE', *, *, #8015, .T. ) ;
#112491 = EDGE_CURVE ( 'NONE', #130380, #75842, #112616, .T. ) ;
#112492 = LINE ( 'NONE', #214147, #148676 ) ;
#112493 = CARTESIAN_POINT ( 'NONE',  ( -20.00857864376270001, 66.65000000001157332, -57.17310748452438673 ) ) ;
#112494 = EDGE_LOOP ( 'NONE', ( #184115, #65304, #12979, #109939, #238042, #3488, #252543, #200295, #102206, #181606, #141408, #131026, #241022, #178301, #153076, #146322, #50143, #131170, #185346, #49128, #175597, #11450, #113866, #178372, #65407, #186523, #108211 ) ) ;
#112495 = CYLINDRICAL_SURFACE ( 'NONE', #9527, 0.09999999999999939493 ) ;
#112496 = CIRCLE ( 'NONE', #145784, 2.000000000000002665 ) ;
#112497 = EDGE_LOOP ( 'NONE', ( #93954, #25957 ) ) ;
#112498 = AXIS2_PLACEMENT_3D ( 'NONE', #234254, #12683, #53057 ) ;
#112499 = EDGE_CURVE ( 'NONE', #7751, #243103, #234682, .T. ) ;
#112500 = ORIENTED_EDGE ( 'NONE', *, *, #246975, .F. ) ;
#112501 = CARTESIAN_POINT ( 'NONE',  ( -16.94107738177415712, 44.01795756907898749, -235.2811900454759666 ) ) ;
#112502 = ORIENTED_EDGE ( 'NONE', *, *, #168728, .F. ) ;
#112503 = AXIS2_PLACEMENT_3D ( 'NONE', #162727, #62332, #216252 ) ;
#112504 = DIRECTION ( 'NONE',  ( 1.000000000000000000, 0.000000000000000000, 0.000000000000000000 ) ) ;
#112505 = CARTESIAN_POINT ( 'NONE',  ( 18.59999999999996945, 7.021664781911246322, -171.3335654018973173 ) ) ;
#112506 = CARTESIAN_POINT ( 'NONE',  ( -18.50000000000000711, 11.75000000001115197, -174.5148057706539930 ) ) ;
#112507 = CARTESIAN_POINT ( 'NONE',  ( -23.49999999999994316, 77.83551161375991967, -47.62760213295649692 ) ) ;
#112508 = DIRECTION ( 'NONE',  ( -0.7071067811864846231, -0.2890913453341779626, 0.6453109281989296564 ) ) ;
#112510 = VERTEX_POINT ( 'NONE', #256754 ) ;
#112509 = CARTESIAN_POINT ( 'NONE',  ( -16.87683809663752044, 29.54312324717474780, -234.4517840742876729 ) ) ;
#112512 = CARTESIAN_POINT ( 'NONE',  ( 18.49999999999998934, 19.05165861791954285, -232.6888762659126826 ) ) ;
#112511 = FACE_OUTER_BOUND ( 'NONE', #234956, .T. ) ;
#112513 = DIRECTION ( 'NONE',  ( -1.000000000000000000, -3.448943450116728005E-16, -6.438528483529605672E-16 ) ) ;
#112514 = FACE_OUTER_BOUND ( 'NONE', #243536, .T. ) ;
#112515 = CARTESIAN_POINT ( 'NONE',  ( -20.94999999999999929, 77.25000000001159606, -61.52310748452431710 ) ) ;
#112516 = VERTEX_POINT ( 'NONE', #96430 ) ;
#112517 = CARTESIAN_POINT ( 'NONE',  ( -21.12230431290519661, 6.457566653304161797, -33.49479014831099022 ) ) ;
#112518 = AXIS2_PLACEMENT_3D ( 'NONE', #99874, #142858, #221125 ) ;
#112519 = ORIENTED_EDGE ( 'NONE', *, *, #169063, .F. ) ;
#112520 = DIRECTION ( 'NONE',  ( 1.000000000000000000, -1.186688945009010077E-16, -8.286604613020808509E-31 ) ) ;
#112521 = ORIENTED_EDGE ( 'NONE', *, *, #231825, .T. ) ;
#112522 = LINE ( 'NONE', #132079, #42975 ) ;
#112523 = DIRECTION ( 'NONE',  ( 0.000000000000000000, -1.000000000000000000, -6.860497997771532351E-15 ) ) ;
#112524 = CARTESIAN_POINT ( 'NONE',  ( 23.24999999999999289, 69.35000000001259934, -191.1731074845243938 ) ) ;
#112525 = ORIENTED_EDGE ( 'NONE', *, *, #248374, .F. ) ;
#112526 = ORIENTED_EDGE ( 'NONE', *, *, #227037, .T. ) ;
#112527 = EDGE_CURVE ( 'NONE', #156184, #86293, #199932, .T. ) ;
#112528 = LINE ( 'NONE', #209053, #210915 ) ;
#112529 = CARTESIAN_POINT ( 'NONE',  ( 20.95483826173899899, 10.49151854554416730, -207.4616709084843080 ) ) ;
#112530 = CIRCLE ( 'NONE', #62471, 0.09999999999998898659 ) ;
#112531 = CARTESIAN_POINT ( 'NONE',  ( -18.59999999999999787, 7.128833340094563376, -233.7327013124401276 ) ) ;
#112533 = FACE_OUTER_BOUND ( 'NONE', #178074, .T. ) ;
#112532 = AXIS2_PLACEMENT_3D ( 'NONE', #186879, #90310, #6931 ) ;
#112534 = ADVANCED_FACE ( 'NONE', ( #114738 ), #237251, .T. ) ;
#112535 = AXIS2_PLACEMENT_3D ( 'NONE', #62081, #256359, #158640 ) ;
#112538 = DIRECTION ( 'NONE',  ( 1.000000000000000000, 0.000000000000000000, 0.000000000000000000 ) ) ;
#112537 = AXIS2_PLACEMENT_3D ( 'NONE', #245906, #249749, #9850 ) ;
#112536 = CARTESIAN_POINT ( 'NONE',  ( -18.59999999999999787, 64.25000000001222134, -148.7731074845244450 ) ) ;
#112539 = CARTESIAN_POINT ( 'NONE',  ( 21.08035267497491105, 6.331706839794169817, -167.4173113752238464 ) ) ;
#112540 = CARTESIAN_POINT ( 'NONE',  ( 15.66039659514495419, 9.360749169926259938, -50.81457014060725896 ) ) ;
#112541 = CARTESIAN_POINT ( 'NONE',  ( -21.05000000000000071, 76.00000000001170974, -69.52310748452431710 ) ) ;
#112542 = ORIENTED_EDGE ( 'NONE', *, *, #57620, .T. ) ;
#112543 = FACE_OUTER_BOUND ( 'NONE', #12852, .T. ) ;
#112545 = ORIENTED_EDGE ( 'NONE', *, *, #218961, .T. ) ;
#112544 = DIRECTION ( 'NONE',  ( -1.000000000000000000, 0.000000000000000000, 0.000000000000000000 ) ) ;
#112546 = VECTOR ( 'NONE', #190152, 1000.000000000000000 ) ;
#112547 = FACE_OUTER_BOUND ( 'NONE', #192893, .T. ) ;
#112548 = CARTESIAN_POINT ( 'NONE',  ( -23.25000000000000000, 68.97833521811233481, -166.1895420826271277 ) ) ;
#112550 = DIRECTION ( 'NONE',  ( 0.000000000000000000, -7.116814260417668513E-15, 1.000000000000000000 ) ) ;
#112549 = DIRECTION ( 'NONE',  ( 0.7071067811865463515, -0.7071067811865487940, 0.000000000000000000 ) ) ;
#112551 = ADVANCED_FACE ( 'NONE', ( #172191, #138125 ), #217659, .F. ) ;
#112552 = DIRECTION ( 'NONE',  ( 1.000000000000000000, 0.000000000000000000, 0.000000000000000000 ) ) ;
#112554 = ORIENTED_EDGE ( 'NONE', *, *, #97517, .F. ) ;
#112553 = LINE ( 'NONE', #231227, #236119 ) ;
#112556 = CARTESIAN_POINT ( 'NONE',  ( -20.54999999999999716, 1.115600667400684642E-11, -134.0000000000000284 ) ) ;
#112555 =( REPRESENTATION_RELATIONSHIP ('NONE','NONE', #36900, #141939 ) REPRESENTATION_RELATIONSHIP_WITH_TRANSFORMATION ( #87175 )SHAPE_REPRESENTATION_RELATIONSHIP( ) );
#112557 = DIRECTION ( 'NONE',  ( -1.000000000000000000, -7.304098846218134667E-16, 0.000000000000000000 ) ) ;
#112558 = DIRECTION ( 'NONE',  ( 1.000000000000000000, 0.000000000000000000, 0.000000000000000000 ) ) ;
#112559 = LINE ( 'NONE', #75989, #253299 ) ;
#112560 = DIRECTION ( 'NONE',  ( 0.000000000000000000, -6.467318590049456648E-15, 1.000000000000000000 ) ) ;
#112561 = EDGE_CURVE ( 'NONE', #173885, #111551, #12678, .T. ) ;
#112562 = EDGE_LOOP ( 'NONE', ( #84510, #183573, #119041, #206652 ) ) ;
#112563 = DIRECTION ( 'NONE',  ( 0.000000000000000000, 0.000000000000000000, -1.000000000000000000 ) ) ;
#112565 = ORIENTED_EDGE ( 'NONE', *, *, #143454, .F. ) ;
#112564 = AXIS2_PLACEMENT_3D ( 'NONE', #189802, #50266, #75014 ) ;
#112566 = CARTESIAN_POINT ( 'NONE',  ( 21.05000000000005400, 77.83551161375991967, -47.52760213295648839 ) ) ;
#112567 = EDGE_CURVE ( 'NONE', #188180, #75064, #255472, .T. ) ;
#112568 = ORIENTED_EDGE ( 'NONE', *, *, #137109, .F. ) ;
#112569 = CARTESIAN_POINT ( 'NONE',  ( 21.05000000000000071, 7.128833340093095217, -233.7327013124392749 ) ) ;
#112570 = ORIENTED_EDGE ( 'NONE', *, *, #4389, .T. ) ;
#112571 = DIRECTION ( 'NONE',  ( -1.000000000000000000, 0.000000000000000000, 0.000000000000000000 ) ) ;
#112572 = LINE ( 'NONE', #154306, #33404 ) ;
#112573 =( BOUNDED_SURFACE ( )  B_SPLINE_SURFACE ( 3, 2, ( 
 ( #39861, #155958, #235451 ),
 ( #136332, #37288, #77651 ),
 ( #157245, #98473, #20286 ),
 ( #178082, #119381, #198904 ) ),
 .UNSPECIFIED., .F., .F., .F. ) 
 B_SPLINE_SURFACE_WITH_KNOTS ( ( 4, 4 ),
 ( 3, 3 ),
 ( 3.658908243880891309, 4.712388980384689674 ),
 ( 0.000000000000000000, 1.000000000000000000 ),
 .UNSPECIFIED. ) 
 GEOMETRIC_REPRESENTATION_ITEM ( )  RATIONAL_B_SPLINE_SURFACE ( (
 ( 1.000000000000000000, 0.8984936768950106956, 1.000000000000000000),
 ( 1.000000000000000000, 0.8646876308618098861, 1.000000000000000000),
 ( 1.000000000000000000, 0.7953136715911073296, 1.000000000000000000),
 ( 1.000000000000000000, 0.7071067811866069697, 1.000000000000000000) ) ) 
 REPRESENTATION_ITEM ( '' )  SURFACE ( )  );
#112574 = DIRECTION ( 'NONE',  ( -1.000000000000000000, 0.000000000000000000, -0.000000000000000000 ) ) ;
#112575 = ORIENTED_EDGE ( 'NONE', *, *, #164519, .F. ) ;
#112576 = EDGE_CURVE ( 'NONE', #171400, #200447, #187455, .T. ) ;
#112577 = CARTESIAN_POINT ( 'NONE',  ( -16.84793658983432607, 9.949999999999985079, -12.73364667781021708 ) ) ;
#112578 = CARTESIAN_POINT ( 'NONE',  ( -21.05000000000000071, 4.193200906077805712, -212.0298262072164164 ) ) ;
#112579 = CARTESIAN_POINT ( 'NONE',  ( 20.94999999999999574, -1.835341550213255957, -112.0551512925630107 ) ) ;
#112580 = CARTESIAN_POINT ( 'NONE',  ( 20.95000000000005258, 87.75000000001122658, -30.02310748452481448 ) ) ;
#112581 = CARTESIAN_POINT ( 'NONE',  ( 18.59999999999997655, 67.23127455305835554, -235.8551265064784559 ) ) ;
#112582 = ORIENTED_EDGE ( 'NONE', *, *, #211975, .F. ) ;
#112583 = DIRECTION ( 'NONE',  ( -3.440080580676164606E-14, 0.8127272543710891695, -0.5826443254700338636 ) ) ;
#112584 = ORIENTED_EDGE ( 'NONE', *, *, #49650, .T. ) ;
#112586 = ORIENTED_EDGE ( 'NONE', *, *, #105097, .F. ) ;
#112585 = CYLINDRICAL_SURFACE ( 'NONE', #131448, 0.09999999999999939493 ) ;
#112587 = VERTEX_POINT ( 'NONE', #212565 ) ;
#112588 = CARTESIAN_POINT ( 'NONE',  ( 21.93340585898645401, 1.115541036281197940E-11, -59.67585297787184118 ) ) ;
#112589 = DIRECTION ( 'NONE',  ( 1.000000000000000000, 0.000000000000000000, 0.000000000000000000 ) ) ;
#112590 = DIRECTION ( 'NONE',  ( 0.000000000000000000, 0.000000000000000000, -1.000000000000000000 ) ) ;
#112591 = DIRECTION ( 'NONE',  ( 0.000000000000000000, 0.000000000000000000, 1.000000000000000000 ) ) ;
#112592 = AXIS2_PLACEMENT_3D ( 'NONE', #209656, #230510, #90983 ) ;
#112593 = EDGE_LOOP ( 'NONE', ( #120479, #164374, #186435, #124583 ) ) ;
#112594 = DIRECTION ( 'NONE',  ( 1.000000000000000000, -0.000000000000000000, -0.000000000000000000 ) ) ;
#112595 = DIRECTION ( 'NONE',  ( 1.734723475976817507E-14, 0.000000000000000000, -1.000000000000000000 ) ) ;
#112596 = ORIENTED_EDGE ( 'NONE', *, *, #167765, .T. ) ;
#112597 = EDGE_CURVE ( 'NONE', #196416, #183798, #183351, .T. ) ;
#112599 = ORIENTED_EDGE ( 'NONE', *, *, #7343, .T. ) ;
#112598 = CARTESIAN_POINT ( 'NONE',  ( 23.24999999999999289, 6.650000000011155876, -188.8499999999999659 ) ) ;
#112600 = CARTESIAN_POINT ( 'NONE',  ( -18.59999999999999787, 11.60000000001115872, -140.9282032302755852 ) ) ;
#112601 = CARTESIAN_POINT ( 'NONE',  ( -22.39999999999999858, 0.1000000000111554016, -167.4999999999999716 ) ) ;
#112602 = AXIS2_PLACEMENT_3D ( 'NONE', #248581, #49087, #51630 ) ;
#112603 = EDGE_LOOP ( 'NONE', ( #244989, #8915, #57693, #155555 ) ) ;
#112604 = ADVANCED_FACE ( 'NONE', ( #14379 ), #93881, .T. ) ;
#112605 = DIRECTION ( 'NONE',  ( 0.000000000000000000, -7.487053152578134969E-15, 1.000000000000000000 ) ) ;
#112606 = VERTEX_POINT ( 'NONE', #160306 ) ;
#112607 = CARTESIAN_POINT ( 'NONE',  ( -18.59999999999999787, 1.866714910068465239, -112.2526752462820525 ) ) ;
#112608 = VECTOR ( 'NONE', #41972, 1000.000000000000000 ) ;
#112609 = DIRECTION ( 'NONE',  ( 1.000000000000000000, 0.000000000000000000, 0.000000000000000000 ) ) ;
#112610 = CIRCLE ( 'NONE', #62720, 11.75000000000000533 ) ;
#112611 = ADVANCED_FACE ( 'NONE', ( #101549 ), #18188, .T. ) ;
#112612 = DIRECTION ( 'NONE',  ( -1.000000000000000000, 0.000000000000000000, 0.000000000000000000 ) ) ;
#112613 = ADVANCED_FACE ( 'NONE', ( #81986 ), #108342, .T. ) ;
#112614 = VECTOR ( 'NONE', #203263, 1000.000000000000000 ) ;
#112615 = AXIS2_PLACEMENT_3D ( 'NONE', #203710, #121628, #62910 ) ;
#112616 = CIRCLE ( 'NONE', #254071, 0.09999999999999939493 ) ;
#112617 = ORIENTED_EDGE ( 'NONE', *, *, #36417, .F. ) ;
#112619 = CARTESIAN_POINT ( 'NONE',  ( 20.95263205890653779, 67.10425989211756814, -61.03359907758274971 ) ) ;
#112618 = TOROIDAL_SURFACE ( 'NONE', #172, 7.800000000000000711, 0.1000000000000000056 ) ;
#112620 = CIRCLE ( 'NONE', #95840, 0.09999999999998898659 ) ;
#112621 = EDGE_LOOP ( 'NONE', ( #98085, #28919, #6932, #191662 ) ) ;
#112622 = CYLINDRICAL_SURFACE ( 'NONE', #18667, 0.1000000000000028644 ) ;
#112625 = EDGE_CURVE ( 'NONE', #64533, #165923, #243662, .T. ) ;
#112624 = ORIENTED_EDGE ( 'NONE', *, *, #102042, .F. ) ;
#112623 = CARTESIAN_POINT ( 'NONE',  ( 20.94999999999999574, 8.926614585098251453, -142.4716830192231498 ) ) ;
#112626 = CARTESIAN_POINT ( 'NONE',  ( -20.94999999999994245, 67.85000000001119247, -3.123107484524795474 ) ) ;
#112627 = CARTESIAN_POINT ( 'NONE',  ( 19.99999999999998934, 64.25000000001250555, -178.6731074845244507 ) ) ;
#112628 = DIRECTION ( 'NONE',  ( 1.000000000000000000, 0.000000000000000000, 0.000000000000000000 ) ) ;
#112629 = CARTESIAN_POINT ( 'NONE',  ( 21.05000000000000071, 64.40000000001175806, -76.45131071479988805 ) ) ;
#112630 = FACE_OUTER_BOUND ( 'NONE', #87345, .T. ) ;
#112631 = ADVANCED_FACE ( 'NONE', ( #65021 ), #229895, .T. ) ;
#112632 = CARTESIAN_POINT ( 'NONE',  ( -21.05000000000000071, 72.91131461869652242, -214.9116992594219369 ) ) ;
#112633 = EDGE_CURVE ( 'NONE', #245252, #88959, #83358, .T. ) ;
#112634 = CARTESIAN_POINT ( 'NONE',  ( 21.13498764882293557, 6.495618143485025975, -66.99834360526871535 ) ) ;
#112635 = AXIS2_PLACEMENT_3D ( 'NONE', #29999, #40899, #88629 ) ;
#112637 = ORIENTED_EDGE ( 'NONE', *, *, #256666, .T. ) ;
#112636 = CARTESIAN_POINT ( 'NONE',  ( -21.12642695952773764, 69.62434007797698143, -136.6220107677137037 ) ) ;
#112639 = EDGE_CURVE ( 'NONE', #52565, #220745, #104219, .T. ) ;
#112638 = CARTESIAN_POINT ( 'NONE',  ( 21.05000000000000071, 84.73084112150763758, -160.4250327655399531 ) ) ;
#112640 = CARTESIAN_POINT ( 'NONE',  ( -23.15000000000000213, 62.92003201576280702, -207.2439188921395612 ) ) ;
#112642 = EDGE_CURVE ( 'NONE', #134912, #173389, #159026, .T. ) ;
#112641 = CARTESIAN_POINT ( 'NONE',  ( -18.49372193242234275, 85.44248452336977095, -62.75832622448970710 ) ) ;
#112643 = CARTESIAN_POINT ( 'NONE',  ( 20.94999999999999574, -11.64999999998883595, -69.90000000000004832 ) ) ;
#112644 = EDGE_CURVE ( 'NONE', #9598, #185818, #70951, .T. ) ;
#112645 = ORIENTED_EDGE ( 'NONE', *, *, #120984, .T. ) ;
#112646 = FACE_OUTER_BOUND ( 'NONE', #224859, .T. ) ;
#112647 = AXIS2_PLACEMENT_3D ( 'NONE', #58759, #100447, #216572 ) ;
#112648 = DIRECTION ( 'NONE',  ( 0.000000000000000000, 0.8814952561688430555, -0.4721928772777346239 ) ) ;
#112649 = AXIS2_PLACEMENT_3D ( 'NONE', #118477, #78037, #157630 ) ;
#112650 = CARTESIAN_POINT ( 'NONE',  ( 20.94999999999999929, -9.499999999988844479, -57.10603087734755690 ) ) ;
#112651 = EDGE_LOOP ( 'NONE', ( #127569, #160590, #251325, #30923 ) ) ;
#112652 = AXIS2_PLACEMENT_3D ( 'NONE', #141985, #42903, #105399 ) ;
#112653 = LINE ( 'NONE', #190930, #101884 ) ;
#112654 =( BOUNDED_SURFACE ( )  B_SPLINE_SURFACE ( 3, 2, ( 
 ( #516, #80031, #140019 ),
 ( #163464, #219568, #40975 ),
 ( #200027, #229859, #51185 ),
 ( #150334, #129479, #189456 ),
 ( #228585, #146443, #207745 ),
 ( #89048, #249433, #206440 ),
 ( #47345, #69520, #48638 ),
 ( #231167, #52484, #27837 ),
 ( #49928, #209009, #30389 ),
 ( #128193, #190764, #225963 ),
 ( #86459, #107332, #29138 ),
 ( #149057, #210306, #186902 ) ),
 .UNSPECIFIED., .F., .F., .F. ) 
 B_SPLINE_SURFACE_WITH_KNOTS ( ( 4, 2, 2, 2, 2, 4 ),
 ( 3, 3 ),
 ( 3.174653483277205090, 3.943930578431714018, 4.713207673586222946, 5.482484768740731873, 5.867123316317986337, 6.251761863895240801 ),
 ( 0.000000000000000000, 1.000000000000000000 ),
 .UNSPECIFIED. ) 
 GEOMETRIC_REPRESENTATION_ITEM ( )  RATIONAL_B_SPLINE_SURFACE ( (
 ( 1.000000000000000000, 0.8659465255642289083, 1.000000000000000000),
 ( 1.000000000000000000, 0.8648614068487607831, 1.000000000000000000),
 ( 1.000000000000000000, 0.8489031841324650163, 1.000000000000000000),
 ( 1.000000000000000000, 0.7927507630160894880, 1.000000000000000000),
 ( 1.000000000000000000, 0.7523013859007505744, 1.000000000000000000),
 ( 1.000000000000000000, 0.6616226951199137840, 1.000000000000000000),
 ( 1.000000000000000000, 0.6112214368721295976, 1.000000000000000000),
 ( 1.000000000000000000, 0.5507684314499833311, 1.000000000000000000),
 ( 1.000000000000000000, 0.5333267243194751428, 1.000000000000000000),
 ( 1.000000000000000000, 0.5084565446437981917, 1.000000000000000000),
 ( 1.000000000000000000, 0.5010722703481732543, 1.000000000000000000),
 ( 1.000000000000000000, 0.5001234037139490329, 1.000000000000000000) ) ) 
 REPRESENTATION_ITEM ( '' )  SURFACE ( )  );
#112655 = DIRECTION ( 'NONE',  ( -0.000000000000000000, 0.000000000000000000, -1.000000000000000000 ) ) ;
#112657 = ORIENTED_EDGE ( 'NONE', *, *, #125868, .T. ) ;
#112656 = AXIS2_PLACEMENT_3D ( 'NONE', #44156, #220231, #179824 ) ;
#112658 = CARTESIAN_POINT ( 'NONE',  ( 20.94999999999999929, 74.34961279258810407, -232.6661986760551315 ) ) ;
#112659 = EDGE_CURVE ( 'NONE', #84649, #4376, #4261, .T. ) ;
#112660 = ORIENTED_EDGE ( 'NONE', *, *, #233241, .T. ) ;
#112661 = ADVANCED_FACE ( 'NONE', ( #70192 ), #89709, .T. ) ;
#112662 = CARTESIAN_POINT ( 'NONE',  ( 21.05000000000000071, 65.27628288308592630, -124.3468678833861958 ) ) ;
#112664 = ORIENTED_EDGE ( 'NONE', *, *, #218201, .F. ) ;
#112663 = CARTESIAN_POINT ( 'NONE',  ( 21.07094088545369814, 75.90110629745997528, -142.8432747064414627 ) ) ;
#112665 = DIRECTION ( 'NONE',  ( 1.000000000000000000, -1.186688945009010077E-16, -8.286604613020808509E-31 ) ) ;
#112666 = ORIENTED_EDGE ( 'NONE', *, *, #113254, .T. ) ;
#112667 = VECTOR ( 'NONE', #242619, 1000.000000000000114 ) ;
#112668 = CARTESIAN_POINT ( 'NONE',  ( -23.49999999999994316, 77.73640333653723644, -47.54092689884382850 ) ) ;
#112669 = EDGE_LOOP ( 'NONE', ( #169553, #132545, #129730, #148360 ) ) ;
#112672 = EDGE_CURVE ( 'NONE', #178157, #17731, #25151, .T. ) ;
#112671 = ORIENTED_EDGE ( 'NONE', *, *, #176528, .T. ) ;
#112670 = EDGE_LOOP ( 'NONE', ( #56507, #30684, #69518, #64872 ) ) ;
#112673 = DIRECTION ( 'NONE',  ( 0.000000000000000000, -6.982962677686266711E-15, 1.000000000000000000 ) ) ;
#112674 = ORIENTED_EDGE ( 'NONE', *, *, #202847, .F. ) ;
#112675 = LINE ( 'NONE', #149249, #135390 ) ;
#112676 = VECTOR ( 'NONE', #256734, 1000.000000000000000 ) ;
#112677 = ORIENTED_EDGE ( 'NONE', *, *, #30368, .T. ) ;
#112678 = AXIS2_PLACEMENT_3D ( 'NONE', #8861, #145782, #222753 ) ;
#112679 = CIRCLE ( 'NONE', #46025, 0.09999999999999939493 ) ;
#112680 = VERTEX_POINT ( 'NONE', #106703 ) ;
#112681 = FACE_OUTER_BOUND ( 'NONE', #56726, .T. ) ;
#112682 = CARTESIAN_POINT ( 'NONE',  ( -18.40000000000000213, 70.35000000001255671, -182.6731074845243938 ) ) ;
#112683 = CYLINDRICAL_SURFACE ( 'NONE', #32397, 0.09999999999999939493 ) ;
#112684 = ORIENTED_EDGE ( 'NONE', *, *, #230608, .T. ) ;
#112685 = CYLINDRICAL_SURFACE ( 'NONE', #116104, 0.09999999999998898659 ) ;
#112686 = CARTESIAN_POINT ( 'NONE',  ( -20.94999999999999929, 74.83729825007388570, -94.92310748452432279 ) ) ;
#112687 = CARTESIAN_POINT ( 'NONE',  ( 18.49999999999999645, 72.02722222756958104, -225.1832529173024398 ) ) ;
#112689 = ORIENTED_EDGE ( 'NONE', *, *, #243343, .F. ) ;
#112688 = EDGE_CURVE ( 'NONE', #249092, #252440, #250172, .T. ) ;
#112690 = CARTESIAN_POINT ( 'NONE',  ( -21.14999999999999858, 0.09779029131994770863, -94.24218538952392521 ) ) ;
#112691 = CARTESIAN_POINT ( 'NONE',  ( -20.54999999999999716, 36.65892442174935439, -249.5511627012433848 ) ) ;
#112692 = AXIS2_PLACEMENT_3D ( 'NONE', #123559, #145672, #223918 ) ;
#112693 = EDGE_CURVE ( 'NONE', #69658, #78788, #187647, .T. ) ;
#112694 = ORIENTED_EDGE ( 'NONE', *, *, #191024, .T. ) ;
#112695 = CARTESIAN_POINT ( 'NONE',  ( -16.95709691156223542, 14.15686132874403214, -219.2452453564496295 ) ) ;
#112696 = ORIENTED_EDGE ( 'NONE', *, *, #11743, .F. ) ;
#112697 = CARTESIAN_POINT ( 'NONE',  ( -18.58693740092158109, -7.674815071417180334, -209.9633246597199445 ) ) ;
#112698 = ORIENTED_EDGE ( 'NONE', *, *, #126416, .T. ) ;
#112699 = LINE ( 'NONE', #93121, #13882 ) ;
#112700 = PLANE ( 'NONE',  #81307 ) ;
#112701 = EDGE_LOOP ( 'NONE', ( #49496, #216425, #5962, #181684 ) ) ;
#112702 = EDGE_LOOP ( 'NONE', ( #92813, #31406, #194175, #82373 ) ) ;
#112704 = ADVANCED_FACE ( 'NONE', ( #67594 ), #148430, .T. ) ;
#112703 = CARTESIAN_POINT ( 'NONE',  ( 20.94999999999999929, 74.92681270650359693, -207.4801605588535551 ) ) ;
#112705 = DIRECTION ( 'NONE',  ( -1.000000000000000000, -8.673617379884087537E-15, 0.000000000000000000 ) ) ;
#112706 = ORIENTED_EDGE ( 'NONE', *, *, #46537, .F. ) ;
#112707 = VERTEX_POINT ( 'NONE', #25914 ) ;
#112708 = LINE ( 'NONE', #9741, #189548 ) ;
#112709 = ADVANCED_FACE ( 'NONE', ( #168026 ), #250088, .F. ) ;
#112710 = CARTESIAN_POINT ( 'NONE',  ( -18.79999999999999716, 1.212568896937007645, -7.900000000000000355 ) ) ;
#112711 = EDGE_LOOP ( 'NONE', ( #230834, #31060, #197095, #11288 ) ) ;
#112712 = CIRCLE ( 'NONE', #245985, 3.900000000000000799 ) ;
#112713 = TOROIDAL_SURFACE ( 'NONE', #21156, 11.70000000000000639, 0.1000000000000000056 ) ;
#112714 = EDGE_CURVE ( 'NONE', #229311, #199945, #108012, .T. ) ;
#112715 = ORIENTED_EDGE ( 'NONE', *, *, #44638, .T. ) ;
#112716 = EDGE_CURVE ( 'NONE', #56541, #248319, #246238, .T. ) ;
#112719 = ADVANCED_FACE ( 'NONE', ( #247519 ), #204527, .T. ) ;
#112718 = EDGE_CURVE ( 'NONE', #158507, #93493, #241786, .T. ) ;
#112717 = PLANE ( 'NONE',  #234869 ) ;
#112720 = CARTESIAN_POINT ( 'NONE',  ( -23.25000000000000000, 67.23127455305835554, -235.8551265064784559 ) ) ;
#112721 = DIRECTION ( 'NONE',  ( 0.000000000000000000, 0.000000000000000000, 1.000000000000000000 ) ) ;
#112723 = ORIENTED_EDGE ( 'NONE', *, *, #198684, .T. ) ;
#112722 = DIRECTION ( 'NONE',  ( 0.000000000000000000, 1.000000000000000000, 6.982962677686266711E-15 ) ) ;
#112724 = DIRECTION ( 'NONE',  ( -1.000000000000000000, 0.000000000000000000, 0.000000000000000000 ) ) ;
#112725 = AXIS2_PLACEMENT_3D ( 'NONE', #23714, #238880, #223148 ) ;
#112726 = CARTESIAN_POINT ( 'NONE',  ( 18.49999999999999289, 65.79142135624927334, -111.7559501969989668 ) ) ;
#112728 = CARTESIAN_POINT ( 'NONE',  ( -21.05000000000000071, 77.83534155023627932, -91.36795619196132634 ) ) ;
#112727 = CARTESIAN_POINT ( 'NONE',  ( 21.11825140030105530, 75.99279637937891607, -75.96851504994447168 ) ) ;
#112729 = CARTESIAN_POINT ( 'NONE',  ( 21.72449340488910252, 10.28395627750227703, -46.15000000000001279 ) ) ;
#112730 = DIRECTION ( 'NONE',  ( 0.000000000000000000, 0.000000000000000000, -1.000000000000000000 ) ) ;
#112731 = CARTESIAN_POINT ( 'NONE',  ( 20.94999999999999929, 7.128833340094563376, -233.7327013124401276 ) ) ;
#112732 = CARTESIAN_POINT ( 'NONE',  ( -21.05000000000000071, 76.08579911628598325, -176.4370863660123518 ) ) ;
#112733 = EDGE_CURVE ( 'NONE', #43374, #49193, #229333, .T. ) ;
#112734 = EDGE_CURVE ( 'NONE', #61669, #227850, #8561, .T. ) ;
#112735 = EDGE_LOOP ( 'NONE', ( #164296, #127087, #116439, #170564 ) ) ;
#112736 = EDGE_CURVE ( 'NONE', #117217, #48866, #133632, .T. ) ;
#112737 = VERTEX_POINT ( 'NONE', #10205 ) ;
#112738 = AXIS2_PLACEMENT_3D ( 'NONE', #24044, #223490, #60566 ) ;
#112739 = EDGE_CURVE ( 'NONE', #5127, #253511, #125278, .T. ) ;
#112740 = CARTESIAN_POINT ( 'NONE',  ( 20.94999999999999574, -11.48912529306490349, -70.10000000000005116 ) ) ;
#112741 = DIRECTION ( 'NONE',  ( 0.000000000000000000, -0.2617529984165031243, -0.9651348961777157509 ) ) ;
#112742 = ADVANCED_FACE ( 'NONE', ( #184976 ), #6325, .T. ) ;
#112743 = ORIENTED_EDGE ( 'NONE', *, *, #6689, .T. ) ;
#112744 = CIRCLE ( 'NONE', #216791, 0.09999999999999939493 ) ;
#112745 = PRESENTATION_STYLE_ASSIGNMENT (( #16236 ) ) ;
#112746 = CARTESIAN_POINT ( 'NONE',  ( -16.89268316805465986, 63.08557629953710943, -213.1216189793661329 ) ) ;
#112747 = AXIS2_PLACEMENT_3D ( 'NONE', #118421, #60989, #180953 ) ;
#112748 = CARTESIAN_POINT ( 'NONE',  ( 21.05000000000000071, 76.00000000001237765, -170.0231074845243597 ) ) ;
#112749 = VERTEX_POINT ( 'NONE', #205820 ) ;
#112750 = EDGE_LOOP ( 'NONE', ( #174976, #156747, #187369, #27264, #155370 ) ) ;
#112751 = CARTESIAN_POINT ( 'NONE',  ( 20.94999999999999574, -11.64999999998883595, -137.1000000000000227 ) ) ;
#112752 = DIRECTION ( 'NONE',  ( 1.000000000000000000, 0.000000000000000000, 0.000000000000000000 ) ) ;
#112753 = ORIENTED_EDGE ( 'NONE', *, *, #229731, .F. ) ;
#112754 = AXIS2_PLACEMENT_3D ( 'NONE', #242692, #105728, #240145 ) ;
#112755 = EDGE_CURVE ( 'NONE', #120584, #79652, #166730, .T. ) ;
#112756 = CYLINDRICAL_SURFACE ( 'NONE', #224416, 0.1000000000000024342 ) ;
#112758 = ORIENTED_EDGE ( 'NONE', *, *, #250771, .T. ) ;
#112757 = DIRECTION ( 'NONE',  ( 0.000000000000000000, -1.000000000000000000, 0.000000000000000000 ) ) ;
#112759 = CARTESIAN_POINT ( 'NONE',  ( -21.07928932188134041, 75.90110485435778287, -142.8516241409176075 ) ) ;
#112760 = EDGE_CURVE ( 'NONE', #215026, #12008, #175203, .T. ) ;
#112762 = VERTEX_POINT ( 'NONE', #157438 ) ;
#112761 = DIRECTION ( 'NONE',  ( 2.952720810173288126E-16, -0.4721928772777345684, -0.8814952561688429444 ) ) ;
#112763 = CARTESIAN_POINT ( 'NONE',  ( 23.14999999999999147, 4.150000000011154988, -100.5000000000000284 ) ) ;
#112764 = CARTESIAN_POINT ( 'NONE',  ( -20.54999999999999716, -9.399999999988846611, -90.60603087734760663 ) ) ;
#112765 = CYLINDRICAL_SURFACE ( 'NONE', #15306, 0.09999999999999939493 ) ;
#112766 = DIRECTION ( 'NONE',  ( 0.000000000000000000, 1.000000000000000000, -0.000000000000000000 ) ) ;
#112767 = ADVANCED_FACE ( 'NONE', ( #132715 ), #195269, .F. ) ;
#112769 = CARTESIAN_POINT ( 'NONE',  ( 20.95512828230152280, 8.876151312336450161, -179.7024302655030965 ) ) ;
#112768 = LINE ( 'NONE', #249711, #36693 ) ;
#112770 = DIRECTION ( 'NONE',  ( 1.000000000000000000, 0.000000000000000000, 0.000000000000000000 ) ) ;
#112772 = LINE ( 'NONE', #107961, #162152 ) ;
#112771 = AXIS2_PLACEMENT_3D ( 'NONE', #169061, #9944, #52914 ) ;
#112773 = CARTESIAN_POINT ( 'NONE',  ( -18.33981767444326039, 85.56957578981658230, -163.2039456407995317 ) ) ;
#112774 = DIRECTION ( 'NONE',  ( 0.000000000000000000, -6.517943393102682774E-15, 1.000000000000000000 ) ) ;
#112775 = LINE ( 'NONE', #252266, #55247 ) ;
#112776 = CIRCLE ( 'NONE', #191913, 0.1000000000000001305 ) ;
#112777 = ORIENTED_EDGE ( 'NONE', *, *, #110025, .F. ) ;
#112779 = DIRECTION ( 'NONE',  ( 1.000000000000000000, 0.000000000000000000, 0.000000000000000000 ) ) ;
#112778 = AXIS2_PLACEMENT_3D ( 'NONE', #172318, #234810, #17067 ) ;
#112780 = ORIENTED_EDGE ( 'NONE', *, *, #26181, .F. ) ;
#112782 = DIRECTION ( 'NONE',  ( -0.000000000000000000, 0.01283462868039629209, -0.9999176327611372095 ) ) ;
#112781 = CIRCLE ( 'NONE', #54512, 0.09999999999999939493 ) ;
#112783 = ORIENTED_EDGE ( 'NONE', *, *, #94363, .F. ) ;
#112784 = EDGE_CURVE ( 'NONE', #151804, #10431, #167005, .T. ) ;
#112785 = CARTESIAN_POINT ( 'NONE',  ( 21.05000000000000071, 77.84908441863908024, -124.8670969630771594 ) ) ;
#112786 = VECTOR ( 'NONE', #188709, 1000.000000000000000 ) ;
#112787 = AXIS2_PLACEMENT_3D ( 'NONE', #237991, #215848, #118052 ) ;
#112788 = VERTEX_POINT ( 'NONE', #236933 ) ;
#112789 = CARTESIAN_POINT ( 'NONE',  ( -21.05000000000000071, 30.78798680020884504, -252.2006866936654319 ) ) ;
#112790 = EDGE_CURVE ( 'NONE', #4454, #256760, #233114, .T. ) ;
#112792 = VERTEX_POINT ( 'NONE', #113139 ) ;
#112791 = AXIS2_PLACEMENT_3D ( 'NONE', #162884, #123738, #6335 ) ;
#112793 = AXIS2_PLACEMENT_3D ( 'NONE', #243808, #182575, #100420 ) ;
#112794 = AXIS2_PLACEMENT_3D ( 'NONE', #235640, #111866, #131411 ) ;
#112795 = ORIENTED_EDGE ( 'NONE', *, *, #85503, .F. ) ;
#112796 = VECTOR ( 'NONE', #110545, 1000.000000000000000 ) ;
#112797 = AXIS2_PLACEMENT_3D ( 'NONE', #231818, #250084, #230527 ) ;
#112798 = DIRECTION ( 'NONE',  ( 1.000000000000000000, 0.000000000000000000, -0.000000000000000000 ) ) ;
#112799 = CARTESIAN_POINT ( 'NONE',  ( -20.54999999999999716, 76.00000000001169553, -67.62310748452431142 ) ) ;
#112800 = DIRECTION ( 'NONE',  ( 0.000000000000000000, 0.9126074666063769270, 0.4088369013363280513 ) ) ;
#112801 = CARTESIAN_POINT ( 'NONE',  ( 13.22461703343584816, 27.73642831988484758, -234.0663351390819571 ) ) ;
#112802 = CARTESIAN_POINT ( 'NONE',  ( -21.14999999999999858, 31.94635157770351341, -238.7871412784868994 ) ) ;
#112803 = DIRECTION ( 'NONE',  ( 0.000000000000000000, 0.6728971962616697722, 0.7397360091702875895 ) ) ;
#112804 = CARTESIAN_POINT ( 'NONE',  ( -14.87779219673429054, 9.430633469083952392, -82.23176579482412762 ) ) ;
#112806 = ORIENTED_EDGE ( 'NONE', *, *, #59897, .T. ) ;
#112805 = CARTESIAN_POINT ( 'NONE',  ( -21.65000000000000213, 7.250000000011139534, -180.1499999999999773 ) ) ;
#112808 = CARTESIAN_POINT ( 'NONE',  ( -22.14074124539699540, 65.20130011066974873, -242.9616211335017226 ) ) ;
#112807 = FACE_OUTER_BOUND ( 'NONE', #136798, .T. ) ;
#112809 = PLANE ( 'NONE',  #211453 ) ;
#112810 = ORIENTED_EDGE ( 'NONE', *, *, #157994, .T. ) ;
#112811 = CARTESIAN_POINT ( 'NONE',  ( -18.47079683080347223, -9.471664105233724484, -174.6088605409921968 ) ) ;
#112812 = CARTESIAN_POINT ( 'NONE',  ( 21.05543885634738288, 8.775771046858691804, -146.1843844707147184 ) ) ;
#112813 = DIRECTION ( 'NONE',  ( 0.000000000000000000, 0.000000000000000000, -1.000000000000000000 ) ) ;
#112814 = ORIENTED_EDGE ( 'NONE', *, *, #155124, .T. ) ;
#112815 = CIRCLE ( 'NONE', #67019, 0.1000000000000002554 ) ;
#112816 = DIRECTION ( 'NONE',  ( 0.000000000000000000, 0.9651348961777149738, -0.2617529984165058998 ) ) ;
#112817 = DIRECTION ( 'NONE',  ( 1.000000000000000000, -3.265361837132813093E-16, -2.280189983783949500E-30 ) ) ;
#112818 = CARTESIAN_POINT ( 'NONE',  ( -18.45068461519105796, 78.23730666619897534, -231.5159245159509567 ) ) ;
#112819 = ORIENTED_EDGE ( 'NONE', *, *, #235713, .F. ) ;
#112820 = ORIENTED_EDGE ( 'NONE', *, *, #15226, .F. ) ;
#112821 = CYLINDRICAL_SURFACE ( 'NONE', #145055, 0.09999999999999939493 ) ;
#112822 = CARTESIAN_POINT ( 'NONE',  ( -18.56579813702276027, 10.33025634372637569, -173.0870929282638997 ) ) ;
#112823 = FACE_OUTER_BOUND ( 'NONE', #250616, .T. ) ;
#112824 = CARTESIAN_POINT ( 'NONE',  ( -23.15000000000000213, 62.33780030268294325, -247.9091949332902516 ) ) ;
#112825 = ORIENTED_EDGE ( 'NONE', *, *, #108538, .T. ) ;
#112826 = VECTOR ( 'NONE', #85694, 1000.000000000000000 ) ;
#112827 = DIRECTION ( 'NONE',  ( 0.000000000000000000, 0.000000000000000000, -1.000000000000000000 ) ) ;
#112829 = EDGE_CURVE ( 'NONE', #121003, #62333, #191938, .T. ) ;
#112828 = DIRECTION ( 'NONE',  ( 0.000000000000000000, -0.5826443254699606999, -0.8127272543711416830 ) ) ;
#112830 = CARTESIAN_POINT ( 'NONE',  ( 20.12500000000000355, 9.258049272928479567, -75.36333883714247861 ) ) ;
#112831 = CARTESIAN_POINT ( 'NONE',  ( -18.40000000000000213, 61.13752757784637026, -224.6182967272386009 ) ) ;
#112832 = CIRCLE ( 'NONE', #50269, 0.09999999999999939493 ) ;
#112833 = DIRECTION ( 'NONE',  ( 0.000000000000000000, 0.000000000000000000, -1.000000000000000000 ) ) ;
#112834 = AXIS2_PLACEMENT_3D ( 'NONE', #205460, #26866, #106346 ) ;
#112836 = ORIENTED_EDGE ( 'NONE', *, *, #194001, .F. ) ;
#112835 = CARTESIAN_POINT ( 'NONE',  ( -16.93234230245721861, 66.00189262946472013, -82.10541720285813483 ) ) ;
#112837 = CARTESIAN_POINT ( 'NONE',  ( 18.59999999999999432, 77.16270174995010223, -128.5231074845242745 ) ) ;
#112838 = CARTESIAN_POINT ( 'NONE',  ( 20.94999999999999929, -9.499999999988844479, -124.1060308773475924 ) ) ;
#112839 = DIRECTION ( 'NONE',  ( 1.000000000000000000, 0.000000000000000000, 0.000000000000000000 ) ) ;
#112840 = DIRECTION ( 'NONE',  ( -1.000000000000000000, 0.000000000000000000, -0.000000000000000000 ) ) ;
#112841 = ADVANCED_FACE ( 'NONE', ( #156147 ), #33654, .F. ) ;
#112842 = LINE ( 'NONE', #172865, #233608 ) ;
#112844 = EDGE_LOOP ( 'NONE', ( #175690, #206581, #168607, #82904, #121070 ) ) ;
#112843 = DIRECTION ( 'NONE',  ( 0.000000000000000000, 0.000000000000000000, -1.000000000000000000 ) ) ;
#112845 = DIRECTION ( 'NONE',  ( 0.000000000000000000, -7.172728831056617961E-15, 1.000000000000000000 ) ) ;
#112846 = DIRECTION ( 'NONE',  ( 1.000000000000000000, 0.000000000000000000, 0.000000000000000000 ) ) ;
#112847 = DIRECTION ( 'NONE',  ( 0.000000000000000000, 6.982962677686266711E-15, -1.000000000000000000 ) ) ;
#112848 = EDGE_CURVE ( 'NONE', #90469, #180736, #79461, .T. ) ;
#112849 = ORIENTED_EDGE ( 'NONE', *, *, #131884, .F. ) ;
#112850 = DIRECTION ( 'NONE',  ( 0.000000000000000000, 0.008583690987128059571, -0.9999631594459056361 ) ) ;
#112851 = DIRECTION ( 'NONE',  ( 1.000000000000000000, 0.000000000000000000, -0.000000000000000000 ) ) ;
#112852 = CARTESIAN_POINT ( 'NONE',  ( -23.15000000000000213, 19.89303971870268839, -235.6353404070293038 ) ) ;
#112853 = LINE ( 'NONE', #197510, #91881 ) ;
#112855 = CIRCLE ( 'NONE', #142065, 4.000000000000003553 ) ;
#112854 = DIRECTION ( 'NONE',  ( 0.000000000000000000, 0.000000000000000000, 1.000000000000000000 ) ) ;
#112856 = EDGE_CURVE ( 'NONE', #176023, #155495, #200101, .T. ) ;
#112858 = AXIS2_PLACEMENT_3D ( 'NONE', #202851, #106302, #84136 ) ;
#112857 = CARTESIAN_POINT ( 'NONE',  ( 0.9000000000000547562, 67.75000000001118394, -10.02310748452479139 ) ) ;
#112859 = ORIENTED_EDGE ( 'NONE', *, *, #4878, .F. ) ;
#112860 = EDGE_LOOP ( 'NONE', ( #162581, #233914, #139166, #163638 ) ) ;
#112861 = AXIS2_PLACEMENT_3D ( 'NONE', #56270, #114979, #175004 ) ;
#112862 = ADVANCED_FACE ( 'NONE', ( #93572 ), #174449, .F. ) ;
#112863 = CARTESIAN_POINT ( 'NONE',  ( 21.05000000000000071, 84.66355140188075268, -59.99900636645695329 ) ) ;
#112864 = CARTESIAN_POINT ( 'NONE',  ( -17.11825945287481687, 66.05000000001201954, -115.7731074845243739 ) ) ;
#112865 = ADVANCED_FACE ( 'NONE', ( #55690 ), #14059, .T. ) ;
#112866 = CARTESIAN_POINT ( 'NONE',  ( -33.72168855820451938, 30.20632856012699108, -234.8070450048000737 ) ) ;
#112867 = DIRECTION ( 'NONE',  ( 0.000000000000000000, 0.000000000000000000, -1.000000000000000000 ) ) ;
#112868 = ADVANCED_FACE ( 'NONE', ( #192688 ), #56983, .F. ) ;
#112869 = CARTESIAN_POINT ( 'NONE',  ( 18.49999999999999289, 11.65000000001115943, -155.7499999999999716 ) ) ;
#112870 = FACE_OUTER_BOUND ( 'NONE', #60639, .T. ) ;
#112871 = ADVANCED_FACE ( 'NONE', ( #37469 ), #94847, .T. ) ;
#112872 = AXIS2_PLACEMENT_3D ( 'NONE', #121664, #82480, #81206 ) ;
#112873 = LINE ( 'NONE', #55426, #91332 ) ;
#112874 = FACE_OUTER_BOUND ( 'NONE', #183851, .T. ) ;
#112875 = B_SPLINE_CURVE_WITH_KNOTS ( 'NONE', 3,
 ( #213855, #56033, #54768, #196844, #19520, #99009, #256774, #159045 ),
 .UNSPECIFIED., .F., .F.,
 ( 4, 2, 2, 4 ),
 ( 0.000000000000000000, 0.0002181133598169196985, 0.0003271700397253618346, 0.0004362267196338040520 ),
 .UNSPECIFIED. ) ;
#112876 = ORIENTED_EDGE ( 'NONE', *, *, #137237, .T. ) ;
#112877 = DIRECTION ( 'NONE',  ( 0.000000000000000000, 1.000000000000000000, -3.469446951953635015E-14 ) ) ;
#112878 = EDGE_LOOP ( 'NONE', ( #41841, #244600, #255361, #96794 ) ) ;
#112879 = FACE_OUTER_BOUND ( 'NONE', #99220, .T. ) ;
#112880 = CARTESIAN_POINT ( 'NONE',  ( 21.05000000000000071, 10.48459288119459032, -7.456713570584089013 ) ) ;
#112882 = ORIENTED_EDGE ( 'NONE', *, *, #216611, .F. ) ;
#112881 = LINE ( 'NONE', #150726, #153586 ) ;
#112883 = CYLINDRICAL_SURFACE ( 'NONE', #98891, 12.87499999999999822 ) ;
#112884 = DIRECTION ( 'NONE',  ( 0.000000000000000000, -6.454785026890510900E-15, 1.000000000000000000 ) ) ;
#112885 = CARTESIAN_POINT ( 'NONE',  ( 18.60000000000000142, 85.48068669529062902, -62.58199231576637089 ) ) ;
#112886 = FACE_OUTER_BOUND ( 'NONE', #73438, .T. ) ;
#112887 = ORIENTED_EDGE ( 'NONE', *, *, #96499, .T. ) ;
#112888 = EDGE_CURVE ( 'NONE', #228673, #57380, #146111, .T. ) ;
#112889 = PLANE ( 'NONE',  #66462 ) ;
#112890 = AXIS2_PLACEMENT_3D ( 'NONE', #49080, #128640, #15107 ) ;
#112891 = CARTESIAN_POINT ( 'NONE',  ( 18.53691006697079757, 65.69784844286128589, -145.3209087672253474 ) ) ;
#112892 = CIRCLE ( 'NONE', #200381, 0.1000000000000028644 ) ;
#112893 = TOROIDAL_SURFACE ( 'NONE', #167094, 1.900000000000002576, 0.1000000000000000056 ) ;
#112894 = DIRECTION ( 'NONE',  ( -1.000000000000000000, 0.000000000000000000, 0.000000000000000000 ) ) ;
#112895 = CARTESIAN_POINT ( 'NONE',  ( 23.25000000000000000, -9.599999999988845900, -76.89396912265249284 ) ) ;
#112896 = AXIS2_PLACEMENT_3D ( 'NONE', #21130, #257090, #238867 ) ;
#112897 = CARTESIAN_POINT ( 'NONE',  ( 20.94999999999999929, 1.115600667400684642E-11, -102.4000000000000483 ) ) ;
#112898 = AXIS2_PLACEMENT_3D ( 'NONE', #92966, #249494, #69575 ) ;
#112899 = ORIENTED_EDGE ( 'NONE', *, *, #88591, .F. ) ;
#112900 = CARTESIAN_POINT ( 'NONE',  ( -22.50485643085238863, 76.07878633908943300, -148.2729024236967064 ) ) ;
#112902 = EDGE_CURVE ( 'NONE', #49823, #255967, #173165, .T. ) ;
#112901 = SPHERICAL_SURFACE ( 'NONE', #133442, 0.1000000000000000056 ) ;
#112903 = EDGE_LOOP ( 'NONE', ( #52422, #26913, #193236, #196313 ) ) ;
#112904 = EDGE_LOOP ( 'NONE', ( #253315, #250383, #203892, #123000 ) ) ;
#112905 = CYLINDRICAL_SURFACE ( 'NONE', #180646, 0.09999999999999939493 ) ;
#112906 = DIRECTION ( 'NONE',  ( -1.000000000000000000, 0.000000000000000000, 0.000000000000000000 ) ) ;
#112907 = AXIS2_PLACEMENT_3D ( 'NONE', #191777, #153950, #13117 ) ;
#112908 = B_SPLINE_CURVE_WITH_KNOTS ( 'NONE', 3,
 ( #196578, #64463, #82695, #136594, #234420, #76633, #216140, #104823, #5735, #3175, #243084, #123152, #57043, #214863, #17940, #77909, #177052, #156208, #97455 ),
 .UNSPECIFIED., .F., .F.,
 ( 4, 3, 3, 3, 3, 3, 4 ),
 ( -2.000416914636979038E-06, 4.235164736271501695E-22, 4.714008503747322393E-05, 9.979203887779805799E-05, 0.0001372215519229540691, 0.0001635031576221083007, 0.0001900083748504232718 ),
 .UNSPECIFIED. ) ;
#112909 = ORIENTED_EDGE ( 'NONE', *, *, #139765, .F. ) ;
#112910 = CARTESIAN_POINT ( 'NONE',  ( 18.52326479938695059, -9.642364444904258036, -174.2147574134058061 ) ) ;
#112911 = CARTESIAN_POINT ( 'NONE',  ( 21.05000000000000426, 61.18186820035567308, -234.2493224657541759 ) ) ;
#112912 = ORIENTED_EDGE ( 'NONE', *, *, #36351, .T. ) ;
#112913 = EDGE_CURVE ( 'NONE', #135352, #116632, #191431, .T. ) ;
#112914 = VERTEX_POINT ( 'NONE', #77848 ) ;
#112915 = LINE ( 'NONE', #13815, #160156 ) ;
#112916 = DIRECTION ( 'NONE',  ( 0.000000000000000000, -1.000000000000000000, 0.000000000000000000 ) ) ;
#112917 = VECTOR ( 'NONE', #182487, 1000.000000000000000 ) ;
#112920 = ADVANCED_FACE ( 'NONE', ( #176997 ), #231821, .T. ) ;
#112919 = ORIENTED_EDGE ( 'NONE', *, *, #4507, .F. ) ;
#112918 = DIRECTION ( 'NONE',  ( 0.000000000000000000, 0.000000000000000000, -1.000000000000000000 ) ) ;
#112921 = DIRECTION ( 'NONE',  ( 0.000000000000000000, -1.000000000000000000, 0.000000000000000000 ) ) ;
#112923 = DIRECTION ( 'NONE',  ( 0.000000000000000000, 0.000000000000000000, -1.000000000000000000 ) ) ;
#112922 = UNCERTAINTY_MEASURE_WITH_UNIT (LENGTH_MEASURE( 1.000000000000000082E-05 ), #184562, 'distance_accuracy_value', 'NONE');
#112924 = CARTESIAN_POINT ( 'NONE',  ( 20.94999999999999929, 7.554435330547283556, -235.6868924355707691 ) ) ;
#112925 = CARTESIAN_POINT ( 'NONE',  ( -22.39999999999999858, 76.00000000001243450, -177.8138870828977360 ) ) ;
#112926 = CARTESIAN_POINT ( 'NONE',  ( -21.05000000000000071, 67.99035824846625076, -233.0562353075630142 ) ) ;
#112927 = AXIS2_PLACEMENT_3D ( 'NONE', #202636, #24026, #103520 ) ;
#112928 = EDGE_CURVE ( 'NONE', #207643, #185852, #99961, .T. ) ;
#112929 = FACE_OUTER_BOUND ( 'NONE', #89162, .T. ) ;
#112930 = DIRECTION ( 'NONE',  ( 0.000000000000000000, 0.000000000000000000, -1.000000000000000000 ) ) ;
#112931 = ADVANCED_FACE ( 'NONE', ( #182104 ), #183535, .F. ) ;
#112933 = ORIENTED_EDGE ( 'NONE', *, *, #97341, .F. ) ;
#112932 = CARTESIAN_POINT ( 'NONE',  ( 18.49999999999998934, 64.35000000001220144, -145.2731074845244450 ) ) ;
#112934 = VERTEX_POINT ( 'NONE', #3442 ) ;
#112936 = CARTESIAN_POINT ( 'NONE',  ( -16.87683809663752399, 50.97313360171293084, -232.3453239361865315 ) ) ;
#112935 = FACE_OUTER_BOUND ( 'NONE', #125281, .T. ) ;
#112938 = ORIENTED_EDGE ( 'NONE', *, *, #137034, .F. ) ;
#112937 = CARTESIAN_POINT ( 'NONE',  ( 21.05000000000000071, 8.872080675389140580, -75.52104741882936878 ) ) ;
#112939 = AXIS2_PLACEMENT_3D ( 'NONE', #192502, #212077, #251164 ) ;
#112940 = ORIENTED_EDGE ( 'NONE', *, *, #234528, .F. ) ;
#112941 = DIRECTION ( 'NONE',  ( 1.000000000000000000, -0.000000000000000000, -0.000000000000000000 ) ) ;
#112942 = ADVANCED_FACE ( 'NONE', ( #118281 ), #179551, .F. ) ;
#112943 = FACE_OUTER_BOUND ( 'NONE', #202971, .T. ) ;
#112944 = AXIS2_PLACEMENT_3D ( 'NONE', #52506, #235020, #252002 ) ;
#112946 = EDGE_CURVE ( 'NONE', #204385, #216335, #246081, .T. ) ;
#112945 = FACE_OUTER_BOUND ( 'NONE', #131186, .T. ) ;
#112947 = CIRCLE ( 'NONE', #487, 0.09999999999999939493 ) ;
#112948 = CARTESIAN_POINT ( 'NONE',  ( 20.04142135391667168, 11.75000000001116263, -58.20250686563003484 ) ) ;
#112949 = DIRECTION ( 'NONE',  ( 0.000000000000000000, 0.000000000000000000, -1.000000000000000000 ) ) ;
#112950 = DIRECTION ( 'NONE',  ( 0.000000000000000000, 1.000000000000000000, 0.000000000000000000 ) ) ;
#112951 = VECTOR ( 'NONE', #154780, 1000.000000000000000 ) ;
#112952 = CARTESIAN_POINT ( 'NONE',  ( -16.94226253665225457, 66.05000000001200533, -115.9698420801400971 ) ) ;
#112953 = EDGE_LOOP ( 'NONE', ( #208130, #138630, #134857, #169807 ) ) ;
#112954 = VERTEX_POINT ( 'NONE', #197798 ) ;
#112955 = LINE ( 'NONE', #192489, #177429 ) ;
#112956 = VECTOR ( 'NONE', #124470, 1000.000000000000000 ) ;
#112957 = ORIENTED_EDGE ( 'NONE', *, *, #220097, .F. ) ;
#112958 = DIRECTION ( 'NONE',  ( 1.000000000000000000, 0.000000000000000000, 0.000000000000000000 ) ) ;
#112960 = ORIENTED_EDGE ( 'NONE', *, *, #128020, .F. ) ;
#112959 = CIRCLE ( 'NONE', #121376, 11.75000000000000000 ) ;
#112961 = FACE_OUTER_BOUND ( 'NONE', #120943, .T. ) ;
#112962 = EDGE_CURVE ( 'NONE', #255868, #226886, #4453, .T. ) ;
#112963 = CIRCLE ( 'NONE', #150562, 11.75000000000000000 ) ;
#112964 = LINE ( 'NONE', #135065, #109564 ) ;
#112965 = CARTESIAN_POINT ( 'NONE',  ( 21.05000000000000071, 5.000000000011153745, -121.5947339810869465 ) ) ;
#112966 = ADVANCED_FACE ( 'NONE', ( #2156 ), #208496, .T. ) ;
#112967 = VERTEX_POINT ( 'NONE', #60850 ) ;
#112968 = EDGE_CURVE ( 'NONE', #124815, #160493, #37810, .T. ) ;
#112969 = DIRECTION ( 'NONE',  ( 1.000000000000000000, 0.000000000000000000, 0.000000000000000000 ) ) ;
#112970 = ORIENTED_EDGE ( 'NONE', *, *, #56135, .F. ) ;
#112971 = DIRECTION ( 'NONE',  ( -1.000000000000000000, 0.000000000000000000, 0.000000000000000000 ) ) ;
#112972 = CARTESIAN_POINT ( 'NONE',  ( 20.95512820512820440, 8.876151316299273120, -109.0586289951409924 ) ) ;
#112973 = ORIENTED_EDGE ( 'NONE', *, *, #182245, .F. ) ;
#112974 = EDGE_CURVE ( 'NONE', #2697, #3155, #123408, .T. ) ;
#112975 = CARTESIAN_POINT ( 'NONE',  ( -20.54999999999999716, 11.15983666280819975, -246.1019239270423213 ) ) ;
#112976 = ORIENTED_EDGE ( 'NONE', *, *, #147266, .F. ) ;
#112979 = VERTEX_POINT ( 'NONE', #62155 ) ;
#112978 = DIRECTION ( 'NONE',  ( 1.000000000000000000, 0.000000000000000000, 0.000000000000000000 ) ) ;
#112977 = CARTESIAN_POINT ( 'NONE',  ( 22.48660254037844197, 55.97436536266718576, -232.8539608197349935 ) ) ;
#112980 = VECTOR ( 'NONE', #26603, 1000.000000000000000 ) ;
#112981 = CARTESIAN_POINT ( 'NONE',  ( 18.49999999999999289, 65.79142135624879018, -44.75595019699900234 ) ) ;
#112982 = CIRCLE ( 'NONE', #527, 0.09999999999999939493 ) ;
#112984 = ORIENTED_EDGE ( 'NONE', *, *, #242156, .F. ) ;
#112983 = CIRCLE ( 'NONE', #133813, 1.899999999999999023 ) ;
#112985 = AXIS2_PLACEMENT_3D ( 'NONE', #93634, #74108, #212318 ) ;
#112986 = ORIENTED_EDGE ( 'NONE', *, *, #186678, .F. ) ;
#112987 = VERTEX_POINT ( 'NONE', #24326 ) ;
#112988 = FACE_BOUND ( 'NONE', #208620, .T. ) ;
#112989 = DIRECTION ( 'NONE',  ( 0.000000000000000000, 0.2128009952263606730, -0.9770955615653313941 ) ) ;
#112990 = CARTESIAN_POINT ( 'NONE',  ( 20.85000000000000142, 6.982009704867603972, -70.69615211825629331 ) ) ;
#112991 = DIRECTION ( 'NONE',  ( 0.000000000000000000, 0.000000000000000000, 1.000000000000000000 ) ) ;
#112992 = DIRECTION ( 'NONE',  ( 0.000000000000000000, -1.000000000000000000, 6.938893903907030216E-14 ) ) ;
#112993 = EDGE_CURVE ( 'NONE', #191177, #10935, #142011, .T. ) ;
#112994 = EDGE_LOOP ( 'NONE', ( #53121, #238131, #229197 ) ) ;
#112995 = CARTESIAN_POINT ( 'NONE',  ( -16.93658211146646408, 44.06789837094380857, -235.2808755401713938 ) ) ;
#112996 = CARTESIAN_POINT ( 'NONE',  ( -20.99780126800948565, 64.39461131213509759, -109.9357549128190641 ) ) ;
#112997 = EDGE_LOOP ( 'NONE', ( #141389, #248480, #55220, #91799 ) ) ;
#112998 = CARTESIAN_POINT ( 'NONE',  ( -21.30740335185486245, 0.09893452577585101770, 6.556657922028001906 ) ) ;
#112999 = EDGE_LOOP ( 'NONE', ( #188021, #49835, #87632, #85947 ) ) ;
#113000 = LINE ( 'NONE', #248654, #143897 ) ;
#113001 = ORIENTED_EDGE ( 'NONE', *, *, #100465, .F. ) ;
#113002 = CARTESIAN_POINT ( 'NONE',  ( -18.59999999999999787, 77.26178616857710324, -128.4366085209788366 ) ) ;
#113003 = DIRECTION ( 'NONE',  ( -0.000000000000000000, -1.000000000000000000, -6.982962677686266711E-15 ) ) ;
#113005 = VERTEX_POINT ( 'NONE', #180824 ) ;
#113004 = LINE ( 'NONE', #232970, #115596 ) ;
#113006 = DIRECTION ( 'NONE',  ( -0.1538461538461510236, 0.9880948137434718559, 0.000000000000000000 ) ) ;
#113007 = VERTEX_POINT ( 'NONE', #199093 ) ;
#113008 = CIRCLE ( 'NONE', #146316, 0.1999999999999987899 ) ;
#113009 = CARTESIAN_POINT ( 'NONE',  ( -21.05000000000000071, 36.02918351690956200, -236.0543695120161090 ) ) ;
#113010 = ADVANCED_FACE ( 'NONE', ( #140385 ), #38745, .F. ) ;
#113011 = CARTESIAN_POINT ( 'NONE',  ( -16.77180007708460607, 9.950000000011137047, -113.1356141189548623 ) ) ;
#113012 = ORIENTED_EDGE ( 'NONE', *, *, #26052, .F. ) ;
#113013 = CARTESIAN_POINT ( 'NONE',  ( 18.59999999999999076, 33.67810952736942198, -236.3734420906320395 ) ) ;
#113015 = EDGE_CURVE ( 'NONE', #230368, #253291, #23049, .T. ) ;
#113014 = CARTESIAN_POINT ( 'NONE',  ( -22.39999999999999858, -3.229117512539506407, -228.1842305956903090 ) ) ;
#113016 = ORIENTED_EDGE ( 'NONE', *, *, #83734, .T. ) ;
#113017 = B_SPLINE_CURVE_WITH_KNOTS ( 'NONE', 3,
 ( #71937, #56192, #154079, #13250, #31553, #111049, #173654, #251839, #131898, #211435 ),
 .UNSPECIFIED., .F., .F.,
 ( 4, 2, 2, 2, 4 ),
 ( 0.000000000000000000, 4.221631689686210128E-05, 8.443263379372420256E-05, 0.0001688652675874484051, 0.0003377305351748950755 ),
 .UNSPECIFIED. ) ;
#113018 = ORIENTED_EDGE ( 'NONE', *, *, #112206, .F. ) ;
#113019 = EDGE_CURVE ( 'NONE', #118580, #33783, #100473, .T. ) ;
#113021 = DIRECTION ( 'NONE',  ( 0.000000000000000000, -1.000000000000000000, 6.308085367188393199E-16 ) ) ;
#113020 = VECTOR ( 'NONE', #201311, 1000.000000000000000 ) ;
#113023 = EDGE_CURVE ( 'NONE', #3872, #41514, #84215, .T. ) ;
#113022 = CARTESIAN_POINT ( 'NONE',  ( 21.05000000000000071, 71.18691588786307989, -191.5815897280005800 ) ) ;
#113025 = ORIENTED_EDGE ( 'NONE', *, *, #119500, .T. ) ;
#113024 = DIRECTION ( 'NONE',  ( -1.000000000000000000, 0.000000000000000000, -0.000000000000000000 ) ) ;
#113026 = DIRECTION ( 'NONE',  ( 1.000000000000000000, -2.952720810173289112E-16, -2.061873921506763405E-30 ) ) ;
#113027 = CARTESIAN_POINT ( 'NONE',  ( 20.94999999999999574, 77.83534155023700407, -191.9679561919613491 ) ) ;
#113028 = CARTESIAN_POINT ( 'NONE',  ( 20.94999999999999929, 10.68863688179707694, -222.5873974249509217 ) ) ;
#113030 = CARTESIAN_POINT ( 'NONE',  ( -15.66061380678752890, 66.63927620602552793, -52.20918028991767557 ) ) ;
#113029 = CARTESIAN_POINT ( 'NONE',  ( -20.94999999999999929, 1.115600667400684642E-11, -134.0000000000000284 ) ) ;
#113031 = FACE_OUTER_BOUND ( 'NONE', #162855, .T. ) ;
#113032 = DIRECTION ( 'NONE',  ( 0.000000000000000000, 0.000000000000000000, -1.000000000000000000 ) ) ;
#113033 = VECTOR ( 'NONE', #62783, 1000.000000000000114 ) ;
#113034 = CARTESIAN_POINT ( 'NONE',  ( 23.14999999999999858, 70.10000000001197407, -113.2422072491807086 ) ) ;
#113035 = CIRCLE ( 'NONE', #146341, 0.09999999999999635569 ) ;
#113036 = CYLINDRICAL_SURFACE ( 'NONE', #63324, 12.87500000000000178 ) ;
#113037 = ADVANCED_FACE ( 'NONE', ( #158713 ), #41330, .F. ) ;
#113038 = ADVANCED_FACE ( 'NONE', ( #20476 ), #159994, .F. ) ;
#113040 = EDGE_LOOP ( 'NONE', ( #207510, #171262, #235598, #132707 ) ) ;
#113039 = AXIS2_PLACEMENT_3D ( 'NONE', #100965, #157168, #180564 ) ;
#113041 = ORIENTED_EDGE ( 'NONE', *, *, #80232, .F. ) ;
#113042 = CARTESIAN_POINT ( 'NONE',  ( -22.59080734064477625, 11.75000000001115907, -33.46925029190298773 ) ) ;
#113044 = VERTEX_POINT ( 'NONE', #187249 ) ;
#113043 = CARTESIAN_POINT ( 'NONE',  ( 21.05000000000000071, -8.999999999988844479, -76.89396912265249284 ) ) ;
#113045 = EDGE_LOOP ( 'NONE', ( #30398, #127749, #32874, #225397 ) ) ;
#113046 = CARTESIAN_POINT ( 'NONE',  ( 21.05000000000000071, 40.88152484246180052, -238.0427780438910474 ) ) ;
#113047 = EDGE_LOOP ( 'NONE', ( #46720, #219900, #135588, #1554, #23372, #27397 ) ) ;
#113048 = FACE_OUTER_BOUND ( 'NONE', #117283, .T. ) ;
#113049 = ADVANCED_FACE ( 'NONE', ( #7301 ), #96212, .T. ) ;
#113050 = ORIENTED_EDGE ( 'NONE', *, *, #69448, .T. ) ;
#113051 = VECTOR ( 'NONE', #231039, 1000.000000000000000 ) ;
#113052 = DIRECTION ( 'NONE',  ( 1.713247197920696616E-14, 0.9876197685951252359, -0.1568667991644863424 ) ) ;
#113053 = EDGE_CURVE ( 'NONE', #113629, #178868, #105081, .T. ) ;
#113055 = ORIENTED_EDGE ( 'NONE', *, *, #48096, .T. ) ;
#113054 = ORIENTED_EDGE ( 'NONE', *, *, #105488, .T. ) ;
#113056 = VERTEX_POINT ( 'NONE', #243347 ) ;
#113057 = EDGE_LOOP ( 'NONE', ( #69249, #114212, #56268 ) ) ;
#113058 = ORIENTED_EDGE ( 'NONE', *, *, #102157, .T. ) ;
#113059 = LINE ( 'NONE', #154779, #226060 ) ;
#113060 = CARTESIAN_POINT ( 'NONE',  ( 21.08750232978087524, 43.43435178450272360, -234.7639638145086849 ) ) ;
#113061 = DIRECTION ( 'NONE',  ( 1.000000000000000000, 0.000000000000000000, 0.000000000000000000 ) ) ;
#113063 = ORIENTED_EDGE ( 'NONE', *, *, #14638, .F. ) ;
#113062 = CARTESIAN_POINT ( 'NONE',  ( 21.05000000000000071, 1.115653327213047955E-11, -171.8000000000000114 ) ) ;
#113064 = LINE ( 'NONE', #12706, #44882 ) ;
#113065 = EDGE_CURVE ( 'NONE', #231120, #53755, #110251, .T. ) ;
#113066 = LINE ( 'NONE', #88332, #107525 ) ;
#113068 = ORIENTED_EDGE ( 'NONE', *, *, #190695, .F. ) ;
#113067 = CARTESIAN_POINT ( 'NONE',  ( 20.99999999999999645, 9.750000000011137757, -154.8500000000000227 ) ) ;
#113069 = CARTESIAN_POINT ( 'NONE',  ( 18.49999999999999645, 77.83534155023646406, -124.9679561919613064 ) ) ;
#113070 = ORIENTED_EDGE ( 'NONE', *, *, #55927, .T. ) ;
#113071 = DIRECTION ( 'NONE',  ( 0.000000000000000000, -1.000000000000000000, -6.860497997771532351E-15 ) ) ;
#113073 = VERTEX_POINT ( 'NONE', #129812 ) ;
#113072 = SPHERICAL_SURFACE ( 'NONE', #77019, 0.1000000000000000056 ) ;
#113074 = DIRECTION ( 'NONE',  ( -1.000000000000000000, 0.000000000000000000, 0.000000000000000000 ) ) ;
#113075 = LINE ( 'NONE', #111796, #212029 ) ;
#113076 = AXIS2_PLACEMENT_3D ( 'NONE', #143708, #4192, #245395 ) ;
#113077 = CIRCLE ( 'NONE', #444, 2.099999999999989875 ) ;
#113078 = AXIS2_PLACEMENT_3D ( 'NONE', #219952, #165118, #7320 ) ;
#113080 = EDGE_CURVE ( 'NONE', #19112, #73683, #112983, .T. ) ;
#113079 = VERTEX_POINT ( 'NONE', #6010 ) ;
#113082 = CARTESIAN_POINT ( 'NONE',  ( -18.50000000000000000, -9.399999999988850163, -140.8820418481727188 ) ) ;
#113081 = CARTESIAN_POINT ( 'NONE',  ( 18.39999999999999858, 77.17949092533254429, -241.9177572069595783 ) ) ;
#113083 = CARTESIAN_POINT ( 'NONE',  ( 21.05000000000000071, 44.05869416168422958, -258.6139110589941197 ) ) ;
#113084 = DIRECTION ( 'NONE',  ( 0.000000000000000000, 0.8814952561688476074, -0.4721928772777262417 ) ) ;
#113085 = DIRECTION ( 'NONE',  ( 0.000000000000000000, -0.1350103645451974088, 0.9908441862701587999 ) ) ;
#113086 = ORIENTED_EDGE ( 'NONE', *, *, #134976, .F. ) ;
#113087 = ORIENTED_EDGE ( 'NONE', *, *, #253496, .T. ) ;
#113088 = CARTESIAN_POINT ( 'NONE',  ( 20.85000000000000142, -1.835859311432481045, -179.0044391687985410 ) ) ;
#113089 = CARTESIAN_POINT ( 'NONE',  ( -20.94999999999999929, 74.16465844978819177, -191.8679561919614116 ) ) ;
#113090 = VERTEX_POINT ( 'NONE', #167693 ) ;
#113091 = FACE_OUTER_BOUND ( 'NONE', #113652, .T. ) ;
#113092 = ORIENTED_EDGE ( 'NONE', *, *, #164813, .T. ) ;
#113093 = EDGE_CURVE ( 'NONE', #124432, #97848, #4623, .T. ) ;
#113094 = DIRECTION ( 'NONE',  ( -0.000000000000000000, 0.9770955615653313941, 0.2128009952263603954 ) ) ;
#113095 = DIRECTION ( 'NONE',  ( 0.000000000000000000, 0.000000000000000000, -1.000000000000000000 ) ) ;
#113096 = CIRCLE ( 'NONE', #171570, 0.09999999999999939493 ) ;
#113097 = DIRECTION ( 'NONE',  ( 0.000000000000000000, 0.000000000000000000, 1.000000000000000000 ) ) ;
#113098 = ORIENTED_EDGE ( 'NONE', *, *, #102915, .F. ) ;
#113099 = CYLINDRICAL_SURFACE ( 'NONE', #11110, 0.09999999999999939493 ) ;
#113100 = VERTEX_POINT ( 'NONE', #29477 ) ;
#113101 = VERTEX_POINT ( 'NONE', #90682 ) ;
#113102 = ORIENTED_EDGE ( 'NONE', *, *, #28504, .F. ) ;
#113103 = CARTESIAN_POINT ( 'NONE',  ( -20.54999999999999716, 85.40000000001262492, -193.6291383618718385 ) ) ;
#113104 = CARTESIAN_POINT ( 'NONE',  ( 13.88302573338719093, 66.54258905524415013, -54.52302351073438302 ) ) ;
#113105 = CARTESIAN_POINT ( 'NONE',  ( -21.05000000000000071, 1.250000000011155299, -142.0000000000000284 ) ) ;
#113106 = CARTESIAN_POINT ( 'NONE',  ( -23.25000000000000000, 85.00000000001251976, -179.9170766071767389 ) ) ;
#113107 = CARTESIAN_POINT ( 'NONE',  ( -18.34374000495059676, 33.92263863280957281, -235.0698407953532296 ) ) ;
#113108 = AXIS2_PLACEMENT_3D ( 'NONE', #142853, #184569, #7206 ) ;
#113110 = DIRECTION ( 'NONE',  ( 1.000000000000000000, -1.335000415235278971E-16, 2.979993593738921214E-16 ) ) ;
#113109 = DIRECTION ( 'NONE',  ( -1.000000000000000000, -0.000000000000000000, -0.000000000000000000 ) ) ;
#113112 = VERTEX_POINT ( 'NONE', #30749 ) ;
#113111 = CARTESIAN_POINT ( 'NONE',  ( -18.40000000000000213, 5.650000000011139001, -91.25000000000005684 ) ) ;
#113113 = CARTESIAN_POINT ( 'NONE',  ( -21.05000000000000071, 36.65892442174935439, -249.5511627012433848 ) ) ;
#113114 = ORIENTED_EDGE ( 'NONE', *, *, #11882, .F. ) ;
#113115 = CARTESIAN_POINT ( 'NONE',  ( -15.75000000000000000, 9.350000000011140955, -150.5215193718251214 ) ) ;
#113116 = EDGE_LOOP ( 'NONE', ( #166348, #63058, #134974, #92475 ) ) ;
#113117 = ORIENTED_EDGE ( 'NONE', *, *, #188275, .T. ) ;
#113118 = DIRECTION ( 'NONE',  ( 0.000000000000000000, 0.000000000000000000, -1.000000000000000000 ) ) ;
#113119 = AXIS2_PLACEMENT_3D ( 'NONE', #27531, #90016, #144852 ) ;
#113120 = CARTESIAN_POINT ( 'NONE',  ( -16.94037747912386394, 10.01353938249748587, -46.05113095797549505 ) ) ;
#113121 = CARTESIAN_POINT ( 'NONE',  ( -21.05000000000000071, 70.15000000001266756, -193.3906102602464330 ) ) ;
#113122 = PLANE ( 'NONE',  #25291 ) ;
#113123 = AXIS2_PLACEMENT_3D ( 'NONE', #104908, #42409, #241886 ) ;
#113124 = CARTESIAN_POINT ( 'NONE',  ( 20.86777300164945004, 18.41441690808118281, -236.9991004306322964 ) ) ;
#113125 = VECTOR ( 'NONE', #146172, 1000.000000000000000 ) ;
#113126 = ORIENTED_EDGE ( 'NONE', *, *, #165243, .T. ) ;
#113127 = ORIENTED_EDGE ( 'NONE', *, *, #77722, .T. ) ;
#113128 = CIRCLE ( 'NONE', #117413, 0.09999999999998898659 ) ;
#113129 = DIRECTION ( 'NONE',  ( 0.000000000000000000, 1.000000000000000000, 0.000000000000000000 ) ) ;
#113130 = EDGE_LOOP ( 'NONE', ( #77078, #201608, #161499, #38992 ) ) ;
#113131 = LINE ( 'NONE', #110556, #148749 ) ;
#113132 = DIRECTION ( 'NONE',  ( 0.7071067811865474617, 0.7071067811865474617, 0.000000000000000000 ) ) ;
#113133 = ORIENTED_EDGE ( 'NONE', *, *, #50252, .T. ) ;
#113134 = CARTESIAN_POINT ( 'NONE',  ( -20.90000000000000213, 11.59510167572422112, 1.901609089591594470 ) ) ;
#113135 = DIRECTION ( 'NONE',  ( 1.000000000000000000, 0.000000000000000000, 0.000000000000000000 ) ) ;
#113136 = CARTESIAN_POINT ( 'NONE',  ( 20.94999999999997442, 7.576017155224048061, -241.7224044826512284 ) ) ;
#113137 = EDGE_LOOP ( 'NONE', ( #155365, #92673, #159365, #141841 ) ) ;
#113138 = CIRCLE ( 'NONE', #233763, 0.2000000000000000944 ) ;
#113139 = CARTESIAN_POINT ( 'NONE',  ( -21.14999999999999858, 76.00000000001169553, -76.06376443622556849 ) ) ;
#113141 = EDGE_CURVE ( 'NONE', #74710, #57461, #158796, .T. ) ;
#113140 = CARTESIAN_POINT ( 'NONE',  ( -20.64999999999999858, 4.350000000011156054, -146.2500000000000284 ) ) ;
#113142 = VECTOR ( 'NONE', #194092, 1000.000000000000000 ) ;
#113143 = CARTESIAN_POINT ( 'NONE',  ( -21.03571358706064487, 57.67743169815677362, -226.1923800109734088 ) ) ;
#113144 = CIRCLE ( 'NONE', #254739, 0.1000000000000028644 ) ;
#113145 = EDGE_LOOP ( 'NONE', ( #133912, #181969, #164520, #171623 ) ) ;
#113146 = CARTESIAN_POINT ( 'NONE',  ( 21.15000000000000213, 10.71339244339988461, -12.25000000000000178 ) ) ;
#113147 = ORIENTED_EDGE ( 'NONE', *, *, #128385, .T. ) ;
#113148 = FACE_OUTER_BOUND ( 'NONE', #225774, .T. ) ;
#113149 = CIRCLE ( 'NONE', #171446, 0.1000000000000028644 ) ;
#113150 = CARTESIAN_POINT ( 'NONE',  ( -16.93262454970419384, 14.22623245403305070, -219.3193133873473641 ) ) ;
#113151 = DIRECTION ( 'NONE',  ( 0.000000000000000000, -0.4999999999999689138, 0.8660254037844565822 ) ) ;
#113152 = DIRECTION ( 'NONE',  ( 1.000000000000000000, 0.000000000000000000, 0.000000000000000000 ) ) ;
#113153 = DIRECTION ( 'NONE',  ( 0.000000000000000000, 1.000000000000000000, 0.000000000000000000 ) ) ;
#113154 = CARTESIAN_POINT ( 'NONE',  ( -20.64999999999999858, 76.00000000001237765, -170.0231074845243597 ) ) ;
#113155 = EDGE_CURVE ( 'NONE', #172714, #162071, #42086, .T. ) ;
#113156 = EDGE_LOOP ( 'NONE', ( #170129, #34584, #192109, #165615 ) ) ;
#113157 = CARTESIAN_POINT ( 'NONE',  ( -16.93772744219066340, 66.00645889125971166, -123.9250455125546750 ) ) ;
#113158 = LINE ( 'NONE', #230549, #185763 ) ;
#113159 = DIRECTION ( 'NONE',  ( 0.000000000000000000, -6.467318590049456648E-15, 1.000000000000000000 ) ) ;
#113160 = DIRECTION ( 'NONE',  ( 0.000000000000000000, 0.000000000000000000, -1.000000000000000000 ) ) ;
#113161 = CIRCLE ( 'NONE', #8931, 0.6000000000000033085 ) ;
#113162 = AXIS2_PLACEMENT_3D ( 'NONE', #182164, #101277, #183448 ) ;
#113163 = CIRCLE ( 'NONE', #697, 11.65000000000001457 ) ;
#113164 = ORIENTED_EDGE ( 'NONE', *, *, #247947, .F. ) ;
#113165 = ORIENTED_EDGE ( 'NONE', *, *, #62311, .T. ) ;
#113166 = CARTESIAN_POINT ( 'NONE',  ( -21.05000000000000071, 76.00000000001170974, -69.52310748452431710 ) ) ;
#113167 = DIRECTION ( 'NONE',  ( 0.000000000000000000, 0.9999631594459056361, -0.008583690987128059571 ) ) ;
#113169 = EDGE_CURVE ( 'NONE', #141252, #15255, #125958, .T. ) ;
#113168 = CARTESIAN_POINT ( 'NONE',  ( -21.05000000000000071, -4.871452838297995136, -233.3782557782877518 ) ) ;
#113170 = DIRECTION ( 'NONE',  ( 0.000000000000000000, -0.4088369013363280513, 0.9126074666063769270 ) ) ;
#113171 = CARTESIAN_POINT ( 'NONE',  ( 23.24999999999999289, 64.35000000001194564, -102.9231074845243938 ) ) ;
#113172 = EDGE_CURVE ( 'NONE', #44121, #181223, #195919, .T. ) ;
#113173 = EDGE_LOOP ( 'NONE', ( #189169, #200340, #193501, #2513 ) ) ;
#113174 = DIRECTION ( 'NONE',  ( 0.000000000000000000, 1.265107689135680095E-16, -1.000000000000000000 ) ) ;
#113175 = EDGE_CURVE ( 'NONE', #60353, #92616, #55376, .T. ) ;
#113176 = CONTEXT_DEPENDENT_SHAPE_REPRESENTATION ( #184118, #60044 ) ;
#113177 = DIRECTION ( 'NONE',  ( 0.000000000000000000, -0.1335171055202901691, -0.9910465087640861759 ) ) ;
#113178 = ORIENTED_EDGE ( 'NONE', *, *, #104890, .T. ) ;
#113179 = CARTESIAN_POINT ( 'NONE',  ( 23.15000000000000213, 87.75000000001197975, -115.1731074845242233 ) ) ;
#113180 = EDGE_CURVE ( 'NONE', #94374, #135260, #108706, .T. ) ;
#113181 = DIRECTION ( 'NONE',  ( -1.000000000000000000, -0.000000000000000000, -0.000000000000000000 ) ) ;
#113182 = AXIS2_PLACEMENT_3D ( 'NONE', #75882, #233686, #248418 ) ;
#113183 = EDGE_CURVE ( 'NONE', #198238, #207656, #34593, .T. ) ;
#113184 = VERTEX_POINT ( 'NONE', #214485 ) ;
#113185 = DIRECTION ( 'NONE',  ( 1.000000000000000000, 0.000000000000000000, 0.000000000000000000 ) ) ;
#113186 = ORIENTED_EDGE ( 'NONE', *, *, #125400, .T. ) ;
#113187 = PLANE ( 'NONE',  #168202 ) ;
#113188 = DIRECTION ( 'NONE',  ( 0.000000000000000000, 0.000000000000000000, -1.000000000000000000 ) ) ;
#113189 = CARTESIAN_POINT ( 'NONE',  ( -20.64999999999999858, 6.757359537351773859, -220.2789794402637824 ) ) ;
#113190 = DIRECTION ( 'NONE',  ( 0.000000000000000000, -0.9126074666063660468, -0.4088369013363524762 ) ) ;
#113191 = FACE_OUTER_BOUND ( 'NONE', #129768, .T. ) ;
#113192 = DIRECTION ( 'NONE',  ( 0.000000000000000000, -0.2128009952263604232, 0.9770955615653316162 ) ) ;
#113193 = DIRECTION ( 'NONE',  ( 0.000000000000000000, -0.4999999999999088507, 0.8660254037844913322 ) ) ;
#113194 = DIRECTION ( 'NONE',  ( 1.000000000000000000, -0.000000000000000000, -0.000000000000000000 ) ) ;
#113195 = EDGE_CURVE ( 'NONE', #152685, #44054, #33927, .T. ) ;
#113197 = DIRECTION ( 'NONE',  ( 0.000000000000000000, -1.000000000000000000, 0.000000000000000000 ) ) ;
#113196 = DIRECTION ( 'NONE',  ( -0.000000000000000000, -0.4856429311786357728, -0.8741572761215358200 ) ) ;
#113198 = DIRECTION ( 'NONE',  ( 1.000000000000000000, -7.304098846218133681E-16, 4.607487905232622991E-31 ) ) ;
#113199 = LINE ( 'NONE', #71532, #210321 ) ;
#113200 = CARTESIAN_POINT ( 'NONE',  ( 20.95545211741311320, 18.81481477104959055, -227.9829527115510643 ) ) ;
#113201 = ORIENTED_EDGE ( 'NONE', *, *, #193121, .T. ) ;
#113202 = CARTESIAN_POINT ( 'NONE',  ( -18.48408745364676520, -9.664322258663098353, -40.18307853332839130 ) ) ;
#113203 = FACE_OUTER_BOUND ( 'NONE', #7449, .T. ) ;
#113204 = FACE_OUTER_BOUND ( 'NONE', #227446, .T. ) ;
#113205 = AXIS2_PLACEMENT_3D ( 'NONE', #53517, #14420, #116072 ) ;
#113206 = CARTESIAN_POINT ( 'NONE',  ( 20.99999999999997868, 76.00000000001267608, -203.5231074845243597 ) ) ;
#113207 = CARTESIAN_POINT ( 'NONE',  ( 21.05000000000000071, 1.115600667400684642E-11, -200.9999999999999432 ) ) ;
#113208 = FACE_OUTER_BOUND ( 'NONE', #64979, .T. ) ;
#113209 = ORIENTED_EDGE ( 'NONE', *, *, #67960, .F. ) ;
#113210 = CARTESIAN_POINT ( 'NONE',  ( -18.50000000000000000, 66.85000000001259934, -191.1731074845244223 ) ) ;
#113211 = VERTEX_POINT ( 'NONE', #151984 ) ;
#113212 = DIRECTION ( 'NONE',  ( 0.000000000000000000, 0.000000000000000000, -1.000000000000000000 ) ) ;
#113213 = VECTOR ( 'NONE', #202555, 1000.000000000000000 ) ;
#113214 = CIRCLE ( 'NONE', #125695, 0.09999999999999950595 ) ;
#113215 = ADVANCED_FACE ( 'NONE', ( #51530 ), #153274, .T. ) ;
#113216 = EDGE_CURVE ( 'NONE', #165955, #195448, #114097, .T. ) ;
#113217 = EDGE_LOOP ( 'NONE', ( #254999, #30653, #37686, #100873 ) ) ;
#113218 = FACE_OUTER_BOUND ( 'NONE', #233022, .T. ) ;
#113219 = VERTEX_POINT ( 'NONE', #32031 ) ;
#113220 = ADVANCED_FACE ( 'NONE', ( #71154 ), #115382, .T. ) ;
#113222 = EDGE_CURVE ( 'NONE', #72558, #102432, #187835, .T. ) ;
#113221 = DIRECTION ( 'NONE',  ( 0.000000000000000000, 0.000000000000000000, 1.000000000000000000 ) ) ;
#113223 = DIRECTION ( 'NONE',  ( 0.000000000000000000, -0.1568667991644863147, 0.9876197685951252359 ) ) ;
#113225 = CARTESIAN_POINT ( 'NONE',  ( 23.14999999999999858, -2.099999999988846344, -67.00000000000000000 ) ) ;
#113224 = PRODUCT_DEFINITION_CONTEXT ( 'detailed design', #99186, 'design' ) ;
#113226 = DIRECTION ( 'NONE',  ( 0.000000000000000000, 1.000000000000000000, 0.000000000000000000 ) ) ;
#113227 = CARTESIAN_POINT ( 'NONE',  ( -20.54999999999999716, -9.499999999988846255, -90.60603087734760663 ) ) ;
#113228 = CARTESIAN_POINT ( 'NONE',  ( -21.59142135623730852, 7.850000000011158718, -79.35000000000005116 ) ) ;
#113229 = CIRCLE ( 'NONE', #25750, 0.2000000000000057288 ) ;
#113230 = EDGE_CURVE ( 'NONE', #102673, #208784, #50408, .T. ) ;
#113231 = CARTESIAN_POINT ( 'NONE',  ( -23.25000000000000000, 1.115600667400684642E-11, -37.54999999999999716 ) ) ;
#113232 = DIRECTION ( 'NONE',  ( 0.000000000000000000, -0.9126074666063769270, -0.4088369013363281623 ) ) ;
#113233 = B_SPLINE_CURVE_WITH_KNOTS ( 'NONE', 3,
 ( #80844, #138251, #178724, #101677, #118731, #156596, #40498, #160439, #120030, #142119, #237380, #199561, #2602, #216523, #37916, #157889, #79563, #159150, #238659 ),
 .UNSPECIFIED., .F., .F.,
 ( 4, 3, 3, 3, 3, 3, 4 ),
 ( 1.387778780781445676E-17, 2.646747978908746348E-05, 5.271166642127513550E-05, 9.008788829882962801E-05, 0.0001426648776560695663, 0.0001897378458659517613, 0.0001917382627806230261 ),
 .UNSPECIFIED. ) ;
#113235 = ORIENTED_EDGE ( 'NONE', *, *, #46938, .T. ) ;
#113234 = CARTESIAN_POINT ( 'NONE',  ( 21.11833042828134666, 69.55435530615672235, -103.0302079935837725 ) ) ;
#113237 = DIRECTION ( 'NONE',  ( 1.000000000000000000, 7.304098846218134667E-16, -0.000000000000000000 ) ) ;
#113236 = DIRECTION ( 'NONE',  ( 3.265361837132812600E-16, -0.9770955615653313941, -0.2128009952263603677 ) ) ;
#113238 = ORIENTED_EDGE ( 'NONE', *, *, #163298, .T. ) ;
#113240 = ORIENTED_EDGE ( 'NONE', *, *, #35004, .T. ) ;
#113239 = DIRECTION ( 'NONE',  ( 0.000000000000000000, 1.776356839400308446E-15, -1.000000000000000000 ) ) ;
#113241 = EDGE_CURVE ( 'NONE', #172022, #75024, #121098, .T. ) ;
#113242 = ORIENTED_EDGE ( 'NONE', *, *, #70383, .F. ) ;
#113243 = FACE_OUTER_BOUND ( 'NONE', #203500, .T. ) ;
#113245 = EDGE_CURVE ( 'NONE', #160781, #97691, #200463, .T. ) ;
#113244 = EDGE_CURVE ( 'NONE', #7959, #48558, #54715, .T. ) ;
#113246 = DIRECTION ( 'NONE',  ( 0.000000000000000000, -1.000000000000000000, 0.000000000000000000 ) ) ;
#113247 = B_SPLINE_CURVE_WITH_KNOTS ( 'NONE', 3,
 ( #236767, #58116, #140222, #21600, #81521, #217197, #161108, #92783, #227163, #52365, #73270, #228474, #232332, #152806, #251859, #151513, #246722, #87643, #9397 ),
 .UNSPECIFIED., .F., .F.,
 ( 4, 3, 3, 3, 3, 3, 4 ),
 ( 0.0001624081864585766950, 0.0001685232196531723725, 0.0001764526673566880696, 0.0001916878551483189471, 0.0002009890782182605323, 0.0002238845907555128808, 0.0002283406619926333443 ),
 .UNSPECIFIED. ) ;
#113249 = EDGE_CURVE ( 'NONE', #102873, #123636, #121210, .T. ) ;
#113248 = CARTESIAN_POINT ( 'NONE',  ( 21.13461538461538325, 8.885417037974459475, -12.35000000000000320 ) ) ;
#113250 = CARTESIAN_POINT ( 'NONE',  ( 21.05000000000000071, 10.72371710471867701, -141.6649135690876165 ) ) ;
#113251 = DIRECTION ( 'NONE',  ( 1.000000000000000000, 0.000000000000000000, -0.000000000000000000 ) ) ;
#113252 = DIRECTION ( 'NONE',  ( 0.7071067811865463515, -0.7071067811865487940, 4.930380657631324879E-32 ) ) ;
#113253 = FACE_OUTER_BOUND ( 'NONE', #62066, .T. ) ;
#113254 = EDGE_CURVE ( 'NONE', #101747, #250639, #196177, .T. ) ;
#113255 = VECTOR ( 'NONE', #227091, 1000.000000000000000 ) ;
#113256 = AXIS2_PLACEMENT_3D ( 'NONE', #31682, #111190, #85545 ) ;
#113258 = AXIS2_PLACEMENT_3D ( 'NONE', #177967, #193671, #76271 ) ;
#113257 = CARTESIAN_POINT ( 'NONE',  ( -20.64999999999999858, -9.399999999988846611, -124.1060308773475924 ) ) ;
#113259 = EDGE_LOOP ( 'NONE', ( #250814, #188640, #54196, #2922 ) ) ;
#113260 = ORIENTED_EDGE ( 'NONE', *, *, #48158, .T. ) ;
#113261 = CARTESIAN_POINT ( 'NONE',  ( 18.49999999999999645, 70.30054753569044124, -115.5653814410941891 ) ) ;
#113262 = EDGE_CURVE ( 'NONE', #205324, #58091, #125460, .T. ) ;
#113263 = ADVANCED_FACE ( 'NONE', ( #157107 ), #175359, .T. ) ;
#113264 = ORIENTED_EDGE ( 'NONE', *, *, #121609, .F. ) ;
#113265 = CARTESIAN_POINT ( 'NONE',  ( -20.54999999999999716, 76.00000000001205080, -123.5481074845242802 ) ) ;
#113266 = EDGE_LOOP ( 'NONE', ( #140652, #196474, #118595, #83925 ) ) ;
#113267 = CARTESIAN_POINT ( 'NONE',  ( 18.54271179734059416, -9.624084290098748440, -40.24096485270028012 ) ) ;
#113268 = EDGE_CURVE ( 'NONE', #4633, #74203, #229516, .T. ) ;
#113269 = DIRECTION ( 'NONE',  ( 1.000000000000000000, 0.000000000000000000, -0.000000000000000000 ) ) ;
#113270 = PLANE ( 'NONE',  #213700 ) ;
#113271 = LINE ( 'NONE', #55827, #164765 ) ;
#113272 = EDGE_CURVE ( 'NONE', #210115, #240059, #177947, .T. ) ;
#113273 = DIRECTION ( 'NONE',  ( -0.000000000000000000, 0.2128009952263604232, -0.9770955615653316162 ) ) ;
#113274 = ORIENTED_EDGE ( 'NONE', *, *, #57442, .F. ) ;
#113275 = EDGE_CURVE ( 'NONE', #57845, #63069, #165780, .T. ) ;
#113276 = CARTESIAN_POINT ( 'NONE',  ( -18.31572283045136729, -9.548437830874727084, -207.8506256510582944 ) ) ;
#113277 = CIRCLE ( 'NONE', #146569, 0.09999999999999080458 ) ;
#113278 = CARTESIAN_POINT ( 'NONE',  ( -23.25000000000000000, 77.85161776048053639, -57.91991776492063337 ) ) ;
#113279 = DIRECTION ( 'NONE',  ( 0.000000000000000000, 7.086529944415894657E-15, -1.000000000000000000 ) ) ;
#113280 = LINE ( 'NONE', #192828, #19888 ) ;
#113281 = ORIENTED_EDGE ( 'NONE', *, *, #153991, .T. ) ;
#113283 = DIRECTION ( 'NONE',  ( -1.000000000000000000, -0.000000000000000000, -0.000000000000000000 ) ) ;
#113282 = CYLINDRICAL_SURFACE ( 'NONE', #37545, 0.1000000000000124678 ) ;
#113284 = EDGE_LOOP ( 'NONE', ( #76882, #218759, #57182, #194481 ) ) ;
#113287 = ORIENTED_EDGE ( 'NONE', *, *, #169747, .T. ) ;
#113286 = DIRECTION ( 'NONE',  ( 1.000000000000000000, 0.000000000000000000, 0.000000000000000000 ) ) ;
#113285 = DIRECTION ( 'NONE',  ( 0.000000000000000000, 0.000000000000000000, -1.000000000000000000 ) ) ;
#113288 = DIRECTION ( 'NONE',  ( 0.000000000000000000, -0.9999631594459057471, 0.008583690987121077309 ) ) ;
#113289 = DIRECTION ( 'NONE',  ( 0.000000000000000000, 0.2128009952263605342, -0.9770955615653315052 ) ) ;
#113290 = ORIENTED_EDGE ( 'NONE', *, *, #237892, .T. ) ;
#113291 = CYLINDRICAL_SURFACE ( 'NONE', #101361, 0.5000000000000014433 ) ;
#113292 = VECTOR ( 'NONE', #183903, 1000.000000000000000 ) ;
#113293 = CARTESIAN_POINT ( 'NONE',  ( -23.15000000000000213, 1.115600667400684642E-11, -146.8750000000000000 ) ) ;
#113294 = CARTESIAN_POINT ( 'NONE',  ( -22.49072729836730034, -3.113923299533181588, -228.1818618411975308 ) ) ;
#113296 = VERTEX_POINT ( 'NONE', #66663 ) ;
#113295 = FACE_OUTER_BOUND ( 'NONE', #32602, .T. ) ;
#113297 = AXIS2_PLACEMENT_3D ( 'NONE', #249278, #91481, #191892 ) ;
#113298 = ORIENTED_EDGE ( 'NONE', *, *, #125362, .F. ) ;
#113299 = AXIS2_PLACEMENT_3D ( 'NONE', #157962, #60083, #220470 ) ;
#113300 = CIRCLE ( 'NONE', #845, 0.09999999999998898659 ) ;
#113301 = DIRECTION ( 'NONE',  ( -1.000000000000000000, 2.952720810173289112E-16, 2.061873921506763405E-30 ) ) ;
#113302 = CARTESIAN_POINT ( 'NONE',  ( 18.40000000000000213, -9.499999999988840926, -73.99936209718019597 ) ) ;
#113303 = CARTESIAN_POINT ( 'NONE',  ( -18.69999999999999929, -8.250000000000005329, 10.52591260281975138 ) ) ;
#113304 = CARTESIAN_POINT ( 'NONE',  ( -22.39999999999999858, 68.20922040163873135, -136.5231074845243313 ) ) ;
#113306 = ORIENTED_EDGE ( 'NONE', *, *, #200155, .F. ) ;
#113305 = AXIS2_PLACEMENT_3D ( 'NONE', #203283, #32385, #190153 ) ;
#113307 = DIRECTION ( 'NONE',  ( -0.000000000000000000, -1.000000000000000000, 0.000000000000000000 ) ) ;
#113308 = CARTESIAN_POINT ( 'NONE',  ( 21.05000000000005400, 65.19115966511134275, -29.92310748452479174 ) ) ;
#113309 = CARTESIAN_POINT ( 'NONE',  ( -21.14999999999999858, -0.09999999998884338825, -21.85042919245520210 ) ) ;
#113310 = EDGE_LOOP ( 'NONE', ( #116748, #135827, #81205, #167455 ) ) ;
#113311 = DIRECTION ( 'NONE',  ( 0.000000000000000000, -0.9651348961777379554, 0.2617529984164210233 ) ) ;
#113312 = CIRCLE ( 'NONE', #208987, 0.1000000000000002137 ) ;
#113313 = CARTESIAN_POINT ( 'NONE',  ( 21.05000000000000071, 76.00000000001126921, -203.5231074845248997 ) ) ;
#113314 = VECTOR ( 'NONE', #181766, 1000.000000000000000 ) ;
#113315 = ADVANCED_FACE ( 'NONE', ( #225693 ), #179243, .F. ) ;
#113316 = ORIENTED_EDGE ( 'NONE', *, *, #70557, .T. ) ;
#113317 = AXIS2_PLACEMENT_3D ( 'NONE', #109075, #9988, #29584 ) ;
#113318 = DIRECTION ( 'NONE',  ( 1.000000000000000000, 0.000000000000000000, -0.000000000000000000 ) ) ;
#113320 = EDGE_CURVE ( 'NONE', #253585, #119237, #126628, .T. ) ;
#113319 = CARTESIAN_POINT ( 'NONE',  ( 20.94999999999999929, 67.22371710471932715, -81.77310748452437394 ) ) ;
#113321 = CIRCLE ( 'NONE', #121718, 0.6000000000000015321 ) ;
#113322 = ORIENTED_EDGE ( 'NONE', *, *, #55778, .T. ) ;
#113323 = ORIENTED_EDGE ( 'NONE', *, *, #225846, .T. ) ;
#113324 = CIRCLE ( 'NONE', #171622, 0.09999999999999939493 ) ;
#113325 = EDGE_CURVE ( 'NONE', #254325, #257538, #18854, .T. ) ;
#113326 = CYLINDRICAL_SURFACE ( 'NONE', #120874, 0.09999999999999939493 ) ;
#113327 = ORIENTED_EDGE ( 'NONE', *, *, #218045, .F. ) ;
#113330 = EDGE_CURVE ( 'NONE', #128673, #62762, #137898, .T. ) ;
#113329 = ORIENTED_EDGE ( 'NONE', *, *, #67581, .F. ) ;
#113328 = DIRECTION ( 'NONE',  ( -0.000000000000000000, -0.000000000000000000, 1.000000000000000000 ) ) ;
#113331 = VECTOR ( 'NONE', #6143, 1000.000000000000114 ) ;
#113334 = VERTEX_POINT ( 'NONE', #137500 ) ;
#113333 = ORIENTED_EDGE ( 'NONE', *, *, #119255, .F. ) ;
#113332 = CARTESIAN_POINT ( 'NONE',  ( 21.33487959338958362, 60.74020368437640371, -234.0946914941910393 ) ) ;
#113335 = DIRECTION ( 'NONE',  ( -0.000000000000000000, 0.9126074666063770380, 0.4088369013363281068 ) ) ;
#113336 = ORIENTED_EDGE ( 'NONE', *, *, #41916, .T. ) ;
#113337 = DIRECTION ( 'NONE',  ( 0.000000000000000000, -7.116814260417676401E-15, 1.000000000000000000 ) ) ;
#113338 = LINE ( 'NONE', #192887, #86784 ) ;
#113339 = AXIS2_PLACEMENT_3D ( 'NONE', #55454, #35950, #175467 ) ;
#113340 = AXIS2_PLACEMENT_3D ( 'NONE', #225402, #49353, #145871 ) ;
#113341 = CARTESIAN_POINT ( 'NONE',  ( -18.59999999999999787, -1.149570369575693807, -41.31591248450196474 ) ) ;
#113342 = VECTOR ( 'NONE', #239263, 1000.000000000000000 ) ;
#113343 = ADVANCED_FACE ( 'NONE', ( #5366 ), #204555, .T. ) ;
#113344 = DIRECTION ( 'NONE',  ( 0.000000000000000000, 0.07893460099012300502, -0.9968797965484754720 ) ) ;
#113346 = DIRECTION ( 'NONE',  ( -0.000000000000000000, 0.4721928772777346239, 0.8814952561688430555 ) ) ;
#113345 = CIRCLE ( 'NONE', #67552, 0.09999999999999939493 ) ;
#113348 = EDGE_CURVE ( 'NONE', #236840, #213491, #25678, .T. ) ;
#113347 = ORIENTED_EDGE ( 'NONE', *, *, #17791, .F. ) ;
#113349 = VERTEX_POINT ( 'NONE', #80071 ) ;
#113350 = ORIENTED_EDGE ( 'NONE', *, *, #199680, .F. ) ;
#113351 = DIRECTION ( 'NONE',  ( 0.7071067811865473507, 0.3338907855510732658, 0.6233112732207619633 ) ) ;
#113353 = ORIENTED_EDGE ( 'NONE', *, *, #41193, .F. ) ;
#113352 = DIRECTION ( 'NONE',  ( 1.000000000000000000, 0.000000000000000000, 0.000000000000000000 ) ) ;
#113354 = CARTESIAN_POINT ( 'NONE',  ( -18.50000000000000000, 11.65000000001115232, -79.15000000000004832 ) ) ;
#113355 = ORIENTED_EDGE ( 'NONE', *, *, #203886, .F. ) ;
#113356 =( BOUNDED_SURFACE ( )  B_SPLINE_SURFACE ( 3, 2, ( 
 ( #108369, #104476, #103202 ),
 ( #62812, #184039, #9256 ),
 ( #4118, #5377, #124088 ),
 ( #142340, #84907, #164499 ) ),
 .UNSPECIFIED., .F., .F., .F. ) 
 B_SPLINE_SURFACE_WITH_KNOTS ( ( 4, 4 ),
 ( 3, 3 ),
 ( -1.028636811145622332E-17, 0.0003124336600439521472 ),
 ( 0.000000000000000000, 1.000000000000000000 ),
 .UNSPECIFIED. ) 
 GEOMETRIC_REPRESENTATION_ITEM ( )  RATIONAL_B_SPLINE_SURFACE ( (
 ( 1.000000000000000000, 0.7071067811865475727, 1.000000000000000000),
 ( 1.000000000000000000, 0.7089187706049935311, 1.000000000000000000),
 ( 1.000000000000000000, 0.7039288185051780777, 1.000000000000000000),
 ( 1.000000000000000000, 0.7040654476015839602, 1.000000000000000000) ) ) 
 REPRESENTATION_ITEM ( '' )  SURFACE ( )  );
#113357 = ORIENTED_EDGE ( 'NONE', *, *, #183609, .T. ) ;
#113358 = CARTESIAN_POINT ( 'NONE',  ( -18.41418431465368499, -0.7490476236419166822, -242.2033265267436377 ) ) ;
#113359 = EDGE_CURVE ( 'NONE', #85475, #1689, #226831, .T. ) ;
#113360 = ORIENTED_EDGE ( 'NONE', *, *, #61009, .T. ) ;
#113361 = CARTESIAN_POINT ( 'NONE',  ( 20.94999999999999574, 39.15282200719421013, -236.7930294976410437 ) ) ;
#113362 = DIRECTION ( 'NONE',  ( 1.000000000000000000, 0.000000000000000000, 0.000000000000000000 ) ) ;
#113363 = ADVANCED_FACE ( 'NONE', ( #138763 ), #39738, .F. ) ;
#113364 = VECTOR ( 'NONE', #167991, 1000.000000000000000 ) ;
#113366 = ORIENTED_EDGE ( 'NONE', *, *, #131358, .F. ) ;
#113365 = ORIENTED_EDGE ( 'NONE', *, *, #113581, .F. ) ;
#113367 = ORIENTED_EDGE ( 'NONE', *, *, #60981, .T. ) ;
#113368 = CARTESIAN_POINT ( 'NONE',  ( -21.64999999999999858, 10.05000000001113847, -154.7500000000000284 ) ) ;
#113369 = VERTEX_POINT ( 'NONE', #60539 ) ;
#113370 =( BOUNDED_SURFACE ( )  B_SPLINE_SURFACE ( 3, 2, ( 
 ( #69243, #70541, #90056 ),
 ( #232169, #53513, #169656 ),
 ( #110916, #190485, #250422 ),
 ( #11847, #91367, #254259 ),
 ( #177349, #75667, #217693 ),
 ( #54782, #19535, #57340 ),
 ( #237292, #256787, #39108 ),
 ( #212601, #18242, #238563 ) ),
 .UNSPECIFIED., .F., .F., .F. ) 
 B_SPLINE_SURFACE_WITH_KNOTS ( ( 4, 2, 2, 4 ),
 ( 3, 3 ),
 ( 0.0001723339234021441008, 0.0002782939632049936159, 0.0003842540030078431582, 0.0005961740826135421886 ),
 ( 0.000000000000000000, 1.000000000000000000 ),
 .UNSPECIFIED. ) 
 GEOMETRIC_REPRESENTATION_ITEM ( )  RATIONAL_B_SPLINE_SURFACE ( (
 ( 1.000000000000000000, 0.9504532311154701985, 1.000000000000000000),
 ( 1.000000000000000000, 0.9506023220711478094, 1.000000000000000000),
 ( 1.000000000000000000, 0.9395774818179351007, 1.000000000000000000),
 ( 1.000000000000000000, 0.9079328464649522035, 1.000000000000000000),
 ( 1.000000000000000000, 0.8875702416205013545, 1.000000000000000000),
 ( 1.000000000000000000, 0.8205919608041974955, 1.000000000000000000),
 ( 1.000000000000000000, 0.7666842783597154209, 1.000000000000000000),
 ( 1.000000000000000000, 0.7071067811864398811, 1.000000000000000000) ) ) 
 REPRESENTATION_ITEM ( '' )  SURFACE ( )  );
#113371 = ORIENTED_EDGE ( 'NONE', *, *, #240800, .F. ) ;
#113372 = CARTESIAN_POINT ( 'NONE',  ( 19.58285714285715073, 66.98499851036405062, -195.1024546684426753 ) ) ;
#113374 = VERTEX_POINT ( 'NONE', #186620 ) ;
#113373 = CARTESIAN_POINT ( 'NONE',  ( 18.39999999999999858, -9.499999999988844479, -107.1001893912220879 ) ) ;
#113375 = FACE_OUTER_BOUND ( 'NONE', #235708, .T. ) ;
#113377 = DIRECTION ( 'NONE',  ( -1.000000000000000000, 0.000000000000000000, 0.000000000000000000 ) ) ;
#113376 = CARTESIAN_POINT ( 'NONE',  ( 20.94999999999999929, 76.00000000001244871, -170.0231074845243597 ) ) ;
#113378 = ADVANCED_FACE ( 'NONE', ( #10546 ), #92621, .F. ) ;
#113379 = FACE_OUTER_BOUND ( 'NONE', #32940, .T. ) ;
#113380 = CARTESIAN_POINT ( 'NONE',  ( 18.49505832270840955, -9.438028062771737225, -74.19847317489390548 ) ) ;
#113381 = CARTESIAN_POINT ( 'NONE',  ( 21.22070241538126467, 30.71396139465468167, -252.1060412414022949 ) ) ;
#113382 = ORIENTED_EDGE ( 'NONE', *, *, #248969, .F. ) ;
#113383 = EDGE_CURVE ( 'NONE', #182454, #221113, #251713, .T. ) ;
#113384 = ORIENTED_EDGE ( 'NONE', *, *, #221498, .F. ) ;
#113385 = CARTESIAN_POINT ( 'NONE',  ( 18.59999999999999787, 18.92285928089247804, -233.3572654221044900 ) ) ;
#113386 = CARTESIAN_POINT ( 'NONE',  ( -20.94999999999999929, 5.900000000011162093, -90.28090023534366537 ) ) ;
#113387 = DIRECTION ( 'NONE',  ( -0.000000000000000000, 6.982962677686266711E-15, -1.000000000000000000 ) ) ;
#113389 = EDGE_CURVE ( 'NONE', #203210, #68317, #171461, .T. ) ;
#113388 = ORIENTED_EDGE ( 'NONE', *, *, #91634, .F. ) ;
#113390 = CARTESIAN_POINT ( 'NONE',  ( -21.14999999999999858, 6.540656951712397138, -67.00000000000004263 ) ) ;
#113391 =( BOUNDED_CURVE ( )  B_SPLINE_CURVE ( 3, ( #13046, #155133, #135512, #234631 ),
 .UNSPECIFIED., .F., .F. ) 
 B_SPLINE_CURVE_WITH_KNOTS ( ( 4, 4 ),
 ( 0.3000847527772391166, 0.5517402753107891744 ),
 .UNSPECIFIED. ) 
 CURVE ( )  GEOMETRIC_REPRESENTATION_ITEM ( )  RATIONAL_B_SPLINE_CURVE ( ( 1.000000000000000000, 0.9947294176030464508, 0.9947294176030464508, 1.000000000000000000 ) ) 
 REPRESENTATION_ITEM ( '' )  );
#113392 = AXIS2_PLACEMENT_3D ( 'NONE', #210669, #71183, #131129 ) ;
#113393 = CARTESIAN_POINT ( 'NONE',  ( -21.05000000000000071, 1.115600667400684642E-11, -167.5000000000000284 ) ) ;
#113394 = CARTESIAN_POINT ( 'NONE',  ( -20.64999999999999858, 71.65000000001259650, -191.1731074845243654 ) ) ;
#113395 = ORIENTED_EDGE ( 'NONE', *, *, #145097, .T. ) ;
#113396 = ORIENTED_EDGE ( 'NONE', *, *, #229619, .T. ) ;
#113397 = CARTESIAN_POINT ( 'NONE',  ( 20.04142135623730070, 64.35000000001198828, -115.2731074845243739 ) ) ;
#113398 = DIRECTION ( 'NONE',  ( 0.000000000000000000, 0.000000000000000000, 1.000000000000000000 ) ) ;
#113399 = ORIENTED_EDGE ( 'NONE', *, *, #104740, .F. ) ;
#113400 = CYLINDRICAL_SURFACE ( 'NONE', #5655, 0.1000000000000028644 ) ;
#113401 = ORIENTED_EDGE ( 'NONE', *, *, #188775, .T. ) ;
#113402 = ADVANCED_FACE ( 'NONE', ( #67936 ), #151352, .F. ) ;
#113403 = CARTESIAN_POINT ( 'NONE',  ( 18.39999999999999858, -9.682403433465237796, -140.6568433774128266 ) ) ;
#113404 = CARTESIAN_POINT ( 'NONE',  ( -16.81744102076748959, 9.950000000011138823, -154.8500000000000227 ) ) ;
#113405 = DIRECTION ( 'NONE',  ( 0.000000000000000000, 0.000000000000000000, -1.000000000000000000 ) ) ;
#113406 = DIRECTION ( 'NONE',  ( 0.000000000000000000, 0.000000000000000000, -1.000000000000000000 ) ) ;
#113408 = ADVANCED_FACE ( 'NONE', ( #148776 ), #9244, .T. ) ;
#113407 = DIRECTION ( 'NONE',  ( 1.000000000000000000, 0.000000000000000000, 0.000000000000000000 ) ) ;
#113409 = AXIS2_PLACEMENT_3D ( 'NONE', #216094, #72783, #252650 ) ;
#113411 = EDGE_LOOP ( 'NONE', ( #27974, #232877, #94527, #64635 ) ) ;
#113410 = LINE ( 'NONE', #174719, #27544 ) ;
#113412 = AXIS2_PLACEMENT_3D ( 'NONE', #242480, #202086, #85949 ) ;
#113414 = EDGE_LOOP ( 'NONE', ( #168980, #230651, #190042, #103131 ) ) ;
#113413 = ORIENTED_EDGE ( 'NONE', *, *, #35793, .T. ) ;
#113415 = VERTEX_POINT ( 'NONE', #13115 ) ;
#113416 = CIRCLE ( 'NONE', #9348, 0.09999999999999817368 ) ;
#113417 = DIRECTION ( 'NONE',  ( -1.000000000000000000, -0.000000000000000000, -0.000000000000000000 ) ) ;
#113418 = CARTESIAN_POINT ( 'NONE',  ( 20.94999999999999929, -1.835859311432481045, -179.0044391687985410 ) ) ;
#113419 = DIRECTION ( 'NONE',  ( 1.000000000000000000, 0.000000000000000000, 0.000000000000000000 ) ) ;
#113421 = DIRECTION ( 'NONE',  ( -1.000000000000000000, 0.000000000000000000, 0.000000000000000000 ) ) ;
#113420 = CARTESIAN_POINT ( 'NONE',  ( -16.77683809663752257, 66.05416425680839154, -182.6870565036286393 ) ) ;
#113422 = DIRECTION ( 'NONE',  ( 1.000000000000000000, 0.000000000000000000, 0.000000000000000000 ) ) ;
#113423 = ORIENTED_EDGE ( 'NONE', *, *, #230785, .T. ) ;
#113424 = DIRECTION ( 'NONE',  ( 0.000000000000000000, -0.9915357197604971473, 0.1298341882519111479 ) ) ;
#113425 = EDGE_LOOP ( 'NONE', ( #153754, #244195, #220186, #196950 ) ) ;
#113426 = ORIENTED_EDGE ( 'NONE', *, *, #152813, .T. ) ;
#113427 = FACE_OUTER_BOUND ( 'NONE', #47924, .T. ) ;
#113429 = CIRCLE ( 'NONE', #46769, 0.1000000000000028644 ) ;
#113428 = CARTESIAN_POINT ( 'NONE',  ( -21.05000000000000071, 70.53171716061257257, -228.4612385850772682 ) ) ;
#113430 = CIRCLE ( 'NONE', #238306, 0.09999999999999939493 ) ;
#113431 = CARTESIAN_POINT ( 'NONE',  ( 20.94999999999999574, 1.115600667400684642E-11, -167.4999999999999716 ) ) ;
#113432 = FACE_OUTER_BOUND ( 'NONE', #226843, .T. ) ;
#113433 = CARTESIAN_POINT ( 'NONE',  ( 23.15000000000000213, -9.499999999988844479, -90.60603087734760663 ) ) ;
#113434 = ORIENTED_EDGE ( 'NONE', *, *, #103873, .F. ) ;
#113435 = ORIENTED_EDGE ( 'NONE', *, *, #83875, .T. ) ;
#113436 = CARTESIAN_POINT ( 'NONE',  ( 22.60000000000000142, 0.04781839071596408891, -88.74997758095283018 ) ) ;
#113437 = DIRECTION ( 'NONE',  ( -0.000000000000000000, 6.982962677686266711E-15, -1.000000000000000000 ) ) ;
#113438 = CARTESIAN_POINT ( 'NONE',  ( -20.85000000000000142, 69.06610602788535402, -65.73746165015079157 ) ) ;
#113439 = DIRECTION ( 'NONE',  ( 1.000000000000000000, 0.000000000000000000, 0.000000000000000000 ) ) ;
#113440 = CARTESIAN_POINT ( 'NONE',  ( -16.84419801905645997, 9.950000000011140600, -188.3305101537779080 ) ) ;
#113441 = LINE ( 'NONE', #195569, #155021 ) ;
#113442 = CARTESIAN_POINT ( 'NONE',  ( -22.00356870141260401, 7.254242362502188790, -33.49999999999084821 ) ) ;
#113445 = CARTESIAN_POINT ( 'NONE',  ( 23.14999999999999503, 6.450000000011156587, -155.1500000000000057 ) ) ;
#113444 = VECTOR ( 'NONE', #209804, 1000.000000000000000 ) ;
#113443 = CARTESIAN_POINT ( 'NONE',  ( -20.94999999999999929, 87.48912529308749697, -39.02310748452423894 ) ) ;
#113447 = CARTESIAN_POINT ( 'NONE',  ( 20.94999999999999574, -11.48912529306490349, -36.39999999999999858 ) ) ;
#113446 = AXIS2_PLACEMENT_3D ( 'NONE', #7027, #202656, #222195 ) ;
#113448 = CARTESIAN_POINT ( 'NONE',  ( 21.05000000000000071, 65.51556651036987944, -62.06630168303249206 ) ) ;
#113449 = CARTESIAN_POINT ( 'NONE',  ( 21.14999999999999858, 69.45934304831114048, -169.9231074845244223 ) ) ;
#113450 = CARTESIAN_POINT ( 'NONE',  ( 20.94983749550516450, 10.29766095125282810, -139.4743663933276139 ) ) ;
#113452 = ORIENTED_EDGE ( 'NONE', *, *, #200336, .T. ) ;
#113451 = CYLINDRICAL_SURFACE ( 'NONE', #132095, 14.30833333333333890 ) ;
#113453 = CARTESIAN_POINT ( 'NONE',  ( 23.14999999999999503, 11.65000000001116298, -79.15000000000004832 ) ) ;
#113454 = EDGE_CURVE ( 'NONE', #161516, #112286, #245305, .T. ) ;
#113455 = DIRECTION ( 'NONE',  ( -1.652117596168391897E-15, 0.4088369013363281068, -0.9126074666063770380 ) ) ;
#113456 = ADVANCED_FACE ( 'NONE', ( #211305 ), #130474, .T. ) ;
#113457 = ADVANCED_FACE ( 'NONE', ( #210036 ), #694, .F. ) ;
#113458 = CARTESIAN_POINT ( 'NONE',  ( 21.05000000000000071, 18.80454058543246276, -232.7833891117047074 ) ) ;
#113459 = DIRECTION ( 'NONE',  ( 0.000000000000000000, 0.000000000000000000, -1.000000000000000000 ) ) ;
#113461 = CIRCLE ( 'NONE', #17759, 2.599999999999998312 ) ;
#113460 = DIRECTION ( 'NONE',  ( -1.000000000000000000, -0.000000000000000000, -0.000000000000000000 ) ) ;
#113462 = CIRCLE ( 'NONE', #205019, 0.6000000000000033085 ) ;
#113463 = CARTESIAN_POINT ( 'NONE',  ( 23.25000000000000000, 84.59626168225560150, -194.0729799673740104 ) ) ;
#113464 = CARTESIAN_POINT ( 'NONE',  ( 18.58143601961869251, 10.43572941509456342, -24.75000000000000000 ) ) ;
#113465 = CARTESIAN_POINT ( 'NONE',  ( -20.94999999999999929, -11.65000000000000036, -30.59999999999999432 ) ) ;
#113466 = ORIENTED_EDGE ( 'NONE', *, *, #37540, .F. ) ;
#113467 = CARTESIAN_POINT ( 'NONE',  ( -21.14999999999999858, 0.000000000000000000, 0.000000000000000000 ) ) ;
#113469 = ORIENTED_EDGE ( 'NONE', *, *, #228041, .T. ) ;
#113468 = DIRECTION ( 'NONE',  ( 0.000000000000000000, 0.2617529984165152257, 0.9651348961777124202 ) ) ;
#113470 = CARTESIAN_POINT ( 'NONE',  ( 13.40000000000005898, 67.65000000001118963, -25.06452884076209742 ) ) ;
#113471 = EDGE_CURVE ( 'NONE', #222093, #123180, #170514, .T. ) ;
#113472 = CIRCLE ( 'NONE', #1003, 4.000000000000003553 ) ;
#113473 = DIRECTION ( 'NONE',  ( 0.000000000000000000, 1.000000000000000000, 0.000000000000000000 ) ) ;
#113474 = FACE_OUTER_BOUND ( 'NONE', #42569, .T. ) ;
#113475 = ORIENTED_EDGE ( 'NONE', *, *, #8665, .T. ) ;
#113476 = CARTESIAN_POINT ( 'NONE',  ( 18.50000000000000000, -9.499999999988842703, -122.2500000000000284 ) ) ;
#113477 = AXIS2_PLACEMENT_3D ( 'NONE', #42576, #219933, #58275 ) ;
#113478 = APPLICATION_PROTOCOL_DEFINITION ( 'draft international standard', 'automotive_design', 1998, #168951 ) ;
#113479 = LINE ( 'NONE', #195616, #31557 ) ;
#113481 = VECTOR ( 'NONE', #100118, 1000.000000000000000 ) ;
#113480 = DIRECTION ( 'NONE',  ( 1.000000000000000000, 0.000000000000000000, 0.000000000000000000 ) ) ;
#113482 = ORIENTED_EDGE ( 'NONE', *, *, #37249, .T. ) ;
#113483 = AXIS2_PLACEMENT_3D ( 'NONE', #257931, #78056, #119787 ) ;
#113484 = DIRECTION ( 'NONE',  ( 0.000000000000000000, 0.000000000000000000, -1.000000000000000000 ) ) ;
#113485 = CARTESIAN_POINT ( 'NONE',  ( 20.94999999999999929, 31.15787740146373253, -259.8205824356103903 ) ) ;
#113486 = AXIS2_PLACEMENT_3D ( 'NONE', #48258, #109503, #70432 ) ;
#113487 = AXIS2_PLACEMENT_3D ( 'NONE', #187284, #105114, #242087 ) ;
#113488 = AXIS2_PLACEMENT_3D ( 'NONE', #43993, #205622, #148228 ) ;
#113489 = FACE_OUTER_BOUND ( 'NONE', #119211, .T. ) ;
#113490 = EDGE_CURVE ( 'NONE', #257629, #109697, #96392, .T. ) ;
#113491 = ORIENTED_EDGE ( 'NONE', *, *, #85724, .T. ) ;
#113492 = EDGE_CURVE ( 'NONE', #62, #85530, #233802, .T. ) ;
#113493 = ORIENTED_EDGE ( 'NONE', *, *, #32115, .F. ) ;
#113495 = AXIS2_PLACEMENT_3D ( 'NONE', #48960, #153240, #149380 ) ;
#113494 = LINE ( 'NONE', #95215, #54836 ) ;
#113497 = CIRCLE ( 'NONE', #192612, 0.09999999999999983902 ) ;
#113496 = DIRECTION ( 'NONE',  ( 0.000000000000000000, -1.224646799142185182E-16, 1.000000000000000000 ) ) ;
#113498 = CARTESIAN_POINT ( 'NONE',  ( -21.55000000000000426, 7.708578643762696636, -12.34999999999999964 ) ) ;
#113499 = CARTESIAN_POINT ( 'NONE',  ( -16.97092634996718274, 30.24786202487886300, -234.7715630666886568 ) ) ;
#113500 = ADVANCED_FACE ( 'NONE', ( #168375 ), #113370, .T. ) ;
#113502 = CARTESIAN_POINT ( 'NONE',  ( 22.43288208788031568, -2.474269879911711101, -189.6161341957261470 ) ) ;
#113501 = CARTESIAN_POINT ( 'NONE',  ( -23.25000000000000000, 1.115600667400684642E-11, -102.6000000000000512 ) ) ;
#113503 = AXIS2_PLACEMENT_3D ( 'NONE', #248598, #12580, #171667 ) ;
#113504 = AXIS2_PLACEMENT_3D ( 'NONE', #36454, #194243, #230797 ) ;
#113505 = CARTESIAN_POINT ( 'NONE',  ( -21.14250536705909411, 76.00000000001242029, -176.5412796614051274 ) ) ;
#113506 = DIRECTION ( 'NONE',  ( 1.000000000000000000, -0.000000000000000000, -0.000000000000000000 ) ) ;
#113507 = CARTESIAN_POINT ( 'NONE',  ( -18.59999999999999787, 9.350000000011156942, -155.1500000000000057 ) ) ;
#113508 = CARTESIAN_POINT ( 'NONE',  ( -23.39999999999994529, 74.73834681386826162, -44.00978271863746016 ) ) ;
#113509 = ORIENTED_EDGE ( 'NONE', *, *, #256562, .T. ) ;
#113511 = ORIENTED_EDGE ( 'NONE', *, *, #2239, .F. ) ;
#113510 = DIRECTION ( 'NONE',  ( 1.000000000000000000, 0.000000000000000000, 0.000000000000000000 ) ) ;
#113512 = FACE_OUTER_BOUND ( 'NONE', #31577, .T. ) ;
#113513 = AXIS2_PLACEMENT_3D ( 'NONE', #29008, #11993, #210185 ) ;
#113514 = CARTESIAN_POINT ( 'NONE',  ( -23.25000000000000000, -1.851617760457748618, -145.6031897196037050 ) ) ;
#113516 = CARTESIAN_POINT ( 'NONE',  ( -16.87036670365548474, 9.989418819312801290, -154.9795601173020714 ) ) ;
#113515 = CARTESIAN_POINT ( 'NONE',  ( -20.64999999999999858, 46.05992536685982230, -240.5730681801377102 ) ) ;
#113517 = CIRCLE ( 'NONE', #75922, 3.999999999999999112 ) ;
#113518 = VERTEX_POINT ( 'NONE', #178626 ) ;
#113519 = CARTESIAN_POINT ( 'NONE',  ( -18.50000000000000000, 1.162701749938009677, -8.099999999999999645 ) ) ;
#113520 = LINE ( 'NONE', #35309, #237315 ) ;
#113521 = CARTESIAN_POINT ( 'NONE',  ( -21.05000000000000071, 69.69503888732695884, -103.0017219185864121 ) ) ;
#113523 = CARTESIAN_POINT ( 'NONE',  ( -22.47071067811865319, 0.09909245470260570621, 7.720074744498060859 ) ) ;
#113522 = AXIS2_PLACEMENT_3D ( 'NONE', #21666, #163744, #64627 ) ;
#113524 = ORIENTED_EDGE ( 'NONE', *, *, #183003, .T. ) ;
#113525 = ORIENTED_EDGE ( 'NONE', *, *, #235477, .T. ) ;
#113526 = EDGE_CURVE ( 'NONE', #109066, #156163, #187999, .T. ) ;
#113527 = CARTESIAN_POINT ( 'NONE',  ( 23.24999999999999645, 70.40000000001246860, -181.7731074845244166 ) ) ;
#113528 = ORIENTED_EDGE ( 'NONE', *, *, #63131, .F. ) ;
#113529 = CARTESIAN_POINT ( 'NONE',  ( 18.49999999999999645, 0.000000000000000000, -33.50000000000000000 ) ) ;
#113530 = VECTOR ( 'NONE', #41370, 1000.000000000000000 ) ;
#113531 = CARTESIAN_POINT ( 'NONE',  ( 23.25000000000000000, -9.599999999988849453, -88.75000000000004263 ) ) ;
#113532 = CIRCLE ( 'NONE', #76107, 0.09999999999999817368 ) ;
#113533 = PLANE ( 'NONE',  #219091 ) ;
#113534 = EDGE_CURVE ( 'NONE', #163189, #153155, #204722, .T. ) ;
#113535 = EDGE_CURVE ( 'NONE', #201212, #146715, #159059, .T. ) ;
#113536 = VERTEX_POINT ( 'NONE', #198152 ) ;
#113537 = DIRECTION ( 'NONE',  ( 0.000000000000000000, -0.9915357197604792727, 0.1298341882520475943 ) ) ;
#113538 = EDGE_CURVE ( 'NONE', #7014, #65920, #97740, .T. ) ;
#113540 = ADVANCED_FACE ( 'NONE', ( #233461 ), #139994, .T. ) ;
#113539 = CARTESIAN_POINT ( 'NONE',  ( 23.15000000000000213, 87.75000000001192291, -106.1231074845242262 ) ) ;
#113541 = DIRECTION ( 'NONE',  ( 0.000000000000000000, 0.9126074666063772600, 0.4088369013363276627 ) ) ;
#113542 = CYLINDRICAL_SURFACE ( 'NONE', #147721, 0.09999999999998898659 ) ;
#113544 = LINE ( 'NONE', #107447, #45787 ) ;
#113543 = DIRECTION ( 'NONE',  ( 1.000000000000000000, 0.000000000000000000, 0.000000000000000000 ) ) ;
#113545 = CARTESIAN_POINT ( 'NONE',  ( -16.89155683852755274, 66.05000000001493277, -149.8004793340643346 ) ) ;
#113546 = VERTEX_POINT ( 'NONE', #76919 ) ;
#113547 = CIRCLE ( 'NONE', #96938, 14.20833333333333748 ) ;
#113548 = DIRECTION ( 'NONE',  ( 0.000000000000000000, 0.000000000000000000, -1.000000000000000000 ) ) ;
#113549 = VERTEX_POINT ( 'NONE', #74401 ) ;
#113551 = ORIENTED_EDGE ( 'NONE', *, *, #105654, .T. ) ;
#113550 = DIRECTION ( 'NONE',  ( 1.000000000000000000, -7.049440681616512959E-16, 1.911869773728117674E-16 ) ) ;
#113552 = EDGE_CURVE ( 'NONE', #117400, #172386, #154699, .T. ) ;
#113553 = ORIENTED_EDGE ( 'NONE', *, *, #118413, .F. ) ;
#113554 = CARTESIAN_POINT ( 'NONE',  ( 22.57320508075687115, 12.67709964810647882, -223.3751320524553705 ) ) ;
#113555 = EDGE_CURVE ( 'NONE', #145192, #223514, #246435, .T. ) ;
#113556 = DIRECTION ( 'NONE',  ( 0.7071067811865463515, -0.7071067811865487940, -5.696443396193425170E-15 ) ) ;
#113557 = DIRECTION ( 'NONE',  ( 0.000000000000000000, 0.1298341882520022694, 0.9915357197604852679 ) ) ;
#113558 = CARTESIAN_POINT ( 'NONE',  ( -20.64999999999999858, -9.500000000000001776, -23.60603087734756045 ) ) ;
#113559 = VECTOR ( 'NONE', #138488, 1000.000000000000000 ) ;
#113560 = ORIENTED_EDGE ( 'NONE', *, *, #253780, .T. ) ;
#113561 = CARTESIAN_POINT ( 'NONE',  ( 21.15000000000000213, 8.786607556611267356, -112.7500000000000284 ) ) ;
#113563 = EDGE_CURVE ( 'NONE', #210574, #57819, #167351, .T. ) ;
#113562 = CARTESIAN_POINT ( 'NONE',  ( -21.45000000000000284, 7.708578643773852157, -88.15000000000004832 ) ) ;
#113564 = ORIENTED_EDGE ( 'NONE', *, *, #60219, .T. ) ;
#113565 = DIRECTION ( 'NONE',  ( 0.000000000000000000, 1.000000000000000000, 0.000000000000000000 ) ) ;
#113566 = ADVANCED_FACE ( 'NONE', ( #234722 ), #56053, .T. ) ;
#113567 = CARTESIAN_POINT ( 'NONE',  ( 21.11927991906888025, 6.448493118491415821, 0.009083679473894629153 ) ) ;
#113568 = VERTEX_POINT ( 'NONE', #116069 ) ;
#113569 = CARTESIAN_POINT ( 'NONE',  ( -23.15000000000000213, 1.999999999999998224, -20.27537807723789953 ) ) ;
#113570 = EDGE_CURVE ( 'NONE', #28860, #56926, #195617, .T. ) ;
#113571 = EDGE_CURVE ( 'NONE', #138609, #234093, #213110, .T. ) ;
#113572 = AXIS2_PLACEMENT_3D ( 'NONE', #94267, #79820, #198508 ) ;
#113573 = VERTEX_POINT ( 'NONE', #242406 ) ;
#113574 = CARTESIAN_POINT ( 'NONE',  ( 18.39999999999999858, -9.499999999988842703, -141.0320693966996828 ) ) ;
#113575 = ORIENTED_EDGE ( 'NONE', *, *, #61688, .F. ) ;
#113576 = CARTESIAN_POINT ( 'NONE',  ( -22.59999999999999787, 75.89914163091376054, -181.7726746080137445 ) ) ;
#113577 = ADVANCED_FACE ( 'NONE', ( #3811 ), #143310, .F. ) ;
#113578 = DIRECTION ( 'NONE',  ( 1.000000000000000000, 0.000000000000000000, 0.000000000000000000 ) ) ;
#113579 = CARTESIAN_POINT ( 'NONE',  ( 22.39999999999999503, 75.90000000001273861, -211.3138870828977360 ) ) ;
#113580 = FACE_OUTER_BOUND ( 'NONE', #209645, .T. ) ;
#113581 = EDGE_CURVE ( 'NONE', #177623, #184620, #196354, .T. ) ;
#113582 = ADVANCED_FACE ( 'NONE', ( #182464 ), #218995, .F. ) ;
#113583 = EDGE_CURVE ( 'NONE', #201185, #235613, #229692, .T. ) ;
#113584 = DIRECTION ( 'NONE',  ( 1.000000000000000000, 0.000000000000000000, 0.000000000000000000 ) ) ;
#113585 = CYLINDRICAL_SURFACE ( 'NONE', #15623, 0.09999999999999609201 ) ;
#113586 = DIRECTION ( 'NONE',  ( 1.000000000000000000, 0.000000000000000000, 0.000000000000000000 ) ) ;
#113587 = ORIENTED_EDGE ( 'NONE', *, *, #187380, .F. ) ;
#113589 = DIRECTION ( 'NONE',  ( 0.000000000000000000, 6.982962677686266711E-15, -1.000000000000000000 ) ) ;
#113588 = DIRECTION ( 'NONE',  ( -0.000000000000000000, 0.4088369013363276072, -0.9126074666063772600 ) ) ;
#113591 = ORIENTED_EDGE ( 'NONE', *, *, #59122, .T. ) ;
#113590 = CIRCLE ( 'NONE', #255176, 0.09999999999999939493 ) ;
#113594 = ORIENTED_EDGE ( 'NONE', *, *, #217790, .F. ) ;
#113593 = DIRECTION ( 'NONE',  ( -1.000000000000000000, -0.000000000000000000, -0.000000000000000000 ) ) ;
#113592 = CARTESIAN_POINT ( 'NONE',  ( -23.25000000000000000, -1.851617760457748618, -145.6031897196037050 ) ) ;
#113595 = ORIENTED_EDGE ( 'NONE', *, *, #135951, .T. ) ;
#113596 = DIRECTION ( 'NONE',  ( 0.000000000000000000, -0.4721928772777489458, -0.8814952561688353949 ) ) ;
#113597 = CARTESIAN_POINT ( 'NONE',  ( 23.24999999999999645, 78.10000000001214460, -136.5231074845243029 ) ) ;
#113599 = CARTESIAN_POINT ( 'NONE',  ( -23.25000000000000000, -1.835859311432481045, -145.5044391687985694 ) ) ;
#113598 = VECTOR ( 'NONE', #124667, 1000.000000000000000 ) ;
#113600 = CARTESIAN_POINT ( 'NONE',  ( 20.95462737510932882, 59.02401302535630379, -225.7858342150956616 ) ) ;
#113601 = ORIENTED_EDGE ( 'NONE', *, *, #46609, .T. ) ;
#113603 = VERTEX_POINT ( 'NONE', #125050 ) ;
#113602 = CARTESIAN_POINT ( 'NONE',  ( 18.49999999999998934, 11.65000000000000391, -24.75000000000000000 ) ) ;
#113604 = ADVANCED_FACE ( 'NONE', ( #204569 ), #179896, .T. ) ;
#113606 = CARTESIAN_POINT ( 'NONE',  ( 18.59999999999999076, 15.51794587355511901, -222.9505302427971003 ) ) ;
#113605 = DIRECTION ( 'NONE',  ( 0.000000000000000000, 6.982962677686267499E-15, -1.000000000000000000 ) ) ;
#113608 = ORIENTED_EDGE ( 'NONE', *, *, #66443, .F. ) ;
#113607 = FACE_OUTER_BOUND ( 'NONE', #4513, .T. ) ;
#113609 = VECTOR ( 'NONE', #206697, 1000.000000000000000 ) ;
#113610 = AXIS2_PLACEMENT_3D ( 'NONE', #128715, #70040, #50425 ) ;
#113611 = EDGE_LOOP ( 'NONE', ( #59776, #23113, #61239 ) ) ;
#113612 = CARTESIAN_POINT ( 'NONE',  ( 20.95378194480896639, 11.90346680009650449, -206.1499410747357786 ) ) ;
#113613 = CARTESIAN_POINT ( 'NONE',  ( 11.60000000000000142, -8.350000000000004974, 19.04142135623731136 ) ) ;
#113614 = ORIENTED_EDGE ( 'NONE', *, *, #229524, .F. ) ;
#113615 = CARTESIAN_POINT ( 'NONE',  ( -23.15000000000000213, 4.250000000011156409, -188.6499999999999488 ) ) ;
#113616 = ORIENTED_EDGE ( 'NONE', *, *, #154720, .F. ) ;
#113617 = VECTOR ( 'NONE', #148553, 1000.000000000000000 ) ;
#113618 = CARTESIAN_POINT ( 'NONE',  ( -18.38204789744325396, 11.47950103717623982, -158.2500000000000284 ) ) ;
#113619 = DIRECTION ( 'NONE',  ( -0.000000000000000000, -0.9770955615653316162, -0.2128009952263597848 ) ) ;
#113620 = EDGE_LOOP ( 'NONE', ( #185572, #29612, #15584, #242517 ) ) ;
#113621 = DIRECTION ( 'NONE',  ( 0.000000000000000000, 0.9968797965484670343, 0.07893460099023182075 ) ) ;
#113622 = AXIS2_PLACEMENT_3D ( 'NONE', #3130, #120559, #61852 ) ;
#113623 = AXIS2_PLACEMENT_3D ( 'NONE', #223893, #221321, #84344 ) ;
#113624 = CIRCLE ( 'NONE', #134274, 0.1000000000000013933 ) ;
#113625 = CIRCLE ( 'NONE', #146916, 0.09999999999998898659 ) ;
#113626 = EDGE_CURVE ( 'NONE', #145347, #204451, #119942, .T. ) ;
#113628 = EDGE_CURVE ( 'NONE', #145358, #197707, #6366, .T. ) ;
#113627 = CARTESIAN_POINT ( 'NONE',  ( 21.05000000000000071, 1.115600667400684642E-11, -100.5000000000000284 ) ) ;
#113629 = VERTEX_POINT ( 'NONE', #23405 ) ;
#113630 = EDGE_LOOP ( 'NONE', ( #88608, #107534, #37454, #214111 ) ) ;
#113631 = CARTESIAN_POINT ( 'NONE',  ( 20.87631937322875331, 18.75490874231121552, -228.0812301260858987 ) ) ;
#113632 = ORIENTED_EDGE ( 'NONE', *, *, #167466, .F. ) ;
#113633 = ADVANCED_FACE ( 'NONE', ( #1215 ), #221541, .T. ) ;
#113634 = CARTESIAN_POINT ( 'NONE',  ( 23.15000000000000213, -12.41227409413852811, -164.4000000000000057 ) ) ;
#113635 = VERTEX_POINT ( 'NONE', #200728 ) ;
#113638 = EDGE_CURVE ( 'NONE', #33602, #144336, #254608, .T. ) ;
#113637 = EDGE_LOOP ( 'NONE', ( #85379, #202966, #148674, #142192 ) ) ;
#113636 = DIRECTION ( 'NONE',  ( -1.000000000000000000, 0.000000000000000000, 0.000000000000000000 ) ) ;
#113639 = EDGE_LOOP ( 'NONE', ( #29596, #20985, #199317, #2067 ) ) ;
#113640 = CARTESIAN_POINT ( 'NONE',  ( 18.59999999999999076, 10.20857864377385127, -188.8499999999999659 ) ) ;
#113641 = ORIENTED_EDGE ( 'NONE', *, *, #21633, .F. ) ;
#113644 = ORIENTED_EDGE ( 'NONE', *, *, #235689, .T. ) ;
#113643 = ORIENTED_EDGE ( 'NONE', *, *, #122780, .F. ) ;
#113642 = CARTESIAN_POINT ( 'NONE',  ( 19.92426406871192412, 11.75000000001116085, -192.3499999999999375 ) ) ;
#113645 = CIRCLE ( 'NONE', #130567, 0.1999999999999996503 ) ;
#113646 = ORIENTED_EDGE ( 'NONE', *, *, #36088, .F. ) ;
#113647 = DIRECTION ( 'NONE',  ( -1.000000000000000000, -2.952720810173289112E-16, 0.000000000000000000 ) ) ;
#113648 = ORIENTED_EDGE ( 'NONE', *, *, #197533, .F. ) ;
#113649 = CIRCLE ( 'NONE', #22662, 0.5000000000000008882 ) ;
#113650 = DIRECTION ( 'NONE',  ( -2.952720810173289112E-16, 1.000000000000000000, 0.000000000000000000 ) ) ;
#113651 = AXIS2_PLACEMENT_3D ( 'NONE', #126841, #124286, #188103 ) ;
#113652 = EDGE_LOOP ( 'NONE', ( #222244, #113423, #237418, #151852 ) ) ;
#113653 = SPHERICAL_SURFACE ( 'NONE', #38281, 0.1000000000000000056 ) ;
#113654 = ORIENTED_EDGE ( 'NONE', *, *, #43006, .T. ) ;
#113655 = ORIENTED_EDGE ( 'NONE', *, *, #194510, .T. ) ;
#113656 = AXIS2_PLACEMENT_3D ( 'NONE', #164479, #136199, #76249 ) ;
#113657 = ORIENTED_EDGE ( 'NONE', *, *, #36107, .F. ) ;
#113658 = CARTESIAN_POINT ( 'NONE',  ( 21.14999999999999858, 10.71339244341104013, -45.75000000000000711 ) ) ;
#113659 = CARTESIAN_POINT ( 'NONE',  ( -20.85000000000000497, 64.25000000001220712, -143.4422547304831710 ) ) ;
#113660 = VECTOR ( 'NONE', #230055, 1000.000000000000000 ) ;
#113661 = AXIS2_PLACEMENT_3D ( 'NONE', #84752, #125213, #67795 ) ;
#113662 = EDGE_LOOP ( 'NONE', ( #177227, #207024, #26623, #73816 ) ) ;
#113663 = ORIENTED_EDGE ( 'NONE', *, *, #8531, .F. ) ;
#113664 = DIRECTION ( 'NONE',  ( 0.000000000000000000, 1.000000000000000000, 0.000000000000000000 ) ) ;
#113665 = EDGE_CURVE ( 'NONE', #50465, #200909, #4793, .T. ) ;
#113666 = AXIS2_PLACEMENT_3D ( 'NONE', #109091, #188637, #83078 ) ;
#113668 = ORIENTED_EDGE ( 'NONE', *, *, #7637, .T. ) ;
#113667 = ORIENTED_EDGE ( 'NONE', *, *, #226879, .T. ) ;
#113669 = ORIENTED_EDGE ( 'NONE', *, *, #119500, .F. ) ;
#113670 = DIRECTION ( 'NONE',  ( 0.000000000000000000, 0.000000000000000000, 1.000000000000000000 ) ) ;
#113671 = ORIENTED_EDGE ( 'NONE', *, *, #136570, .F. ) ;
#113672 = ORIENTED_EDGE ( 'NONE', *, *, #139362, .F. ) ;
#113673 = CARTESIAN_POINT ( 'NONE',  ( -18.50000000000000000, 52.27009174976920747, -232.4217594817395138 ) ) ;
#113674 = ORIENTED_EDGE ( 'NONE', *, *, #93260, .F. ) ;
#113675 = CARTESIAN_POINT ( 'NONE',  ( -22.59999999999999787, 11.74956712350054744, -133.8991416309013118 ) ) ;
#113676 = AXIS2_PLACEMENT_3D ( 'NONE', #30721, #33298, #112800 ) ;
#113677 = DIRECTION ( 'NONE',  ( -0.000000000000000000, -0.000000000000000000, -1.000000000000000000 ) ) ;
#113678 = ADVANCED_FACE ( 'NONE', ( #165464 ), #102881, .T. ) ;
#113680 = ORIENTED_EDGE ( 'NONE', *, *, #142822, .T. ) ;
#113679 = AXIS2_PLACEMENT_3D ( 'NONE', #256779, #242397, #226686 ) ;
#113681 = EDGE_CURVE ( 'NONE', #90989, #71337, #123764, .T. ) ;
#113682 = ORIENTED_EDGE ( 'NONE', *, *, #160854, .T. ) ;
#113683 = CIRCLE ( 'NONE', #234476, 0.09999999999999939493 ) ;
#113684 = CARTESIAN_POINT ( 'NONE',  ( 18.59999999999999076, 77.85161776048073534, -91.41991776492061206 ) ) ;
#113685 = VERTEX_POINT ( 'NONE', #239863 ) ;
#113686 = B_SPLINE_CURVE_WITH_KNOTS ( 'NONE', 3,
 ( #142922, #21729, #42557, #162535, #62137, #197783, #102502, #81653 ),
 .UNSPECIFIED., .F., .F.,
 ( 4, 2, 2, 4 ),
 ( 0.000000000000000000, 6.534141206313191720E-05, 0.0001306828241262638344, 0.0002613656482524775245 ),
 .UNSPECIFIED. ) ;
#113687 = VECTOR ( 'NONE', #27417, 1000.000000000000114 ) ;
#113688 = TOROIDAL_SURFACE ( 'NONE', #76083, 11.89999999999999858, 0.1000000000000000056 ) ;
#113689 = AXIS2_PLACEMENT_3D ( 'NONE', #200850, #40531, #120057 ) ;
#113690 = ADVANCED_FACE ( 'NONE', ( #24684 ), #61215, .T. ) ;
#113691 = CIRCLE ( 'NONE', #176259, 0.09999999999998898659 ) ;
#113692 = VERTEX_POINT ( 'NONE', #144583 ) ;
#113693 = ORIENTED_EDGE ( 'NONE', *, *, #103798, .T. ) ;
#113694 = CARTESIAN_POINT ( 'NONE',  ( -20.64999999999999858, 63.56320957583155717, -222.0641766000055668 ) ) ;
#113697 = EDGE_CURVE ( 'NONE', #32374, #138502, #38171, .T. ) ;
#113696 = ORIENTED_EDGE ( 'NONE', *, *, #145479, .F. ) ;
#113695 = CARTESIAN_POINT ( 'NONE',  ( 18.58703555225036297, 85.40633674080073945, -162.8981628432770208 ) ) ;
#113698 = PLANE ( 'NONE',  #89300 ) ;
#113699 = ADVANCED_FACE ( 'NONE', ( #181182 ), #82023, .T. ) ;
#113700 = CARTESIAN_POINT ( 'NONE',  ( -20.90000000000000213, -1.800000000000000044, -11.61130914238355771 ) ) ;
#113701 = CARTESIAN_POINT ( 'NONE',  ( 18.56308993302910437, 33.83802916238668246, -236.2638560227619564 ) ) ;
#113702 = LINE ( 'NONE', #214089, #94580 ) ;
#113703 = DIRECTION ( 'NONE',  ( 0.000000000000000000, 0.8814952561688476074, -0.4721928772777262417 ) ) ;
#113704 = DIRECTION ( 'NONE',  ( 1.000000000000000000, 0.000000000000000000, 0.000000000000000000 ) ) ;
#113705 = CYLINDRICAL_SURFACE ( 'NONE', #74179, 0.09999999999998898659 ) ;
#113706 = DIRECTION ( 'NONE',  ( 1.000000000000000000, 0.000000000000000000, 0.000000000000000000 ) ) ;
#113708 = EDGE_CURVE ( 'NONE', #38706, #221411, #125625, .T. ) ;
#113707 = CARTESIAN_POINT ( 'NONE',  ( 22.47809213839789066, 75.96246293238370129, -148.1730808193121049 ) ) ;
#113709 = CARTESIAN_POINT ( 'NONE',  ( 18.49999999999999289, 33.78138312054863945, -236.4287629273227651 ) ) ;
#113710 = AXIS2_PLACEMENT_3D ( 'NONE', #192845, #255313, #91162 ) ;
#113712 = ORIENTED_EDGE ( 'NONE', *, *, #174940, .T. ) ;
#113711 = CIRCLE ( 'NONE', #5348, 0.9750000000000036415 ) ;
#113713 = TOROIDAL_SURFACE ( 'NONE', #184434, 4.150000000000000355, 0.1000000000000000056 ) ;
#113715 = ORIENTED_EDGE ( 'NONE', *, *, #180393, .F. ) ;
#113714 = VERTEX_POINT ( 'NONE', #131455 ) ;
#113716 = ORIENTED_EDGE ( 'NONE', *, *, #250446, .F. ) ;
#113718 = EDGE_CURVE ( 'NONE', #177733, #186334, #10240, .T. ) ;
#113717 = CYLINDRICAL_SURFACE ( 'NONE', #244625, 0.1000000000000055844 ) ;
#113719 = CARTESIAN_POINT ( 'NONE',  ( 18.39999999999998082, 11.47316190337362585, -143.2500000000000284 ) ) ;
#113721 = CARTESIAN_POINT ( 'NONE',  ( 18.69999999999999929, -8.175168544775697654, 10.42878401658402510 ) ) ;
#113720 = DIRECTION ( 'NONE',  ( -1.000000000000000000, -0.000000000000000000, -0.000000000000000000 ) ) ;
#113722 = EDGE_LOOP ( 'NONE', ( #94645, #148951, #187065, #56525 ) ) ;
#113723 = VERTEX_POINT ( 'NONE', #27263 ) ;
#113724 = SURFACE_STYLE_FILL_AREA ( #190726 ) ;
#113725 = LINE ( 'NONE', #38067, #8440 ) ;
#113726 = DIRECTION ( 'NONE',  ( 0.000000000000000000, -1.000000000000000000, -6.982962677686265922E-15 ) ) ;
#113727 = DIRECTION ( 'NONE',  ( 0.000000000000000000, 0.000000000000000000, -1.000000000000000000 ) ) ;
#113728 = ORIENTED_EDGE ( 'NONE', *, *, #177607, .T. ) ;
#113729 = ORIENTED_EDGE ( 'NONE', *, *, #58529, .F. ) ;
#113730 = CARTESIAN_POINT ( 'NONE',  ( 20.94999999999999574, -1.261786168553869603, -75.08649896354552311 ) ) ;
#113731 = DIRECTION ( 'NONE',  ( 1.000000000000000000, 2.952720810173289112E-16, -0.000000000000000000 ) ) ;
#113732 = AXIS2_PLACEMENT_3D ( 'NONE', #3186, #181852, #26649 ) ;
#113733 = ORIENTED_EDGE ( 'NONE', *, *, #161606, .T. ) ;
#113734 = LINE ( 'NONE', #156748, #8140 ) ;
#113736 = VERTEX_POINT ( 'NONE', #209714 ) ;
#113735 = DIRECTION ( 'NONE',  ( 0.000000000000000000, 0.2605042016806672911, -0.9654727137038716656 ) ) ;
#113737 = CARTESIAN_POINT ( 'NONE',  ( -18.59999999999999787, 67.23127455305841238, -235.8551265064783991 ) ) ;
#113738 = VERTEX_POINT ( 'NONE', #91048 ) ;
#113739 = CARTESIAN_POINT ( 'NONE',  ( 12.48201962039795809, 66.62334006147830223, -85.39491493630707453 ) ) ;
#113740 = CARTESIAN_POINT ( 'NONE',  ( 18.49999999999999645, 7.128833340093095217, -233.7327013124392749 ) ) ;
#113741 = DIRECTION ( 'NONE',  ( 2.259780016855445309E-14, -0.9875055080513764905, 0.1575844902526679359 ) ) ;
#113742 = DIRECTION ( 'NONE',  ( 1.000000000000000000, -0.000000000000000000, -0.000000000000000000 ) ) ;
#113743 = CARTESIAN_POINT ( 'NONE',  ( -16.90128866880176162, 9.953795777214113016, -121.3626761833886718 ) ) ;
#113744 = DIRECTION ( 'NONE',  ( 0.000000000000000000, -1.000000000000000000, 0.000000000000000000 ) ) ;
#113745 = CARTESIAN_POINT ( 'NONE',  ( -21.07928932188134041, 69.67148334361884565, -136.6220026301787414 ) ) ;
#113746 = ORIENTED_EDGE ( 'NONE', *, *, #57913, .T. ) ;
#113747 = EDGE_CURVE ( 'NONE', #7281, #142411, #196540, .T. ) ;
#113748 = CIRCLE ( 'NONE', #238844, 0.09999999999999939493 ) ;
#113749 = ORIENTED_EDGE ( 'NONE', *, *, #72571, .F. ) ;
#113750 = DIRECTION ( 'NONE',  ( 0.000000000000000000, 0.4999999999999689138, -0.8660254037844565822 ) ) ;
#113751 = CARTESIAN_POINT ( 'NONE',  ( -21.05000000000000071, -1.162701749926853712, -175.4999999999999716 ) ) ;
#113752 = ORIENTED_EDGE ( 'NONE', *, *, #254355, .T. ) ;
#113753 = EDGE_CURVE ( 'NONE', #207794, #170116, #163250, .T. ) ;
#113754 = CARTESIAN_POINT ( 'NONE',  ( -20.64999999999999858, 76.00000000001267608, -203.5231074845243597 ) ) ;
#113755 = ORIENTED_EDGE ( 'NONE', *, *, #86892, .T. ) ;
#113756 = ADVANCED_FACE ( 'NONE', ( #106742 ), #7673, .F. ) ;
#113757 =( NAMED_UNIT ( * ) SI_UNIT ( $, .STERADIAN. ) SOLID_ANGLE_UNIT ( ) );
#113758 = EDGE_CURVE ( 'NONE', #218074, #231169, #71667, .T. ) ;
#113759 = AXIS2_PLACEMENT_3D ( 'NONE', #18929, #239277, #157195 ) ;
#113760 = EDGE_LOOP ( 'NONE', ( #208491, #61394, #170968, #202979 ) ) ;
#113761 = CARTESIAN_POINT ( 'NONE',  ( 21.13435531349814767, 76.00000000001199396, -109.5168285481162940 ) ) ;
#113762 = ORIENTED_EDGE ( 'NONE', *, *, #102157, .F. ) ;
#113763 = AXIS2_PLACEMENT_3D ( 'NONE', #246035, #9986, #167806 ) ;
#113764 = CARTESIAN_POINT ( 'NONE',  ( 18.54116936837188234, -7.746869717850485948, -209.9009554631552987 ) ) ;
#113765 = DIRECTION ( 'NONE',  ( 0.000000000000000000, 7.026728003956695223E-15, -1.000000000000000000 ) ) ;
#113766 = CARTESIAN_POINT ( 'NONE',  ( 21.00000000000000000, -11.65000000000000036, 0.000000000000000000 ) ) ;
#113767 = AXIS2_PLACEMENT_3D ( 'NONE', #213694, #31258, #110741 ) ;
#113768 = DIRECTION ( 'NONE',  ( 1.000000000000000000, -0.000000000000000000, -0.000000000000000000 ) ) ;
#113769 = CARTESIAN_POINT ( 'NONE',  ( -18.50000000000000711, 64.25000000001233502, -163.0083017138704236 ) ) ;
#113771 = ORIENTED_EDGE ( 'NONE', *, *, #32502, .F. ) ;
#113770 = CARTESIAN_POINT ( 'NONE',  ( 18.49999999999999645, 78.48087866980282001, -232.8271061603568910 ) ) ;
#113773 = FACE_OUTER_BOUND ( 'NONE', #29749, .T. ) ;
#113772 = CARTESIAN_POINT ( 'NONE',  ( 20.09999999999999787, 9.750000000011137757, -46.15000000000000568 ) ) ;
#113774 = EDGE_CURVE ( 'NONE', #52520, #257124, #170641, .T. ) ;
#113775 = DIRECTION ( 'NONE',  ( -1.000000000000000000, -0.000000000000000000, -0.000000000000000000 ) ) ;
#113776 = DIRECTION ( 'NONE',  ( -1.000000000000000000, 0.000000000000000000, 0.000000000000000000 ) ) ;
#113777 = LINE ( 'NONE', #91657, #6511 ) ;
#113779 = EDGE_CURVE ( 'NONE', #105678, #212150, #92485, .T. ) ;
#113778 = DIRECTION ( 'NONE',  ( 0.000000000000000000, 6.982962677686267499E-15, -1.000000000000000000 ) ) ;
#113780 = ORIENTED_EDGE ( 'NONE', *, *, #42330, .T. ) ;
#113781 = VECTOR ( 'NONE', #11745, 1000.000000000000000 ) ;
#113783 = CARTESIAN_POINT ( 'NONE',  ( -21.05000000000000071, 76.00000000001242029, -166.0231074845243597 ) ) ;
#113782 = AXIS2_PLACEMENT_3D ( 'NONE', #138637, #235212, #116548 ) ;
#113784 = PRODUCT_RELATED_PRODUCT_CATEGORY ( 'part', '', ( #228439 ) ) ;
#113785 = CIRCLE ( 'NONE', #17917, 0.1000000000000000472 ) ;
#113786 = ORIENTED_EDGE ( 'NONE', *, *, #241781, .T. ) ;
#113787 = DIRECTION ( 'NONE',  ( 0.000000000000000000, -0.000000000000000000, 1.000000000000000000 ) ) ;
#113788 = ORIENTED_EDGE ( 'NONE', *, *, #151834, .F. ) ;
#113789 = DIRECTION ( 'NONE',  ( -3.265361837132813093E-16, 1.000000000000000000, 0.000000000000000000 ) ) ;
#113790 = ADVANCED_FACE ( 'NONE', ( #230568 ), #46768, .T. ) ;
#113791 = VECTOR ( 'NONE', #236874, 1000.000000000000114 ) ;
#113792 = DIRECTION ( 'NONE',  ( 0.000000000000000000, -1.000000000000000000, -6.982962677686265922E-15 ) ) ;
#113793 = DIRECTION ( 'NONE',  ( 0.000000000000000000, 1.000000000000000000, 0.000000000000000000 ) ) ;
#113794 = EDGE_CURVE ( 'NONE', #10283, #188501, #213279, .T. ) ;
#113795 = EDGE_LOOP ( 'NONE', ( #20685, #77893, #16276, #130508 ) ) ;
#113796 = EDGE_CURVE ( 'NONE', #115375, #255725, #100821, .T. ) ;
#113797 = VERTEX_POINT ( 'NONE', #169344 ) ;
#113798 = AXIS2_PLACEMENT_3D ( 'NONE', #185450, #179365, #65488 ) ;
#113799 = VECTOR ( 'NONE', #111954, 1000.000000000000000 ) ;
#113800 = VECTOR ( 'NONE', #44861, 1000.000000000000000 ) ;
#113801 = DIRECTION ( 'NONE',  ( -1.000000000000000000, -0.000000000000000000, -0.000000000000000000 ) ) ;
#113802 = CARTESIAN_POINT ( 'NONE',  ( -21.64999999999999858, 30.25354784785470486, -234.7188954791831748 ) ) ;
#113803 = DIRECTION ( 'NONE',  ( 0.000000000000000000, -0.2128009952263605342, 0.9770955615653315052 ) ) ;
#113804 = CARTESIAN_POINT ( 'NONE',  ( -18.52139480978222963, -9.481358845055737561, -141.0245565671190491 ) ) ;
#113805 = EDGE_CURVE ( 'NONE', #61925, #227290, #84060, .T. ) ;
#113807 = DIRECTION ( 'NONE',  ( 1.000000000000000000, 0.000000000000000000, 0.000000000000000000 ) ) ;
#113806 = DIRECTION ( 'NONE',  ( 0.000000000000000000, -0.9999631594459057471, 0.008583690987121077309 ) ) ;
#113808 = DIRECTION ( 'NONE',  ( -1.000000000000000000, -0.000000000000000000, -0.000000000000000000 ) ) ;
#113809 = FACE_OUTER_BOUND ( 'NONE', #235059, .T. ) ;
#113810 = CARTESIAN_POINT ( 'NONE',  ( 21.05000000000000071, 30.78880722230112710, -252.2904790204486574 ) ) ;
#113811 = VERTEX_POINT ( 'NONE', #67628 ) ;
#113812 = FACE_OUTER_BOUND ( 'NONE', #139919, .T. ) ;
#113814 = ORIENTED_EDGE ( 'NONE', *, *, #175517, .F. ) ;
#113813 = DIRECTION ( 'NONE',  ( 0.000000000000000000, 0.9770955615653313941, 0.2128009952263603677 ) ) ;
#113815 = DIRECTION ( 'NONE',  ( 1.000000000000000000, 0.000000000000000000, -0.000000000000000000 ) ) ;
#113817 = DIRECTION ( 'NONE',  ( 0.000000000000000000, 0.000000000000000000, -1.000000000000000000 ) ) ;
#113816 = DIRECTION ( 'NONE',  ( 1.000000000000000000, -1.207181226542539700E-16, 2.694675058168174199E-16 ) ) ;
#113819 = ORIENTED_EDGE ( 'NONE', *, *, #129936, .T. ) ;
#113818 = CARTESIAN_POINT ( 'NONE',  ( 23.25000000000000000, 85.00000000001149658, -45.91707660717670336 ) ) ;
#113820 = DIRECTION ( 'NONE',  ( 0.000000000000000000, -7.147358527629766941E-15, 1.000000000000000000 ) ) ;
#113821 = CARTESIAN_POINT ( 'NONE',  ( -20.64999999999999858, 1.115600667400684642E-11, -202.8999999999999773 ) ) ;
#113822 = DIRECTION ( 'NONE',  ( 2.659396599871503635E-15, -0.6132151058540604716, 0.7899159663865477077 ) ) ;
#113823 = CARTESIAN_POINT ( 'NONE',  ( 23.14999999999999858, 1.115600667400684642E-11, -134.0000000000000284 ) ) ;
#113824 = LINE ( 'NONE', #53861, #190854 ) ;
#113825 = EDGE_LOOP ( 'NONE', ( #2104, #56136, #545, #38960 ) ) ;
#113826 = CARTESIAN_POINT ( 'NONE',  ( 18.46082813848008897, -7.756037395792517053, -209.9396195450558480 ) ) ;
#113827 = VERTEX_POINT ( 'NONE', #147162 ) ;
#113828 = EDGE_CURVE ( 'NONE', #29621, #169297, #204912, .T. ) ;
#113829 = TOROIDAL_SURFACE ( 'NONE', #105414, 0.2000000000000000111, 0.1000000000000000056 ) ;
#113830 = TOROIDAL_SURFACE ( 'NONE', #80671, 0.6000000000000015321, 0.1000000000000000056 ) ;
#113831 = CARTESIAN_POINT ( 'NONE',  ( -17.01473183483379970, 9.950000000011140600, -121.2500000000000284 ) ) ;
#113832 = ORIENTED_EDGE ( 'NONE', *, *, #248219, .F. ) ;
#113833 = FACE_OUTER_BOUND ( 'NONE', #112669, .T. ) ;
#113834 = AXIS2_PLACEMENT_3D ( 'NONE', #14469, #36611, #74455 ) ;
#113835 = EDGE_LOOP ( 'NONE', ( #113434, #25333, #48869, #81830 ) ) ;
#113836 = CARTESIAN_POINT ( 'NONE',  ( -20.94999999999999929, 74.14897176987174987, -191.8691942151018850 ) ) ;
#113837 = CARTESIAN_POINT ( 'NONE',  ( -23.15000000000000213, 78.00142589229885459, -228.9845759368473637 ) ) ;
#113838 = AXIS2_PLACEMENT_3D ( 'NONE', #100786, #18728, #120437 ) ;
#113839 = ADVANCED_FACE ( 'NONE', ( #227994 ), #209019, .F. ) ;
#113840 = CIRCLE ( 'NONE', #205391, 11.80000000000000426 ) ;
#113841 = CARTESIAN_POINT ( 'NONE',  ( 20.73486653747088582, 68.75000000001203659, -123.8731074845243540 ) ) ;
#113842 = ORIENTED_EDGE ( 'NONE', *, *, #175926, .F. ) ;
#113843 = AXIS2_PLACEMENT_3D ( 'NONE', #126310, #125047, #27258 ) ;
#113844 = EDGE_CURVE ( 'NONE', #13286, #188914, #109306, .T. ) ;
#113845 = CARTESIAN_POINT ( 'NONE',  ( 20.94999999999999929, 76.00000000001244871, -170.0231074845243597 ) ) ;
#113847 = AXIS2_PLACEMENT_3D ( 'NONE', #102072, #202488, #117806 ) ;
#113846 = DIRECTION ( 'NONE',  ( 0.000000000000000000, 0.3427706569149635007, -0.9394191166662961834 ) ) ;
#113848 = DIRECTION ( 'NONE',  ( 0.000000000000000000, 0.000000000000000000, -1.000000000000000000 ) ) ;
#113849 = CIRCLE ( 'NONE', #197035, 0.09999999999998898659 ) ;
#113850 = CIRCLE ( 'NONE', #213813, 0.1000000000000028644 ) ;
#113851 = CARTESIAN_POINT ( 'NONE',  ( 21.30740335185486245, 6.385427988779872166, -199.5080681828139859 ) ) ;
#113852 = DIRECTION ( 'NONE',  ( -4.391705002472924160E-16, -0.4088369013363268301, 0.9126074666063775931 ) ) ;
#113853 = ORIENTED_EDGE ( 'NONE', *, *, #4664, .T. ) ;
#113854 = DIRECTION ( 'NONE',  ( -0.000000000000000000, 0.000000000000000000, -1.000000000000000000 ) ) ;
#113855 = VERTEX_POINT ( 'NONE', #50617 ) ;
#113857 = ORIENTED_EDGE ( 'NONE', *, *, #108959, .T. ) ;
#113856 = LINE ( 'NONE', #133426, #118993 ) ;
#113858 = VECTOR ( 'NONE', #29953, 1000.000000000000000 ) ;
#113859 = EDGE_CURVE ( 'NONE', #67371, #98189, #89750, .T. ) ;
#113860 = ORIENTED_EDGE ( 'NONE', *, *, #10581, .F. ) ;
#113861 = CARTESIAN_POINT ( 'NONE',  ( 22.00356870068402770, -5.670589261373817377E-12, -59.74575763823897034 ) ) ;
#113862 = ADVANCED_FACE ( 'NONE', ( #19210 ), #236979, .F. ) ;
#113863 = CARTESIAN_POINT ( 'NONE',  ( -21.65000000000000213, 7.750000000011155521, -112.8500000000000369 ) ) ;
#113864 = DIRECTION ( 'NONE',  ( -1.000000000000000000, 0.000000000000000000, -0.000000000000000000 ) ) ;
#113865 = CARTESIAN_POINT ( 'NONE',  ( -22.50047199487877947, 75.95509394809148773, -81.27315490344393822 ) ) ;
#113866 = ORIENTED_EDGE ( 'NONE', *, *, #19944, .T. ) ;
#113867 = FACE_BOUND ( 'NONE', #93059, .T. ) ;
#113869 = DIRECTION ( 'NONE',  ( 0.000000000000000000, 1.000000000000000000, -5.551115123125777653E-14 ) ) ;
#113868 = AXIS2_PLACEMENT_3D ( 'NONE', #77201, #254534, #116354 ) ;
#113870 = ORIENTED_EDGE ( 'NONE', *, *, #94129, .T. ) ;
#113871 = AXIS2_PLACEMENT_3D ( 'NONE', #85635, #187359, #47809 ) ;
#113873 = ORIENTED_EDGE ( 'NONE', *, *, #125494, .F. ) ;
#113872 = CARTESIAN_POINT ( 'NONE',  ( -20.94999999999999929, 11.65000000001115232, -60.21613433702190576 ) ) ;
#113874 = DIRECTION ( 'NONE',  ( -1.000000000000000000, 0.000000000000000000, -0.000000000000000000 ) ) ;
#113875 = DIRECTION ( 'NONE',  ( 2.952720810173289112E-16, -1.000000000000000000, 0.000000000000000000 ) ) ;
#113876 = VECTOR ( 'NONE', #96619, 1000.000000000000000 ) ;
#113877 = DIRECTION ( 'NONE',  ( 0.000000000000000000, -4.336808689942494997E-15, -1.000000000000000000 ) ) ;
#113878 = VERTEX_POINT ( 'NONE', #96159 ) ;
#113879 = EDGE_CURVE ( 'NONE', #97885, #27566, #184077, .T. ) ;
#113880 = VECTOR ( 'NONE', #40239, 1000.000000000000000 ) ;
#113881 = EDGE_LOOP ( 'NONE', ( #124603, #9157, #191703 ) ) ;
#113882 = CIRCLE ( 'NONE', #59680, 7.800000000000001599 ) ;
#113883 = AXIS2_PLACEMENT_3D ( 'NONE', #190939, #72262, #230040 ) ;
#113884 = CYLINDRICAL_SURFACE ( 'NONE', #54617, 0.1000000000000214190 ) ;
#113885 = ORIENTED_EDGE ( 'NONE', *, *, #42449, .T. ) ;
#113886 = DIRECTION ( 'NONE',  ( 0.000000000000000000, -1.000000000000000000, -6.982962677686266711E-15 ) ) ;
#113887 = ADVANCED_FACE ( 'NONE', ( #235678 ), #135286, .T. ) ;
#113888 = CARTESIAN_POINT ( 'NONE',  ( -22.39999999999999858, -2.479040261794000610, -189.6172560698084624 ) ) ;
#113889 = CARTESIAN_POINT ( 'NONE',  ( -18.59999999999999787, -1.835859311432481045, -212.5044391687984842 ) ) ;
#113890 = EDGE_CURVE ( 'NONE', #250378, #40334, #36233, .T. ) ;
#113891 = ADVANCED_FACE ( 'NONE', ( #217390 ), #115743, .F. ) ;
#113892 = CIRCLE ( 'NONE', #105481, 0.1000000000000054040 ) ;
#113893 = CIRCLE ( 'NONE', #134719, 0.09999999999999031886 ) ;
#113894 = STYLED_ITEM ( 'NONE', ( #147944 ), #25248 ) ;
#113895 = CIRCLE ( 'NONE', #84625, 11.75000000000000000 ) ;
#113896 = ORIENTED_EDGE ( 'NONE', *, *, #150988, .T. ) ;
#113897 = CARTESIAN_POINT ( 'NONE',  ( -23.25000000000000000, 64.25000000001277556, -215.2731074845244450 ) ) ;
#113898 = EDGE_LOOP ( 'NONE', ( #114412, #244136, #19706, #49937 ) ) ;
#113899 = DIRECTION ( 'NONE',  ( -1.000000000000000000, 0.000000000000000000, 0.000000000000000000 ) ) ;
#113900 = FACE_OUTER_BOUND ( 'NONE', #40905, .T. ) ;
#113902 = VERTEX_POINT ( 'NONE', #16659 ) ;
#113901 = CARTESIAN_POINT ( 'NONE',  ( -23.15000000000000213, 1.115600667400684642E-11, -122.2000000000000313 ) ) ;
#113904 = EDGE_CURVE ( 'NONE', #218857, #218618, #50771, .T. ) ;
#113903 = CYLINDRICAL_SURFACE ( 'NONE', #90807, 0.09999999999998898659 ) ;
#113905 = DIRECTION ( 'NONE',  ( 0.000000000000000000, 0.000000000000000000, -1.000000000000000000 ) ) ;
#113906 = CARTESIAN_POINT ( 'NONE',  ( 18.59999999999999076, 11.75000000001115907, -158.8500000000000227 ) ) ;
#113907 = CARTESIAN_POINT ( 'NONE',  ( -16.89268316805466341, 22.97380970494227626, -230.9308293615217451 ) ) ;
#113908 = EDGE_CURVE ( 'NONE', #246634, #6219, #125799, .T. ) ;
#113909 = DIRECTION ( 'NONE',  ( 1.000000000000000000, 0.000000000000000000, 0.000000000000000000 ) ) ;
#113910 = CARTESIAN_POINT ( 'NONE',  ( 21.05000000000000071, 87.48912529308798014, -100.1231074845242262 ) ) ;
#113912 = ORIENTED_EDGE ( 'NONE', *, *, #148157, .F. ) ;
#113911 = CARTESIAN_POINT ( 'NONE',  ( 21.05000000000000071, 76.00000000001165290, -69.52310748452431710 ) ) ;
#113913 = CARTESIAN_POINT ( 'NONE',  ( 20.94999999999999929, 1.115600667400684642E-11, -167.5000000000000284 ) ) ;
#113914 = VECTOR ( 'NONE', #44611, 1000.000000000000000 ) ;
#113915 = CARTESIAN_POINT ( 'NONE',  ( -21.44999999999999929, 68.65000000001157332, -57.17310748452437252 ) ) ;
#113916 = CARTESIAN_POINT ( 'NONE',  ( 23.15000000000000213, -11.64999999998883595, -164.5000000000000000 ) ) ;
#113917 = ORIENTED_EDGE ( 'NONE', *, *, #238606, .F. ) ;
#113918 = DIRECTION ( 'NONE',  ( 2.952720810173289112E-16, 1.000000000000000000, 6.938893903907222067E-15 ) ) ;
#113919 = DIRECTION ( 'NONE',  ( -0.000000000000000000, 0.8814952561688430555, -0.4721928772777346239 ) ) ;
#113920 = CARTESIAN_POINT ( 'NONE',  ( -11.59999999999994458, 67.65000000001118963, -16.98168612828748536 ) ) ;
#113921 = ORIENTED_EDGE ( 'NONE', *, *, #199456, .F. ) ;
#113922 = AXIS2_PLACEMENT_3D ( 'NONE', #25117, #142461, #26393 ) ;
#113924 = EDGE_CURVE ( 'NONE', #228499, #168221, #179998, .T. ) ;
#113923 = DIRECTION ( 'NONE',  ( 1.000000000000000000, 0.000000000000000000, 0.000000000000000000 ) ) ;
#113925 = CIRCLE ( 'NONE', #230654, 0.1000000000000028644 ) ;
#113926 = VECTOR ( 'NONE', #5930, 1000.000000000000000 ) ;
#113927 = CARTESIAN_POINT ( 'NONE',  ( -16.93440969289731513, 9.995185175825110235, -79.59123418501083336 ) ) ;
#113928 = ORIENTED_EDGE ( 'NONE', *, *, #36772, .F. ) ;
#113929 = CARTESIAN_POINT ( 'NONE',  ( -17.27223548803035058, 65.65460260866045417, -47.38950130531501514 ) ) ;
#113930 = ORIENTED_EDGE ( 'NONE', *, *, #37667, .F. ) ;
#113932 = ORIENTED_EDGE ( 'NONE', *, *, #60221, .T. ) ;
#113931 = CARTESIAN_POINT ( 'NONE',  ( -20.54999999999999716, 1.940186915899004161, -54.17088078894667547 ) ) ;
#113933 = DIRECTION ( 'NONE',  ( -1.186688945009010077E-16, -1.000000000000000000, -6.982962677686266711E-15 ) ) ;
#113934 = ORIENTED_EDGE ( 'NONE', *, *, #117126, .T. ) ;
#113935 = CARTESIAN_POINT ( 'NONE',  ( 21.05000000000000071, 1.115600667400684642E-11, -100.5000000000000426 ) ) ;
#113936 = ORIENTED_EDGE ( 'NONE', *, *, #112928, .F. ) ;
#113938 = ORIENTED_EDGE ( 'NONE', *, *, #134187, .T. ) ;
#113937 = ORIENTED_EDGE ( 'NONE', *, *, #170241, .T. ) ;
#113940 = DIRECTION ( 'NONE',  ( -3.265361837132813093E-16, 1.000000000000000000, -0.000000000000000000 ) ) ;
#113939 = CIRCLE ( 'NONE', #80598, 0.09999999999999063804 ) ;
#113942 = EDGE_LOOP ( 'NONE', ( #255227, #52650 ) ) ;
#113941 = CARTESIAN_POINT ( 'NONE',  ( 15.70340296795548163, 9.355888454513701546, -49.78864289677800770 ) ) ;
#113943 = ADVANCED_FACE ( 'NONE', ( #53202 ), #234393, .T. ) ;
#113944 = CARTESIAN_POINT ( 'NONE',  ( 20.86777300164945004, 65.66799936921512426, -63.92993998886009877 ) ) ;
#113945 = VERTEX_POINT ( 'NONE', #255192 ) ;
#113946 = AXIS2_PLACEMENT_3D ( 'NONE', #15973, #36824, #56327 ) ;
#113947 = TOROIDAL_SURFACE ( 'NONE', #188981, 12.77500000000000036, 0.1000000000000000056 ) ;
#113948 = ORIENTED_EDGE ( 'NONE', *, *, #115411, .F. ) ;
#113949 = DIRECTION ( 'NONE',  ( 0.000000000000000000, -0.9770955615653315052, -0.2128009952263603954 ) ) ;
#113950 = CARTESIAN_POINT ( 'NONE',  ( 20.94999999999999929, 87.65000000001141700, -36.02310748452423894 ) ) ;
#113951 = DIRECTION ( 'NONE',  ( -1.000000000000000000, -0.000000000000000000, -0.000000000000000000 ) ) ;
#113952 = ORIENTED_EDGE ( 'NONE', *, *, #80269, .T. ) ;
#113953 = DIRECTION ( 'NONE',  ( 1.000000000000000000, 0.000000000000000000, 0.000000000000000000 ) ) ;
#113954 = CARTESIAN_POINT ( 'NONE',  ( -18.47079683080345092, -9.471664105233751130, -74.10886054099226783 ) ) ;
#113955 = CARTESIAN_POINT ( 'NONE',  ( -23.15000000000000213, 2.000000000011154189, -180.7246219227620543 ) ) ;
#113956 = AXIS2_PLACEMENT_3D ( 'NONE', #219874, #201592, #242005 ) ;
#113957 = ORIENTED_EDGE ( 'NONE', *, *, #28808, .T. ) ;
#113958 = CIRCLE ( 'NONE', #197346, 0.5999999999999992006 ) ;
#113959 = CARTESIAN_POINT ( 'NONE',  ( -23.25000000000000000, 86.27712145182582049, -209.5223386573213702 ) ) ;
#113960 = CARTESIAN_POINT ( 'NONE',  ( -18.58744394320964233, 38.15605368352883175, -261.2055860874503992 ) ) ;
#113961 = CARTESIAN_POINT ( 'NONE',  ( 18.39999999999999858, 85.50000000001166711, -62.60844914155458696 ) ) ;
#113962 = AXIS2_PLACEMENT_3D ( 'NONE', #203674, #163277, #43325 ) ;
#113963 = ORIENTED_EDGE ( 'NONE', *, *, #115090, .F. ) ;
#113964 = DIRECTION ( 'NONE',  ( 1.000000000000000000, 0.000000000000000000, 0.000000000000000000 ) ) ;
#113965 = ORIENTED_EDGE ( 'NONE', *, *, #33865, .T. ) ;
#113966 = ORIENTED_EDGE ( 'NONE', *, *, #188346, .F. ) ;
#113967 = CARTESIAN_POINT ( 'NONE',  ( -12.47155713865591231, 25.54333932933834106, -232.9607505220590156 ) ) ;
#113968 = VERTEX_POINT ( 'NONE', #233153 ) ;
#113969 = VERTEX_POINT ( 'NONE', #231863 ) ;
#113970 = CARTESIAN_POINT ( 'NONE',  ( -22.49436431346200038, 11.36887822570846041, -198.4555077020579290 ) ) ;
#113971 = CARTESIAN_POINT ( 'NONE',  ( -20.94999999999994600, 87.75000000001119815, -4.523107484524794053 ) ) ;
#113972 = EDGE_LOOP ( 'NONE', ( #135052, #119710, #58645 ) ) ;
#113973 = VERTEX_POINT ( 'NONE', #195310 ) ;
#113974 = CARTESIAN_POINT ( 'NONE',  ( 22.50000000000000000, 1.115600667400684642E-11, -100.5000000000000284 ) ) ;
#113975 = CIRCLE ( 'NONE', #30622, 0.09999999999998898659 ) ;
#113976 = AXIS2_PLACEMENT_3D ( 'NONE', #926, #123482, #60929 ) ;
#113977 = CARTESIAN_POINT ( 'NONE',  ( 18.54999999999999716, 8.750000000011182166, -121.3500000000000369 ) ) ;
#113978 = CIRCLE ( 'NONE', #230532, 4.049999999999998934 ) ;
#113979 = ORIENTED_EDGE ( 'NONE', *, *, #22050, .T. ) ;
#113980 = EDGE_CURVE ( 'NONE', #59112, #168899, #252672, .T. ) ;
#113981 = ORIENTED_EDGE ( 'NONE', *, *, #166526, .F. ) ;
#113982 = B_SPLINE_CURVE_WITH_KNOTS ( 'NONE', 3,
 ( #236735, #217167, #17688, #81494, #201464, #39864, #38556, #197615, #240604, #239325, #61974, #141496, #97191, #60663, #200200, #98474, #221024, #78930, #21570, #140194, #178083, #257535, #222287, #42403, #158524, #238026 ),
 .UNSPECIFIED., .F., .F.,
 ( 4, 2, 2, 2, 2, 2, 2, 2, 2, 2, 2, 2, 4 ),
 ( 0.005476422646581357787, 0.006160811967703573935, 0.006845201288825792686, 0.007187395949386896424, 0.007529590609947999294, 0.007871785270509103899, 0.008213979931070206769, 0.008556174591631311374, 0.008898369252192415979, 0.009240563912753518849, 0.009582758573314621720, 0.01026714789443683266, 0.01095153721555904187 ),
 .UNSPECIFIED. ) ;
#113983 = CARTESIAN_POINT ( 'NONE',  ( -18.59999999999999787, 64.35000000001198828, -115.1731074845243796 ) ) ;
#113984 = EDGE_CURVE ( 'NONE', #5236, #133804, #150755, .T. ) ;
#113985 = CARTESIAN_POINT ( 'NONE',  ( -20.85000000000000142, 77.83585931145526615, -58.01866831572577610 ) ) ;
#113986 = EDGE_CURVE ( 'NONE', #235252, #51770, #134174, .T. ) ;
#113987 = CARTESIAN_POINT ( 'NONE',  ( 23.14999999999999858, 1.115600667400684642E-11, -134.0000000000000284 ) ) ;
#113989 = ORIENTED_EDGE ( 'NONE', *, *, #139811, .F. ) ;
#113988 = DIRECTION ( 'NONE',  ( -0.000000000000000000, -1.000000000000000000, -7.272083257015735086E-15 ) ) ;
#113990 = CYLINDRICAL_SURFACE ( 'NONE', #78465, 0.1000000000000142025 ) ;
#113991 = CARTESIAN_POINT ( 'NONE',  ( -22.50000000000000711, 12.58798907299599534, -223.3278890275437334 ) ) ;
#113992 = CARTESIAN_POINT ( 'NONE',  ( -22.94999999999999929, 7.900000000000000355, 1.300000000000000044 ) ) ;
#113993 = CIRCLE ( 'NONE', #213972, 0.1000000000000000472 ) ;
#113995 = CARTESIAN_POINT ( 'NONE',  ( -19.99999999999999645, 5.474129339729826960, 16.54142135623731136 ) ) ;
#113994 = CARTESIAN_POINT ( 'NONE',  ( 21.04999999999999716, 76.00000000001169553, -76.06376443622555428 ) ) ;
#113996 = LINE ( 'NONE', #51433, #161454 ) ;
#113997 = DIRECTION ( 'NONE',  ( 0.000000000000000000, 1.000000000000000000, 0.000000000000000000 ) ) ;
#113998 = EDGE_CURVE ( 'NONE', #168103, #245454, #214837, .T. ) ;
#113999 = CARTESIAN_POINT ( 'NONE',  ( -20.54999999999999716, 1.115600667400684642E-11, -100.5000000000000426 ) ) ;
#114000 = CARTESIAN_POINT ( 'NONE',  ( 22.47071067811865319, 76.00000000001213607, -136.5231074845242745 ) ) ;
#114001 = ORIENTED_EDGE ( 'NONE', *, *, #25515, .T. ) ;
#114002 = VECTOR ( 'NONE', #17020, 1000.000000000000000 ) ;
#114003 = AXIS2_PLACEMENT_3D ( 'NONE', #121132, #215061, #118555 ) ;
#114005 = EDGE_LOOP ( 'NONE', ( #210186, #5637, #230825 ) ) ;
#114004 = FACE_OUTER_BOUND ( 'NONE', #90675, .T. ) ;
#114006 = EDGE_CURVE ( 'NONE', #81280, #173016, #38342, .T. ) ;
#114007 = FACE_OUTER_BOUND ( 'NONE', #155901, .T. ) ;
#114008 = DIRECTION ( 'NONE',  ( -1.000000000000000000, 0.000000000000000000, 0.000000000000000000 ) ) ;
#114009 = EDGE_LOOP ( 'NONE', ( #247412, #216669, #215302, #79536 ) ) ;
#114010 = CIRCLE ( 'NONE', #218234, 0.1000000000000018374 ) ;
#114011 = TOROIDAL_SURFACE ( 'NONE', #84958, 11.70000000000000107, 0.1000000000000000056 ) ;
#114012 = FACE_OUTER_BOUND ( 'NONE', #161208, .T. ) ;
#114013 = TOROIDAL_SURFACE ( 'NONE', #176419, 0.4000000000000005773, 0.1000000000000000056 ) ;
#114014 = PRODUCT_DEFINITION_SHAPE ( 'NONE', 'NONE',  #132936 ) ;
#114015 = FACE_OUTER_BOUND ( 'NONE', #191491, .T. ) ;
#114016 = ORIENTED_EDGE ( 'NONE', *, *, #215165, .F. ) ;
#114017 = AXIS2_PLACEMENT_3D ( 'NONE', #152467, #250253, #96291 ) ;
#114018 = DIRECTION ( 'NONE',  ( 0.000000000000000000, 0.000000000000000000, -1.000000000000000000 ) ) ;
#114019 = DIRECTION ( 'NONE',  ( -1.000000000000000000, -0.000000000000000000, -0.000000000000000000 ) ) ;
#114020 = CARTESIAN_POINT ( 'NONE',  ( -21.05000000000000071, 1.115653327213047955E-11, -163.2000000000000171 ) ) ;
#114022 = ORIENTED_EDGE ( 'NONE', *, *, #232160, .T. ) ;
#114021 = LINE ( 'NONE', #93181, #155928 ) ;
#114023 = CARTESIAN_POINT ( 'NONE',  ( -16.87331047859651179, 44.13548170601895038, -235.2989316066074821 ) ) ;
#114024 = VECTOR ( 'NONE', #147456, 1000.000000000000000 ) ;
#114026 = ORIENTED_EDGE ( 'NONE', *, *, #230832, .T. ) ;
#114025 = LINE ( 'NONE', #247117, #110522 ) ;
#114027 = CARTESIAN_POINT ( 'NONE',  ( 20.99999999999999645, 9.750000000011137757, -54.34999999999999432 ) ) ;
#114028 = DIRECTION ( 'NONE',  ( -1.000000000000000000, -0.000000000000000000, -0.000000000000000000 ) ) ;
#114029 = CARTESIAN_POINT ( 'NONE',  ( -18.50000000000000000, 68.48451787451661232, -224.2224406095231757 ) ) ;
#114030 = CARTESIAN_POINT ( 'NONE',  ( 20.12500000000000000, 66.25000000001189449, -94.91133620241009794 ) ) ;
#114031 = CIRCLE ( 'NONE', #218089, 0.1000000000000028644 ) ;
#114032 = B_SPLINE_CURVE_WITH_KNOTS ( 'NONE', 3,
 ( #233452, #57333, #218987, #156496, #135590, #95200 ),
 .UNSPECIFIED., .F., .F.,
 ( 4, 2, 4 ),
 ( 0.000000000000000000, 0.0001497467027049253347, 0.0002994934054098506693 ),
 .UNSPECIFIED. ) ;
#114034 = CARTESIAN_POINT ( 'NONE',  ( 23.14999999999999858, 64.40000000001175806, -76.45131071479988805 ) ) ;
#114033 = CARTESIAN_POINT ( 'NONE',  ( -16.88783316861808714, 9.950000000011137047, -154.7477359580207406 ) ) ;
#114035 = DIRECTION ( 'NONE',  ( 0.000000000000000000, 0.1350103645451835865, 0.9908441862701605762 ) ) ;
#114036 = DIRECTION ( 'NONE',  ( -0.000000000000000000, 0.8103668758649523740, -0.5859227990963290500 ) ) ;
#114037 = CARTESIAN_POINT ( 'NONE',  ( -18.33682934331497094, 85.51118559110597062, -163.1174527158505612 ) ) ;
#114038 = CARTESIAN_POINT ( 'NONE',  ( -20.64999999999999858, -8.999999999988844479, -158.1060308773475924 ) ) ;
#114039 = CYLINDRICAL_SURFACE ( 'NONE', #92690, 0.1000000000000052097 ) ;
#114040 = VECTOR ( 'NONE', #34799, 1000.000000000000114 ) ;
#114042 = ORIENTED_EDGE ( 'NONE', *, *, #184687, .T. ) ;
#114041 = AXIS2_PLACEMENT_3D ( 'NONE', #39581, #216885, #37002 ) ;
#114043 = EDGE_CURVE ( 'NONE', #121041, #130825, #196555, .T. ) ;
#114044 = DIRECTION ( 'NONE',  ( 0.8049926720990051576, -0.5932847527679298016, -4.142885285818778274E-15 ) ) ;
#114045 = CIRCLE ( 'NONE', #184783, 11.74999999999999822 ) ;
#114046 = ORIENTED_EDGE ( 'NONE', *, *, #230648, .T. ) ;
#114047 = ORIENTED_EDGE ( 'NONE', *, *, #31543, .F. ) ;
#114048 = CARTESIAN_POINT ( 'NONE',  ( -20.54999999999999716, 74.00000000001151079, -49.24772940728643533 ) ) ;
#114049 = VERTEX_POINT ( 'NONE', #77884 ) ;
#114050 = APPLICATION_CONTEXT ( 'automotive_design' ) ;
#114051 = EDGE_CURVE ( 'NONE', #163468, #149860, #88371, .T. ) ;
#114052 = ORIENTED_EDGE ( 'NONE', *, *, #128157, .T. ) ;
#114053 = CARTESIAN_POINT ( 'NONE',  ( -21.11833042828143547, 30.77367799691945294, -252.1799001274110310 ) ) ;
#114054 = FILL_AREA_STYLE ('',( #254806 ) ) ;
#114055 = EDGE_CURVE ( 'NONE', #188850, #109895, #121738, .T. ) ;
#114056 = CIRCLE ( 'NONE', #118170, 0.1000000000000028644 ) ;
#114057 = ORIENTED_EDGE ( 'NONE', *, *, #31655, .F. ) ;
#114058 = AXIS2_PLACEMENT_3D ( 'NONE', #221302, #64811, #257830 ) ;
#114059 = AXIS2_PLACEMENT_3D ( 'NONE', #76147, #16211, #38330 ) ;
#114060 = ORIENTED_EDGE ( 'NONE', *, *, #194790, .T. ) ;
#114061 = CYLINDRICAL_SURFACE ( 'NONE', #254642, 0.1000000000000028644 ) ;
#114062 = DIRECTION ( 'NONE',  ( 0.000000000000000000, 0.000000000000000000, 1.000000000000000000 ) ) ;
#114063 = DIRECTION ( 'NONE',  ( 0.7071359030027766224, 0.000000000000000000, -0.7070776581709024011 ) ) ;
#114064 = DIRECTION ( 'NONE',  ( -1.000000000000000000, -0.000000000000000000, -0.000000000000000000 ) ) ;
#114065 = FACE_OUTER_BOUND ( 'NONE', #109527, .T. ) ;
#114067 = EDGE_CURVE ( 'NONE', #187820, #221706, #13398, .T. ) ;
#114066 =( BOUNDED_CURVE ( )  B_SPLINE_CURVE ( 3, ( #30813, #189858, #90740, #230258 ),
 .UNSPECIFIED., .F., .F. ) 
 B_SPLINE_CURVE_WITH_KNOTS ( ( 4, 4 ),
 ( 4.712388980384690562, 5.672655318024641069 ),
 .UNSPECIFIED. ) 
 CURVE ( )  GEOMETRIC_REPRESENTATION_ITEM ( )  RATIONAL_B_SPLINE_CURVE ( ( 1.000000000000000000, 0.9246222802177432865, 0.9246222802177432865, 1.000000000000000000 ) ) 
 REPRESENTATION_ITEM ( '' )  );
#114069 = DIRECTION ( 'NONE',  ( 1.000000000000000000, 0.000000000000000000, -0.000000000000000000 ) ) ;
#114068 = FACE_OUTER_BOUND ( 'NONE', #52395, .T. ) ;
#114070 = DIRECTION ( 'NONE',  ( -1.000000000000000000, -0.000000000000000000, -0.000000000000000000 ) ) ;
#114072 = ORIENTED_EDGE ( 'NONE', *, *, #33729, .F. ) ;
#114071 = DIRECTION ( 'NONE',  ( 1.000000000000000000, 0.000000000000000000, 0.000000000000000000 ) ) ;
#114074 = CYLINDRICAL_SURFACE ( 'NONE', #183452, 0.09999999999999609201 ) ;
#114073 = DIRECTION ( 'NONE',  ( 0.000000000000000000, -1.000000000000000000, -3.469446951953515108E-14 ) ) ;
#114075 = CARTESIAN_POINT ( 'NONE',  ( -18.59999999999999787, 66.65000000001150227, -48.27310748452438816 ) ) ;
#114076 = VERTEX_POINT ( 'NONE', #140425 ) ;
#114077 = CARTESIAN_POINT ( 'NONE',  ( 21.05095171578076574, 8.776179878782192745, -146.1658732766379103 ) ) ;
#114079 = EDGE_CURVE ( 'NONE', #80843, #16782, #217376, .T. ) ;
#114078 = DIRECTION ( 'NONE',  ( -1.000000000000000000, 0.000000000000000000, 0.000000000000000000 ) ) ;
#114081 = EDGE_CURVE ( 'NONE', #93242, #206465, #159165, .T. ) ;
#114080 = ORIENTED_EDGE ( 'NONE', *, *, #140931, .F. ) ;
#114082 = DIRECTION ( 'NONE',  ( 0.000000000000000000, 1.000000000000000000, 7.116814260417668513E-15 ) ) ;
#114083 = B_SPLINE_CURVE_WITH_KNOTS ( 'NONE', 3,
 ( #77034, #236114, #37941, #57462, #137016, #216549, #32825, #232291, #112333, #191887 ),
 .UNSPECIFIED., .F., .F.,
 ( 4, 3, 3, 4 ),
 ( 0.000000000000000000, 3.394313611811463347E-05, 6.779740500699467213E-05, 0.0001049857339142579784 ),
 .UNSPECIFIED. ) ;
#114084 = DIRECTION ( 'NONE',  ( 0.000000000000000000, 0.9126074666063765939, 0.4088369013363289950 ) ) ;
#114085 = CARTESIAN_POINT ( 'NONE',  ( -20.94999999999999929, 70.15000000001211333, -126.3906102602463619 ) ) ;
#114086 = ORIENTED_EDGE ( 'NONE', *, *, #193872, .T. ) ;
#114087 = ORIENTED_EDGE ( 'NONE', *, *, #198811, .F. ) ;
#114088 = EDGE_CURVE ( 'NONE', #235880, #6238, #121580, .T. ) ;
#114089 = CIRCLE ( 'NONE', #193223, 2.000000000000002665 ) ;
#114090 = DIRECTION ( 'NONE',  ( 1.000000000000000000, -2.986185139342070877E-16, 6.665775143889692774E-16 ) ) ;
#114091 = DIRECTION ( 'NONE',  ( -1.000000000000000000, 0.000000000000000000, 0.000000000000000000 ) ) ;
#114092 = CARTESIAN_POINT ( 'NONE',  ( 20.94999999999999929, 74.16465844978765176, -124.9679561919613207 ) ) ;
#114094 = EDGE_CURVE ( 'NONE', #244838, #2789, #218675, .T. ) ;
#114093 = DIRECTION ( 'NONE',  ( 2.952720810173289112E-16, 1.000000000000000000, -6.088138035986627436E-46 ) ) ;
#114095 = ORIENTED_EDGE ( 'NONE', *, *, #172282, .F. ) ;
#114096 = ADVANCED_FACE ( 'NONE', ( #894 ), #178310, .F. ) ;
#114097 = LINE ( 'NONE', #37159, #179631 ) ;
#114098 = DIRECTION ( 'NONE',  ( 0.000000000000000000, 0.000000000000000000, -1.000000000000000000 ) ) ;
#114099 = CYLINDRICAL_SURFACE ( 'NONE', #182970, 0.8750000000000007772 ) ;
#114100 = CARTESIAN_POINT ( 'NONE',  ( -18.59999999999999787, 80.78317333349157536, -192.9003134612049166 ) ) ;
#114101 = VECTOR ( 'NONE', #100445, 1000.000000000000000 ) ;
#114102 = AXIS2_PLACEMENT_3D ( 'NONE', #92364, #57064, #251444 ) ;
#114103 = CARTESIAN_POINT ( 'NONE',  ( -20.64999999999999858, 25.94586868676353575, -241.5435999122864530 ) ) ;
#114104 = TOROIDAL_SURFACE ( 'NONE', #51729, 0.2000000000000000111, 0.1000000000000000056 ) ;
#114106 = VERTEX_POINT ( 'NONE', #25630 ) ;
#114105 = CARTESIAN_POINT ( 'NONE',  ( -18.37013991200266005, 64.50025238380065673, -194.3161304950415627 ) ) ;
#114107 = SPHERICAL_SURFACE ( 'NONE', #218251, 0.1000000000000000056 ) ;
#114109 = EDGE_CURVE ( 'NONE', #183416, #97655, #202974, .T. ) ;
#114108 = DIRECTION ( 'NONE',  ( -0.000000000000000000, 0.8814952561688428334, -0.4721928772777352346 ) ) ;
#114110 = SPHERICAL_SURFACE ( 'NONE', #75143, 0.1000000000000000056 ) ;
#114111 = DIRECTION ( 'NONE',  ( 1.000000000000000000, 0.000000000000000000, 0.000000000000000000 ) ) ;
#114112 = EDGE_CURVE ( 'NONE', #185078, #32552, #196719, .T. ) ;
#114113 = DIRECTION ( 'NONE',  ( 0.000000000000000000, -0.8814952561673441433, 0.4721928772805327745 ) ) ;
#114115 = VERTEX_POINT ( 'NONE', #43907 ) ;
#114114 = DIRECTION ( 'NONE',  ( 1.040834085586001836E-13, -0.4105728183244014562, -0.9118278131605539460 ) ) ;
#114116 = DIRECTION ( 'NONE',  ( -0.000000000000000000, 0.1686199900910312910, -0.9856811345164826488 ) ) ;
#114117 = DIRECTION ( 'NONE',  ( -3.265361837132814079E-16, 0.4721928772777359007, 0.8814952561688425003 ) ) ;
#114118 = CARTESIAN_POINT ( 'NONE',  ( -18.35663730107557257, 11.47390742651120021, -9.250000000000001776 ) ) ;
#114119 = ORIENTED_EDGE ( 'NONE', *, *, #191183, .F. ) ;
#114120 = CYLINDRICAL_SURFACE ( 'NONE', #5408, 0.09999999999999939493 ) ;
#114121 = DIRECTION ( 'NONE',  ( 1.000000000000000000, 0.000000000000000000, 0.000000000000000000 ) ) ;
#114122 = FACE_OUTER_BOUND ( 'NONE', #243247, .T. ) ;
#114123 = CARTESIAN_POINT ( 'NONE',  ( -18.59999999999999787, 68.97833521811159585, -65.68954208262705663 ) ) ;
#114124 = EDGE_CURVE ( 'NONE', #251232, #249371, #239547, .T. ) ;
#114125 = VECTOR ( 'NONE', #70636, 1000.000000000000000 ) ;
#114126 = CARTESIAN_POINT ( 'NONE',  ( -16.87036670365549895, 66.01058118070993430, -57.00266760182645243 ) ) ;
#114127 = AXIS2_PLACEMENT_3D ( 'NONE', #177236, #201905, #37722 ) ;
#114128 = DIRECTION ( 'NONE',  ( -0.000000000000000000, -0.1298341882519737922, -0.9915357197604890427 ) ) ;
#114130 = VERTEX_POINT ( 'NONE', #59581 ) ;
#114129 = CIRCLE ( 'NONE', #84874, 0.09999999999998898659 ) ;
#114131 = EDGE_LOOP ( 'NONE', ( #7244, #125461, #13389, #101463 ) ) ;
#114132 = AXIS2_PLACEMENT_3D ( 'NONE', #183261, #58143, #158581 ) ;
#114133 = CARTESIAN_POINT ( 'NONE',  ( -18.40000000000000213, 62.48575673152180343, -209.5207689439494345 ) ) ;
#114135 = CYLINDRICAL_SURFACE ( 'NONE', #124773, 0.09999999999999939493 ) ;
#114134 = AXIS2_PLACEMENT_3D ( 'NONE', #254292, #213899, #35308 ) ;
#114136 = DIRECTION ( 'NONE',  ( 1.000000000000000000, 0.000000000000000000, 0.000000000000000000 ) ) ;
#114137 = DIRECTION ( 'NONE',  ( 0.000000000000000000, 0.000000000000000000, 1.000000000000000000 ) ) ;
#114138 = CARTESIAN_POINT ( 'NONE',  ( -21.05000000000000071, 30.43677443282724937, -239.5249545687858870 ) ) ;
#114139 = VECTOR ( 'NONE', #90622, 1000.000000000000000 ) ;
#114140 = EDGE_CURVE ( 'NONE', #104543, #129019, #201692, .T. ) ;
#114141 = CIRCLE ( 'NONE', #64270, 0.1000000000000013933 ) ;
#114142 = CYLINDRICAL_SURFACE ( 'NONE', #104854, 0.09999999999999939493 ) ;
#114143 = AXIS2_PLACEMENT_3D ( 'NONE', #191843, #234788, #138231 ) ;
#114144 = CARTESIAN_POINT ( 'NONE',  ( -16.94180778212362881, 9.992443055743304825, -113.1041835705332801 ) ) ;
#114145 = EDGE_CURVE ( 'NONE', #91499, #128875, #50961, .T. ) ;
#114146 = AXIS2_PLACEMENT_3D ( 'NONE', #132199, #29290, #188317 ) ;
#114147 = B_SPLINE_CURVE_WITH_KNOTS ( 'NONE', 3,
 ( #121757, #138687, #102136, #21376, #100839, #77444, #1773, #59153, #256049, #482, #119175, #158331, #39663, #198702, #236534, #240407, #57888, #78736, #61761 ),
 .UNSPECIFIED., .F., .F.,
 ( 4, 3, 3, 3, 3, 3, 4 ),
 ( 0.000000000000000000, 2.646747978908900846E-05, 5.271166642128170848E-05, 9.008788829884258422E-05, 0.0001426648776560945301, 0.0001897378458659844771, 0.0001917382627806300734 ),
 .UNSPECIFIED. ) ;
#114148 = CARTESIAN_POINT ( 'NONE',  ( -20.64999999999999858, -9.000000000000001776, -23.60603087734756045 ) ) ;
#114149 = ORIENTED_EDGE ( 'NONE', *, *, #27094, .T. ) ;
#114150 = FACE_BOUND ( 'NONE', #184147, .T. ) ;
#114151 = ADVANCED_FACE ( 'NONE', ( #199132 ), #124736, .T. ) ;
#114152 = EDGE_CURVE ( 'NONE', #163086, #14870, #211624, .T. ) ;
#114153 = ORIENTED_EDGE ( 'NONE', *, *, #86724, .T. ) ;
#114154 = DIRECTION ( 'NONE',  ( 0.000000000000000000, 0.9126074666063770380, 0.4088369013363278848 ) ) ;
#114155 = LINE ( 'NONE', #178008, #184502 ) ;
#114156 = DIRECTION ( 'NONE',  ( 0.000000000000000000, -6.982962677686266711E-15, 1.000000000000000000 ) ) ;
#114158 = ORIENTED_EDGE ( 'NONE', *, *, #215880, .T. ) ;
#114157 = CARTESIAN_POINT ( 'NONE',  ( -16.87683809663752399, 9.864913447291341342, -87.22428155130397442 ) ) ;
#114160 = VECTOR ( 'NONE', #77040, 1000.000000000000000 ) ;
#114159 = CARTESIAN_POINT ( 'NONE',  ( -18.50000000000000000, 66.65000000001150227, -48.17310748452438673 ) ) ;
#114162 = EDGE_CURVE ( 'NONE', #11331, #160449, #99993, .T. ) ;
#114161 = DIRECTION ( 'NONE',  ( 0.000000000000000000, 1.000000000000000000, 0.000000000000000000 ) ) ;
#114163 = CARTESIAN_POINT ( 'NONE',  ( 22.39999999999999858, 75.90000000001170122, -77.31388708289770761 ) ) ;
#114164 = VECTOR ( 'NONE', #142419, 1000.000000000000000 ) ;
#114165 = EDGE_LOOP ( 'NONE', ( #201794, #200303, #43439, #34211 ) ) ;
#114167 = DIRECTION ( 'NONE',  ( 0.000000000000000000, 0.000000000000000000, -1.000000000000000000 ) ) ;
#114166 = AXIS2_PLACEMENT_3D ( 'NONE', #24376, #225093, #226375 ) ;
#114168 = CARTESIAN_POINT ( 'NONE',  ( 18.49999999999999289, 65.55993210786904513, -145.2559897356427996 ) ) ;
#114169 = DIRECTION ( 'NONE',  ( 0.000000000000000000, 0.4930308989874980785, 0.8700118002898462599 ) ) ;
#114170 = DIRECTION ( 'NONE',  ( 0.000000000000000000, -0.2128009952263568982, 0.9770955615653323934 ) ) ;
#114171 = DIRECTION ( 'NONE',  ( 0.000000000000000000, -1.000000000000000000, 0.000000000000000000 ) ) ;
#114172 = EDGE_CURVE ( 'NONE', #146220, #249282, #40090, .T. ) ;
#114173 = ADVANCED_FACE ( 'NONE', ( #119613 ), #242096, .T. ) ;
#114174 = ORIENTED_EDGE ( 'NONE', *, *, #246306, .T. ) ;
#114175 =( BOUNDED_SURFACE ( )  B_SPLINE_SURFACE ( 3, 2, ( 
 ( #5323, #26221, #165737 ),
 ( #142291, #67898, #84852 ),
 ( #186579, #245262, #164445 ),
 ( #87447, #147436, #103151 ),
 ( #226974, #62766, #202278 ),
 ( #221807, #43206, #182729 ) ),
 .UNSPECIFIED., .F., .F., .F. ) 
 B_SPLINE_SURFACE_WITH_KNOTS ( ( 4, 2, 4 ),
 ( 3, 3 ),
 ( 6.719893378902767184E-05, 0.0002757154632485745360, 0.0004842319927081213866 ),
 ( 0.000000000000000000, 1.000000000000000000 ),
 .UNSPECIFIED. ) 
 GEOMETRIC_REPRESENTATION_ITEM ( )  RATIONAL_B_SPLINE_SURFACE ( (
 ( 1.000000000000000000, 0.7250110520819758042, 1.000000000000000000),
 ( 1.000000000000000000, 0.7277932058380147673, 1.000000000000000000),
 ( 1.000000000000000000, 0.7278452872589648015, 1.000000000000000000),
 ( 1.000000000000000000, 0.7221445671577165770, 1.000000000000000000),
 ( 1.000000000000000000, 0.7163662143758368073, 1.000000000000000000),
 ( 1.000000000000000000, 0.7071067811865475727, 1.000000000000000000) ) ) 
 REPRESENTATION_ITEM ( '' )  SURFACE ( )  );
#114176 = DIRECTION ( 'NONE',  ( 1.000000000000000000, 0.000000000000000000, 0.000000000000000000 ) ) ;
#114177 = CARTESIAN_POINT ( 'NONE',  ( -16.85939591225058720, 66.09477352162400621, -90.06303923805535305 ) ) ;
#114178 = ORIENTED_EDGE ( 'NONE', *, *, #120988, .T. ) ;
#114179 = CARTESIAN_POINT ( 'NONE',  ( -21.05000000000000071, 76.00000000001244871, -170.0231074845243597 ) ) ;
#114180 = EDGE_CURVE ( 'NONE', #4242, #150112, #162589, .T. ) ;
#114181 = CARTESIAN_POINT ( 'NONE',  ( 22.49999999999999645, 55.86495732666937641, -232.8769840133978164 ) ) ;
#114182 = CARTESIAN_POINT ( 'NONE',  ( -18.50000000000000000, 61.38756220455727686, -221.6813469827248184 ) ) ;
#114183 = AXIS2_PLACEMENT_3D ( 'NONE', #108421, #247915, #71874 ) ;
#114184 = EDGE_LOOP ( 'NONE', ( #214261, #146242, #164358, #51842 ) ) ;
#114185 = CARTESIAN_POINT ( 'NONE',  ( 20.95512820512820440, 39.31056039967181448, -236.7220595557971023 ) ) ;
#114186 = CARTESIAN_POINT ( 'NONE',  ( -16.89155683852450807, 9.950000000011137047, -147.2773718495397475 ) ) ;
#114187 = VECTOR ( 'NONE', #247299, 1000.000000000000000 ) ;
#114189 = VERTEX_POINT ( 'NONE', #206832 ) ;
#114188 = CIRCLE ( 'NONE', #222502, 0.1000000000000089567 ) ;
#114190 = EDGE_CURVE ( 'NONE', #145748, #230477, #142277, .T. ) ;
#114191 = ADVANCED_FACE ( 'NONE', ( #6047 ), #188548, .T. ) ;
#114192 = AXIS2_PLACEMENT_3D ( 'NONE', #32295, #12733, #76517 ) ;
#114193 = ORIENTED_EDGE ( 'NONE', *, *, #216837, .F. ) ;
#114194 = DIRECTION ( 'NONE',  ( -1.000000000000000000, 0.000000000000000000, 0.000000000000000000 ) ) ;
#114195 = CARTESIAN_POINT ( 'NONE',  ( 21.14999999999999858, 43.45833571831320796, -234.7657887233443716 ) ) ;
#114197 = ORIENTED_EDGE ( 'NONE', *, *, #257807, .F. ) ;
#114196 = CARTESIAN_POINT ( 'NONE',  ( 20.94999999999999929, -1.349153571964892606, -141.7874973355899328 ) ) ;
#114198 = EDGE_CURVE ( 'NONE', #195203, #60760, #71191, .T. ) ;
#114199 = CARTESIAN_POINT ( 'NONE',  ( -12.25000000000000178, 66.65000000001204228, -119.7731074845243739 ) ) ;
#114201 = AXIS2_PLACEMENT_3D ( 'NONE', #159404, #155578, #178996 ) ;
#114200 = CARTESIAN_POINT ( 'NONE',  ( -22.49436431346200038, 11.64995094766461392, -133.9330964702777749 ) ) ;
#114202 = DIRECTION ( 'NONE',  ( 2.952720810173289112E-16, 0.4088369013363246096, -0.9126074666063785923 ) ) ;
#114203 = DIRECTION ( 'NONE',  ( 1.000000000000000000, 0.000000000000000000, 0.000000000000000000 ) ) ;
#114204 = ADVANCED_FACE ( 'NONE', ( #169029 ), #100996, .F. ) ;
#114205 = DIRECTION ( 'NONE',  ( 0.000000000000000000, -1.000000000000000000, 0.000000000000000000 ) ) ;
#114206 = AXIS2_PLACEMENT_3D ( 'NONE', #67206, #86747, #25527 ) ;
#114207 = DIRECTION ( 'NONE',  ( 0.000000000000000000, 1.000000000000000000, 0.000000000000000000 ) ) ;
#114208 = CARTESIAN_POINT ( 'NONE',  ( -16.81095280782811230, 66.05000000001230376, -157.3731074845252920 ) ) ;
#114209 = AXIS2_PLACEMENT_3D ( 'NONE', #162600, #221258, #240850 ) ;
#114211 = VERTEX_POINT ( 'NONE', #129847 ) ;
#114210 = CARTESIAN_POINT ( 'NONE',  ( 21.14999999999999858, 6.550000000011156231, -146.1500000000000341 ) ) ;
#114212 = ORIENTED_EDGE ( 'NONE', *, *, #161341, .T. ) ;
#114214 = CARTESIAN_POINT ( 'NONE',  ( -16.85697194749120698, 51.37571476901084822, -232.1008225933170479 ) ) ;
#114213 = CARTESIAN_POINT ( 'NONE',  ( -22.57320508075687115, 64.25000000001269029, -203.5231074845244166 ) ) ;
#114215 = AXIS2_PLACEMENT_3D ( 'NONE', #2731, #39336, #58842 ) ;
#114217 = ORIENTED_EDGE ( 'NONE', *, *, #53766, .F. ) ;
#114216 = DIRECTION ( 'NONE',  ( 0.000000000000000000, -0.9126074666063773710, -0.4088369013363274962 ) ) ;
#114218 = EDGE_LOOP ( 'NONE', ( #96066, #243992, #9792, #42782 ) ) ;
#114219 = CARTESIAN_POINT ( 'NONE',  ( -16.78805706634180694, 66.05174750694135355, -182.6789542764925898 ) ) ;
#114220 = CARTESIAN_POINT ( 'NONE',  ( 20.05000000000002913, 7.250000000011171508, -87.85000000000003695 ) ) ;
#114221 = CIRCLE ( 'NONE', #234438, 0.1000000000000055705 ) ;
#114222 = CARTESIAN_POINT ( 'NONE',  ( -18.40000000000000213, 64.52683809664981140, -157.4731074845244621 ) ) ;
#114223 = CARTESIAN_POINT ( 'NONE',  ( -20.85000000000000142, 68.97833521811131163, -32.18954208262707795 ) ) ;
#114224 = EDGE_CURVE ( 'NONE', #95913, #60331, #210681, .T. ) ;
#114225 = DIRECTION ( 'NONE',  ( 0.000000000000000000, 0.000000000000000000, 1.000000000000000000 ) ) ;
#114226 = AXIS2_PLACEMENT_3D ( 'NONE', #73734, #151994, #226680 ) ;
#114227 = CARTESIAN_POINT ( 'NONE',  ( -18.40000000000000213, 64.52683809664951298, -115.5731074845243853 ) ) ;
#114228 = CARTESIAN_POINT ( 'NONE',  ( -20.64999999999999858, 4.350000000011156054, -121.6500000000000341 ) ) ;
#114229 = EDGE_CURVE ( 'NONE', #182399, #221407, #167721, .T. ) ;
#114230 = AXIS2_PLACEMENT_3D ( 'NONE', #174343, #97273, #176880 ) ;
#114231 = ORIENTED_EDGE ( 'NONE', *, *, #231550, .T. ) ;
#114232 = VERTEX_POINT ( 'NONE', #225084 ) ;
#114233 = CARTESIAN_POINT ( 'NONE',  ( 21.05000000000000071, 30.91371304215671145, -252.1483800927532002 ) ) ;
#114234 = ORIENTED_EDGE ( 'NONE', *, *, #124260, .T. ) ;
#114235 = CARTESIAN_POINT ( 'NONE',  ( 23.15000000000000213, 11.39998237908105594, -245.7725481090871540 ) ) ;
#114236 = ORIENTED_EDGE ( 'NONE', *, *, #6621, .T. ) ;
#114238 = VECTOR ( 'NONE', #172737, 1000.000000000000000 ) ;
#114237 = CARTESIAN_POINT ( 'NONE',  ( -21.14999999999999858, 76.00000000001213607, -136.5231074845242745 ) ) ;
#114239 = AXIS2_PLACEMENT_3D ( 'NONE', #167229, #87641, #190634 ) ;
#114240 = CIRCLE ( 'NONE', #235060, 0.5000000000000004441 ) ;
#114241 = DIRECTION ( 'NONE',  ( 1.000000000000000000, 0.000000000000000000, -0.000000000000000000 ) ) ;
#114242 = ORIENTED_EDGE ( 'NONE', *, *, #256521, .F. ) ;
#114243 = EDGE_CURVE ( 'NONE', #64537, #242736, #171826, .T. ) ;
#114244 = DIRECTION ( 'NONE',  ( 0.000000000000000000, 0.000000000000000000, -1.000000000000000000 ) ) ;
#114245 = ORIENTED_EDGE ( 'NONE', *, *, #4367, .F. ) ;
#114246 = CARTESIAN_POINT ( 'NONE',  ( 21.05000000000000071, 71.00000000001253397, -182.4283735034374843 ) ) ;
#114247 = ORIENTED_EDGE ( 'NONE', *, *, #91347, .F. ) ;
#114248 = DIRECTION ( 'NONE',  ( -1.000000000000000000, 0.000000000000000000, 0.000000000000000000 ) ) ;
#114249 = DIRECTION ( 'NONE',  ( -1.000000000000000000, -0.000000000000000000, -0.000000000000000000 ) ) ;
#114250 = ORIENTED_EDGE ( 'NONE', *, *, #94348, .F. ) ;
#114251 = CARTESIAN_POINT ( 'NONE',  ( -18.40000000000000213, 13.90230816252087642, -210.9187585823742666 ) ) ;
#114252 = ORIENTED_EDGE ( 'NONE', *, *, #188753, .F. ) ;
#114255 = ORIENTED_EDGE ( 'NONE', *, *, #228199, .T. ) ;
#114254 = DIRECTION ( 'NONE',  ( -1.000000000000000000, -2.952720810173289112E-16, 0.000000000000000000 ) ) ;
#114253 = CYLINDRICAL_SURFACE ( 'NONE', #203470, 0.09999999999999939493 ) ;
#114256 = EDGE_CURVE ( 'NONE', #188719, #227881, #226363, .T. ) ;
#114257 = CARTESIAN_POINT ( 'NONE',  ( -20.85000000106584750, 64.25000000001148237, -42.86760282805085609 ) ) ;
#114258 = CIRCLE ( 'NONE', #35197, 0.09999999999999939493 ) ;
#114259 = EDGE_LOOP ( 'NONE', ( #173077, #110323, #17950, #102469, #130613, #127287, #123786, #64939, #161193, #190387, #244631, #229690, #228044, #224550, #166127, #152494, #892, #221736 ) ) ;
#114260 = EDGE_LOOP ( 'NONE', ( #141450, #184199, #73954, #1326 ) ) ;
#114261 = AXIS2_PLACEMENT_3D ( 'NONE', #169329, #145855, #164156 ) ;
#114262 = CARTESIAN_POINT ( 'NONE',  ( 21.05000000000000071, 4.850467289730772791, -112.5342674090017141 ) ) ;
#114263 = EDGE_LOOP ( 'NONE', ( #207573, #8894, #47318 ) ) ;
#114264 = CARTESIAN_POINT ( 'NONE',  ( -22.39999999999999858, 75.90000000001268177, -203.5231074845243597 ) ) ;
#114265 = CARTESIAN_POINT ( 'NONE',  ( 22.39999999999999503, 64.18196446391819165, -247.0985338183330668 ) ) ;
#114266 = CARTESIAN_POINT ( 'NONE',  ( -21.14999999999994174, 64.35000000001120668, -5.923107484524795296 ) ) ;
#114267 = DIRECTION ( 'NONE',  ( 0.000000000000000000, -0.9126074666063769270, -0.4088369013363280513 ) ) ;
#114268 = DIRECTION ( 'NONE',  ( 0.000000000000000000, 0.8636236514130390951, -0.5041370733441546959 ) ) ;
#114269 = ORIENTED_EDGE ( 'NONE', *, *, #105144, .T. ) ;
#114270 = DIRECTION ( 'NONE',  ( 0.000000000000000000, -0.8660254037844419273, 0.4999999999999942824 ) ) ;
#114271 = DIRECTION ( 'NONE',  ( 4.408576920032447355E-17, 0.1350103645451807555, 0.9908441862701610203 ) ) ;
#114272 = DIRECTION ( 'NONE',  ( 0.000000000000000000, 1.000000000000000000, 1.387778780781444413E-14 ) ) ;
#114273 = ORIENTED_EDGE ( 'NONE', *, *, #176606, .F. ) ;
#114274 = DIRECTION ( 'NONE',  ( -0.000000000000000000, -0.4088369013363281623, 0.9126074666063771490 ) ) ;
#114275 = VERTEX_POINT ( 'NONE', #227669 ) ;
#114276 = DIRECTION ( 'NONE',  ( 0.000000000000000000, 0.000000000000000000, 1.000000000000000000 ) ) ;
#114277 = ORIENTED_EDGE ( 'NONE', *, *, #111197, .F. ) ;
#114278 =( GEOMETRIC_REPRESENTATION_CONTEXT ( 3 ) GLOBAL_UNCERTAINTY_ASSIGNED_CONTEXT ( ( #227720 ) ) GLOBAL_UNIT_ASSIGNED_CONTEXT ( ( #7090, #86608, #178385 ) ) REPRESENTATION_CONTEXT ( 'NONE', 'WORKASPACE' ) );
#114279 = CARTESIAN_POINT ( 'NONE',  ( -21.05000000000000071, -1.835341550224411922, -11.65515129256297833 ) ) ;
#114280 = CARTESIAN_POINT ( 'NONE',  ( -21.05000000000000071, -11.41227409414968719, -3.000000000000002665 ) ) ;
#114282 = ORIENTED_EDGE ( 'NONE', *, *, #1096, .F. ) ;
#114281 = CARTESIAN_POINT ( 'NONE',  ( -18.59999999999999787, 77.83585931145570669, -125.0186683157258329 ) ) ;
#114283 = LINE ( 'NONE', #170461, #13083 ) ;
#114284 = VERTEX_POINT ( 'NONE', #8637 ) ;
#114285 = CARTESIAN_POINT ( 'NONE',  ( -21.05000000000000071, 36.02367271998545561, -235.8812521208699025 ) ) ;
#114286 = ADVANCED_FACE ( 'NONE', ( #105118 ), #246786, .F. ) ;
#114287 = LINE ( 'NONE', #249953, #97865 ) ;
#114288 = VERTEX_POINT ( 'NONE', #184688 ) ;
#114289 = CARTESIAN_POINT ( 'NONE',  ( -21.07016717457010557, 1.115297090792388540E-11, -127.6790591618991044 ) ) ;
#114290 = CARTESIAN_POINT ( 'NONE',  ( -21.05000000000000071, 1.851028230152016674, -112.1539132694225316 ) ) ;
#114291 = ORIENTED_EDGE ( 'NONE', *, *, #161259, .T. ) ;
#114292 = AXIS2_PLACEMENT_3D ( 'NONE', #113309, #76743, #57160 ) ;
#114293 = AXIS2_PLACEMENT_3D ( 'NONE', #43338, #5457, #181575 ) ;
#114294 = ORIENTED_EDGE ( 'NONE', *, *, #32952, .F. ) ;
#114295 = VECTOR ( 'NONE', #230506, 1000.000000000000000 ) ;
#114296 = AXIS2_PLACEMENT_3D ( 'NONE', #62406, #196763, #118549 ) ;
#114297 = CARTESIAN_POINT ( 'NONE',  ( 15.07585980824113925, 9.417632963117448242, -118.6489484657323175 ) ) ;
#114298 = DIRECTION ( 'NONE',  ( -1.020425574104003999E-15, -0.2128009952263603677, 0.9770955615653313941 ) ) ;
#114299 =( GEOMETRIC_REPRESENTATION_CONTEXT ( 3 ) GLOBAL_UNCERTAINTY_ASSIGNED_CONTEXT ( ( #191203 ) ) GLOBAL_UNIT_ASSIGNED_CONTEXT ( ( #133583, #174043, #171470 ) ) REPRESENTATION_CONTEXT ( 'NONE', 'WORKASPACE' ) );
#114300 = EDGE_CURVE ( 'NONE', #4264, #257620, #155067, .T. ) ;
#114301 = EDGE_CURVE ( 'NONE', #231796, #112321, #128581, .T. ) ;
#114303 = EDGE_LOOP ( 'NONE', ( #51143, #56208, #155342, #161415 ) ) ;
#114302 = DIRECTION ( 'NONE',  ( 0.000000000000000000, 0.1350103645451876666, -0.9908441862701600211 ) ) ;
#114304 = CYLINDRICAL_SURFACE ( 'NONE', #36823, 0.09999999999999939493 ) ;
#114305 = PLANE ( 'NONE',  #160726 ) ;
#114306 = FACE_OUTER_BOUND ( 'NONE', #72655, .T. ) ;
#114307 = CIRCLE ( 'NONE', #222044, 0.1000000000000028644 ) ;
#114309 = DIRECTION ( 'NONE',  ( -1.000000000000000000, -0.000000000000000000, 0.000000000000000000 ) ) ;
#114308 = FACE_OUTER_BOUND ( 'NONE', #12962, .T. ) ;
#114310 = DIRECTION ( 'NONE',  ( 0.000000000000000000, -0.8068669527896844551, -0.5907332058517525963 ) ) ;
#114311 = CARTESIAN_POINT ( 'NONE',  ( -20.94999999999999929, 69.08367151115869831, -247.5088222940653679 ) ) ;
#114312 = EDGE_CURVE ( 'NONE', #190717, #167341, #188353, .T. ) ;
#114313 = DIRECTION ( 'NONE',  ( -0.7071067811865474617, 0.7071067811865474617, 4.937700262164531476E-15 ) ) ;
#114314 = AXIS2_PLACEMENT_3D ( 'NONE', #229179, #93502, #132641 ) ;
#114315 = DIRECTION ( 'NONE',  ( -1.000000000000000000, 0.000000000000000000, 0.000000000000000000 ) ) ;
#114316 = CIRCLE ( 'NONE', #180969, 0.3999999999999975797 ) ;
#114317 = ORIENTED_EDGE ( 'NONE', *, *, #171731, .T. ) ;
#114318 = ORIENTED_EDGE ( 'NONE', *, *, #82261, .T. ) ;
#114319 = CIRCLE ( 'NONE', #251864, 0.09999999999999939493 ) ;
#114320 = ADVANCED_FACE ( 'NONE', ( #26940 ), #167734, .T. ) ;
#114321 = CARTESIAN_POINT ( 'NONE',  ( 18.59999999999998366, 1.115600667400684642E-11, -200.9999999999999432 ) ) ;
#114322 = CIRCLE ( 'NONE', #26869, 2.100000000000004530 ) ;
#114325 = ORIENTED_EDGE ( 'NONE', *, *, #67360, .T. ) ;
#114324 = ADVANCED_FACE ( 'NONE', ( #254876 ), #34451, .F. ) ;
#114323 = DIRECTION ( 'NONE',  ( -1.000000000000000000, 0.000000000000000000, -0.000000000000000000 ) ) ;
#114326 = EDGE_LOOP ( 'NONE', ( #136715, #153231, #225316, #174251 ) ) ;
#114327 = CARTESIAN_POINT ( 'NONE',  ( -21.00000000000000000, 0.3305886640091971196, 0.04453801223857078301 ) ) ;
#114328 = EDGE_LOOP ( 'NONE', ( #68125, #101042, #61426 ) ) ;
#114329 = ADVANCED_FACE ( 'NONE', ( #13766 ), #97110, .F. ) ;
#114330 = AXIS2_PLACEMENT_3D ( 'NONE', #10583, #130507, #225742 ) ;
#114331 = CIRCLE ( 'NONE', #234965, 12.87499999999999822 ) ;
#114332 = AXIS2_PLACEMENT_3D ( 'NONE', #209764, #173251, #71558 ) ;
#114333 = ORIENTED_EDGE ( 'NONE', *, *, #247014, .T. ) ;
#114334 = CIRCLE ( 'NONE', #130905, 0.1000000000000017680 ) ;
#114335 = ADVANCED_FACE ( 'NONE', ( #33372 ), #95849, .F. ) ;
#114336 = LINE ( 'NONE', #2065, #15748 ) ;
#114337 = CIRCLE ( 'NONE', #85082, 0.09999999999999939493 ) ;
#114339 = ORIENTED_EDGE ( 'NONE', *, *, #241021, .F. ) ;
#114338 = EDGE_LOOP ( 'NONE', ( #183209, #241750, #245296, #33776, #49748 ) ) ;
#114340 = ORIENTED_EDGE ( 'NONE', *, *, #100541, .T. ) ;
#114341 = ORIENTED_EDGE ( 'NONE', *, *, #170993, .T. ) ;
#114342 = ORIENTED_EDGE ( 'NONE', *, *, #22415, .T. ) ;
#114344 = CARTESIAN_POINT ( 'NONE',  ( -23.15000000000000213, 36.65892442174935439, -249.5511627012433848 ) ) ;
#114343 = CIRCLE ( 'NONE', #193472, 0.1000000000000028644 ) ;
#114345 = FACE_OUTER_BOUND ( 'NONE', #36081, .T. ) ;
#114346 = CARTESIAN_POINT ( 'NONE',  ( -16.86337532320260735, 30.30768031064097912, -234.8273404860777873 ) ) ;
#114348 = ORIENTED_EDGE ( 'NONE', *, *, #125400, .F. ) ;
#114347 = LINE ( 'NONE', #32266, #66724 ) ;
#114349 = DIRECTION ( 'NONE',  ( 1.000000000000000000, -3.965082230804126670E-15, 0.000000000000000000 ) ) ;
#114350 = CARTESIAN_POINT ( 'NONE',  ( 21.05000000000000426, 12.09419596560308641, -206.1384538536135267 ) ) ;
#114351 = EDGE_LOOP ( 'NONE', ( #214238, #84784, #39214, #240609, #143797 ) ) ;
#114352 = CARTESIAN_POINT ( 'NONE',  ( -23.15000000000000213, 87.48912529308779540, -72.62310748452422615 ) ) ;
#114353 = ORIENTED_EDGE ( 'NONE', *, *, #242793, .F. ) ;
#114354 = CARTESIAN_POINT ( 'NONE',  ( -20.64999999999999858, 1.115600667400684642E-11, -134.0000000000000284 ) ) ;
#114355 = AXIS2_PLACEMENT_3D ( 'NONE', #171992, #152414, #251474 ) ;
#114358 = EDGE_CURVE ( 'NONE', #108161, #86456, #235368, .T. ) ;
#114357 = ORIENTED_EDGE ( 'NONE', *, *, #45778, .F. ) ;
#114356 = CARTESIAN_POINT ( 'NONE',  ( 21.05995757104869526, 8.775389244732430427, -112.6949051229912442 ) ) ;
#114359 = DIRECTION ( 'NONE',  ( -1.000000000000000000, 0.000000000000000000, 0.000000000000000000 ) ) ;
#114360 = CARTESIAN_POINT ( 'NONE',  ( -21.45000000000000284, 68.29142135624984178, -182.3731074845244109 ) ) ;
#114361 = ORIENTED_EDGE ( 'NONE', *, *, #21529, .T. ) ;
#114363 = CARTESIAN_POINT ( 'NONE',  ( 20.94999999999999574, 74.16465844978819177, -191.9679561919613775 ) ) ;
#114362 = CARTESIAN_POINT ( 'NONE',  ( -16.89155683852518663, 9.950000000011138823, -46.77737184953971905 ) ) ;
#114364 = CARTESIAN_POINT ( 'NONE',  ( -23.25000000000000000, 76.00000000001170974, -69.52310748452431710 ) ) ;
#114365 = DIRECTION ( 'NONE',  ( 1.000000000000000000, 0.000000000000000000, 0.000000000000000000 ) ) ;
#114366 = DIRECTION ( 'NONE',  ( -1.000000000000000000, 0.000000000000000000, 0.000000000000000000 ) ) ;
#114367 = ORIENTED_EDGE ( 'NONE', *, *, #188646, .F. ) ;
#114368 = EDGE_LOOP ( 'NONE', ( #208431, #63936, #190963, #115622 ) ) ;
#114369 = EDGE_CURVE ( 'NONE', #148648, #72740, #17598, .T. ) ;
#114370 = DIRECTION ( 'NONE',  ( -1.000000000000000000, -0.000000000000000000, -0.000000000000000000 ) ) ;
#114371 = DIRECTION ( 'NONE',  ( 0.000000000000000000, 0.000000000000000000, 1.000000000000000000 ) ) ;
#114372 = ORIENTED_EDGE ( 'NONE', *, *, #162810, .F. ) ;
#114373 = CARTESIAN_POINT ( 'NONE',  ( -20.64999999999999858, -3.685352791942197115, -226.3713951780953550 ) ) ;
#114374 = EDGE_LOOP ( 'NONE', ( #215801, #108587, #85706, #46099 ) ) ;
#114375 = DIRECTION ( 'NONE',  ( 1.000000000000000000, 0.000000000000000000, 0.000000000000000000 ) ) ;
#114376 = VECTOR ( 'NONE', #65166, 1000.000000000000000 ) ;
#114377 = VERTEX_POINT ( 'NONE', #176708 ) ;
#114378 = CARTESIAN_POINT ( 'NONE',  ( 21.05000000000000071, 67.22371710471961137, -127.9644784893834100 ) ) ;
#114379 =( NAMED_UNIT ( * ) PLANE_ANGLE_UNIT ( ) SI_UNIT ( $, .RADIAN. ) );
#114380 = EDGE_CURVE ( 'NONE', #58178, #100214, #38517, .T. ) ;
#114381 = AXIS2_PLACEMENT_3D ( 'NONE', #63200, #219714, #20253 ) ;
#114382 = ADVANCED_FACE ( 'NONE', ( #73769 ), #231542, .F. ) ;
#114383 = ORIENTED_EDGE ( 'NONE', *, *, #177728, .F. ) ;
#114384 = ORIENTED_EDGE ( 'NONE', *, *, #126321, .F. ) ;
#114385 = VERTEX_POINT ( 'NONE', #253640 ) ;
#114386 = CIRCLE ( 'NONE', #214342, 0.1000000000000053069 ) ;
#114387 = DIRECTION ( 'NONE',  ( 1.000000000000000000, 0.000000000000000000, 0.000000000000000000 ) ) ;
#114388 = DIRECTION ( 'NONE',  ( 0.000000000000000000, 0.4088369013363281623, -0.9126074666063771490 ) ) ;
#114389 = AXIS2_PLACEMENT_3D ( 'NONE', #81012, #200986, #83567 ) ;
#114390 = CARTESIAN_POINT ( 'NONE',  ( -21.05000000000000071, 61.95000000001162022, -64.00941241376342816 ) ) ;
#114391 = DIRECTION ( 'NONE',  ( 1.000000000000000000, 0.000000000000000000, 0.000000000000000000 ) ) ;
#114392 = CARTESIAN_POINT ( 'NONE',  ( 12.30626653967340722, 66.64320997496615462, -119.3182809759104828 ) ) ;
#114393 = EDGE_CURVE ( 'NONE', #231702, #162766, #80163, .T. ) ;
#114395 = DIRECTION ( 'NONE',  ( 1.000000000000000000, 0.000000000000000000, 0.000000000000000000 ) ) ;
#114394 = CARTESIAN_POINT ( 'NONE',  ( 22.50000000000000000, -3.092988775432913506, -228.1437074281570858 ) ) ;
#114396 = VERTEX_POINT ( 'NONE', #236655 ) ;
#114397 = CARTESIAN_POINT ( 'NONE',  ( -20.94999999999999929, 1.250000000011155299, -142.0000000000000284 ) ) ;
#114398 = EDGE_LOOP ( 'NONE', ( #40476, #163772, #41003, #217823 ) ) ;
#114399 = CARTESIAN_POINT ( 'NONE',  ( -20.94999999999999929, 77.26178616857765746, -195.4366085209788935 ) ) ;
#114400 = ORIENTED_EDGE ( 'NONE', *, *, #59596, .F. ) ;
#114401 = VERTEX_POINT ( 'NONE', #215796 ) ;
#114402 = FACE_OUTER_BOUND ( 'NONE', #237748, .T. ) ;
#114403 = AXIS2_PLACEMENT_3D ( 'NONE', #30677, #95736, #72364 ) ;
#114404 = CARTESIAN_POINT ( 'NONE',  ( -21.04999999999999716, 6.497017786442110143, -134.0145456905664503 ) ) ;
#114406 = EDGE_CURVE ( 'NONE', #255134, #183554, #192405, .T. ) ;
#114405 = CARTESIAN_POINT ( 'NONE',  ( -21.05000000000000071, 1.835341550224411922, -11.65515129256298010 ) ) ;
#114407 = EDGE_CURVE ( 'NONE', #181739, #82856, #184252, .T. ) ;
#114408 = CARTESIAN_POINT ( 'NONE',  ( -21.05000000000000071, 1.250000000011155299, -75.00000000000004263 ) ) ;
#114409 = AXIS2_PLACEMENT_3D ( 'NONE', #136147, #236553, #174071 ) ;
#114410 = CARTESIAN_POINT ( 'NONE',  ( 22.59999999999999076, 55.87393739788256397, -232.8427108587849261 ) ) ;
#114411 = ORIENTED_EDGE ( 'NONE', *, *, #20214, .T. ) ;
#114412 = ORIENTED_EDGE ( 'NONE', *, *, #207385, .F. ) ;
#114413 = ADVANCED_FACE ( 'NONE', ( #34637 ), #137547, .T. ) ;
#114414 = DIRECTION ( 'NONE',  ( 0.000000000000000000, -0.4721928772777346239, -0.8814952561688430555 ) ) ;
#114415 = ORIENTED_EDGE ( 'NONE', *, *, #202946, .T. ) ;
#114416 = DIRECTION ( 'NONE',  ( 1.296989514748957922E-15, -0.9887567792719341719, 0.1495327102803664099 ) ) ;
#114417 = FACE_OUTER_BOUND ( 'NONE', #119384, .T. ) ;
#114418 = ORIENTED_EDGE ( 'NONE', *, *, #222621, .F. ) ;
#114419 = CARTESIAN_POINT ( 'NONE',  ( 23.24999999999999289, 64.25000000001165290, -69.42310748452440805 ) ) ;
#114421 = CIRCLE ( 'NONE', #18559, 0.09999999999998898659 ) ;
#114420 = CARTESIAN_POINT ( 'NONE',  ( 23.14999999999999858, 76.00000000001210765, -132.5231074845243313 ) ) ;
#114422 = DIRECTION ( 'NONE',  ( 1.000000000000000000, -0.000000000000000000, -0.000000000000000000 ) ) ;
#114423 = CARTESIAN_POINT ( 'NONE',  ( 21.05000000000000071, 65.27628288308724791, -157.8468678833862100 ) ) ;
#114424 = VERTEX_POINT ( 'NONE', #12508 ) ;
#114425 = DIRECTION ( 'NONE',  ( 1.000000000000000000, -0.000000000000000000, -0.000000000000000000 ) ) ;
#114426 = VECTOR ( 'NONE', #63014, 1000.000000000000000 ) ;
#114427 = CARTESIAN_POINT ( 'NONE',  ( 21.14999999999999858, 21.10816309994747186, -233.7904894189133813 ) ) ;
#114428 = DIRECTION ( 'NONE',  ( -1.000000000000000000, 0.000000000000000000, -0.000000000000000000 ) ) ;
#114429 = AXIS2_PLACEMENT_3D ( 'NONE', #8830, #144459, #29705 ) ;
#114430 = AXIS2_PLACEMENT_3D ( 'NONE', #63642, #222700, #205713 ) ;
#114431 = VERTEX_POINT ( 'NONE', #114138 ) ;
#114432 = AXIS2_PLACEMENT_3D ( 'NONE', #149471, #33394, #111610 ) ;
#114433 = CARTESIAN_POINT ( 'NONE',  ( 21.05000000000000071, 0.09779029131994770863, -161.2421853895238542 ) ) ;
#114434 = ORIENTED_EDGE ( 'NONE', *, *, #10558, .F. ) ;
#114435 = EDGE_CURVE ( 'NONE', #36049, #228338, #30164, .T. ) ;
#114436 = CARTESIAN_POINT ( 'NONE',  ( -18.59999999999999787, 74.93036000061670165, -233.6816308724374949 ) ) ;
#114437 = ADVANCED_FACE ( 'NONE', ( #232835 ), #132433, .T. ) ;
#114438 = DIRECTION ( 'NONE',  ( 7.304098846218134667E-16, 1.000000000000000000, 6.982962677686266711E-15 ) ) ;
#114439 = DIRECTION ( 'NONE',  ( 0.000000000000000000, 0.2617529984165152257, 0.9651348961777124202 ) ) ;
#114440 = FACE_OUTER_BOUND ( 'NONE', #89833, .T. ) ;
#114441 = CARTESIAN_POINT ( 'NONE',  ( -16.94107738177415712, 10.01423928514777550, -46.04999999999999716 ) ) ;
#114442 = VERTEX_POINT ( 'NONE', #252357 ) ;
#114443 = CARTESIAN_POINT ( 'NONE',  ( 18.49999999999999645, 1.866714910068465239, -78.75267524628205251 ) ) ;
#114444 = LINE ( 'NONE', #173185, #223171 ) ;
#114445 = CARTESIAN_POINT ( 'NONE',  ( 21.07094088545302668, 10.02599695582151007, -228.1148069861733063 ) ) ;
#114446 = CARTESIAN_POINT ( 'NONE',  ( -18.50000000000000000, 1.162701749949165642, -175.5999999999999659 ) ) ;
#114447 = EDGE_CURVE ( 'NONE', #86957, #255533, #46872, .T. ) ;
#114448 = CIRCLE ( 'NONE', #122842, 0.5000000000000004441 ) ;
#114449 = CARTESIAN_POINT ( 'NONE',  ( 18.59999999999999076, 64.35000000001251408, -178.7731074845244450 ) ) ;
#114450 = ORIENTED_EDGE ( 'NONE', *, *, #106870, .T. ) ;
#114451 = ORIENTED_EDGE ( 'NONE', *, *, #82271, .T. ) ;
#114452 = DIRECTION ( 'NONE',  ( -1.000000000000000000, -0.000000000000000000, -0.000000000000000000 ) ) ;
#114453 = CARTESIAN_POINT ( 'NONE',  ( 21.30000000000002558, 1.115650265596050101E-11, -96.45000000000003126 ) ) ;
#114454 = CARTESIAN_POINT ( 'NONE',  ( 20.94999999999999929, 1.115600667400684642E-11, -67.00000000000000000 ) ) ;
#114455 = TOROIDAL_SURFACE ( 'NONE', #93608, 11.65000000000000036, 0.1000000000000000056 ) ;
#114456 = CARTESIAN_POINT ( 'NONE',  ( -23.15000000000000213, 4.350000000011156054, -155.3500000000000227 ) ) ;
#114457 = ORIENTED_EDGE ( 'NONE', *, *, #226797, .F. ) ;
#114458 = CARTESIAN_POINT ( 'NONE',  ( -20.64999999999999858, 7.150000000011155876, -54.65000000000000568 ) ) ;
#114459 = DIRECTION ( 'NONE',  ( -0.000000000000000000, 1.000000000000000000, -0.000000000000000000 ) ) ;
#114460 = ORIENTED_EDGE ( 'NONE', *, *, #186080, .T. ) ;
#114461 = PLANE ( 'NONE',  #241174 ) ;
#114462 = ADVANCED_FACE ( 'NONE', ( #174170 ), #250882, .T. ) ;
#114463 = CIRCLE ( 'NONE', #27014, 0.1000000000000043493 ) ;
#114464 = AXIS2_PLACEMENT_3D ( 'NONE', #220710, #141178, #25106 ) ;
#114465 = ORIENTED_EDGE ( 'NONE', *, *, #159451, .F. ) ;
#114466 = CARTESIAN_POINT ( 'NONE',  ( 20.12500000000000000, 9.750000000011153745, -142.1117712821142902 ) ) ;
#114467 = EDGE_CURVE ( 'NONE', #43703, #225394, #242520, .T. ) ;
#114468 = ORIENTED_EDGE ( 'NONE', *, *, #81708, .F. ) ;
#114469 = CARTESIAN_POINT ( 'NONE',  ( -16.86133551771148831, 9.950000000011137047, -154.8013434345467090 ) ) ;
#114470 = CARTESIAN_POINT ( 'NONE',  ( 16.27683809663750125, 66.65000000001209912, -127.2731074845243597 ) ) ;
#114471 = CARTESIAN_POINT ( 'NONE',  ( -21.65000000000000213, 7.250000000011139534, -121.3500000000000369 ) ) ;
#114472 = CYLINDRICAL_SURFACE ( 'NONE', #40641, 0.1000000000000024342 ) ;
#114473 = LINE ( 'NONE', #148475, #202975 ) ;
#114474 = EDGE_CURVE ( 'NONE', #122594, #69026, #138989, .T. ) ;
#114475 = CARTESIAN_POINT ( 'NONE',  ( 21.05000000000000071, -11.29603075032412995, -170.5478991596638423 ) ) ;
#114476 = DIRECTION ( 'NONE',  ( 1.000000000000000000, 0.000000000000000000, 0.000000000000000000 ) ) ;
#114478 = CARTESIAN_POINT ( 'NONE',  ( -22.50000000000000000, 76.00000000001276135, -215.1726782920691505 ) ) ;
#114477 = CARTESIAN_POINT ( 'NONE',  ( -23.15000000000000213, 71.75000000001259082, -191.1731074845243654 ) ) ;
#114479 = FACE_OUTER_BOUND ( 'NONE', #58999, .T. ) ;
#114480 = ADVANCED_FACE ( 'NONE', ( #179290 ), #118000, .T. ) ;
#114481 = FACE_OUTER_BOUND ( 'NONE', #5047, .T. ) ;
#114482 = DIRECTION ( 'NONE',  ( -1.000000000000000000, -0.000000000000000000, 0.000000000000000000 ) ) ;
#114484 = CARTESIAN_POINT ( 'NONE',  ( -21.52071067811865746, 10.22920135959988563, -211.4116896754832169 ) ) ;
#114483 = CIRCLE ( 'NONE', #177239, 1.899999999999999023 ) ;
#114485 = ORIENTED_EDGE ( 'NONE', *, *, #211233, .T. ) ;
#114486 = TOROIDAL_SURFACE ( 'NONE', #52110, 0.2000000000000000111, 0.1000000000000000056 ) ;
#114487 = CARTESIAN_POINT ( 'NONE',  ( 20.97468175916167965, 10.62526516438217783, -79.25476143541247609 ) ) ;
#114489 = DIRECTION ( 'NONE',  ( -1.000000000000000000, 0.000000000000000000, -0.000000000000000000 ) ) ;
#114488 = AXIS2_PLACEMENT_3D ( 'NONE', #256098, #140047, #200053 ) ;
#114490 = AXIS2_PLACEMENT_3D ( 'NONE', #65763, #243112, #147883 ) ;
#114491 = EDGE_CURVE ( 'NONE', #156829, #126928, #117346, .T. ) ;
#114493 = ADVANCED_FACE ( 'NONE', ( #138805 ), #159706, .T. ) ;
#114492 = EDGE_CURVE ( 'NONE', #75549, #120323, #30071, .T. ) ;
#114494 = ORIENTED_EDGE ( 'NONE', *, *, #77880, .T. ) ;
#114495 = DIRECTION ( 'NONE',  ( 1.000000000000000000, -0.000000000000000000, -0.000000000000000000 ) ) ;
#114496 = LINE ( 'NONE', #76640, #62709 ) ;
#114497 = DIRECTION ( 'NONE',  ( 0.000000000000000000, -0.8814952561688398358, 0.4721928772777406746 ) ) ;
#114498 = ORIENTED_EDGE ( 'NONE', *, *, #160460, .F. ) ;
#114499 = LINE ( 'NONE', #231900, #201111 ) ;
#114500 = VERTEX_POINT ( 'NONE', #220935 ) ;
#114501 = CARTESIAN_POINT ( 'NONE',  ( 21.05000000000000426, 6.108305422032350052, -199.6352550756156745 ) ) ;
#114502 = DIRECTION ( 'NONE',  ( 0.000000000000000000, 0.000000000000000000, -1.000000000000000000 ) ) ;
#114503 = ADVANCED_FACE ( 'NONE', ( #20197 ), #192643, .T. ) ;
#114504 = EDGE_CURVE ( 'NONE', #61748, #90944, #22154, .T. ) ;
#114505 = VECTOR ( 'NONE', #67764, 1000.000000000000000 ) ;
#114506 = CIRCLE ( 'NONE', #2054, 12.77500000000000924 ) ;
#114507 = EDGE_LOOP ( 'NONE', ( #190026, #104801, #69434, #88655 ) ) ;
#114508 = DIRECTION ( 'NONE',  ( 2.952720810173289112E-16, 1.000000000000000000, 9.912705577010238578E-15 ) ) ;
#114509 = EDGE_CURVE ( 'NONE', #195077, #163280, #194448, .T. ) ;
#114510 = VERTEX_POINT ( 'NONE', #34107 ) ;
#114511 = DIRECTION ( 'NONE',  ( -0.000000000000000000, 6.982962677686266711E-15, -1.000000000000000000 ) ) ;
#114512 = DIRECTION ( 'NONE',  ( 0.000000000000000000, -0.7397890806274223241, -0.6728388485993012091 ) ) ;
#114514 = VECTOR ( 'NONE', #9628, 1000.000000000000000 ) ;
#114513 = LINE ( 'NONE', #173259, #65979 ) ;
#114516 = DIRECTION ( 'NONE',  ( -1.000000000000000000, -2.952720810173289112E-16, 0.000000000000000000 ) ) ;
#114515 = AXIS2_PLACEMENT_3D ( 'NONE', #208180, #11249, #177743 ) ;
#114517 = CARTESIAN_POINT ( 'NONE',  ( 18.59999999999999787, 85.40000000001137437, -29.14106563635157698 ) ) ;
#114518 = ADVANCED_FACE ( 'NONE', ( #36667 ), #174919, .F. ) ;
#114520 = CIRCLE ( 'NONE', #214467, 0.09999999999999971412 ) ;
#114519 = CARTESIAN_POINT ( 'NONE',  ( -18.40000000000000213, 11.48667500175766953, -9.250000000000001776 ) ) ;
#114521 = DIRECTION ( 'NONE',  ( -1.000000000000000000, -0.000000000000000000, -0.000000000000000000 ) ) ;
#114522 = DIRECTION ( 'NONE',  ( 0.000000000000000000, 0.000000000000000000, 1.000000000000000000 ) ) ;
#114525 = ORIENTED_EDGE ( 'NONE', *, *, #172195, .F. ) ;
#114524 = EDGE_CURVE ( 'NONE', #6496, #203964, #101183, .T. ) ;
#114523 = CARTESIAN_POINT ( 'NONE',  ( 21.05000000000000071, 69.74115287693277310, -103.0548658375798965 ) ) ;
#114526 = VERTEX_POINT ( 'NONE', #75771 ) ;
#114528 = DIRECTION ( 'NONE',  ( 0.000000000000000000, 0.000000000000000000, -1.000000000000000000 ) ) ;
#114527 = CARTESIAN_POINT ( 'NONE',  ( -23.15000000000000213, 46.10080905699345521, -240.6643289267983334 ) ) ;
#114529 = ORIENTED_EDGE ( 'NONE', *, *, #158121, .F. ) ;
#114531 = ORIENTED_EDGE ( 'NONE', *, *, #98695, .T. ) ;
#114530 = LINE ( 'NONE', #91111, #206827 ) ;
#114532 = ORIENTED_EDGE ( 'NONE', *, *, #4078, .T. ) ;
#114533 = CARTESIAN_POINT ( 'NONE',  ( 21.14999999999999858, 21.06723286205836487, -233.6551206055687260 ) ) ;
#114534 = CARTESIAN_POINT ( 'NONE',  ( 20.13684514579856000, 9.495855392757592384, -175.6430316856907723 ) ) ;
#114535 = AXIS2_PLACEMENT_3D ( 'NONE', #37318, #179395, #238056 ) ;
#114536 = COLOUR_RGB ( '', 0.08235294, 0.09019608, 0.10196078) ;
#114537 = LINE ( 'NONE', #213628, #113142 ) ;
#114538 = CARTESIAN_POINT ( 'NONE',  ( 18.43579564894469769, -9.519327535292646303, -6.972976643860169688 ) ) ;
#114539 = DIRECTION ( 'NONE',  ( 3.469446951953150970E-14, 0.3042567129660163627, 0.9525900758537824142 ) ) ;
#114540 = EDGE_CURVE ( 'NONE', #115854, #73802, #14531, .T. ) ;
#114541 = CIRCLE ( 'NONE', #156263, 0.1000000000000017958 ) ;
#114542 = CARTESIAN_POINT ( 'NONE',  ( -20.94999999999994600, 65.35000000001120668, -4.523107484524794053 ) ) ;
#114543 = AXIS2_PLACEMENT_3D ( 'NONE', #157562, #54559, #94969 ) ;
#114544 = CYLINDRICAL_SURFACE ( 'NONE', #36126, 7.900000000000003908 ) ;
#114545 = CYLINDRICAL_SURFACE ( 'NONE', #51978, 0.09999999999999939493 ) ;
#114546 = EDGE_CURVE ( 'NONE', #115618, #29625, #151466, .T. ) ;
#114547 = VERTEX_POINT ( 'NONE', #134423 ) ;
#114548 = ORIENTED_EDGE ( 'NONE', *, *, #80936, .F. ) ;
#114549 = DIRECTION ( 'NONE',  ( 0.000000000000000000, 0.000000000000000000, -1.000000000000000000 ) ) ;
#114550 = VERTEX_POINT ( 'NONE', #251824 ) ;
#114551 = DIRECTION ( 'NONE',  ( 0.000000000000000000, 0.9651348961777161950, -0.2617529984165014589 ) ) ;
#114552 = VERTEX_POINT ( 'NONE', #96578 ) ;
#114553 = CARTESIAN_POINT ( 'NONE',  ( 22.48970261584622321, 11.65000000001115588, -33.44463051178259860 ) ) ;
#114554 = DIRECTION ( 'NONE',  ( 1.000000000000000000, 0.000000000000000000, 0.000000000000000000 ) ) ;
#114555 = CARTESIAN_POINT ( 'NONE',  ( -18.59999999999999787, 79.24821784679178904, -196.3217825494968736 ) ) ;
#114556 = EDGE_CURVE ( 'NONE', #108264, #187685, #242693, .T. ) ;
#114558 = EDGE_LOOP ( 'NONE', ( #78660, #107589, #107265, #253831 ) ) ;
#114557 = CARTESIAN_POINT ( 'NONE',  ( -21.22070241538126112, 6.469946272880768845, -33.40108096946497795 ) ) ;
#114559 = CARTESIAN_POINT ( 'NONE',  ( 20.85000000000000142, 0.1610488207298751417, -66.71581015563977246 ) ) ;
#114560 = VERTEX_POINT ( 'NONE', #215271 ) ;
#114561 = CARTESIAN_POINT ( 'NONE',  ( 23.24999999999999645, 73.97321671803808840, -202.9734261878502366 ) ) ;
#114562 = AXIS2_PLACEMENT_3D ( 'NONE', #132496, #215858, #212049 ) ;
#114563 = CARTESIAN_POINT ( 'NONE',  ( -20.64999999999999858, 4.350000000011156054, -155.1500000000000057 ) ) ;
#114564 = CARTESIAN_POINT ( 'NONE',  ( 20.85000000000000142, 6.933893972137497030, -104.2856458343736250 ) ) ;
#114565 = VECTOR ( 'NONE', #119716, 1000.000000000000114 ) ;
#114566 = CARTESIAN_POINT ( 'NONE',  ( -18.59999999999999787, 5.900000000011102586, -144.2190997646564483 ) ) ;
#114567 = FACE_OUTER_BOUND ( 'NONE', #59069, .T. ) ;
#114568 = AXIS2_PLACEMENT_3D ( 'NONE', #240931, #183523, #144355 ) ;
#114569 = ORIENTED_EDGE ( 'NONE', *, *, #141546, .T. ) ;
#114571 = CARTESIAN_POINT ( 'NONE',  ( 23.14999999999998437, 68.29137419664525055, -231.9463301769586394 ) ) ;
#114570 = CARTESIAN_POINT ( 'NONE',  ( -21.07016717456945543, 6.320940838111416049, -134.0000000000000000 ) ) ;
#114572 = ORIENTED_EDGE ( 'NONE', *, *, #11974, .T. ) ;
#114575 = VERTEX_POINT ( 'NONE', #155331 ) ;
#114574 = DIRECTION ( 'NONE',  ( -1.000000000000000000, 0.000000000000000000, 0.000000000000000000 ) ) ;
#114573 = CARTESIAN_POINT ( 'NONE',  ( -20.85000000000000142, 77.83585931145526615, -57.91866831572577468 ) ) ;
#114576 = CARTESIAN_POINT ( 'NONE',  ( -20.94999999999999929, 1.835341550224413698, -11.55515129256298401 ) ) ;
#114577 = CIRCLE ( 'NONE', #10530, 0.1000000000000028644 ) ;
#114578 = B_SPLINE_CURVE_WITH_KNOTS ( 'NONE', 3,
 ( #210742, #114208, #249868, #90776, #192466, #229033, #169089, #93353, #111640, #232900, #54222, #133765, #213296 ),
 .UNSPECIFIED., .F., .F.,
 ( 4, 3, 3, 3, 4 ),
 ( 1.075528555105620399E-16, 1.946463881814325270E-05, 3.922356109943460204E-05, 4.215060953239334383E-05, 4.415117091092807429E-05 ),
 .UNSPECIFIED. ) ;
#114579 = DIRECTION ( 'NONE',  ( -0.000000000000000000, -0.000000000000000000, 1.000000000000000000 ) ) ;
#114580 = CIRCLE ( 'NONE', #160577, 0.1000000000000028644 ) ;
#114581 = ORIENTED_EDGE ( 'NONE', *, *, #195990, .T. ) ;
#114582 = DIRECTION ( 'NONE',  ( -0.000000000000000000, 0.9770955615653313941, 0.2128009952263603954 ) ) ;
#114583 = CYLINDRICAL_SURFACE ( 'NONE', #219656, 1.500000000000001332 ) ;
#114584 = LINE ( 'NONE', #59712, #80115 ) ;
#114586 = ORIENTED_EDGE ( 'NONE', *, *, #96490, .F. ) ;
#114585 = CARTESIAN_POINT ( 'NONE',  ( 20.94999999999999574, 72.02722222756958104, -225.1832529173024398 ) ) ;
#114587 = CIRCLE ( 'NONE', #131141, 4.149999999999999467 ) ;
#114588 = AXIS2_PLACEMENT_3D ( 'NONE', #248980, #191593, #132881 ) ;
#114589 = EDGE_LOOP ( 'NONE', ( #167193, #174265, #143335, #6474 ) ) ;
#114590 = CARTESIAN_POINT ( 'NONE',  ( -20.85000000000000142, -0.3238857010591806307, -66.95758958931398297 ) ) ;
#114591 = CARTESIAN_POINT ( 'NONE',  ( 18.43473516226068298, -9.494942282747077300, -74.04589868334953451 ) ) ;
#114592 = CARTESIAN_POINT ( 'NONE',  ( -16.81744102076749314, 44.13548170601895038, -235.2989316066074821 ) ) ;
#114593 = DIRECTION ( 'NONE',  ( 1.000000000000000000, 0.000000000000000000, 0.000000000000000000 ) ) ;
#114594 = ORIENTED_EDGE ( 'NONE', *, *, #216011, .T. ) ;
#114595 = CARTESIAN_POINT ( 'NONE',  ( -23.25000000000000000, 4.768403829798271154, -213.4961173936592331 ) ) ;
#114596 = CARTESIAN_POINT ( 'NONE',  ( -0.8999999999999993561, -8.279289321881350361, 26.00000000000000355 ) ) ;
#114597 = DIRECTION ( 'NONE',  ( -6.938893903907224433E-15, 1.000000000000000000, 0.000000000000000000 ) ) ;
#114598 = AXIS2_PLACEMENT_3D ( 'NONE', #151835, #172707, #252178 ) ;
#114599 = ORIENTED_EDGE ( 'NONE', *, *, #134920, .F. ) ;
#114600 = CARTESIAN_POINT ( 'NONE',  ( 18.59999999999999076, 68.48451787451661232, -224.2224406095231757 ) ) ;
#114601 = DIRECTION ( 'NONE',  ( 0.000000000000000000, -0.9126074666063770380, -0.4088369013363281068 ) ) ;
#114602 = EDGE_CURVE ( 'NONE', #150108, #15934, #234837, .T. ) ;
#114603 = ORIENTED_EDGE ( 'NONE', *, *, #237494, .F. ) ;
#114604 = DIRECTION ( 'NONE',  ( 0.000000000000000000, 0.9126074666063769270, 0.4088369013363282733 ) ) ;
#114605 = CARTESIAN_POINT ( 'NONE',  ( -23.15000000000000213, 76.00000000001179501, -82.39810748452430289 ) ) ;
#114606 = FACE_OUTER_BOUND ( 'NONE', #48282, .T. ) ;
#114607 = CIRCLE ( 'NONE', #64528, 11.65000000000000036 ) ;
#114608 = ORIENTED_EDGE ( 'NONE', *, *, #234616, .T. ) ;
#114609 = AXIS2_PLACEMENT_3D ( 'NONE', #82714, #183153, #21516 ) ;
#114610 = ORIENTED_EDGE ( 'NONE', *, *, #175092, .T. ) ;
#114611 = CARTESIAN_POINT ( 'NONE',  ( -23.25000000000000000, 10.69888912757691024, -235.6450824654141059 ) ) ;
#114612 = ORIENTED_EDGE ( 'NONE', *, *, #176470, .F. ) ;
#114614 = VERTEX_POINT ( 'NONE', #135718 ) ;
#114613 = FACE_OUTER_BOUND ( 'NONE', #162120, .T. ) ;
#114615 = EDGE_CURVE ( 'NONE', #72909, #168030, #71922, .T. ) ;
#114618 = ORIENTED_EDGE ( 'NONE', *, *, #145239, .T. ) ;
#114617 = EDGE_LOOP ( 'NONE', ( #169561, #138401, #217336, #17426 ) ) ;
#114616 = CARTESIAN_POINT ( 'NONE',  ( 21.30000000000002558, 1.115600667400684642E-11, -37.54999999999999716 ) ) ;
#114619 = DIRECTION ( 'NONE',  ( 1.000000000000000000, 0.000000000000000000, -0.000000000000000000 ) ) ;
#114620 = CARTESIAN_POINT ( 'NONE',  ( -16.88705144915432754, 12.47382595179198184, -211.5174318890890390 ) ) ;
#114621 = DIRECTION ( 'NONE',  ( 0.000000000000000000, 1.000000000000000000, 6.853228547068871147E-15 ) ) ;
#114622 = AXIS2_PLACEMENT_3D ( 'NONE', #91901, #231439, #171484 ) ;
#114623 = DIRECTION ( 'NONE',  ( -1.000000000000000000, 7.304098846218134667E-16, -4.217023435051678980E-16 ) ) ;
#114624 = CARTESIAN_POINT ( 'NONE',  ( -18.50000000000000000, -0.8760381862371811046, -190.6771195118613207 ) ) ;
#114625 = DIRECTION ( 'NONE',  ( -1.000000000000000000, -0.000000000000000000, -0.000000000000000000 ) ) ;
#114626 = ORIENTED_EDGE ( 'NONE', *, *, #35219, .F. ) ;
#114627 = ORIENTED_EDGE ( 'NONE', *, *, #59368, .T. ) ;
#114628 = ORIENTED_EDGE ( 'NONE', *, *, #82052, .T. ) ;
#114629 = ADVANCED_FACE ( 'NONE', ( #52320 ), #176168, .F. ) ;
#114630 = DIRECTION ( 'NONE',  ( -1.000000000000000000, 0.000000000000000000, 0.000000000000000000 ) ) ;
#114633 = ORIENTED_EDGE ( 'NONE', *, *, #35281, .T. ) ;
#114632 = EDGE_CURVE ( 'NONE', #47348, #28076, #255628, .T. ) ;
#114631 = CARTESIAN_POINT ( 'NONE',  ( -16.94445028196807002, 66.00793639031481064, -182.6304376629428816 ) ) ;
#114634 = FACE_OUTER_BOUND ( 'NONE', #210527, .T. ) ;
#114635 = EDGE_LOOP ( 'NONE', ( #14853, #227191 ) ) ;
#114636 = CARTESIAN_POINT ( 'NONE',  ( 22.47071067811865319, 75.90090754530910999, -77.24318222902238062 ) ) ;
#114637 = VERTEX_POINT ( 'NONE', #152763 ) ;
#114638 = CARTESIAN_POINT ( 'NONE',  ( -18.39999999999999858, 64.52132590001336609, -194.2484142681837795 ) ) ;
#114639 = EDGE_CURVE ( 'NONE', #176065, #107411, #114083, .T. ) ;
#114640 = ORIENTED_EDGE ( 'NONE', *, *, #164686, .T. ) ;
#114641 = ADVANCED_FACE ( 'NONE', ( #13236 ), #92741, .T. ) ;
#114642 = DIRECTION ( 'NONE',  ( 0.000000000000000000, -0.000000000000000000, -1.000000000000000000 ) ) ;
#114643 = LINE ( 'NONE', #134193, #69530 ) ;
#114646 = ORIENTED_EDGE ( 'NONE', *, *, #137362, .T. ) ;
#114645 = ORIENTED_EDGE ( 'NONE', *, *, #59673, .F. ) ;
#114644 = AXIS2_PLACEMENT_3D ( 'NONE', #157294, #116857, #158578 ) ;
#114647 = AXIS2_PLACEMENT_3D ( 'NONE', #67608, #66338, #168042 ) ;
#114648 = ORIENTED_EDGE ( 'NONE', *, *, #77318, .F. ) ;
#114649 = LINE ( 'NONE', #174678, #45050 ) ;
#114651 = ORIENTED_EDGE ( 'NONE', *, *, #233988, .T. ) ;
#114650 = EDGE_CURVE ( 'NONE', #162266, #44866, #176479, .T. ) ;
#114652 = ORIENTED_EDGE ( 'NONE', *, *, #123182, .T. ) ;
#114653 = CARTESIAN_POINT ( 'NONE',  ( -20.94999999999999929, -1.362429037182149694, -141.8888812479212334 ) ) ;
#114655 = VERTEX_POINT ( 'NONE', #83428 ) ;
#114654 = CARTESIAN_POINT ( 'NONE',  ( 18.43630871534874416, -9.679800874791798293, -107.1606320679841247 ) ) ;
#114656 = DIRECTION ( 'NONE',  ( 0.000000000000000000, 0.2128009952263605897, -0.9770955615653315052 ) ) ;
#114658 = DIRECTION ( 'NONE',  ( 0.000000000000000000, -1.000000000000000000, -0.000000000000000000 ) ) ;
#114657 = DIRECTION ( 'NONE',  ( 0.000000000000000000, 0.000000000000000000, 1.000000000000000000 ) ) ;
#114659 = CARTESIAN_POINT ( 'NONE',  ( -20.64999999999999858, 6.878457983866232972, -212.1414458560986986 ) ) ;
#114660 = CARTESIAN_POINT ( 'NONE',  ( 18.44364597020194552, -9.490487317151101720, -74.05797788968389739 ) ) ;
#114661 = CARTESIAN_POINT ( 'NONE',  ( 21.05000000000000071, 85.00000000001261924, -193.6291383618718385 ) ) ;
#114662 = ORIENTED_EDGE ( 'NONE', *, *, #71559, .F. ) ;
#114664 = EDGE_CURVE ( 'NONE', #233248, #116470, #76103, .T. ) ;
#114663 = ORIENTED_EDGE ( 'NONE', *, *, #63221, .F. ) ;
#114665 = FACE_OUTER_BOUND ( 'NONE', #18558, .T. ) ;
#114666 = CARTESIAN_POINT ( 'NONE',  ( -21.05000000000000426, 76.02103547655231353, -142.8275633064719443 ) ) ;
#114667 = DIRECTION ( 'NONE',  ( -1.000000000000000000, -0.000000000000000000, -0.000000000000000000 ) ) ;
#114668 = AXIS2_PLACEMENT_3D ( 'NONE', #186479, #66531, #126495 ) ;
#114669 = ORIENTED_EDGE ( 'NONE', *, *, #180172, .T. ) ;
#114670 = CARTESIAN_POINT ( 'NONE',  ( 20.94999999999999929, 5.000000000011153745, -188.5947339810868755 ) ) ;
#114671 = VECTOR ( 'NONE', #185098, 1000.000000000000000 ) ;
#114672 = CIRCLE ( 'NONE', #73196, 0.1000000000000002554 ) ;
#114673 = CIRCLE ( 'NONE', #231218, 0.1999999999999987899 ) ;
#114674 = CARTESIAN_POINT ( 'NONE',  ( -16.93234230245721861, 51.66096952035064049, -231.8748915850824801 ) ) ;
#114675 = DIRECTION ( 'NONE',  ( 0.000000000000000000, 2.168404344970946942E-15, 1.000000000000000000 ) ) ;
#114676 = EDGE_LOOP ( 'NONE', ( #42814, #220346, #125137, #8732 ) ) ;
#114677 = ORIENTED_EDGE ( 'NONE', *, *, #149871, .F. ) ;
#114678 = CARTESIAN_POINT ( 'NONE',  ( -21.65000000000000213, 7.708578643773852157, -188.6499999999999488 ) ) ;
#114679 = CARTESIAN_POINT ( 'NONE',  ( 18.39999999999999503, 5.650000000011139001, -54.35000000000000142 ) ) ;
#114680 = ORIENTED_EDGE ( 'NONE', *, *, #183746, .F. ) ;
#114681 = CARTESIAN_POINT ( 'NONE',  ( -23.15000000000000213, 31.49702336731128582, -233.4564499823349877 ) ) ;
#114682 = ORIENTED_EDGE ( 'NONE', *, *, #172152, .T. ) ;
#114683 = CARTESIAN_POINT ( 'NONE',  ( 18.33996824403501691, -9.569639859420098205, -140.8190656375171272 ) ) ;
#114684 = DIRECTION ( 'NONE',  ( -1.000000000000000000, -0.000000000000000000, -0.000000000000000000 ) ) ;
#114686 = CARTESIAN_POINT ( 'NONE',  ( -21.05000000000000071, -1.476139073305543281, -194.6920926048172191 ) ) ;
#114685 = DIRECTION ( 'NONE',  ( 0.000000000000000000, 0.000000000000000000, 1.000000000000000000 ) ) ;
#114687 = CARTESIAN_POINT ( 'NONE',  ( 18.51697539158856642, 65.68434038414410736, -164.4866880726065972 ) ) ;
#114688 = CARTESIAN_POINT ( 'NONE',  ( 21.05563370358598263, 65.27576964416535077, -90.84001666856131862 ) ) ;
#114689 = CARTESIAN_POINT ( 'NONE',  ( -23.15000000000000213, 11.65000000001115588, -112.6500000000000341 ) ) ;
#114690 = CIRCLE ( 'NONE', #10465, 0.1000000000000028644 ) ;
#114691 = VECTOR ( 'NONE', #15572, 1000.000000000000000 ) ;
#114692 = ADVANCED_FACE ( 'NONE', ( #221667 ), #256479, .T. ) ;
#114694 = ORIENTED_EDGE ( 'NONE', *, *, #80845, .T. ) ;
#114693 = EDGE_LOOP ( 'NONE', ( #1022, #12387, #94812, #232950 ) ) ;
#114695 = EDGE_LOOP ( 'NONE', ( #158689, #70405, #207315, #87167 ) ) ;
#114696 = AXIS2_PLACEMENT_3D ( 'NONE', #158780, #217418, #101284 ) ;
#114697 = DIRECTION ( 'NONE',  ( 0.000000000000000000, 0.000000000000000000, -1.000000000000000000 ) ) ;
#114698 = CYLINDRICAL_SURFACE ( 'NONE', #144854, 0.09999999999999976963 ) ;
#114699 = CARTESIAN_POINT ( 'NONE',  ( -21.14999999999999858, 1.115600667400684642E-11, -33.50000000000000000 ) ) ;
#114700 = EDGE_CURVE ( 'NONE', #25805, #87941, #220419, .T. ) ;
#114701 = EDGE_CURVE ( 'NONE', #194619, #196891, #105289, .T. ) ;
#114703 = CARTESIAN_POINT ( 'NONE',  ( -13.88555196119803270, 66.54256847116292306, -88.02319054662470421 ) ) ;
#114702 = FACE_OUTER_BOUND ( 'NONE', #7415, .T. ) ;
#114704 = ORIENTED_EDGE ( 'NONE', *, *, #133098, .F. ) ;
#114705 = TOROIDAL_SURFACE ( 'NONE', #77098, 11.65000000000000036, 0.1000000000000000056 ) ;
#114706 = FACE_OUTER_BOUND ( 'NONE', #122179, .T. ) ;
#114707 = AXIS2_PLACEMENT_3D ( 'NONE', #131180, #17363, #52929 ) ;
#114708 = CIRCLE ( 'NONE', #147852, 11.90000000000001457 ) ;
#114709 = ORIENTED_EDGE ( 'NONE', *, *, #223994, .T. ) ;
#114710 = ORIENTED_EDGE ( 'NONE', *, *, #5873, .F. ) ;
#114711 = CARTESIAN_POINT ( 'NONE',  ( -21.09107601085561257, 69.63612202465148471, -69.56241464924151785 ) ) ;
#114712 = CARTESIAN_POINT ( 'NONE',  ( -22.41119224318417125, 1.115600667400684642E-11, -88.85042919245522341 ) ) ;
#114713 = EDGE_CURVE ( 'NONE', #170518, #20030, #122608, .T. ) ;
#114714 = DIRECTION ( 'NONE',  ( -1.000000000000000000, 0.000000000000000000, 0.000000000000000000 ) ) ;
#114715 = EDGE_CURVE ( 'NONE', #217175, #22291, #63, .T. ) ;
#114716 = EDGE_CURVE ( 'NONE', #209604, #233466, #38702, .T. ) ;
#114718 = DIRECTION ( 'NONE',  ( -0.000000000000000000, -0.9651348961777157509, 0.2617529984165031243 ) ) ;
#114717 = B_SPLINE_CURVE_WITH_KNOTS ( 'NONE', 3,
 ( #224717, #87769, #146461, #245591, #65654, #167358, #89061, #86476, #246852, #68231, #166081, #147776, #227296, #104749, #48656, #106042, #128210, #209026, #10830 ),
 .UNSPECIFIED., .F., .F.,
 ( 4, 3, 3, 3, 3, 3, 4 ),
 ( 0.000000000000000000, 1.655171619026003227E-05, 2.773500582848852791E-05, 5.941817267378676065E-05, 0.0001114174635873525684, 0.0001914169455916370536, 0.0002627181070750628472 ),
 .UNSPECIFIED. ) ;
#114719 = VECTOR ( 'NONE', #244168, 1000.000000000000000 ) ;
#114720 = CARTESIAN_POINT ( 'NONE',  ( -21.05000000000000071, -11.48912529306490349, -103.4000000000000341 ) ) ;
#114721 = ORIENTED_EDGE ( 'NONE', *, *, #151213, .F. ) ;
#114722 = ORIENTED_EDGE ( 'NONE', *, *, #97584, .F. ) ;
#114723 = AXIS2_PLACEMENT_3D ( 'NONE', #179111, #177815, #218170 ) ;
#114724 = DIRECTION ( 'NONE',  ( 0.000000000000000000, 0.000000000000000000, -1.000000000000000000 ) ) ;
#114725 = EDGE_CURVE ( 'NONE', #50639, #12116, #1261, .T. ) ;
#114726 = CARTESIAN_POINT ( 'NONE',  ( -21.65000000000000213, 7.708578643762696636, -21.15000000000000213 ) ) ;
#114727 = DIRECTION ( 'NONE',  ( 0.000000000000000000, -0.8660254037844377084, -0.5000000000000016653 ) ) ;
#114728 = CYLINDRICAL_SURFACE ( 'NONE', #131926, 0.1000000000000028644 ) ;
#114729 = AXIS2_PLACEMENT_3D ( 'NONE', #34989, #37528, #77908 ) ;
#114730 = CARTESIAN_POINT ( 'NONE',  ( 0.9000000000000547562, 64.25000000001119815, -7.323107484524790323 ) ) ;
#114731 = AXIS2_PLACEMENT_3D ( 'NONE', #34719, #115501, #17681 ) ;
#114732 = CYLINDRICAL_SURFACE ( 'NONE', #25808, 0.5000000000000004441 ) ;
#114733 = LINE ( 'NONE', #135559, #4263 ) ;
#114734 = EDGE_CURVE ( 'NONE', #240059, #119449, #97855, .T. ) ;
#114736 = DIRECTION ( 'NONE',  ( 0.000000000000000000, 0.000000000000000000, -1.000000000000000000 ) ) ;
#114735 = DIRECTION ( 'NONE',  ( 0.000000000000000000, 0.000000000000000000, 1.000000000000000000 ) ) ;
#114737 = DIRECTION ( 'NONE',  ( 1.000000000000000000, 0.000000000000000000, 0.000000000000000000 ) ) ;
#114738 = FACE_OUTER_BOUND ( 'NONE', #86259, .T. ) ;
#114739 = DIRECTION ( 'NONE',  ( -1.000000000000000000, 0.000000000000000000, 0.000000000000000000 ) ) ;
#114740 = DIRECTION ( 'NONE',  ( 0.000000000000000000, -0.000000000000000000, -1.000000000000000000 ) ) ;
#114741 = EDGE_CURVE ( 'NONE', #24761, #227999, #58733, .T. ) ;
#114743 = EDGE_LOOP ( 'NONE', ( #242753, #212102, #59035, #124079 ) ) ;
#114742 = CARTESIAN_POINT ( 'NONE',  ( 19.97071067811863898, 54.41629874617179041, -228.7529758933203539 ) ) ;
#114744 = ADVANCED_FACE ( 'NONE', ( #198266, #138277, #217813 ), #256912, .T. ) ;
#114745 = DIRECTION ( 'NONE',  ( -3.469446951953515108E-14, -1.000000000000000000, 0.000000000000000000 ) ) ;
#114746 = ORIENTED_EDGE ( 'NONE', *, *, #12791, .F. ) ;
#114747 = EDGE_CURVE ( 'NONE', #248444, #203718, #61334, .T. ) ;
#114748 = ADVANCED_FACE ( 'NONE', ( #180012 ), #204673, .T. ) ;
#114750 = AXIS2_PLACEMENT_3D ( 'NONE', #213980, #233554, #152751 ) ;
#114749 = DIRECTION ( 'NONE',  ( -1.000000000000000000, 7.304098846218135653E-16, 0.000000000000000000 ) ) ;
#114751 = TOROIDAL_SURFACE ( 'NONE', #64665, 0.2000000000000000111, 0.1000000000000000056 ) ;
#114752 = DIRECTION ( 'NONE',  ( 1.000000000000000000, 0.000000000000000000, -0.000000000000000000 ) ) ;
#114753 = TOROIDAL_SURFACE ( 'NONE', #2293, 0.2000000000000000111, 0.1000000000000000056 ) ;
#114754 = CARTESIAN_POINT ( 'NONE',  ( 15.51872946208854920, 9.376580978055097049, -84.62694624701198620 ) ) ;
#114755 = CARTESIAN_POINT ( 'NONE',  ( 22.39999999999999503, 1.115600667400684642E-11, -21.85042919245520210 ) ) ;
#114756 = DIRECTION ( 'NONE',  ( 0.000000000000000000, -0.2128009952263603677, 0.9770955615653313941 ) ) ;
#114757 = CARTESIAN_POINT ( 'NONE',  ( 18.49999999999999289, 10.23906162412143672, -24.75439743459708808 ) ) ;
#114758 = LINE ( 'NONE', #110902, #177736 ) ;
#114759 = TOROIDAL_SURFACE ( 'NONE', #85482, 11.90000000000000391, 0.1000000000000000056 ) ;
#114760 = EDGE_LOOP ( 'NONE', ( #62272, #28269, #213411, #30557 ) ) ;
#114761 = DIRECTION ( 'NONE',  ( 0.000000000000000000, 3.552713678800407449E-15, -1.000000000000000000 ) ) ;
#114763 = EDGE_LOOP ( 'NONE', ( #254451, #156229, #29545, #130042, #111302, #162113, #106806, #172734, #219482, #164283, #234253, #210480, #117246, #178348, #9103, #185523, #102313, #104807, #106202, #229439, #63407, #40873, #183193 ) ) ;
#114762 = FACE_OUTER_BOUND ( 'NONE', #47445, .T. ) ;
#114764 = DIRECTION ( 'NONE',  ( -4.801466763864313332E-15, -0.2605042016806672911, -0.9654727137038716656 ) ) ;
#114765 = DIRECTION ( 'NONE',  ( 0.000000000000000000, 0.2617529984165152257, 0.9651348961777124202 ) ) ;
#114766 = CARTESIAN_POINT ( 'NONE',  ( -22.50000000000000000, 31.82071903192811746, -238.9531407059545813 ) ) ;
#114767 = AXIS2_PLACEMENT_3D ( 'NONE', #51132, #12060, #190705 ) ;
#114768 = ORIENTED_EDGE ( 'NONE', *, *, #194260, .F. ) ;
#114769 = CARTESIAN_POINT ( 'NONE',  ( -21.14999999999999858, -11.74999999998884448, -33.50000000000000000 ) ) ;
#114770 = AXIS2_PLACEMENT_3D ( 'NONE', #96094, #214770, #77817 ) ;
#114771 = PRODUCT_CONTEXT ( 'NONE', #70691, 'mechanical' ) ;
#114772 = CARTESIAN_POINT ( 'NONE',  ( 18.59999999999999076, 69.01799029515494510, -32.32695536626807353 ) ) ;
#114773 = DIRECTION ( 'NONE',  ( 0.000000000000000000, -1.000000000000000000, 0.000000000000000000 ) ) ;
#114774 = AXIS2_PLACEMENT_3D ( 'NONE', #221520, #63751, #184990 ) ;
#114775 = VERTEX_POINT ( 'NONE', #164297 ) ;
#114776 = DIRECTION ( 'NONE',  ( 0.000000000000000000, -1.000000000000000000, 0.000000000000000000 ) ) ;
#114777 = LINE ( 'NONE', #36558, #67406 ) ;
#114778 = CARTESIAN_POINT ( 'NONE',  ( -22.59999999999999787, 75.89914163091332000, -114.7726746080137019 ) ) ;
#114779 = ORIENTED_EDGE ( 'NONE', *, *, #79029, .T. ) ;
#114780 = AXIS2_PLACEMENT_3D ( 'NONE', #44394, #198634, #194815 ) ;
#114781 = ORIENTED_EDGE ( 'NONE', *, *, #123759, .T. ) ;
#114782 = CARTESIAN_POINT ( 'NONE',  ( -18.50000000000000000, 14.76289716703255728, -235.7888246855571026 ) ) ;
#114783 = DIRECTION ( 'NONE',  ( -0.000000000000000000, -0.1575546449569685259, 0.9875102702516485031 ) ) ;
#114784 = DIRECTION ( 'NONE',  ( -0.000000000000000000, -1.000000000000000000, -6.982962677686266711E-15 ) ) ;
#114785 = ADVANCED_FACE ( 'NONE', ( #65172 ), #123885, .F. ) ;
#114786 = CARTESIAN_POINT ( 'NONE',  ( -22.16821283564876666, 68.44102665923117002, -103.0231074845243739 ) ) ;
#114788 = DIRECTION ( 'NONE',  ( 0.000000000000000000, -1.000000000000000000, 0.000000000000000000 ) ) ;
#114787 = CARTESIAN_POINT ( 'NONE',  ( 21.05000000000000071, -1.489567864901282235, -194.6304332222954372 ) ) ;
#114789 = FACE_OUTER_BOUND ( 'NONE', #146657, .T. ) ;
#114790 = EDGE_CURVE ( 'NONE', #75757, #116101, #66468, .T. ) ;
#114791 = DIRECTION ( 'NONE',  ( 0.000000000000000000, 0.4999999999999929501, 0.8660254037844427044 ) ) ;
#114792 = CARTESIAN_POINT ( 'NONE',  ( 18.53317502108576420, 65.67736539654895012, -30.46251168765719797 ) ) ;
#114793 = CARTESIAN_POINT ( 'NONE',  ( -23.15000000000000213, 76.00000000001190870, -103.0231074845243029 ) ) ;
#114794 = AXIS2_PLACEMENT_3D ( 'NONE', #106058, #68252, #147794 ) ;
#114795 = ORIENTED_EDGE ( 'NONE', *, *, #69913, .F. ) ;
#114796 = AXIS2_PLACEMENT_3D ( 'NONE', #156716, #61434, #58833 ) ;
#114797 = ORIENTED_EDGE ( 'NONE', *, *, #139284, .T. ) ;
#114798 = CIRCLE ( 'NONE', #2342, 1.900000000000012790 ) ;
#114799 = DIRECTION ( 'NONE',  ( -1.000000000000000000, -3.469446951953635015E-14, -2.422701857770461054E-28 ) ) ;
#114800 = CARTESIAN_POINT ( 'NONE',  ( 21.05000000000000071, 1.115649653272650466E-11, -130.0000000000000284 ) ) ;
#114802 = DIRECTION ( 'NONE',  ( 3.469446951953515108E-14, -1.000000000000000000, 0.000000000000000000 ) ) ;
#114801 = CARTESIAN_POINT ( 'NONE',  ( -20.54999999999999716, 65.86663596189677605, -213.5709895136416776 ) ) ;
#114803 = ADVANCED_FACE ( 'NONE', ( #168182 ), #165583, .T. ) ;
#114804 = ADVANCED_FACE ( 'NONE', ( #183843 ), #149878, .F. ) ;
#114805 = FACE_OUTER_BOUND ( 'NONE', #249747, .T. ) ;
#114806 = CARTESIAN_POINT ( 'NONE',  ( 21.05000000000000071, 42.98415524044398950, -233.9519173640447889 ) ) ;
#114807 = CARTESIAN_POINT ( 'NONE',  ( 13.77030915526558275, 13.17382239637293040, -217.0529139566851597 ) ) ;
#114808 = ORIENTED_EDGE ( 'NONE', *, *, #249144, .T. ) ;
#114809 = ORIENTED_EDGE ( 'NONE', *, *, #251342, .F. ) ;
#114810 = FACE_OUTER_BOUND ( 'NONE', #62318, .T. ) ;
#114811 = ORIENTED_EDGE ( 'NONE', *, *, #112659, .F. ) ;
#114812 = DIRECTION ( 'NONE',  ( 0.000000000000000000, -0.9915357197604804940, 0.1298341882520397950 ) ) ;
#114813 = AXIS2_PLACEMENT_3D ( 'NONE', #118897, #39374, #155479 ) ;
#114814 = DIRECTION ( 'NONE',  ( 4.377807931758639578E-15, -0.2605042016806606298, -0.9654727137038736640 ) ) ;
#114815 = EDGE_CURVE ( 'NONE', #12728, #241189, #9654, .T. ) ;
#114816 = CARTESIAN_POINT ( 'NONE',  ( 20.95512820512820440, 8.876151316299273120, -142.5586289951409640 ) ) ;
#114817 = ORIENTED_EDGE ( 'NONE', *, *, #13962, .F. ) ;
#114818 = CARTESIAN_POINT ( 'NONE',  ( 18.59999999999998721, 48.66983769917126779, -228.4584249288054423 ) ) ;
#114819 = CARTESIAN_POINT ( 'NONE',  ( -22.57320508075687115, 31.89597452117654086, -238.9192857152811484 ) ) ;
#114820 = CARTESIAN_POINT ( 'NONE',  ( -23.25000000000000000, 1.115600667400684642E-11, -137.9000000000000341 ) ) ;
#114821 = CARTESIAN_POINT ( 'NONE',  ( 20.94999999999999929, 76.00000000001142553, -36.02310748452432421 ) ) ;
#114822 = DIRECTION ( 'NONE',  ( 1.000000000000000000, 0.000000000000000000, 0.000000000000000000 ) ) ;
#114823 = CARTESIAN_POINT ( 'NONE',  ( 21.05000000000000071, 65.53249566929501668, -241.9221741022459469 ) ) ;
#114824 = EDGE_CURVE ( 'NONE', #176884, #33376, #246970, .T. ) ;
#114826 = CARTESIAN_POINT ( 'NONE',  ( -20.85000000000000142, 77.83585931145498193, -24.51866831572578320 ) ) ;
#114825 = CARTESIAN_POINT ( 'NONE',  ( -18.50000000000000000, 68.97833521811159585, -65.68954208262705663 ) ) ;
#114827 = CARTESIAN_POINT ( 'NONE',  ( -16.82055514392372686, 66.05000000001226113, -149.1999055590666217 ) ) ;
#114829 = VERTEX_POINT ( 'NONE', #105553 ) ;
#114828 = EDGE_CURVE ( 'NONE', #90505, #162955, #87296, .T. ) ;
#114831 = CARTESIAN_POINT ( 'NONE',  ( -16.79140778683509794, 66.05505840115743865, -115.6933702507535742 ) ) ;
#114830 = CYLINDRICAL_SURFACE ( 'NONE', #111823, 0.1000000000000052097 ) ;
#114832 = ORIENTED_EDGE ( 'NONE', *, *, #21633, .T. ) ;
#114834 = ORIENTED_EDGE ( 'NONE', *, *, #82060, .T. ) ;
#114833 = DIRECTION ( 'NONE',  ( 0.000000000000000000, 0.8814952561688437216, -0.4721928772777334582 ) ) ;
#114835 = VECTOR ( 'NONE', #38314, 1000.000000000000000 ) ;
#114836 = ORIENTED_EDGE ( 'NONE', *, *, #180026, .F. ) ;
#114837 = VECTOR ( 'NONE', #182127, 1000.000000000000000 ) ;
#114838 = CARTESIAN_POINT ( 'NONE',  ( -21.05000000000000071, 18.60982576078065165, -226.6665746245395496 ) ) ;
#114839 = DIRECTION ( 'NONE',  ( 0.000000000000000000, 6.982962677686266711E-15, -1.000000000000000000 ) ) ;
#114840 = DIRECTION ( 'NONE',  ( -0.000000000000000000, -0.8454177738465993297, -0.5341055959866553016 ) ) ;
#114841 = CARTESIAN_POINT ( 'NONE',  ( -16.94107738177415357, 22.92025126680846014, -230.8312174982872591 ) ) ;
#114842 = EDGE_LOOP ( 'NONE', ( #96639, #219454, #88085, #253581 ) ) ;
#114843 = CARTESIAN_POINT ( 'NONE',  ( 23.14999999999999503, 69.35000000001222986, -148.6731074845243938 ) ) ;
#114844 = DIRECTION ( 'NONE',  ( 1.000000000000000000, 7.304098846218134667E-16, 5.100424963727256530E-30 ) ) ;
#114845 = EDGE_CURVE ( 'NONE', #196258, #180208, #63631, .T. ) ;
#114846 = ORIENTED_EDGE ( 'NONE', *, *, #145328, .F. ) ;
#114847 = EDGE_CURVE ( 'NONE', #72156, #19640, #144703, .T. ) ;
#114848 = CARTESIAN_POINT ( 'NONE',  ( -2.995603634470884209E-16, -11.74999999998884448, -54.75000000000000000 ) ) ;
#114850 = AXIS2_PLACEMENT_3D ( 'NONE', #89472, #213274, #34673 ) ;
#114849 = CARTESIAN_POINT ( 'NONE',  ( 21.07971444708685738, 6.329792081626547606, 0.08782343631790544281 ) ) ;
#114851 = EDGE_CURVE ( 'NONE', #207747, #252194, #187719, .T. ) ;
#114852 = EDGE_LOOP ( 'NONE', ( #182573, #242578, #197804 ) ) ;
#114853 = ORIENTED_EDGE ( 'NONE', *, *, #110095, .F. ) ;
#114855 = CARTESIAN_POINT ( 'NONE',  ( -21.45000000000000284, 52.90028168070691095, -233.8284721206281915 ) ) ;
#114854 = VECTOR ( 'NONE', #169112, 1000.000000000000227 ) ;
#114856 = AXIS2_PLACEMENT_3D ( 'NONE', #129833, #127280, #148129 ) ;
#114857 = AXIS2_PLACEMENT_3D ( 'NONE', #144745, #82191, #224294 ) ;
#114858 = ORIENTED_EDGE ( 'NONE', *, *, #191807, .F. ) ;
#114859 = FACE_OUTER_BOUND ( 'NONE', #7397, .T. ) ;
#114860 = EDGE_LOOP ( 'NONE', ( #28274, #10194, #117993, #94228 ) ) ;
#114861 = CARTESIAN_POINT ( 'NONE',  ( -23.25000000000000000, 11.75000000001115552, -54.84999999999999432 ) ) ;
#114862 = COLOUR_RGB ( '', 0.31764706, 0.68627451, 0.89019608) ;
#114863 = CARTESIAN_POINT ( 'NONE',  ( 22.60000000000000142, 1.148907358139439339E-11, -201.0000000000015064 ) ) ;
#114864 = CARTESIAN_POINT ( 'NONE',  ( 21.51976009735019346, 69.08954155835347422, -203.5231074845243882 ) ) ;
#114865 = ADVANCED_FACE ( 'NONE', ( #205975 ), #203418, .F. ) ;
#114866 = ADVANCED_FACE ( 'NONE', ( #125169 ), #169461, .T. ) ;
#114867 = CARTESIAN_POINT ( 'NONE',  ( -21.53551880898957904, 0.09896973458281840830, -26.71520223858367160 ) ) ;
#114868 = FACE_OUTER_BOUND ( 'NONE', #70427, .T. ) ;
#114869 = DIRECTION ( 'NONE',  ( 0.000000000000000000, 0.8660254037844352659, -0.5000000000000058842 ) ) ;
#114870 = VERTEX_POINT ( 'NONE', #46884 ) ;
#114872 = CARTESIAN_POINT ( 'NONE',  ( 20.27550659511089037, 51.91893134239705887, -232.6162829946506179 ) ) ;
#114871 = DIRECTION ( 'NONE',  ( -1.000000000000000000, 0.000000000000000000, 0.000000000000000000 ) ) ;
#114873 = CIRCLE ( 'NONE', #231406, 0.9750000000000036415 ) ;
#114874 = EDGE_LOOP ( 'NONE', ( #143495, #48253, #248727, #157832 ) ) ;
#114877 = ORIENTED_EDGE ( 'NONE', *, *, #253302, .T. ) ;
#114876 = CARTESIAN_POINT ( 'NONE',  ( -22.39999999999999858, 1.115600667400684642E-11, -122.3504291924552234 ) ) ;
#114875 = CARTESIAN_POINT ( 'NONE',  ( -20.94999999999999574, 64.37928932189355180, -143.3915241368654279 ) ) ;
#114878 = MECHANICAL_DESIGN_GEOMETRIC_PRESENTATION_REPRESENTATION (  '', ( #185604 ), #52312 ) ;
#114879 = VERTEX_POINT ( 'NONE', #28677 ) ;
#114880 = FACE_OUTER_BOUND ( 'NONE', #29544, .T. ) ;
#114881 = AXIS2_PLACEMENT_3D ( 'NONE', #140852, #220395, #48155 ) ;
#114882 = SPHERICAL_SURFACE ( 'NONE', #5775, 0.1000000000000000056 ) ;
#114883 = CARTESIAN_POINT ( 'NONE',  ( -23.25000000000000000, 80.69087520990402140, -192.8618289658565743 ) ) ;
#114884 = DIRECTION ( 'NONE',  ( 1.000000000000000000, 0.000000000000000000, 0.000000000000000000 ) ) ;
#114885 = VERTEX_POINT ( 'NONE', #166889 ) ;
#114887 = VERTEX_POINT ( 'NONE', #108171 ) ;
#114886 = DIRECTION ( 'NONE',  ( -0.000000000000000000, -0.000000000000000000, -1.000000000000000000 ) ) ;
#114888 = AXIS2_PLACEMENT_3D ( 'NONE', #23781, #58987, #159420 ) ;
#114889 =( BOUNDED_CURVE ( )  B_SPLINE_CURVE ( 3, ( #151754, #30515, #111321, #188277 ),
 .UNSPECIFIED., .F., .F. ) 
 B_SPLINE_CURVE_WITH_KNOTS ( ( 4, 4 ),
 ( 1.570796326794908992, 2.617993877991549034 ),
 .UNSPECIFIED. ) 
 CURVE ( )  GEOMETRIC_REPRESENTATION_ITEM ( )  RATIONAL_B_SPLINE_CURVE ( ( 1.000000000000000000, 0.9106836025229521070, 0.9106836025229521070, 1.000000000000000000 ) ) 
 REPRESENTATION_ITEM ( '' )  );
#114890 = AXIS2_PLACEMENT_3D ( 'NONE', #143390, #140832, #243779 ) ;
#114892 = CARTESIAN_POINT ( 'NONE',  ( 20.95420533658165141, 10.54586447475957733, -7.567506020693237190 ) ) ;
#114891 = DIRECTION ( 'NONE',  ( 0.000000000000000000, 0.8814952561688476074, -0.4721928772777262417 ) ) ;
#114893 = AXIS2_PLACEMENT_3D ( 'NONE', #181581, #78600, #99435 ) ;
#114894 = CIRCLE ( 'NONE', #252236, 0.1000000000000021844 ) ;
#114896 = VERTEX_POINT ( 'NONE', #27385 ) ;
#114895 = CARTESIAN_POINT ( 'NONE',  ( -16.89268316805465986, 9.951721813253337601, -54.35575247854554704 ) ) ;
#114897 = ORIENTED_EDGE ( 'NONE', *, *, #98136, .T. ) ;
#114898 = CARTESIAN_POINT ( 'NONE',  ( 20.95017935633852346, 11.84804081051113123, -206.1746882498729292 ) ) ;
#114899 = CIRCLE ( 'NONE', #210568, 0.1000000000000028644 ) ;
#114900 = CARTESIAN_POINT ( 'NONE',  ( -20.94999999999999929, 87.65000000001172964, -72.62310748452422615 ) ) ;
#114901 = ORIENTED_EDGE ( 'NONE', *, *, #79135, .F. ) ;
#114902 = DIRECTION ( 'NONE',  ( 0.000000000000000000, 0.000000000000000000, -1.000000000000000000 ) ) ;
#114903 = EDGE_LOOP ( 'NONE', ( #24160, #126505, #164903, #240822, #64557 ) ) ;
#114905 =( BOUNDED_CURVE ( )  B_SPLINE_CURVE ( 3, ( #185923, #47676, #206776, #78475 ),
 .UNSPECIFIED., .F., .F. ) 
 B_SPLINE_CURVE_WITH_KNOTS ( ( 4, 4 ),
 ( 4.712388980384690562, 6.283185307179586232 ),
 .UNSPECIFIED. ) 
 CURVE ( )  GEOMETRIC_REPRESENTATION_ITEM ( )  RATIONAL_B_SPLINE_CURVE ( ( 1.000000000000000000, 0.8047378541243652705, 0.8047378541243652705, 1.000000000000000000 ) ) 
 REPRESENTATION_ITEM ( '' )  );
#114904 = AXIS2_PLACEMENT_3D ( 'NONE', #185343, #167101, #125376 ) ;
#114906 = FACE_OUTER_BOUND ( 'NONE', #54141, .T. ) ;
#114907 = CARTESIAN_POINT ( 'NONE',  ( 18.59999999999999432, -1.261786168553869603, -75.08649896354552311 ) ) ;
#114908 = B_SPLINE_CURVE_WITH_KNOTS ( 'NONE', 3,
 ( #246239, #106704, #208416, #164144, #147125, #184978, #104134, #222800 ),
 .UNSPECIFIED., .F., .F.,
 ( 4, 2, 2, 4 ),
 ( 0.000000000000000000, 0.0001049670497869896891, 0.0002099340995739793782, 0.0004198681991480113403 ),
 .UNSPECIFIED. ) ;
#114909 = TOROIDAL_SURFACE ( 'NONE', #243890, 0.6000000000000009770, 0.1000000000000000056 ) ;
#114911 = VERTEX_POINT ( 'NONE', #104287 ) ;
#114910 = VECTOR ( 'NONE', #64085, 1000.000000000000000 ) ;
#114912 = CARTESIAN_POINT ( 'NONE',  ( 0.8999999999999992450, -8.250000000000005329, 21.95857864376268864 ) ) ;
#114913 = EDGE_CURVE ( 'NONE', #251809, #85514, #29932, .T. ) ;
#114914 = DIRECTION ( 'NONE',  ( -1.000000000000000000, 3.265361837132813093E-16, 2.280189983783949500E-30 ) ) ;
#114915 =( BOUNDED_SURFACE ( )  B_SPLINE_SURFACE ( 3, 2, ( 
 ( #175752, #101266, #197848 ),
 ( #201704, #217403, #216125 ),
 ( #178323, #239557, #140436 ),
 ( #79174, #42631, #41379 ),
 ( #17925, #120919, #257774 ),
 ( #199144, #59597, #158760 ) ),
 .UNSPECIFIED., .F., .F., .F. ) 
 B_SPLINE_SURFACE_WITH_KNOTS ( ( 4, 2, 4 ),
 ( 3, 3 ),
 ( 0.0001792624049599534481, 0.0003686986002124517745, 0.0005581347954649500467 ),
 ( 0.000000000000000000, 1.000000000000000000 ),
 .UNSPECIFIED. ) 
 GEOMETRIC_REPRESENTATION_ITEM ( )  RATIONAL_B_SPLINE_SURFACE ( (
 ( 1.000000000000000000, 0.9238795325112856283, 1.000000000000000000),
 ( 1.000000000000000000, 0.9229318695237381798, 1.000000000000000000),
 ( 1.000000000000000000, 0.8926288119231814422, 1.000000000000000000),
 ( 1.000000000000000000, 0.8123777807270232687, 1.000000000000000000),
 ( 1.000000000000000000, 0.7629087100932465670, 1.000000000000000000),
 ( 1.000000000000000000, 0.7071067811865475727, 1.000000000000000000) ) ) 
 REPRESENTATION_ITEM ( '' )  SURFACE ( )  );
#114916 = ORIENTED_EDGE ( 'NONE', *, *, #19353, .F. ) ;
#114917 = VERTEX_POINT ( 'NONE', #229403 ) ;
#114918 = CARTESIAN_POINT ( 'NONE',  ( 20.44999100639848066, 18.89797881968811666, -228.1939261438453173 ) ) ;
#114919 = ORIENTED_EDGE ( 'NONE', *, *, #87451, .T. ) ;
#114921 = EDGE_CURVE ( 'NONE', #26064, #168680, #106861, .T. ) ;
#114920 = ORIENTED_EDGE ( 'NONE', *, *, #114747, .F. ) ;
#114923 = ORIENTED_EDGE ( 'NONE', *, *, #225296, .T. ) ;
#114922 = CARTESIAN_POINT ( 'NONE',  ( 21.22070241538126467, 75.90108096947696481, -109.4930537573939375 ) ) ;
#114924 = ORIENTED_EDGE ( 'NONE', *, *, #28411, .F. ) ;
#114925 = TOROIDAL_SURFACE ( 'NONE', #239837, 12.97499999999999609, 0.1000000000000000056 ) ;
#114926 = EDGE_CURVE ( 'NONE', #64653, #52602, #226103, .T. ) ;
#114927 = CARTESIAN_POINT ( 'NONE',  ( -20.94999999999999929, 1.681127862299736098, -208.7190549363676269 ) ) ;
#114928 = ADVANCED_FACE ( 'NONE', ( #50721 ), #84429, .T. ) ;
#114929 = EDGE_LOOP ( 'NONE', ( #38533, #86321, #140175, #160892 ) ) ;
#114930 = VECTOR ( 'NONE', #108508, 1000.000000000000000 ) ;
#114933 = ORIENTED_EDGE ( 'NONE', *, *, #226791, .T. ) ;
#114932 = ORIENTED_EDGE ( 'NONE', *, *, #53704, .F. ) ;
#114931 = LINE ( 'NONE', #194488, #47878 ) ;
#114934 = VECTOR ( 'NONE', #164080, 1000.000000000000000 ) ;
#114935 = VECTOR ( 'NONE', #198913, 1000.000000000000000 ) ;
#114936 = EDGE_LOOP ( 'NONE', ( #129780, #198565, #140557, #10103 ) ) ;
#114937 = DIRECTION ( 'NONE',  ( 0.000000000000000000, -0.2617529984165152257, -0.9651348961777124202 ) ) ;
#114938 = CIRCLE ( 'NONE', #214885, 0.1000000000000028644 ) ;
#114939 = DIRECTION ( 'NONE',  ( -0.000000000000000000, 1.000000000000000000, 0.000000000000000000 ) ) ;
#114940 = ORIENTED_EDGE ( 'NONE', *, *, #158991, .F. ) ;
#114941 = EDGE_CURVE ( 'NONE', #44131, #242050, #11648, .T. ) ;
#114942 = DIRECTION ( 'NONE',  ( 1.000000000000000000, 0.000000000000000000, 0.000000000000000000 ) ) ;
#114943 = EDGE_LOOP ( 'NONE', ( #203118, #209593, #104058, #113921, #10175 ) ) ;
#114944 = CARTESIAN_POINT ( 'NONE',  ( -18.50000000000000000, 72.08710075277841156, -91.54128451151336776 ) ) ;
#114945 = ORIENTED_EDGE ( 'NONE', *, *, #135893, .F. ) ;
#114946 = ORIENTED_EDGE ( 'NONE', *, *, #111020, .F. ) ;
#114947 = CARTESIAN_POINT ( 'NONE',  ( 21.00023020733505064, 1.115539681028482333E-11, -161.1091307547316092 ) ) ;
#114948 = CARTESIAN_POINT ( 'NONE',  ( 23.14999999999999147, 76.00000000001165290, -69.52310748452431710 ) ) ;
#114949 = CIRCLE ( 'NONE', #214898, 0.1000000000000070832 ) ;
#114950 = ORIENTED_EDGE ( 'NONE', *, *, #80276, .T. ) ;
#114951 = ORIENTED_EDGE ( 'NONE', *, *, #13192, .F. ) ;
#114952 = CARTESIAN_POINT ( 'NONE',  ( -16.94309007106720699, 9.992226192581142641, -180.1057912825554581 ) ) ;
#114953 = FACE_OUTER_BOUND ( 'NONE', #212781, .T. ) ;
#114955 = VERTEX_POINT ( 'NONE', #92430 ) ;
#114954 = ORIENTED_EDGE ( 'NONE', *, *, #215007, .F. ) ;
#114956 = ORIENTED_EDGE ( 'NONE', *, *, #157951, .T. ) ;
#114957 = CARTESIAN_POINT ( 'NONE',  ( 18.59999999999999432, 77.16270174995064224, -195.4231074845243370 ) ) ;
#114959 = ORIENTED_EDGE ( 'NONE', *, *, #3146, .F. ) ;
#114958 = EDGE_CURVE ( 'NONE', #514, #122992, #230231, .T. ) ;
#114960 = VERTEX_POINT ( 'NONE', #172027 ) ;
#114961 = DIRECTION ( 'NONE',  ( -0.000000000000000000, 0.4088369013363281068, -0.9126074666063770380 ) ) ;
#114962 = AXIS2_PLACEMENT_3D ( 'NONE', #123611, #83151, #162750 ) ;
#114963 = ORIENTED_EDGE ( 'NONE', *, *, #246052, .T. ) ;
#114964 = FACE_OUTER_BOUND ( 'NONE', #216225, .T. ) ;
#114965 = DIRECTION ( 'NONE',  ( -1.000000000000000000, -2.952720810173289112E-16, 0.000000000000000000 ) ) ;
#114966 = ORIENTED_EDGE ( 'NONE', *, *, #177181, .F. ) ;
#114968 = EDGE_CURVE ( 'NONE', #116784, #206263, #173322, .T. ) ;
#114967 = ORIENTED_EDGE ( 'NONE', *, *, #186197, .T. ) ;
#114969 = CARTESIAN_POINT ( 'NONE',  ( -14.00000000000000178, 66.15000000001185754, -86.27310748452437394 ) ) ;
#114970 = ORIENTED_EDGE ( 'NONE', *, *, #110658, .F. ) ;
#114971 = CIRCLE ( 'NONE', #81610, 0.09999999999999939493 ) ;
#114972 = VECTOR ( 'NONE', #166678, 1000.000000000000000 ) ;
#114973 = AXIS2_PLACEMENT_3D ( 'NONE', #20912, #162982, #183806 ) ;
#114974 = AXIS2_PLACEMENT_3D ( 'NONE', #169583, #213791, #71731 ) ;
#114975 = CARTESIAN_POINT ( 'NONE',  ( -20.64999999999999858, 74.00000000001186606, -89.79848556176222019 ) ) ;
#114976 = ORIENTED_EDGE ( 'NONE', *, *, #229883, .F. ) ;
#114977 = ORIENTED_EDGE ( 'NONE', *, *, #209871, .T. ) ;
#114978 = LINE ( 'NONE', #175003, #33608 ) ;
#114980 = VERTEX_POINT ( 'NONE', #115864 ) ;
#114979 = DIRECTION ( 'NONE',  ( 1.000000000000000000, 0.000000000000000000, 0.000000000000000000 ) ) ;
#114981 = CARTESIAN_POINT ( 'NONE',  ( -20.94999999999999929, -11.74999999998884448, -170.3999999999999773 ) ) ;
#114982 = CARTESIAN_POINT ( 'NONE',  ( 21.14999999999999858, -0.09999999999999939493, 11.64957080754479968 ) ) ;
#114983 = ORIENTED_EDGE ( 'NONE', *, *, #60201, .T. ) ;
#114984 = CARTESIAN_POINT ( 'NONE',  ( 18.49999999999999289, 33.72439408143423378, -236.3982354565453363 ) ) ;
#114985 = LINE ( 'NONE', #135816, #248714 ) ;
#114986 = FACE_OUTER_BOUND ( 'NONE', #161084, .T. ) ;
#114987 = CYLINDRICAL_SURFACE ( 'NONE', #87109, 0.09999999999999543976 ) ;
#114988 = CARTESIAN_POINT ( 'NONE',  ( 23.14999999999999147, 7.128833340093095217, -233.7327013124392749 ) ) ;
#114989 = DIRECTION ( 'NONE',  ( 1.000000000000000000, -7.304098846218135653E-16, 0.000000000000000000 ) ) ;
#114990 = DIRECTION ( 'NONE',  ( -1.000000000000000000, -0.000000000000000000, -0.000000000000000000 ) ) ;
#114991 = LINE ( 'NONE', #112440, #122233 ) ;
#114992 = CIRCLE ( 'NONE', #164881, 11.80000000000000426 ) ;
#114993 = TOROIDAL_SURFACE ( 'NONE', #69229, 0.9750000000000019762, 0.1000000000000000056 ) ;
#114994 = ORIENTED_EDGE ( 'NONE', *, *, #42607, .F. ) ;
#114995 = ADVANCED_FACE ( 'NONE', ( #175853 ), #170758, .F. ) ;
#114997 = EDGE_LOOP ( 'NONE', ( #203577, #52206, #15287, #217018 ) ) ;
#114996 = VERTEX_POINT ( 'NONE', #32516 ) ;
#114998 = TOROIDAL_SURFACE ( 'NONE', #98200, 0.2000000000000000111, 0.1000000000000000056 ) ;
#115000 = ORIENTED_EDGE ( 'NONE', *, *, #2583, .F. ) ;
#114999 = EDGE_CURVE ( 'NONE', #92834, #89858, #226288, .T. ) ;
#115001 = CARTESIAN_POINT ( 'NONE',  ( -21.08134388332232589, 0.07581891751813445157, -94.16531941948205997 ) ) ;
#115002 = DIRECTION ( 'NONE',  ( 1.000000000000000000, -0.000000000000000000, -0.000000000000000000 ) ) ;
#115003 = ADVANCED_FACE ( 'NONE', ( #231980 ), #15500, .T. ) ;
#115004 = EDGE_CURVE ( 'NONE', #177537, #17741, #151331, .T. ) ;
#115006 = CARTESIAN_POINT ( 'NONE',  ( 21.05000000000000071, -8.999999999988842703, -191.1060308773475072 ) ) ;
#115005 = DIRECTION ( 'NONE',  ( 7.589415207398576792E-15, 1.000000000000000000, 6.982962677686266711E-15 ) ) ;
#115007 = EDGE_LOOP ( 'NONE', ( #176092, #178351, #84099, #162019 ) ) ;
#115008 = ORIENTED_EDGE ( 'NONE', *, *, #32053, .F. ) ;
#115009 = CARTESIAN_POINT ( 'NONE',  ( -23.25000000000000000, 1.115600667400684642E-11, -67.00000000000004263 ) ) ;
#115010 = CARTESIAN_POINT ( 'NONE',  ( 23.24999999999999645, 11.74999999999998224, -12.65000000000000746 ) ) ;
#115011 = CARTESIAN_POINT ( 'NONE',  ( -22.59999999999999787, 64.25043287652255231, -103.1239658536231047 ) ) ;
#115012 = EDGE_CURVE ( 'NONE', #172097, #101237, #242885, .T. ) ;
#115013 = FACE_OUTER_BOUND ( 'NONE', #215278, .T. ) ;
#115014 = VERTEX_POINT ( 'NONE', #212413 ) ;
#115015 = ORIENTED_EDGE ( 'NONE', *, *, #179889, .F. ) ;
#115016 = EDGE_CURVE ( 'NONE', #215662, #184556, #9832, .T. ) ;
#115017 = AXIS2_PLACEMENT_3D ( 'NONE', #27468, #207357, #87374 ) ;
#115018 = CARTESIAN_POINT ( 'NONE',  ( 21.05000000000000071, -1.162701749926853712, -108.4000000000000341 ) ) ;
#115020 = ADVANCED_FACE ( 'NONE', ( #93728, #52016 ), #55853, .F. ) ;
#115019 = ADVANCED_FACE ( 'NONE', ( #110726 ), #113291, .F. ) ;
#115021 = CARTESIAN_POINT ( 'NONE',  ( 18.39999999999999858, -9.599999999988845900, -140.6001893912220737 ) ) ;
#115022 = ORIENTED_EDGE ( 'NONE', *, *, #153677, .F. ) ;
#115023 = DIRECTION ( 'NONE',  ( 0.000000000000000000, 0.000000000000000000, -1.000000000000000000 ) ) ;
#115024 = CARTESIAN_POINT ( 'NONE',  ( 23.50000000000005684, 76.00000000001119815, -40.17310748452479174 ) ) ;
#115025 = ADVANCED_FACE ( 'NONE', ( #213678 ), #51316, .F. ) ;
#115026 = CARTESIAN_POINT ( 'NONE',  ( -20.54999999999999716, 85.40000000001221281, -146.4170766071767389 ) ) ;
#115027 = SPHERICAL_SURFACE ( 'NONE', #35731, 0.1000000000000000056 ) ;
#115028 = CARTESIAN_POINT ( 'NONE',  ( 18.39999999999999858, 85.51932773110434027, -96.05013110796491560 ) ) ;
#115029 = ORIENTED_EDGE ( 'NONE', *, *, #99529, .F. ) ;
#115030 = DIRECTION ( 'NONE',  ( 0.000000000000000000, -0.2818822000685679008, 0.9594490217226259166 ) ) ;
#115031 = FACE_OUTER_BOUND ( 'NONE', #42140, .T. ) ;
#115032 = DIRECTION ( 'NONE',  ( -0.000000000000000000, -1.000000000000000000, 6.308085367188393199E-16 ) ) ;
#115033 = ADVANCED_FACE ( 'NONE', ( #211113 ), #35083, .T. ) ;
#115035 = LINE ( 'NONE', #135859, #66269 ) ;
#115034 = CARTESIAN_POINT ( 'NONE',  ( -16.81453046979148880, 66.06089771857114101, -123.8113809609213689 ) ) ;
#115036 = CARTESIAN_POINT ( 'NONE',  ( -20.00857864376270001, 66.65000000001198543, -115.2731074845243597 ) ) ;
#115037 = AXIS2_PLACEMENT_3D ( 'NONE', #19863, #240191, #195937 ) ;
#115038 = CARTESIAN_POINT ( 'NONE',  ( -16.93301857435212554, 9.976309354746611291, -121.3857755711614601 ) ) ;
#115039 = CARTESIAN_POINT ( 'NONE',  ( 20.90000000000000213, 11.59510167572422112, 1.901609089591594470 ) ) ;
#115040 = CARTESIAN_POINT ( 'NONE',  ( 20.85000000000000142, 6.846123162363745074, -204.7377262668498190 ) ) ;
#115041 = EDGE_CURVE ( 'NONE', #195949, #18361, #109782, .T. ) ;
#115042 = ADVANCED_FACE ( 'NONE', ( #37628 ), #134718, .T. ) ;
#115043 = AXIS2_PLACEMENT_3D ( 'NONE', #107708, #167717, #244646 ) ;
#115044 = ORIENTED_EDGE ( 'NONE', *, *, #246345, .F. ) ;
#115045 = AXIS2_PLACEMENT_3D ( 'NONE', #247390, #10076, #70080 ) ;
#115047 = EDGE_LOOP ( 'NONE', ( #215218, #164270, #46730, #1539 ) ) ;
#115046 = STYLED_ITEM ( 'NONE', ( #66932 ), #14150 ) ;
#115048 = EDGE_CURVE ( 'NONE', #96616, #37588, #240945, .T. ) ;
#115049 = CARTESIAN_POINT ( 'NONE',  ( -23.25000000000000000, -2.598867842139046314, -189.5410128746472083 ) ) ;
#115050 = ORIENTED_EDGE ( 'NONE', *, *, #183615, .T. ) ;
#115051 = DIRECTION ( 'NONE',  ( 1.000000000000000000, 0.000000000000000000, 0.000000000000000000 ) ) ;
#115052 = EDGE_CURVE ( 'NONE', #135846, #198608, #126364, .T. ) ;
#115053 = ORIENTED_EDGE ( 'NONE', *, *, #40727, .T. ) ;
#115054 = FILL_AREA_STYLE ('',( #14699 ) ) ;
#115055 = ADVANCED_FACE ( 'NONE', ( #235797 ), #41479, .T. ) ;
#115056 = DIRECTION ( 'NONE',  ( 0.000000000000000000, -7.034366652768107165E-15, 1.000000000000000000 ) ) ;
#115057 = AXIS2_PLACEMENT_3D ( 'NONE', #93960, #74447, #75704 ) ;
#115058 = ORIENTED_EDGE ( 'NONE', *, *, #9540, .F. ) ;
#115059 = CARTESIAN_POINT ( 'NONE',  ( 18.39999999999999503, 20.94763808724815846, -234.7254930126486556 ) ) ;
#115060 = VECTOR ( 'NONE', #56799, 1000.000000000000227 ) ;
#115061 = CARTESIAN_POINT ( 'NONE',  ( -12.26136940704872025, 9.351403174152810749, -50.47953043683849472 ) ) ;
#115062 = DIRECTION ( 'NONE',  ( 0.000000000000000000, 0.000000000000000000, 1.000000000000000000 ) ) ;
#115063 = DIRECTION ( 'NONE',  ( 1.000000000000000000, 0.000000000000000000, -0.000000000000000000 ) ) ;
#115065 = ORIENTED_EDGE ( 'NONE', *, *, #226672, .T. ) ;
#115064 = DIRECTION ( 'NONE',  ( -1.000000000000000000, -2.952720810173289112E-16, 0.000000000000000000 ) ) ;
#115067 = DIRECTION ( 'NONE',  ( 0.000000000000000000, 0.000000000000000000, 1.000000000000000000 ) ) ;
#115066 = CARTESIAN_POINT ( 'NONE',  ( 21.13422380239052600, 6.344600517422461117, -199.6182136553211706 ) ) ;
#115068 = EDGE_CURVE ( 'NONE', #148396, #219363, #178430, .T. ) ;
#115069 = PLANE ( 'NONE',  #98589 ) ;
#115070 = DIRECTION ( 'NONE',  ( 1.000000000000000000, 2.952720810173289112E-16, -0.000000000000000000 ) ) ;
#115071 = VECTOR ( 'NONE', #251470, 1000.000000000000000 ) ;
#115072 = CARTESIAN_POINT ( 'NONE',  ( -19.89999999999999503, 5.572646938319268273, 16.50000000000000000 ) ) ;
#115073 = DIRECTION ( 'NONE',  ( 0.000000000000000000, 0.9126074666063771490, 0.4088369013363281623 ) ) ;
#115075 = ORIENTED_EDGE ( 'NONE', *, *, #144056, .F. ) ;
#115074 = VECTOR ( 'NONE', #230772, 1000.000000000000000 ) ;
#115076 = CARTESIAN_POINT ( 'NONE',  ( -18.59999999999999787, 13.35316836840606669, -247.8440497049677731 ) ) ;
#115077 = ORIENTED_EDGE ( 'NONE', *, *, #90052, .T. ) ;
#115078 = CARTESIAN_POINT ( 'NONE',  ( -22.50000000000000000, 36.61804073161109585, -249.4599019545848364 ) ) ;
#115079 = VERTEX_POINT ( 'NONE', #136691 ) ;
#115080 = CIRCLE ( 'NONE', #2638, 0.5000000000000004441 ) ;
#115081 = DIRECTION ( 'NONE',  ( -0.000000000000000000, -6.982962677686266711E-15, 1.000000000000000000 ) ) ;
#115082 = AXIS2_PLACEMENT_3D ( 'NONE', #12421, #90634, #30706 ) ;
#115083 = AXIS2_PLACEMENT_3D ( 'NONE', #899, #24374, #84264 ) ;
#115084 = CARTESIAN_POINT ( 'NONE',  ( -16.94445028196807002, 9.992063609697737547, -20.89266982158155628 ) ) ;
#115085 = ORIENTED_EDGE ( 'NONE', *, *, #150159, .T. ) ;
#115086 = CIRCLE ( 'NONE', #194223, 0.2000000000000106137 ) ;
#115087 = ORIENTED_EDGE ( 'NONE', *, *, #113175, .F. ) ;
#115088 = DIRECTION ( 'NONE',  ( -0.000000000000000000, 0.2128009952263603677, -0.9770955615653313941 ) ) ;
#115089 = DIRECTION ( 'NONE',  ( -0.000000000000000000, 0.8814952561688430555, -0.4721928772777346239 ) ) ;
#115090 = EDGE_CURVE ( 'NONE', #68335, #29322, #238802, .T. ) ;
#115091 = CARTESIAN_POINT ( 'NONE',  ( -16.84793658983424436, 63.06383758434998299, -213.2083519146329422 ) ) ;
#115092 = CARTESIAN_POINT ( 'NONE',  ( 21.05000000000000071, 87.48912529308822172, -139.6231074845242688 ) ) ;
#115093 = CIRCLE ( 'NONE', #61106, 4.300000000000039790 ) ;
#115095 = DIRECTION ( 'NONE',  ( 1.000000000000000000, 0.000000000000000000, 0.000000000000000000 ) ) ;
#115094 = DIRECTION ( 'NONE',  ( 0.000000000000000000, 0.000000000000000000, -1.000000000000000000 ) ) ;
#115096 = DIRECTION ( 'NONE',  ( 1.000000000000000000, -0.000000000000000000, -0.000000000000000000 ) ) ;
#115097 = EDGE_CURVE ( 'NONE', #78774, #74786, #197087, .T. ) ;
#115098 = DIRECTION ( 'NONE',  ( 0.000000000000000000, 0.000000000000000000, -1.000000000000000000 ) ) ;
#115099 = CARTESIAN_POINT ( 'NONE',  ( -20.64999999999999858, 46.15118611352045974, -240.5321844900040844 ) ) ;
#115100 = ORIENTED_EDGE ( 'NONE', *, *, #236842, .T. ) ;
#115101 = PLANE ( 'NONE',  #131273 ) ;
#115103 = ORIENTED_EDGE ( 'NONE', *, *, #131192, .T. ) ;
#115102 = CARTESIAN_POINT ( 'NONE',  ( 23.24999999999999645, 9.957490673325210651, -220.1701168356097469 ) ) ;
#115104 = CARTESIAN_POINT ( 'NONE',  ( 18.59999999999999432, -1.835859311432481045, -145.5044391687985694 ) ) ;
#115105 = CARTESIAN_POINT ( 'NONE',  ( 22.48970261584621966, 11.37138061004976386, -198.4667671244310441 ) ) ;
#115107 = CARTESIAN_POINT ( 'NONE',  ( -23.15000000000000213, 85.00000000001222134, -145.9170766071767389 ) ) ;
#115106 = CARTESIAN_POINT ( 'NONE',  ( -21.44999999999999929, 7.350000000011155166, -121.6500000000000341 ) ) ;
#115108 = ADVANCED_FACE ( 'NONE', ( #216226 ), #159844, .T. ) ;
#115109 = EDGE_CURVE ( 'NONE', #112934, #247963, #209182, .T. ) ;
#115111 = ORIENTED_EDGE ( 'NONE', *, *, #247167, .T. ) ;
#115110 = CARTESIAN_POINT ( 'NONE',  ( 21.53752568617689178, 69.21319212550830002, -136.6220819458087306 ) ) ;
#115112 = DIRECTION ( 'NONE',  ( 0.000000000000000000, -0.8814952561688398358, 0.4721928772777406746 ) ) ;
#115113 = DIRECTION ( 'NONE',  ( 1.000000000000000000, -0.000000000000000000, -0.000000000000000000 ) ) ;
#115114 = CARTESIAN_POINT ( 'NONE',  ( -20.94999999999999929, 26.34542992457388522, -244.0265060370938954 ) ) ;
#115115 = CARTESIAN_POINT ( 'NONE',  ( 20.94999999999999929, 53.70241689174373079, -235.9987767062293074 ) ) ;
#115116 = DIRECTION ( 'NONE',  ( -2.827886303505248766E-16, 0.8660254037844411501, 0.4999999999999956146 ) ) ;
#115117 = ORIENTED_EDGE ( 'NONE', *, *, #136042, .T. ) ;
#115118 = DIRECTION ( 'NONE',  ( -0.000000000000000000, 0.000000000000000000, 1.000000000000000000 ) ) ;
#115119 = AXIS2_PLACEMENT_3D ( 'NONE', #257549, #97206, #78945 ) ;
#115120 = ADVANCED_FACE ( 'NONE', ( #231339 ), #184615, .T. ) ;
#115121 = EDGE_LOOP ( 'NONE', ( #54378, #121957, #177369, #14861 ) ) ;
#115122 = AXIS2_PLACEMENT_3D ( 'NONE', #233056, #252583, #34863 ) ;
#115123 = VECTOR ( 'NONE', #214328, 1000.000000000000000 ) ;
#115124 = CARTESIAN_POINT ( 'NONE',  ( -18.47690164073607022, -9.464844538012236796, -40.20138093983610617 ) ) ;
#115125 = ORIENTED_EDGE ( 'NONE', *, *, #196603, .F. ) ;
#115126 = CARTESIAN_POINT ( 'NONE',  ( -20.94999027547553894, 46.33166059915855328, -243.0555356998360423 ) ) ;
#115127 = VERTEX_POINT ( 'NONE', #132219 ) ;
#115128 = VECTOR ( 'NONE', #80266, 1000.000000000000000 ) ;
#115129 = EDGE_CURVE ( 'NONE', #52715, #96287, #59698, .T. ) ;
#115130 = DIRECTION ( 'NONE',  ( 0.000000000000000000, 0.000000000000000000, -1.000000000000000000 ) ) ;
#115131 = DIRECTION ( 'NONE',  ( 1.000000000000000000, 0.000000000000000000, 0.000000000000000000 ) ) ;
#115132 = DIRECTION ( 'NONE',  ( 1.000000000000000000, 0.000000000000000000, 0.000000000000000000 ) ) ;
#115133 = VERTEX_POINT ( 'NONE', #51357 ) ;
#115134 = AXIS2_PLACEMENT_3D ( 'NONE', #79048, #239446, #119501 ) ;
#115136 = AXIS2_PLACEMENT_3D ( 'NONE', #104795, #186970, #249497 ) ;
#115135 = CARTESIAN_POINT ( 'NONE',  ( -22.47071067811865319, -1.546016791165058635, -193.4356622592196970 ) ) ;
#115137 = DIRECTION ( 'NONE',  ( 0.000000000000000000, 0.000000000000000000, 1.000000000000000000 ) ) ;
#115138 = VECTOR ( 'NONE', #197184, 1000.000000000000000 ) ;
#115139 = CARTESIAN_POINT ( 'NONE',  ( -23.15000000000000213, 1.115600667400684642E-11, -167.5000000000000284 ) ) ;
#115140 = CARTESIAN_POINT ( 'NONE',  ( -20.54999999999999716, 19.25956423861613231, -238.0467473098318010 ) ) ;
#115141 = DIRECTION ( 'NONE',  ( 0.000000000000000000, 0.8660254037844420383, -0.4999999999999941713 ) ) ;
#115143 = ORIENTED_EDGE ( 'NONE', *, *, #213360, .T. ) ;
#115142 = EDGE_CURVE ( 'NONE', #52138, #51901, #113892, .T. ) ;
#115144 = CARTESIAN_POINT ( 'NONE',  ( -18.40904629823847571, 85.50000000001210765, -129.9229179220422452 ) ) ;
#115145 = ORIENTED_EDGE ( 'NONE', *, *, #217073, .F. ) ;
#115147 = ORIENTED_EDGE ( 'NONE', *, *, #178859, .F. ) ;
#115146 = CARTESIAN_POINT ( 'NONE',  ( 21.11747605621531321, 67.22129199451896397, -90.77854431473458874 ) ) ;
#115148 = ORIENTED_EDGE ( 'NONE', *, *, #248808, .F. ) ;
#115149 = DIRECTION ( 'NONE',  ( 1.000000000000000000, 0.000000000000000000, 0.000000000000000000 ) ) ;
#115150 = CARTESIAN_POINT ( 'NONE',  ( 23.14999999999999858, 76.00000000001213607, -136.5231074845243313 ) ) ;
#115151 = CARTESIAN_POINT ( 'NONE',  ( -20.94999999999999929, 68.97833521811233481, -166.1895420826271277 ) ) ;
#115152 = CARTESIAN_POINT ( 'NONE',  ( 18.59999999999999432, 1.637172712981537659, -78.58215336547205254 ) ) ;
#115154 = ORIENTED_EDGE ( 'NONE', *, *, #5172, .F. ) ;
#115153 = AXIS2_PLACEMENT_3D ( 'NONE', #93146, #249673, #211834 ) ;
#115155 = CARTESIAN_POINT ( 'NONE',  ( -16.97683809663752186, 9.950000000011138823, -147.4023640181965220 ) ) ;
#115156 = CARTESIAN_POINT ( 'NONE',  ( 23.15000000000000213, 85.00000000001207923, -126.6291383618717816 ) ) ;
#115157 = ADVANCED_FACE ( 'NONE', ( #190936 ), #144373, .T. ) ;
#115158 = ORIENTED_EDGE ( 'NONE', *, *, #228458, .T. ) ;
#115160 = ORIENTED_EDGE ( 'NONE', *, *, #124916, .T. ) ;
#115159 = LINE ( 'NONE', #73494, #63445 ) ;
#115162 = ADVANCED_FACE ( 'NONE', ( #242213 ), #25063, .F. ) ;
#115161 = CARTESIAN_POINT ( 'NONE',  ( -21.05000000000000071, 76.00000000001244871, -170.0231074845243597 ) ) ;
#115163 = DIRECTION ( 'NONE',  ( 0.000000000000000000, 0.000000000000000000, -1.000000000000000000 ) ) ;
#115164 = CARTESIAN_POINT ( 'NONE',  ( -16.77308656112214535, 9.950000000011135270, -79.65019319170235690 ) ) ;
#115165 = VECTOR ( 'NONE', #185610, 1000.000000000000000 ) ;
#115166 = VECTOR ( 'NONE', #134878, 1000.000000000000000 ) ;
#115167 = CIRCLE ( 'NONE', #198547, 0.2000000000000057288 ) ;
#115168 = CIRCLE ( 'NONE', #111059, 0.1000000000000060146 ) ;
#115169 = ORIENTED_EDGE ( 'NONE', *, *, #147130, .F. ) ;
#115170 = EDGE_CURVE ( 'NONE', #90118, #240031, #166716, .T. ) ;
#115171 = CARTESIAN_POINT ( 'NONE',  ( -23.25000000000000000, 44.25095746879271985, -258.9156452930671435 ) ) ;
#115172 = ORIENTED_EDGE ( 'NONE', *, *, #145017, .F. ) ;
#115173 = CARTESIAN_POINT ( 'NONE',  ( 20.94999999999999929, 18.94908112497232011, -227.8991131484155517 ) ) ;
#115174 = EDGE_CURVE ( 'NONE', #39555, #58451, #251241, .T. ) ;
#115175 = DIRECTION ( 'NONE',  ( 0.000000000000000000, 0.000000000000000000, -1.000000000000000000 ) ) ;
#115176 = ADVANCED_FACE ( 'NONE', ( #183541 ), #184809, .F. ) ;
#115177 = DIRECTION ( 'NONE',  ( 0.000000000000000000, 0.000000000000000000, 1.000000000000000000 ) ) ;
#115178 = EDGE_CURVE ( 'NONE', #26247, #179805, #6163, .T. ) ;
#115179 = AXIS2_PLACEMENT_3D ( 'NONE', #136861, #183375, #195579 ) ;
#115180 = AXIS2_PLACEMENT_3D ( 'NONE', #68889, #166720, #6315 ) ;
#115181 = AXIS2_PLACEMENT_3D ( 'NONE', #196973, #155328, #56172 ) ;
#115182 = ORIENTED_EDGE ( 'NONE', *, *, #129606, .T. ) ;
#115183 = DIRECTION ( 'NONE',  ( 1.000000000000000000, 0.000000000000000000, 0.000000000000000000 ) ) ;
#115184 = CIRCLE ( 'NONE', #48538, 0.09999999999999917288 ) ;
#115185 = EDGE_LOOP ( 'NONE', ( #195511, #188348, #130710 ) ) ;
#115186 = DIRECTION ( 'NONE',  ( -1.000000000000000000, 0.000000000000000000, -0.000000000000000000 ) ) ;
#115188 = EDGE_CURVE ( 'NONE', #64202, #250227, #30524, .T. ) ;
#115187 = CARTESIAN_POINT ( 'NONE',  ( -22.59999999999999787, 0.1008583691098682150, -88.75043287651064361 ) ) ;
#115190 = ORIENTED_EDGE ( 'NONE', *, *, #14856, .F. ) ;
#115189 = CARTESIAN_POINT ( 'NONE',  ( 23.15000000000000213, -11.48912529306489994, -164.4000000000000057 ) ) ;
#115191 = DIRECTION ( 'NONE',  ( -1.000000000000000000, -0.000000000000000000, -0.000000000000000000 ) ) ;
#115192 = LINE ( 'NONE', #19958, #82495 ) ;
#115193 = DIRECTION ( 'NONE',  ( 0.000000000000000000, -0.4721928772777344019, -0.8814952561688431665 ) ) ;
#115194 = CARTESIAN_POINT ( 'NONE',  ( 20.94999999999999929, 5.000000000011153745, -179.9052660189130677 ) ) ;
#115195 = DIRECTION ( 'NONE',  ( 0.000000000000000000, 0.8700118002898357128, -0.4930308989875170633 ) ) ;
#115196 = FACE_OUTER_BOUND ( 'NONE', #47934, .T. ) ;
#115197 = CARTESIAN_POINT ( 'NONE',  ( 21.14999999999999858, 6.540656951712400691, -67.00000000000004263 ) ) ;
#115199 = ORIENTED_EDGE ( 'NONE', *, *, #10680, .F. ) ;
#115198 = LINE ( 'NONE', #154371, #111249 ) ;
#115200 = VECTOR ( 'NONE', #194867, 1000.000000000000114 ) ;
#115201 = DIRECTION ( 'NONE',  ( 0.000000000000000000, 6.982962677686266711E-15, -1.000000000000000000 ) ) ;
#115202 = LINE ( 'NONE', #130914, #132325 ) ;
#115203 = CARTESIAN_POINT ( 'NONE',  ( -18.49346865148325492, 85.44307379853751172, -196.3379112292089985 ) ) ;
#115204 = AXIS2_PLACEMENT_3D ( 'NONE', #237588, #219293, #198450 ) ;
#115205 = ORIENTED_EDGE ( 'NONE', *, *, #91326, .T. ) ;
#115206 = DIRECTION ( 'NONE',  ( -1.000000000000000000, 0.000000000000000000, -0.000000000000000000 ) ) ;
#115207 = CARTESIAN_POINT ( 'NONE',  ( 21.30000000000002558, 1.115600667400684642E-11, -134.0000000000000000 ) ) ;
#115208 = CARTESIAN_POINT ( 'NONE',  ( 23.14999999999999858, 5.500000000011153745, -54.59473398108690390 ) ) ;
#115209 = AXIS2_PLACEMENT_3D ( 'NONE', #154599, #134973, #193700 ) ;
#115210 = ORIENTED_EDGE ( 'NONE', *, *, #6684, .T. ) ;
#115211 = CIRCLE ( 'NONE', #156934, 0.1000000000000028644 ) ;
#115212 = VECTOR ( 'NONE', #256317, 1000.000000000000114 ) ;
#115213 = DIRECTION ( 'NONE',  ( 0.000000000000000000, -1.000000000000000000, -6.982962677686266711E-15 ) ) ;
#115214 = FACE_OUTER_BOUND ( 'NONE', #21962, .T. ) ;
#115215 = AXIS2_PLACEMENT_3D ( 'NONE', #240165, #138457, #217996 ) ;
#115216 = EDGE_LOOP ( 'NONE', ( #147546, #242067, #73152, #76356 ) ) ;
#115217 = DIRECTION ( 'NONE',  ( 1.000000000000000000, 0.000000000000000000, 0.000000000000000000 ) ) ;
#115218 = VERTEX_POINT ( 'NONE', #66150 ) ;
#115219 = DIRECTION ( 'NONE',  ( -0.000000000000000000, -0.000000000000000000, -1.000000000000000000 ) ) ;
#115220 = EDGE_CURVE ( 'NONE', #216057, #109854, #225201, .T. ) ;
#115222 = EDGE_LOOP ( 'NONE', ( #83597, #82185, #110480, #90800, #71716, #204965 ) ) ;
#115221 = CARTESIAN_POINT ( 'NONE',  ( 21.05000000000000071, 6.300183336278856849, -133.9486725676586616 ) ) ;
#115223 = DIRECTION ( 'NONE',  ( 0.000000000000000000, -6.308085367188367561E-15, 1.000000000000000000 ) ) ;
#115224 = ORIENTED_EDGE ( 'NONE', *, *, #63541, .T. ) ;
#115225 = ADVANCED_FACE ( 'NONE', ( #10986 ), #90508, .F. ) ;
#115226 = B_SPLINE_CURVE_WITH_KNOTS ( 'NONE', 3,
 ( #93803, #196754, #215043, #255396, #36436, #115954 ),
 .UNSPECIFIED., .F., .F.,
 ( 4, 2, 4 ),
 ( 0.000000000000000000, 0.0001568709654583423218, 0.0003137419309166846436 ),
 .UNSPECIFIED. ) ;
#115227 = ADVANCED_FACE ( 'NONE', ( #136039 ), #71515, .T. ) ;
#115228 = ORIENTED_EDGE ( 'NONE', *, *, #242261, .F. ) ;
#115230 = ORIENTED_EDGE ( 'NONE', *, *, #93518, .T. ) ;
#115229 = EDGE_LOOP ( 'NONE', ( #41339, #182814, #148099, #17157 ) ) ;
#115231 = DIRECTION ( 'NONE',  ( -2.557131231893036985E-16, 0.1022405907414164900, 0.9947597004326451664 ) ) ;
#115232 = ORIENTED_EDGE ( 'NONE', *, *, #198288, .F. ) ;
#115233 = DIRECTION ( 'NONE',  ( -1.000000000000000000, 0.000000000000000000, 0.000000000000000000 ) ) ;
#115235 = ORIENTED_EDGE ( 'NONE', *, *, #160011, .F. ) ;
#115234 = AXIS2_PLACEMENT_3D ( 'NONE', #229900, #109941, #129519 ) ;
#115236 = AXIS2_PLACEMENT_3D ( 'NONE', #42125, #83751, #40850 ) ;
#115237 = VECTOR ( 'NONE', #85150, 1000.000000000000000 ) ;
#115238 = ORIENTED_EDGE ( 'NONE', *, *, #151885, .F. ) ;
#115239 = CIRCLE ( 'NONE', #252603, 4.099999999999999645 ) ;
#115240 = ADVANCED_FACE ( 'NONE', ( #138603 ), #93041, .T. ) ;
#115241 = DIRECTION ( 'NONE',  ( 0.000000000000000000, 0.000000000000000000, -1.000000000000000000 ) ) ;
#115242 = DIRECTION ( 'NONE',  ( -1.000000000000000000, -1.836970198721029934E-16, -3.186635328391151676E-31 ) ) ;
#115243 = DIRECTION ( 'NONE',  ( 0.000000000000000000, 0.000000000000000000, 1.000000000000000000 ) ) ;
#115244 = VERTEX_POINT ( 'NONE', #237738 ) ;
#115245 = CIRCLE ( 'NONE', #23704, 0.3999999999999926392 ) ;
#115246 = DIRECTION ( 'NONE',  ( 1.000000000000000000, 0.000000000000000000, 0.000000000000000000 ) ) ;
#115247 = CIRCLE ( 'NONE', #235859, 0.1000000000000035305 ) ;
#115248 = DIRECTION ( 'NONE',  ( 1.000000000000000000, 0.000000000000000000, 0.000000000000000000 ) ) ;
#115249 = LINE ( 'NONE', #215620, #210464 ) ;
#115250 = ORIENTED_EDGE ( 'NONE', *, *, #25557, .T. ) ;
#115251 = CARTESIAN_POINT ( 'NONE',  ( -17.01825945287481545, 14.13772148853350252, -219.1573629999798811 ) ) ;
#115252 = CARTESIAN_POINT ( 'NONE',  ( -18.44232395689977722, 38.17981730268489571, -261.2023171126317607 ) ) ;
#115254 = DIRECTION ( 'NONE',  ( 0.000000000000000000, -1.000000000000000000, 0.000000000000000000 ) ) ;
#115253 = PRODUCT_RELATED_PRODUCT_CATEGORY ( 'part', '', ( #257766 ) ) ;
#115255 = EDGE_LOOP ( 'NONE', ( #182957, #44771, #214037, #47355 ) ) ;
#115256 = DIRECTION ( 'NONE',  ( 0.000000000000000000, 1.000000000000000000, 6.982962677686266711E-15 ) ) ;
#115257 = ORIENTED_EDGE ( 'NONE', *, *, #190113, .F. ) ;
#115258 = VERTEX_POINT ( 'NONE', #252151 ) ;
#115259 = AXIS2_PLACEMENT_3D ( 'NONE', #100811, #223361, #23921 ) ;
#115260 = AXIS2_PLACEMENT_3D ( 'NONE', #517, #239151, #60490 ) ;
#115261 = CIRCLE ( 'NONE', #215226, 0.2000000000000005107 ) ;
#115262 = DIRECTION ( 'NONE',  ( -2.915501640297154776E-16, 0.4721928772777348460, 0.8814952561688429444 ) ) ;
#115263 = VERTEX_POINT ( 'NONE', #218150 ) ;
#115264 = VERTEX_POINT ( 'NONE', #113931 ) ;
#115265 = CARTESIAN_POINT ( 'NONE',  ( -14.00000000000000178, 66.15000000001185754, -86.27310748452437394 ) ) ;
#115266 = ADVANCED_FACE ( 'NONE', ( #194786 ), #216879, .T. ) ;
#115267 = CARTESIAN_POINT ( 'NONE',  ( -16.93658211146644987, 9.994108662352344297, -188.4042950699556513 ) ) ;
#115268 = ORIENTED_EDGE ( 'NONE', *, *, #240821, .F. ) ;
#115269 = ADVANCED_FACE ( 'NONE', ( #154391 ), #253437, .F. ) ;
#115270 = ORIENTED_EDGE ( 'NONE', *, *, #25644, .T. ) ;
#115271 = DIRECTION ( 'NONE',  ( 0.000000000000000000, 0.000000000000000000, 1.000000000000000000 ) ) ;
#115272 = DIRECTION ( 'NONE',  ( 7.304098846218134667E-16, -1.000000000000000000, 0.000000000000000000 ) ) ;
#115273 = ORIENTED_EDGE ( 'NONE', *, *, #42579, .F. ) ;
#115274 = EDGE_CURVE ( 'NONE', #22565, #31535, #155670, .T. ) ;
#115275 = ORIENTED_EDGE ( 'NONE', *, *, #51399, .F. ) ;
#115276 = DIRECTION ( 'NONE',  ( -0.7070776581708965169, -0.7071359030027827286, -0.000000000000000000 ) ) ;
#115277 = FACE_OUTER_BOUND ( 'NONE', #21070, .T. ) ;
#115278 = LINE ( 'NONE', #190995, #221776 ) ;
#115279 = DIRECTION ( 'NONE',  ( 0.000000000000000000, -1.176083712526648525E-14, 1.000000000000000000 ) ) ;
#115280 = VECTOR ( 'NONE', #53969, 999.9999999999998863 ) ;
#115281 = DIRECTION ( 'NONE',  ( 0.000000000000000000, 0.3738317757009345654, 0.9274965247785492695 ) ) ;
#115282 = CARTESIAN_POINT ( 'NONE',  ( 23.14999999999999858, 5.000000000011153745, -121.5947339810869465 ) ) ;
#115283 = AXIS2_PLACEMENT_3D ( 'NONE', #77691, #239355, #159834 ) ;
#115285 = EDGE_CURVE ( 'NONE', #69698, #125644, #213850, .T. ) ;
#115284 = DIRECTION ( 'NONE',  ( -1.000000000000000000, -0.000000000000000000, -0.000000000000000000 ) ) ;
#115287 = PLANE ( 'NONE',  #49534 ) ;
#115286 = CARTESIAN_POINT ( 'NONE',  ( -18.50000000000000000, 15.92646454033039305, -219.3818586450342707 ) ) ;
#115289 = AXIS2_PLACEMENT_3D ( 'NONE', #13364, #109869, #147736 ) ;
#115288 = CARTESIAN_POINT ( 'NONE',  ( -22.39999999999999858, 0.1000000000111554016, -159.7092204016265384 ) ) ;
#115290 = CIRCLE ( 'NONE', #2854, 1.749999999999998002 ) ;
#115291 = LINE ( 'NONE', #57865, #198659 ) ;
#115292 = DIRECTION ( 'NONE',  ( 0.000000000000000000, -8.987377189994711700E-15, 1.000000000000000000 ) ) ;
#115293 = ORIENTED_EDGE ( 'NONE', *, *, #245430, .F. ) ;
#115294 = EDGE_CURVE ( 'NONE', #114960, #222885, #142898, .T. ) ;
#115296 = VERTEX_POINT ( 'NONE', #177792 ) ;
#115295 = DIRECTION ( 'NONE',  ( 0.000000000000000000, 0.000000000000000000, -1.000000000000000000 ) ) ;
#115297 = DIRECTION ( 'NONE',  ( 0.000000000000000000, 0.000000000000000000, 1.000000000000000000 ) ) ;
#115298 = ADVANCED_FACE ( 'NONE', ( #215593 ), #236447, .T. ) ;
#115299 = EDGE_CURVE ( 'NONE', #45873, #121232, #55584, .T. ) ;
#115300 = CARTESIAN_POINT ( 'NONE',  ( -16.97683809663752186, 9.850000000011137402, -120.5976359818037196 ) ) ;
#115301 = ORIENTED_EDGE ( 'NONE', *, *, #196082, .F. ) ;
#115302 = CIRCLE ( 'NONE', #36234, 11.70000000000001528 ) ;
#115303 = CYLINDRICAL_SURFACE ( 'NONE', #66519, 0.09999999999999648059 ) ;
#115304 = CARTESIAN_POINT ( 'NONE',  ( -16.95709691156204002, 9.950000000011062440, -54.33994243748958297 ) ) ;
#115305 = EDGE_LOOP ( 'NONE', ( #166512, #210868, #211093, #193604 ) ) ;
#115306 = AXIS2_PLACEMENT_3D ( 'NONE', #231200, #130786, #107368 ) ;
#115307 = EDGE_CURVE ( 'NONE', #86585, #56972, #94360, .T. ) ;
#115308 = CARTESIAN_POINT ( 'NONE',  ( 21.05193202509564543, 60.06742710682065933, -221.2999661778954419 ) ) ;
#115309 = CARTESIAN_POINT ( 'NONE',  ( -20.85000000000000142, -1.835859311432481045, -112.0044391687985694 ) ) ;
#115310 = ADVANCED_FACE ( 'NONE', ( #196054 ), #225897, .T. ) ;
#115311 = CARTESIAN_POINT ( 'NONE',  ( -20.64999999999999858, 7.150000000011155876, -179.8499999999999943 ) ) ;
#115313 = ORIENTED_EDGE ( 'NONE', *, *, #105712, .T. ) ;
#115312 = DIRECTION ( 'NONE',  ( 0.000000000000000000, 0.000000000000000000, -1.000000000000000000 ) ) ;
#115314 = CARTESIAN_POINT ( 'NONE',  ( -21.07971444708686093, 75.91217656369435929, -142.8528995661508532 ) ) ;
#115315 = EDGE_CURVE ( 'NONE', #37087, #158566, #163967, .T. ) ;
#115317 = ORIENTED_EDGE ( 'NONE', *, *, #33819, .F. ) ;
#115316 = DIRECTION ( 'NONE',  ( 0.000000000000000000, -0.9651348961777155289, 0.2617529984165037904 ) ) ;
#115318 = DIRECTION ( 'NONE',  ( 1.000000000000000000, 0.000000000000000000, 0.000000000000000000 ) ) ;
#115319 = LINE ( 'NONE', #237842, #141552 ) ;
#115320 = CARTESIAN_POINT ( 'NONE',  ( -18.59999999999999787, -9.321008403361290107, -7.235938249077882745 ) ) ;
#115321 = CARTESIAN_POINT ( 'NONE',  ( -18.50000000000000000, 77.16412189325286874, -61.60825939895269698 ) ) ;
#115322 = ADVANCED_FACE ( 'NONE', ( #202470 ), #251445, .T. ) ;
#115324 = DIRECTION ( 'NONE',  ( -1.000000000000000000, 0.000000000000000000, 0.000000000000000000 ) ) ;
#115323 = CARTESIAN_POINT ( 'NONE',  ( 21.14999999999999858, 12.71802988599559470, -223.5105008658000258 ) ) ;
#115325 = LINE ( 'NONE', #191047, #199432 ) ;
#115326 = CARTESIAN_POINT ( 'NONE',  ( -21.00448002041592233, 64.25000000001232081, -163.1747666222132409 ) ) ;
#115327 = CYLINDRICAL_SURFACE ( 'NONE', #222524, 11.79999999999999361 ) ;
#115328 = VECTOR ( 'NONE', #39405, 1000.000000000000000 ) ;
#115329 = CIRCLE ( 'NONE', #2898, 0.09999999999999520384 ) ;
#115330 = LINE ( 'NONE', #171494, #209842 ) ;
#115332 = ADVANCED_FACE ( 'NONE', ( #60374 ), #64239, .T. ) ;
#115331 = VECTOR ( 'NONE', #52327, 1000.000000000000000 ) ;
#115333 = CIRCLE ( 'NONE', #248611, 12.87500000000000000 ) ;
#115334 = EDGE_CURVE ( 'NONE', #124124, #209902, #118168, .T. ) ;
#115335 = ORIENTED_EDGE ( 'NONE', *, *, #54973, .T. ) ;
#115336 = DIRECTION ( 'NONE',  ( -2.915501640297152804E-16, -1.000000000000000000, -6.997203936713167125E-15 ) ) ;
#115337 = ORIENTED_EDGE ( 'NONE', *, *, #109292, .F. ) ;
#115338 = ORIENTED_EDGE ( 'NONE', *, *, #180098, .F. ) ;
#115339 = ADVANCED_FACE ( 'NONE', ( #179083 ), #42129, .T. ) ;
#115340 = DIRECTION ( 'NONE',  ( 0.000000000000000000, 0.2617529984165031243, 0.9651348961777158619 ) ) ;
#115341 = FACE_OUTER_BOUND ( 'NONE', #16702, .T. ) ;
#115342 = VERTEX_POINT ( 'NONE', #25135 ) ;
#115343 = EDGE_CURVE ( 'NONE', #38092, #104152, #64011, .T. ) ;
#115344 = ADVANCED_FACE ( 'NONE', ( #85048 ), #92658, .T. ) ;
#115345 = ORIENTED_EDGE ( 'NONE', *, *, #92606, .T. ) ;
#115346 = CIRCLE ( 'NONE', #148699, 0.5000000000000004441 ) ;
#115347 = PLANE ( 'NONE',  #152791 ) ;
#115348 = ADVANCED_FACE ( 'NONE', ( #220744 ), #394, .F. ) ;
#115349 = TOROIDAL_SURFACE ( 'NONE', #44059, 0.2000000000000000111, 0.1000000000000000056 ) ;
#115350 = CIRCLE ( 'NONE', #106976, 0.1000000000000028644 ) ;
#115351 = ORIENTED_EDGE ( 'NONE', *, *, #46232, .T. ) ;
#115352 = VERTEX_POINT ( 'NONE', #224586 ) ;
#115353 = CARTESIAN_POINT ( 'NONE',  ( 18.49999999999999289, 64.35000000001221565, -148.2731074845243882 ) ) ;
#115354 = CIRCLE ( 'NONE', #2921, 0.9750000000000036415 ) ;
#115355 = LINE ( 'NONE', #232757, #38668 ) ;
#115356 = DIRECTION ( 'NONE',  ( 1.000000000000000000, 0.000000000000000000, 0.000000000000000000 ) ) ;
#115358 = DIRECTION ( 'NONE',  ( 0.000000000000000000, -0.9968797965484670343, -0.07893460099023179299 ) ) ;
#115357 = CARTESIAN_POINT ( 'NONE',  ( -18.60000000000000142, 77.40559867739671063, -241.7331358027584827 ) ) ;
#115359 = PLANE ( 'NONE',  #128552 ) ;
#115361 = VERTEX_POINT ( 'NONE', #82482 ) ;
#115360 = CARTESIAN_POINT ( 'NONE',  ( -21.59142135623730852, 68.15000000001155911, -57.17310748452437963 ) ) ;
#115363 = DIRECTION ( 'NONE',  ( 0.000000000000000000, 0.9999176327611370985, -0.01283462868041289687 ) ) ;
#115362 = CARTESIAN_POINT ( 'NONE',  ( -23.15000000000000213, 11.75000000001115552, -33.50000000000000000 ) ) ;
#115364 = EDGE_CURVE ( 'NONE', #229929, #217493, #105091, .T. ) ;
#115365 = DIRECTION ( 'NONE',  ( -1.000000000000000000, 0.000000000000000000, 0.000000000000000000 ) ) ;
#115366 = ADVANCED_FACE ( 'NONE', ( #201178 ), #139900, .F. ) ;
#115367 = EDGE_LOOP ( 'NONE', ( #245027, #12904, #234185 ) ) ;
#115368 = DIRECTION ( 'NONE',  ( 0.000000000000000000, -0.9770955615654159931, -0.2128009952259723447 ) ) ;
#115369 = CARTESIAN_POINT ( 'NONE',  ( 23.14999999999999858, 7.128833340094563376, -233.7327013124401276 ) ) ;
#115370 = ORIENTED_EDGE ( 'NONE', *, *, #256860, .T. ) ;
#115371 = DIRECTION ( 'NONE',  ( -1.836970198721030427E-16, 0.4721928772777346239, 0.8814952561688430555 ) ) ;
#115372 = AXIS2_PLACEMENT_3D ( 'NONE', #150297, #168613, #91594 ) ;
#115373 = CARTESIAN_POINT ( 'NONE',  ( -21.05000000000000071, 76.00000000001192291, -100.1231074845243256 ) ) ;
#115374 = ORIENTED_EDGE ( 'NONE', *, *, #81437, .T. ) ;
#115375 = VERTEX_POINT ( 'NONE', #142478 ) ;
#115376 = DIRECTION ( 'NONE',  ( 0.000000000000000000, 0.000000000000000000, 1.000000000000000000 ) ) ;
#115377 = CARTESIAN_POINT ( 'NONE',  ( -23.15000000000000213, -8.999999999988846255, -109.8939691226524786 ) ) ;
#115378 = DIRECTION ( 'NONE',  ( 0.000000000000000000, 0.1290532225515392817, 0.9916376685811522096 ) ) ;
#115379 = CARTESIAN_POINT ( 'NONE',  ( -21.44999999999999929, 68.75000000001179501, -81.77310748452435973 ) ) ;
#115380 = VERTEX_POINT ( 'NONE', #22559 ) ;
#115381 = VECTOR ( 'NONE', #55701, 1000.000000000000000 ) ;
#115382 = SPHERICAL_SURFACE ( 'NONE', #58784, 0.1000000000000000056 ) ;
#115383 = DIRECTION ( 'NONE',  ( 4.377807931758639578E-15, -0.2605042016806606298, -0.9654727137038736640 ) ) ;
#115384 = CIRCLE ( 'NONE', #36306, 0.09999999999998898659 ) ;
#115385 = DIRECTION ( 'NONE',  ( 0.000000000000000000, 0.6728971962617388280, 0.7397360091702248619 ) ) ;
#115386 = EDGE_CURVE ( 'NONE', #126102, #136069, #221998, .T. ) ;
#115387 = CARTESIAN_POINT ( 'NONE',  ( -21.14999999999999858, 87.65000000001195701, -103.0231074845242318 ) ) ;
#115388 = AXIS2_PLACEMENT_3D ( 'NONE', #201763, #43982, #23165 ) ;
#115389 = AXIS2_PLACEMENT_3D ( 'NONE', #126847, #145107, #205077 ) ;
#115390 = EDGE_CURVE ( 'NONE', #38731, #224903, #39089, .T. ) ;
#115391 = DIRECTION ( 'NONE',  ( 0.000000000000000000, 0.8814952561688444987, -0.4721928772777320149 ) ) ;
#115392 = PRODUCT_DEFINITION_FORMATION_WITH_SPECIFIED_SOURCE ( 'ANY', '', #72353, .NOT_KNOWN. ) ;
#115394 = ORIENTED_EDGE ( 'NONE', *, *, #92308, .T. ) ;
#115393 = CARTESIAN_POINT ( 'NONE',  ( -16.87036670365549540, 66.01058118071094327, -191.0026676018264880 ) ) ;
#115395 = DIRECTION ( 'NONE',  ( 0.000000000000000000, 0.1568667991644863147, -0.9876197685951252359 ) ) ;
#115396 = CIRCLE ( 'NONE', #165496, 0.09999999999999695244 ) ;
#115397 = CARTESIAN_POINT ( 'NONE',  ( 18.59999999999999432, -1.835859311443637010, -45.00443916879852679 ) ) ;
#115398 = CARTESIAN_POINT ( 'NONE',  ( -23.25000000000000355, 11.75000000001113953, -109.7500000000000426 ) ) ;
#115399 = DIRECTION ( 'NONE',  ( 1.000000000000000000, -0.000000000000000000, -0.000000000000000000 ) ) ;
#115400 = TOROIDAL_SURFACE ( 'NONE', #27967, 4.099999999999999645, 0.1000000000000000056 ) ;
#115401 = CARTESIAN_POINT ( 'NONE',  ( 18.52928932188133970, 10.27928932188134326, -24.70857864376268509 ) ) ;
#115403 = EDGE_LOOP ( 'NONE', ( #152489, #67337, #236692, #255143 ) ) ;
#115402 = CARTESIAN_POINT ( 'NONE',  ( -18.59999999999999787, -1.835859311443640340, -45.00443916879852679 ) ) ;
#115404 = DIRECTION ( 'NONE',  ( 1.000000000000000000, 0.000000000000000000, 0.000000000000000000 ) ) ;
#115405 = DIRECTION ( 'NONE',  ( 1.000000000000000000, 0.000000000000000000, 0.000000000000000000 ) ) ;
#115406 = ORIENTED_EDGE ( 'NONE', *, *, #13954, .F. ) ;
#115407 = CARTESIAN_POINT ( 'NONE',  ( -21.04999999999994387, 67.82483145523551116, -25.59432346794077162 ) ) ;
#115408 = LINE ( 'NONE', #94557, #123414 ) ;
#115409 = CARTESIAN_POINT ( 'NONE',  ( 21.05000000000000071, 69.56804783242856161, -248.4091712263733882 ) ) ;
#115410 = LINE ( 'NONE', #171575, #221051 ) ;
#115411 = EDGE_CURVE ( 'NONE', #196055, #111741, #171809, .T. ) ;
#115412 = CARTESIAN_POINT ( 'NONE',  ( -18.48550754432065801, 78.20977376872917830, -231.5291668078544376 ) ) ;
#115413 = AXIS2_PLACEMENT_3D ( 'NONE', #237305, #14428, #93930 ) ;
#115414 = CIRCLE ( 'NONE', #207003, 11.65000000000001457 ) ;
#115415 = EDGE_LOOP ( 'NONE', ( #105867, #173108, #8897, #49452 ) ) ;
#115416 = VERTEX_POINT ( 'NONE', #100748 ) ;
#115417 = AXIS2_PLACEMENT_3D ( 'NONE', #142289, #101860, #43204 ) ;
#115418 = CARTESIAN_POINT ( 'NONE',  ( -20.65000000000000568, 7.250000000011138646, -87.85000000000003695 ) ) ;
#115419 = CARTESIAN_POINT ( 'NONE',  ( 20.99999999999999645, 9.750000000011137757, -176.7499999999999716 ) ) ;
#115420 = AXIS2_PLACEMENT_3D ( 'NONE', #53923, #176461, #255917 ) ;
#115421 = DIRECTION ( 'NONE',  ( 0.000000000000000000, -7.429790795770652649E-15, 1.000000000000000000 ) ) ;
#115422 = DIRECTION ( 'NONE',  ( 1.000000000000000000, 0.000000000000000000, 0.000000000000000000 ) ) ;
#115423 = VECTOR ( 'NONE', #46886, 1000.000000000000000 ) ;
#115424 = CIRCLE ( 'NONE', #15506, 0.09999999999999602263 ) ;
#115425 = DIRECTION ( 'NONE',  ( 1.000000000000000000, 0.000000000000000000, 0.000000000000000000 ) ) ;
#115426 = DIRECTION ( 'NONE',  ( 0.000000000000000000, 1.000000000000000000, 0.000000000000000000 ) ) ;
#115427 = CARTESIAN_POINT ( 'NONE',  ( -16.93339986808596720, 10.00510392857707664, -113.0659936718128904 ) ) ;
#115428 = DIRECTION ( 'NONE',  ( -0.000000000000000000, -0.000000000000000000, -1.000000000000000000 ) ) ;
#115429 = TOROIDAL_SURFACE ( 'NONE', #86192, 11.65000000000000036, 0.1000000000000000056 ) ;
#115430 = AXIS2_PLACEMENT_3D ( 'NONE', #93568, #214795, #92277 ) ;
#115431 = ORIENTED_EDGE ( 'NONE', *, *, #118304, .F. ) ;
#115432 = DIRECTION ( 'NONE',  ( 0.000000000000000000, 3.469446951953995998E-14, 1.000000000000000000 ) ) ;
#115433 = ORIENTED_EDGE ( 'NONE', *, *, #20114, .T. ) ;
#115434 = ORIENTED_EDGE ( 'NONE', *, *, #17879, .F. ) ;
#115435 = CARTESIAN_POINT ( 'NONE',  ( -21.04999999999999716, 85.60000000001210196, -129.4910380878245633 ) ) ;
#115436 = DIRECTION ( 'NONE',  ( 0.000000000000000000, 0.000000000000000000, -1.000000000000000000 ) ) ;
#115437 = CARTESIAN_POINT ( 'NONE',  ( -17.11825945287482753, 66.05000000001187743, -90.27310748452438816 ) ) ;
#115439 = ORIENTED_EDGE ( 'NONE', *, *, #241057, .F. ) ;
#115438 = DIRECTION ( 'NONE',  ( 1.000000000000000000, 3.265361837132813093E-16, -0.000000000000000000 ) ) ;
#115440 = CARTESIAN_POINT ( 'NONE',  ( 20.94999999999999574, 77.73625713160946304, -124.9544551555067926 ) ) ;
#115441 = CYLINDRICAL_SURFACE ( 'NONE', #105315, 0.1000000000000028644 ) ;
#115442 = DIRECTION ( 'NONE',  ( -0.000000000000000000, 0.9126074666063769270, 0.4088369013363280513 ) ) ;
#115443 = ADVANCED_FACE ( 'NONE', ( #1680 ), #192625, .F. ) ;
#115444 = ORIENTED_EDGE ( 'NONE', *, *, #104944, .T. ) ;
#115445 = CARTESIAN_POINT ( 'NONE',  ( 20.95000000000005258, 66.25000000001119815, -5.923107484524795296 ) ) ;
#115446 = CIRCLE ( 'NONE', #111359, 0.1000000000000064587 ) ;
#115447 = CARTESIAN_POINT ( 'NONE',  ( 18.59999999999999076, 65.50857864377491069, -145.2731074845244166 ) ) ;
#115449 = EDGE_CURVE ( 'NONE', #129536, #243362, #30712, .T. ) ;
#115448 = CARTESIAN_POINT ( 'NONE',  ( -18.59999999999999787, 68.87972903831452243, -132.8635444426850825 ) ) ;
#115450 = AXIS2_PLACEMENT_3D ( 'NONE', #9466, #109838, #130692 ) ;
#115451 = CARTESIAN_POINT ( 'NONE',  ( -18.43473496883401097, 85.49495241101172383, -162.9772359122965781 ) ) ;
#115452 = EDGE_LOOP ( 'NONE', ( #245908, #69176, #18884, #212450 ) ) ;
#115453 = CIRCLE ( 'NONE', #232007, 4.150000000000001243 ) ;
#115454 = CARTESIAN_POINT ( 'NONE',  ( -21.05000000000000071, 76.00000000001195133, -103.0231074845243171 ) ) ;
#115456 = EDGE_CURVE ( 'NONE', #247087, #75163, #59297, .T. ) ;
#115455 = DIRECTION ( 'NONE',  ( -0.000000000000000000, -0.9910827722268049644, -0.1332476588733589318 ) ) ;
#115457 = VERTEX_POINT ( 'NONE', #169803 ) ;
#115458 = CARTESIAN_POINT ( 'NONE',  ( 21.09316766718127667, 6.370153312485567376, -133.9607365976853259 ) ) ;
#115460 = EDGE_CURVE ( 'NONE', #118204, #136977, #255492, .T. ) ;
#115459 = DIRECTION ( 'NONE',  ( -0.000000000000000000, -0.3850724248243104775, 0.9228863568391969530 ) ) ;
#115461 = LINE ( 'NONE', #243118, #159744 ) ;
#115462 = AXIS2_PLACEMENT_3D ( 'NONE', #139909, #199926, #104619 ) ;
#115463 = AXIS2_PLACEMENT_3D ( 'NONE', #124256, #224613, #45982 ) ;
#115464 = ORIENTED_EDGE ( 'NONE', *, *, #218653, .F. ) ;
#115466 = CIRCLE ( 'NONE', #190322, 0.1000000000000028644 ) ;
#115465 = CARTESIAN_POINT ( 'NONE',  ( 23.14999999999999503, 63.99342642423710714, -222.3880800784493772 ) ) ;
#115467 = CARTESIAN_POINT ( 'NONE',  ( -18.59999999999999787, 11.75000000001115197, -79.15000000000004832 ) ) ;
#115468 = CIRCLE ( 'NONE', #236279, 4.300000000000025580 ) ;
#115469 = EDGE_CURVE ( 'NONE', #254425, #64641, #246716, .T. ) ;
#115470 = EDGE_LOOP ( 'NONE', ( #69305, #189990 ) ) ;
#115471 = CIRCLE ( 'NONE', #215436, 0.09999999999999939493 ) ;
#115472 = ORIENTED_EDGE ( 'NONE', *, *, #187862, .T. ) ;
#115473 = DIRECTION ( 'NONE',  ( 1.000000000000000000, -0.000000000000000000, -0.000000000000000000 ) ) ;
#115475 = EDGE_CURVE ( 'NONE', #136961, #47997, #209759, .T. ) ;
#115474 = LINE ( 'NONE', #213285, #150319 ) ;
#115477 = ORIENTED_EDGE ( 'NONE', *, *, #136852, .T. ) ;
#115476 = CARTESIAN_POINT ( 'NONE',  ( -20.54999999999999716, 2.000000000011154189, -113.2246219227621395 ) ) ;
#115478 = DIRECTION ( 'NONE',  ( 0.000000000000000000, -0.2128009952263403282, 0.9770955615653358350 ) ) ;
#115479 = CARTESIAN_POINT ( 'NONE',  ( -20.94403535211772294, 65.69367753730678317, -131.0189238066348594 ) ) ;
#115480 = FACE_OUTER_BOUND ( 'NONE', #218648, .T. ) ;
#115481 = LINE ( 'NONE', #174225, #145 ) ;
#115482 = AXIS2_PLACEMENT_3D ( 'NONE', #79177, #139137, #117048 ) ;
#115483 = DIRECTION ( 'NONE',  ( 1.000000000000000000, 0.000000000000000000, 0.000000000000000000 ) ) ;
#115484 = CARTESIAN_POINT ( 'NONE',  ( -20.94999999999999929, -1.835341550213255957, -112.0551512925630107 ) ) ;
#115485 = B_SPLINE_CURVE_WITH_KNOTS ( 'NONE', 3,
 ( #98838, #20645, #97561, #100130 ),
 .UNSPECIFIED., .F., .F.,
 ( 4, 4 ),
 ( 0.000000000000000000, 0.001767853679387116229 ),
 .UNSPECIFIED. ) ;
#115487 = ORIENTED_EDGE ( 'NONE', *, *, #102290, .F. ) ;
#115486 = CARTESIAN_POINT ( 'NONE',  ( 21.05000000000000071, 8.876614585098254295, -142.3850804788447135 ) ) ;
#115489 = ORIENTED_EDGE ( 'NONE', *, *, #31730, .F. ) ;
#115488 = CARTESIAN_POINT ( 'NONE',  ( -20.64999999999999858, 71.75000000001259082, -191.1731074845243654 ) ) ;
#115491 = DIRECTION ( 'NONE',  ( 9.044546369203339308E-15, -0.7397360091702694929, -0.6728971962616898672 ) ) ;
#115490 = CARTESIAN_POINT ( 'NONE',  ( -16.87036670365549895, 60.86740053880574663, -221.1564527318009254 ) ) ;
#115492 = ORIENTED_EDGE ( 'NONE', *, *, #189408, .T. ) ;
#115493 = ORIENTED_EDGE ( 'NONE', *, *, #41723, .F. ) ;
#115494 = CARTESIAN_POINT ( 'NONE',  ( -18.55121869061588669, 10.32747123227773045, -106.0774032850249853 ) ) ;
#115495 = DIRECTION ( 'NONE',  ( 0.000000000000000000, 0.000000000000000000, -1.000000000000000000 ) ) ;
#115496 = AXIS2_PLACEMENT_3D ( 'NONE', #239251, #24077, #103561 ) ;
#115497 = DIRECTION ( 'NONE',  ( -0.000000000000000000, 0.000000000000000000, -1.000000000000000000 ) ) ;
#115498 = DIRECTION ( 'NONE',  ( 1.000000000000000000, 0.000000000000000000, 0.000000000000000000 ) ) ;
#115499 = DIRECTION ( 'NONE',  ( 1.000000000000000000, -2.952720810173289112E-16, -2.061873921506763405E-30 ) ) ;
#115500 = LINE ( 'NONE', #37279, #136390 ) ;
#115501 = DIRECTION ( 'NONE',  ( -1.000000000000000000, 0.000000000000000000, -0.000000000000000000 ) ) ;
#115502 = ORIENTED_EDGE ( 'NONE', *, *, #76755, .F. ) ;
#115503 = ORIENTED_EDGE ( 'NONE', *, *, #54382, .F. ) ;
#115504 = CARTESIAN_POINT ( 'NONE',  ( 21.05000000000000071, 30.86266526676358879, -252.1316881318525986 ) ) ;
#115505 = AXIS2_PLACEMENT_3D ( 'NONE', #198138, #78178, #100301 ) ;
#115506 = CIRCLE ( 'NONE', #3073, 0.09999999999999854838 ) ;
#115507 = VERTEX_POINT ( 'NONE', #27721 ) ;
#115508 = CIRCLE ( 'NONE', #64100, 0.09999999999999939493 ) ;
#115510 = CARTESIAN_POINT ( 'NONE',  ( -23.15000000000000213, 1.115600667400684642E-11, -67.00000000000004263 ) ) ;
#115509 = CIRCLE ( 'NONE', #111429, 0.1000000000000028644 ) ;
#115511 = CARTESIAN_POINT ( 'NONE',  ( -18.50000000000000000, 64.35000000001247145, -181.7731074845244450 ) ) ;
#115513 = EDGE_CURVE ( 'NONE', #197418, #242821, #143091, .T. ) ;
#115512 = DIRECTION ( 'NONE',  ( 0.000000000000000000, 0.000000000000000000, 1.000000000000000000 ) ) ;
#115514 = CARTESIAN_POINT ( 'NONE',  ( -16.94445028196808778, 9.992063609708889516, -79.60733017841850767 ) ) ;
#115515 = ORIENTED_EDGE ( 'NONE', *, *, #168710, .T. ) ;
#115516 = CARTESIAN_POINT ( 'NONE',  ( -12.33960340485503693, 66.63925083009691264, -119.2085373439170866 ) ) ;
#115517 = ORIENTED_EDGE ( 'NONE', *, *, #110289, .T. ) ;
#115519 = EDGE_CURVE ( 'NONE', #181381, #118267, #163403, .T. ) ;
#115518 = DIRECTION ( 'NONE',  ( -0.000000000000000000, 0.4721928772777345684, 0.8814952561688429444 ) ) ;
#115520 = ORIENTED_EDGE ( 'NONE', *, *, #236251, .F. ) ;
#115521 = DIRECTION ( 'NONE',  ( 0.000000000000000000, 0.000000000000000000, 1.000000000000000000 ) ) ;
#115522 = CARTESIAN_POINT ( 'NONE',  ( 22.60000000000000142, -2.401771312552908544, -189.4980873520049727 ) ) ;
#115523 = ADVANCED_FACE ( 'NONE', ( #86335 ), #147625, .F. ) ;
#115524 = CARTESIAN_POINT ( 'NONE',  ( 18.59999999999999076, 11.65000000001115943, -88.75000000000004263 ) ) ;
#115525 = CIRCLE ( 'NONE', #78115, 0.5000000000000004441 ) ;
#115526 = EDGE_CURVE ( 'NONE', #201406, #136022, #250569, .T. ) ;
#115527 = VERTEX_POINT ( 'NONE', #227156 ) ;
#115529 = DIRECTION ( 'NONE',  ( -1.000000000000000000, -0.000000000000000000, -0.000000000000000000 ) ) ;
#115528 = CIRCLE ( 'NONE', #36468, 0.1000000000000046685 ) ;
#115531 = ORIENTED_EDGE ( 'NONE', *, *, #31674, .F. ) ;
#115530 = DIRECTION ( 'NONE',  ( 1.000000000000000000, 0.000000000000000000, 0.000000000000000000 ) ) ;
#115532 = CARTESIAN_POINT ( 'NONE',  ( -20.94999999999999929, 77.83534155023627932, -91.46795619196130644 ) ) ;
#115533 = ORIENTED_EDGE ( 'NONE', *, *, #147826, .T. ) ;
#115534 = CIRCLE ( 'NONE', #128033, 0.09999999999999939493 ) ;
#115535 = ORIENTED_EDGE ( 'NONE', *, *, #212159, .F. ) ;
#115536 = CARTESIAN_POINT ( 'NONE',  ( 21.05000000000000071, 0.000000000000000000, -35.40000000000000568 ) ) ;
#115537 = ORIENTED_EDGE ( 'NONE', *, *, #35578, .F. ) ;
#115538 = EDGE_CURVE ( 'NONE', #59396, #6487, #71954, .T. ) ;
#115539 = CARTESIAN_POINT ( 'NONE',  ( -20.64999999999999858, -8.663551401869161950, -9.524101118067305194 ) ) ;
#115540 = DIRECTION ( 'NONE',  ( 0.000000000000000000, -0.000000000000000000, -1.000000000000000000 ) ) ;
#115541 = CARTESIAN_POINT ( 'NONE',  ( -20.94999999999999929, 1.115600667400684642E-11, -167.5000000000000284 ) ) ;
#115542 = CARTESIAN_POINT ( 'NONE',  ( -23.25000000000000000, 64.25000000001244871, -170.0231074845244166 ) ) ;
#115543 = ADVANCED_FACE ( 'NONE', ( #68091 ), #105903, .T. ) ;
#115544 = DIRECTION ( 'NONE',  ( 0.000000000000000000, -6.982962677686266711E-15, 1.000000000000000000 ) ) ;
#115545 = B_SPLINE_CURVE_WITH_KNOTS ( 'NONE', 3,
 ( #221617, #132480, #128638, #33418, #229021, #252402, #188590, #54212 ),
 .UNSPECIFIED., .F., .F.,
 ( 4, 2, 2, 4 ),
 ( 0.000000000000000000, 0.0001306511400391407042, 0.0001959767100587063806, 0.0002613022800782720300 ),
 .UNSPECIFIED. ) ;
#115546 = ORIENTED_EDGE ( 'NONE', *, *, #198361, .F. ) ;
#115547 = CARTESIAN_POINT ( 'NONE',  ( 21.05000000000000071, 11.75000000000000711, -26.48519422934605316 ) ) ;
#115548 = CARTESIAN_POINT ( 'NONE',  ( -20.85000000106584750, 64.25000000001195133, -109.8676028280505790 ) ) ;
#115549 = DIRECTION ( 'NONE',  ( 1.000000000000000000, 0.000000000000000000, 0.000000000000000000 ) ) ;
#115550 = CIRCLE ( 'NONE', #244723, 0.09999999999999917288 ) ;
#115551 = VERTEX_POINT ( 'NONE', #146329 ) ;
#115552 = CARTESIAN_POINT ( 'NONE',  ( 20.87600722750343252, 68.10911674539558192, -224.1414149070238864 ) ) ;
#115553 = ORIENTED_EDGE ( 'NONE', *, *, #19684, .F. ) ;
#115554 = DIRECTION ( 'NONE',  ( 0.000000000000000000, -6.938893903907222067E-15, 1.000000000000000000 ) ) ;
#115555 = AXIS2_PLACEMENT_3D ( 'NONE', #124548, #184492, #60688 ) ;
#115556 = ORIENTED_EDGE ( 'NONE', *, *, #178987, .F. ) ;
#115557 = DIRECTION ( 'NONE',  ( 1.000000000000000000, 0.000000000000000000, 0.000000000000000000 ) ) ;
#115558 = DIRECTION ( 'NONE',  ( 1.000000000000000000, 1.836970198721029934E-16, -0.000000000000000000 ) ) ;
#115559 = EDGE_CURVE ( 'NONE', #147057, #219071, #84818, .T. ) ;
#115561 = ORIENTED_EDGE ( 'NONE', *, *, #201541, .T. ) ;
#115560 = CYLINDRICAL_SURFACE ( 'NONE', #136237, 0.1000000000000028644 ) ;
#115562 = ADVANCED_FACE ( 'NONE', ( #87633 ), #8125, .T. ) ;
#115563 = CARTESIAN_POINT ( 'NONE',  ( -18.46093223321767596, 8.897120040860684753, -245.4351526656046758 ) ) ;
#115564 = ORIENTED_EDGE ( 'NONE', *, *, #88989, .T. ) ;
#115565 = EDGE_CURVE ( 'NONE', #188452, #97404, #130063, .T. ) ;
#115566 = AXIS2_PLACEMENT_3D ( 'NONE', #179566, #81685, #160006 ) ;
#115567 = CARTESIAN_POINT ( 'NONE',  ( -20.54999999999999716, 70.22209180797715078, -215.6584443947398313 ) ) ;
#115568 = CARTESIAN_POINT ( 'NONE',  ( -16.77431908686106254, 9.945805754529134290, -113.1641607823497964 ) ) ;
#115569 = ORIENTED_EDGE ( 'NONE', *, *, #83471, .F. ) ;
#115570 = AXIS2_PLACEMENT_3D ( 'NONE', #249214, #91423, #250479 ) ;
#115571 = CARTESIAN_POINT ( 'NONE',  ( -23.15000000000000213, -9.599999999988845900, -57.10603087734755690 ) ) ;
#115572 = CARTESIAN_POINT ( 'NONE',  ( -20.99749315643151348, 11.75000000001115197, -193.9851942312420192 ) ) ;
#115573 = ORIENTED_EDGE ( 'NONE', *, *, #21439, .F. ) ;
#115574 = CARTESIAN_POINT ( 'NONE',  ( 21.09096482362047098, 10.09888019307431684, -228.1046399456574818 ) ) ;
#115575 = TOROIDAL_SURFACE ( 'NONE', #219805, 0.2000000000000000111, 0.1000000000000000056 ) ;
#115576 = CIRCLE ( 'NONE', #86323, 0.09999999999998898659 ) ;
#115577 = EDGE_LOOP ( 'NONE', ( #92971, #118193 ) ) ;
#115578 = CARTESIAN_POINT ( 'NONE',  ( -20.94999999999999929, 87.41227409416205774, -167.0231074845242745 ) ) ;
#115580 = CARTESIAN_POINT ( 'NONE',  ( -22.59999999999999787, 64.25012875563587045, -170.0885370755381132 ) ) ;
#115579 = CIRCLE ( 'NONE', #228212, 0.09999999999999363565 ) ;
#115581 = ADVANCED_FACE ( 'NONE', ( #248000 ), #230026, .T. ) ;
#115582 = CIRCLE ( 'NONE', #223724, 0.09999999999999892308 ) ;
#115584 = EDGE_LOOP ( 'NONE', ( #164346, #255445, #40242, #26782 ) ) ;
#115583 = DIRECTION ( 'NONE',  ( -0.7071067811865475727, -0.7071067811865475727, 0.000000000000000000 ) ) ;
#115585 = CARTESIAN_POINT ( 'NONE',  ( 23.15000000000000213, 85.60000000001159037, -59.62913836187181005 ) ) ;
#115586 = CARTESIAN_POINT ( 'NONE',  ( -18.59999999999999787, 67.85909929089923764, -227.8797997985275856 ) ) ;
#115588 = EDGE_CURVE ( 'NONE', #6826, #209310, #84224, .T. ) ;
#115587 = CARTESIAN_POINT ( 'NONE',  ( 20.46382478191414833, 67.09862044130927927, -94.47737938964125703 ) ) ;
#115590 = CARTESIAN_POINT ( 'NONE',  ( -20.54999999999999716, 74.00000000001259082, -190.2984855617622770 ) ) ;
#115589 = CARTESIAN_POINT ( 'NONE',  ( -20.85000000000000142, 68.87972903831379767, -32.36354444268504693 ) ) ;
#115591 = FACE_OUTER_BOUND ( 'NONE', #223308, .T. ) ;
#115592 = DIRECTION ( 'NONE',  ( 1.000000000000000000, 0.000000000000000000, 0.000000000000000000 ) ) ;
#115593 = AXIS2_PLACEMENT_3D ( 'NONE', #252683, #156197, #195323 ) ;
#115594 = DIRECTION ( 'NONE',  ( 0.000000000000000000, -0.000000000000000000, -1.000000000000000000 ) ) ;
#115595 = DIRECTION ( 'NONE',  ( 1.000000000000000000, 1.836970198721029934E-16, 3.186635328391151676E-31 ) ) ;
#115596 = VECTOR ( 'NONE', #133843, 1000.000000000000000 ) ;
#115597 = ORIENTED_EDGE ( 'NONE', *, *, #223462, .T. ) ;
#115598 = VERTEX_POINT ( 'NONE', #208883 ) ;
#115599 = AXIS2_PLACEMENT_3D ( 'NONE', #32598, #91253, #70436 ) ;
#115600 = VECTOR ( 'NONE', #104639, 1000.000000000000000 ) ;
#115602 = VERTEX_POINT ( 'NONE', #109773 ) ;
#115601 = CARTESIAN_POINT ( 'NONE',  ( -21.10000000000000142, 5.021051876504148371E-16, -4.100000000000000533 ) ) ;
#115603 = AXIS2_PLACEMENT_3D ( 'NONE', #71913, #211411, #172333 ) ;
#115604 = ORIENTED_EDGE ( 'NONE', *, *, #108831, .T. ) ;
#115605 = EDGE_CURVE ( 'NONE', #44096, #242024, #189332, .T. ) ;
#115606 = DIRECTION ( 'NONE',  ( 0.000000000000000000, -1.000000000000000000, 0.000000000000000000 ) ) ;
#115607 =( BOUNDED_CURVE ( )  B_SPLINE_CURVE ( 3, ( #38771, #118311, #197827, #19200 ),
 .UNSPECIFIED., .F., .F. ) 
 B_SPLINE_CURVE_WITH_KNOTS ( ( 4, 4 ),
 ( 3.141592653589791784, 4.712388980384628390 ),
 .UNSPECIFIED. ) 
 CURVE ( )  GEOMETRIC_REPRESENTATION_ITEM ( )  RATIONAL_B_SPLINE_CURVE ( ( 1.000000000000000000, 0.8047378541243791483, 0.8047378541243791483, 1.000000000000000000 ) ) 
 REPRESENTATION_ITEM ( '' )  );
#115608 = ORIENTED_EDGE ( 'NONE', *, *, #104091, .T. ) ;
#115609 = CARTESIAN_POINT ( 'NONE',  ( 18.39999999999998082, 13.17878477875124865, -207.5966336730521391 ) ) ;
#115610 = AXIS2_PLACEMENT_3D ( 'NONE', #32518, #10363, #70354 ) ;
#115611 = ADVANCED_FACE ( 'NONE', ( #17128 ), #117611, .F. ) ;
#115612 = EDGE_LOOP ( 'NONE', ( #175447, #246915, #41127, #176821, #150693 ) ) ;
#115614 = EDGE_CURVE ( 'NONE', #151389, #168873, #172387, .T. ) ;
#115613 = CARTESIAN_POINT ( 'NONE',  ( 0.000000000000000000, 1.350000000000000089, 21.90000000000000213 ) ) ;
#115617 = ORIENTED_EDGE ( 'NONE', *, *, #256209, .F. ) ;
#115616 = VERTEX_POINT ( 'NONE', #117494 ) ;
#115615 = AXIS2_PLACEMENT_3D ( 'NONE', #41592, #121136, #200645 ) ;
#115618 = VERTEX_POINT ( 'NONE', #73261 ) ;
#115619 = AXIS2_PLACEMENT_3D ( 'NONE', #87507, #125378, #143641 ) ;
#115620 = CIRCLE ( 'NONE', #132382, 11.64999999999999325 ) ;
#115621 = ORIENTED_EDGE ( 'NONE', *, *, #177512, .F. ) ;
#115622 = ORIENTED_EDGE ( 'NONE', *, *, #191504, .F. ) ;
#115623 = EDGE_CURVE ( 'NONE', #123658, #182622, #238985, .T. ) ;
#115624 = CARTESIAN_POINT ( 'NONE',  ( 20.04142135623731136, 64.25000000001176659, -78.25595019699900945 ) ) ;
#115625 = DIRECTION ( 'NONE',  ( 0.7071359030028288029, 0.000000000000000000, 0.7070776581708504427 ) ) ;
#115628 = ADVANCED_FACE ( 'NONE', ( #75798 ), #53664, .T. ) ;
#115627 = ORIENTED_EDGE ( 'NONE', *, *, #166267, .F. ) ;
#115626 = CARTESIAN_POINT ( 'NONE',  ( -16.87036670365549895, 66.01058118071065905, -157.5026676018264880 ) ) ;
#115629 = CARTESIAN_POINT ( 'NONE',  ( -22.47007471830799119, 33.50241300269673417, -242.5051845127899526 ) ) ;
#115630 = CARTESIAN_POINT ( 'NONE',  ( 21.05000000000000071, 76.00000000001142553, -36.02310748452432421 ) ) ;
#115632 = EDGE_LOOP ( 'NONE', ( #193188, #70822, #37419, #175213 ) ) ;
#115631 = CARTESIAN_POINT ( 'NONE',  ( -16.94275863009466576, 60.89032433645830622, -221.0716331249102495 ) ) ;
#115633 = CARTESIAN_POINT ( 'NONE',  ( -13.40000000000000213, -11.65000000000000036, 12.30000000000000426 ) ) ;
#115634 = ORIENTED_EDGE ( 'NONE', *, *, #215535, .T. ) ;
#115635 = DIRECTION ( 'NONE',  ( -0.000000000000000000, -1.000000000000000000, -8.609265936414532828E-15 ) ) ;
#115637 = VERTEX_POINT ( 'NONE', #97890 ) ;
#115636 = FACE_OUTER_BOUND ( 'NONE', #25801, .T. ) ;
#115638 = VECTOR ( 'NONE', #221474, 1000.000000000000000 ) ;
#115639 = CARTESIAN_POINT ( 'NONE',  ( -23.15000000000000213, 87.65000000001246860, -173.1231074845242688 ) ) ;
#115640 = CARTESIAN_POINT ( 'NONE',  ( -20.64999999999999858, 74.07476635515175190, -56.79286395139820343 ) ) ;
#115641 = AXIS2_PLACEMENT_3D ( 'NONE', #209955, #187828, #206090 ) ;
#115642 = CARTESIAN_POINT ( 'NONE',  ( 20.04142135623731136, 11.75000000001116263, -91.65000000000004832 ) ) ;
#115643 = EDGE_LOOP ( 'NONE', ( #42414, #155452, #175192, #140026 ) ) ;
#115645 = DIRECTION ( 'NONE',  ( 1.000000000000000000, -0.000000000000000000, -0.000000000000000000 ) ) ;
#115644 = DIRECTION ( 'NONE',  ( 0.000000000000000000, -0.9910827722268050755, 0.1332476588733589318 ) ) ;
#115646 = AXIS2_PLACEMENT_3D ( 'NONE', #202638, #163520, #243048 ) ;
#115647 = EDGE_CURVE ( 'NONE', #65528, #14901, #184233, .T. ) ;
#115648 = CARTESIAN_POINT ( 'NONE',  ( -18.59999999999999787, -1.835859311432484375, -179.0044391687985410 ) ) ;
#115649 = CARTESIAN_POINT ( 'NONE',  ( 23.14999999999999858, 36.65892442174935439, -249.5511627012433848 ) ) ;
#115650 = EDGE_CURVE ( 'NONE', #181805, #154400, #209359, .T. ) ;
#115651 = ORIENTED_EDGE ( 'NONE', *, *, #251682, .T. ) ;
#115652 = ORIENTED_EDGE ( 'NONE', *, *, #126168, .F. ) ;
#115653 = VECTOR ( 'NONE', #157010, 1000.000000000000000 ) ;
#115654 = CARTESIAN_POINT ( 'NONE',  ( 21.05000000000000071, 8.926614585087097709, -8.471683019223119615 ) ) ;
#115655 = CARTESIAN_POINT ( 'NONE',  ( -18.34374000495059676, 62.50563584222673796, -209.4474707446456421 ) ) ;
#115656 = ORIENTED_EDGE ( 'NONE', *, *, #127896, .T. ) ;
#115657 = FACE_OUTER_BOUND ( 'NONE', #183577, .T. ) ;
#115658 = ORIENTED_EDGE ( 'NONE', *, *, #47715, .F. ) ;
#115659 = EDGE_CURVE ( 'NONE', #128029, #213316, #100980, .T. ) ;
#115660 = DIRECTION ( 'NONE',  ( 1.000000000000000000, 0.000000000000000000, 0.000000000000000000 ) ) ;
#115661 = CYLINDRICAL_SURFACE ( 'NONE', #96082, 4.000000000000003553 ) ;
#115662 = AXIS2_PLACEMENT_3D ( 'NONE', #157301, #158584, #20357 ) ;
#115663 = CIRCLE ( 'NONE', #207262, 0.09999999999999939493 ) ;
#115664 = VECTOR ( 'NONE', #38395, 1000.000000000000000 ) ;
#115665 = EDGE_LOOP ( 'NONE', ( #253652, #86988, #117476, #64292, #96473 ) ) ;
#115666 = TOROIDAL_SURFACE ( 'NONE', #61505, 4.149999999999999467, 0.1000000000000000056 ) ;
#115667 = CARTESIAN_POINT ( 'NONE',  ( 18.59999999999999076, 1.750000000011155743, -145.6695115579016715 ) ) ;
#115668 = EDGE_CURVE ( 'NONE', #161835, #186134, #251854, .T. ) ;
#115669 = CIRCLE ( 'NONE', #149008, 0.1000000000000088318 ) ;
#115670 = VERTEX_POINT ( 'NONE', #37979 ) ;
#115671 = ORIENTED_EDGE ( 'NONE', *, *, #71738, .T. ) ;
#115672 = ORIENTED_EDGE ( 'NONE', *, *, #155762, .T. ) ;
#115673 = EDGE_CURVE ( 'NONE', #236893, #154872, #217724, .T. ) ;
#115674 = CARTESIAN_POINT ( 'NONE',  ( -20.09999999999999787, 4.645987002755569861, 21.91686199900910736 ) ) ;
#115675 = DIRECTION ( 'NONE',  ( 1.000000000000000000, 0.000000000000000000, 0.000000000000000000 ) ) ;
#115676 = DIRECTION ( 'NONE',  ( 1.000000000000000000, 0.000000000000000000, 0.000000000000000000 ) ) ;
#115677 = FACE_OUTER_BOUND ( 'NONE', #17511, .T. ) ;
#115678 = DIRECTION ( 'NONE',  ( 1.000000000000000000, -3.265361837132813093E-16, -2.280189983783949500E-30 ) ) ;
#115680 = DIRECTION ( 'NONE',  ( 1.000000000000000000, -0.000000000000000000, -0.000000000000000000 ) ) ;
#115679 = CARTESIAN_POINT ( 'NONE',  ( 20.95000000000005258, 65.15000000001120384, -3.123107484524795474 ) ) ;
#115682 = EDGE_LOOP ( 'NONE', ( #114610, #18405, #53522, #231353 ) ) ;
#115681 = CARTESIAN_POINT ( 'NONE',  ( -23.25000000000000000, 64.27847795353595473, -247.1247091181747066 ) ) ;
#115683 = DIRECTION ( 'NONE',  ( 0.000000000000000000, 0.2128009952263603677, -0.9770955615653315052 ) ) ;
#115684 = EDGE_LOOP ( 'NONE', ( #248636, #126421, #25060, #254167, #214045 ) ) ;
#115685 = CARTESIAN_POINT ( 'NONE',  ( -15.52965525596987462, 9.375538102059163492, -149.8698758809908611 ) ) ;
#115686 = EDGE_CURVE ( 'NONE', #192857, #209005, #95150, .T. ) ;
#115687 = ORIENTED_EDGE ( 'NONE', *, *, #43134, .T. ) ;
#115688 = VERTEX_POINT ( 'NONE', #193193 ) ;
#115689 = DIRECTION ( 'NONE',  ( 0.000000000000000000, -0.1568667991644693838, -0.9876197685951279004 ) ) ;
#115690 = AXIS2_PLACEMENT_3D ( 'NONE', #35328, #17024, #254312 ) ;
#115691 = CARTESIAN_POINT ( 'NONE',  ( -21.05000000000000071, 6.344723404101401343, -133.9852821434760699 ) ) ;
#115692 = DIRECTION ( 'NONE',  ( 0.000000000000000000, 5.329070518200686707E-15, 1.000000000000000000 ) ) ;
#115693 = CARTESIAN_POINT ( 'NONE',  ( 20.95392731769792150, 8.883061479199918509, -75.52222797957135469 ) ) ;
#115694 = AXIS2_PLACEMENT_3D ( 'NONE', #105825, #167147, #163275 ) ;
#115695 = DIRECTION ( 'NONE',  ( 0.000000000000000000, -6.982962677686266711E-15, 1.000000000000000000 ) ) ;
#115696 = ORIENTED_EDGE ( 'NONE', *, *, #9740, .F. ) ;
#115697 = ORIENTED_EDGE ( 'NONE', *, *, #239012, .F. ) ;
#115698 = CARTESIAN_POINT ( 'NONE',  ( 18.49999999999999645, -1.866714910046153308, -112.2526752462820525 ) ) ;
#115700 = ADVANCED_FACE ( 'NONE', ( #173671 ), #74559, .F. ) ;
#115699 = VERTEX_POINT ( 'NONE', #14563 ) ;
#115701 = CARTESIAN_POINT ( 'NONE',  ( 19.88284271247461987, 64.30857864377466626, -111.7731074845243739 ) ) ;
#115702 = DIRECTION ( 'NONE',  ( 0.000000000000000000, 0.000000000000000000, 1.000000000000000000 ) ) ;
#115703 = ORIENTED_EDGE ( 'NONE', *, *, #17879, .T. ) ;
#115704 = LINE ( 'NONE', #120866, #257296 ) ;
#115705 = CARTESIAN_POINT ( 'NONE',  ( -21.37071067811865532, 67.92928932189313684, -81.77310748452435973 ) ) ;
#115706 = CYLINDRICAL_SURFACE ( 'NONE', #63396, 4.049999999999997158 ) ;
#115707 = VERTEX_POINT ( 'NONE', #54923 ) ;
#115708 = DIRECTION ( 'NONE',  ( 0.000000000000000000, -6.853228547068871147E-15, 1.000000000000000000 ) ) ;
#115709 = CARTESIAN_POINT ( 'NONE',  ( -18.79999999999999716, -1.311673547813416718, -7.986648289447971116 ) ) ;
#115710 = CIRCLE ( 'NONE', #3251, 3.970710678118653636 ) ;
#115712 = CIRCLE ( 'NONE', #119826, 0.2000000000000057288 ) ;
#115711 = DIRECTION ( 'NONE',  ( 0.000000000000000000, 1.000000000000000000, -0.000000000000000000 ) ) ;
#115713 = AXIS2_PLACEMENT_3D ( 'NONE', #191435, #12787, #74050 ) ;
#115714 = ORIENTED_EDGE ( 'NONE', *, *, #188246, .T. ) ;
#115715 =( BOUNDED_SURFACE ( )  B_SPLINE_SURFACE ( 3, 2, ( 
 ( #207216, #105493, #149814 ),
 ( #7727, #229342, #26004 ),
 ( #185064, #85932, #165520 ),
 ( #110665, #28618, #50664 ),
 ( #108105, #130210, #45559 ),
 ( #209771, #243756, #65114 ),
 ( #125112, #190213, #164236 ),
 ( #245042, #204615, #66407 ) ),
 .UNSPECIFIED., .F., .F., .T. ) 
 B_SPLINE_SURFACE_WITH_KNOTS ( ( 4, 2, 2, 4 ),
 ( 3, 3 ),
 ( 0.0001704874539069909148, 0.0003809798300636642191, 0.0004862260181420008441, 0.0005914722062203374691 ),
 ( 0.000000000000000000, 1.000000000000000000 ),
 .UNSPECIFIED. ) 
 GEOMETRIC_REPRESENTATION_ITEM ( )  RATIONAL_B_SPLINE_SURFACE ( (
 ( 1.000000000000000000, 0.7071067811864942820, 1.000000000000000000),
 ( 1.000000000000000000, 0.7670648383576345042, 1.000000000000000000),
 ( 1.000000000000000000, 0.8204820770252110318, 1.000000000000000000),
 ( 1.000000000000000000, 0.8877218296113941198, 1.000000000000000000),
 ( 1.000000000000000000, 0.9080815932663666157, 1.000000000000000000),
 ( 1.000000000000000000, 0.9395541505863373999, 1.000000000000000000),
 ( 1.000000000000000000, 0.9506520335377883768, 1.000000000000000000),
 ( 1.000000000000000000, 0.9504532311154454405, 1.000000000000000000) ) ) 
 REPRESENTATION_ITEM ( '' )  SURFACE ( )  );
#115717 = EDGE_CURVE ( 'NONE', #104106, #198025, #57493, .T. ) ;
#115716 = DIRECTION ( 'NONE',  ( 1.000000000000000000, -0.000000000000000000, 0.000000000000000000 ) ) ;
#115718 = ORIENTED_EDGE ( 'NONE', *, *, #212079, .T. ) ;
#115719 = DIRECTION ( 'NONE',  ( 0.000000000000000000, 0.8814952561688476074, -0.4721928772777262417 ) ) ;
#115720 = DIRECTION ( 'NONE',  ( 1.000000000000000000, 0.000000000000000000, -0.000000000000000000 ) ) ;
#115721 = DIRECTION ( 'NONE',  ( 1.000000000000000000, 0.000000000000000000, 0.000000000000000000 ) ) ;
#115722 = CARTESIAN_POINT ( 'NONE',  ( 20.95512820512820795, 67.12384868372447499, -191.3229346253956180 ) ) ;
#115723 = CARTESIAN_POINT ( 'NONE',  ( 18.59999999999999076, 11.65000000001115943, -158.8500000000000227 ) ) ;
#115724 = DIRECTION ( 'NONE',  ( 0.000000000000000000, 0.9126074666063545004, 0.4088369013363783999 ) ) ;
#115725 = ORIENTED_EDGE ( 'NONE', *, *, #35042, .T. ) ;
#115726 = CARTESIAN_POINT ( 'NONE',  ( -16.93440969289731157, 66.00481482419810675, -123.9318732995135832 ) ) ;
#115727 = DIRECTION ( 'NONE',  ( 0.000000000000000000, -6.530723674265620862E-15, 1.000000000000000000 ) ) ;
#115728 = AXIS2_PLACEMENT_3D ( 'NONE', #127401, #105213, #6146 ) ;
#115729 = CARTESIAN_POINT ( 'NONE',  ( 20.94999999999999574, 77.83534155023670564, -158.4679561919613491 ) ) ;
#115730 = LINE ( 'NONE', #15365, #188139 ) ;
#115731 = CIRCLE ( 'NONE', #207323, 0.09999999999999939493 ) ;
#115732 = ADVANCED_FACE ( 'NONE', ( #35422 ), #194483, .T. ) ;
#115733 = CARTESIAN_POINT ( 'NONE',  ( 20.97565083910961548, 65.52538259873279003, -61.94516430793584760 ) ) ;
#115734 = ORIENTED_EDGE ( 'NONE', *, *, #73612, .T. ) ;
#115735 = ORIENTED_EDGE ( 'NONE', *, *, #63460, .T. ) ;
#115736 = DIRECTION ( 'NONE',  ( 3.469446951953515108E-14, 1.000000000000000000, 0.000000000000000000 ) ) ;
#115737 = CARTESIAN_POINT ( 'NONE',  ( 23.14999999999999858, 9.960715529987961503, -220.4198853720552904 ) ) ;
#115738 = CARTESIAN_POINT ( 'NONE',  ( -18.39999999999999858, 11.47316190336248631, -20.89142135623730212 ) ) ;
#115739 = FACE_OUTER_BOUND ( 'NONE', #222350, .T. ) ;
#115740 = DIRECTION ( 'NONE',  ( 0.000000000000000000, 0.000000000000000000, -1.000000000000000000 ) ) ;
#115741 = EDGE_LOOP ( 'NONE', ( #40016, #131962, #200294, #153308 ) ) ;
#115742 = CARTESIAN_POINT ( 'NONE',  ( -20.94999999999999929, -11.64999999998884306, -36.60000000000000853 ) ) ;
#115743 = CYLINDRICAL_SURFACE ( 'NONE', #46688, 0.09999999999998898659 ) ;
#115744 = ORIENTED_EDGE ( 'NONE', *, *, #4137, .T. ) ;
#115745 = CARTESIAN_POINT ( 'NONE',  ( 23.14999999999999503, 11.01970663298110154, -220.3481540650095098 ) ) ;
#115746 = DIRECTION ( 'NONE',  ( -1.000000000000000000, -0.000000000000000000, -0.000000000000000000 ) ) ;
#115747 = AXIS2_PLACEMENT_3D ( 'NONE', #200664, #239795, #63706 ) ;
#115748 = VECTOR ( 'NONE', #237758, 1000.000000000000000 ) ;
#115749 = TOROIDAL_SURFACE ( 'NONE', #99531, 11.65000000000000036, 0.1000000000000000056 ) ;
#115750 = ORIENTED_EDGE ( 'NONE', *, *, #57573, .F. ) ;
#115751 = DIRECTION ( 'NONE',  ( -0.9880948137434723000, -0.1538461538461483591, -1.074301950413233512E-15 ) ) ;
#115752 = ORIENTED_EDGE ( 'NONE', *, *, #70303, .T. ) ;
#115753 = DIRECTION ( 'NONE',  ( 1.000000000000000000, -0.000000000000000000, 0.000000000000000000 ) ) ;
#115754 = DIRECTION ( 'NONE',  ( 0.000000000000000000, -1.000000000000000000, 0.000000000000000000 ) ) ;
#115755 = VECTOR ( 'NONE', #55400, 1000.000000000000114 ) ;
#115756 = DIRECTION ( 'NONE',  ( 2.710505431213777355E-16, 1.000000000000000000, 6.982962677686266711E-15 ) ) ;
#115757 = DIRECTION ( 'NONE',  ( 0.000000000000000000, 7.026728003956683390E-15, -1.000000000000000000 ) ) ;
#115758 = DIRECTION ( 'NONE',  ( -1.000000000000000000, 3.265361837132813093E-16, 2.280189983783949500E-30 ) ) ;
#115759 = DIRECTION ( 'NONE',  ( 0.000000000000000000, 0.9126074666063774821, 0.4088369013363273297 ) ) ;
#115760 = LINE ( 'NONE', #195327, #107959 ) ;
#115761 = EDGE_CURVE ( 'NONE', #224344, #253301, #88548, .T. ) ;
#115762 = DIRECTION ( 'NONE',  ( 0.000000000000000000, 0.9654727137038715545, -0.2605042016806676242 ) ) ;
#115763 = DIRECTION ( 'NONE',  ( -1.000000000000000000, -1.875376730785737719E-16, -0.000000000000000000 ) ) ;
#115764 = CARTESIAN_POINT ( 'NONE',  ( -18.59999999999999787, 66.65000000001205649, -124.1731074845243654 ) ) ;
#115765 = DIRECTION ( 'NONE',  ( 0.000000000000000000, 0.000000000000000000, -1.000000000000000000 ) ) ;
#115766 = CARTESIAN_POINT ( 'NONE',  ( 23.14999999999999858, 64.40000000001218439, -143.4513107147999449 ) ) ;
#115767 = AXIS2_PLACEMENT_3D ( 'NONE', #17391, #215576, #36983 ) ;
#115768 = ORIENTED_EDGE ( 'NONE', *, *, #14037, .F. ) ;
#115769 = VECTOR ( 'NONE', #151918, 1000.000000000000000 ) ;
#115770 = AXIS2_PLACEMENT_3D ( 'NONE', #144309, #103904, #179638 ) ;
#115771 = CARTESIAN_POINT ( 'NONE',  ( 20.95512840106819752, 10.62384869378447583, -79.20247922079923342 ) ) ;
#115772 = FACE_OUTER_BOUND ( 'NONE', #53274, .T. ) ;
#115773 = VECTOR ( 'NONE', #182994, 1000.000000000000114 ) ;
#115774 = ORIENTED_EDGE ( 'NONE', *, *, #122194, .T. ) ;
#115775 = DIRECTION ( 'NONE',  ( 0.000000000000000000, 0.000000000000000000, -1.000000000000000000 ) ) ;
#115777 = EDGE_CURVE ( 'NONE', #52293, #206485, #100460, .T. ) ;
#115776 = DIRECTION ( 'NONE',  ( 1.000000000000000000, 0.000000000000000000, 0.000000000000000000 ) ) ;
#115778 = DIRECTION ( 'NONE',  ( 1.000000000000000000, -0.000000000000000000, -0.000000000000000000 ) ) ;
#115779 = ORIENTED_EDGE ( 'NONE', *, *, #38106, .T. ) ;
#115781 = EDGE_CURVE ( 'NONE', #141186, #84620, #118786, .T. ) ;
#115780 = DIRECTION ( 'NONE',  ( 0.000000000000000000, 0.9889818879709274535, 0.1480365673253065395 ) ) ;
#115782 = CARTESIAN_POINT ( 'NONE',  ( -23.25000000000000000, 23.34004772283015328, -229.2004250369967338 ) ) ;
#115783 = ORIENTED_EDGE ( 'NONE', *, *, #225532, .T. ) ;
#115784 = CARTESIAN_POINT ( 'NONE',  ( 21.05000000000000071, -8.999999999988844479, -110.3939691226524786 ) ) ;
#115785 = DIRECTION ( 'NONE',  ( -1.000000000000000000, 0.000000000000000000, 0.000000000000000000 ) ) ;
#115787 = EDGE_CURVE ( 'NONE', #190690, #93783, #217846, .T. ) ;
#115786 = AXIS2_PLACEMENT_3D ( 'NONE', #123461, #139136, #162596 ) ;
#115788 = TOROIDAL_SURFACE ( 'NONE', #119923, 14.20833333333334103, 0.1000000000000000056 ) ;
#115789 = TOROIDAL_SURFACE ( 'NONE', #7450, 12.77500000000000036, 0.1000000000000000056 ) ;
#115790 = AXIS2_PLACEMENT_3D ( 'NONE', #95385, #70717, #94088 ) ;
#115792 = ORIENTED_EDGE ( 'NONE', *, *, #35118, .F. ) ;
#115791 = AXIS2_PLACEMENT_3D ( 'NONE', #11640, #110718, #16771 ) ;
#115793 = CARTESIAN_POINT ( 'NONE',  ( 21.14999999999999858, 6.257814610487280937, -133.9022097086912311 ) ) ;
#115794 = VERTEX_POINT ( 'NONE', #41831 ) ;
#115795 = CIRCLE ( 'NONE', #186547, 4.000000000000010658 ) ;
#115796 = EDGE_CURVE ( 'NONE', #32558, #252649, #121383, .T. ) ;
#115797 = CARTESIAN_POINT ( 'NONE',  ( -20.00857864376270001, 66.75000000001253397, -182.3731074845244393 ) ) ;
#115798 = CARTESIAN_POINT ( 'NONE',  ( -20.94999999999999929, 74.83729825007360148, -61.42310748452432989 ) ) ;
#115800 = LINE ( 'NONE', #12874, #36975 ) ;
#115799 = PRODUCT_DEFINITION_CONTEXT ( 'detailed design', #37539, 'design' ) ;
#115801 = CARTESIAN_POINT ( 'NONE',  ( -20.00857864376270001, 13.46244553689443535, -219.8161515769436107 ) ) ;
#115802 = CARTESIAN_POINT ( 'NONE',  ( -23.25000000000000000, 76.00000000001185185, -95.12310748452429721 ) ) ;
#115803 = CARTESIAN_POINT ( 'NONE',  ( 20.90000000000000213, 7.900000000000000355, 1.300000000000000044 ) ) ;
#115804 = EDGE_CURVE ( 'NONE', #166638, #172600, #176085, .T. ) ;
#115805 = LINE ( 'NONE', #134068, #142550 ) ;
#115806 = CARTESIAN_POINT ( 'NONE',  ( 21.30000000000002558, 1.115600667400684642E-11, -29.45000000000000284 ) ) ;
#115808 = ORIENTED_EDGE ( 'NONE', *, *, #159478, .F. ) ;
#115807 = CARTESIAN_POINT ( 'NONE',  ( -18.41353343127310538, -9.499999999988848032, -40.53206939669965436 ) ) ;
#115809 = ORIENTED_EDGE ( 'NONE', *, *, #228508, .T. ) ;
#115811 = CARTESIAN_POINT ( 'NONE',  ( -20.94999999999999929, 64.40000000001161595, -62.59490425424883853 ) ) ;
#115810 = CARTESIAN_POINT ( 'NONE',  ( -21.05000000000000426, 6.477046381789849150, -0.09999999999999885369 ) ) ;
#115813 = EDGE_LOOP ( 'NONE', ( #102651, #66570, #226519, #193076 ) ) ;
#115812 = CARTESIAN_POINT ( 'NONE',  ( -20.94999999999999929, 0.4810385098657082859, -209.0827657365571213 ) ) ;
#115814 = ORIENTED_EDGE ( 'NONE', *, *, #45170, .F. ) ;
#115815 = DIRECTION ( 'NONE',  ( 1.000000000000000000, 0.000000000000000000, 0.000000000000000000 ) ) ;
#115816 = TOROIDAL_SURFACE ( 'NONE', #3349, 6.258578643762700899, 0.1000000000000000056 ) ;
#115817 = AXIS2_PLACEMENT_3D ( 'NONE', #257106, #135909, #138468 ) ;
#115818 = DIRECTION ( 'NONE',  ( 0.000000000000000000, 6.982962677686266711E-15, -1.000000000000000000 ) ) ;
#115819 = CARTESIAN_POINT ( 'NONE',  ( 18.52928932188133970, 65.72071067813043044, -78.27310748452438816 ) ) ;
#115820 = DIRECTION ( 'NONE',  ( 0.000000000000000000, -0.8660254037844411501, -0.4999999999999956146 ) ) ;
#115821 = DIRECTION ( 'NONE',  ( -1.000000000000000000, -0.000000000000000000, -0.000000000000000000 ) ) ;
#115822 = ADVANCED_FACE ( 'NONE', ( #159205 ), #200874, .F. ) ;
#115823 = AXIS2_PLACEMENT_3D ( 'NONE', #51820, #193937, #75290 ) ;
#115824 = DIRECTION ( 'NONE',  ( -0.000000000000000000, 0.3896596508880146303, 0.9209589331071341700 ) ) ;
#115825 = EDGE_LOOP ( 'NONE', ( #223095, #54893, #7205, #60973 ) ) ;
#115826 = ORIENTED_EDGE ( 'NONE', *, *, #166988, .T. ) ;
#115827 = CARTESIAN_POINT ( 'NONE',  ( -21.05000000000000071, 76.00000000001264766, -200.6231074845243825 ) ) ;
#115828 = AXIS2_PLACEMENT_3D ( 'NONE', #53542, #207499, #133085 ) ;
#115829 = EDGE_LOOP ( 'NONE', ( #227152, #241589, #4811, #8967, #52411 ) ) ;
#115830 = CARTESIAN_POINT ( 'NONE',  ( 20.94999999999999574, 8.926614585098251453, -142.4716830192231498 ) ) ;
#115831 = EDGE_LOOP ( 'NONE', ( #228731, #58219, #223369, #65817 ) ) ;
#115832 = CARTESIAN_POINT ( 'NONE',  ( 18.49362639424895605, -9.442604367888192129, -40.26444093351152276 ) ) ;
#115833 = AXIS2_PLACEMENT_3D ( 'NONE', #199692, #139664, #95428 ) ;
#115834 = EDGE_CURVE ( 'NONE', #185932, #8739, #21935, .T. ) ;
#115835 = DIRECTION ( 'NONE',  ( -1.000000000000000000, 0.000000000000000000, 0.000000000000000000 ) ) ;
#115836 = LINE ( 'NONE', #77978, #130491 ) ;
#115838 = EDGE_LOOP ( 'NONE', ( #173975, #93558, #57745, #149194 ) ) ;
#115837 = CARTESIAN_POINT ( 'NONE',  ( -21.78635804494510708, 7.035661485164336426, -33.40099493449231716 ) ) ;
#115839 = DIRECTION ( 'NONE',  ( 0.000000000000000000, 0.000000000000000000, -1.000000000000000000 ) ) ;
#115840 = ORIENTED_EDGE ( 'NONE', *, *, #177789, .T. ) ;
#115841 = TOROIDAL_SURFACE ( 'NONE', #220074, 0.4000000000000012990, 0.1000000000000000056 ) ;
#115843 = EDGE_CURVE ( 'NONE', #8334, #216369, #182616, .T. ) ;
#115842 = CARTESIAN_POINT ( 'NONE',  ( -23.25000000000000000, -1.149570369564537842, -175.3159124845019790 ) ) ;
#115844 = DIRECTION ( 'NONE',  ( 1.073024830501117725E-15, 6.982962677686266711E-15, -1.000000000000000000 ) ) ;
#115845 = CIRCLE ( 'NONE', #165755, 1.999999999999997335 ) ;
#115847 = DIRECTION ( 'NONE',  ( -1.000000000000000000, -1.652117596168391700E-15, -1.153667551319263085E-29 ) ) ;
#115846 = AXIS2_PLACEMENT_3D ( 'NONE', #233734, #138441, #135880 ) ;
#115848 = LINE ( 'NONE', #257868, #208825 ) ;
#115849 = AXIS2_PLACEMENT_3D ( 'NONE', #13094, #33973, #173495 ) ;
#115850 = CARTESIAN_POINT ( 'NONE',  ( -20.94999999999999929, 11.75000000001115552, -141.0148057706540214 ) ) ;
#115851 = EDGE_CURVE ( 'NONE', #52077, #77989, #226090, .T. ) ;
#115852 = ORIENTED_EDGE ( 'NONE', *, *, #54722, .T. ) ;
#115853 = CARTESIAN_POINT ( 'NONE',  ( -18.54260524012588007, 85.62421939008508787, -29.28233443875340924 ) ) ;
#115854 = VERTEX_POINT ( 'NONE', #83464 ) ;
#115857 = ORIENTED_EDGE ( 'NONE', *, *, #36088, .T. ) ;
#115856 = CARTESIAN_POINT ( 'NONE',  ( 21.15000000000005187, 87.60324567546805952, -34.17184040628037422 ) ) ;
#115855 = FACE_OUTER_BOUND ( 'NONE', #114374, .T. ) ;
#115858 = VECTOR ( 'NONE', #233312, 1000.000000000000000 ) ;
#115859 = EDGE_CURVE ( 'NONE', #107516, #159940, #38683, .T. ) ;
#115860 = B_SPLINE_CURVE_WITH_KNOTS ( 'NONE', 3,
 ( #196218, #175409, #179256, #57976, #159678, #239204, #160968, #35891 ),
 .UNSPECIFIED., .F., .F.,
 ( 4, 2, 2, 4 ),
 ( 0.000000000000000000, 0.0002181133598169259869, 0.0003271700397253583651, 0.0004362267196337907705 ),
 .UNSPECIFIED. ) ;
#115861 = CARTESIAN_POINT ( 'NONE',  ( 22.57856590037848576, 76.00412833007638369, -114.7731659471998000 ) ) ;
#115862 = CARTESIAN_POINT ( 'NONE',  ( -22.59066674512259709, 64.25000000001163869, -69.55361160815476751 ) ) ;
#115863 = ORIENTED_EDGE ( 'NONE', *, *, #86112, .F. ) ;
#115864 = CARTESIAN_POINT ( 'NONE',  ( -23.15000000000000213, 76.00000000001222134, -148.3231074845243427 ) ) ;
#115866 = EDGE_CURVE ( 'NONE', #34288, #135228, #205254, .T. ) ;
#115865 = DIRECTION ( 'NONE',  ( -1.000000000000000000, -0.000000000000000000, -0.000000000000000000 ) ) ;
#115867 = CARTESIAN_POINT ( 'NONE',  ( -17.11825945287482753, 9.949999999999983302, -12.65000000000000213 ) ) ;
#115869 = EDGE_LOOP ( 'NONE', ( #111201, #200048, #15699 ) ) ;
#115868 = LINE ( 'NONE', #172031, #59986 ) ;
#115870 = TOROIDAL_SURFACE ( 'NONE', #236656, 0.4000000000000003553, 0.1000000000000000056 ) ;
#115871 = EDGE_CURVE ( 'NONE', #72194, #124432, #172002, .T. ) ;
#115872 = EDGE_CURVE ( 'NONE', #57548, #202111, #2661, .T. ) ;
#115873 = CARTESIAN_POINT ( 'NONE',  ( 18.59999999999999787, -1.263275465217258198, -41.40186466674640542 ) ) ;
#115874 = ORIENTED_EDGE ( 'NONE', *, *, #29386, .F. ) ;
#115875 = DIRECTION ( 'NONE',  ( -0.000000000000000000, 6.982962677686266711E-15, -1.000000000000000000 ) ) ;
#115876 = DIRECTION ( 'NONE',  ( -2.141321560717106639E-14, 0.1575546449569727447, -0.9875102702516477260 ) ) ;
#115877 = CARTESIAN_POINT ( 'NONE',  ( 20.94999999999999574, 14.83422855357708414, -203.3235740904736417 ) ) ;
#115878 = VECTOR ( 'NONE', #46833, 1000.000000000000114 ) ;
#115879 = ORIENTED_EDGE ( 'NONE', *, *, #162245, .F. ) ;
#115880 = DIRECTION ( 'NONE',  ( -0.000000000000000000, 0.9770955615653316162, 0.2128009952263604232 ) ) ;
#115881 = ORIENTED_EDGE ( 'NONE', *, *, #58971, .T. ) ;
#115882 = CARTESIAN_POINT ( 'NONE',  ( 18.59999999999999076, -1.164121893230052995, -141.9148480855716343 ) ) ;
#115883 = EDGE_CURVE ( 'NONE', #221894, #6267, #144530, .T. ) ;
#115884 = CARTESIAN_POINT ( 'NONE',  ( -23.25000000000000000, 42.94327155031035659, -233.8606566173841372 ) ) ;
#115885 = FACE_OUTER_BOUND ( 'NONE', #10327, .T. ) ;
#115886 = VERTEX_POINT ( 'NONE', #247704 ) ;
#115887 = EDGE_CURVE ( 'NONE', #68978, #205992, #50760, .T. ) ;
#115888 = DIRECTION ( 'NONE',  ( 1.000000000000000000, -0.000000000000000000, -0.000000000000000000 ) ) ;
#115889 = ADVANCED_FACE ( 'NONE', ( #10391 ), #46913, .F. ) ;
#115890 = LINE ( 'NONE', #173344, #22219 ) ;
#115891 = ORIENTED_EDGE ( 'NONE', *, *, #193695, .F. ) ;
#115892 = VECTOR ( 'NONE', #82363, 1000.000000000000000 ) ;
#115893 = AXIS2_PLACEMENT_3D ( 'NONE', #116378, #98047, #135908 ) ;
#115895 = AXIS2_PLACEMENT_3D ( 'NONE', #50161, #210540, #249670 ) ;
#115894 = DIRECTION ( 'NONE',  ( 0.000000000000000000, 1.000000000000000000, 0.000000000000000000 ) ) ;
#115896 = CARTESIAN_POINT ( 'NONE',  ( -21.55000000000000426, 52.79208635511305658, -233.8315543717827154 ) ) ;
#115897 = AXIS2_PLACEMENT_3D ( 'NONE', #45152, #25603, #26909 ) ;
#115898 = LINE ( 'NONE', #1042, #236275 ) ;
#115899 = ORIENTED_EDGE ( 'NONE', *, *, #158928, .T. ) ;
#115900 = DIRECTION ( 'NONE',  ( 1.000000000000000000, 0.000000000000000000, 0.000000000000000000 ) ) ;
#115901 = B_SPLINE_CURVE_WITH_KNOTS ( 'NONE', 3,
 ( #234751, #195650, #174830, #56085, #13149, #15736, #92668, #253023, #95238, #134346, #36590, #251748, #256822, #172261, #114807, #93952, #97772, #18272, #177381, #73147, #193073, #151387, #37859, #152683, #74435, #135638, #215188, #153984, #233491, #116100 ),
 .UNSPECIFIED., .F., .F.,
 ( 4, 2, 2, 2, 2, 2, 2, 2, 2, 2, 2, 2, 2, 2, 4 ),
 ( 0.000000000000000000, 0.0003422764154113345906, 0.0006845528308226691812, 0.001026829246234003826, 0.001369105661645338362, 0.002053658492468006351, 0.002738211323290674556, 0.003080487738702008659, 0.003422764154113342328, 0.003765040569524676431, 0.004107316984936010100, 0.004449593400347344636, 0.004791869815758678305, 0.005134146231170011974, 0.005476422646581346511 ),
 .UNSPECIFIED. ) ;
#115902 = EDGE_LOOP ( 'NONE', ( #99610, #32365, #13874, #199472 ) ) ;
#115904 = ORIENTED_EDGE ( 'NONE', *, *, #118288, .F. ) ;
#115903 = FACE_OUTER_BOUND ( 'NONE', #120663, .T. ) ;
#115905 = EDGE_CURVE ( 'NONE', #19688, #167418, #82154, .T. ) ;
#115906 = EDGE_CURVE ( 'NONE', #255180, #99123, #6519, .T. ) ;
#115909 = ORIENTED_EDGE ( 'NONE', *, *, #90302, .F. ) ;
#115908 = ORIENTED_EDGE ( 'NONE', *, *, #100577, .T. ) ;
#115907 = CARTESIAN_POINT ( 'NONE',  ( 23.24999999999999645, 13.44928205424795564, -207.5377222505711075 ) ) ;
#115911 = CIRCLE ( 'NONE', #240813, 0.09999999999999939493 ) ;
#115910 = CARTESIAN_POINT ( 'NONE',  ( -23.25000000000000000, 2.000000000011154189, -187.7753780772378889 ) ) ;
#115913 = EDGE_CURVE ( 'NONE', #161829, #183594, #167702, .T. ) ;
#115912 = DIRECTION ( 'NONE',  ( 0.000000000000000000, 7.086529944415886769E-15, -1.000000000000000000 ) ) ;
#115914 = CIRCLE ( 'NONE', #132668, 2.100000000000002309 ) ;
#115915 = CARTESIAN_POINT ( 'NONE',  ( -16.89935556175678855, 12.51823704456101005, -211.7213495520792037 ) ) ;
#115916 = DIRECTION ( 'NONE',  ( 2.952720810173289112E-16, -0.9770955615653301729, -0.2128009952263660853 ) ) ;
#115917 = DIRECTION ( 'NONE',  ( -1.000000000000000000, -2.952720810173289112E-16, 0.000000000000000000 ) ) ;
#115918 = FACE_OUTER_BOUND ( 'NONE', #162273, .T. ) ;
#115919 = CIRCLE ( 'NONE', #24354, 0.1999999999999987899 ) ;
#115920 = DIRECTION ( 'NONE',  ( 0.000000000000000000, 2.891205793294679805E-16, -1.000000000000000000 ) ) ;
#115921 = VERTEX_POINT ( 'NONE', #190312 ) ;
#115922 = ORIENTED_EDGE ( 'NONE', *, *, #103283, .F. ) ;
#115923 = ORIENTED_EDGE ( 'NONE', *, *, #127082, .F. ) ;
#115924 = DIRECTION ( 'NONE',  ( -0.000000000000000000, 0.9908441862701591329, 0.1350103645451946055 ) ) ;
#115926 = ORIENTED_EDGE ( 'NONE', *, *, #251336, .T. ) ;
#115925 = DIRECTION ( 'NONE',  ( 3.469446951953243109E-14, 0.4999999999999608646, 0.8660254037844612451 ) ) ;
#115927 = LINE ( 'NONE', #38965, #109172 ) ;
#115928 = ORIENTED_EDGE ( 'NONE', *, *, #101785, .F. ) ;
#115929 = DIRECTION ( 'NONE',  ( 1.000000000000000000, 0.000000000000000000, 0.000000000000000000 ) ) ;
#115930 = ORIENTED_EDGE ( 'NONE', *, *, #84122, .T. ) ;
#115931 = CYLINDRICAL_SURFACE ( 'NONE', #4464, 0.1000000000000013933 ) ;
#115932 = EDGE_CURVE ( 'NONE', #249694, #120125, #109399, .T. ) ;
#115933 = ORIENTED_EDGE ( 'NONE', *, *, #19046, .T. ) ;
#115934 = DIRECTION ( 'NONE',  ( 0.000000000000000000, 0.8814952561688438326, -0.4721928772777332362 ) ) ;
#115936 = ADVANCED_FACE ( 'NONE', ( #9099 ), #203239, .T. ) ;
#115935 = CARTESIAN_POINT ( 'NONE',  ( 23.25000000000000000, -11.48912529306489994, -130.9000000000000341 ) ) ;
#115937 = AXIS2_PLACEMENT_3D ( 'NONE', #99932, #81644, #221178 ) ;
#115938 = CIRCLE ( 'NONE', #111652, 0.09999999999998807065 ) ;
#115940 = ORIENTED_EDGE ( 'NONE', *, *, #120997, .T. ) ;
#115939 = ORIENTED_EDGE ( 'NONE', *, *, #37378, .T. ) ;
#115941 = VERTEX_POINT ( 'NONE', #168212 ) ;
#115942 = DIRECTION ( 'NONE',  ( -0.000000000000000000, -0.4721928772777346239, -0.8814952561688430555 ) ) ;
#115943 = ORIENTED_EDGE ( 'NONE', *, *, #103385, .T. ) ;
#115944 = EDGE_LOOP ( 'NONE', ( #170302, #150520, #83253, #189733 ) ) ;
#115945 = CARTESIAN_POINT ( 'NONE',  ( -20.64999999999999858, 5.256951610580939516, -213.3897168960460533 ) ) ;
#115948 = ADVANCED_FACE ( 'NONE', ( #148619 ), #6753, .T. ) ;
#115947 = ORIENTED_EDGE ( 'NONE', *, *, #27256, .F. ) ;
#115946 = DIRECTION ( 'NONE',  ( 0.000000000000000000, -0.8660254037844411501, -0.4999999999999956146 ) ) ;
#115949 = FACE_OUTER_BOUND ( 'NONE', #53326, .T. ) ;
#115950 = CIRCLE ( 'NONE', #174245, 0.1000000000000028644 ) ;
#115952 = FACE_OUTER_BOUND ( 'NONE', #130535, .T. ) ;
#115951 = DIRECTION ( 'NONE',  ( 0.7070776581709139474, -0.7071359030027652981, -2.453168425935592377E-14 ) ) ;
#115953 = CARTESIAN_POINT ( 'NONE',  ( -18.59999999999999787, 70.53171716061257257, -228.4612385850772682 ) ) ;
#115954 = CARTESIAN_POINT ( 'NONE',  ( -22.59999999999999787, 75.89914163091405896, -215.2726746080137445 ) ) ;
#115955 = FACE_OUTER_BOUND ( 'NONE', #147019, .T. ) ;
#115956 = VERTEX_POINT ( 'NONE', #135445 ) ;
#115957 = ADVANCED_FACE ( 'NONE', ( #57174 ), #63613, .F. ) ;
#115958 = ORIENTED_EDGE ( 'NONE', *, *, #180082, .F. ) ;
#115959 = FACE_OUTER_BOUND ( 'NONE', #206922, .T. ) ;
#115960 = CARTESIAN_POINT ( 'NONE',  ( -23.25000000000000000, 64.35000000001150511, -48.17310748452440805 ) ) ;
#115961 = DIRECTION ( 'NONE',  ( -2.141321560717181029E-15, 0.1575546449569727447, 0.9875102702516478370 ) ) ;
#115962 = EDGE_CURVE ( 'NONE', #178561, #74222, #71653, .T. ) ;
#115963 = ORIENTED_EDGE ( 'NONE', *, *, #162743, .T. ) ;
#115964 = VECTOR ( 'NONE', #166905, 1000.000000000000227 ) ;
#115966 = DIRECTION ( 'NONE',  ( -0.000000000000000000, -0.000000000000000000, 1.000000000000000000 ) ) ;
#115965 = AXIS2_PLACEMENT_3D ( 'NONE', #211, #4068, #138418 ) ;
#115967 = AXIS2_PLACEMENT_3D ( 'NONE', #67075, #209142, #108766 ) ;
#115968 = EDGE_CURVE ( 'NONE', #185096, #17682, #112060, .T. ) ;
#115969 = CYLINDRICAL_SURFACE ( 'NONE', #42880, 0.09999999999999609201 ) ;
#115970 = FACE_OUTER_BOUND ( 'NONE', #89353, .T. ) ;
#115973 = ADVANCED_FACE ( 'NONE', ( #114613 ), #52050, .T. ) ;
#115972 = ADVANCED_FACE ( 'NONE', ( #151183 ), #238592, .F. ) ;
#115971 = AXIS2_PLACEMENT_3D ( 'NONE', #26273, #126647, #87500 ) ;
#115974 = EDGE_LOOP ( 'NONE', ( #41033, #124566, #154081 ) ) ;
#115975 = ORIENTED_EDGE ( 'NONE', *, *, #207433, .T. ) ;
#115976 = CARTESIAN_POINT ( 'NONE',  ( -23.25000000000000000, 7.567413955921500346, -241.6205176796878504 ) ) ;
#115977 = DIRECTION ( 'NONE',  ( 1.000000000000000000, 0.000000000000000000, 0.000000000000000000 ) ) ;
#115978 = ORIENTED_EDGE ( 'NONE', *, *, #90529, .F. ) ;
#115979 = FACE_OUTER_BOUND ( 'NONE', #250204, .T. ) ;
#115980 = ORIENTED_EDGE ( 'NONE', *, *, #110811, .F. ) ;
#115981 = DIRECTION ( 'NONE',  ( -0.000000000000000000, 0.3896596508880098009, 0.9209589331071360574 ) ) ;
#115982 = DIRECTION ( 'NONE',  ( 0.000000000000000000, 7.109473446599835262E-15, -1.000000000000000000 ) ) ;
#115984 = DIRECTION ( 'NONE',  ( 0.000000000000000000, 0.000000000000000000, 1.000000000000000000 ) ) ;
#115983 = CARTESIAN_POINT ( 'NONE',  ( -18.59999999999999787, 1.115600667400684642E-11, -200.9999999999999432 ) ) ;
#115985 = VECTOR ( 'NONE', #207484, 1000.000000000000227 ) ;
#115986 = DIRECTION ( 'NONE',  ( -1.000000000000000000, 2.952720810173289112E-16, 2.061873921506763405E-30 ) ) ;
#115987 = CARTESIAN_POINT ( 'NONE',  ( 21.08750232978087524, 65.27513661400170975, -90.79424931152482259 ) ) ;
#115988 = CARTESIAN_POINT ( 'NONE',  ( -23.25000000000000000, 76.00000000001213607, -136.5231074845242745 ) ) ;
#115989 = EDGE_CURVE ( 'NONE', #135773, #177869, #250272, .T. ) ;
#115990 = EDGE_CURVE ( 'NONE', #126474, #192558, #126140, .T. ) ;
#115993 = ORIENTED_EDGE ( 'NONE', *, *, #97573, .F. ) ;
#115992 = VERTEX_POINT ( 'NONE', #55891 ) ;
#115991 = TOROIDAL_SURFACE ( 'NONE', #178353, 0.2000000000000000111, 0.1000000000000000056 ) ;
#115994 = ORIENTED_EDGE ( 'NONE', *, *, #85555, .T. ) ;
#115995 = AXIS2_PLACEMENT_3D ( 'NONE', #153966, #11861, #70559 ) ;
#115996 = CIRCLE ( 'NONE', #253347, 3.999999999999996447 ) ;
#115997 = VECTOR ( 'NONE', #222624, 1000.000000000000000 ) ;
#115998 = EDGE_CURVE ( 'NONE', #149075, #9130, #173354, .T. ) ;
#115999 = CARTESIAN_POINT ( 'NONE',  ( -17.11825945287482753, 12.43531352672262003, -211.3405985074572300 ) ) ;
#116000 = DIRECTION ( 'NONE',  ( 0.000000000000000000, 0.000000000000000000, -1.000000000000000000 ) ) ;
#116001 = CARTESIAN_POINT ( 'NONE',  ( 23.15000000000000213, -11.64999999998883595, -130.9000000000000341 ) ) ;
#116002 = CARTESIAN_POINT ( 'NONE',  ( -18.50000000000000000, -9.399999999988850163, -107.7972597596633193 ) ) ;
#116003 = VECTOR ( 'NONE', #200272, 1000.000000000000114 ) ;
#116005 = CARTESIAN_POINT ( 'NONE',  ( -20.94999999999999929, 64.23744694032046709, -224.5446448091673233 ) ) ;
#116004 = CARTESIAN_POINT ( 'NONE',  ( 20.44999100639894962, 10.43971070321203953, -7.759075725970426163 ) ) ;
#116006 = EDGE_CURVE ( 'NONE', #15467, #239176, #230210, .T. ) ;
#116007 = DIRECTION ( 'NONE',  ( 1.000000000000000000, -3.469446951953718318E-14, 2.003086131649645455E-14 ) ) ;
#116008 = VERTEX_POINT ( 'NONE', #251546 ) ;
#116009 = DIRECTION ( 'NONE',  ( 0.000000000000000000, 0.000000000000000000, 1.000000000000000000 ) ) ;
#116010 = EDGE_CURVE ( 'NONE', #172714, #17513, #180330, .T. ) ;
#116011 = ORIENTED_EDGE ( 'NONE', *, *, #210476, .T. ) ;
#116012 = EDGE_LOOP ( 'NONE', ( #249720, #253386, #117456, #80966, #216661 ) ) ;
#116013 = CARTESIAN_POINT ( 'NONE',  ( -21.05000000000000071, 69.58633726514248963, -69.43751462116246387 ) ) ;
#116014 = CARTESIAN_POINT ( 'NONE',  ( -20.94999999999999929, 36.65892442174935439, -249.5511627012433848 ) ) ;
#116015 = CARTESIAN_POINT ( 'NONE',  ( 20.95512820512820440, 67.12384868372447499, -191.3731074845244109 ) ) ;
#116016 = CIRCLE ( 'NONE', #49359, 0.2000000000000000944 ) ;
#116017 = DIRECTION ( 'NONE',  ( -0.7071067811865127117, -0.7071067811865821007, 0.000000000000000000 ) ) ;
#116018 = ORIENTED_EDGE ( 'NONE', *, *, #131865, .F. ) ;
#116019 = VERTEX_POINT ( 'NONE', #156341 ) ;
#116020 = CARTESIAN_POINT ( 'NONE',  ( -21.00448002041600759, 11.75000000001115730, -40.34834086231045802 ) ) ;
#116021 = DIRECTION ( 'NONE',  ( 0.000000000000000000, 0.000000000000000000, -1.000000000000000000 ) ) ;
#116022 = EDGE_CURVE ( 'NONE', #178868, #211462, #47041, .T. ) ;
#116023 = CARTESIAN_POINT ( 'NONE',  ( 21.15000000000005542, 67.85000000001119247, -3.023107484524792277 ) ) ;
#116024 = FACE_OUTER_BOUND ( 'NONE', #70359, .T. ) ;
#116025 = CARTESIAN_POINT ( 'NONE',  ( -20.54999999999999716, 74.00000000001156764, -56.29848556176223440 ) ) ;
#116026 = DIRECTION ( 'NONE',  ( 1.000000000000000000, 0.000000000000000000, 0.000000000000000000 ) ) ;
#116027 = DIRECTION ( 'NONE',  ( 0.000000000000000000, 0.000000000000000000, -1.000000000000000000 ) ) ;
#116028 = AXIS2_PLACEMENT_3D ( 'NONE', #164763, #130450, #203876 ) ;
#116030 = DIRECTION ( 'NONE',  ( -1.462545276649518737E-15, -0.1686199900910448357, 0.9856811345164805394 ) ) ;
#116029 = CARTESIAN_POINT ( 'NONE',  ( 20.04142135623730070, 64.35000000001201670, -114.7731074845243882 ) ) ;
#116031 = CARTESIAN_POINT ( 'NONE',  ( 18.59999999999999076, 1.835341550235567887, -179.0551512925629538 ) ) ;
#116032 = CIRCLE ( 'NONE', #224144, 0.1000000000000054040 ) ;
#116034 = ADVANCED_FACE ( 'NONE', ( #115903 ), #146984, .T. ) ;
#116033 = CARTESIAN_POINT ( 'NONE',  ( 22.39999999999999503, 76.00000000001243450, -177.7731074845243597 ) ) ;
#116035 = DIRECTION ( 'NONE',  ( 0.000000000000000000, -0.4088369013363283844, 0.9126074666063768159 ) ) ;
#116037 = DIRECTION ( 'NONE',  ( 1.000000000000000000, 0.000000000000000000, 0.000000000000000000 ) ) ;
#116036 = VECTOR ( 'NONE', #190510, 1000.000000000000000 ) ;
#116039 = EDGE_LOOP ( 'NONE', ( #253359, #4372, #33416 ) ) ;
#116038 = DIRECTION ( 'NONE',  ( -1.000000000000000000, -0.000000000000000000, -0.000000000000000000 ) ) ;
#116040 = AXIS2_PLACEMENT_3D ( 'NONE', #118212, #158650, #219870 ) ;
#116042 = EDGE_CURVE ( 'NONE', #232478, #81812, #180169, .T. ) ;
#116041 = DIRECTION ( 'NONE',  ( 0.000000000000000000, 0.000000000000000000, -1.000000000000000000 ) ) ;
#116043 = VERTEX_POINT ( 'NONE', #93758 ) ;
#116044 = VECTOR ( 'NONE', #238811, 1000.000000000000000 ) ;
#116045 = CARTESIAN_POINT ( 'NONE',  ( -18.38817693311004575, 54.09559807286957067, -229.1587729586515820 ) ) ;
#116046 = CARTESIAN_POINT ( 'NONE',  ( -21.64999999999999858, 7.350000000011155166, -121.7500000000000426 ) ) ;
#116047 = CIRCLE ( 'NONE', #3585, 4.149999999999999467 ) ;
#116048 = CIRCLE ( 'NONE', #91089, 0.09999999999998898659 ) ;
#116049 = ORIENTED_EDGE ( 'NONE', *, *, #190767, .F. ) ;
#116050 = DIRECTION ( 'NONE',  ( -0.000000000000000000, 0.2128009952263604232, -0.9770955615653316162 ) ) ;
#116051 = AXIS2_PLACEMENT_3D ( 'NONE', #59383, #219766, #104925 ) ;
#116052 = CARTESIAN_POINT ( 'NONE',  ( 12.25000000000000000, 9.350000000011140955, -83.75000000000004263 ) ) ;
#116053 = CARTESIAN_POINT ( 'NONE',  ( 22.49066049874202022, 0.05634325154338428593, -21.84998776248290042 ) ) ;
#116054 = EDGE_CURVE ( 'NONE', #145735, #75834, #246958, .T. ) ;
#116055 = DIRECTION ( 'NONE',  ( 0.000000000000000000, 0.000000000000000000, -1.000000000000000000 ) ) ;
#116056 = CARTESIAN_POINT ( 'NONE',  ( 18.49999999999999289, 10.20857864376268864, -24.65000000000000213 ) ) ;
#116057 = DIRECTION ( 'NONE',  ( -7.304098846218134667E-16, -1.000000000000000000, 0.000000000000000000 ) ) ;
#116058 = VERTEX_POINT ( 'NONE', #74241 ) ;
#116059 = CARTESIAN_POINT ( 'NONE',  ( 23.14999999999999858, 70.40000000001180069, -81.92837350343744163 ) ) ;
#116061 = VERTEX_POINT ( 'NONE', #233300 ) ;
#116060 = CARTESIAN_POINT ( 'NONE',  ( 22.10000000000000497, 6.322468214605804882, 12.11686199900910310 ) ) ;
#116062 = CARTESIAN_POINT ( 'NONE',  ( 18.60000000000000142, -9.321008403350125704, -40.73593824907789696 ) ) ;
#116063 = DIRECTION ( 'NONE',  ( 0.000000000000000000, 0.000000000000000000, -1.000000000000000000 ) ) ;
#116064 = ORIENTED_EDGE ( 'NONE', *, *, #115906, .T. ) ;
#116065 = LINE ( 'NONE', #173515, #101122 ) ;
#116066 = AXIS2_PLACEMENT_3D ( 'NONE', #93664, #213602, #174545 ) ;
#116067 = SHAPE_DEFINITION_REPRESENTATION ( #207591, #233377 ) ;
#116068 = CARTESIAN_POINT ( 'NONE',  ( -20.54999999999999716, 66.26558728512915764, -222.7970849955717938 ) ) ;
#116069 = CARTESIAN_POINT ( 'NONE',  ( -23.49999999999994316, 82.64476912853859858, -26.37791261425322986 ) ) ;
#116070 = VERTEX_POINT ( 'NONE', #16814 ) ;
#116071 = DIRECTION ( 'NONE',  ( 0.000000000000000000, 1.000000000000000000, 1.387778780781444413E-14 ) ) ;
#116072 = DIRECTION ( 'NONE',  ( 0.000000000000000000, 0.000000000000000000, -1.000000000000000000 ) ) ;
#116073 = FILL_AREA_STYLE ('',( #36563 ) ) ;
#116074 = VERTEX_POINT ( 'NONE', #196706 ) ;
#116075 = ORIENTED_EDGE ( 'NONE', *, *, #215503, .T. ) ;
#116076 = CYLINDRICAL_SURFACE ( 'NONE', #18133, 0.09999999999998898659 ) ;
#116077 = DIRECTION ( 'NONE',  ( 1.000000000000000000, 0.000000000000000000, 0.000000000000000000 ) ) ;
#116078 = FACE_OUTER_BOUND ( 'NONE', #250131, .T. ) ;
#116079 = DIRECTION ( 'NONE',  ( 0.000000000000000000, -6.352154140967427193E-15, 1.000000000000000000 ) ) ;
#116080 = DIRECTION ( 'NONE',  ( 0.000000000000000000, 8.783410004945854632E-15, -1.000000000000000000 ) ) ;
#116081 = ADVANCED_FACE ( 'NONE', ( #76760 ), #242247, .F. ) ;
#116083 = CARTESIAN_POINT ( 'NONE',  ( -5.900000000000003020, -11.34999999999999964, 10.10000000000000142 ) ) ;
#116082 = DIRECTION ( 'NONE',  ( 1.000000000000000000, 0.000000000000000000, 0.000000000000000000 ) ) ;
#116084 = VECTOR ( 'NONE', #196895, 1000.000000000000000 ) ;
#116086 = CARTESIAN_POINT ( 'NONE',  ( -16.89268316805466341, 66.04827818677041762, -190.8788599630699707 ) ) ;
#116085 = CIRCLE ( 'NONE', #257476, 0.1000000000000008937 ) ;
#116087 = CARTESIAN_POINT ( 'NONE',  ( 18.79999999999999716, 5.488301202077012775, 16.40000000000000213 ) ) ;
#116088 = AXIS2_PLACEMENT_3D ( 'NONE', #175746, #115746, #9262 ) ;
#116089 = DIRECTION ( 'NONE',  ( 1.000000000000000000, -0.000000000000000000, -0.000000000000000000 ) ) ;
#116090 = ORIENTED_EDGE ( 'NONE', *, *, #197086, .F. ) ;
#116091 = EDGE_LOOP ( 'NONE', ( #3565, #217661, #234028, #173957 ) ) ;
#116092 = DIRECTION ( 'NONE',  ( 0.000000000000000000, -6.982962677686266711E-15, 1.000000000000000000 ) ) ;
#116093 = CARTESIAN_POINT ( 'NONE',  ( -22.50000000000000000, 64.35000000001268461, -203.5231074845244166 ) ) ;
#116095 = CARTESIAN_POINT ( 'NONE',  ( -18.40000000000000213, 43.57057518228153015, -234.0379448663882442 ) ) ;
#116094 = CARTESIAN_POINT ( 'NONE',  ( 18.49999999999999645, 76.00000000001213607, -136.5231074845243313 ) ) ;
#116096 = VECTOR ( 'NONE', #203881, 1000.000000000000114 ) ;
#116097 = CARTESIAN_POINT ( 'NONE',  ( -21.05000000000000071, 77.83534155023670564, -158.4679561919613491 ) ) ;
#116099 = EDGE_CURVE ( 'NONE', #233797, #143749, #41515, .T. ) ;
#116098 = DIRECTION ( 'NONE',  ( 0.000000000000000000, 0.8814952561688476074, -0.4721928772777262417 ) ) ;
#116100 = CARTESIAN_POINT ( 'NONE',  ( 12.25000000000000000, 12.70026017068886937, -215.3766613508543628 ) ) ;
#116101 = VERTEX_POINT ( 'NONE', #3635 ) ;
#116102 = EDGE_LOOP ( 'NONE', ( #150016, #111310, #190527, #144800 ) ) ;
#116103 = ADVANCED_FACE ( 'NONE', ( #19369 ), #42777, .F. ) ;
#116104 = AXIS2_PLACEMENT_3D ( 'NONE', #53987, #193516, #255985 ) ;
#116105 = VECTOR ( 'NONE', #148708, 1000.000000000000000 ) ;
#116107 = VECTOR ( 'NONE', #74148, 1000.000000000000000 ) ;
#116106 = DIRECTION ( 'NONE',  ( 0.000000000000000000, 0.1455152366551500653, 0.9893560106964507384 ) ) ;
#116108 = ORIENTED_EDGE ( 'NONE', *, *, #69145, .F. ) ;
#116109 = LINE ( 'NONE', #195658, #18066 ) ;
#116110 = EDGE_CURVE ( 'NONE', #225349, #254638, #139282, .T. ) ;
#116111 = DIRECTION ( 'NONE',  ( 1.000000000000000000, -2.952720810173289112E-16, -2.061873921506763405E-30 ) ) ;
#116112 = DIRECTION ( 'NONE',  ( 0.000000000000000000, -0.1335171055202867274, 0.9910465087640866200 ) ) ;
#116113 = EDGE_CURVE ( 'NONE', #97776, #117118, #33445, .T. ) ;
#116114 = EDGE_CURVE ( 'NONE', #39510, #74897, #121065, .T. ) ;
#116115 = ORIENTED_EDGE ( 'NONE', *, *, #66536, .T. ) ;
#116116 = LINE ( 'NONE', #15754, #126487 ) ;
#116117 = VERTEX_POINT ( 'NONE', #138004 ) ;
#116118 = EDGE_CURVE ( 'NONE', #169719, #132474, #84606, .T. ) ;
#116119 = DIRECTION ( 'NONE',  ( 1.000000000000000000, 0.000000000000000000, 0.000000000000000000 ) ) ;
#116120 = CARTESIAN_POINT ( 'NONE',  ( -23.25000000000000355, 45.89348038176515843, -239.2231437130149061 ) ) ;
#116121 = DIRECTION ( 'NONE',  ( 1.000000000000000000, 0.000000000000000000, 0.000000000000000000 ) ) ;
#116122 = CARTESIAN_POINT ( 'NONE',  ( -21.05000000000000071, 16.44800918141279666, -240.8068063186265135 ) ) ;
#116123 = FACE_OUTER_BOUND ( 'NONE', #176970, .T. ) ;
#116125 = DIRECTION ( 'NONE',  ( 1.000000000000000000, 0.000000000000000000, 0.000000000000000000 ) ) ;
#116124 = DIRECTION ( 'NONE',  ( -0.000000000000000000, -0.8660254037844377084, -0.5000000000000016653 ) ) ;
#116126 = EDGE_CURVE ( 'NONE', #246420, #100043, #1430, .T. ) ;
#116127 = CARTESIAN_POINT ( 'NONE',  ( 16.87683809663749557, 66.05000000001226113, -149.1731074845244223 ) ) ;
#116128 = ORIENTED_EDGE ( 'NONE', *, *, #176955, .F. ) ;
#116130 = CARTESIAN_POINT ( 'NONE',  ( -18.79999999999999716, 11.49641995933507843, 1.885425182446133885 ) ) ;
#116129 = CARTESIAN_POINT ( 'NONE',  ( -23.15000000000000213, 31.44980407958351165, -233.5445995079518866 ) ) ;
#116132 = ORIENTED_EDGE ( 'NONE', *, *, #185083, .T. ) ;
#116131 = CIRCLE ( 'NONE', #211987, 0.09999999999999939493 ) ;
#116134 = EDGE_LOOP ( 'NONE', ( #47939, #179716, #49759, #232080 ) ) ;
#116133 = CARTESIAN_POINT ( 'NONE',  ( 18.59999999999998721, 6.933893972137497030, -104.2856458343736250 ) ) ;
#116135 = AXIS2_PLACEMENT_3D ( 'NONE', #193709, #42031, #133718 ) ;
#116136 = VERTEX_POINT ( 'NONE', #23244 ) ;
#116137 = CARTESIAN_POINT ( 'NONE',  ( -18.36973785203556275, 11.47550320049537476, -91.25000000000005684 ) ) ;
#116138 = FACE_OUTER_BOUND ( 'NONE', #192880, .T. ) ;
#116139 = CARTESIAN_POINT ( 'NONE',  ( 18.49999999999999289, 65.50857864377447015, -78.27310748452438816 ) ) ;
#116140 = DIRECTION ( 'NONE',  ( 0.000000000000000000, 1.265107689135680095E-16, -1.000000000000000000 ) ) ;
#116141 = EDGE_LOOP ( 'NONE', ( #102440, #134046, #164625, #134978 ) ) ;
#116142 = CARTESIAN_POINT ( 'NONE',  ( 21.72449340488910607, 10.28395627750226815, -188.3499999999999659 ) ) ;
#116143 = EDGE_CURVE ( 'NONE', #222885, #89898, #184598, .T. ) ;
#116144 = DIRECTION ( 'NONE',  ( 0.000000000000000000, 0.000000000000000000, 1.000000000000000000 ) ) ;
#116145 = CIRCLE ( 'NONE', #132708, 0.09999999999999986677 ) ;
#116146 = CARTESIAN_POINT ( 'NONE',  ( 22.48660254037845618, 64.25000000001269029, -203.5731074845244564 ) ) ;
#116147 = ORIENTED_EDGE ( 'NONE', *, *, #201196, .T. ) ;
#116149 = EDGE_CURVE ( 'NONE', #30084, #152240, #13924, .T. ) ;
#116148 = LINE ( 'NONE', #14495, #56668 ) ;
#116150 = CARTESIAN_POINT ( 'NONE',  ( -16.97683809663752186, 44.17636539615257618, -235.3901923532681053 ) ) ;
#116151 = AXIS2_PLACEMENT_3D ( 'NONE', #93104, #252172, #115243 ) ;
#116152 = ORIENTED_EDGE ( 'NONE', *, *, #35996, .F. ) ;
#116153 = ORIENTED_EDGE ( 'NONE', *, *, #135001, .F. ) ;
#116154 = VECTOR ( 'NONE', #190439, 1000.000000000000000 ) ;
#116155 = LINE ( 'NONE', #33, #18795 ) ;
#116156 = AXIS2_PLACEMENT_3D ( 'NONE', #153279, #227630, #192370 ) ;
#116157 = EDGE_LOOP ( 'NONE', ( #188722, #69234, #104943, #93271 ) ) ;
#116158 = DIRECTION ( 'NONE',  ( -0.000000000000000000, 0.9126074666063770380, 0.4088369013363281068 ) ) ;
#116160 = EDGE_LOOP ( 'NONE', ( #107839, #55080, #174456, #145208 ) ) ;
#116159 = AXIS2_PLACEMENT_3D ( 'NONE', #120596, #121873, #55749 ) ;
#116161 = CARTESIAN_POINT ( 'NONE',  ( 20.94999999999999574, 87.75000000001162448, -66.42310748452423752 ) ) ;
#116162 = ADVANCED_FACE ( 'NONE', ( #162741 ), #217540, .T. ) ;
#116163 = DIRECTION ( 'NONE',  ( 1.000000000000000000, -0.000000000000000000, 0.000000000000000000 ) ) ;
#116164 = FACE_OUTER_BOUND ( 'NONE', #94875, .T. ) ;
#116165 = DIRECTION ( 'NONE',  ( 1.000000000000000000, 0.000000000000000000, -0.000000000000000000 ) ) ;
#116166 = CIRCLE ( 'NONE', #16212, 7.800000000000001599 ) ;
#116167 = TOROIDAL_SURFACE ( 'NONE', #53790, 12.97499999999999787, 0.1000000000000000056 ) ;
#116168 = CARTESIAN_POINT ( 'NONE',  ( -21.05000000000000071, 74.83729825007388570, -95.12310748452432563 ) ) ;
#116169 = VECTOR ( 'NONE', #230623, 1000.000000000000000 ) ;
#116170 = SPHERICAL_SURFACE ( 'NONE', #103046, 0.1000000000000000056 ) ;
#116171 = CARTESIAN_POINT ( 'NONE',  ( 20.12500000000000000, 9.749999999999998224, -8.111771282114276005 ) ) ;
#116172 = EDGE_LOOP ( 'NONE', ( #39508, #46000, #53294, #191219 ) ) ;
#116174 = CARTESIAN_POINT ( 'NONE',  ( 18.59999999999999076, 69.45000000001199680, -115.3731074845243398 ) ) ;
#116173 = DIRECTION ( 'NONE',  ( 0.000000000000000000, -2.775557561562888827E-14, 1.000000000000000000 ) ) ;
#116175 = ORIENTED_EDGE ( 'NONE', *, *, #131018, .F. ) ;
#116178 = EDGE_LOOP ( 'NONE', ( #12310, #131085, #106832, #148971 ) ) ;
#116177 = CARTESIAN_POINT ( 'NONE',  ( -18.41353343127311248, 85.50000000001161027, -62.49103808782458458 ) ) ;
#116176 = FACE_OUTER_BOUND ( 'NONE', #121916, .T. ) ;
#116179 = ADVANCED_FACE ( 'NONE', ( #20665 ), #143136, .T. ) ;
#116180 = CIRCLE ( 'NONE', #120303, 0.09999999999999939493 ) ;
#116181 = VERTEX_POINT ( 'NONE', #178466 ) ;
#116182 = CARTESIAN_POINT ( 'NONE',  ( 20.95000000000005258, 66.15000000001120384, -4.623107484524796362 ) ) ;
#116183 = CIRCLE ( 'NONE', #37078, 12.87499999999999822 ) ;
#116184 = CIRCLE ( 'NONE', #232698, 0.09999999999998898659 ) ;
#116185 = CARTESIAN_POINT ( 'NONE',  ( 13.22261339317535445, 66.56344716000785411, -154.8451520117640996 ) ) ;
#116186 = AXIS2_PLACEMENT_3D ( 'NONE', #109520, #229488, #92522 ) ;
#116187 = DIRECTION ( 'NONE',  ( 1.000000000000000000, 0.000000000000000000, 0.000000000000000000 ) ) ;
#116188 = DIRECTION ( 'NONE',  ( 0.000000000000000000, 0.000000000000000000, 1.000000000000000000 ) ) ;
#116189 = ORIENTED_EDGE ( 'NONE', *, *, #137200, .T. ) ;
#116191 = EDGE_LOOP ( 'NONE', ( #16565, #117164, #132714, #138847 ) ) ;
#116190 = CARTESIAN_POINT ( 'NONE',  ( -20.54999999999999716, 4.349999999999999645, -12.35000000000000142 ) ) ;
#116192 = CIRCLE ( 'NONE', #257562, 0.1000000000000001027 ) ;
#116193 = EDGE_CURVE ( 'NONE', #116101, #218186, #155425, .T. ) ;
#116195 = DIRECTION ( 'NONE',  ( 0.000000000000000000, -1.000000000000000000, -6.352154140967427193E-15 ) ) ;
#116194 = CARTESIAN_POINT ( 'NONE',  ( 18.39999999999999858, -9.599999999988845900, -107.1001893912220879 ) ) ;
#116197 = EDGE_LOOP ( 'NONE', ( #65246, #30984, #101098, #71097 ) ) ;
#116196 = CYLINDRICAL_SURFACE ( 'NONE', #247437, 12.87500000000000178 ) ;
#116198 = EDGE_CURVE ( 'NONE', #164331, #186491, #220139, .T. ) ;
#116199 = ADVANCED_FACE ( 'NONE', ( #1048 ), #80589, .T. ) ;
#116200 = PRODUCT_DEFINITION_SHAPE ( 'NONE', 'NONE',  #258114 ) ;
#116201 = ORIENTED_EDGE ( 'NONE', *, *, #78697, .F. ) ;
#116202 = EDGE_CURVE ( 'NONE', #143129, #33310, #181018, .T. ) ;
#116203 = CIRCLE ( 'NONE', #187116, 0.09999999999998898659 ) ;
#116204 = CARTESIAN_POINT ( 'NONE',  ( 20.95203847575071521, 11.87081995860093819, -206.1591156951000130 ) ) ;
#116205 = CARTESIAN_POINT ( 'NONE',  ( -16.85718274719362597, 44.04571297885565428, -235.3105011521292909 ) ) ;
#116206 = ORIENTED_EDGE ( 'NONE', *, *, #31808, .T. ) ;
#116207 = CARTESIAN_POINT ( 'NONE',  ( 20.94999999999999929, 1.835341550235569663, -145.5551512925629822 ) ) ;
#116208 = ORIENTED_EDGE ( 'NONE', *, *, #188434, .F. ) ;
#116209 = EDGE_CURVE ( 'NONE', #98368, #161437, #63813, .T. ) ;
#116210 = CARTESIAN_POINT ( 'NONE',  ( -20.64999999999999858, 82.09643798151613225, -215.4278993322501208 ) ) ;
#116211 = DIRECTION ( 'NONE',  ( 1.000000000000000000, 0.000000000000000000, -0.000000000000000000 ) ) ;
#116212 = ORIENTED_EDGE ( 'NONE', *, *, #150456, .T. ) ;
#116213 = DIRECTION ( 'NONE',  ( -0.000000000000000000, -0.000000000000000000, -1.000000000000000000 ) ) ;
#116214 = CIRCLE ( 'NONE', #158556, 0.09999999999999996392 ) ;
#116215 = TOROIDAL_SURFACE ( 'NONE', #91065, 0.2000000000000000111, 0.1000000000000000056 ) ;
#116216 = AXIS2_PLACEMENT_3D ( 'NONE', #67658, #168093, #248873 ) ;
#116217 = DIRECTION ( 'NONE',  ( 0.000000000000000000, 0.8660254037844385966, -0.5000000000000003331 ) ) ;
#116218 = CIRCLE ( 'NONE', #20542, 11.80000000000000426 ) ;
#116219 = ADVANCED_FACE ( 'NONE', ( #187433 ), #127449, .T. ) ;
#116220 = ORIENTED_EDGE ( 'NONE', *, *, #34449, .T. ) ;
#116221 = VERTEX_POINT ( 'NONE', #46600 ) ;
#116222 = CARTESIAN_POINT ( 'NONE',  ( 20.94999999999999929, 1.115600667400684642E-11, -131.1000000000000227 ) ) ;
#116223 = VERTEX_POINT ( 'NONE', #88286 ) ;
#116224 = ORIENTED_EDGE ( 'NONE', *, *, #192144, .T. ) ;
#116226 = ORIENTED_EDGE ( 'NONE', *, *, #110653, .F. ) ;
#116225 = DIRECTION ( 'NONE',  ( 0.000000000000000000, 0.4930308989874980785, 0.8700118002898462599 ) ) ;
#116227 = ADVANCED_FACE ( 'NONE', ( #126146 ), #255283, .T. ) ;
#116228 = EDGE_CURVE ( 'NONE', #209659, #86629, #109149, .T. ) ;
#116229 = ORIENTED_EDGE ( 'NONE', *, *, #139362, .T. ) ;
#116230 = DIRECTION ( 'NONE',  ( 0.000000000000000000, 6.467318590049456648E-15, -1.000000000000000000 ) ) ;
#116231 = AXIS2_PLACEMENT_3D ( 'NONE', #15696, #155208, #56043 ) ;
#116234 = ORIENTED_EDGE ( 'NONE', *, *, #155616, .F. ) ;
#116233 = VERTEX_POINT ( 'NONE', #246120 ) ;
#116232 = CARTESIAN_POINT ( 'NONE',  ( 20.04142135623730070, 11.75000000001115907, -192.1499999999999488 ) ) ;
#116235 = AXIS2_PLACEMENT_3D ( 'NONE', #51071, #5542, #224604 ) ;
#116236 = EDGE_LOOP ( 'NONE', ( #202168, #53066, #73835, #219439 ) ) ;
#116237 = DIRECTION ( 'NONE',  ( 0.000000000000000000, 0.2617529984164506107, 0.9651348961777299618 ) ) ;
#116238 = CIRCLE ( 'NONE', #74758, 14.30833333333333890 ) ;
#116239 = CARTESIAN_POINT ( 'NONE',  ( 20.04999999999999716, 67.25000000001178080, -82.17310748452437963 ) ) ;
#116240 = CARTESIAN_POINT ( 'NONE',  ( 23.14999999999999858, 67.92720994251783395, -214.1870976236629929 ) ) ;
#116241 = VERTEX_POINT ( 'NONE', #206987 ) ;
#116242 = CARTESIAN_POINT ( 'NONE',  ( -16.93826681692523195, 10.01142872029886632, -154.9454584673594582 ) ) ;
#116244 = ORIENTED_EDGE ( 'NONE', *, *, #151524, .T. ) ;
#116243 = CARTESIAN_POINT ( 'NONE',  ( -21.04999999999994387, 74.94272479589878344, -3.123107484524795474 ) ) ;
#116245 = DIRECTION ( 'NONE',  ( 0.000000000000000000, 0.000000000000000000, 1.000000000000000000 ) ) ;
#116246 = ORIENTED_EDGE ( 'NONE', *, *, #179507, .F. ) ;
#116247 = VERTEX_POINT ( 'NONE', #144410 ) ;
#116248 = DIRECTION ( 'NONE',  ( -1.000000000000000000, -2.952720810173289112E-16, 0.000000000000000000 ) ) ;
#116250 = EDGE_CURVE ( 'NONE', #74869, #203555, #72202, .T. ) ;
#116249 = CARTESIAN_POINT ( 'NONE',  ( 18.54116936837188589, 85.46356419838433283, -95.97456499363596549 ) ) ;
#116251 = ORIENTED_EDGE ( 'NONE', *, *, #74938, .F. ) ;
#116252 = EDGE_LOOP ( 'NONE', ( #102746, #9737, #84842, #102975 ) ) ;
#116253 = CARTESIAN_POINT ( 'NONE',  ( -16.93262454970420094, 10.00202046794151300, -180.0729237737626534 ) ) ;
#116255 = ORIENTED_EDGE ( 'NONE', *, *, #170864, .F. ) ;
#116254 = ORIENTED_EDGE ( 'NONE', *, *, #69680, .T. ) ;
#116256 = EDGE_LOOP ( 'NONE', ( #204799, #70358, #225479, #95698, #66837, #14544, #195149, #64372, #235359 ) ) ;
#116257 = CARTESIAN_POINT ( 'NONE',  ( 16.27683809663749770, 9.350000000011137402, -109.7500000000000426 ) ) ;
#116258 = EDGE_LOOP ( 'NONE', ( #178714, #195249, #123893, #172756 ) ) ;
#116259 = ORIENTED_EDGE ( 'NONE', *, *, #202124, .F. ) ;
#116260 = DIRECTION ( 'NONE',  ( 0.000000000000000000, 0.000000000000000000, 1.000000000000000000 ) ) ;
#116261 = ORIENTED_EDGE ( 'NONE', *, *, #132217, .T. ) ;
#116262 = DIRECTION ( 'NONE',  ( 0.000000000000000000, -1.000000000000000000, 0.000000000000000000 ) ) ;
#116263 = CARTESIAN_POINT ( 'NONE',  ( 23.14999999999999858, 70.50000000001205080, -124.1178414656112352 ) ) ;
#116264 = ORIENTED_EDGE ( 'NONE', *, *, #210708, .T. ) ;
#116265 = EDGE_CURVE ( 'NONE', #40869, #231259, #205686, .T. ) ;
#116266 = ORIENTED_EDGE ( 'NONE', *, *, #77976, .F. ) ;
#116267 = AXIS2_PLACEMENT_3D ( 'NONE', #174525, #31146, #253986 ) ;
#116268 = DIRECTION ( 'NONE',  ( 0.000000000000000000, 0.000000000000000000, 1.000000000000000000 ) ) ;
#116269 = CIRCLE ( 'NONE', #16319, 0.09999999999999939493 ) ;
#116270 = EDGE_CURVE ( 'NONE', #185056, #210716, #165289, .T. ) ;
#116271 = CIRCLE ( 'NONE', #178836, 0.09999999999999834022 ) ;
#116272 = CONICAL_SURFACE ( 'NONE', #145463, 4.050000000000006040, 0.7853981633974604915 ) ;
#116273 = ORIENTED_EDGE ( 'NONE', *, *, #87094, .F. ) ;
#116274 = EDGE_CURVE ( 'NONE', #57537, #246198, #147194, .T. ) ;
#116275 = AXIS2_PLACEMENT_3D ( 'NONE', #192054, #92916, #172523 ) ;
#116276 = DIRECTION ( 'NONE',  ( 0.000000000000000000, 6.938893903907222067E-15, -1.000000000000000000 ) ) ;
#116277 = EDGE_CURVE ( 'NONE', #65124, #29396, #51303, .T. ) ;
#116278 = ORIENTED_EDGE ( 'NONE', *, *, #150810, .F. ) ;
#116279 = VERTEX_POINT ( 'NONE', #25780 ) ;
#116280 = CARTESIAN_POINT ( 'NONE',  ( 20.85000000000000142, -11.74999999998883560, -131.1000000000000227 ) ) ;
#116282 = VERTEX_POINT ( 'NONE', #183576 ) ;
#116281 = CARTESIAN_POINT ( 'NONE',  ( 18.46947024752544309, 85.50929715716830515, -163.0364180358262445 ) ) ;
#116283 = CARTESIAN_POINT ( 'NONE',  ( 21.13614978966381841, 1.115456470629326115E-11, -127.5008952981661565 ) ) ;
#116284 = DIRECTION ( 'NONE',  ( 1.000000000000000000, 7.304098846218105085E-16, 4.217023435051676515E-16 ) ) ;
#116285 = VERTEX_POINT ( 'NONE', #29662 ) ;
#116286 = FACE_OUTER_BOUND ( 'NONE', #254968, .T. ) ;
#116287 = FACE_OUTER_BOUND ( 'NONE', #110805, .T. ) ;
#116288 = CARTESIAN_POINT ( 'NONE',  ( 18.57071067811864040, 65.82071067813089371, -148.6731074845244223 ) ) ;
#116289 = LINE ( 'NONE', #100523, #52384 ) ;
#116291 = DIRECTION ( 'NONE',  ( 0.000000000000000000, -1.000000000000000000, -1.445602896647339410E-16 ) ) ;
#116290 = AXIS2_PLACEMENT_3D ( 'NONE', #21947, #183582, #164021 ) ;
#116293 = CARTESIAN_POINT ( 'NONE',  ( -20.85000000000000142, 7.021664781911246322, -70.83356540189728889 ) ) ;
#116292 = CIRCLE ( 'NONE', #99675, 6.329289321881370611 ) ;
#116294 = CARTESIAN_POINT ( 'NONE',  ( -21.05000000000000071, -1.261786168553869603, -142.0864989635454947 ) ) ;
#116295 = VECTOR ( 'NONE', #46519, 1000.000000000000114 ) ;
#116296 = CARTESIAN_POINT ( 'NONE',  ( 21.05000000000000071, 76.10000000001215881, -143.0001538663141503 ) ) ;
#116297 = CARTESIAN_POINT ( 'NONE',  ( 18.59999999999999076, 11.75000000001115907, -142.1000000000000227 ) ) ;
#116298 = ORIENTED_EDGE ( 'NONE', *, *, #51237, .T. ) ;
#116300 = EDGE_CURVE ( 'NONE', #88769, #167256, #93030, .T. ) ;
#116299 = TOROIDAL_SURFACE ( 'NONE', #203765, 0.2000000000000000111, 0.1000000000000000056 ) ;
#116301 = ADVANCED_FACE ( 'NONE', ( #167889 ), #66192, .T. ) ;
#116303 = ORIENTED_EDGE ( 'NONE', *, *, #78876, .F. ) ;
#116302 = EDGE_LOOP ( 'NONE', ( #166533, #56922, #84421, #113102 ) ) ;
#116304 = VERTEX_POINT ( 'NONE', #67465 ) ;
#116305 = CARTESIAN_POINT ( 'NONE',  ( 18.39999999999999503, 11.47316190336248454, -12.65000000000000213 ) ) ;
#116306 = DIRECTION ( 'NONE',  ( -1.000000000000000000, 0.000000000000000000, 0.000000000000000000 ) ) ;
#116308 = LINE ( 'NONE', #139683, #190423 ) ;
#116307 = FACE_OUTER_BOUND ( 'NONE', #45139, .T. ) ;
#116309 = ORIENTED_EDGE ( 'NONE', *, *, #61159, .F. ) ;
#116310 = DIRECTION ( 'NONE',  ( 0.000000000000000000, -0.9999176327611369874, 0.01283462868041984617 ) ) ;
#116311 = PRESENTATION_STYLE_ASSIGNMENT (( #112459 ) ) ;
#116312 = EDGE_CURVE ( 'NONE', #69711, #7639, #88731, .T. ) ;
#116313 = DIRECTION ( 'NONE',  ( 6.484947573744954877E-15, 0.9274965247785529332, -0.3738317757009255171 ) ) ;
#116314 = CARTESIAN_POINT ( 'NONE',  ( 18.79999999999999716, 1.350000000000000089, 16.60000000000000142 ) ) ;
#116315 = EDGE_CURVE ( 'NONE', #50700, #237460, #70068, .T. ) ;
#116316 = CARTESIAN_POINT ( 'NONE',  ( -21.05000000000000071, 57.81354981234518675, -226.1844220500876474 ) ) ;
#116317 = EDGE_LOOP ( 'NONE', ( #67947, #21590, #148663, #247699 ) ) ;
#116318 = ORIENTED_EDGE ( 'NONE', *, *, #256341, .T. ) ;
#116319 = AXIS2_PLACEMENT_3D ( 'NONE', #91418, #232225, #52258 ) ;
#116320 = CARTESIAN_POINT ( 'NONE',  ( -23.15000000000000213, 11.60058429089262333, -246.3380203656811887 ) ) ;
#116321 = ORIENTED_EDGE ( 'NONE', *, *, #191408, .T. ) ;
#116322 = DIRECTION ( 'NONE',  ( 1.000000000000000000, 0.000000000000000000, 0.000000000000000000 ) ) ;
#116323 = CARTESIAN_POINT ( 'NONE',  ( 18.49362639424905552, 77.26503896671080440, -241.7069646862937304 ) ) ;
#116324 = CIRCLE ( 'NONE', #82949, 0.1000000000000053763 ) ;
#116325 = DIRECTION ( 'NONE',  ( -1.000000000000000000, 0.000000000000000000, 0.000000000000000000 ) ) ;
#116326 = ADVANCED_FACE ( 'NONE', ( #6201 ), #229117, .F. ) ;
#116327 = DIRECTION ( 'NONE',  ( 1.000000000000000000, 0.000000000000000000, 0.000000000000000000 ) ) ;
#116328 = FACE_OUTER_BOUND ( 'NONE', #94216, .T. ) ;
#116329 = ORIENTED_EDGE ( 'NONE', *, *, #140919, .F. ) ;
#116330 = DIRECTION ( 'NONE',  ( 0.000000000000000000, 0.000000000000000000, -1.000000000000000000 ) ) ;
#116331 = LINE ( 'NONE', #17233, #72510 ) ;
#116332 = DIRECTION ( 'NONE',  ( 1.000000000000000000, 0.000000000000000000, 0.000000000000000000 ) ) ;
#116334 = DIRECTION ( 'NONE',  ( 1.000000000000000000, 0.000000000000000000, 0.000000000000000000 ) ) ;
#116333 = DIRECTION ( 'NONE',  ( 0.000000000000000000, 0.000000000000000000, 1.000000000000000000 ) ) ;
#116335 = DIRECTION ( 'NONE',  ( 0.000000000000000000, 0.000000000000000000, -1.000000000000000000 ) ) ;
#116337 = ADVANCED_FACE ( 'NONE', ( #208282 ), #68763, .T. ) ;
#116336 = CARTESIAN_POINT ( 'NONE',  ( -16.92563707711778065, 9.968990694407935393, -121.3807582995240040 ) ) ;
#116338 = AXIS2_PLACEMENT_3D ( 'NONE', #145197, #42269, #163494 ) ;
#116339 = DIRECTION ( 'NONE',  ( 0.000000000000000000, -1.000000000000000000, 0.000000000000000000 ) ) ;
#116340 = DIRECTION ( 'NONE',  ( 0.000000000000000000, 0.9887567792719329507, 0.1495327102803732933 ) ) ;
#116341 = AXIS2_PLACEMENT_3D ( 'NONE', #171553, #48999, #208099 ) ;
#116342 = ORIENTED_EDGE ( 'NONE', *, *, #19366, .F. ) ;
#116343 = VECTOR ( 'NONE', #130843, 1000.000000000000000 ) ;
#116344 = ORIENTED_EDGE ( 'NONE', *, *, #2473, .T. ) ;
#116345 = CARTESIAN_POINT ( 'NONE',  ( 21.72449340488910252, 10.28395627750227526, -76.25000000000004263 ) ) ;
#116346 = ORIENTED_EDGE ( 'NONE', *, *, #142950, .T. ) ;
#116347 = EDGE_CURVE ( 'NONE', #247506, #14875, #4900, .T. ) ;
#116348 = DIRECTION ( 'NONE',  ( 0.000000000000000000, 0.9915357197604862671, -0.1298341882519953583 ) ) ;
#116349 = CIRCLE ( 'NONE', #3907, 0.1000000000000053901 ) ;
#116350 = CIRCLE ( 'NONE', #66449, 0.1999999999999987899 ) ;
#116351 =( NAMED_UNIT ( * ) SI_UNIT ( $, .STERADIAN. ) SOLID_ANGLE_UNIT ( ) );
#116352 = CARTESIAN_POINT ( 'NONE',  ( 22.39999999999999858, 76.00000000001195133, -103.0231074845243171 ) ) ;
#116353 = ORIENTED_EDGE ( 'NONE', *, *, #36559, .T. ) ;
#116354 = DIRECTION ( 'NONE',  ( 0.000000000000000000, 0.000000000000000000, 1.000000000000000000 ) ) ;
#116355 = AXIS2_PLACEMENT_3D ( 'NONE', #146852, #68633, #227687 ) ;
#116356 = CIRCLE ( 'NONE', #3924, 11.70000000000001528 ) ;
#116357 = CARTESIAN_POINT ( 'NONE',  ( -22.39999999999999858, 75.90000000001236913, -170.0231074845243597 ) ) ;
#116358 = CARTESIAN_POINT ( 'NONE',  ( -21.05000000000000071, 0.000000000000000000, 0.000000000000000000 ) ) ;
#116359 = AXIS2_PLACEMENT_3D ( 'NONE', #24574, #162794, #200626 ) ;
#116360 = CARTESIAN_POINT ( 'NONE',  ( -33.72168855820452649, 52.34166666667870516, -119.7731074845244592 ) ) ;
#116362 = ORIENTED_EDGE ( 'NONE', *, *, #228510, .T. ) ;
#116361 = CARTESIAN_POINT ( 'NONE',  ( -20.00857864376270001, 66.65000000001229807, -157.7731074845244166 ) ) ;
#116364 = DIRECTION ( 'NONE',  ( 0.000000000000000000, -0.2617529984165031243, -0.9651348961777157509 ) ) ;
#116363 = CARTESIAN_POINT ( 'NONE',  ( 20.12500000000000000, 9.750000000011153745, -54.75000000000000000 ) ) ;
#116365 = AXIS2_PLACEMENT_3D ( 'NONE', #49248, #229184, #11423 ) ;
#116366 = DIRECTION ( 'NONE',  ( 0.000000000000000000, 0.4088369013363287729, -0.9126074666063767049 ) ) ;
#116367 = CARTESIAN_POINT ( 'NONE',  ( 20.99142135623731065, 64.40000000001194280, -109.9513107147998880 ) ) ;
#116368 = CARTESIAN_POINT ( 'NONE',  ( 19.97071067811864609, 11.72071067812981404, -91.65000000000004832 ) ) ;
#116369 = DIRECTION ( 'NONE',  ( -1.000000000000000000, 7.304098846218134667E-16, 5.100424963727256530E-30 ) ) ;
#116370 = ORIENTED_EDGE ( 'NONE', *, *, #74399, .T. ) ;
#116371 = DIRECTION ( 'NONE',  ( 1.000000000000000000, 0.000000000000000000, 0.000000000000000000 ) ) ;
#116372 = DIRECTION ( 'NONE',  ( 1.000000000000000000, 0.000000000000000000, 0.000000000000000000 ) ) ;
#116373 = ORIENTED_EDGE ( 'NONE', *, *, #155642, .F. ) ;
#116374 = LINE ( 'NONE', #17275, #152809 ) ;
#116376 = ORIENTED_EDGE ( 'NONE', *, *, #9386, .T. ) ;
#116375 = AXIS2_PLACEMENT_3D ( 'NONE', #161846, #242629, #100522 ) ;
#116377 = CARTESIAN_POINT ( 'NONE',  ( 18.49999999999945999, 54.99804363260582818, -230.1039092834927828 ) ) ;
#116378 = CARTESIAN_POINT ( 'NONE',  ( 21.05000000000000071, 10.29970289650803572, -222.9162226222096308 ) ) ;
#116379 = FACE_OUTER_BOUND ( 'NONE', #210513, .T. ) ;
#116380 = VERTEX_POINT ( 'NONE', #231700 ) ;
#116381 = EDGE_LOOP ( 'NONE', ( #69122, #75185, #205759, #211420 ) ) ;
#116382 = CIRCLE ( 'NONE', #66319, 11.65000000000000036 ) ;
#116383 = CARTESIAN_POINT ( 'NONE',  ( 20.97239005616515684, 8.874843841361279573, -112.7501528021532238 ) ) ;
#116384 = DIRECTION ( 'NONE',  ( 1.000000000000000000, 0.000000000000000000, 0.000000000000000000 ) ) ;
#116385 = DIRECTION ( 'NONE',  ( 1.000000000000000000, 0.000000000000000000, 0.000000000000000000 ) ) ;
#116386 = EDGE_CURVE ( 'NONE', #135869, #119689, #221986, .T. ) ;
#116387 = VECTOR ( 'NONE', #108595, 1000.000000000000000 ) ;
#116389 = DIRECTION ( 'NONE',  ( 0.000000000000000000, 1.000000000000000000, 0.000000000000000000 ) ) ;
#116388 = DIRECTION ( 'NONE',  ( 1.000000000000000000, 0.000000000000000000, 0.000000000000000000 ) ) ;
#116390 = DIRECTION ( 'NONE',  ( 0.000000000000000000, 0.000000000000000000, 1.000000000000000000 ) ) ;
#116391 = CARTESIAN_POINT ( 'NONE',  ( 12.25000000000000000, 9.350000000011140955, -50.24999999999999289 ) ) ;
#116392 = DIRECTION ( 'NONE',  ( -0.000000000000000000, 0.4721928772777345684, 0.8814952561688429444 ) ) ;
#116393 = ORIENTED_EDGE ( 'NONE', *, *, #102963, .F. ) ;
#116394 = DIRECTION ( 'NONE',  ( 1.000000000000000000, 0.000000000000000000, 0.000000000000000000 ) ) ;
#116395 = TOROIDAL_SURFACE ( 'NONE', #199613, 12.97499999999999787, 0.1000000000000000056 ) ;
#116397 = ORIENTED_EDGE ( 'NONE', *, *, #13208, .F. ) ;
#116396 = DIRECTION ( 'NONE',  ( 0.000000000000000000, 0.000000000000000000, -1.000000000000000000 ) ) ;
#116398 = CARTESIAN_POINT ( 'NONE',  ( 22.48660254037844197, 11.65000000000000036, 0.04999999999999833050 ) ) ;
#116399 = DIRECTION ( 'NONE',  ( 1.000000000000000000, 2.952720810173289112E-16, -0.000000000000000000 ) ) ;
#116401 = CARTESIAN_POINT ( 'NONE',  ( 22.47071067811865319, 7.128833340093095217, -233.7327013124392749 ) ) ;
#116400 = LINE ( 'NONE', #233780, #84265 ) ;
#116402 = EDGE_CURVE ( 'NONE', #176438, #244844, #209555, .T. ) ;
#116403 = ORIENTED_EDGE ( 'NONE', *, *, #103489, .T. ) ;
#116405 = LINE ( 'NONE', #173854, #30091 ) ;
#116404 = DIRECTION ( 'NONE',  ( 0.000000000000000000, 0.000000000000000000, -1.000000000000000000 ) ) ;
#116406 = CARTESIAN_POINT ( 'NONE',  ( 18.59999999999999787, 78.45218979564165807, -232.7313097695096076 ) ) ;
#116407 = CYLINDRICAL_SURFACE ( 'NONE', #176089, 0.1000000000000028644 ) ;
#116408 = PLANE ( 'NONE',  #182601 ) ;
#116409 = DIRECTION ( 'NONE',  ( 1.000000000000000000, -0.000000000000000000, 0.000000000000000000 ) ) ;
#116410 = VERTEX_POINT ( 'NONE', #90881 ) ;
#116411 = CARTESIAN_POINT ( 'NONE',  ( 18.48536876927993688, -7.746817490806097162, -209.9010216391053802 ) ) ;
#116414 = EDGE_CURVE ( 'NONE', #248047, #50036, #193003, .T. ) ;
#116413 = VERTEX_POINT ( 'NONE', #193848 ) ;
#116412 = AXIS2_PLACEMENT_3D ( 'NONE', #43904, #891, #62191 ) ;
#116415 = AXIS2_PLACEMENT_3D ( 'NONE', #71971, #31585, #12010 ) ;
#116416 = DIRECTION ( 'NONE',  ( 2.952720810173289112E-16, -1.000000000000000000, 0.000000000000000000 ) ) ;
#116417 = EDGE_LOOP ( 'NONE', ( #162367, #156882, #227243, #60756 ) ) ;
#116418 = CARTESIAN_POINT ( 'NONE',  ( -18.59999999999999787, -9.321008403350132809, -141.2359382490778899 ) ) ;
#116419 = AXIS2_PLACEMENT_3D ( 'NONE', #57882, #194869, #78731 ) ;
#116420 = VERTEX_POINT ( 'NONE', #135128 ) ;
#116421 = DIRECTION ( 'NONE',  ( 0.000000000000000000, -0.7965107556683636014, 0.6046243595031649543 ) ) ;
#116422 = DIRECTION ( 'NONE',  ( 0.000000000000000000, -1.000000000000000000, -0.000000000000000000 ) ) ;
#116423 = EDGE_CURVE ( 'NONE', #145358, #9191, #150537, .T. ) ;
#116425 = EDGE_CURVE ( 'NONE', #234281, #139747, #30511, .T. ) ;
#116424 = DIRECTION ( 'NONE',  ( 0.000000000000000000, 0.2128009952263605897, -0.9770955615653315052 ) ) ;
#116426 = VERTEX_POINT ( 'NONE', #110444 ) ;
#116427 =( BOUNDED_SURFACE ( )  B_SPLINE_SURFACE ( 3, 2, ( 
 ( #11140, #47672, #48971 ),
 ( #51511, #150649, #72413 ),
 ( #110225, #28163, #148083 ),
 ( #108940, #30730, #149389 ),
 ( #89369, #32006, #8574 ),
 ( #166394, #225023, #88072 ),
 ( #249748, #245905, #107661 ),
 ( #127235, #227606, #68549 ),
 ( #12442, #146762, #91950 ),
 ( #189772, #188483, #171526 ),
 ( #46392, #206771, #230177 ),
 ( #226305, #125931, #128519 ) ),
 .UNSPECIFIED., .F., .F., .F. ) 
 B_SPLINE_SURFACE_WITH_KNOTS ( ( 4, 2, 2, 2, 2, 4 ),
 ( 3, 3 ),
 ( 3.174653483277205090, 3.943930578431714018, 4.713207673586222946, 5.482484768740731873, 5.867123316317986337, 6.251761863895240801 ),
 ( 0.000000000000000000, 1.000000000000000000 ),
 .UNSPECIFIED. ) 
 GEOMETRIC_REPRESENTATION_ITEM ( )  RATIONAL_B_SPLINE_SURFACE ( (
 ( 1.000000000000000000, 0.8659465255642401216, 1.000000000000000000),
 ( 1.000000000000000000, 0.8648614068488887918, 1.000000000000000000),
 ( 1.000000000000000000, 0.8489031841323232408, 1.000000000000000000),
 ( 1.000000000000000000, 0.7927507630162343721, 1.000000000000000000),
 ( 1.000000000000000000, 0.7523013859014273663, 1.000000000000000000),
 ( 1.000000000000000000, 0.6616226951191639394, 1.000000000000000000),
 ( 1.000000000000000000, 0.6112214368725455982, 1.000000000000000000),
 ( 1.000000000000000000, 0.5507684314497544031, 1.000000000000000000),
 ( 1.000000000000000000, 0.5333267243152143289, 1.000000000000000000),
 ( 1.000000000000000000, 0.5084565446480221462, 1.000000000000000000),
 ( 1.000000000000000000, 0.5010722703450330995, 1.000000000000000000),
 ( 1.000000000000000000, 0.5001234037138393429, 1.000000000000000000) ) ) 
 REPRESENTATION_ITEM ( '' )  SURFACE ( )  );
#116428 = EDGE_CURVE ( 'NONE', #19640, #213808, #255027, .T. ) ;
#116429 = CARTESIAN_POINT ( 'NONE',  ( -22.39999999999999858, 76.10085836911075319, -114.7726746080137019 ) ) ;
#116430 = DIRECTION ( 'NONE',  ( 0.000000000000000000, 0.000000000000000000, -1.000000000000000000 ) ) ;
#116431 = CARTESIAN_POINT ( 'NONE',  ( -20.94999999999999929, 68.97833521811203639, -132.6895420826271277 ) ) ;
#116433 = AXIS2_PLACEMENT_3D ( 'NONE', #66412, #225459, #46823 ) ;
#116432 = CARTESIAN_POINT ( 'NONE',  ( -17.01473183483381035, 60.96553306590055854, -220.9452142459682875 ) ) ;
#116434 = CARTESIAN_POINT ( 'NONE',  ( -21.14999999999999858, 76.10000000001241460, -176.5637644362255969 ) ) ;
#116435 = ORIENTED_EDGE ( 'NONE', *, *, #227411, .F. ) ;
#116436 = CARTESIAN_POINT ( 'NONE',  ( 20.85000000000000142, 45.93315328338058379, -256.6017782078560003 ) ) ;
#116437 = VERTEX_POINT ( 'NONE', #76448 ) ;
#116439 = ORIENTED_EDGE ( 'NONE', *, *, #60452, .F. ) ;
#116438 = DIRECTION ( 'NONE',  ( 0.7071067811865475727, -0.7071067811865475727, -4.937700262164531476E-15 ) ) ;
#116440 = VERTEX_POINT ( 'NONE', #131293 ) ;
#116441 = FACE_OUTER_BOUND ( 'NONE', #222016, .T. ) ;
#116442 = EDGE_CURVE ( 'NONE', #237280, #20561, #110357, .T. ) ;
#116443 = DIRECTION ( 'NONE',  ( -0.7071067811865214825, -0.7071067811865735520, 0.000000000000000000 ) ) ;
#116444 = CARTESIAN_POINT ( 'NONE',  ( -21.05000000000000071, 55.49311008795314137, -234.6486875357297492 ) ) ;
#116445 = DIRECTION ( 'NONE',  ( -1.836970198721029934E-16, -1.000000000000000000, -6.982962677686266711E-15 ) ) ;
#116446 = VERTEX_POINT ( 'NONE', #152174 ) ;
#116447 = CARTESIAN_POINT ( 'NONE',  ( -16.90137573187933384, 9.950000000011137047, -146.7884174240969628 ) ) ;
#116448 = CARTESIAN_POINT ( 'NONE',  ( 20.04142135623730070, 64.35000000001150511, -48.17310748452440095 ) ) ;
#116449 = ORIENTED_EDGE ( 'NONE', *, *, #33516, .F. ) ;
#116451 = ORIENTED_EDGE ( 'NONE', *, *, #87919, .F. ) ;
#116450 = DIRECTION ( 'NONE',  ( -1.000000000000000000, 0.000000000000000000, -0.000000000000000000 ) ) ;
#116453 = EDGE_CURVE ( 'NONE', #127095, #205367, #253794, .T. ) ;
#116452 = CYLINDRICAL_SURFACE ( 'NONE', #185718, 0.1000000000000013933 ) ;
#116454 = TOROIDAL_SURFACE ( 'NONE', #153915, 0.4000000000000005773, 0.1000000000000000056 ) ;
#116455 = CIRCLE ( 'NONE', #4007, 0.4000000000000010214 ) ;
#116456 = CIRCLE ( 'NONE', #212321, 0.09999999999999939493 ) ;
#116458 = CIRCLE ( 'NONE', #99833, 0.1000000000000046685 ) ;
#116457 = CARTESIAN_POINT ( 'NONE',  ( 21.14999999999999858, 6.540656951712400691, -100.5000000000000284 ) ) ;
#116459 = EDGE_LOOP ( 'NONE', ( #145822, #237759, #20243, #179122 ) ) ;
#116460 =( BOUNDED_SURFACE ( )  B_SPLINE_SURFACE ( 3, 2, ( 
 ( #201374, #3156, #85247 ),
 ( #125690, #44879, #124424 ),
 ( #240504, #164833, #61877 ),
 ( #46153, #43597, #7030 ),
 ( #65720, #146521, #224778 ),
 ( #141398, #205214, #220922 ),
 ( #183115, #42308, #203946 ),
 ( #206519, #222198, #121856 ),
 ( #4451, #244347, #145245 ),
 ( #83948, #47425, #26620 ) ),
 .UNSPECIFIED., .F., .F., .F. ) 
 B_SPLINE_SURFACE_WITH_KNOTS ( ( 4, 2, 2, 2, 4 ),
 ( 3, 3 ),
 ( 0.002161241639767248670, 0.002579950749615824400, 0.002789305304540112482, 0.002893982582002256523, 0.002998659859464400564 ),
 ( 0.000000000000000000, 1.000000000000000000 ),
 .UNSPECIFIED. ) 
 GEOMETRIC_REPRESENTATION_ITEM ( )  RATIONAL_B_SPLINE_SURFACE ( (
 ( 1.000000000000000000, 0.7071067811865536790, 1.000000000000000000),
 ( 1.000000000000000000, 0.7632447400666954040, 1.000000000000000000),
 ( 1.000000000000000000, 0.8158073005106659670, 1.000000000000000000),
 ( 1.000000000000000000, 0.8906973462397590469, 1.000000000000000000),
 ( 1.000000000000000000, 0.9149408947800071745, 1.000000000000000000),
 ( 1.000000000000000000, 0.9493368785275861921, 1.000000000000000000),
 ( 1.000000000000000000, 0.9605194247156703113, 1.000000000000000000),
 ( 1.000000000000000000, 0.9803630264781235670, 1.000000000000000000),
 ( 1.000000000000000000, 0.9900844824271131106, 1.000000000000000000),
 ( 1.000000000000000000, 0.9894588281429246290, 1.000000000000000000) ) ) 
 REPRESENTATION_ITEM ( '' )  SURFACE ( )  );
#116461 = CIRCLE ( 'NONE', #74801, 11.65000000000000746 ) ;
#116462 = DIRECTION ( 'NONE',  ( 0.000000000000000000, 0.9910465087640865089, 0.1335171055202867274 ) ) ;
#116463 = ORIENTED_EDGE ( 'NONE', *, *, #72575, .F. ) ;
#116464 = CYLINDRICAL_SURFACE ( 'NONE', #163248, 4.049999999999998046 ) ;
#116465 = DIRECTION ( 'NONE',  ( 1.000000000000000000, 0.000000000000000000, 0.000000000000000000 ) ) ;
#116466 = CARTESIAN_POINT ( 'NONE',  ( 13.43663047529819998, 66.55335465531629779, -51.11230102842420564 ) ) ;
#116467 = DIRECTION ( 'NONE',  ( 0.000000000000000000, 0.9947597004326491632, -0.1022405907413782566 ) ) ;
#116468 = VECTOR ( 'NONE', #250091, 1000.000000000000000 ) ;
#116469 = AXIS2_PLACEMENT_3D ( 'NONE', #244598, #182077, #185916 ) ;
#116470 = VERTEX_POINT ( 'NONE', #113022 ) ;
#116471 = DIRECTION ( 'NONE',  ( 2.715809747126116508E-16, -1.000000000000000000, 0.000000000000000000 ) ) ;
#116472 = EDGE_CURVE ( 'NONE', #234500, #133719, #130446, .T. ) ;
#116473 = EDGE_CURVE ( 'NONE', #94706, #140520, #205619, .T. ) ;
#116474 = ORIENTED_EDGE ( 'NONE', *, *, #109828, .F. ) ;
#116475 = DIRECTION ( 'NONE',  ( 0.000000000000000000, 0.000000000000000000, -1.000000000000000000 ) ) ;
#116477 = ORIENTED_EDGE ( 'NONE', *, *, #46479, .T. ) ;
#116476 = CARTESIAN_POINT ( 'NONE',  ( -20.94999999999999929, 76.00000000001145395, -40.02310748452431710 ) ) ;
#116478 = CARTESIAN_POINT ( 'NONE',  ( -23.15000000000000213, 76.00000000001190870, -103.0231074845243029 ) ) ;
#116479 = CYLINDRICAL_SURFACE ( 'NONE', #149192, 0.5000000000000004441 ) ;
#116481 = EDGE_CURVE ( 'NONE', #135978, #88325, #93441, .T. ) ;
#116480 = DIRECTION ( 'NONE',  ( 0.000000000000000000, 0.000000000000000000, -1.000000000000000000 ) ) ;
#116483 = EDGE_CURVE ( 'NONE', #140969, #139968, #1621, .T. ) ;
#116482 = CARTESIAN_POINT ( 'NONE',  ( -23.25000000000000000, 76.00000000001126921, -203.5231074845248997 ) ) ;
#116484 = CARTESIAN_POINT ( 'NONE',  ( 18.49999999999998934, 69.45000000001158469, -59.50608031408435039 ) ) ;
#116485 = FACE_OUTER_BOUND ( 'NONE', #215630, .T. ) ;
#116486 = CARTESIAN_POINT ( 'NONE',  ( 22.39999999999999503, 11.75000000000000711, 0.09999999999999592548 ) ) ;
#116488 = ORIENTED_EDGE ( 'NONE', *, *, #147322, .T. ) ;
#116487 = CARTESIAN_POINT ( 'NONE',  ( -22.01447462590973103, 68.73619979878222352, -136.6221444845839130 ) ) ;
#116489 = ADVANCED_FACE ( 'NONE', ( #73927 ), #54312, .F. ) ;
#116490 = AXIS2_PLACEMENT_3D ( 'NONE', #157533, #55779, #180907 ) ;
#116491 = EDGE_CURVE ( 'NONE', #11331, #3782, #247131, .T. ) ;
#116493 = EDGE_CURVE ( 'NONE', #88973, #103882, #247319, .T. ) ;
#116492 = EDGE_CURVE ( 'NONE', #54060, #57422, #154739, .T. ) ;
#116494 = CARTESIAN_POINT ( 'NONE',  ( 23.15000000000000213, -8.663551401857999323, -57.47589888193269303 ) ) ;
#116495 = AXIS2_PLACEMENT_3D ( 'NONE', #111164, #152893, #90292 ) ;
#116496 = CARTESIAN_POINT ( 'NONE',  ( 18.49999999999999289, 68.97833521811203639, -132.6895420826271277 ) ) ;
#116497 = CARTESIAN_POINT ( 'NONE',  ( 22.00356870143220078, 68.74575763754050683, -103.0231074845243597 ) ) ;
#116498 = ORIENTED_EDGE ( 'NONE', *, *, #224582, .T. ) ;
#116499 = CARTESIAN_POINT ( 'NONE',  ( 18.49999999999999645, 77.83585931145570669, -125.0186683157258045 ) ) ;
#116500 = ADVANCED_FACE ( 'NONE', ( #37351 ), #21631, .T. ) ;
#116501 = CARTESIAN_POINT ( 'NONE',  ( -18.51555513499745942, 85.35265705451639917, -62.32793758882646529 ) ) ;
#116502 = ORIENTED_EDGE ( 'NONE', *, *, #18135, .F. ) ;
#116503 = EDGE_CURVE ( 'NONE', #141665, #111495, #77721, .T. ) ;
#116504 = EDGE_CURVE ( 'NONE', #75223, #136961, #151498, .T. ) ;
#116505 = CIRCLE ( 'NONE', #191547, 4.099999999999992539 ) ;
#116506 = DIRECTION ( 'NONE',  ( 0.000000000000000000, -6.982962677686266711E-15, 1.000000000000000000 ) ) ;
#116507 = AXIS2_PLACEMENT_3D ( 'NONE', #105814, #143677, #66723 ) ;
#116508 = DIRECTION ( 'NONE',  ( 0.000000000000000000, 0.000000000000000000, 1.000000000000000000 ) ) ;
#116509 = ADVANCED_FACE ( 'NONE', ( #141563 ), #140261, .T. ) ;
#116510 = ORIENTED_EDGE ( 'NONE', *, *, #23725, .T. ) ;
#116511 = CARTESIAN_POINT ( 'NONE',  ( -23.15000000000000213, 87.75000000001173817, -81.27310748452423184 ) ) ;
#116512 = TOROIDAL_SURFACE ( 'NONE', #16571, 0.2000000000000000111, 0.1000000000000000056 ) ;
#116513 = VERTEX_POINT ( 'NONE', #20361 ) ;
#116514 = DIRECTION ( 'NONE',  ( -0.000000000000000000, -1.000000000000000000, -6.982962677686266711E-15 ) ) ;
#116516 = ORIENTED_EDGE ( 'NONE', *, *, #198057, .F. ) ;
#116515 = DIRECTION ( 'NONE',  ( 0.000000000000000000, 6.982962677686266711E-15, -1.000000000000000000 ) ) ;
#116517 = EDGE_CURVE ( 'NONE', #34317, #163039, #134705, .T. ) ;
#116518 = AXIS2_PLACEMENT_3D ( 'NONE', #232128, #32674, #33961 ) ;
#116519 = CIRCLE ( 'NONE', #49868, 12.97499999999999964 ) ;
#116520 = PLANE ( 'NONE',  #85859 ) ;
#116521 = VERTEX_POINT ( 'NONE', #219812 ) ;
#116522 = SPHERICAL_SURFACE ( 'NONE', #151500, 0.1000000000000000056 ) ;
#116523 = ORIENTED_EDGE ( 'NONE', *, *, #246878, .F. ) ;
#116525 = ORIENTED_EDGE ( 'NONE', *, *, #206539, .T. ) ;
#116524 = ORIENTED_EDGE ( 'NONE', *, *, #166282, .T. ) ;
#116526 = DIRECTION ( 'NONE',  ( 1.000000000000000000, 0.000000000000000000, 0.000000000000000000 ) ) ;
#116527 = ORIENTED_EDGE ( 'NONE', *, *, #226682, .T. ) ;
#116528 = DIRECTION ( 'NONE',  ( 0.000000000000000000, 0.000000000000000000, -1.000000000000000000 ) ) ;
#116529 = ORIENTED_EDGE ( 'NONE', *, *, #243049, .F. ) ;
#116530 = AXIS2_PLACEMENT_3D ( 'NONE', #25572, #180793, #127230 ) ;
#116531 = CIRCLE ( 'NONE', #229137, 0.09999999999998898659 ) ;
#116532 = VECTOR ( 'NONE', #189446, 1000.000000000000000 ) ;
#116533 = VECTOR ( 'NONE', #86755, 1000.000000000000000 ) ;
#116534 = AXIS2_PLACEMENT_3D ( 'NONE', #231930, #252740, #153717 ) ;
#116535 = EDGE_LOOP ( 'NONE', ( #253428, #31480, #151541, #208041 ) ) ;
#116536 = CIRCLE ( 'NONE', #74871, 0.09999999999999520384 ) ;
#116537 = FACE_OUTER_BOUND ( 'NONE', #62132, .T. ) ;
#116538 = DIRECTION ( 'NONE',  ( -1.000000000000000000, 0.000000000000000000, 0.000000000000000000 ) ) ;
#116539 = VERTEX_POINT ( 'NONE', #196397 ) ;
#116540 = CARTESIAN_POINT ( 'NONE',  ( -18.59999999999999787, 65.66751761918692409, -130.9282609406112670 ) ) ;
#116541 = CARTESIAN_POINT ( 'NONE',  ( -18.51991288638526001, -9.392436789662124141, -74.14326640395924528 ) ) ;
#116542 = CARTESIAN_POINT ( 'NONE',  ( 21.14999999999999858, 6.540656951712400691, -134.1000000000000227 ) ) ;
#116543 = EDGE_LOOP ( 'NONE', ( #206207, #182511, #7541, #229024 ) ) ;
#116544 = CARTESIAN_POINT ( 'NONE',  ( 21.14999999999999858, 9.083217576421224848, -211.4565844547649931 ) ) ;
#116545 = CARTESIAN_POINT ( 'NONE',  ( -18.59999994787167310, 38.22877715459324577, -261.1960477947820891 ) ) ;
#116546 = DIRECTION ( 'NONE',  ( 0.000000000000000000, 0.000000000000000000, 1.000000000000000000 ) ) ;
#116547 = ORIENTED_EDGE ( 'NONE', *, *, #67942, .F. ) ;
#116548 = DIRECTION ( 'NONE',  ( 0.000000000000000000, 0.000000000000000000, -1.000000000000000000 ) ) ;
#116549 = ORIENTED_EDGE ( 'NONE', *, *, #160975, .F. ) ;
#116550 = ORIENTED_EDGE ( 'NONE', *, *, #34909, .F. ) ;
#116551 = DIRECTION ( 'NONE',  ( 0.000000000000000000, 0.000000000000000000, 1.000000000000000000 ) ) ;
#116552 = ORIENTED_EDGE ( 'NONE', *, *, #170019, .T. ) ;
#116553 = ORIENTED_EDGE ( 'NONE', *, *, #30190, .T. ) ;
#116554 = CARTESIAN_POINT ( 'NONE',  ( -21.05000000000000071, -1.360870587180885716, -142.0729979270909951 ) ) ;
#116555 = CARTESIAN_POINT ( 'NONE',  ( -16.93521499325732549, 9.994786119814676795, -188.4071085410935211 ) ) ;
#116556 = VERTEX_POINT ( 'NONE', #58154 ) ;
#116557 = ORIENTED_EDGE ( 'NONE', *, *, #115673, .F. ) ;
#116558 = DIRECTION ( 'NONE',  ( 1.000000000000000000, 2.952720810173289112E-16, -0.000000000000000000 ) ) ;
#116559 = CARTESIAN_POINT ( 'NONE',  ( -20.85000000000000142, -1.835859311432481045, -179.1044391687985353 ) ) ;
#116560 = AXIS2_PLACEMENT_3D ( 'NONE', #199236, #124830, #222609 ) ;
#116561 = ORIENTED_EDGE ( 'NONE', *, *, #73659, .F. ) ;
#116562 = EDGE_CURVE ( 'NONE', #174664, #205367, #240667, .T. ) ;
#116563 = VECTOR ( 'NONE', #28705, 1000.000000000000000 ) ;
#116564 = ORIENTED_EDGE ( 'NONE', *, *, #149056, .T. ) ;
#116565 = EDGE_CURVE ( 'NONE', #112246, #8515, #176867, .T. ) ;
#116566 = ORIENTED_EDGE ( 'NONE', *, *, #145496, .F. ) ;
#116567 = DIRECTION ( 'NONE',  ( 1.000000000000000000, -0.000000000000000000, -0.000000000000000000 ) ) ;
#116568 = EDGE_CURVE ( 'NONE', #174664, #238512, #217230, .T. ) ;
#116569 = CARTESIAN_POINT ( 'NONE',  ( -22.57320508075687115, 11.65000000001115588, -134.0000000000000568 ) ) ;
#116570 = EDGE_CURVE ( 'NONE', #252130, #191945, #99838, .T. ) ;
#116571 = CARTESIAN_POINT ( 'NONE',  ( -18.79999999999999716, 1.786320531569725478, -11.50977166988710820 ) ) ;
#116572 = LINE ( 'NONE', #257304, #222370 ) ;
#116573 = DIRECTION ( 'NONE',  ( 0.000000000000000000, -0.5283051335749160415, 0.8490545835447742551 ) ) ;
#116574 = AXIS2_PLACEMENT_3D ( 'NONE', #121860, #20192, #222203 ) ;
#116575 = DIRECTION ( 'NONE',  ( -0.000000000000000000, 1.000000000000000000, -0.000000000000000000 ) ) ;
#116576 = FACE_OUTER_BOUND ( 'NONE', #47700, .T. ) ;
#116577 = B_SPLINE_CURVE_WITH_KNOTS ( 'NONE', 3,
 ( #169864, #66863, #145099, #224638, #51123, #146373, #248064, #49858 ),
 .UNSPECIFIED., .F., .F.,
 ( 4, 2, 2, 4 ),
 ( 0.000000000000000000, 0.0001049670497869988235, 0.0002099340995739976470, 0.0004198681991479772963 ),
 .UNSPECIFIED. ) ;
#116578 = AXIS2_PLACEMENT_3D ( 'NONE', #196728, #160205, #239720 ) ;
#116580 = CARTESIAN_POINT ( 'NONE',  ( -18.59999999999999787, 1.115600667400684642E-11, -100.5000000000000426 ) ) ;
#116579 = DIRECTION ( 'NONE',  ( 0.000000000000000000, -0.4856429311786292224, -0.8741572761215394838 ) ) ;
#116581 = CYLINDRICAL_SURFACE ( 'NONE', #215586, 0.09999999999999939493 ) ;
#116582 = DIRECTION ( 'NONE',  ( 0.000000000000000000, 1.000000000000000000, 0.000000000000000000 ) ) ;
#116583 = FACE_OUTER_BOUND ( 'NONE', #45033, .T. ) ;
#116584 = FACE_OUTER_BOUND ( 'NONE', #131793, .T. ) ;
#116585 = VECTOR ( 'NONE', #257040, 1000.000000000000227 ) ;
#116586 = ORIENTED_EDGE ( 'NONE', *, *, #61513, .T. ) ;
#116587 = ADVANCED_FACE ( 'NONE', ( #198969 ), #98541, .F. ) ;
#116588 = ADVANCED_FACE ( 'NONE', ( #738 ), #238087, .T. ) ;
#116590 = ORIENTED_EDGE ( 'NONE', *, *, #222090, .F. ) ;
#116589 = DIRECTION ( 'NONE',  ( 0.000000000000000000, 0.2868887416116073785, -0.9579639084728132081 ) ) ;
#116591 = DIRECTION ( 'NONE',  ( -0.000000000000000000, -1.000000000000000000, -6.982962677686266711E-15 ) ) ;
#116592 = CARTESIAN_POINT ( 'NONE',  ( -22.39999999999999858, 64.18196446391819165, -247.0985338183330668 ) ) ;
#116593 = ORIENTED_EDGE ( 'NONE', *, *, #1853, .F. ) ;
#116594 = EDGE_CURVE ( 'NONE', #68874, #131693, #42459, .T. ) ;
#116596 = CARTESIAN_POINT ( 'NONE',  ( 20.27550659511088682, 66.78395627750300889, -90.37310748452436826 ) ) ;
#116595 = TOROIDAL_SURFACE ( 'NONE', #4165, 0.2000000000000000111, 0.1000000000000000056 ) ;
#116597 = CIRCLE ( 'NONE', #29167, 0.5000000000000004441 ) ;
#116598 = EDGE_CURVE ( 'NONE', #4968, #66389, #80272, .T. ) ;
#116599 = CARTESIAN_POINT ( 'NONE',  ( -16.87036670365549895, 66.01058118071064484, -157.5026676018264595 ) ) ;
#116600 = EDGE_LOOP ( 'NONE', ( #4898, #237673, #99907 ) ) ;
#116601 = DIRECTION ( 'NONE',  ( 0.000000000000000000, 0.000000000000000000, -1.000000000000000000 ) ) ;
#116602 = CYLINDRICAL_SURFACE ( 'NONE', #38134, 0.09999999999998898659 ) ;
#116603 = CARTESIAN_POINT ( 'NONE',  ( 23.15000000000000213, -11.39257802169451139, -197.9260504201680249 ) ) ;
#116605 = ORIENTED_EDGE ( 'NONE', *, *, #95193, .F. ) ;
#116604 = LINE ( 'NONE', #117878, #101896 ) ;
#116606 = EDGE_CURVE ( 'NONE', #241144, #173164, #222172, .T. ) ;
#116608 = ORIENTED_EDGE ( 'NONE', *, *, #215991, .T. ) ;
#116607 = CARTESIAN_POINT ( 'NONE',  ( -18.59999999999999787, 9.250000000011157297, -79.25000000000004263 ) ) ;
#116609 = LINE ( 'NONE', #176605, #33550 ) ;
#116610 = DIRECTION ( 'NONE',  ( 1.000000000000000000, 0.000000000000000000, 0.000000000000000000 ) ) ;
#116611 = DIRECTION ( 'NONE',  ( 0.000000000000000000, -0.8700118002898357128, 0.4930308989875170633 ) ) ;
#116612 = ADVANCED_FACE ( 'NONE', ( #120752 ), #238973, .F. ) ;
#116613 = DIRECTION ( 'NONE',  ( 0.000000000000000000, 0.000000000000000000, -1.000000000000000000 ) ) ;
#116614 = AXIS2_PLACEMENT_3D ( 'NONE', #122867, #245380, #64168 ) ;
#116617 = CARTESIAN_POINT ( 'NONE',  ( 23.40000000000005187, 76.00000000001119815, -40.07310748452479032 ) ) ;
#116616 = VECTOR ( 'NONE', #180442, 1000.000000000000000 ) ;
#116615 = CARTESIAN_POINT ( 'NONE',  ( -16.80070461187903419, 9.950000000011137047, -154.8530361708395162 ) ) ;
#116618 = DIRECTION ( 'NONE',  ( 1.000000000000000000, 0.000000000000000000, 0.000000000000000000 ) ) ;
#116619 = VECTOR ( 'NONE', #206720, 1000.000000000000000 ) ;
#116620 = CIRCLE ( 'NONE', #229254, 0.1000000000000028644 ) ;
#116622 = ADVANCED_FACE ( 'NONE', ( #162435 ), #8489, .F. ) ;
#116621 = CARTESIAN_POINT ( 'NONE',  ( -18.40000000000000213, 20.94763808724815846, -234.7254930126486556 ) ) ;
#116623 = CARTESIAN_POINT ( 'NONE',  ( -22.94999999999999929, 4.611773100472912112, 22.11686199900910665 ) ) ;
#116624 = ORIENTED_EDGE ( 'NONE', *, *, #78991, .F. ) ;
#116625 = CARTESIAN_POINT ( 'NONE',  ( 21.05000000000000071, 1.115486826172573664E-11, -93.95934304829879125 ) ) ;
#116626 = AXIS2_PLACEMENT_3D ( 'NONE', #63765, #41662, #143301 ) ;
#116627 = ORIENTED_EDGE ( 'NONE', *, *, #217818, .T. ) ;
#116629 = ORIENTED_EDGE ( 'NONE', *, *, #117776, .T. ) ;
#116628 = B_SPLINE_CURVE_WITH_KNOTS ( 'NONE', 3,
 ( #220211, #121135, #149345, #208029, #210580, #72371, #188440, #247120, #211880, #50201 ),
 .UNSPECIFIED., .F., .F.,
 ( 4, 2, 2, 2, 4 ),
 ( 5.273673492279070357E-16, 9.930191194501526101E-05, 0.0001986038238895031390, 0.0003972076477784386439, 0.0007944152955563512329 ),
 .UNSPECIFIED. ) ;
#116630 = FACE_OUTER_BOUND ( 'NONE', #122263, .T. ) ;
#116631 = CARTESIAN_POINT ( 'NONE',  ( 21.05000000000000071, 70.60000000001200249, -115.4283735034374274 ) ) ;
#116632 = VERTEX_POINT ( 'NONE', #46301 ) ;
#116633 = EDGE_CURVE ( 'NONE', #73311, #203104, #55568, .T. ) ;
#116634 = CIRCLE ( 'NONE', #179207, 0.1000000000000028644 ) ;
#116635 = ORIENTED_EDGE ( 'NONE', *, *, #154094, .T. ) ;
#116636 = AXIS2_PLACEMENT_3D ( 'NONE', #215996, #34842, #176916 ) ;
#116637 = ADVANCED_FACE ( 'NONE', ( #207981 ), #89285, .T. ) ;
#116638 = CARTESIAN_POINT ( 'NONE',  ( 18.52928932188133970, 55.00560498697586098, -230.0684277855484652 ) ) ;
#116639 = VERTEX_POINT ( 'NONE', #146671 ) ;
#116640 = EDGE_LOOP ( 'NONE', ( #32661, #91483, #24337 ) ) ;
#116641 = CARTESIAN_POINT ( 'NONE',  ( -18.59999999999999787, 11.65000000001115232, -88.35000000000003695 ) ) ;
#116642 = FACE_OUTER_BOUND ( 'NONE', #53382, .T. ) ;
#116643 = FACE_OUTER_BOUND ( 'NONE', #122670, .T. ) ;
#116644 = CARTESIAN_POINT ( 'NONE',  ( -22.39999999999999858, 7.790779598384560245, -133.9000000000000057 ) ) ;
#116645 = CARTESIAN_POINT ( 'NONE',  ( 13.76927104934457624, 9.455987233612738407, -15.01153116689782507 ) ) ;
#116646 = ADVANCED_FACE ( 'NONE', ( #166305 ), #65881, .F. ) ;
#116647 = FACE_OUTER_BOUND ( 'NONE', #66814, .T. ) ;
#116648 = CARTESIAN_POINT ( 'NONE',  ( -20.64999999999999858, 68.85000000001186038, -90.67310748452435121 ) ) ;
#116650 = EDGE_LOOP ( 'NONE', ( #221875, #77327, #81620, #42823 ) ) ;
#116649 = DIRECTION ( 'NONE',  ( 1.000000000000000000, 2.885090398161910739E-16, 6.283419270304611573E-17 ) ) ;
#116652 = DIRECTION ( 'NONE',  ( 0.000000000000000000, 0.01283462868040226822, 0.9999176327611370985 ) ) ;
#116651 = CARTESIAN_POINT ( 'NONE',  ( -22.50485643085239928, -0.07878633907718655960, 11.74979493917241413 ) ) ;
#116653 = FACE_OUTER_BOUND ( 'NONE', #28682, .T. ) ;
#116654 = ORIENTED_EDGE ( 'NONE', *, *, #49365, .T. ) ;
#116655 = CARTESIAN_POINT ( 'NONE',  ( -16.94275863006528482, 63.05852775302872715, -213.0770397792431083 ) ) ;
#116656 = LINE ( 'NONE', #196195, #33343 ) ;
#116657 = EDGE_LOOP ( 'NONE', ( #249998, #41208, #36556, #171173 ) ) ;
#116659 = CARTESIAN_POINT ( 'NONE',  ( 21.05000000000000071, 0.000000000000000000, -12.97499999999999787 ) ) ;
#116658 = CARTESIAN_POINT ( 'NONE',  ( -22.39999999999999858, 76.00000000001219291, -144.3138870828977076 ) ) ;
#116660 = CIRCLE ( 'NONE', #150013, 0.09999999999999543976 ) ;
#116661 = DIRECTION ( 'NONE',  ( -1.000000000000000000, 0.000000000000000000, -0.000000000000000000 ) ) ;
#116662 = CARTESIAN_POINT ( 'NONE',  ( 20.94999999999999929, 76.00000000001126921, -203.5231074845248997 ) ) ;
#116663 = VERTEX_POINT ( 'NONE', #222354 ) ;
#116664 = VERTEX_POINT ( 'NONE', #168880 ) ;
#116665 = CYLINDRICAL_SURFACE ( 'NONE', #90889, 0.09999999999999939493 ) ;
#116667 = CARTESIAN_POINT ( 'NONE',  ( -22.59999999999999787, 0.1008583691098682150, -55.25043287651065782 ) ) ;
#116666 = CIRCLE ( 'NONE', #58377, 0.09999999999999864553 ) ;
#116668 = CARTESIAN_POINT ( 'NONE',  ( -20.94999999999999929, 47.95459712139159336, -246.5019368548292675 ) ) ;
#116669 = CARTESIAN_POINT ( 'NONE',  ( 23.15000000000000213, -11.39257802170566691, -30.42605042016806394 ) ) ;
#116670 = EDGE_LOOP ( 'NONE', ( #202224, #162098, #42926, #123478 ) ) ;
#116671 = CARTESIAN_POINT ( 'NONE',  ( -20.64999999999999858, 49.36776662947724503, -253.7196102226803021 ) ) ;
#116672 = FACE_BOUND ( 'NONE', #233338, .T. ) ;
#116673 = CARTESIAN_POINT ( 'NONE',  ( 20.85000000000000142, -1.835859311432481045, -212.5044391687984842 ) ) ;
#116674 = VECTOR ( 'NONE', #207193, 1000.000000000000000 ) ;
#116676 = DIRECTION ( 'NONE',  ( 0.000000000000000000, 0.2128009952263601456, -0.9770955615653316162 ) ) ;
#116675 = AXIS2_PLACEMENT_3D ( 'NONE', #212356, #149816, #187661 ) ;
#116678 = ORIENTED_EDGE ( 'NONE', *, *, #165988, .T. ) ;
#116677 = SPHERICAL_SURFACE ( 'NONE', #254548, 0.1000000000000000056 ) ;
#116679 = CARTESIAN_POINT ( 'NONE',  ( 21.14999999999999858, 1.115600667400684642E-11, -146.1500000000000341 ) ) ;
#116680 = DIRECTION ( 'NONE',  ( 0.000000000000000000, 6.982962677686267499E-15, -1.000000000000000000 ) ) ;
#116681 = CARTESIAN_POINT ( 'NONE',  ( -20.85000000000000142, 42.99798587058931076, -254.2674462307522560 ) ) ;
#116682 = AXIS2_PLACEMENT_3D ( 'NONE', #52513, #171244, #106055 ) ;
#116683 = DIRECTION ( 'NONE',  ( -1.000000000000000000, -2.952720810173289112E-16, 0.000000000000000000 ) ) ;
#116684 = ADVANCED_FACE ( 'NONE', ( #104964 ), #18208, .T. ) ;
#116685 = CARTESIAN_POINT ( 'NONE',  ( 18.59999999999999076, 10.49142135623730709, -24.75000000000000000 ) ) ;
#116687 = ORIENTED_EDGE ( 'NONE', *, *, #184577, .T. ) ;
#116686 = DIRECTION ( 'NONE',  ( 0.000000000000000000, -1.000000000000000000, -7.272083257015735086E-15 ) ) ;
#116688 = DIRECTION ( 'NONE',  ( 0.000000000000000000, 0.000000000000000000, 1.000000000000000000 ) ) ;
#116689 = VECTOR ( 'NONE', #159648, 1000.000000000000000 ) ;
#116690 = CARTESIAN_POINT ( 'NONE',  ( -18.59999999999999787, 64.65966496992309942, -200.4475097531309586 ) ) ;
#116691 = CARTESIAN_POINT ( 'NONE',  ( -23.15000000000000213, 4.349999999999999645, -12.35000000000000142 ) ) ;
#116692 = VECTOR ( 'NONE', #205908, 1000.000000000000114 ) ;
#116693 = EDGE_LOOP ( 'NONE', ( #122452, #192606, #234712, #132270 ) ) ;
#116694 = DIRECTION ( 'NONE',  ( 0.000000000000000000, 0.000000000000000000, -1.000000000000000000 ) ) ;
#116695 = FACE_OUTER_BOUND ( 'NONE', #72970, .T. ) ;
#116697 = EDGE_CURVE ( 'NONE', #247315, #253910, #72382, .T. ) ;
#116696 = DIRECTION ( 'NONE',  ( 1.000000000000000000, 0.000000000000000000, 0.000000000000000000 ) ) ;
#116698 = EDGE_CURVE ( 'NONE', #1820, #257983, #164979, .T. ) ;
#116699 = DIRECTION ( 'NONE',  ( 0.000000000000000000, -0.8660254037844343777, 0.5000000000000074385 ) ) ;
#116700 = CYLINDRICAL_SURFACE ( 'NONE', #75843, 0.1000000000000028644 ) ;
#116702 = CARTESIAN_POINT ( 'NONE',  ( -20.94999999999999929, 76.00000000001168132, -65.52310748452430289 ) ) ;
#116701 = VECTOR ( 'NONE', #235301, 1000.000000000000114 ) ;
#116703 = AXIS2_PLACEMENT_3D ( 'NONE', #138217, #117396, #76978 ) ;
#116705 = EDGE_LOOP ( 'NONE', ( #41051, #113041, #240944, #102400 ) ) ;
#116704 = AXIS2_PLACEMENT_3D ( 'NONE', #83274, #2470, #218957 ) ;
#116706 = ORIENTED_EDGE ( 'NONE', *, *, #2542, .F. ) ;
#116707 = AXIS2_PLACEMENT_3D ( 'NONE', #143863, #219545, #4349 ) ;
#116708 = VECTOR ( 'NONE', #97698, 1000.000000000000227 ) ;
#116709 = CYLINDRICAL_SURFACE ( 'NONE', #105657, 0.09999999999999939493 ) ;
#116710 = CARTESIAN_POINT ( 'NONE',  ( 18.59999999999999787, -8.150000000000007461, 32.89999999999999858 ) ) ;
#116711 = EDGE_CURVE ( 'NONE', #150487, #166239, #209744, .T. ) ;
#116712 = CARTESIAN_POINT ( 'NONE',  ( 23.40000000000005187, 64.25000000001119815, -36.02310748452479316 ) ) ;
#116713 = CARTESIAN_POINT ( 'NONE',  ( 18.59999999999999787, 76.00000000001237765, -170.0231074845243597 ) ) ;
#116714 = VERTEX_POINT ( 'NONE', #244510 ) ;
#116715 = CARTESIAN_POINT ( 'NONE',  ( 20.94999999999999929, 10.72371710471867701, -155.2500000000000284 ) ) ;
#116716 = CARTESIAN_POINT ( 'NONE',  ( 20.97438252431638972, 10.52392060743736835, -207.3789767912604702 ) ) ;
#116717 = CIRCLE ( 'NONE', #112635, 0.09999999999999939493 ) ;
#116718 = DIRECTION ( 'NONE',  ( -0.000000000000000000, 1.000000000000000000, 6.982962677686266711E-15 ) ) ;
#116719 = CARTESIAN_POINT ( 'NONE',  ( 20.94999999999999929, 71.00000000001205080, -124.1178414656112352 ) ) ;
#116720 = ORIENTED_EDGE ( 'NONE', *, *, #68615, .T. ) ;
#116721 = LINE ( 'NONE', #196257, #2817 ) ;
#116722 = VERTEX_POINT ( 'NONE', #24209 ) ;
#116723 = ORIENTED_EDGE ( 'NONE', *, *, #33293, .F. ) ;
#116724 = ADVANCED_FACE ( 'NONE', ( #103694 ), #9815, .T. ) ;
#116725 = CARTESIAN_POINT ( 'NONE',  ( -17.11825945287481687, 9.950000000011140600, -154.8500000000000227 ) ) ;
#116726 = CARTESIAN_POINT ( 'NONE',  ( -21.11825140030088122, 6.445407565431050756, -100.4927963793672205 ) ) ;
#116727 = EDGE_CURVE ( 'NONE', #130829, #12569, #187138, .T. ) ;
#116728 = CARTESIAN_POINT ( 'NONE',  ( -17.01473183483381391, 66.05000000001187743, -90.27310748452437394 ) ) ;
#116729 = ORIENTED_EDGE ( 'NONE', *, *, #21564, .T. ) ;
#116730 = DIRECTION ( 'NONE',  ( 0.000000000000000000, -6.938893903907222067E-15, 1.000000000000000000 ) ) ;
#116731 = CARTESIAN_POINT ( 'NONE',  ( -20.94999999999999929, -11.48912529307605901, -3.000000000000002665 ) ) ;
#116732 = CARTESIAN_POINT ( 'NONE',  ( -16.77828822459933633, 30.19341635460695983, -234.8044058226641653 ) ) ;
#116734 = ORIENTED_EDGE ( 'NONE', *, *, #15627, .F. ) ;
#116733 = VECTOR ( 'NONE', #14548, 1000.000000000000000 ) ;
#116735 = DIRECTION ( 'NONE',  ( -1.000000000000000000, 0.000000000000000000, 0.000000000000000000 ) ) ;
#116737 = ORIENTED_EDGE ( 'NONE', *, *, #3981, .T. ) ;
#116736 = CARTESIAN_POINT ( 'NONE',  ( -33.72168855820452649, 64.52683809664912928, -60.27310748452440947 ) ) ;
#116738 = AXIS2_PLACEMENT_3D ( 'NONE', #71344, #210837, #55571 ) ;
#116739 = CARTESIAN_POINT ( 'NONE',  ( 20.09999999999999787, 66.25000000001185185, -82.17310748452439384 ) ) ;
#116741 = EDGE_CURVE ( 'NONE', #240580, #159212, #167577, .T. ) ;
#116740 = DIRECTION ( 'NONE',  ( -1.000000000000000000, -0.000000000000000000, -0.000000000000000000 ) ) ;
#116742 = CIRCLE ( 'NONE', #112652, 0.09999999999999939493 ) ;
#116743 = B_SPLINE_CURVE_WITH_KNOTS ( 'NONE', 3,
 ( #101788, #100507, #99238, #223050, #22316, #177552 ),
 .UNSPECIFIED., .F., .F.,
 ( 4, 2, 4 ),
 ( 0.000000000000000000, 0.0001891491689349488760, 0.0003782983378698977521 ),
 .UNSPECIFIED. ) ;
#116744 = ORIENTED_EDGE ( 'NONE', *, *, #17207, .T. ) ;
#116745 = LINE ( 'NONE', #235397, #189323 ) ;
#116746 = CYLINDRICAL_SURFACE ( 'NONE', #183704, 0.1000000000000028644 ) ;
#116747 = CARTESIAN_POINT ( 'NONE',  ( -20.94999999999999929, 7.120270961708750512, -137.6595630418393625 ) ) ;
#116748 = ORIENTED_EDGE ( 'NONE', *, *, #90255, .T. ) ;
#116749 = FACE_OUTER_BOUND ( 'NONE', #248298, .T. ) ;
#116750 = CARTESIAN_POINT ( 'NONE',  ( 22.50014994443972682, 55.86946353937215548, -232.8597856945308422 ) ) ;
#116751 = CARTESIAN_POINT ( 'NONE',  ( 18.59999999999997655, 1.115600667400684642E-11, -100.5000000000000426 ) ) ;
#116752 = CIRCLE ( 'NONE', #62602, 0.1000000000000040579 ) ;
#116753 = ADVANCED_FACE ( 'NONE', ( #243222 ), #204095, .F. ) ;
#116754 = AXIS2_PLACEMENT_3D ( 'NONE', #64296, #83813, #214697 ) ;
#116755 = ORIENTED_EDGE ( 'NONE', *, *, #31353, .F. ) ;
#116756 = CARTESIAN_POINT ( 'NONE',  ( -23.15000000000000213, 36.65892442174935439, -249.5511627012433848 ) ) ;
#116757 = EDGE_LOOP ( 'NONE', ( #255990, #44412, #141771, #119085 ) ) ;
#116758 = CIRCLE ( 'NONE', #4322, 0.09999999999999939493 ) ;
#116759 = EDGE_CURVE ( 'NONE', #191070, #248248, #243042, .T. ) ;
#116760 = VERTEX_POINT ( 'NONE', #184532 ) ;
#116761 = DIRECTION ( 'NONE',  ( 0.000000000000000000, 0.8814952561688476074, -0.4721928772777262417 ) ) ;
#116762 = DIRECTION ( 'NONE',  ( -0.000000000000000000, -1.000000000000000000, 0.000000000000000000 ) ) ;
#116764 = ORIENTED_EDGE ( 'NONE', *, *, #213005, .T. ) ;
#116763 = CARTESIAN_POINT ( 'NONE',  ( 22.50000000000000000, 0.1000000000111554016, -21.75000000000000355 ) ) ;
#116765 = DIRECTION ( 'NONE',  ( -1.000000000000000000, -0.000000000000000000, -0.000000000000000000 ) ) ;
#116766 = PLANE ( 'NONE',  #7920 ) ;
#116767 = EDGE_CURVE ( 'NONE', #118463, #94180, #247069, .T. ) ;
#116769 = EDGE_CURVE ( 'NONE', #181023, #68571, #163948, .T. ) ;
#116768 = FACE_OUTER_BOUND ( 'NONE', #3614, .T. ) ;
#116770 = CYLINDRICAL_SURFACE ( 'NONE', #26734, 11.74999999999999289 ) ;
#116771 = DIRECTION ( 'NONE',  ( 1.000000000000000000, 3.265361837132813093E-16, -0.000000000000000000 ) ) ;
#116772 = DIRECTION ( 'NONE',  ( 0.000000000000000000, -1.000000000000000000, 0.000000000000000000 ) ) ;
#116773 = CARTESIAN_POINT ( 'NONE',  ( -20.64999999999999858, 76.00000000001199396, -115.8981074845243029 ) ) ;
#116775 = ORIENTED_EDGE ( 'NONE', *, *, #248602, .T. ) ;
#116774 = DIRECTION ( 'NONE',  ( 1.000000000000000000, 0.000000000000000000, 0.000000000000000000 ) ) ;
#116777 = VERTEX_POINT ( 'NONE', #189684 ) ;
#116776 = DIRECTION ( 'NONE',  ( 1.000000000000000000, 0.000000000000000000, 0.000000000000000000 ) ) ;
#116780 = CARTESIAN_POINT ( 'NONE',  ( -16.88705144915407175, 51.36243976870036931, -232.0613434336529508 ) ) ;
#116779 = PLANE ( 'NONE',  #249568 ) ;
#116778 = AXIS2_PLACEMENT_3D ( 'NONE', #128784, #136443, #210876 ) ;
#116781 = AXIS2_PLACEMENT_3D ( 'NONE', #169761, #71920, #9350 ) ;
#116783 = ORIENTED_EDGE ( 'NONE', *, *, #34638, .F. ) ;
#116782 = DIRECTION ( 'NONE',  ( -1.000000000000000000, 0.000000000000000000, 0.000000000000000000 ) ) ;
#116784 = VERTEX_POINT ( 'NONE', #154447 ) ;
#116785 = DIRECTION ( 'NONE',  ( 1.000000000000000000, 0.000000000000000000, 0.000000000000000000 ) ) ;
#116786 = DIRECTION ( 'NONE',  ( -1.000000000000000000, 0.000000000000000000, -0.000000000000000000 ) ) ;
#116787 = EDGE_CURVE ( 'NONE', #74814, #132343, #197266, .T. ) ;
#116788 = EDGE_CURVE ( 'NONE', #163200, #212474, #71041, .T. ) ;
#116789 = CARTESIAN_POINT ( 'NONE',  ( -21.05000000000000071, 43.52285900727589762, -245.0935880436369985 ) ) ;
#116790 = DIRECTION ( 'NONE',  ( 0.000000000000000000, 0.2617529984165180013, 0.9651348961777117541 ) ) ;
#116791 = DIRECTION ( 'NONE',  ( -1.000000000000000000, -0.000000000000000000, -0.000000000000000000 ) ) ;
#116792 = EDGE_CURVE ( 'NONE', #176760, #61299, #118150, .T. ) ;
#116793 = DIRECTION ( 'NONE',  ( 0.000000000000000000, -0.4721928772778937189, -0.8814952561687577903 ) ) ;
#116794 = FACE_OUTER_BOUND ( 'NONE', #26320, .T. ) ;
#116795 = AXIS2_PLACEMENT_3D ( 'NONE', #204938, #185395, #6755 ) ;
#116797 = ORIENTED_EDGE ( 'NONE', *, *, #230436, .T. ) ;
#116796 = EDGE_CURVE ( 'NONE', #17335, #50465, #153167, .T. ) ;
#116798 = VERTEX_POINT ( 'NONE', #93138 ) ;
#116799 = VECTOR ( 'NONE', #96713, 1000.000000000000000 ) ;
#116800 = CARTESIAN_POINT ( 'NONE',  ( -18.40000000000000213, 11.47316190337364183, -154.9500000000000455 ) ) ;
#116801 = AXIS2_PLACEMENT_3D ( 'NONE', #179223, #119234, #83899 ) ;
#116802 = VERTEX_POINT ( 'NONE', #14916 ) ;
#116803 = EDGE_CURVE ( 'NONE', #224921, #182454, #138958, .T. ) ;
#116804 = FACE_OUTER_BOUND ( 'NONE', #191231, .T. ) ;
#116805 = ADVANCED_FACE ( 'NONE', ( #174017 ), #112717, .F. ) ;
#116806 = CYLINDRICAL_SURFACE ( 'NONE', #193448, 11.80000000000000426 ) ;
#116807 = FACE_OUTER_BOUND ( 'NONE', #184163, .T. ) ;
#116808 = CIRCLE ( 'NONE', #241710, 0.09999999999999789613 ) ;
#116809 = PLANE ( 'NONE',  #234465 ) ;
#116810 = EDGE_CURVE ( 'NONE', #83522, #151223, #69754, .T. ) ;
#116811 = EDGE_LOOP ( 'NONE', ( #92993, #95116, #199658, #25995 ) ) ;
#116812 = DIRECTION ( 'NONE',  ( 1.000000000000000000, 0.000000000000000000, 0.000000000000000000 ) ) ;
#116813 = ORIENTED_EDGE ( 'NONE', *, *, #13394, .T. ) ;
#116814 = CARTESIAN_POINT ( 'NONE',  ( -16.91256925476569606, 9.985731158139328656, -87.96764248900531413 ) ) ;
#116815 = VERTEX_POINT ( 'NONE', #13617 ) ;
#116816 = EDGE_CURVE ( 'NONE', #785, #85465, #253494, .T. ) ;
#116817 = CIRCLE ( 'NONE', #120945, 0.09999999999998898659 ) ;
#116818 = DIRECTION ( 'NONE',  ( 1.186688945009009831E-16, 1.000000000000000000, 6.982962677686266711E-15 ) ) ;
#116819 = EDGE_CURVE ( 'NONE', #99517, #201727, #209237, .T. ) ;
#116820 = DIRECTION ( 'NONE',  ( 0.000000000000000000, 6.982962677686266711E-15, -1.000000000000000000 ) ) ;
#116821 = DIRECTION ( 'NONE',  ( 0.000000000000000000, 6.982962677686266711E-15, -1.000000000000000000 ) ) ;
#116823 = ORIENTED_EDGE ( 'NONE', *, *, #136060, .F. ) ;
#116822 = EDGE_CURVE ( 'NONE', #8739, #17513, #12354, .T. ) ;
#116824 = FACE_OUTER_BOUND ( 'NONE', #100512, .T. ) ;
#116826 = VERTEX_POINT ( 'NONE', #95703 ) ;
#116825 = DIRECTION ( 'NONE',  ( 1.000000000000000000, 0.000000000000000000, 0.000000000000000000 ) ) ;
#116827 = CARTESIAN_POINT ( 'NONE',  ( -21.05000000000000071, 64.25000000001148237, -43.03791325517834565 ) ) ;
#116828 = ORIENTED_EDGE ( 'NONE', *, *, #70009, .F. ) ;
#116829 = FACE_OUTER_BOUND ( 'NONE', #236825, .T. ) ;
#116830 = ORIENTED_EDGE ( 'NONE', *, *, #220438, .F. ) ;
#116831 = EDGE_CURVE ( 'NONE', #78788, #200509, #147564, .T. ) ;
#116832 = DIRECTION ( 'NONE',  ( 0.000000000000000000, -6.982962677686266711E-15, 1.000000000000000000 ) ) ;
#116834 = CARTESIAN_POINT ( 'NONE',  ( 21.05000000000000071, 69.74115287693250309, -69.55486583757952701 ) ) ;
#116833 = VECTOR ( 'NONE', #18878, 1000.000000000000000 ) ;
#116835 = DIRECTION ( 'NONE',  ( 1.000000000000000000, -0.000000000000000000, -0.000000000000000000 ) ) ;
#116836 = DIRECTION ( 'NONE',  ( -0.000000000000000000, -0.000000000000000000, -1.000000000000000000 ) ) ;
#116837 = CARTESIAN_POINT ( 'NONE',  ( -21.09316766718153247, 0.03926340232583033080, -60.62984668752533679 ) ) ;
#116838 = AXIS2_PLACEMENT_3D ( 'NONE', #80396, #158722, #238216 ) ;
#116839 = EDGE_LOOP ( 'NONE', ( #87271, #230617, #77675, #20036, #16285 ) ) ;
#116840 = CARTESIAN_POINT ( 'NONE',  ( -23.25000000000000000, 7.128833340094563376, -233.7327013124401276 ) ) ;
#116841 = CARTESIAN_POINT ( 'NONE',  ( -21.05000000000000071, 64.25000000001195133, -110.0379132551783243 ) ) ;
#116842 = DIRECTION ( 'NONE',  ( 1.000000000000000000, -0.000000000000000000, -0.000000000000000000 ) ) ;
#116843 = AXIS2_PLACEMENT_3D ( 'NONE', #93049, #237707, #56472 ) ;
#116844 = EDGE_LOOP ( 'NONE', ( #163386, #68490, #36180, #228892, #175769 ) ) ;
#116845 = LINE ( 'NONE', #17721, #217822 ) ;
#116846 = EDGE_LOOP ( 'NONE', ( #10729, #75136, #137492, #128493 ) ) ;
#116847 = CARTESIAN_POINT ( 'NONE',  ( 20.99999999999999645, 9.750000000011137757, -54.34999999999999432 ) ) ;
#116848 = ORIENTED_EDGE ( 'NONE', *, *, #175392, .F. ) ;
#116849 = CARTESIAN_POINT ( 'NONE',  ( -22.50000000000000000, 1.115600667400684642E-11, -134.0000000000000000 ) ) ;
#116850 = CARTESIAN_POINT ( 'NONE',  ( 21.14999999999999503, 87.65000000001221281, -148.2731074845242176 ) ) ;
#116851 = CIRCLE ( 'NONE', #183496, 0.09999999999999761857 ) ;
#116853 = EDGE_LOOP ( 'NONE', ( #230981, #158748, #147765, #43756 ) ) ;
#116852 = CARTESIAN_POINT ( 'NONE',  ( -16.27683809663751191, 9.350000000011133849, -76.25000000000001421 ) ) ;
#116854 = FACE_OUTER_BOUND ( 'NONE', #142746, .T. ) ;
#116855 = ORIENTED_EDGE ( 'NONE', *, *, #245508, .T. ) ;
#116856 = CARTESIAN_POINT ( 'NONE',  ( -20.94999999999999929, 13.63177590472475487, -238.5351604075707144 ) ) ;
#116857 = DIRECTION ( 'NONE',  ( -0.000000000000000000, -0.000000000000000000, -1.000000000000000000 ) ) ;
#116858 = VERTEX_POINT ( 'NONE', #91862 ) ;
#116859 = ORIENTED_EDGE ( 'NONE', *, *, #223015, .T. ) ;
#116860 = ADVANCED_FACE ( 'NONE', ( #194845 ), #228820, .F. ) ;
#116861 = CARTESIAN_POINT ( 'NONE',  ( -20.95000000000000639, 11.75000000001115019, -194.2161343370218560 ) ) ;
#116862 = VERTEX_POINT ( 'NONE', #90565 ) ;
#116863 = CARTESIAN_POINT ( 'NONE',  ( 21.05000000000000071, 10.27563683788935300, -228.0699890633274833 ) ) ;
#116864 = AXIS2_PLACEMENT_3D ( 'NONE', #144287, #182175, #180890 ) ;
#116865 = ADVANCED_FACE ( 'NONE', ( #249664 ), #73616, .F. ) ;
#116866 = CIRCLE ( 'NONE', #141796, 0.1000000000000002554 ) ;
#116867 = ORIENTED_EDGE ( 'NONE', *, *, #58101, .T. ) ;
#116868 = CARTESIAN_POINT ( 'NONE',  ( -17.11825945287481687, 66.05000000001153637, -48.67310748452439384 ) ) ;
#116869 = DIRECTION ( 'NONE',  ( 1.000000000000000000, 0.000000000000000000, -0.000000000000000000 ) ) ;
#116870 = CIRCLE ( 'NONE', #4432, 0.5000000000000013323 ) ;
#116871 = CIRCLE ( 'NONE', #216828, 11.74999999999999645 ) ;
#116872 = AXIS2_PLACEMENT_3D ( 'NONE', #209447, #30845, #110347 ) ;
#116874 = ORIENTED_EDGE ( 'NONE', *, *, #79970, .T. ) ;
#116873 = CARTESIAN_POINT ( 'NONE',  ( 18.50000000000000000, 85.40000000001190017, -95.72584772486095517 ) ) ;
#116875 = CARTESIAN_POINT ( 'NONE',  ( 20.94999999999999574, -1.736257131586239844, -78.56865232901753870 ) ) ;
#116876 = DIRECTION ( 'NONE',  ( 0.000000000000000000, -0.8660254037844383745, 0.5000000000000003331 ) ) ;
#116877 = DIRECTION ( 'NONE',  ( -1.000000000000000000, -0.000000000000000000, 0.000000000000000000 ) ) ;
#116879 = FACE_OUTER_BOUND ( 'NONE', #101828, .T. ) ;
#116878 = CARTESIAN_POINT ( 'NONE',  ( 20.95224633520496127, 8.900522166568386240, -41.99327644792126790 ) ) ;
#116881 = EDGE_CURVE ( 'NONE', #189017, #52458, #130992, .T. ) ;
#116880 = CARTESIAN_POINT ( 'NONE',  ( -20.54999999999999716, 7.250000000011155521, -155.1500000000000057 ) ) ;
#116882 = CARTESIAN_POINT ( 'NONE',  ( -20.85000000000000142, -1.835859311432479268, -212.5044391687984842 ) ) ;
#116883 = CARTESIAN_POINT ( 'NONE',  ( 18.42636655943172030, 85.49694431578203080, -29.41402691336874753 ) ) ;
#116884 = TOROIDAL_SURFACE ( 'NONE', #16949, 0.2000000000000000111, 0.1000000000000000056 ) ;
#116885 = CARTESIAN_POINT ( 'NONE',  ( 23.14999999999999503, 15.92646454033040371, -219.3818586450342423 ) ) ;
#116886 = AXIS2_PLACEMENT_3D ( 'NONE', #53839, #10866, #69562 ) ;
#116887 = ORIENTED_EDGE ( 'NONE', *, *, #54084, .T. ) ;
#116888 = VECTOR ( 'NONE', #136833, 1000.000000000000000 ) ;
#116890 = ORIENTED_EDGE ( 'NONE', *, *, #144846, .T. ) ;
#116889 = AXIS2_PLACEMENT_3D ( 'NONE', #226653, #49309, #171869 ) ;
#116891 = DIRECTION ( 'NONE',  ( 0.000000000000000000, 0.000000000000000000, -1.000000000000000000 ) ) ;
#116893 = ORIENTED_EDGE ( 'NONE', *, *, #78639, .F. ) ;
#116892 = DIRECTION ( 'NONE',  ( -1.000000000000000000, 0.000000000000000000, 0.000000000000000000 ) ) ;
#116894 = ORIENTED_EDGE ( 'NONE', *, *, #687, .T. ) ;
#116895 = DIRECTION ( 'NONE',  ( 0.000000000000000000, -0.8814952561688476074, 0.4721928772777262417 ) ) ;
#116896 = VERTEX_POINT ( 'NONE', #232679 ) ;
#116897 = DIRECTION ( 'NONE',  ( 1.000000000000000000, -3.151514657663852580E-16, 8.547182517843351137E-17 ) ) ;
#116898 = AXIS2_PLACEMENT_3D ( 'NONE', #27126, #166639, #7525 ) ;
#116899 = ORIENTED_EDGE ( 'NONE', *, *, #86107, .F. ) ;
#116900 =( NAMED_UNIT ( * ) PLANE_ANGLE_UNIT ( ) SI_UNIT ( $, .RADIAN. ) );
#116901 = CARTESIAN_POINT ( 'NONE',  ( -18.39999999999999858, -9.600000000000004974, -40.10018939122204529 ) ) ;
#116903 = ORIENTED_EDGE ( 'NONE', *, *, #182721, .F. ) ;
#116902 = ORIENTED_EDGE ( 'NONE', *, *, #183091, .T. ) ;
#116904 = EDGE_LOOP ( 'NONE', ( #181828, #161439, #233638, #74588 ) ) ;
#116905 = EDGE_LOOP ( 'NONE', ( #216601, #189949, #37655, #257944 ) ) ;
#116906 = VERTEX_POINT ( 'NONE', #133556 ) ;
#116907 = DIRECTION ( 'NONE',  ( 0.000000000000000000, 0.000000000000000000, -1.000000000000000000 ) ) ;
#116908 = CARTESIAN_POINT ( 'NONE',  ( -18.60000000000001208, -9.364240527590910190, -7.180248581840769972 ) ) ;
#116910 = ORIENTED_EDGE ( 'NONE', *, *, #241190, .T. ) ;
#116909 = LINE ( 'NONE', #131334, #75117 ) ;
#116911 = CARTESIAN_POINT ( 'NONE',  ( 22.57320508075687115, 55.89093952297024970, -232.7795287750844579 ) ) ;
#116912 = DIRECTION ( 'NONE',  ( -1.000000000000000000, 0.000000000000000000, 0.000000000000000000 ) ) ;
#116914 = EDGE_LOOP ( 'NONE', ( #233236, #105947, #174692, #128989 ) ) ;
#116913 = CARTESIAN_POINT ( 'NONE',  ( -16.90257928357875272, 60.93180429990802338, -221.0538891728311057 ) ) ;
#116915 = DIRECTION ( 'NONE',  ( 0.000000000000000000, 0.000000000000000000, -1.000000000000000000 ) ) ;
#116916 = ORIENTED_EDGE ( 'NONE', *, *, #59341, .F. ) ;
#116917 = FACE_OUTER_BOUND ( 'NONE', #198954, .T. ) ;
#116918 = EDGE_CURVE ( 'NONE', #251509, #137582, #68455, .T. ) ;
#116919 = CIRCLE ( 'NONE', #150260, 0.1000000000000028644 ) ;
#116921 = VERTEX_POINT ( 'NONE', #52725 ) ;
#116920 = DIRECTION ( 'NONE',  ( -1.000000000000000000, 0.000000000000000000, 0.000000000000000000 ) ) ;
#116922 = CARTESIAN_POINT ( 'NONE',  ( -23.15000000000000213, 40.44624540816119662, -247.8544895606997329 ) ) ;
#116923 = FACE_OUTER_BOUND ( 'NONE', #212366, .T. ) ;
#116924 = EDGE_CURVE ( 'NONE', #212797, #4741, #211826, .T. ) ;
#116925 = CARTESIAN_POINT ( 'NONE',  ( 19.75857864376269291, 11.75000000001116263, -91.85000000000005116 ) ) ;
#116926 = ORIENTED_EDGE ( 'NONE', *, *, #60814, .T. ) ;
#116928 = CARTESIAN_POINT ( 'NONE',  ( -21.05000000000000071, 76.00000000001195133, -103.0231074845243171 ) ) ;
#116927 = CARTESIAN_POINT ( 'NONE',  ( -16.96982749440684657, 9.950000000011137047, -46.62477840881235380 ) ) ;
#116929 = CARTESIAN_POINT ( 'NONE',  ( 21.05000000000000071, 76.00000000001210765, -132.5231074845243313 ) ) ;
#116930 = TOROIDAL_SURFACE ( 'NONE', #133675, 0.2000000000000000111, 0.1000000000000000056 ) ;
#116931 = CARTESIAN_POINT ( 'NONE',  ( 20.85000000000000142, 77.14957036958755054, -95.20719500002232394 ) ) ;
#116932 = CARTESIAN_POINT ( 'NONE',  ( -21.05000000000000071, -1.835341550213255957, -145.6551512925629766 ) ) ;
#116933 = ORIENTED_EDGE ( 'NONE', *, *, #223325, .F. ) ;
#116934 = EDGE_LOOP ( 'NONE', ( #24453, #5011, #123285, #190029 ) ) ;
#116935 = EDGE_CURVE ( 'NONE', #148681, #156004, #122449, .T. ) ;
#116937 = AXIS2_PLACEMENT_3D ( 'NONE', #68860, #10158, #166693 ) ;
#116936 = DIRECTION ( 'NONE',  ( -0.000000000000000000, 0.000000000000000000, -1.000000000000000000 ) ) ;
#116938 = CYLINDRICAL_SURFACE ( 'NONE', #194429, 0.1000000000000052097 ) ;
#116939 = ORIENTED_EDGE ( 'NONE', *, *, #248792, .T. ) ;
#116940 = CARTESIAN_POINT ( 'NONE',  ( -22.50000000000000000, 64.35000000001166143, -69.52310748452438816 ) ) ;
#116941 = ORIENTED_EDGE ( 'NONE', *, *, #187033, .F. ) ;
#116942 = DIRECTION ( 'NONE',  ( -1.000000000000000000, -2.952720810173289112E-16, 0.000000000000000000 ) ) ;
#116943 = CARTESIAN_POINT ( 'NONE',  ( -18.59999999999999787, 18.72524884453914851, -226.7284036107340341 ) ) ;
#116944 = EDGE_CURVE ( 'NONE', #127382, #179546, #14316, .T. ) ;
#116945 = EDGE_CURVE ( 'NONE', #12197, #129355, #76634, .T. ) ;
#116946 = CIRCLE ( 'NONE', #58659, 0.09999999999999939493 ) ;
#116947 = ORIENTED_EDGE ( 'NONE', *, *, #166041, .F. ) ;
#116948 = EDGE_CURVE ( 'NONE', #139104, #108958, #223041, .T. ) ;
#116949 = DIRECTION ( 'NONE',  ( -3.890533409366484652E-14, 0.1298341882520054891, 0.9915357197604850459 ) ) ;
#116951 = ORIENTED_EDGE ( 'NONE', *, *, #187832, .T. ) ;
#116950 = VECTOR ( 'NONE', #49261, 1000.000000000000227 ) ;
#116952 = ORIENTED_EDGE ( 'NONE', *, *, #137452, .T. ) ;
#116953 = ORIENTED_EDGE ( 'NONE', *, *, #16731, .F. ) ;
#116954 = AXIS2_PLACEMENT_3D ( 'NONE', #252535, #193868, #234255 ) ;
#116955 = FACE_OUTER_BOUND ( 'NONE', #162372, .T. ) ;
#116956 = CARTESIAN_POINT ( 'NONE',  ( -20.64999999999999858, 29.23678660621682113, -237.4641088729839282 ) ) ;
#116957 = CARTESIAN_POINT ( 'NONE',  ( -21.65000000000000213, 29.41239393758413811, -236.9245051605820720 ) ) ;
#116958 = CARTESIAN_POINT ( 'NONE',  ( -23.15000000000000213, 1.910280373842930812, -154.8686321448010972 ) ) ;
#116959 = LINE ( 'NONE', #195242, #242575 ) ;
#116960 = EDGE_CURVE ( 'NONE', #117463, #7468, #218267, .T. ) ;
#116962 = CARTESIAN_POINT ( 'NONE',  ( 18.59999999999999076, 63.62814136979439184, -224.4990371885399441 ) ) ;
#116961 = DIRECTION ( 'NONE',  ( 0.000000000000000000, -0.3738317757008748909, -0.9274965247785733613 ) ) ;
#116963 = CARTESIAN_POINT ( 'NONE',  ( 23.14999999999999858, -3.899999999988843502, -67.00000000000000000 ) ) ;
#116965 = VERTEX_POINT ( 'NONE', #216932 ) ;
#116964 = LINE ( 'NONE', #17845, #247856 ) ;
#116966 = CARTESIAN_POINT ( 'NONE',  ( -16.97683809663752186, 61.13629130372252973, -220.3155949669961444 ) ) ;
#116967 = ORIENTED_EDGE ( 'NONE', *, *, #240472, .F. ) ;
#116968 = LINE ( 'NONE', #97362, #86332 ) ;
#116969 = ORIENTED_EDGE ( 'NONE', *, *, #173557, .F. ) ;
#116970 = ORIENTED_EDGE ( 'NONE', *, *, #26286, .F. ) ;
#116971 = CARTESIAN_POINT ( 'NONE',  ( -16.93262454970419384, 65.99797953208116041, -48.59603125828708414 ) ) ;
#116972 = DIRECTION ( 'NONE',  ( -1.000000000000000000, -0.000000000000000000, 0.000000000000000000 ) ) ;
#116973 = CARTESIAN_POINT ( 'NONE',  ( -23.25000000000000000, 77.83585931145498193, -24.51866831572578675 ) ) ;
#116974 = ORIENTED_EDGE ( 'NONE', *, *, #257812, .F. ) ;
#116975 = DIRECTION ( 'NONE',  ( -3.265361837132813093E-16, -1.000000000000000000, -7.086529944415894657E-15 ) ) ;
#116976 = AXIS2_PLACEMENT_3D ( 'NONE', #15498, #238360, #216224 ) ;
#116977 = LINE ( 'NONE', #196499, #50964 ) ;
#116978 = EDGE_LOOP ( 'NONE', ( #118943, #253141, #17455, #41914 ) ) ;
#116979 = ORIENTED_EDGE ( 'NONE', *, *, #128117, .T. ) ;
#116980 = CARTESIAN_POINT ( 'NONE',  ( 20.94999999999999574, 16.44800918141279311, -240.8068063186265135 ) ) ;
#116981 = ORIENTED_EDGE ( 'NONE', *, *, #118735, .T. ) ;
#116982 = CARTESIAN_POINT ( 'NONE',  ( -20.94999999999999929, 1.835341550235569663, -145.5551512925629822 ) ) ;
#116983 = FACE_OUTER_BOUND ( 'NONE', #163891, .T. ) ;
#116984 = ORIENTED_EDGE ( 'NONE', *, *, #87414, .T. ) ;
#116985 = FACE_OUTER_BOUND ( 'NONE', #641, .T. ) ;
#116986 = FACE_OUTER_BOUND ( 'NONE', #84175, .T. ) ;
#116987 = CARTESIAN_POINT ( 'NONE',  ( 22.59066674512266104, 11.75000000001115552, -133.9694958763694217 ) ) ;
#116988 = ORIENTED_EDGE ( 'NONE', *, *, #120330, .F. ) ;
#116989 = DIRECTION ( 'NONE',  ( 0.000000000000000000, -0.8660254037844412611, -0.4999999999999956701 ) ) ;
#116990 = AXIS2_PLACEMENT_3D ( 'NONE', #133752, #112916, #51620 ) ;
#116991 = CIRCLE ( 'NONE', #137815, 0.09999999999999939493 ) ;
#116993 = DIRECTION ( 'NONE',  ( 1.000000000000000000, -0.000000000000000000, -0.000000000000000000 ) ) ;
#116992 = CIRCLE ( 'NONE', #4540, 0.09999999999999939493 ) ;
#116994 = AXIS2_PLACEMENT_3D ( 'NONE', #175089, #250716, #254541 ) ;
#116995 = CARTESIAN_POINT ( 'NONE',  ( -22.47886152344871391, 26.01172603257827731, -254.2798843218626530 ) ) ;
#116996 = ADVANCED_FACE ( 'NONE', ( #56553 ), #22306, .T. ) ;
#116997 = ORIENTED_EDGE ( 'NONE', *, *, #32878, .F. ) ;
#116998 = CARTESIAN_POINT ( 'NONE',  ( 21.13461538461538680, 10.61458296202553875, -12.25000000000000000 ) ) ;
#116999 = ORIENTED_EDGE ( 'NONE', *, *, #100669, .T. ) ;
#117000 = DIRECTION ( 'NONE',  ( -0.000000000000000000, 6.982962677686266711E-15, -1.000000000000000000 ) ) ;
#117001 = EDGE_CURVE ( 'NONE', #88576, #256296, #105843, .T. ) ;
#117002 = CARTESIAN_POINT ( 'NONE',  ( -13.39999999999994351, 67.75000000001118394, -23.62310748452479103 ) ) ;
#117003 = DIRECTION ( 'NONE',  ( 1.000000000000000000, 3.265361837132813093E-16, -0.000000000000000000 ) ) ;
#117004 = CARTESIAN_POINT ( 'NONE',  ( 18.59999999999997655, 76.00000000001207923, -128.6231074845243540 ) ) ;
#117005 = CARTESIAN_POINT ( 'NONE',  ( 23.14999999999999858, 36.65892442174472876, -249.5511627012454596 ) ) ;
#117006 = DIRECTION ( 'NONE',  ( -1.000000000000000000, -0.000000000000000000, 0.000000000000000000 ) ) ;
#117007 = VECTOR ( 'NONE', #125052, 1000.000000000000000 ) ;
#117008 = VERTEX_POINT ( 'NONE', #82214 ) ;
#117009 = CARTESIAN_POINT ( 'NONE',  ( -16.93339986808596365, 65.99489607144613501, -123.9571138127115120 ) ) ;
#117010 = LINE ( 'NONE', #218658, #77412 ) ;
#117011 = ADVANCED_FACE ( 'NONE', ( #221735 ), #241343, .T. ) ;
#117012 = ADVANCED_FACE ( 'NONE', ( #104358 ), #143504, .T. ) ;
#117013 = CARTESIAN_POINT ( 'NONE',  ( -18.33981767444349131, 77.36688828064514212, -241.8004678266106851 ) ) ;
#117014 = DIRECTION ( 'NONE',  ( 0.000000000000000000, 0.000000000000000000, -1.000000000000000000 ) ) ;
#117015 = B_SPLINE_CURVE_WITH_KNOTS ( 'NONE', 3,
 ( #132682, #127540, #148392, #28483, #227924, #212230, #31044, #190084, #208381, #10166, #33624, #89676, #107979, #169273, #248780, #70161 ),
 .UNSPECIFIED., .F., .F.,
 ( 4, 3, 3, 3, 3, 4 ),
 ( 0.000000000000000000, 2.372700795693896277E-05, 5.739057815866941569E-05, 9.073899019179925297E-05, 0.0001243544287365695982, 0.0001585386695601168831 ),
 .UNSPECIFIED. ) ;
#117016 = CARTESIAN_POINT ( 'NONE',  ( 20.22894356738409272, 66.72150177717388431, -61.25458457828101189 ) ) ;
#117017 = ORIENTED_EDGE ( 'NONE', *, *, #174907, .T. ) ;
#117018 = ORIENTED_EDGE ( 'NONE', *, *, #4722, .T. ) ;
#117019 = CARTESIAN_POINT ( 'NONE',  ( 23.14999999999999503, 64.35000000001228670, -157.8731074845244393 ) ) ;
#117020 = FACE_OUTER_BOUND ( 'NONE', #202430, .T. ) ;
#117021 = CARTESIAN_POINT ( 'NONE',  ( -18.40000000000000213, 11.47316190336248809, -20.94999999999999929 ) ) ;
#117022 = DIRECTION ( 'NONE',  ( 0.000000000000000000, 0.3634403228828347321, -0.9316174814283063599 ) ) ;
#117023 = LINE ( 'NONE', #57015, #124590 ) ;
#117024 = EDGE_CURVE ( 'NONE', #111426, #26411, #142221, .T. ) ;
#117025 = VECTOR ( 'NONE', #117986, 1000.000000000000000 ) ;
#117026 = VERTEX_POINT ( 'NONE', #202206 ) ;
#117027 = DIRECTION ( 'NONE',  ( -1.000000000000000000, 0.000000000000000000, -0.000000000000000000 ) ) ;
#117028 = EDGE_CURVE ( 'NONE', #211866, #16002, #196110, .T. ) ;
#117029 = DIRECTION ( 'NONE',  ( 0.000000000000000000, 0.000000000000000000, -1.000000000000000000 ) ) ;
#117030 = VECTOR ( 'NONE', #129535, 999.9999999999998863 ) ;
#117031 = ORIENTED_EDGE ( 'NONE', *, *, #83486, .T. ) ;
#117032 = CYLINDRICAL_SURFACE ( 'NONE', #237975, 0.1000000000000028644 ) ;
#117033 = PRODUCT_RELATED_PRODUCT_CATEGORY ( 'part', '', ( #168068 ) ) ;
#117034 = CARTESIAN_POINT ( 'NONE',  ( 18.59999999999999076, 1.115600667400684642E-11, -67.00000000000000000 ) ) ;
#117035 = AXIS2_PLACEMENT_3D ( 'NONE', #37607, #196649, #218771 ) ;
#117036 = AXIS2_PLACEMENT_3D ( 'NONE', #253582, #55353, #134900 ) ;
#117037 = ORIENTED_EDGE ( 'NONE', *, *, #229178, .T. ) ;
#117038 = CARTESIAN_POINT ( 'NONE',  ( -21.14999999893415250, 12.93738826932868591, -205.1873143274057441 ) ) ;
#117039 = EDGE_CURVE ( 'NONE', #237441, #161574, #45691, .T. ) ;
#117040 = CIRCLE ( 'NONE', #83682, 0.1000000000000028644 ) ;
#117041 = ORIENTED_EDGE ( 'NONE', *, *, #248566, .F. ) ;
#117042 = EDGE_CURVE ( 'NONE', #87114, #164666, #37059, .T. ) ;
#117043 = DIRECTION ( 'NONE',  ( -1.000000000000000000, 0.000000000000000000, 0.000000000000000000 ) ) ;
#117044 = EDGE_CURVE ( 'NONE', #94097, #149671, #226661, .T. ) ;
#117045 = DIRECTION ( 'NONE',  ( 0.000000000000000000, -0.3738317757009345654, 0.9274965247785492695 ) ) ;
#117046 = LINE ( 'NONE', #15390, #36679 ) ;
#117047 = CARTESIAN_POINT ( 'NONE',  ( 22.24259225415828212, 75.90093411655959699, -177.5150453550897680 ) ) ;
#117048 = DIRECTION ( 'NONE',  ( 0.000000000000000000, 7.086529944415886769E-15, -1.000000000000000000 ) ) ;
#117049 = CARTESIAN_POINT ( 'NONE',  ( 21.05000000000000071, 18.65488991999773916, -228.0822300706204544 ) ) ;
#117050 = DIRECTION ( 'NONE',  ( 0.000000000000000000, -0.01562499999999307672, 0.9998779222360100194 ) ) ;
#117051 = DIRECTION ( 'NONE',  ( -4.701977403289177357E-30, 0.8814952561688512711, -0.4721928772777193584 ) ) ;
#117052 = DIRECTION ( 'NONE',  ( 0.000000000000000000, 3.552713678800446104E-15, -1.000000000000000000 ) ) ;
#117053 = DIRECTION ( 'NONE',  ( 0.000000000000000000, 0.000000000000000000, -1.000000000000000000 ) ) ;
#117054 = DIRECTION ( 'NONE',  ( -1.000000000000000000, 1.836970198721029934E-16, 1.282749433769087757E-30 ) ) ;
#117055 = CARTESIAN_POINT ( 'NONE',  ( -18.59999999999999787, 9.350000000011156942, -54.75000000000000000 ) ) ;
#117056 = PLANE ( 'NONE',  #57257 ) ;
#117057 = CIRCLE ( 'NONE', #146265, 0.09999999999999714673 ) ;
#117058 = TOROIDAL_SURFACE ( 'NONE', #46122, 0.4000000000000009104, 0.1000000000000000056 ) ;
#117059 = CARTESIAN_POINT ( 'NONE',  ( 21.09793522318426540, 10.72462451022393282, -79.23929087097731383 ) ) ;
#117060 = CARTESIAN_POINT ( 'NONE',  ( 20.04142135623731136, 11.75000000001116085, -158.7671572875253787 ) ) ;
#117061 = VECTOR ( 'NONE', #143710, 1000.000000000000000 ) ;
#117062 = VERTEX_POINT ( 'NONE', #242598 ) ;
#117063 = CIRCLE ( 'NONE', #212745, 0.1000000000000106498 ) ;
#117064 = DIRECTION ( 'NONE',  ( 0.000000000000000000, 0.000000000000000000, -1.000000000000000000 ) ) ;
#117065 = DIRECTION ( 'NONE',  ( 0.000000000000000000, 0.000000000000000000, 1.000000000000000000 ) ) ;
#117066 = DIRECTION ( 'NONE',  ( 0.000000000000000000, -1.000000000000000000, 0.000000000000000000 ) ) ;
#117067 = VECTOR ( 'NONE', #192570, 1000.000000000000000 ) ;
#117068 = CIRCLE ( 'NONE', #150409, 0.2000000000000027867 ) ;
#117069 = ORIENTED_EDGE ( 'NONE', *, *, #121225, .F. ) ;
#117070 = DIRECTION ( 'NONE',  ( 0.000000000000000000, 0.000000000000000000, -1.000000000000000000 ) ) ;
#117071 = EDGE_CURVE ( 'NONE', #34161, #208409, #64181, .T. ) ;
#117072 = CARTESIAN_POINT ( 'NONE',  ( -23.25000000000000000, 45.96866462019919197, -240.6139518702713360 ) ) ;
#117073 = ORIENTED_EDGE ( 'NONE', *, *, #91802, .T. ) ;
#117074 = CARTESIAN_POINT ( 'NONE',  ( -21.14999999999999858, 38.04609728753136011, -236.0545303518866547 ) ) ;
#117075 = DIRECTION ( 'NONE',  ( 0.000000000000000000, -0.5283051335750404975, 0.8490545835446967615 ) ) ;
#117076 = CIRCLE ( 'NONE', #137895, 0.1000000000000055705 ) ;
#117077 = ORIENTED_EDGE ( 'NONE', *, *, #83706, .T. ) ;
#117078 = AXIS2_PLACEMENT_3D ( 'NONE', #10647, #51014, #212705 ) ;
#117079 = VECTOR ( 'NONE', #245301, 1000.000000000000000 ) ;
#117080 = CIRCLE ( 'NONE', #104574, 0.1000000000000013933 ) ;
#117081 = VERTEX_POINT ( 'NONE', #26147 ) ;
#117082 = CARTESIAN_POINT ( 'NONE',  ( -18.50000000000000711, 64.25000000001210765, -129.5083017138703667 ) ) ;
#117083 = EDGE_CURVE ( 'NONE', #163525, #206950, #135059, .T. ) ;
#117084 = ORIENTED_EDGE ( 'NONE', *, *, #50270, .T. ) ;
#117085 = CARTESIAN_POINT ( 'NONE',  ( -21.05000000000000071, 57.76315019072730905, -226.2583585926041110 ) ) ;
#117086 = CARTESIAN_POINT ( 'NONE',  ( 21.05000000000000071, 67.22371710471958295, -124.3731074845243683 ) ) ;
#117087 = FACE_OUTER_BOUND ( 'NONE', #150458, .T. ) ;
#117088 = EDGE_CURVE ( 'NONE', #65528, #141019, #109951, .T. ) ;
#117089 = FACE_OUTER_BOUND ( 'NONE', #217228, .T. ) ;
#117090 = CARTESIAN_POINT ( 'NONE',  ( -16.87372386987899375, 9.880600233636760876, -13.14926987186641405 ) ) ;
#117091 = CARTESIAN_POINT ( 'NONE',  ( -14.45443560709636444, 46.53556350520271678, -234.7709563976631841 ) ) ;
#117092 = DIRECTION ( 'NONE',  ( -1.000000000000000000, 0.000000000000000000, 0.000000000000000000 ) ) ;
#117093 = DIRECTION ( 'NONE',  ( 1.000000000000000000, 0.000000000000000000, 0.000000000000000000 ) ) ;
#117094 = EDGE_CURVE ( 'NONE', #148712, #68027, #184981, .T. ) ;
#117096 = ORIENTED_EDGE ( 'NONE', *, *, #1863, .F. ) ;
#117095 = CARTESIAN_POINT ( 'NONE',  ( -18.59999999999999787, -1.835341550213255957, -45.05515129256298223 ) ) ;
#117097 = EDGE_LOOP ( 'NONE', ( #73559, #69905, #164148, #18110, #84000, #185567, #139367, #249559, #72393, #243432, #67776, #50795, #115561, #253097 ) ) ;
#117099 = CARTESIAN_POINT ( 'NONE',  ( -21.14999999999999858, 76.00000000001165290, -69.52310748452431710 ) ) ;
#117098 = DIRECTION ( 'NONE',  ( -1.000000000000000000, 0.000000000000000000, 0.000000000000000000 ) ) ;
#117101 = VERTEX_POINT ( 'NONE', #130352 ) ;
#117100 = LINE ( 'NONE', #119672, #194383 ) ;
#117102 = EDGE_LOOP ( 'NONE', ( #202380, #54076, #163173, #24712 ) ) ;
#117103 = CARTESIAN_POINT ( 'NONE',  ( 23.25000000000000000, 87.75000000001222134, -148.2731074845242176 ) ) ;
#117104 = CARTESIAN_POINT ( 'NONE',  ( -20.54999999999999716, 7.250000000011155521, -179.7499999999999716 ) ) ;
#117105 = EDGE_CURVE ( 'NONE', #163070, #67817, #208641, .T. ) ;
#117106 = EDGE_CURVE ( 'NONE', #256102, #19594, #124807, .T. ) ;
#117107 = CARTESIAN_POINT ( 'NONE',  ( -22.59999999999999787, 75.89914163091303578, -81.27267460801371612 ) ) ;
#117108 = DIRECTION ( 'NONE',  ( 0.000000000000000000, 6.982962677686266711E-15, -1.000000000000000000 ) ) ;
#117109 = CYLINDRICAL_SURFACE ( 'NONE', #48419, 0.1000000000000028644 ) ;
#117110 = DIRECTION ( 'NONE',  ( 1.000000000000000000, -0.000000000000000000, -0.000000000000000000 ) ) ;
#117111 = LINE ( 'NONE', #157559, #7064 ) ;
#117112 = VECTOR ( 'NONE', #212432, 1000.000000000000000 ) ;
#117113 = DIRECTION ( 'NONE',  ( 0.000000000000000000, -6.982962677686266711E-15, 1.000000000000000000 ) ) ;
#117114 = ORIENTED_EDGE ( 'NONE', *, *, #234694, .T. ) ;
#117115 = ORIENTED_EDGE ( 'NONE', *, *, #92615, .T. ) ;
#117116 = DIRECTION ( 'NONE',  ( 1.000000000000000000, 8.674042436075353235E-17, 1.619280515896125144E-16 ) ) ;
#117117 = ADVANCED_FACE ( 'NONE', ( #190361 ), #147362, .T. ) ;
#117118 = VERTEX_POINT ( 'NONE', #127810 ) ;
#117119 = DIRECTION ( 'NONE',  ( 0.000000000000000000, -6.982962677686266711E-15, 1.000000000000000000 ) ) ;
#117121 = ADVANCED_FACE ( 'NONE', ( #11725 ), #228194, .T. ) ;
#117120 = EDGE_LOOP ( 'NONE', ( #138988, #136315, #133176, #201842, #161511, #218171, #156688, #220061, #145322, #178223, #3306, #68095, #137801, #63161, #22092, #110899, #240738, #32704, #68104, #253459, #207705, #94498, #169115, #47650, #250863, #101590, #116552 ) ) ;
#117122 = CARTESIAN_POINT ( 'NONE',  ( -22.49231231312463208, 64.35001509633487160, -136.5841603721257513 ) ) ;
#117123 = AXIS2_PLACEMENT_3D ( 'NONE', #149378, #228894, #85483 ) ;
#117124 = CARTESIAN_POINT ( 'NONE',  ( -14.22969084473441370, 49.66582466164803833, -233.3627041835000000 ) ) ;
#117125 = CARTESIAN_POINT ( 'NONE',  ( -23.15000000000000213, 76.00000000001197975, -107.1731074845243086 ) ) ;
#117126 = EDGE_CURVE ( 'NONE', #214000, #52139, #97457, .T. ) ;
#117128 = ORIENTED_EDGE ( 'NONE', *, *, #78130, .T. ) ;
#117127 = CARTESIAN_POINT ( 'NONE',  ( 23.14999999999999503, 6.649999999999999467, -21.15000000000000213 ) ) ;
#117129 = CARTESIAN_POINT ( 'NONE',  ( 19.97071067811864609, 34.39212750349580006, -235.0405048756463486 ) ) ;
#117130 = ORIENTED_EDGE ( 'NONE', *, *, #191058, .T. ) ;
#117131 = DIRECTION ( 'NONE',  ( -1.000000000000000000, 0.000000000000000000, 0.000000000000000000 ) ) ;
#117132 = DIRECTION ( 'NONE',  ( 0.000000000000000000, -0.2617529984165031243, -0.9651348961777157509 ) ) ;
#117133 = DIRECTION ( 'NONE',  ( 1.186688945009009831E-16, -1.000000000000000000, 0.000000000000000000 ) ) ;
#117134 = EDGE_CURVE ( 'NONE', #191649, #129114, #130802, .T. ) ;
#117135 = DIRECTION ( 'NONE',  ( 1.000000000000000000, 0.000000000000000000, 0.000000000000000000 ) ) ;
#117137 = ORIENTED_EDGE ( 'NONE', *, *, #88066, .T. ) ;
#117136 = EDGE_CURVE ( 'NONE', #194619, #160806, #164146, .T. ) ;
#117139 = CARTESIAN_POINT ( 'NONE',  ( 21.05000000000000071, 5.850000000011156942, -56.86750277572208034 ) ) ;
#117138 = CIRCLE ( 'NONE', #208731, 0.1000000000000021427 ) ;
#117140 = VERTEX_POINT ( 'NONE', #87369 ) ;
#117143 = ORIENTED_EDGE ( 'NONE', *, *, #41904, .F. ) ;
#117142 = PLANE ( 'NONE',  #38901 ) ;
#117141 = DIRECTION ( 'NONE',  ( 0.000000000000000000, 0.000000000000000000, -1.000000000000000000 ) ) ;
#117144 = CARTESIAN_POINT ( 'NONE',  ( -21.07928932188134041, 0.09889514566555068775, -161.1714833436066669 ) ) ;
#117145 = CIRCLE ( 'NONE', #108756, 11.80000000000000249 ) ;
#117147 = EDGE_CURVE ( 'NONE', #220516, #1991, #197432, .T. ) ;
#117146 = B_SPLINE_CURVE_WITH_KNOTS ( 'NONE', 3,
 ( #84394, #221370, #205667, #27078, #117490, #223947, #201829, #83125, #204384, #162721 ),
 .UNSPECIFIED., .F., .F.,
 ( 4, 3, 3, 4 ),
 ( 1.886399917053072492E-15, 3.877043166999333273E-05, 7.336897548476527698E-05, 7.659383120239750958E-05 ),
 .UNSPECIFIED. ) ;
#117148 = CARTESIAN_POINT ( 'NONE',  ( 21.15000000000005187, 77.83551161375991967, -47.52760213295649550 ) ) ;
#117149 = ORIENTED_EDGE ( 'NONE', *, *, #47550, .T. ) ;
#117150 = CARTESIAN_POINT ( 'NONE',  ( 18.39999999999999858, 85.50000000001209344, -129.6009576351939074 ) ) ;
#117152 = FACE_OUTER_BOUND ( 'NONE', #176556, .T. ) ;
#117151 =( BOUNDED_SURFACE ( )  B_SPLINE_SURFACE ( 3, 2, ( 
 ( #37768, #33945, #76859 ),
 ( #194281, #93861, #117287 ),
 ( #258022, #192978, #118585 ),
 ( #75613, #155162, #54733 ) ),
 .UNSPECIFIED., .F., .F., .F. ) 
 B_SPLINE_SURFACE_WITH_KNOTS ( ( 4, 4 ),
 ( 3, 3 ),
 ( -3.469446951953614189E-18, 0.001979672783031532438 ),
 ( 0.000000000000000000, 1.000000000000000000 ),
 .UNSPECIFIED. ) 
 GEOMETRIC_REPRESENTATION_ITEM ( )  RATIONAL_B_SPLINE_SURFACE ( (
 ( 1.000000000000000000, 0.7103081912008384347, 1.000000000000000000),
 ( 1.000000000000000000, 0.7104998333558053547, 1.000000000000000000),
 ( 1.000000000000000000, 0.7107238315755477487, 1.000000000000000000),
 ( 1.000000000000000000, 0.7110073749539295163, 1.000000000000000000) ) ) 
 REPRESENTATION_ITEM ( '' )  SURFACE ( )  );
#117153 = EDGE_CURVE ( 'NONE', #46953, #109034, #72562, .T. ) ;
#117154 = CARTESIAN_POINT ( 'NONE',  ( 20.85000000000000142, 76.00000000001170974, -69.52310748452431710 ) ) ;
#117155 = EDGE_CURVE ( 'NONE', #47266, #2253, #118349, .T. ) ;
#117157 = EDGE_LOOP ( 'NONE', ( #189956, #6577, #207391, #224857 ) ) ;
#117156 = CARTESIAN_POINT ( 'NONE',  ( -21.14999999999999858, -11.74999999998884448, -67.00000000000004263 ) ) ;
#117158 = DIRECTION ( 'NONE',  ( -1.000000000000000000, 0.000000000000000000, 0.000000000000000000 ) ) ;
#117159 = VECTOR ( 'NONE', #166564, 1000.000000000000000 ) ;
#117160 = EDGE_LOOP ( 'NONE', ( #253193, #239443, #97626, #88907 ) ) ;
#117161 = DIRECTION ( 'NONE',  ( 1.000000000000000000, 0.000000000000000000, 0.000000000000000000 ) ) ;
#117162 = CARTESIAN_POINT ( 'NONE',  ( 18.49999999999998579, -9.321008403350155902, -74.23593824907788985 ) ) ;
#117163 = CARTESIAN_POINT ( 'NONE',  ( -18.59999999999999787, 78.48087866980282001, -232.8271061603568910 ) ) ;
#117164 = ORIENTED_EDGE ( 'NONE', *, *, #136335, .F. ) ;
#117165 = CARTESIAN_POINT ( 'NONE',  ( -16.87368910959167678, 66.03872618332088962, -157.4106143878838395 ) ) ;
#117166 = ORIENTED_EDGE ( 'NONE', *, *, #58530, .F. ) ;
#117167 = DIRECTION ( 'NONE',  ( 1.000000000000000000, 0.000000000000000000, -0.000000000000000000 ) ) ;
#117168 = DIRECTION ( 'NONE',  ( -1.000000000000000000, 0.000000000000000000, 0.000000000000000000 ) ) ;
#117169 = CARTESIAN_POINT ( 'NONE',  ( -21.64999999999999858, 7.250000000011148416, -121.7500000000000426 ) ) ;
#117170 = B_SPLINE_CURVE_WITH_KNOTS ( 'NONE', 3,
 ( #115135, #194701, #16065, #215509, #95563, #235091, #56425, #135962, #195971, #36920 ),
 .UNSPECIFIED., .F., .F.,
 ( 4, 3, 3, 4 ),
 ( 4.336808689942017736E-19, 0.0002000000000002811161, 0.001000000000045105867, 0.001967863649472137346 ),
 .UNSPECIFIED. ) ;
#117171 = ORIENTED_EDGE ( 'NONE', *, *, #239374, .F. ) ;
#117172 = CYLINDRICAL_SURFACE ( 'NONE', #196209, 0.5000000000000004441 ) ;
#117173 = DIRECTION ( 'NONE',  ( 0.000000000000000000, 0.2002428086779743377, -0.9797463026583749235 ) ) ;
#117174 = VECTOR ( 'NONE', #133969, 1000.000000000000000 ) ;
#117175 = CIRCLE ( 'NONE', #150496, 3.999999999999996447 ) ;
#117176 = LINE ( 'NONE', #201836, #125162 ) ;
#117177 = ORIENTED_EDGE ( 'NONE', *, *, #237101, .F. ) ;
#117178 = SPHERICAL_SURFACE ( 'NONE', #164034, 0.1000000000000000056 ) ;
#117179 = DIRECTION ( 'NONE',  ( -1.000000000000000000, 0.000000000000000000, 0.000000000000000000 ) ) ;
#117180 = DIRECTION ( 'NONE',  ( 0.000000000000000000, 0.000000000000000000, 1.000000000000000000 ) ) ;
#117181 = ADVANCED_FACE ( 'NONE', ( #166965 ), #151692, .F. ) ;
#117182 = ORIENTED_EDGE ( 'NONE', *, *, #143549, .F. ) ;
#117183 = ORIENTED_EDGE ( 'NONE', *, *, #223331, .T. ) ;
#117185 = EDGE_LOOP ( 'NONE', ( #42109, #152279, #96537, #34000 ) ) ;
#117184 = CARTESIAN_POINT ( 'NONE',  ( 23.14999999999999858, 67.23127455305835554, -235.8551265064784559 ) ) ;
#117186 = TOROIDAL_SURFACE ( 'NONE', #9040, 11.89999999999999858, 0.1000000000000000056 ) ;
#117189 = ORIENTED_EDGE ( 'NONE', *, *, #76367, .T. ) ;
#117188 = VERTEX_POINT ( 'NONE', #52093 ) ;
#117187 = LINE ( 'NONE', #18073, #34629 ) ;
#117190 = FACE_OUTER_BOUND ( 'NONE', #170046, .T. ) ;
#117191 = CARTESIAN_POINT ( 'NONE',  ( -21.08376601933334271, 0.06377601094103295398, -161.1580527287242433 ) ) ;
#117192 = FACE_OUTER_BOUND ( 'NONE', #159769, .T. ) ;
#117193 = CARTESIAN_POINT ( 'NONE',  ( -16.83233564386407366, 12.42141036011986621, -211.3697030754569255 ) ) ;
#117195 = ADVANCED_FACE ( 'NONE', ( #185207 ), #108245, .T. ) ;
#117194 = CARTESIAN_POINT ( 'NONE',  ( 21.05933563467872460, 10.72452471209247626, -112.6936477489559820 ) ) ;
#117196 = DIRECTION ( 'NONE',  ( 1.000000000000000000, 0.000000000000000000, 0.000000000000000000 ) ) ;
#117197 = CARTESIAN_POINT ( 'NONE',  ( -18.50000000000000000, 2.319530388122570841, -217.8268657444419887 ) ) ;
#117199 = DIRECTION ( 'NONE',  ( -1.000000000000000000, 0.000000000000000000, 0.000000000000000000 ) ) ;
#117198 = DIRECTION ( 'NONE',  ( 0.000000000000000000, 6.982962677686266711E-15, -1.000000000000000000 ) ) ;
#117200 = ORIENTED_EDGE ( 'NONE', *, *, #257494, .T. ) ;
#117201 = ORIENTED_EDGE ( 'NONE', *, *, #172732, .F. ) ;
#117202 = ORIENTED_EDGE ( 'NONE', *, *, #109828, .T. ) ;
#117203 = LINE ( 'NONE', #58483, #195717 ) ;
#117205 = ORIENTED_EDGE ( 'NONE', *, *, #91827, .T. ) ;
#117204 = FACE_OUTER_BOUND ( 'NONE', #185740, .T. ) ;
#117206 = DIRECTION ( 'NONE',  ( 0.7070776581708965169, 0.000000000000000000, 0.7071359030027827286 ) ) ;
#117207 = ORIENTED_EDGE ( 'NONE', *, *, #22072, .T. ) ;
#117209 = DIRECTION ( 'NONE',  ( 1.000000000000000000, -3.469446951953635646E-14, 0.000000000000000000 ) ) ;
#117208 = TOROIDAL_SURFACE ( 'NONE', #37942, 0.2000000000000000111, 0.1000000000000000056 ) ;
#117210 = EDGE_LOOP ( 'NONE', ( #64853, #224743 ) ) ;
#117211 = DIRECTION ( 'NONE',  ( 1.000000000000000000, 0.000000000000000000, 0.000000000000000000 ) ) ;
#117212 = CIRCLE ( 'NONE', #154649, 6.258578643762700011 ) ;
#117213 = ORIENTED_EDGE ( 'NONE', *, *, #49037, .T. ) ;
#117215 = AXIS2_PLACEMENT_3D ( 'NONE', #71292, #70010, #230330 ) ;
#117214 = FACE_OUTER_BOUND ( 'NONE', #112334, .T. ) ;
#117216 = CARTESIAN_POINT ( 'NONE',  ( -23.25000000000000000, 0.000000000000000000, -33.50000000000000000 ) ) ;
#117218 = ORIENTED_EDGE ( 'NONE', *, *, #235505, .F. ) ;
#117217 = VERTEX_POINT ( 'NONE', #86070 ) ;
#117219 = ORIENTED_EDGE ( 'NONE', *, *, #147826, .F. ) ;
#117221 = DIRECTION ( 'NONE',  ( 0.000000000000000000, -0.9654727137038715545, -0.2605042016806676242 ) ) ;
#117220 = VECTOR ( 'NONE', #169649, 1000.000000000000000 ) ;
#117222 = ORIENTED_EDGE ( 'NONE', *, *, #127211, .F. ) ;
#117223 = ORIENTED_EDGE ( 'NONE', *, *, #201304, .T. ) ;
#117224 = B_SPLINE_CURVE_WITH_KNOTS ( 'NONE', 3,
 ( #86904, #83040, #127341, #8677, #84297, #184732 ),
 .UNSPECIFIED., .F., .F.,
 ( 4, 2, 4 ),
 ( 0.000000000000000000, 0.0001891491689349559776, 0.0003782983378699119551 ),
 .UNSPECIFIED. ) ;
#117225 = DIRECTION ( 'NONE',  ( -1.000000000000000000, -0.000000000000000000, 0.000000000000000000 ) ) ;
#117226 = CIRCLE ( 'NONE', #217149, 0.09999999999999938105 ) ;
#117228 = ORIENTED_EDGE ( 'NONE', *, *, #254114, .F. ) ;
#117227 = DIRECTION ( 'NONE',  ( -1.000000000000000000, 0.000000000000000000, 0.000000000000000000 ) ) ;
#117230 = DIRECTION ( 'NONE',  ( -1.000000000000000000, -3.439547145395919517E-14, -4.624352451196577991E-15 ) ) ;
#117229 = DIRECTION ( 'NONE',  ( -1.000000000000000000, 0.000000000000000000, 0.000000000000000000 ) ) ;
#117231 = CARTESIAN_POINT ( 'NONE',  ( -20.94999999999999929, 76.00000000001244871, -170.0231074845243597 ) ) ;
#117232 = CARTESIAN_POINT ( 'NONE',  ( -15.55912972643740488, 52.30666975485627290, -233.2371980086100507 ) ) ;
#117233 = DIRECTION ( 'NONE',  ( 0.000000000000000000, 0.000000000000000000, -1.000000000000000000 ) ) ;
#117234 = ORIENTED_EDGE ( 'NONE', *, *, #143595, .T. ) ;
#117235 = VECTOR ( 'NONE', #256051, 1000.000000000000000 ) ;
#117236 = ORIENTED_EDGE ( 'NONE', *, *, #127109, .F. ) ;
#117237 = CARTESIAN_POINT ( 'NONE',  ( -18.40000000000000213, 11.47316190337362762, -46.15000000000000568 ) ) ;
#117238 = DIRECTION ( 'NONE',  ( 0.000000000000000000, 0.000000000000000000, -1.000000000000000000 ) ) ;
#117239 = FACE_OUTER_BOUND ( 'NONE', #252162, .T. ) ;
#117240 = EDGE_CURVE ( 'NONE', #156138, #28028, #187790, .T. ) ;
#117242 = VERTEX_POINT ( 'NONE', #9141 ) ;
#117241 = CIRCLE ( 'NONE', #54688, 0.09999999999999939493 ) ;
#117243 = DIRECTION ( 'NONE',  ( 0.000000000000000000, -0.9915357197604853789, 0.1298341882520022694 ) ) ;
#117244 = DIRECTION ( 'NONE',  ( 0.000000000000000000, 0.000000000000000000, -1.000000000000000000 ) ) ;
#117245 = LINE ( 'NONE', #101477, #146744 ) ;
#117246 = ORIENTED_EDGE ( 'NONE', *, *, #134080, .T. ) ;
#117247 = VERTEX_POINT ( 'NONE', #67821 ) ;
#117249 =( BOUNDED_SURFACE ( )  B_SPLINE_SURFACE ( 3, 2, ( 
 ( #145881, #224137, #187610 ),
 ( #24695, #87182, #127621 ),
 ( #183743, #166778, #246285 ),
 ( #45511, #207165, #108060 ),
 ( #168074, #62515, #142036 ),
 ( #221552, #23415, #102891 ) ),
 .UNSPECIFIED., .F., .F., .T. ) 
 B_SPLINE_SURFACE_WITH_KNOTS ( ( 4, 2, 4 ),
 ( 3, 3 ),
 ( 6.719893378901017553E-05, 0.0002757154632485590319, 0.0004842319927081078341 ),
 ( 0.000000000000000000, 1.000000000000000000 ),
 .UNSPECIFIED. ) 
 GEOMETRIC_REPRESENTATION_ITEM ( )  RATIONAL_B_SPLINE_SURFACE ( (
 ( 1.000000000000000000, 0.7250110520819756932, 1.000000000000000000),
 ( 1.000000000000000000, 0.7277932058357919898, 1.000000000000000000),
 ( 1.000000000000000000, 0.7278452872619233238, 1.000000000000000000),
 ( 1.000000000000000000, 0.7221445671547584988, 1.000000000000000000),
 ( 1.000000000000000000, 0.7163662143780743508, 1.000000000000000000),
 ( 1.000000000000000000, 0.7071067811865475727, 1.000000000000000000) ) ) 
 REPRESENTATION_ITEM ( '' )  SURFACE ( )  );
#117248 = TOROIDAL_SURFACE ( 'NONE', #146276, 11.90000000000000391, 0.1000000000000000056 ) ;
#117250 = EDGE_CURVE ( 'NONE', #164531, #241241, #31080, .T. ) ;
#117251 = DIRECTION ( 'NONE',  ( -1.000000000000000000, -0.000000000000000000, -0.000000000000000000 ) ) ;
#117252 = LINE ( 'NONE', #97654, #107115 ) ;
#117253 = VERTEX_POINT ( 'NONE', #10430 ) ;
#117254 = LINE ( 'NONE', #216339, #47362 ) ;
#117255 = ORIENTED_EDGE ( 'NONE', *, *, #142002, .T. ) ;
#117257 = AXIS2_PLACEMENT_3D ( 'NONE', #38235, #61639, #141179 ) ;
#117256 = DIRECTION ( 'NONE',  ( -2.602085213965226419E-14, -0.000000000000000000, 1.000000000000000000 ) ) ;
#117259 = CARTESIAN_POINT ( 'NONE',  ( -22.50000000000000000, 55.96597777900654336, -232.8853806925634444 ) ) ;
#117258 = FACE_OUTER_BOUND ( 'NONE', #134744, .T. ) ;
#117260 = ADVANCED_FACE ( 'NONE', ( #89944 ), #139342, .T. ) ;
#117261 = FACE_OUTER_BOUND ( 'NONE', #62609, .T. ) ;
#117262 = LINE ( 'NONE', #18152, #141120 ) ;
#117263 = EDGE_CURVE ( 'NONE', #8049, #235252, #64362, .T. ) ;
#117264 = DIRECTION ( 'NONE',  ( 0.000000000000000000, -0.6728971962616697722, -0.7397360091702875895 ) ) ;
#117265 = VECTOR ( 'NONE', #6412, 1000.000000000000000 ) ;
#117266 = AXIS2_PLACEMENT_3D ( 'NONE', #243702, #62506, #41671 ) ;
#117267 = AXIS2_PLACEMENT_3D ( 'NONE', #11227, #187306, #68635 ) ;
#117269 = ORIENTED_EDGE ( 'NONE', *, *, #67586, .F. ) ;
#117268 = ORIENTED_EDGE ( 'NONE', *, *, #142983, .F. ) ;
#117271 = VERTEX_POINT ( 'NONE', #233345 ) ;
#117270 = AXIS2_PLACEMENT_3D ( 'NONE', #60170, #154501, #43197 ) ;
#117272 = CARTESIAN_POINT ( 'NONE',  ( 23.40000000000005542, 64.35000000001120668, -3.123107484524795474 ) ) ;
#117273 = CARTESIAN_POINT ( 'NONE',  ( -16.79184697841823848, 60.94163718135611418, -221.0380540244521228 ) ) ;
#117274 = CARTESIAN_POINT ( 'NONE',  ( -20.94999999999999929, 1.115600667400684642E-11, -129.9000000000000341 ) ) ;
#117275 = CARTESIAN_POINT ( 'NONE',  ( 21.14999999999999503, 36.65892442174472876, -249.5511627012454596 ) ) ;
#117276 = ADVANCED_FACE ( 'NONE', ( #53396 ), #216309, .T. ) ;
#117278 = CARTESIAN_POINT ( 'NONE',  ( -14.11697426661281085, 66.54258905524443435, -88.02302351073434750 ) ) ;
#117277 = DIRECTION ( 'NONE',  ( 0.000000000000000000, -0.000000000000000000, 1.000000000000000000 ) ) ;
#117279 = CARTESIAN_POINT ( 'NONE',  ( 23.14999999999999858, 7.128833340094563376, -233.7327013124401276 ) ) ;
#117280 = EDGE_LOOP ( 'NONE', ( #112723, #10449, #205318, #166966 ) ) ;
#117281 = CARTESIAN_POINT ( 'NONE',  ( 20.94999999999999929, 78.48087866980282001, -232.8271061603568910 ) ) ;
#117282 = EDGE_LOOP ( 'NONE', ( #114628, #191613, #8337, #248704 ) ) ;
#117283 = EDGE_LOOP ( 'NONE', ( #40039, #169700, #69244, #222197 ) ) ;
#117284 = DIRECTION ( 'NONE',  ( 0.000000000000000000, -6.982962677686266711E-15, 1.000000000000000000 ) ) ;
#117285 = CARTESIAN_POINT ( 'NONE',  ( -22.45372860728439690, 0.01492061955964464268, -88.85020286529615419 ) ) ;
#117286 = DIRECTION ( 'NONE',  ( 1.020425574104004196E-15, 6.982962677686266711E-15, -1.000000000000000000 ) ) ;
#117287 = CARTESIAN_POINT ( 'NONE',  ( 22.00411653889218400, 75.90096189422571626, -210.7765503521648327 ) ) ;
#117288 = CIRCLE ( 'NONE', #4819, 0.2000000000000048683 ) ;
#117289 = DIRECTION ( 'NONE',  ( 0.000000000000000000, -7.086529944415893080E-15, 1.000000000000000000 ) ) ;
#117290 = ORIENTED_EDGE ( 'NONE', *, *, #174597, .F. ) ;
#117291 = ORIENTED_EDGE ( 'NONE', *, *, #55797, .F. ) ;
#117292 = DIRECTION ( 'NONE',  ( -1.000000000000000000, 0.000000000000000000, -0.000000000000000000 ) ) ;
#117293 = CARTESIAN_POINT ( 'NONE',  ( -20.54999999999999716, 71.65000000001154490, -52.77310748452435263 ) ) ;
#117294 = ORIENTED_EDGE ( 'NONE', *, *, #235106, .F. ) ;
#117295 = CARTESIAN_POINT ( 'NONE',  ( -17.01764560440512852, 23.06621698446732083, -230.9822826984797359 ) ) ;
#117296 = CARTESIAN_POINT ( 'NONE',  ( -21.05000000000000071, 67.23127455305835554, -235.8551265064784559 ) ) ;
#117297 = CARTESIAN_POINT ( 'NONE',  ( -23.25000000000000000, 1.115650265596050101E-11, -62.95000000000004547 ) ) ;
#117298 = FACE_OUTER_BOUND ( 'NONE', #12547, .T. ) ;
#117299 = AXIS2_PLACEMENT_3D ( 'NONE', #239372, #58135, #138943 ) ;
#117301 = EDGE_CURVE ( 'NONE', #218857, #62106, #201718, .T. ) ;
#117300 = PLANE ( 'NONE',  #150053 ) ;
#117303 = DIRECTION ( 'NONE',  ( -1.000000000000000000, 0.000000000000000000, 0.000000000000000000 ) ) ;
#117302 = CARTESIAN_POINT ( 'NONE',  ( -22.39999999999999858, 0.000000000000000000, 11.64957080754479968 ) ) ;
#117304 = DIRECTION ( 'NONE',  ( -1.000000000000000000, 0.000000000000000000, -0.000000000000000000 ) ) ;
#117305 = CARTESIAN_POINT ( 'NONE',  ( -20.65000000000000568, 68.75000000001232081, -157.3731074845244109 ) ) ;
#117306 = FACE_OUTER_BOUND ( 'NONE', #105222, .T. ) ;
#117307 = CARTESIAN_POINT ( 'NONE',  ( 21.08884785362045378, 69.64280663258743687, -203.5728905795912453 ) ) ;
#117309 = EDGE_LOOP ( 'NONE', ( #831, #177838, #42123, #241457 ) ) ;
#117308 = DIRECTION ( 'NONE',  ( 1.000000000000000000, -0.000000000000000000, -0.000000000000000000 ) ) ;
#117310 = EDGE_CURVE ( 'NONE', #134771, #74886, #122640, .T. ) ;
#117311 = CIRCLE ( 'NONE', #104786, 0.5999999999999998668 ) ;
#117312 = CARTESIAN_POINT ( 'NONE',  ( 21.00000000000000000, 9.750000000011153745, -188.6499999999999488 ) ) ;
#117313 = ORIENTED_EDGE ( 'NONE', *, *, #92026, .T. ) ;
#117314 = EDGE_CURVE ( 'NONE', #246557, #96104, #175940, .T. ) ;
#117315 = DIRECTION ( 'NONE',  ( 1.000000000000000000, 0.000000000000000000, 0.000000000000000000 ) ) ;
#117316 = CARTESIAN_POINT ( 'NONE',  ( 23.24999999999999645, 20.42498087366621817, -235.1829032864613396 ) ) ;
#117317 = ORIENTED_EDGE ( 'NONE', *, *, #3683, .F. ) ;
#117318 = CARTESIAN_POINT ( 'NONE',  ( -21.05000000000000071, 47.95459712139159336, -246.5019368548292675 ) ) ;
#117319 = EDGE_CURVE ( 'NONE', #98456, #88017, #173397, .T. ) ;
#117320 = DIRECTION ( 'NONE',  ( 0.000000000000000000, 7.086529944415886769E-15, -1.000000000000000000 ) ) ;
#117321 = AXIS2_PLACEMENT_3D ( 'NONE', #126605, #208729, #225672 ) ;
#117322 = AXIS2_PLACEMENT_3D ( 'NONE', #98276, #177876, #26504 ) ;
#117323 = FACE_OUTER_BOUND ( 'NONE', #87263, .T. ) ;
#117324 = FACE_OUTER_BOUND ( 'NONE', #21412, .T. ) ;
#117325 = CARTESIAN_POINT ( 'NONE',  ( -23.25000000000000000, 64.35000000001222986, -148.7731074845244450 ) ) ;
#117326 = B_SPLINE_CURVE_WITH_KNOTS ( 'NONE', 3,
 ( #142131, #122591, #202114, #23511, #97838, #102990, #177444, #256896, #157899, #58717, #138260, #126419, #204660, #186416, #205957, #188968, #109412, #222942, #10345 ),
 .UNSPECIFIED., .F., .F.,
 ( 4, 3, 3, 3, 3, 3, 4 ),
 ( 0.000000000000000000, 1.655171619026035414E-05, 2.773500582848518044E-05, 5.941817267378563579E-05, 0.0001114174635873545742, 0.0001914169455916377854, 0.0002627181070750677803 ),
 .UNSPECIFIED. ) ;
#117327 = VERTEX_POINT ( 'NONE', #172104 ) ;
#117328 = DIRECTION ( 'NONE',  ( -1.000000000000000000, -0.000000000000000000, -0.000000000000000000 ) ) ;
#117330 = ORIENTED_EDGE ( 'NONE', *, *, #91509, .T. ) ;
#117329 = CARTESIAN_POINT ( 'NONE',  ( 21.14999999999999858, 34.07612324756792077, -243.5412266404783566 ) ) ;
#117331 = CARTESIAN_POINT ( 'NONE',  ( 19.75857864376268935, 64.35000000001177511, -78.27310748452438816 ) ) ;
#117332 = EDGE_CURVE ( 'NONE', #195092, #69727, #256677, .T. ) ;
#117333 = CARTESIAN_POINT ( 'NONE',  ( -16.81744102076748959, 9.950000000011138823, -188.3499999999999659 ) ) ;
#117334 = CARTESIAN_POINT ( 'NONE',  ( -21.05000000000000071, 74.25000000001205080, -124.8535959266226598 ) ) ;
#117335 = B_SPLINE_CURVE_WITH_KNOTS ( 'NONE', 3,
 ( #199565, #78290, #100410, #155309, #56154, #17071, #96560, #77013, #156600, #236091 ),
 .UNSPECIFIED., .F., .F.,
 ( 4, 3, 3, 4 ),
 ( 7.632826238677508298E-06, 4.756916949875313879E-05, 9.484459048148540536E-05, 0.0001435500935099941200 ),
 .UNSPECIFIED. ) ;
#117336 = ORIENTED_EDGE ( 'NONE', *, *, #171881, .T. ) ;
#117337 = CARTESIAN_POINT ( 'NONE',  ( 23.25000000000000000, 62.12679871018153932, -248.6611778639222337 ) ) ;
#117338 = EDGE_CURVE ( 'NONE', #112707, #138031, #86677, .T. ) ;
#117339 = APPLICATION_PROTOCOL_DEFINITION ( 'draft international standard', 'automotive_design', 1998, #32618 ) ;
#117340 = EDGE_CURVE ( 'NONE', #19019, #14729, #230976, .T. ) ;
#117341 = DIRECTION ( 'NONE',  ( 1.000000000000000000, 0.000000000000000000, -0.000000000000000000 ) ) ;
#117342 = CIRCLE ( 'NONE', #92377, 2.600000000000001421 ) ;
#117343 = ORIENTED_EDGE ( 'NONE', *, *, #167538, .F. ) ;
#117344 = DIRECTION ( 'NONE',  ( -1.000000000000000000, -0.000000000000000000, -0.000000000000000000 ) ) ;
#117345 = CARTESIAN_POINT ( 'NONE',  ( -23.25000000000000000, 18.60970618848720903, -231.2322896185303875 ) ) ;
#117346 = B_SPLINE_CURVE_WITH_KNOTS ( 'NONE', 3,
 ( #78852, #60580, #158445, #237941 ),
 .UNSPECIFIED., .F., .F.,
 ( 4, 4 ),
 ( 0.000000000000000000, 0.001767853679387133359 ),
 .UNSPECIFIED. ) ;
#117347 = ADVANCED_FACE ( 'NONE', ( #78081 ), #43517, .T. ) ;
#117348 = EDGE_LOOP ( 'NONE', ( #89884, #31179, #121059, #49848 ) ) ;
#117349 = EDGE_LOOP ( 'NONE', ( #129004, #161353, #208614, #76639 ) ) ;
#117350 = EDGE_CURVE ( 'NONE', #83634, #176927, #130989, .T. ) ;
#117351 = CARTESIAN_POINT ( 'NONE',  ( 20.90000000000000213, 7.900000000000000355, -1.300000000000000044 ) ) ;
#117352 = EDGE_CURVE ( 'NONE', #198456, #203538, #55936, .T. ) ;
#117353 = CARTESIAN_POINT ( 'NONE',  ( 23.14999999999999503, 6.649999999999999467, -21.15000000000000213 ) ) ;
#117354 = CARTESIAN_POINT ( 'NONE',  ( 20.94999999999999929, 5.000000000011153745, -155.4947339810869380 ) ) ;
#117355 = DIRECTION ( 'NONE',  ( -1.000000000000000000, 0.000000000000000000, 0.000000000000000000 ) ) ;
#117357 = FACE_OUTER_BOUND ( 'NONE', #74719, .T. ) ;
#117356 = VECTOR ( 'NONE', #184114, 1000.000000000000000 ) ;
#117358 = VECTOR ( 'NONE', #222504, 1000.000000000000000 ) ;
#117361 = DIRECTION ( 'NONE',  ( 0.000000000000000000, 6.982962677686266711E-15, -1.000000000000000000 ) ) ;
#117360 = AXIS2_PLACEMENT_3D ( 'NONE', #180531, #91695, #226031 ) ;
#117359 = DIRECTION ( 'NONE',  ( 0.000000000000000000, 0.9126074666063777041, 0.4088369013363265525 ) ) ;
#117362 = CARTESIAN_POINT ( 'NONE',  ( 20.90851465518106167, 65.67467670974367877, -30.45317318268843820 ) ) ;
#117363 = CARTESIAN_POINT ( 'NONE',  ( -16.94275863009466576, 9.989496048673542461, -113.1083026179589126 ) ) ;
#117364 = DIRECTION ( 'NONE',  ( -1.000000000000000000, 0.000000000000000000, 0.000000000000000000 ) ) ;
#117365 = CYLINDRICAL_SURFACE ( 'NONE', #251353, 4.049999999999998046 ) ;
#117366 = ORIENTED_EDGE ( 'NONE', *, *, #15082, .T. ) ;
#117367 = ORIENTED_EDGE ( 'NONE', *, *, #42305, .T. ) ;
#117368 = CARTESIAN_POINT ( 'NONE',  ( -21.59142135623730852, 68.15000000001180069, -81.87310748452436826 ) ) ;
#117369 = DIRECTION ( 'NONE',  ( 0.000000000000000000, -0.9999631594459056361, -0.008583690987124413183 ) ) ;
#117371 = CARTESIAN_POINT ( 'NONE',  ( -20.54999999999999716, -9.499999999988848032, -177.3939691226524076 ) ) ;
#117370 = CARTESIAN_POINT ( 'NONE',  ( 21.07971444708685738, 69.67020791838511684, -69.61093092084226441 ) ) ;
#117372 = ADVANCED_FACE ( 'NONE', ( #33884 ), #121760, .T. ) ;
#117373 = FACE_OUTER_BOUND ( 'NONE', #1303, .T. ) ;
#117375 = ADVANCED_FACE ( 'NONE', ( #83192 ), #2385, .T. ) ;
#117374 = CARTESIAN_POINT ( 'NONE',  ( 21.05000000000005400, 87.75000000001122658, -30.12310748452481235 ) ) ;
#117376 = CARTESIAN_POINT ( 'NONE',  ( -18.59999999999999787, 1.115600667400684642E-11, -175.4000000000000341 ) ) ;
#117377 = EDGE_LOOP ( 'NONE', ( #16796, #254740, #62679 ) ) ;
#117379 = VERTEX_POINT ( 'NONE', #220178 ) ;
#117378 = TOROIDAL_SURFACE ( 'NONE', #13327, 11.65000000000000036, 0.1000000000000000056 ) ;
#117380 = EDGE_CURVE ( 'NONE', #3872, #155298, #121106, .T. ) ;
#117381 = DIRECTION ( 'NONE',  ( 1.000000000000000000, 0.000000000000000000, 0.000000000000000000 ) ) ;
#117382 = EDGE_LOOP ( 'NONE', ( #152733, #123359, #115768, #78348 ) ) ;
#117383 = DIRECTION ( 'NONE',  ( 0.000000000000000000, 0.000000000000000000, -1.000000000000000000 ) ) ;
#117384 = CARTESIAN_POINT ( 'NONE',  ( 18.46932045258645161, 85.67068520027710576, -29.34924711152760324 ) ) ;
#117385 = VERTEX_POINT ( 'NONE', #218869 ) ;
#117386 = CYLINDRICAL_SURFACE ( 'NONE', #126809, 0.09999999999999939493 ) ;
#117387 = VECTOR ( 'NONE', #177522, 1000.000000000000000 ) ;
#117388 = EDGE_LOOP ( 'NONE', ( #215046, #131635, #186744, #35091, #56769, #62732, #69091, #181909, #133846, #173152, #77051, #42397, #239320, #8618, #23569, #130652, #31762 ) ) ;
#117389 = LINE ( 'NONE', #136948, #82607 ) ;
#117391 = VECTOR ( 'NONE', #180155, 1000.000000000000000 ) ;
#117390 = FACE_OUTER_BOUND ( 'NONE', #12643, .T. ) ;
#117392 = ADVANCED_FACE ( 'NONE', ( #242291 ), #24562, .T. ) ;
#117393 = DIRECTION ( 'NONE',  ( 0.000000000000000000, 0.000000000000000000, -1.000000000000000000 ) ) ;
#117394 = CARTESIAN_POINT ( 'NONE',  ( 21.04999999999940741, 65.54469922025401729, -242.1294324713720698 ) ) ;
#117396 = DIRECTION ( 'NONE',  ( -0.000000000000000000, 0.1350103645451974088, -0.9908441862701587999 ) ) ;
#117395 = PLANE ( 'NONE',  #137506 ) ;
#117398 = DIRECTION ( 'NONE',  ( 0.000000000000000000, 1.224646799147316229E-16, 1.000000000000000000 ) ) ;
#117397 = AXIS2_PLACEMENT_3D ( 'NONE', #30130, #92637, #173527 ) ;
#117399 = ADVANCED_FACE ( 'NONE', ( #38985, #4940 ), #63657, .F. ) ;
#117400 = VERTEX_POINT ( 'NONE', #243583 ) ;
#117402 = CARTESIAN_POINT ( 'NONE',  ( 18.59999999999999076, 46.01276039807270024, -256.6622985126337539 ) ) ;
#117401 = CARTESIAN_POINT ( 'NONE',  ( 18.54999999999999716, 8.750000000011173285, -46.15000000000000568 ) ) ;
#117403 = ORIENTED_EDGE ( 'NONE', *, *, #40124, .T. ) ;
#117405 = EDGE_LOOP ( 'NONE', ( #203056, #136004, #105980, #85295, #215854, #256172 ) ) ;
#117404 = DIRECTION ( 'NONE',  ( 1.000000000000000000, 0.000000000000000000, 0.000000000000000000 ) ) ;
#117406 = ORIENTED_EDGE ( 'NONE', *, *, #127185, .T. ) ;
#117407 = DIRECTION ( 'NONE',  ( 1.000000000000000000, 0.000000000000000000, 0.000000000000000000 ) ) ;
#117408 = TOROIDAL_SURFACE ( 'NONE', #4933, 11.65000000000000036, 0.1000000000000000056 ) ;
#117409 = CARTESIAN_POINT ( 'NONE',  ( -16.87683809663752399, 50.04486772930183491, -218.0870470535037100 ) ) ;
#117410 = CARTESIAN_POINT ( 'NONE',  ( 21.14999999999999503, 87.65000000001202807, -114.7731074845242318 ) ) ;
#117411 = EDGE_CURVE ( 'NONE', #28188, #186764, #239323, .T. ) ;
#117412 = CARTESIAN_POINT ( 'NONE',  ( 21.05000000000000071, 71.18691588786253988, -124.5815897280005089 ) ) ;
#117413 = AXIS2_PLACEMENT_3D ( 'NONE', #217374, #195293, #156166 ) ;
#117414 = ORIENTED_EDGE ( 'NONE', *, *, #243758, .T. ) ;
#117415 = ADVANCED_FACE ( 'NONE', ( #1094 ), #81085, .F. ) ;
#117416 = DIRECTION ( 'NONE',  ( 0.000000000000000000, -1.776356839400250465E-15, -1.000000000000000000 ) ) ;
#117417 = CARTESIAN_POINT ( 'NONE',  ( 20.12500000000000000, 9.750000000011153745, -88.25000000000005684 ) ) ;
#117418 = CARTESIAN_POINT ( 'NONE',  ( 20.94999999999999929, 76.00000000001190870, -103.0231074845243029 ) ) ;
#117419 = ADVANCED_FACE ( 'NONE', ( #40289 ), #110137, .T. ) ;
#117420 = ORIENTED_EDGE ( 'NONE', *, *, #83520, .T. ) ;
#117421 = DIRECTION ( 'NONE',  ( 0.000000000000000000, 0.8814952561688437216, -0.4721928772777334582 ) ) ;
#117422 = AXIS2_PLACEMENT_3D ( 'NONE', #99621, #179220, #202608 ) ;
#117423 = CARTESIAN_POINT ( 'NONE',  ( 21.08035267497491105, 6.331706839783013407, 0.08268862477613450612 ) ) ;
#117424 = CIRCLE ( 'NONE', #225720, 3.999999999999996447 ) ;
#117425 = EDGE_LOOP ( 'NONE', ( #153166, #158289, #213704, #136561 ) ) ;
#117426 = ORIENTED_EDGE ( 'NONE', *, *, #26353, .F. ) ;
#117427 = LINE ( 'NONE', #17059, #185406 ) ;
#117428 = AXIS2_PLACEMENT_3D ( 'NONE', #243484, #64843, #124837 ) ;
#117429 = EDGE_CURVE ( 'NONE', #134704, #234500, #181081, .T. ) ;
#117430 = ORIENTED_EDGE ( 'NONE', *, *, #74826, .T. ) ;
#117431 = CARTESIAN_POINT ( 'NONE',  ( 18.54999999999999716, 8.750000000011182166, -54.35000000000000142 ) ) ;
#117433 = EDGE_CURVE ( 'NONE', #110939, #6455, #168468, .T. ) ;
#117432 = ORIENTED_EDGE ( 'NONE', *, *, #106220, .T. ) ;
#117434 = DIRECTION ( 'NONE',  ( 1.000000000000000000, 0.000000000000000000, 0.000000000000000000 ) ) ;
#117435 = AXIS2_PLACEMENT_3D ( 'NONE', #231835, #188836, #227969 ) ;
#117436 = FACE_OUTER_BOUND ( 'NONE', #217604, .T. ) ;
#117437 = CARTESIAN_POINT ( 'NONE',  ( 20.95263205890701030, 60.86783962820125993, -225.3331190451696955 ) ) ;
#117438 = ADVANCED_FACE ( 'NONE', ( #21988 ), #101921, .T. ) ;
#117439 = CIRCLE ( 'NONE', #184240, 0.2000000000000057288 ) ;
#117440 = CARTESIAN_POINT ( 'NONE',  ( 20.94999999999999574, -11.48912529306490349, -103.6000000000000369 ) ) ;
#117441 = CARTESIAN_POINT ( 'NONE',  ( -23.25000000000000000, 84.59626168225530307, -160.5729799673740104 ) ) ;
#117442 = CARTESIAN_POINT ( 'NONE',  ( 18.69999999999998153, 1.311673547813416718, -7.986648289447971116 ) ) ;
#117443 = CYLINDRICAL_SURFACE ( 'NONE', #80868, 0.09999999999999438505 ) ;
#117444 = VECTOR ( 'NONE', #111326, 1000.000000000000114 ) ;
#117446 = EDGE_LOOP ( 'NONE', ( #15961, #16204, #169075, #194156 ) ) ;
#117445 = EDGE_CURVE ( 'NONE', #68890, #139380, #62386, .T. ) ;
#117449 = EDGE_CURVE ( 'NONE', #233797, #139650, #68639, .T. ) ;
#117448 = CARTESIAN_POINT ( 'NONE',  ( -21.93642651522410247, 7.327166239336959208, -33.50000000000000000 ) ) ;
#117447 = CARTESIAN_POINT ( 'NONE',  ( -23.15000000000000213, 5.900000000011162093, -157.2809002353436654 ) ) ;
#117450 = AXIS2_PLACEMENT_3D ( 'NONE', #66353, #110608, #166769 ) ;
#117451 = ORIENTED_EDGE ( 'NONE', *, *, #87049, .T. ) ;
#117454 = ORIENTED_EDGE ( 'NONE', *, *, #102668, .F. ) ;
#117453 = LINE ( 'NONE', #178740, #8744 ) ;
#117452 = DIRECTION ( 'NONE',  ( 0.000000000000000000, -0.2617529984165152257, -0.9651348961777124202 ) ) ;
#117455 = AXIS2_PLACEMENT_3D ( 'NONE', #22807, #81432, #83980 ) ;
#117456 = ORIENTED_EDGE ( 'NONE', *, *, #142338, .F. ) ;
#117457 = FACE_OUTER_BOUND ( 'NONE', #148145, .T. ) ;
#117458 = AXIS2_PLACEMENT_3D ( 'NONE', #123712, #188805, #164125 ) ;
#117459 = DIRECTION ( 'NONE',  ( 1.000000000000000000, 0.000000000000000000, 0.000000000000000000 ) ) ;
#117460 = FACE_OUTER_BOUND ( 'NONE', #40182, .T. ) ;
#117461 = ADVANCED_FACE ( 'NONE', ( #147033 ), #247696, .T. ) ;
#117462 = CARTESIAN_POINT ( 'NONE',  ( 21.05000000000000071, 86.58125133469154378, -209.3975964148341973 ) ) ;
#117463 = VERTEX_POINT ( 'NONE', #165338 ) ;
#117464 = DIRECTION ( 'NONE',  ( 0.000000000000000000, 0.000000000000000000, -1.000000000000000000 ) ) ;
#117465 = DIRECTION ( 'NONE',  ( -1.000000000000000000, 0.000000000000000000, 0.000000000000000000 ) ) ;
#117466 = ADVANCED_FACE ( 'NONE', ( #127491 ), #10113, .F. ) ;
#117468 = CARTESIAN_POINT ( 'NONE',  ( 15.74999999999999645, 9.850000000011137402, -150.7500000000000284 ) ) ;
#117467 = DIRECTION ( 'NONE',  ( 0.000000000000000000, 0.4088369013363281623, -0.9126074666063771490 ) ) ;
#117469 = EDGE_CURVE ( 'NONE', #123238, #205753, #251795, .T. ) ;
#117471 = VERTEX_POINT ( 'NONE', #66237 ) ;
#117470 = CARTESIAN_POINT ( 'NONE',  ( -16.94333152882355975, 9.990342011468824168, -54.39203153110149458 ) ) ;
#117472 = VERTEX_POINT ( 'NONE', #45382 ) ;
#117473 = B_SPLINE_CURVE_WITH_KNOTS ( 'NONE', 3,
 ( #194923, #18825, #138735, #237878, #98322, #177922, #78781, #243004 ),
 .UNSPECIFIED., .F., .F.,
 ( 4, 2, 2, 4 ),
 ( 0.000000000000000000, 0.0001306511400390957911, 0.0001959767100586836666, 0.0002613022800782715421 ),
 .UNSPECIFIED. ) ;
#117474 = AXIS2_PLACEMENT_3D ( 'NONE', #64026, #223090, #44477 ) ;
#117475 = CARTESIAN_POINT ( 'NONE',  ( 18.49999999999999645, 74.27191306321776665, -149.6386724793565577 ) ) ;
#117476 = ORIENTED_EDGE ( 'NONE', *, *, #200262, .F. ) ;
#117477 = SPHERICAL_SURFACE ( 'NONE', #201614, 0.1000000000000000056 ) ;
#117478 = ORIENTED_EDGE ( 'NONE', *, *, #145611, .T. ) ;
#117479 = CARTESIAN_POINT ( 'NONE',  ( -18.50000000000000000, -1.135018845899022466, -208.7169768834322952 ) ) ;
#117481 = EDGE_CURVE ( 'NONE', #129778, #170331, #206008, .T. ) ;
#117480 = CARTESIAN_POINT ( 'NONE',  ( 20.94999999999999929, 7.128833340094563376, -233.7327013124401276 ) ) ;
#117482 = CARTESIAN_POINT ( 'NONE',  ( -18.59999999999999787, 11.65000000001115232, -79.15000000000003411 ) ) ;
#117483 = ORIENTED_EDGE ( 'NONE', *, *, #209091, .F. ) ;
#117484 = DIRECTION ( 'NONE',  ( -1.000000000000000000, -0.000000000000000000, 0.000000000000000000 ) ) ;
#117485 = EDGE_CURVE ( 'NONE', #239872, #104152, #67509, .T. ) ;
#117486 = DIRECTION ( 'NONE',  ( -1.000000000000000000, 0.000000000000000000, 0.000000000000000000 ) ) ;
#117488 = ORIENTED_EDGE ( 'NONE', *, *, #190780, .F. ) ;
#117487 = VECTOR ( 'NONE', #33997, 1000.000000000000000 ) ;
#117489 = ORIENTED_EDGE ( 'NONE', *, *, #167132, .F. ) ;
#117490 = CARTESIAN_POINT ( 'NONE',  ( -16.92925196614876171, 9.972331796421276096, -146.6167448477168023 ) ) ;
#117491 = ORIENTED_EDGE ( 'NONE', *, *, #69359, .T. ) ;
#117492 = EDGE_CURVE ( 'NONE', #243170, #162196, #225278, .T. ) ;
#117493 = ORIENTED_EDGE ( 'NONE', *, *, #156037, .T. ) ;
#117495 = VERTEX_POINT ( 'NONE', #68813 ) ;
#117494 = CARTESIAN_POINT ( 'NONE',  ( -23.25000000000000000, 1.115649040949250830E-11, -163.6000000000000512 ) ) ;
#117496 =( REPRESENTATION_RELATIONSHIP ('NONE','NONE', #36900, #198303 ) REPRESENTATION_RELATIONSHIP_WITH_TRANSFORMATION ( #229283 )SHAPE_REPRESENTATION_RELATIONSHIP( ) );
#117497 = EDGE_LOOP ( 'NONE', ( #23901, #105523, #105436, #137608 ) ) ;
#117500 = ORIENTED_EDGE ( 'NONE', *, *, #199516, .T. ) ;
#117499 = ORIENTED_EDGE ( 'NONE', *, *, #136756, .F. ) ;
#117498 = CARTESIAN_POINT ( 'NONE',  ( -20.94999999999999929, 7.021664781911246322, -137.6335654018973287 ) ) ;
#117501 = ORIENTED_EDGE ( 'NONE', *, *, #125992, .F. ) ;
#117502 = CARTESIAN_POINT ( 'NONE',  ( -23.15000000000000213, 52.91185528119410009, -244.1460391050142960 ) ) ;
#117503 = EDGE_CURVE ( 'NONE', #236918, #111107, #172733, .T. ) ;
#117504 = DIRECTION ( 'NONE',  ( -1.000000000000000000, -0.000000000000000000, 0.000000000000000000 ) ) ;
#117505 = CIRCLE ( 'NONE', #150817, 4.049999999999998046 ) ;
#117506 = DIRECTION ( 'NONE',  ( -0.000000000000000000, -6.982962677686266711E-15, 1.000000000000000000 ) ) ;
#117507 = ORIENTED_EDGE ( 'NONE', *, *, #204317, .F. ) ;
#117508 = LINE ( 'NONE', #83478, #166316 ) ;
#117510 = ORIENTED_EDGE ( 'NONE', *, *, #68582, .T. ) ;
#117509 = DIRECTION ( 'NONE',  ( 1.000000000000000000, 0.000000000000000000, 0.000000000000000000 ) ) ;
#117511 = DIRECTION ( 'NONE',  ( -1.000000000000000000, 0.000000000000000000, 0.000000000000000000 ) ) ;
#117513 = ORIENTED_EDGE ( 'NONE', *, *, #94114, .F. ) ;
#117512 = DIRECTION ( 'NONE',  ( 0.000000000000000000, -0.4999999999999088507, 0.8660254037844913322 ) ) ;
#117514 = ORIENTED_EDGE ( 'NONE', *, *, #164212, .F. ) ;
#117515 = CARTESIAN_POINT ( 'NONE',  ( 21.53699400384776297, 1.117343393059872131E-11, -160.7122882067608600 ) ) ;
#117516 = CIRCLE ( 'NONE', #146699, 4.149999999999996803 ) ;
#117517 = CIRCLE ( 'NONE', #168021, 0.09999999999998898659 ) ;
#117518 = ORIENTED_EDGE ( 'NONE', *, *, #157447, .T. ) ;
#117519 = VERTEX_POINT ( 'NONE', #105316 ) ;
#117520 = CARTESIAN_POINT ( 'NONE',  ( -22.50000000000000000, 1.115600667400684642E-11, -100.5000000000000284 ) ) ;
#117521 = FACE_OUTER_BOUND ( 'NONE', #235741, .T. ) ;
#117523 = ORIENTED_EDGE ( 'NONE', *, *, #202822, .T. ) ;
#117522 = ORIENTED_EDGE ( 'NONE', *, *, #213593, .T. ) ;
#117524 = ORIENTED_EDGE ( 'NONE', *, *, #254698, .T. ) ;
#117525 = LINE ( 'NONE', #159240, #20119 ) ;
#117526 = ORIENTED_EDGE ( 'NONE', *, *, #64702, .T. ) ;
#117527 = EDGE_LOOP ( 'NONE', ( #129456, #173868, #204773, #170675 ) ) ;
#117528 = DIRECTION ( 'NONE',  ( -6.938893903907222067E-15, 1.000000000000000000, 0.000000000000000000 ) ) ;
#117529 = EDGE_LOOP ( 'NONE', ( #244089, #19156, #137636, #7383, #113098 ) ) ;
#117530 = DIRECTION ( 'NONE',  ( 1.000000000000000000, -0.000000000000000000, -0.000000000000000000 ) ) ;
#117532 = CARTESIAN_POINT ( 'NONE',  ( -18.50000000000000000, 68.87972903831381188, -32.36354444268503983 ) ) ;
#117531 = LINE ( 'NONE', #197052, #61262 ) ;
#117533 = VERTEX_POINT ( 'NONE', #166652 ) ;
#117534 = AXIS2_PLACEMENT_3D ( 'NONE', #93698, #251481, #127705 ) ;
#117536 = ADVANCED_FACE ( 'NONE', ( #106615 ), #7540, .T. ) ;
#117535 = CIRCLE ( 'NONE', #238329, 0.09999999999999917288 ) ;
#117537 = ORIENTED_EDGE ( 'NONE', *, *, #240009, .F. ) ;
#117538 = AXIS2_PLACEMENT_3D ( 'NONE', #122830, #159386, #42012 ) ;
#117539 = DIRECTION ( 'NONE',  ( -1.000000000000000000, 0.000000000000000000, 0.000000000000000000 ) ) ;
#117540 = ORIENTED_EDGE ( 'NONE', *, *, #155649, .F. ) ;
#117541 = DIRECTION ( 'NONE',  ( 0.000000000000000000, -0.8454177738465953329, -0.5341055959866617409 ) ) ;
#117542 = EDGE_LOOP ( 'NONE', ( #168850, #99901, #63134, #177144 ) ) ;
#117543 = ORIENTED_EDGE ( 'NONE', *, *, #199219, .F. ) ;
#117544 = EDGE_CURVE ( 'NONE', #245081, #33915, #60246, .T. ) ;
#117545 = CARTESIAN_POINT ( 'NONE',  ( 23.24999999999999645, 64.25000000001210765, -127.2731074845243882 ) ) ;
#117546 = ORIENTED_EDGE ( 'NONE', *, *, #170538, .F. ) ;
#117547 = CARTESIAN_POINT ( 'NONE',  ( 18.39999999999999503, 45.89348038176515843, -239.2231437130149061 ) ) ;
#117548 = CARTESIAN_POINT ( 'NONE',  ( 22.39999999999999503, 12.76524917372336887, -223.4223513401831269 ) ) ;
#117549 = VERTEX_POINT ( 'NONE', #27142 ) ;
#117550 = DIRECTION ( 'NONE',  ( -1.000000000000000000, 0.000000000000000000, 0.000000000000000000 ) ) ;
#117551 = AXIS2_PLACEMENT_3D ( 'NONE', #201084, #84953, #82389 ) ;
#117553 = DIRECTION ( 'NONE',  ( -0.000000000000000000, -0.000000000000000000, 1.000000000000000000 ) ) ;
#117552 = DIRECTION ( 'NONE',  ( -3.265361837132813093E-16, -1.000000000000000000, -6.938893903907229955E-15 ) ) ;
#117554 = EDGE_CURVE ( 'NONE', #33224, #254767, #1972, .T. ) ;
#117555 = DIRECTION ( 'NONE',  ( 0.000000000000000000, -1.000000000000000000, -6.982962677686265922E-15 ) ) ;
#117556 = CARTESIAN_POINT ( 'NONE',  ( 23.24999999999999289, 59.16775194334852017, -221.0793150863668473 ) ) ;
#117557 = PLANE ( 'NONE',  #240739 ) ;
#117558 = DIRECTION ( 'NONE',  ( -0.000000000000000000, 1.000000000000000000, -0.000000000000000000 ) ) ;
#117559 = CARTESIAN_POINT ( 'NONE',  ( 18.59999999999998721, 43.27008861172207332, -245.2265230569236110 ) ) ;
#117560 = EDGE_CURVE ( 'NONE', #114401, #215804, #87052, .T. ) ;
#117561 = ORIENTED_EDGE ( 'NONE', *, *, #158461, .F. ) ;
#117562 = CIRCLE ( 'NONE', #122226, 0.1000000000000026007 ) ;
#117563 = EDGE_CURVE ( 'NONE', #189870, #39562, #229232, .T. ) ;
#117565 = ORIENTED_EDGE ( 'NONE', *, *, #134033, .T. ) ;
#117564 = ORIENTED_EDGE ( 'NONE', *, *, #207992, .T. ) ;
#117566 = VERTEX_POINT ( 'NONE', #224009 ) ;
#117567 = VERTEX_POINT ( 'NONE', #246156 ) ;
#117568 = ADVANCED_FACE ( 'NONE', ( #6241 ), #83436, .T. ) ;
#117569 = CARTESIAN_POINT ( 'NONE',  ( -21.14999999999999858, 1.115600667400684642E-11, -93.95934304829879125 ) ) ;
#117570 = AXIS2_PLACEMENT_3D ( 'NONE', #135774, #215322, #17151 ) ;
#117571 = CARTESIAN_POINT ( 'NONE',  ( -23.25000000000000000, 76.00000000001168132, -73.67310748452432279 ) ) ;
#117572 = EDGE_CURVE ( 'NONE', #137421, #121769, #133363, .T. ) ;
#117574 = CARTESIAN_POINT ( 'NONE',  ( 21.00000000000000000, 8.000000000000000000, -1.212568896937008089 ) ) ;
#117573 = DIRECTION ( 'NONE',  ( 1.000000000000000000, -2.952720810173289112E-16, -2.061873921506763405E-30 ) ) ;
#117575 = ORIENTED_EDGE ( 'NONE', *, *, #208898, .T. ) ;
#117576 = AXIS2_PLACEMENT_3D ( 'NONE', #187564, #125010, #204522 ) ;
#117577 = FACE_OUTER_BOUND ( 'NONE', #176186, .T. ) ;
#117578 = SURFACE_SIDE_STYLE ('',( #236238 ) ) ;
#117579 = CARTESIAN_POINT ( 'NONE',  ( 20.27550659511089037, 63.79409916874961795, -213.3197368432687426 ) ) ;
#117581 = EDGE_CURVE ( 'NONE', #257362, #11797, #245780, .T. ) ;
#117580 = CIRCLE ( 'NONE', #79941, 0.09999999999999438505 ) ;
#117582 = CARTESIAN_POINT ( 'NONE',  ( 20.94999999999999929, -8.730841121484171907, -177.0980747189843214 ) ) ;
#117583 = VECTOR ( 'NONE', #59917, 1000.000000000000000 ) ;
#117584 = AXIS2_PLACEMENT_3D ( 'NONE', #118831, #60105, #19727 ) ;
#117585 = LINE ( 'NONE', #19785, #45580 ) ;
#117586 = ORIENTED_EDGE ( 'NONE', *, *, #233623, .T. ) ;
#117587 = CARTESIAN_POINT ( 'NONE',  ( -21.65000000000000213, 68.29142135624952914, -148.8731074845244109 ) ) ;
#117588 = VECTOR ( 'NONE', #26045, 1000.000000000000000 ) ;
#117589 = VERTEX_POINT ( 'NONE', #51779 ) ;
#117590 = DIRECTION ( 'NONE',  ( -1.000000000000000000, -0.000000000000000000, -0.000000000000000000 ) ) ;
#117591 = CARTESIAN_POINT ( 'NONE',  ( 23.24999999999999645, 5.600000000011153389, -179.9052660189130677 ) ) ;
#117592 = CARTESIAN_POINT ( 'NONE',  ( -16.94445028196807002, 9.992063609708893068, -121.3926698215815918 ) ) ;
#117593 = DIRECTION ( 'NONE',  ( -0.000000000000000000, -6.982962677686266711E-15, 1.000000000000000000 ) ) ;
#117595 = VECTOR ( 'NONE', #191073, 1000.000000000000000 ) ;
#117594 = CYLINDRICAL_SURFACE ( 'NONE', #62650, 12.87500000000000178 ) ;
#117596 = ORIENTED_EDGE ( 'NONE', *, *, #97905, .F. ) ;
#117597 = CARTESIAN_POINT ( 'NONE',  ( -22.19999999999999929, -11.75000000000000178, 12.09999999999999609 ) ) ;
#117599 = EDGE_CURVE ( 'NONE', #102921, #213545, #114347, .T. ) ;
#117598 = DIRECTION ( 'NONE',  ( -1.000000000000000000, 0.000000000000000000, 0.000000000000000000 ) ) ;
#117600 = TOROIDAL_SURFACE ( 'NONE', #234108, 1.900000000000002576, 0.1000000000000000056 ) ;
#117602 = DIRECTION ( 'NONE',  ( 0.000000000000000000, 0.000000000000000000, 1.000000000000000000 ) ) ;
#117601 = DIRECTION ( 'NONE',  ( 0.000000000000000000, 0.000000000000000000, -1.000000000000000000 ) ) ;
#117603 = CARTESIAN_POINT ( 'NONE',  ( 18.59999999999999076, 7.070967871809997973, -204.7465642218682547 ) ) ;
#117605 = CARTESIAN_POINT ( 'NONE',  ( -16.94052228080551359, 9.986279733109993728, -121.3903755026694569 ) ) ;
#117604 = VECTOR ( 'NONE', #43678, 1000.000000000000000 ) ;
#117606 = AXIS2_PLACEMENT_3D ( 'NONE', #257984, #117251, #19435 ) ;
#117607 = DIRECTION ( 'NONE',  ( 1.000000000000000000, 0.000000000000000000, 0.000000000000000000 ) ) ;
#117608 = CARTESIAN_POINT ( 'NONE',  ( 22.47110162079220785, 75.97120258720933350, -114.6730434212086465 ) ) ;
#117609 = CIRCLE ( 'NONE', #146613, 0.1000000000000043771 ) ;
#117610 = ORIENTED_EDGE ( 'NONE', *, *, #219697, .F. ) ;
#117611 = TOROIDAL_SURFACE ( 'NONE', #5148, 12.97499999999999787, 0.1000000000000000056 ) ;
#117612 = AXIS2_PLACEMENT_3D ( 'NONE', #180837, #223789, #222493 ) ;
#117613 = ORIENTED_EDGE ( 'NONE', *, *, #133033, .T. ) ;
#117614 = EDGE_CURVE ( 'NONE', #113549, #31606, #37700, .T. ) ;
#117615 = FACE_OUTER_BOUND ( 'NONE', #197759, .T. ) ;
#117616 = ORIENTED_EDGE ( 'NONE', *, *, #8448, .F. ) ;
#117617 = AXIS2_PLACEMENT_3D ( 'NONE', #91894, #88020, #247108 ) ;
#117618 = LINE ( 'NONE', #197141, #247029 ) ;
#117619 = DIRECTION ( 'NONE',  ( -0.000000000000000000, 0.8660254037844502539, 0.4999999999999799050 ) ) ;
#117620 = DIRECTION ( 'NONE',  ( 1.000000000000000000, 0.000000000000000000, 0.000000000000000000 ) ) ;
#117621 = VECTOR ( 'NONE', #228971, 1000.000000000000000 ) ;
#117622 = ORIENTED_EDGE ( 'NONE', *, *, #201271, .F. ) ;
#117623 = ADVANCED_FACE ( 'NONE', ( #175614 ), #230441, .F. ) ;
#117625 = CARTESIAN_POINT ( 'NONE',  ( -20.64999999999999858, 1.115600667400684642E-11, -167.5000000000000284 ) ) ;
#117624 = AXIS2_PLACEMENT_3D ( 'NONE', #24314, #106373, #185931 ) ;
#117626 = CARTESIAN_POINT ( 'NONE',  ( -15.66061380678752180, 9.360723793997191677, -50.81392719460674101 ) ) ;
#117627 = CARTESIAN_POINT ( 'NONE',  ( -18.51024323315077424, 65.68895814178239334, -97.50265578621379348 ) ) ;
#117628 = CARTESIAN_POINT ( 'NONE',  ( -21.14999999999994174, 64.35000000001120668, -3.123107484524795474 ) ) ;
#117630 = ORIENTED_EDGE ( 'NONE', *, *, #201740, .F. ) ;
#117629 = DIRECTION ( 'NONE',  ( 0.000000000000000000, 0.01562499999998609446, -0.9998779222360101304 ) ) ;
#117632 = DIRECTION ( 'NONE',  ( -1.000000000000000000, -0.000000000000000000, -0.000000000000000000 ) ) ;
#117631 = CARTESIAN_POINT ( 'NONE',  ( -16.77683809663752257, 52.34166666667870516, -119.7731074845244592 ) ) ;
#117633 = LINE ( 'NONE', #160643, #161184 ) ;
#117634 = EDGE_CURVE ( 'NONE', #109854, #192518, #4334, .T. ) ;
#117635 = CARTESIAN_POINT ( 'NONE',  ( -21.59142135623730852, 7.850000000000003197, -12.34999999999999964 ) ) ;
#117636 = CARTESIAN_POINT ( 'NONE',  ( 18.39999999999999858, 87.08727414655710675, -199.6327537731849873 ) ) ;
#117637 = FACE_OUTER_BOUND ( 'NONE', #10308, .T. ) ;
#117638 = ORIENTED_EDGE ( 'NONE', *, *, #59960, .F. ) ;
#117639 = ADVANCED_FACE ( 'NONE', ( #150903 ), #53079, .T. ) ;
#117640 = CARTESIAN_POINT ( 'NONE',  ( 0.000000000000000000, 0.000000000000000000, 0.000000000000000000 ) ) ;
#117641 = CARTESIAN_POINT ( 'NONE',  ( 23.14999999999999503, 11.65000000001116298, -155.7499999999999716 ) ) ;
#117642 = EDGE_CURVE ( 'NONE', #68090, #22326, #60051, .T. ) ;
#117643 = ORIENTED_EDGE ( 'NONE', *, *, #18492, .F. ) ;
#117644 = CARTESIAN_POINT ( 'NONE',  ( -16.88853107394619357, 66.04912151666556497, -182.6701711376321953 ) ) ;
#117645 = AXIS2_PLACEMENT_3D ( 'NONE', #57274, #175990, #216366 ) ;
#117646 = VERTEX_POINT ( 'NONE', #255075 ) ;
#117647 = DIRECTION ( 'NONE',  ( 0.000000000000000000, 0.2128009952263403282, -0.9770955615653358350 ) ) ;
#117648 = ADVANCED_FACE ( 'NONE', ( #173084 ), #233030, .T. ) ;
#117649 = CIRCLE ( 'NONE', #126007, 0.09999999999999939493 ) ;
#117650 = DIRECTION ( 'NONE',  ( -1.000000000000000000, 0.000000000000000000, 0.000000000000000000 ) ) ;
#117651 = CARTESIAN_POINT ( 'NONE',  ( -20.85000000000000142, 14.61354176542825201, -235.9279552357344016 ) ) ;
#117652 = VERTEX_POINT ( 'NONE', #235558 ) ;
#117653 = ORIENTED_EDGE ( 'NONE', *, *, #6057, .F. ) ;
#117654 = CARTESIAN_POINT ( 'NONE',  ( -20.85000000000000142, 1.115600667400684642E-11, -167.5000000000000284 ) ) ;
#117655 = DIRECTION ( 'NONE',  ( 0.000000000000000000, 0.000000000000000000, 1.000000000000000000 ) ) ;
#117656 = DIRECTION ( 'NONE',  ( -0.000000000000000000, 0.000000000000000000, 1.000000000000000000 ) ) ;
#117657 = DIRECTION ( 'NONE',  ( 1.000000000000000000, 1.186688945009010077E-16, 0.000000000000000000 ) ) ;
#117659 = DIRECTION ( 'NONE',  ( 0.000000000000000000, 1.000000000000000000, 6.982962677686266711E-15 ) ) ;
#117658 = DIRECTION ( 'NONE',  ( 0.000000000000000000, -1.000000000000000000, 0.000000000000000000 ) ) ;
#117660 = DIRECTION ( 'NONE',  ( -1.000000000000000000, -2.952720810173289112E-16, 0.000000000000000000 ) ) ;
#117661 = CARTESIAN_POINT ( 'NONE',  ( 21.08804281139606829, 65.37816569817070445, -90.67310751714592243 ) ) ;
#117662 = EDGE_LOOP ( 'NONE', ( #199270, #209312, #245656, #116261, #161813, #234391, #241555, #82497, #242694, #104507 ) ) ;
#117663 = CARTESIAN_POINT ( 'NONE',  ( 21.00000000000000000, 66.25000000001199396, -115.3731074845243683 ) ) ;
#117664 = AXIS2_PLACEMENT_3D ( 'NONE', #13757, #170311, #231533 ) ;
#117666 = ORIENTED_EDGE ( 'NONE', *, *, #154513, .F. ) ;
#117665 = CARTESIAN_POINT ( 'NONE',  ( 22.60000000000000142, 64.25043287652329127, -203.6239658536231332 ) ) ;
#117667 = DIRECTION ( 'NONE',  ( -0.000000000000000000, 1.000000000000000000, 6.982962677686267499E-15 ) ) ;
#117668 = LINE ( 'NONE', #18579, #74172 ) ;
#117670 = DIRECTION ( 'NONE',  ( 1.000000000000000000, 0.000000000000000000, 0.000000000000000000 ) ) ;
#117669 = DIRECTION ( 'NONE',  ( 0.000000000000000000, 0.9126074666064696306, 0.4088369013361213278 ) ) ;
#117671 = EDGE_CURVE ( 'NONE', #236424, #189704, #116909, .T. ) ;
#117672 = EDGE_LOOP ( 'NONE', ( #196338, #90517, #25278, #53818 ) ) ;
#117674 = CARTESIAN_POINT ( 'NONE',  ( -22.94999999999999929, 4.837354856632045057E-16, -3.900000000000000355 ) ) ;
#117673 = DIRECTION ( 'NONE',  ( 1.000000000000000000, 0.000000000000000000, 0.000000000000000000 ) ) ;
#117676 = EDGE_CURVE ( 'NONE', #172714, #185932, #96045, .T. ) ;
#117675 = DIRECTION ( 'NONE',  ( 1.000000000000000000, 0.000000000000000000, -0.000000000000000000 ) ) ;
#117677 = DIRECTION ( 'NONE',  ( 0.000000000000000000, -6.938893903907222067E-15, 1.000000000000000000 ) ) ;
#117678 = CARTESIAN_POINT ( 'NONE',  ( -20.65000000000000568, 63.54522198573874192, -221.7484608313106378 ) ) ;
#117679 = CARTESIAN_POINT ( 'NONE',  ( -18.55121869061588669, 10.32747123227773045, -139.5774032850249569 ) ) ;
#117680 = ORIENTED_EDGE ( 'NONE', *, *, #183341, .T. ) ;
#117681 = DIRECTION ( 'NONE',  ( 1.000000000000000000, 0.000000000000000000, 0.000000000000000000 ) ) ;
#117682 = VERTEX_POINT ( 'NONE', #191346 ) ;
#117683 = ADVANCED_FACE ( 'NONE', ( #196435 ), #20960, .F. ) ;
#117685 = AXIS2_PLACEMENT_3D ( 'NONE', #141694, #223793, #120889 ) ;
#117684 = CARTESIAN_POINT ( 'NONE',  ( 22.45463910399148588, 76.00000000001365663, -215.1726782947082484 ) ) ;
#117686 = EDGE_LOOP ( 'NONE', ( #145553, #58487, #211458, #83200 ) ) ;
#117687 = DIRECTION ( 'NONE',  ( -1.000000000000000000, -0.000000000000000000, 0.000000000000000000 ) ) ;
#117688 = EDGE_LOOP ( 'NONE', ( #147026, #101248, #176432, #158415 ) ) ;
#117689 = CIRCLE ( 'NONE', #192517, 12.77500000000000924 ) ;
#117690 = CARTESIAN_POINT ( 'NONE',  ( 23.14999999999999858, 76.00000000001126921, -203.5231074845248997 ) ) ;
#117691 = AXIS2_PLACEMENT_3D ( 'NONE', #36154, #58249, #234327 ) ;
#117692 = CARTESIAN_POINT ( 'NONE',  ( -18.59999999999999787, 5.950000000011100632, -177.8057023050348278 ) ) ;
#117693 = ORIENTED_EDGE ( 'NONE', *, *, #227044, .T. ) ;
#117694 = CARTESIAN_POINT ( 'NONE',  ( -18.50000000000000000, -9.499999999988849808, -88.75000000000004263 ) ) ;
#117695 = FACE_OUTER_BOUND ( 'NONE', #36056, .T. ) ;
#117696 = AXIS2_PLACEMENT_3D ( 'NONE', #191008, #219519, #139966 ) ;
#117697 = DIRECTION ( 'NONE',  ( 1.000000000000000000, -0.000000000000000000, 0.000000000000000000 ) ) ;
#117698 = AXIS2_PLACEMENT_3D ( 'NONE', #84387, #221365, #64873 ) ;
#117699 = CARTESIAN_POINT ( 'NONE',  ( -20.94999999999999929, 77.83534155023670564, -158.4679561919613491 ) ) ;
#117700 = DIRECTION ( 'NONE',  ( 0.000000000000000000, 0.8814952561688476074, -0.4721928772777262417 ) ) ;
#117701 = DIRECTION ( 'NONE',  ( -1.000000000000000000, -0.000000000000000000, -0.000000000000000000 ) ) ;
#117702 = ADVANCED_FACE ( 'NONE', ( #15260 ), #150127, .F. ) ;
#117703 = ORIENTED_EDGE ( 'NONE', *, *, #220718, .T. ) ;
#117704 = DIRECTION ( 'NONE',  ( 0.000000000000000000, -0.9856811345164803173, -0.1686199900910455851 ) ) ;
#117705 = VERTEX_POINT ( 'NONE', #97306 ) ;
#117707 = VERTEX_POINT ( 'NONE', #212176 ) ;
#117706 = CARTESIAN_POINT ( 'NONE',  ( 21.05281448260627641, 67.22398984147423562, -90.84954957271294518 ) ) ;
#117708 = VERTEX_POINT ( 'NONE', #72678 ) ;
#117709 = CARTESIAN_POINT ( 'NONE',  ( -23.49999999999994316, 76.00000000001119815, -31.97310748452479601 ) ) ;
#117710 = DIRECTION ( 'NONE',  ( 0.000000000000000000, 0.000000000000000000, -1.000000000000000000 ) ) ;
#117711 = DIRECTION ( 'NONE',  ( 0.000000000000000000, 0.000000000000000000, -1.000000000000000000 ) ) ;
#117712 = VECTOR ( 'NONE', #229679, 1000.000000000000000 ) ;
#117713 = FACE_OUTER_BOUND ( 'NONE', #167833, .T. ) ;
#117714 = VERTEX_POINT ( 'NONE', #113062 ) ;
#117715 = ADVANCED_FACE ( 'NONE', ( #192601 ), #13973, .T. ) ;
#117716 = LINE ( 'NONE', #214259, #188940 ) ;
#117717 = DIRECTION ( 'NONE',  ( 1.000000000000000000, 0.000000000000000000, 0.000000000000000000 ) ) ;
#117718 = ORIENTED_EDGE ( 'NONE', *, *, #191812, .T. ) ;
#117719 = VECTOR ( 'NONE', #226335, 1000.000000000000000 ) ;
#117720 = EDGE_CURVE ( 'NONE', #42394, #207660, #129262, .T. ) ;
#117722 = EDGE_LOOP ( 'NONE', ( #194086, #89230, #41614, #238888 ) ) ;
#117721 = DIRECTION ( 'NONE',  ( 0.000000000000000000, 0.000000000000000000, -1.000000000000000000 ) ) ;
#117723 = CIRCLE ( 'NONE', #109321, 0.09999999999998898659 ) ;
#117724 = AXIS2_PLACEMENT_3D ( 'NONE', #37863, #215191, #36596 ) ;
#117725 = DIRECTION ( 'NONE',  ( 0.000000000000000000, -0.9770955615653316162, -0.2128009952263604232 ) ) ;
#117726 = CIRCLE ( 'NONE', #163509, 0.09999999999999990841 ) ;
#117727 = EDGE_CURVE ( 'NONE', #184550, #92142, #195914, .T. ) ;
#117728 = FACE_OUTER_BOUND ( 'NONE', #40269, .T. ) ;
#117729 = EDGE_LOOP ( 'NONE', ( #137136, #190479, #132275, #140600, #14701 ) ) ;
#117730 = EDGE_CURVE ( 'NONE', #150811, #73797, #62632, .T. ) ;
#117731 = SPHERICAL_SURFACE ( 'NONE', #29897, 0.1000000000000000056 ) ;
#117734 = EDGE_CURVE ( 'NONE', #44761, #251678, #256349, .T. ) ;
#117733 = EDGE_CURVE ( 'NONE', #86243, #195513, #158326, .T. ) ;
#117732 = ORIENTED_EDGE ( 'NONE', *, *, #112693, .F. ) ;
#117735 = CARTESIAN_POINT ( 'NONE',  ( 19.99999999999998934, 64.35000000001150511, -48.27310748452440237 ) ) ;
#117736 = CARTESIAN_POINT ( 'NONE',  ( -20.64999999999999858, -8.999999999988846255, -177.3939691226524076 ) ) ;
#117737 = CARTESIAN_POINT ( 'NONE',  ( -22.39999999999999858, 76.00000000001165290, -69.62310748452432563 ) ) ;
#117738 = LINE ( 'NONE', #180287, #238545 ) ;
#117739 = TOROIDAL_SURFACE ( 'NONE', #42723, 12.97499999999999787, 0.1000000000000000056 ) ;
#117740 = AXIS2_PLACEMENT_3D ( 'NONE', #200633, #22004, #141929 ) ;
#117741 = EDGE_CURVE ( 'NONE', #177774, #94125, #159907, .T. ) ;
#117742 = EDGE_CURVE ( 'NONE', #157963, #70299, #166712, .T. ) ;
#117743 = EDGE_LOOP ( 'NONE', ( #62347, #237548, #159751, #3386, #191916 ) ) ;
#117744 = DIRECTION ( 'NONE',  ( -2.940209281316621509E-16, 1.000000000000000000, 1.176083712526648603E-15 ) ) ;
#117745 = ORIENTED_EDGE ( 'NONE', *, *, #117727, .F. ) ;
#117746 = FACE_OUTER_BOUND ( 'NONE', #241927, .T. ) ;
#117747 = EDGE_CURVE ( 'NONE', #70387, #74900, #29338, .T. ) ;
#117748 = CARTESIAN_POINT ( 'NONE',  ( -16.94107738177414291, 10.01423928513661998, -20.94999999999999929 ) ) ;
#117749 = CIRCLE ( 'NONE', #230171, 12.87499999999999822 ) ;
#117750 = ORIENTED_EDGE ( 'NONE', *, *, #251888, .T. ) ;
#117751 = CARTESIAN_POINT ( 'NONE',  ( -23.25000000000000000, 11.65000000001115588, -121.7500000000000426 ) ) ;
#117752 = CYLINDRICAL_SURFACE ( 'NONE', #156189, 0.09999999999999939493 ) ;
#117753 = DIRECTION ( 'NONE',  ( 0.000000000000000000, -6.982962677686267499E-15, 1.000000000000000000 ) ) ;
#117754 = CARTESIAN_POINT ( 'NONE',  ( -16.78493832629887450, 9.945835743215301505, -79.66394901910423698 ) ) ;
#117755 = TOROIDAL_SURFACE ( 'NONE', #176053, 0.2000000000000000111, 0.1000000000000000056 ) ;
#117756 = CARTESIAN_POINT ( 'NONE',  ( -23.25000000000000000, -9.682403433465239573, -107.1568433774128408 ) ) ;
#117758 = EDGE_CURVE ( 'NONE', #245573, #65906, #104294, .T. ) ;
#117757 = CARTESIAN_POINT ( 'NONE',  ( -18.50000000000000355, 85.40000000001207070, -129.2258477248609552 ) ) ;
#117760 = VERTEX_POINT ( 'NONE', #222389 ) ;
#117759 = DIRECTION ( 'NONE',  ( 0.000000000000000000, 0.000000000000000000, -1.000000000000000000 ) ) ;
#117761 = TOROIDAL_SURFACE ( 'NONE', #113483, 0.2000000000000000111, 0.1000000000000000056 ) ;
#117762 = AXIS2_PLACEMENT_3D ( 'NONE', #173396, #92510, #18117 ) ;
#117763 = EDGE_CURVE ( 'NONE', #54282, #171691, #197722, .T. ) ;
#117764 = AXIS2_PLACEMENT_3D ( 'NONE', #75356, #53192, #229277 ) ;
#117765 = CIRCLE ( 'NONE', #151101, 0.1000000000000028644 ) ;
#117766 = CARTESIAN_POINT ( 'NONE',  ( 23.25000000000000000, 11.75000000001116263, -88.35000000000003695 ) ) ;
#117767 = VERTEX_POINT ( 'NONE', #39970 ) ;
#117769 = EDGE_CURVE ( 'NONE', #51680, #231796, #204252, .T. ) ;
#117768 = CARTESIAN_POINT ( 'NONE',  ( -18.47130263965443220, 85.47115558597558049, -62.83970271904723859 ) ) ;
#117770 = CARTESIAN_POINT ( 'NONE',  ( -23.25000000000000000, 68.62136427087769164, -214.1108709299723500 ) ) ;
#117771 = AXIS2_PLACEMENT_3D ( 'NONE', #176640, #175366, #179214 ) ;
#117772 = EDGE_LOOP ( 'NONE', ( #38656, #132050, #182896 ) ) ;
#117773 = DIRECTION ( 'NONE',  ( 0.000000000000000000, 6.308085367182471812E-16, 1.000000000000000000 ) ) ;
#117774 = CIRCLE ( 'NONE', #251033, 0.09999999999999520384 ) ;
#117775 = DIRECTION ( 'NONE',  ( 0.000000000000000000, -1.000000000000000000, 0.000000000000000000 ) ) ;
#117776 = EDGE_CURVE ( 'NONE', #76006, #169429, #99996, .T. ) ;
#117777 = CIRCLE ( 'NONE', #84403, 0.1000000000000121764 ) ;
#117778 = ORIENTED_EDGE ( 'NONE', *, *, #174858, .F. ) ;
#117779 = CARTESIAN_POINT ( 'NONE',  ( 23.14999999999999503, 64.25000000001202238, -114.7731074845243882 ) ) ;
#117780 = AXIS2_PLACEMENT_3D ( 'NONE', #234556, #113328, #72953 ) ;
#117781 = CIRCLE ( 'NONE', #234303, 0.1000000000000000472 ) ;
#117783 = CIRCLE ( 'NONE', #39274, 0.09999999999999854838 ) ;
#117782 = DIRECTION ( 'NONE',  ( -1.000000000000000000, 0.000000000000000000, 0.000000000000000000 ) ) ;
#117784 = ORIENTED_EDGE ( 'NONE', *, *, #214845, .F. ) ;
#117785 = VECTOR ( 'NONE', #86493, 1000.000000000000000 ) ;
#117786 = DIRECTION ( 'NONE',  ( 0.000000000000000000, 0.000000000000000000, 1.000000000000000000 ) ) ;
#117787 = ORIENTED_EDGE ( 'NONE', *, *, #24545, .T. ) ;
#117789 = EDGE_CURVE ( 'NONE', #136769, #129423, #137603, .T. ) ;
#117788 = DIRECTION ( 'NONE',  ( 1.000000000000000000, 0.000000000000000000, 0.000000000000000000 ) ) ;
#117791 = EDGE_LOOP ( 'NONE', ( #51396, #39295, #11696, #192131 ) ) ;
#117790 = DIRECTION ( 'NONE',  ( 1.186688945009010077E-16, -1.000000000000000000, -0.000000000000000000 ) ) ;
#117792 = DIRECTION ( 'NONE',  ( 1.000000000000000000, 0.000000000000000000, 0.000000000000000000 ) ) ;
#117793 = ORIENTED_EDGE ( 'NONE', *, *, #236614, .T. ) ;
#117794 = DIRECTION ( 'NONE',  ( 0.000000000000000000, 0.000000000000000000, 1.000000000000000000 ) ) ;
#117795 = ORIENTED_EDGE ( 'NONE', *, *, #100041, .F. ) ;
#117797 = ORIENTED_EDGE ( 'NONE', *, *, #175324, .F. ) ;
#117796 = ORIENTED_EDGE ( 'NONE', *, *, #73763, .T. ) ;
#117798 = CARTESIAN_POINT ( 'NONE',  ( 18.52165635395186172, 85.48115071129440423, -129.4982699016618994 ) ) ;
#117799 = VERTEX_POINT ( 'NONE', #122045 ) ;
#117800 = FACE_OUTER_BOUND ( 'NONE', #202439, .T. ) ;
#117802 = ORIENTED_EDGE ( 'NONE', *, *, #150906, .T. ) ;
#117801 = VECTOR ( 'NONE', #56177, 1000.000000000000000 ) ;
#117803 = TOROIDAL_SURFACE ( 'NONE', #167906, 1.900000000000002576, 0.1000000000000000056 ) ;
#117804 = ORIENTED_EDGE ( 'NONE', *, *, #29649, .T. ) ;
#117805 = FACE_OUTER_BOUND ( 'NONE', #13040, .T. ) ;
#117806 = DIRECTION ( 'NONE',  ( 0.000000000000000000, 0.000000000000000000, 1.000000000000000000 ) ) ;
#117808 = ORIENTED_EDGE ( 'NONE', *, *, #82074, .T. ) ;
#117807 = DIRECTION ( 'NONE',  ( 0.7071067811865474617, -0.7071067811865474617, -4.937700262164531476E-15 ) ) ;
#117809 = DIRECTION ( 'NONE',  ( 0.000000000000000000, -0.008583690987135041833, 0.9999631594459055250 ) ) ;
#117810 = ORIENTED_EDGE ( 'NONE', *, *, #96204, .F. ) ;
#117811 = DIRECTION ( 'NONE',  ( 0.000000000000000000, -0.8096735173027139743, 0.5868805631290339164 ) ) ;
#117812 = DIRECTION ( 'NONE',  ( 0.000000000000000000, 0.000000000000000000, 1.000000000000000000 ) ) ;
#117813 = CARTESIAN_POINT ( 'NONE',  ( 21.05000000000000071, 86.48473784507378070, -209.3714211149925575 ) ) ;
#117814 = ORIENTED_EDGE ( 'NONE', *, *, #181465, .T. ) ;
#117815 = DIRECTION ( 'NONE',  ( -1.000000000000000000, -0.000000000000000000, -0.000000000000000000 ) ) ;
#117816 = CARTESIAN_POINT ( 'NONE',  ( -18.49999999999999289, 38.22547802645942028, -261.0781739499484502 ) ) ;
#117817 = CARTESIAN_POINT ( 'NONE',  ( 23.24999999999999645, 1.115600667400684642E-11, -134.0000000000000284 ) ) ;
#117818 = ORIENTED_EDGE ( 'NONE', *, *, #125154, .F. ) ;
#117820 = DIRECTION ( 'NONE',  ( 1.073024830501117725E-15, 0.2128009952263604232, -0.9770955615653316162 ) ) ;
#117819 = AXIS2_PLACEMENT_3D ( 'NONE', #178886, #217947, #159305 ) ;
#117821 = ORIENTED_EDGE ( 'NONE', *, *, #117560, .F. ) ;
#117822 = EDGE_LOOP ( 'NONE', ( #126173, #203528, #214051, #166409 ) ) ;
#117823 = CYLINDRICAL_SURFACE ( 'NONE', #88872, 4.000000000000003553 ) ;
#117824 = ORIENTED_EDGE ( 'NONE', *, *, #213954, .T. ) ;
#117825 = CIRCLE ( 'NONE', #17864, 0.1000000000000013933 ) ;
#117826 = ORIENTED_EDGE ( 'NONE', *, *, #223944, .F. ) ;
#117827 = CARTESIAN_POINT ( 'NONE',  ( -16.97683809663752186, 9.950000000011138823, -80.40236401819653622 ) ) ;
#117828 = DIRECTION ( 'NONE',  ( -1.000000000000000000, 7.304098846218164250E-16, -4.217023435051628197E-16 ) ) ;
#117829 = ORIENTED_EDGE ( 'NONE', *, *, #228516, .T. ) ;
#117830 = ORIENTED_EDGE ( 'NONE', *, *, #251332, .F. ) ;
#117831 = LINE ( 'NONE', #197367, #193815 ) ;
#117832 = LINE ( 'NONE', #240366, #27394 ) ;
#117833 = ORIENTED_EDGE ( 'NONE', *, *, #114088, .F. ) ;
#117834 = EDGE_CURVE ( 'NONE', #35839, #9389, #237413, .T. ) ;
#117835 = ORIENTED_EDGE ( 'NONE', *, *, #149767, .F. ) ;
#117836 = ORIENTED_EDGE ( 'NONE', *, *, #92479, .T. ) ;
#117837 = AXIS2_PLACEMENT_3D ( 'NONE', #142667, #226042, #123137 ) ;
#117838 = CARTESIAN_POINT ( 'NONE',  ( 18.49999999999999645, 1.115600667400684642E-11, -100.5000000000000426 ) ) ;
#117839 = LINE ( 'NONE', #171445, #155396 ) ;
#117840 = DIRECTION ( 'NONE',  ( -1.000000000000000000, 0.000000000000000000, 0.000000000000000000 ) ) ;
#117841 = CARTESIAN_POINT ( 'NONE',  ( -20.54999999999999716, 87.75000000001156764, -57.17310748452423752 ) ) ;
#117842 = DIRECTION ( 'NONE',  ( 0.000000000000000000, 0.000000000000000000, 1.000000000000000000 ) ) ;
#117843 = EDGE_CURVE ( 'NONE', #51021, #257124, #236845, .T. ) ;
#117844 = CARTESIAN_POINT ( 'NONE',  ( -20.54999999999999716, 1.115600667400684642E-11, -200.9999999999999432 ) ) ;
#117845 = ADVANCED_FACE ( 'NONE', ( #182021 ), #199014, .F. ) ;
#117846 = CARTESIAN_POINT ( 'NONE',  ( 20.12500000000000000, 9.749999999999998224, -8.111771282114276005 ) ) ;
#117848 = CARTESIAN_POINT ( 'NONE',  ( 20.94999999999999929, 1.115600667400684642E-11, -71.00000000000001421 ) ) ;
#117847 = PLANE ( 'NONE',  #252575 ) ;
#117849 = CYLINDRICAL_SURFACE ( 'NONE', #248942, 0.1000000000000054040 ) ;
#117850 = DIRECTION ( 'NONE',  ( 2.952720810173289112E-16, -1.000000000000000000, 0.000000000000000000 ) ) ;
#117851 = VECTOR ( 'NONE', #7326, 1000.000000000000000 ) ;
#117852 = DIRECTION ( 'NONE',  ( 0.000000000000000000, 1.000000000000000000, 6.982962677686266711E-15 ) ) ;
#117853 = FACE_OUTER_BOUND ( 'NONE', #251255, .T. ) ;
#117854 = VECTOR ( 'NONE', #69011, 1000.000000000000000 ) ;
#117855 = VERTEX_POINT ( 'NONE', #178193 ) ;
#117856 = AXIS2_PLACEMENT_3D ( 'NONE', #28156, #55047, #212873 ) ;
#117857 = EDGE_CURVE ( 'NONE', #87436, #76729, #58494, .T. ) ;
#117858 =( BOUNDED_CURVE ( )  B_SPLINE_CURVE ( 3, ( #232572, #49070, #13505, #226403 ),
 .UNSPECIFIED., .F., .F. ) 
 B_SPLINE_CURVE_WITH_KNOTS ( ( 4, 4 ),
 ( 3.192897208853993085, 4.712388980384696779 ),
 .UNSPECIFIED. ) 
 CURVE ( )  GEOMETRIC_REPRESENTATION_ITEM ( )  RATIONAL_B_SPLINE_CURVE ( ( 1.000000000000000000, 0.8166740347213210516, 0.8166740347213210516, 1.000000000000000000 ) ) 
 REPRESENTATION_ITEM ( '' )  );
#117860 = EDGE_LOOP ( 'NONE', ( #245748, #201298, #36308, #149621 ) ) ;
#117859 = CARTESIAN_POINT ( 'NONE',  ( 20.85000000000000142, 7.783179459866048866, -245.3643104511423303 ) ) ;
#117861 = EDGE_CURVE ( 'NONE', #87416, #28439, #237596, .T. ) ;
#117862 = LINE ( 'NONE', #81282, #94575 ) ;
#117863 = ADVANCED_FACE ( 'NONE', ( #80311 ), #41803, .T. ) ;
#117864 = DIRECTION ( 'NONE',  ( 0.000000000000000000, -7.086529944415894657E-15, 1.000000000000000000 ) ) ;
#117865 = EDGE_LOOP ( 'NONE', ( #62062, #236273, #237416, #164850, #39760 ) ) ;
#117866 = CIRCLE ( 'NONE', #205336, 4.149999999999999467 ) ;
#117867 = AXIS2_PLACEMENT_3D ( 'NONE', #145383, #141532, #101073 ) ;
#117868 = CARTESIAN_POINT ( 'NONE',  ( 20.85000000000000142, -1.835859311432481045, -78.60443916879853532 ) ) ;
#117869 = EDGE_CURVE ( 'NONE', #184776, #70370, #118192, .T. ) ;
#117870 = CARTESIAN_POINT ( 'NONE',  ( -16.88853107394619357, 9.950878483346977887, -20.85293634689222841 ) ) ;
#117871 = ORIENTED_EDGE ( 'NONE', *, *, #1734, .F. ) ;
#117872 = CARTESIAN_POINT ( 'NONE',  ( -20.94999999999999929, 11.75000000001115197, -141.0148057706540214 ) ) ;
#117873 = CARTESIAN_POINT ( 'NONE',  ( -22.57320508075687115, 64.35000000001268461, -203.5231074845243882 ) ) ;
#117874 = EDGE_CURVE ( 'NONE', #52328, #189336, #208394, .T. ) ;
#117875 = CYLINDRICAL_SURFACE ( 'NONE', #34554, 0.09999999999999939493 ) ;
#117876 = AXIS2_PLACEMENT_3D ( 'NONE', #99903, #116936, #176938 ) ;
#117877 = DIRECTION ( 'NONE',  ( 1.000000000000000000, 0.000000000000000000, 0.000000000000000000 ) ) ;
#117879 = ORIENTED_EDGE ( 'NONE', *, *, #145854, .F. ) ;
#117878 = CARTESIAN_POINT ( 'NONE',  ( -18.59999999999999787, 9.250000000011157297, -88.25000000000005684 ) ) ;
#117881 = EDGE_LOOP ( 'NONE', ( #228652, #78582, #8666, #198509 ) ) ;
#117880 = DIRECTION ( 'NONE',  ( 0.000000000000000000, 3.552713678800509607E-15, 1.000000000000000000 ) ) ;
#117882 = AXIS2_PLACEMENT_3D ( 'NONE', #5691, #205189, #69569 ) ;
#117883 = DIRECTION ( 'NONE',  ( 0.000000000000000000, 0.2128009952263403282, -0.9770955615653358350 ) ) ;
#117885 = CARTESIAN_POINT ( 'NONE',  ( 21.12769345151713196, 10.71928767694057072, -12.24748034619748616 ) ) ;
#117884 = VECTOR ( 'NONE', #107181, 1000.000000000000114 ) ;
#117886 = CARTESIAN_POINT ( 'NONE',  ( 20.85000000000000142, 64.25000000001249134, -176.8069731475025321 ) ) ;
#117888 = ADVANCED_FACE ( 'NONE', ( #7211 ), #104996, .T. ) ;
#117887 = DIRECTION ( 'NONE',  ( 1.000000000000000000, 7.304098846218133681E-16, 5.100424963727255128E-30 ) ) ;
#117889 = VECTOR ( 'NONE', #78822, 1000.000000000000000 ) ;
#117891 = DIRECTION ( 'NONE',  ( 0.000000000000000000, 0.000000000000000000, 1.000000000000000000 ) ) ;
#117890 = CARTESIAN_POINT ( 'NONE',  ( 18.39999999999999858, 8.841736820195473356, -245.4273993276876240 ) ) ;
#117892 = DIRECTION ( 'NONE',  ( -1.000000000000000000, 0.000000000000000000, 0.000000000000000000 ) ) ;
#117893 = DIRECTION ( 'NONE',  ( 0.000000000000000000, 1.000000000000000000, 7.272083257015735086E-15 ) ) ;
#117894 = FACE_OUTER_BOUND ( 'NONE', #209671, .T. ) ;
#117895 = CARTESIAN_POINT ( 'NONE',  ( 21.78635804494511419, 0.09900506551883611617, -160.4643385148467871 ) ) ;
#117896 = SPHERICAL_SURFACE ( 'NONE', #164042, 0.1000000000000000056 ) ;
#117897 = VERTEX_POINT ( 'NONE', #25523 ) ;
#117898 = CARTESIAN_POINT ( 'NONE',  ( -21.05000000000000071, -1.835341550213255957, -78.55515129256302487 ) ) ;
#117899 = ORIENTED_EDGE ( 'NONE', *, *, #63089, .F. ) ;
#117900 = ORIENTED_EDGE ( 'NONE', *, *, #69057, .F. ) ;
#117901 = DIRECTION ( 'NONE',  ( 2.659396599871503635E-15, 0.6132151058540549204, -0.7899159663865520375 ) ) ;
#117902 = DIRECTION ( 'NONE',  ( 0.000000000000000000, -0.9651348961777155289, 0.2617529984165036794 ) ) ;
#117903 = ORIENTED_EDGE ( 'NONE', *, *, #126515, .F. ) ;
#117904 = VERTEX_POINT ( 'NONE', #184575 ) ;
#117905 = AXIS2_PLACEMENT_3D ( 'NONE', #17951, #69290, #208793 ) ;
#117906 = SURFACE_STYLE_USAGE ( .BOTH. , #234008 ) ;
#117907 = VECTOR ( 'NONE', #237834, 1000.000000000000000 ) ;
#117908 = ORIENTED_EDGE ( 'NONE', *, *, #170786, .F. ) ;
#117909 = ORIENTED_EDGE ( 'NONE', *, *, #161141, .T. ) ;
#117910 = ADVANCED_FACE ( 'NONE', ( #5921 ), #47616, .T. ) ;
#117911 = DIRECTION ( 'NONE',  ( 1.000000000000000000, 0.000000000000000000, 0.000000000000000000 ) ) ;
#117912 = CARTESIAN_POINT ( 'NONE',  ( 21.05000000000000071, 67.92720994251783395, -214.1870976236629929 ) ) ;
#117913 = FACE_OUTER_BOUND ( 'NONE', #61827, .T. ) ;
#117914 = EDGE_CURVE ( 'NONE', #148927, #41773, #232949, .T. ) ;
#117915 = DIRECTION ( 'NONE',  ( 0.000000000000000000, 0.000000000000000000, -1.000000000000000000 ) ) ;
#117916 = DIRECTION ( 'NONE',  ( 0.000000000000000000, -0.08413937888704772772, 0.9964539953858894128 ) ) ;
#117917 = AXIS2_PLACEMENT_3D ( 'NONE', #4586, #147972, #5868 ) ;
#117918 = AXIS2_PLACEMENT_3D ( 'NONE', #114981, #12055, #34196 ) ;
#117919 = CARTESIAN_POINT ( 'NONE',  ( 20.94999999999999929, 24.07562609839690637, -252.7152152143214892 ) ) ;
#117921 = VERTEX_POINT ( 'NONE', #4639 ) ;
#117920 = DIRECTION ( 'NONE',  ( 0.000000000000000000, 0.000000000000000000, -1.000000000000000000 ) ) ;
#117923 = DIRECTION ( 'NONE',  ( 1.000000000000000000, 0.000000000000000000, 0.000000000000000000 ) ) ;
#117922 = LINE ( 'NONE', #196190, #158755 ) ;
#117924 = EDGE_CURVE ( 'NONE', #68130, #122855, #108036, .T. ) ;
#117925 = CARTESIAN_POINT ( 'NONE',  ( -21.55000000000000071, 52.95562111564758823, -234.1965973584252652 ) ) ;
#117927 = EDGE_CURVE ( 'NONE', #229988, #202898, #208000, .T. ) ;
#117926 =( BOUNDED_SURFACE ( )  B_SPLINE_SURFACE ( 3, 2, ( 
 ( #132213, #33154, #172674 ),
 ( #93075, #252147, #188335 ),
 ( #73557, #50097, #232624 ),
 ( #168820, #14858, #253431 ) ),
 .UNSPECIFIED., .F., .F., .F. ) 
 B_SPLINE_SURFACE_WITH_KNOTS ( ( 4, 4 ),
 ( 3, 3 ),
 ( 0.04058434257139457990, 0.04256401539001584966 ),
 ( 0.000000000000000000, 1.000000000000000000 ),
 .UNSPECIFIED. ) 
 GEOMETRIC_REPRESENTATION_ITEM ( )  RATIONAL_B_SPLINE_SURFACE ( (
 ( 1.000000000000000000, 0.7103081912008947230, 1.000000000000000000),
 ( 1.000000000000000000, 0.7104998333553655954, 1.000000000000000000),
 ( 1.000000000000000000, 0.7107238315756251312, 1.000000000000000000),
 ( 1.000000000000000000, 0.7110073749539724819, 1.000000000000000000) ) ) 
 REPRESENTATION_ITEM ( '' )  SURFACE ( )  );
#117928 = ORIENTED_EDGE ( 'NONE', *, *, #27920, .F. ) ;
#117929 = AXIS2_PLACEMENT_3D ( 'NONE', #41669, #122483, #2503 ) ;
#117930 = CARTESIAN_POINT ( 'NONE',  ( -20.54999999999999716, 85.50000000001222134, -146.4170766071767389 ) ) ;
#117931 = DIRECTION ( 'NONE',  ( 0.000000000000000000, 1.000000000000000000, 0.000000000000000000 ) ) ;
#117932 = ORIENTED_EDGE ( 'NONE', *, *, #155045, .F. ) ;
#117933 = VECTOR ( 'NONE', #82797, 1000.000000000000000 ) ;
#117934 = EDGE_CURVE ( 'NONE', #254767, #30904, #257808, .T. ) ;
#117937 = CARTESIAN_POINT ( 'NONE',  ( -20.64999999999999858, 1.115600667400684642E-11, -68.90000000000000568 ) ) ;
#117936 = FACE_OUTER_BOUND ( 'NONE', #232038, .T. ) ;
#117935 = AXIS2_PLACEMENT_3D ( 'NONE', #177846, #164683, #125549 ) ;
#117938 = AXIS2_PLACEMENT_3D ( 'NONE', #130033, #187480, #184889 ) ;
#117939 = ADVANCED_FACE ( 'NONE', ( #26824 ), #51648, .F. ) ;
#117940 = CYLINDRICAL_SURFACE ( 'NONE', #36071, 11.74999999999999645 ) ;
#117941 = DIRECTION ( 'NONE',  ( 0.000000000000000000, 0.000000000000000000, -1.000000000000000000 ) ) ;
#117942 = ADVANCED_FACE ( 'NONE', ( #158212 ), #1641, .F. ) ;
#117943 = EDGE_LOOP ( 'NONE', ( #115100, #100664, #134590, #251702 ) ) ;
#117944 = ORIENTED_EDGE ( 'NONE', *, *, #162500, .T. ) ;
#117945 = AXIS2_PLACEMENT_3D ( 'NONE', #170418, #229064, #253732 ) ;
#117946 = DIRECTION ( 'NONE',  ( 0.000000000000000000, 1.000000000000000000, 2.891205793294679805E-16 ) ) ;
#117947 = EDGE_CURVE ( 'NONE', #58136, #55301, #116238, .T. ) ;
#117948 = CARTESIAN_POINT ( 'NONE',  ( 18.59999999999999076, 16.67126802362266247, -222.8016931105129004 ) ) ;
#117949 = DIRECTION ( 'NONE',  ( 0.000000000000000000, -0.4721928772777343464, -0.8814952561688431665 ) ) ;
#117950 = CARTESIAN_POINT ( 'NONE',  ( -20.54999999999999716, 74.05981308412415842, -115.8522266955776416 ) ) ;
#117951 = ORIENTED_EDGE ( 'NONE', *, *, #222809, .T. ) ;
#117952 = VECTOR ( 'NONE', #30104, 1000.000000000000000 ) ;
#117954 = AXIS2_PLACEMENT_3D ( 'NONE', #98465, #18963, #181907 ) ;
#117953 = DIRECTION ( 'NONE',  ( -1.000000000000000000, 0.000000000000000000, 0.000000000000000000 ) ) ;
#117955 = EDGE_CURVE ( 'NONE', #233025, #173202, #4213, .T. ) ;
#117956 = CARTESIAN_POINT ( 'NONE',  ( 21.51976009735019346, 6.910458441670357388, -167.4999999999999716 ) ) ;
#117957 = SPHERICAL_SURFACE ( 'NONE', #57619, 0.1000000000000000056 ) ;
#117958 = EDGE_CURVE ( 'NONE', #37771, #69698, #242831, .T. ) ;
#117959 = EDGE_CURVE ( 'NONE', #112448, #95210, #6861, .T. ) ;
#117960 = CARTESIAN_POINT ( 'NONE',  ( -20.85000000000000142, 1.115600667400684642E-11, -167.5000000000000284 ) ) ;
#117961 = DIRECTION ( 'NONE',  ( 1.000000000000000000, 0.000000000000000000, 0.000000000000000000 ) ) ;
#117962 = AXIS2_PLACEMENT_3D ( 'NONE', #203128, #61044, #119769 ) ;
#117964 =( BOUNDED_CURVE ( )  B_SPLINE_CURVE ( 3, ( #23962, #142581, #206426, #103451 ),
 .UNSPECIFIED., .F., .F. ) 
 B_SPLINE_CURVE_WITH_KNOTS ( ( 4, 4 ),
 ( 0.5235987755983078085, 1.570796326794896558 ),
 .UNSPECIFIED. ) 
 CURVE ( )  GEOMETRIC_REPRESENTATION_ITEM ( )  RATIONAL_B_SPLINE_CURVE ( ( 1.000000000000000000, 0.9106836025229606557, 0.9106836025229606557, 1.000000000000000000 ) ) 
 REPRESENTATION_ITEM ( '' )  );
#117963 = AXIS2_PLACEMENT_3D ( 'NONE', #212311, #47102, #206203 ) ;
#117965 = AXIS2_PLACEMENT_3D ( 'NONE', #223595, #41159, #63248 ) ;
#117966 = ADVANCED_FACE ( 'NONE', ( #237709 ), #203717, .F. ) ;
#117968 = ORIENTED_EDGE ( 'NONE', *, *, #124735, .F. ) ;
#117967 = CARTESIAN_POINT ( 'NONE',  ( 18.59999999999999787, 77.83585931145600512, -158.5186683157258187 ) ) ;
#117969 = AXIS2_PLACEMENT_3D ( 'NONE', #166103, #209045, #111230 ) ;
#117970 = DIRECTION ( 'NONE',  ( -3.469446951953677298E-14, -0.9908441862701782288, -0.1350103645450542456 ) ) ;
#117971 = CARTESIAN_POINT ( 'NONE',  ( 21.05000000000000071, 8.876614585098254295, -142.3850804788447135 ) ) ;
#117972 = PLANE ( 'NONE',  #200201 ) ;
#117973 = DIRECTION ( 'NONE',  ( 0.000000000000000000, 0.000000000000000000, -1.000000000000000000 ) ) ;
#117974 = DIRECTION ( 'NONE',  ( 0.000000000000000000, 0.000000000000000000, -1.000000000000000000 ) ) ;
#117975 = EDGE_CURVE ( 'NONE', #203019, #172330, #3797, .T. ) ;
#117977 = ORIENTED_EDGE ( 'NONE', *, *, #74160, .T. ) ;
#117976 = CARTESIAN_POINT ( 'NONE',  ( 21.08832698747859169, 67.22463560659436155, -57.29439001806023413 ) ) ;
#117978 = FACE_OUTER_BOUND ( 'NONE', #77824, .T. ) ;
#117979 = ADVANCED_FACE ( 'NONE', ( #162041 ), #104580, .F. ) ;
#117980 = PLANE ( 'NONE',  #13561 ) ;
#117981 = DIRECTION ( 'NONE',  ( 0.000000000000000000, 6.608470384673558123E-15, -1.000000000000000000 ) ) ;
#117982 = ORIENTED_EDGE ( 'NONE', *, *, #76044, .F. ) ;
#117983 = DIRECTION ( 'NONE',  ( 0.000000000000000000, 0.2617529984164955192, 0.9651348961777177493 ) ) ;
#117984 = CYLINDRICAL_SURFACE ( 'NONE', #148356, 4.000000000000003553 ) ;
#117985 = DIRECTION ( 'NONE',  ( 0.000000000000000000, 6.982962677686266711E-15, -1.000000000000000000 ) ) ;
#117986 = DIRECTION ( 'NONE',  ( 1.000000000000000000, 0.000000000000000000, 0.000000000000000000 ) ) ;
#117987 = DIRECTION ( 'NONE',  ( -0.000000000000000000, 0.9910465087640860649, 0.1335171055202901413 ) ) ;
#117988 = VECTOR ( 'NONE', #95006, 1000.000000000000114 ) ;
#117989 = CIRCLE ( 'NONE', #126365, 7.900000000000000355 ) ;
#117990 = DIRECTION ( 'NONE',  ( 0.000000000000000000, 0.8777080977375072424, -0.4791956752371691608 ) ) ;
#117991 = VECTOR ( 'NONE', #161414, 1000.000000000000000 ) ;
#117992 = VECTOR ( 'NONE', #253797, 1000.000000000000000 ) ;
#117993 = ORIENTED_EDGE ( 'NONE', *, *, #121536, .F. ) ;
#117994 = ORIENTED_EDGE ( 'NONE', *, *, #192932, .F. ) ;
#117995 = CARTESIAN_POINT ( 'NONE',  ( -18.38639463286148867, 64.51980042617634581, -160.7731074845244450 ) ) ;
#117996 = FACE_OUTER_BOUND ( 'NONE', #65182, .T. ) ;
#117997 = CARTESIAN_POINT ( 'NONE',  ( 22.57320508075687115, 11.48087284840413425, -198.4995883060917663 ) ) ;
#117998 = CARTESIAN_POINT ( 'NONE',  ( -21.05000000000000071, 10.68863688179707694, -222.5873974249509217 ) ) ;
#117999 = ORIENTED_EDGE ( 'NONE', *, *, #171255, .F. ) ;
#118000 = CYLINDRICAL_SURFACE ( 'NONE', #238421, 0.1000000000000028644 ) ;
#118001 = CARTESIAN_POINT ( 'NONE',  ( 20.74625933824097146, 10.50000428349506265, -207.4689267983004868 ) ) ;
#118002 = DIRECTION ( 'NONE',  ( 0.000000000000000000, 1.000000000000000000, 8.717686153663073805E-15 ) ) ;
#118003 = DIRECTION ( 'NONE',  ( 0.000000000000000000, 1.224646799142185182E-16, 1.000000000000000000 ) ) ;
#118004 = ORIENTED_EDGE ( 'NONE', *, *, #218611, .T. ) ;
#118005 = CARTESIAN_POINT ( 'NONE',  ( -21.05000000000000071, 69.70000000001164153, -69.42310748452436542 ) ) ;
#118006 = EDGE_LOOP ( 'NONE', ( #233620, #141068, #71152, #88047 ) ) ;
#118007 = CIRCLE ( 'NONE', #43196, 0.1000000000000026007 ) ;
#118008 = CARTESIAN_POINT ( 'NONE',  ( -18.48179518609178018, -9.518325300493765795, -40.38970557676145745 ) ) ;
#118009 = VERTEX_POINT ( 'NONE', #79880 ) ;
#118010 = CARTESIAN_POINT ( 'NONE',  ( -21.05000000000000071, -0.09999999998884473440, -26.95934304829875927 ) ) ;
#118011 = FACE_OUTER_BOUND ( 'NONE', #200794, .T. ) ;
#118012 = FACE_OUTER_BOUND ( 'NONE', #150289, .T. ) ;
#118013 = EDGE_LOOP ( 'NONE', ( #181435, #227391, #83855, #77690 ) ) ;
#118014 = LINE ( 'NONE', #196264, #40710 ) ;
#118015 = CARTESIAN_POINT ( 'NONE',  ( -18.50000000000000000, 77.16270174995064224, -195.4231074845243370 ) ) ;
#118016 = DIRECTION ( 'NONE',  ( 0.000000000000000000, 0.000000000000000000, -1.000000000000000000 ) ) ;
#118017 = ORIENTED_EDGE ( 'NONE', *, *, #226076, .F. ) ;
#118018 = CARTESIAN_POINT ( 'NONE',  ( 23.14999999999998437, 1.115600667400684642E-11, -100.5000000000000284 ) ) ;
#118019 = EDGE_CURVE ( 'NONE', #149704, #98813, #193352, .T. ) ;
#118021 = ORIENTED_EDGE ( 'NONE', *, *, #224787, .T. ) ;
#118020 = CARTESIAN_POINT ( 'NONE',  ( 18.39999999999999503, 64.52683809664938508, -90.37310748452438247 ) ) ;
#118022 = CARTESIAN_POINT ( 'NONE',  ( 18.59999999999999787, 65.76686835164943545, -247.8575435273897938 ) ) ;
#118023 = CARTESIAN_POINT ( 'NONE',  ( 18.59999999999999787, -10.35479209691423996, -161.2565409830737906 ) ) ;
#118024 = EDGE_CURVE ( 'NONE', #135417, #127391, #23825, .T. ) ;
#118025 = AXIS2_PLACEMENT_3D ( 'NONE', #146313, #85031, #241571 ) ;
#118026 = AXIS2_PLACEMENT_3D ( 'NONE', #113529, #232219, #39150 ) ;
#118027 = ORIENTED_EDGE ( 'NONE', *, *, #4037, .F. ) ;
#118028 = AXIS2_PLACEMENT_3D ( 'NONE', #205423, #4650, #105005 ) ;
#118029 = DIRECTION ( 'NONE',  ( -0.000000000000000000, 0.4791956752371485107, 0.8777080977375185666 ) ) ;
#118031 = ADVANCED_FACE ( 'NONE', ( #199881 ), #20562, .T. ) ;
#118030 = LINE ( 'NONE', #157189, #233584 ) ;
#118032 = FACE_OUTER_BOUND ( 'NONE', #161859, .T. ) ;
#118034 = EDGE_CURVE ( 'NONE', #95961, #235551, #43365, .T. ) ;
#118033 = ORIENTED_EDGE ( 'NONE', *, *, #38828, .T. ) ;
#118035 = LINE ( 'NONE', #109349, #225747 ) ;
#118036 = DIRECTION ( 'NONE',  ( -1.000000000000000000, 0.000000000000000000, -0.000000000000000000 ) ) ;
#118037 = CARTESIAN_POINT ( 'NONE',  ( -22.50000000000000000, 64.35000000001269882, -203.5231074845244166 ) ) ;
#118038 = VERTEX_POINT ( 'NONE', #227114 ) ;
#118039 = AXIS2_PLACEMENT_3D ( 'NONE', #154295, #31763, #111270 ) ;
#118040 = VERTEX_POINT ( 'NONE', #26369 ) ;
#118041 = AXIS2_PLACEMENT_3D ( 'NONE', #146904, #69983, #110361 ) ;
#118042 = EDGE_CURVE ( 'NONE', #100689, #243191, #99611, .T. ) ;
#118043 = VECTOR ( 'NONE', #112485, 1000.000000000000000 ) ;
#118044 = VECTOR ( 'NONE', #52038, 1000.000000000000000 ) ;
#118045 = ORIENTED_EDGE ( 'NONE', *, *, #188234, .F. ) ;
#118046 = DIRECTION ( 'NONE',  ( -1.000000000000000000, 0.000000000000000000, -0.000000000000000000 ) ) ;
#118047 = LINE ( 'NONE', #39828, #54616 ) ;
#118049 = ORIENTED_EDGE ( 'NONE', *, *, #144624, .F. ) ;
#118048 = FACE_OUTER_BOUND ( 'NONE', #201412, .T. ) ;
#118050 = DIRECTION ( 'NONE',  ( 1.000000000000000000, 0.000000000000000000, 0.000000000000000000 ) ) ;
#118051 = CYLINDRICAL_SURFACE ( 'NONE', #257079, 0.4999999999999944489 ) ;
#118052 = DIRECTION ( 'NONE',  ( 0.000000000000000000, 0.000000000000000000, -1.000000000000000000 ) ) ;
#118053 = DIRECTION ( 'NONE',  ( 0.000000000000000000, -0.9651348961777157509, 0.2617529984165031243 ) ) ;
#118054 = CARTESIAN_POINT ( 'NONE',  ( -20.94999999999999929, 64.35000000001141984, -36.02310748452440237 ) ) ;
#118055 = VECTOR ( 'NONE', #224618, 1000.000000000000000 ) ;
#118058 = ORIENTED_EDGE ( 'NONE', *, *, #249892, .T. ) ;
#118057 = EDGE_CURVE ( 'NONE', #148979, #20649, #68053, .T. ) ;
#118056 = DIRECTION ( 'NONE',  ( -0.000000000000000000, 0.7397360091702694929, 0.6728971962616898672 ) ) ;
#118060 = ORIENTED_EDGE ( 'NONE', *, *, #53519, .F. ) ;
#118059 = LINE ( 'NONE', #235425, #111058 ) ;
#118063 = DIRECTION ( 'NONE',  ( 0.000000000000000000, 0.6728971962617483760, -0.7397360091702162022 ) ) ;
#118062 = CARTESIAN_POINT ( 'NONE',  ( -16.94107738177415712, 60.85118289042637940, -221.1214263997032106 ) ) ;
#118061 = AXIS2_PLACEMENT_3D ( 'NONE', #177722, #232557, #154326 ) ;
#118064 = ORIENTED_EDGE ( 'NONE', *, *, #203904, .F. ) ;
#118065 = EDGE_LOOP ( 'NONE', ( #170051, #122123, #87431, #47527 ) ) ;
#118066 = EDGE_CURVE ( 'NONE', #231868, #48459, #220468, .T. ) ;
#118067 = CARTESIAN_POINT ( 'NONE',  ( -18.52643265882458579, 10.31973158071402530, -106.0505334713354983 ) ) ;
#118068 = DIRECTION ( 'NONE',  ( 0.000000000000000000, 0.2617529984165024026, 0.9651348961777158619 ) ) ;
#118069 = DIRECTION ( 'NONE',  ( 1.000000000000000000, -0.000000000000000000, -0.000000000000000000 ) ) ;
#118070 = AXIS2_PLACEMENT_3D ( 'NONE', #235277, #60486, #98302 ) ;
#118071 = DIRECTION ( 'NONE',  ( 0.000000000000000000, 1.000000000000000000, 0.000000000000000000 ) ) ;
#118072 = DIRECTION ( 'NONE',  ( 0.000000000000000000, 0.000000000000000000, -1.000000000000000000 ) ) ;
#118074 = ADVANCED_FACE ( 'NONE', ( #88878 ), #225815, .T. ) ;
#118073 = SPHERICAL_SURFACE ( 'NONE', #153049, 0.1000000000000000056 ) ;
#118075 = AXIS2_PLACEMENT_3D ( 'NONE', #107078, #167100, #64114 ) ;
#118076 = B_SPLINE_CURVE_WITH_KNOTS ( 'NONE', 3,
 ( #219052, #99092, #78258, #39174, #174861, #156563, #134373, #37888, #1285, #254321, #19596, #114831, #18298, #238635 ),
 .UNSPECIFIED., .F., .F.,
 ( 4, 2, 2, 2, 2, 2, 4 ),
 ( 1.387778780781445676E-17, 0.0003823333598418262582, 0.0005735000397627122281, 0.0006690833797231313064, 0.0007168750497033422008, 0.0007407708846934429317, 0.0007646667196835435542 ),
 .UNSPECIFIED. ) ;
#118077 = AXIS2_PLACEMENT_3D ( 'NONE', #152775, #94040, #190603 ) ;
#118078 = AXIS2_PLACEMENT_3D ( 'NONE', #206870, #28268, #247262 ) ;
#118079 = ADVANCED_FACE ( 'NONE', ( #168491 ), #164597, .T. ) ;
#118081 = CIRCLE ( 'NONE', #89035, 0.1000000000000028644 ) ;
#118080 = DIRECTION ( 'NONE',  ( -1.000000000000000000, 0.000000000000000000, 0.000000000000000000 ) ) ;
#118082 = ORIENTED_EDGE ( 'NONE', *, *, #50010, .T. ) ;
#118083 = ORIENTED_EDGE ( 'NONE', *, *, #129217, .F. ) ;
#118084 = CARTESIAN_POINT ( 'NONE',  ( 22.39999999999999503, 64.25000000001237765, -170.1231074845244393 ) ) ;
#118085 = EDGE_CURVE ( 'NONE', #141361, #135547, #124601, .T. ) ;
#118086 = EDGE_LOOP ( 'NONE', ( #16981, #245750, #197671, #125862 ) ) ;
#118087 = DIRECTION ( 'NONE',  ( 0.000000000000000000, 0.9424537609900487389, 0.3343365196859479638 ) ) ;
#118088 = CARTESIAN_POINT ( 'NONE',  ( 18.53317502108576775, 68.08564185115264422, -224.1612363371343122 ) ) ;
#118089 = DIRECTION ( 'NONE',  ( 1.000000000000000000, 0.000000000000000000, 0.000000000000000000 ) ) ;
#118090 = CARTESIAN_POINT ( 'NONE',  ( 23.14999999999999858, 36.65892442174935439, -249.5511627012433848 ) ) ;
#118091 = ORIENTED_EDGE ( 'NONE', *, *, #193872, .F. ) ;
#118092 = DIRECTION ( 'NONE',  ( -0.000000000000000000, 0.000000000000000000, 1.000000000000000000 ) ) ;
#118093 = ORIENTED_EDGE ( 'NONE', *, *, #23202, .F. ) ;
#118094 = EDGE_CURVE ( 'NONE', #210716, #204739, #245419, .T. ) ;
#118095 = DIRECTION ( 'NONE',  ( 0.000000000000000000, 0.000000000000000000, -1.000000000000000000 ) ) ;
#118096 = EDGE_LOOP ( 'NONE', ( #101213, #59780, #125612, #192634 ) ) ;
#118097 = CARTESIAN_POINT ( 'NONE',  ( 22.39999999999999858, 1.148907358139439339E-11, -201.0000000000015064 ) ) ;
#118098 = CARTESIAN_POINT ( 'NONE',  ( 21.05000000000000071, 74.63912941282058000, -195.4501095574334215 ) ) ;
#118099 = EDGE_CURVE ( 'NONE', #206320, #87394, #112152, .T. ) ;
#118100 = AXIS2_PLACEMENT_3D ( 'NONE', #30822, #110329, #129882 ) ;
#118101 = CARTESIAN_POINT ( 'NONE',  ( 20.85000000000000142, -11.64999999998883595, -67.00000000000000000 ) ) ;
#118102 = ORIENTED_EDGE ( 'NONE', *, *, #23220, .T. ) ;
#118103 = VECTOR ( 'NONE', #191718, 1000.000000000000000 ) ;
#118104 = DIRECTION ( 'NONE',  ( -1.000000000000000000, -2.952720810173289112E-16, 0.000000000000000000 ) ) ;
#118106 = ORIENTED_EDGE ( 'NONE', *, *, #30170, .T. ) ;
#118105 = FACE_OUTER_BOUND ( 'NONE', #522, .T. ) ;
#118107 = AXIS2_PLACEMENT_3D ( 'NONE', #76662, #72857, #217441 ) ;
#118108 = CARTESIAN_POINT ( 'NONE',  ( -20.85000000000000142, 77.14957036958736580, -61.70719500002233815 ) ) ;
#118109 = ORIENTED_EDGE ( 'NONE', *, *, #153006, .F. ) ;
#118110 = VECTOR ( 'NONE', #73207, 1000.000000000000000 ) ;
#118111 = AXIS2_PLACEMENT_3D ( 'NONE', #87398, #226921, #48283 ) ;
#118112 = CARTESIAN_POINT ( 'NONE',  ( -16.86132326855785735, 66.05000000001260219, -190.8244716998561046 ) ) ;
#118113 = ORIENTED_EDGE ( 'NONE', *, *, #256337, .F. ) ;
#118114 = CARTESIAN_POINT ( 'NONE',  ( 20.94999999999999574, 10.42338541492406279, -174.9920519238700649 ) ) ;
#118115 = CARTESIAN_POINT ( 'NONE',  ( 20.94999999999999929, -8.999999999988842703, -157.6060308773475640 ) ) ;
#118116 = LINE ( 'NONE', #73892, #120267 ) ;
#118117 = DIRECTION ( 'NONE',  ( 0.000000000000000000, -1.000000000000000000, 0.000000000000000000 ) ) ;
#118118 = AXIS2_PLACEMENT_3D ( 'NONE', #108049, #110602, #11523 ) ;
#118119 = CARTESIAN_POINT ( 'NONE',  ( -1.739115166359751801E-14, 11.65000000001114699, -58.35000000000000142 ) ) ;
#118120 = AXIS2_PLACEMENT_3D ( 'NONE', #20016, #79926, #62972 ) ;
#118121 = ORIENTED_EDGE ( 'NONE', *, *, #190036, .T. ) ;
#118122 = CIRCLE ( 'NONE', #109741, 0.09999999999999939493 ) ;
#118123 = CARTESIAN_POINT ( 'NONE',  ( 16.87683809663749557, 9.950000000011131718, -154.8500000000000227 ) ) ;
#118124 = CARTESIAN_POINT ( 'NONE',  ( 21.05000000000000071, 6.413978881499639684, -100.5857991162744867 ) ) ;
#118126 = DIRECTION ( 'NONE',  ( 0.000000000000000000, -0.2617529984165031243, -0.9651348961777158619 ) ) ;
#118125 = AXIS2_PLACEMENT_3D ( 'NONE', #244208, #65592, #198681 ) ;
#118127 = ORIENTED_EDGE ( 'NONE', *, *, #3900, .F. ) ;
#118128 = DIRECTION ( 'NONE',  ( 0.7071067811865460184, 0.6824534298470606997, -0.1850873201761399356 ) ) ;
#118129 = ORIENTED_EDGE ( 'NONE', *, *, #12690, .F. ) ;
#118130 = CARTESIAN_POINT ( 'NONE',  ( 23.15000000000000213, 23.40438595358394736, -253.3416554127419431 ) ) ;
#118132 = ORIENTED_EDGE ( 'NONE', *, *, #72305, .T. ) ;
#118131 = VECTOR ( 'NONE', #124218, 1000.000000000000000 ) ;
#118133 = DIRECTION ( 'NONE',  ( -0.000000000000000000, -0.000000000000000000, 1.000000000000000000 ) ) ;
#118134 = CARTESIAN_POINT ( 'NONE',  ( -23.25000000000000000, 4.250000000011156409, -146.1500000000000341 ) ) ;
#118136 = ORIENTED_EDGE ( 'NONE', *, *, #218913, .F. ) ;
#118135 = FACE_OUTER_BOUND ( 'NONE', #67414, .T. ) ;
#118137 = LINE ( 'NONE', #197662, #62562 ) ;
#118138 = ORIENTED_EDGE ( 'NONE', *, *, #35954, .F. ) ;
#118139 = AXIS2_PLACEMENT_3D ( 'NONE', #161609, #122470, #40395 ) ;
#118140 = DIRECTION ( 'NONE',  ( -1.000000000000000000, 0.000000000000000000, -0.000000000000000000 ) ) ;
#118141 = FACE_OUTER_BOUND ( 'NONE', #45392, .T. ) ;
#118142 = EDGE_LOOP ( 'NONE', ( #85961, #130247, #239592, #115621 ) ) ;
#118143 = ORIENTED_EDGE ( 'NONE', *, *, #146864, .T. ) ;
#118144 = AXIS2_PLACEMENT_3D ( 'NONE', #132917, #110768, #70400 ) ;
#118145 = DIRECTION ( 'NONE',  ( 1.000000000000000000, 0.000000000000000000, -0.000000000000000000 ) ) ;
#118147 = EDGE_CURVE ( 'NONE', #100973, #161687, #16466, .T. ) ;
#118146 = CARTESIAN_POINT ( 'NONE',  ( 20.94999999999999574, 67.07338541492480033, -94.55142446530125255 ) ) ;
#118148 = ORIENTED_EDGE ( 'NONE', *, *, #56740, .T. ) ;
#118149 = CARTESIAN_POINT ( 'NONE',  ( 23.14999999999999503, 11.75000000001116263, -54.85000000000000142 ) ) ;
#118151 = VERTEX_POINT ( 'NONE', #128037 ) ;
#118150 = CIRCLE ( 'NONE', #5692, 0.09999999999999344136 ) ;
#118152 = EDGE_LOOP ( 'NONE', ( #16030, #244931, #172984, #38495 ) ) ;
#118153 = TOROIDAL_SURFACE ( 'NONE', #5695, 0.6000000000000009770, 0.1000000000000000056 ) ;
#118154 = CIRCLE ( 'NONE', #151324, 0.9750000000000036415 ) ;
#118155 = DIRECTION ( 'NONE',  ( 1.000000000000000000, 0.000000000000000000, 0.000000000000000000 ) ) ;
#118156 = ADVANCED_FACE ( 'NONE', ( #188010 ), #109731, .T. ) ;
#118158 = EDGE_LOOP ( 'NONE', ( #46677, #256358, #142502, #184408, #188849 ) ) ;
#118157 = CARTESIAN_POINT ( 'NONE',  ( 18.46858270002952551, 85.47420267472247701, -95.92108554982041824 ) ) ;
#118159 = EDGE_CURVE ( 'NONE', #139066, #31859, #30226, .T. ) ;
#118160 = CARTESIAN_POINT ( 'NONE',  ( 23.14999999999999858, 74.95298800634525094, -207.3836470692357636 ) ) ;
#118161 = ADVANCED_FACE ( 'NONE', ( #86302 ), #47182, .T. ) ;
#118162 = CARTESIAN_POINT ( 'NONE',  ( -18.50000000000000000, 1.091828907200461884, -220.1187534104809913 ) ) ;
#118163 = CARTESIAN_POINT ( 'NONE',  ( -20.64999999999999858, 74.00000000001223555, -149.3477294072864652 ) ) ;
#118165 = DIRECTION ( 'NONE',  ( 0.000000000000000000, 0.2128009952263601179, -0.9770955615653315052 ) ) ;
#118164 = DIRECTION ( 'NONE',  ( 1.000000000000000000, 3.265361837132813093E-16, -0.000000000000000000 ) ) ;
#118166 = CARTESIAN_POINT ( 'NONE',  ( -18.40000000000000213, 11.47316190337364183, -158.1740539331920559 ) ) ;
#118167 = LINE ( 'NONE', #119463, #248368 ) ;
#118168 = CIRCLE ( 'NONE', #238404, 2.000000000000013323 ) ;
#118169 = DIRECTION ( 'NONE',  ( -0.000000000000000000, 0.1298341882520054891, 0.9915357197604850459 ) ) ;
#118170 = AXIS2_PLACEMENT_3D ( 'NONE', #69668, #249583, #70968 ) ;
#118171 = DIRECTION ( 'NONE',  ( -0.000000000000000000, -0.000000000000000000, 1.000000000000000000 ) ) ;
#118172 = AXIS2_PLACEMENT_3D ( 'NONE', #93093, #153124, #134770 ) ;
#118173 = ORIENTED_EDGE ( 'NONE', *, *, #27920, .T. ) ;
#118174 = ORIENTED_EDGE ( 'NONE', *, *, #155855, .T. ) ;
#118175 = DIRECTION ( 'NONE',  ( 1.000000000000000000, 0.000000000000000000, 0.000000000000000000 ) ) ;
#118177 = VERTEX_POINT ( 'NONE', #129314 ) ;
#118176 = CARTESIAN_POINT ( 'NONE',  ( -21.07928932188134041, 0.000000000000000000, 0.000000000000000000 ) ) ;
#118178 = ORIENTED_EDGE ( 'NONE', *, *, #219735, .F. ) ;
#118179 = ADVANCED_FACE ( 'NONE', ( #206285 ), #210148, .T. ) ;
#118180 = CYLINDRICAL_SURFACE ( 'NONE', #185159, 0.09999999999999781286 ) ;
#118181 = ORIENTED_EDGE ( 'NONE', *, *, #9014, .F. ) ;
#118182 = CARTESIAN_POINT ( 'NONE',  ( 20.95159278453404283, 8.907896337949049226, -8.484720185109249968 ) ) ;
#118183 = ORIENTED_EDGE ( 'NONE', *, *, #256461, .F. ) ;
#118184 = SURFACE_STYLE_FILL_AREA ( #236835 ) ;
#118185 = DIRECTION ( 'NONE',  ( 2.952720810173289112E-16, 1.000000000000000000, 6.530723674265620862E-15 ) ) ;
#118187 = ORIENTED_EDGE ( 'NONE', *, *, #129444, .T. ) ;
#118186 = ORIENTED_EDGE ( 'NONE', *, *, #237494, .T. ) ;
#118188 = ORIENTED_EDGE ( 'NONE', *, *, #38892, .F. ) ;
#118189 = ORIENTED_EDGE ( 'NONE', *, *, #19973, .T. ) ;
#118190 = AXIS2_PLACEMENT_3D ( 'NONE', #182542, #80831, #143389 ) ;
#118191 = CARTESIAN_POINT ( 'NONE',  ( -16.87036670365548474, 30.33914847462231279, -234.8334748671511818 ) ) ;
#118193 = ORIENTED_EDGE ( 'NONE', *, *, #12018, .T. ) ;
#118192 = LINE ( 'NONE', #158630, #175101 ) ;
#118194 = EDGE_CURVE ( 'NONE', #123343, #35945, #128888, .T. ) ;
#118195 = EDGE_CURVE ( 'NONE', #159618, #152369, #10655, .T. ) ;
#118196 = DIRECTION ( 'NONE',  ( -1.000000000000000000, 0.000000000000000000, 0.000000000000000000 ) ) ;
#118197 = CARTESIAN_POINT ( 'NONE',  ( 15.74999999999999645, 12.70026017068886226, -215.3766613508543628 ) ) ;
#118199 = ORIENTED_EDGE ( 'NONE', *, *, #125511, .T. ) ;
#118198 = FACE_OUTER_BOUND ( 'NONE', #55796, .T. ) ;
#118200 = CARTESIAN_POINT ( 'NONE',  ( -23.25000000000000000, 64.35000000001275566, -215.2731074845244450 ) ) ;
#118201 = EDGE_LOOP ( 'NONE', ( #19480, #138196, #9586, #143983 ) ) ;
#118202 = CARTESIAN_POINT ( 'NONE',  ( -18.79999999999999716, -10.84999999999999076, 33.00000000000000000 ) ) ;
#118204 = VERTEX_POINT ( 'NONE', #113385 ) ;
#118203 = LINE ( 'NONE', #214728, #101944 ) ;
#118205 = DIRECTION ( 'NONE',  ( 0.000000000000000000, 0.2128009952263403282, -0.9770955615653358350 ) ) ;
#118206 = CARTESIAN_POINT ( 'NONE',  ( 20.94999999999999574, 1.750000000011155743, -78.66951155790169992 ) ) ;
#118208 = EDGE_CURVE ( 'NONE', #169303, #155471, #235882, .T. ) ;
#118207 = CARTESIAN_POINT ( 'NONE',  ( 20.94999999999999929, 11.65000000001116121, -60.21613433702191287 ) ) ;
#118209 = ORIENTED_EDGE ( 'NONE', *, *, #162551, .F. ) ;
#118211 = DIRECTION ( 'NONE',  ( 0.000000000000000000, -0.9998779222360104635, -0.01562499999996343723 ) ) ;
#118210 = CARTESIAN_POINT ( 'NONE',  ( -16.84793658983426212, 9.950000000011137047, -46.23364667781012116 ) ) ;
#118212 = CARTESIAN_POINT ( 'NONE',  ( -21.05000000000000071, 7.128833340093095217, -233.7327013124392749 ) ) ;
#118213 = AXIS2_PLACEMENT_3D ( 'NONE', #120074, #116211, #37961 ) ;
#118214 = CARTESIAN_POINT ( 'NONE',  ( 22.14074124539698829, 7.390077851054901892, -133.9009471041559607 ) ) ;
#118215 = TOROIDAL_SURFACE ( 'NONE', #51535, 3.899999999999999467, 0.1000000000000000056 ) ;
#118216 = DIRECTION ( 'NONE',  ( 3.616040088954490704E-32, 7.105427357601001859E-15, -1.000000000000000000 ) ) ;
#118217 = CYLINDRICAL_SURFACE ( 'NONE', #35055, 0.1000000000000028644 ) ;
#118218 = EDGE_LOOP ( 'NONE', ( #58444, #221666, #71311, #188113 ) ) ;
#118220 = EDGE_LOOP ( 'NONE', ( #242206, #182995, #129955, #10665 ) ) ;
#118219 = VECTOR ( 'NONE', #124015, 1000.000000000000000 ) ;
#118221 = ORIENTED_EDGE ( 'NONE', *, *, #134470, .T. ) ;
#118222 = LINE ( 'NONE', #218580, #96996 ) ;
#118223 = ORIENTED_EDGE ( 'NONE', *, *, #250161, .T. ) ;
#118224 = DIRECTION ( 'NONE',  ( 0.000000000000000000, -0.9915357197604853789, 0.1298341882520022694 ) ) ;
#118225 = VERTEX_POINT ( 'NONE', #195514 ) ;
#118226 = DIRECTION ( 'NONE',  ( 0.000000000000000000, 0.9126074666063769270, 0.4088369013363280513 ) ) ;
#118227 = DIRECTION ( 'NONE',  ( 1.000000000000000000, 0.000000000000000000, 0.000000000000000000 ) ) ;
#118228 = ORIENTED_EDGE ( 'NONE', *, *, #30815, .T. ) ;
#118229 = DIRECTION ( 'NONE',  ( 0.000000000000000000, -0.000000000000000000, 1.000000000000000000 ) ) ;
#118230 = AXIS2_PLACEMENT_3D ( 'NONE', #196527, #158726, #175714 ) ;
#118231 = VERTEX_POINT ( 'NONE', #15595 ) ;
#118232 = VERTEX_POINT ( 'NONE', #174693 ) ;
#118233 = AXIS2_PLACEMENT_3D ( 'NONE', #213321, #231634, #52971 ) ;
#118234 = ORIENTED_EDGE ( 'NONE', *, *, #174697, .F. ) ;
#118235 = VECTOR ( 'NONE', #61033, 999.9999999999998863 ) ;
#118236 = ADVANCED_FACE ( 'NONE', ( #211196 ), #148413, .T. ) ;
#118237 = DIRECTION ( 'NONE',  ( 0.000000000000000000, -0.1350103645451904977, -0.9908441862701596881 ) ) ;
#118238 = CARTESIAN_POINT ( 'NONE',  ( -18.40000000000000213, 64.51332499825466016, -160.7731074845244450 ) ) ;
#118239 = DIRECTION ( 'NONE',  ( 1.000000000000000000, 0.000000000000000000, 0.000000000000000000 ) ) ;
#118240 = ADVANCED_FACE ( 'NONE', ( #232064 ), #128702, .F. ) ;
#118241 = CARTESIAN_POINT ( 'NONE',  ( 20.94999999999999929, 5.000000000011153745, -122.0947339810869465 ) ) ;
#118243 = DIRECTION ( 'NONE',  ( -2.952720810173289112E-16, -0.4088369013363282733, 0.9126074666063769270 ) ) ;
#118242 = CARTESIAN_POINT ( 'NONE',  ( -20.54999999999999716, 7.150000000011155876, -112.8500000000000369 ) ) ;
#118244 = CARTESIAN_POINT ( 'NONE',  ( -21.05000000000000071, -1.162701749926853712, -41.60000000000000142 ) ) ;
#118246 = ORIENTED_EDGE ( 'NONE', *, *, #239912, .T. ) ;
#118245 = DIRECTION ( 'NONE',  ( 1.000000000000000000, 0.000000000000000000, 0.000000000000000000 ) ) ;
#118247 = DIRECTION ( 'NONE',  ( 0.000000000000000000, 0.000000000000000000, -1.000000000000000000 ) ) ;
#118248 = ORIENTED_EDGE ( 'NONE', *, *, #60994, .F. ) ;
#118249 = ADVANCED_FACE ( 'NONE', ( #115959 ), #216158, .F. ) ;
#118250 = CARTESIAN_POINT ( 'NONE',  ( -18.43599941264915998, -9.519327428583796546, -140.9729767895211126 ) ) ;
#118251 = ADVANCED_FACE ( 'NONE', ( #216321 ), #14310, .F. ) ;
#118252 = EDGE_LOOP ( 'NONE', ( #241337, #44804, #132843, #179957, #48365, #105367, #197003 ) ) ;
#118253 = ORIENTED_EDGE ( 'NONE', *, *, #116697, .F. ) ;
#118254 = DIRECTION ( 'NONE',  ( -1.000000000000000000, 0.000000000000000000, 0.000000000000000000 ) ) ;
#118256 = AXIS2_PLACEMENT_3D ( 'NONE', #219558, #140012, #40967 ) ;
#118255 = DIRECTION ( 'NONE',  ( 0.000000000000000000, 0.000000000000000000, -1.000000000000000000 ) ) ;
#118257 = DIRECTION ( 'NONE',  ( -1.646408749285562691E-14, -0.4088369013363281068, 0.9126074666063770380 ) ) ;
#118258 = VECTOR ( 'NONE', #223984, 1000.000000000000227 ) ;
#118259 = VERTEX_POINT ( 'NONE', #233356 ) ;
#118260 = VECTOR ( 'NONE', #247924, 1000.000000000000114 ) ;
#118261 = AXIS2_PLACEMENT_3D ( 'NONE', #168807, #50084, #69676 ) ;
#118262 = ADVANCED_FACE ( 'NONE', ( #213766 ), #24672, .T. ) ;
#118263 = DIRECTION ( 'NONE',  ( 1.000000000000000000, 0.000000000000000000, 0.000000000000000000 ) ) ;
#118265 = EDGE_CURVE ( 'NONE', #6907, #43706, #195353, .T. ) ;
#118264 = ADVANCED_FACE ( 'NONE', ( #114665 ), #75566, .F. ) ;
#118266 = ORIENTED_EDGE ( 'NONE', *, *, #55261, .F. ) ;
#118267 = VERTEX_POINT ( 'NONE', #166334 ) ;
#118268 = AXIS2_PLACEMENT_3D ( 'NONE', #180028, #176182, #1355 ) ;
#118269 = CARTESIAN_POINT ( 'NONE',  ( -23.15000000000000213, 0.8618440306782485516, -204.9572370243411115 ) ) ;
#118270 = ORIENTED_EDGE ( 'NONE', *, *, #237370, .F. ) ;
#118271 = CARTESIAN_POINT ( 'NONE',  ( 19.97071067811864609, 64.27928932189330169, -111.8731074845243825 ) ) ;
#118272 = ORIENTED_EDGE ( 'NONE', *, *, #243309, .F. ) ;
#118273 = PLANE ( 'NONE',  #78095 ) ;
#118274 = EDGE_CURVE ( 'NONE', #61430, #167205, #12199, .T. ) ;
#118275 = DIRECTION ( 'NONE',  ( 0.000000000000000000, 0.000000000000000000, 1.000000000000000000 ) ) ;
#118276 = DIRECTION ( 'NONE',  ( -1.000000000000000000, 3.469446951953635015E-14, 0.000000000000000000 ) ) ;
#118277 = ORIENTED_EDGE ( 'NONE', *, *, #16924, .T. ) ;
#118278 = AXIS2_PLACEMENT_3D ( 'NONE', #87302, #166893, #28680 ) ;
#118279 = CIRCLE ( 'NONE', #226579, 0.1000000000000028644 ) ;
#118280 = CIRCLE ( 'NONE', #222478, 0.2000000000000057288 ) ;
#118281 = FACE_OUTER_BOUND ( 'NONE', #167070, .T. ) ;
#118282 = ADVANCED_FACE ( 'NONE', ( #101468 ), #199631, .F. ) ;
#118283 = CYLINDRICAL_SURFACE ( 'NONE', #125028, 0.09999999999999939493 ) ;
#118284 = DIRECTION ( 'NONE',  ( 0.000000000000000000, 0.9955484899852913294, -0.09425075112701486457 ) ) ;
#118285 = EDGE_CURVE ( 'NONE', #181023, #202644, #49936, .T. ) ;
#118286 = ADVANCED_FACE ( 'NONE', ( #1105 ), #120703, .T. ) ;
#118287 = ORIENTED_EDGE ( 'NONE', *, *, #212836, .F. ) ;
#118288 = EDGE_CURVE ( 'NONE', #209903, #119379, #138060, .T. ) ;
#118290 = ORIENTED_EDGE ( 'NONE', *, *, #9305, .F. ) ;
#118289 = DIRECTION ( 'NONE',  ( 1.000000000000000000, 0.000000000000000000, 0.000000000000000000 ) ) ;
#118291 = ORIENTED_EDGE ( 'NONE', *, *, #177525, .T. ) ;
#118292 = CARTESIAN_POINT ( 'NONE',  ( 20.12499999999999645, 18.87266177492467278, -229.5208838261441713 ) ) ;
#118293 = FACE_OUTER_BOUND ( 'NONE', #39352, .T. ) ;
#118294 = SPHERICAL_SURFACE ( 'NONE', #229606, 0.1000000000000000056 ) ;
#118295 = EDGE_CURVE ( 'NONE', #20544, #225270, #79367, .T. ) ;
#118296 = DIRECTION ( 'NONE',  ( -3.265361837132813093E-16, -1.000000000000000000, 7.445645354460596589E-46 ) ) ;
#118297 = CARTESIAN_POINT ( 'NONE',  ( -16.89318236219977010, 9.951535257886288122, -46.14487036789414276 ) ) ;
#118298 = CARTESIAN_POINT ( 'NONE',  ( -16.87435696428308063, 66.04999753707983245, -123.8731157193577985 ) ) ;
#118299 = ORIENTED_EDGE ( 'NONE', *, *, #79105, .F. ) ;
#118300 = DIRECTION ( 'NONE',  ( 0.000000000000000000, -1.000000000000000000, -6.982962677686265922E-15 ) ) ;
#118301 = CIRCLE ( 'NONE', #172511, 11.90000000000000036 ) ;
#118302 = CARTESIAN_POINT ( 'NONE',  ( -16.81095280782810875, 9.950000000011138823, -146.6499999999991530 ) ) ;
#118304 = EDGE_CURVE ( 'NONE', #69522, #34828, #219979, .T. ) ;
#118303 = CARTESIAN_POINT ( 'NONE',  ( -18.48408745364668349, 77.28143348823819281, -241.9425700404712529 ) ) ;
#118305 = CYLINDRICAL_SURFACE ( 'NONE', #225526, 0.1000000000000028644 ) ;
#118306 = VECTOR ( 'NONE', #101310, 1000.000000000000000 ) ;
#118307 = CARTESIAN_POINT ( 'NONE',  ( 20.94999999999999929, 1.148907358139439339E-11, -201.0000000000015064 ) ) ;
#118308 =( BOUNDED_SURFACE ( )  B_SPLINE_SURFACE ( 3, 2, ( 
 ( #122949, #82494, #182931 ),
 ( #242882, #198614, #202480 ),
 ( #39586, #119093, #162086 ),
 ( #241601, #120411, #163359 ),
 ( #85057, #159512, #25145 ),
 ( #20006, #223304, #164643 ) ),
 .UNSPECIFIED., .F., .F., .T. ) 
 B_SPLINE_SURFACE_WITH_KNOTS ( ( 4, 2, 4 ),
 ( 3, 3 ),
 ( 0.0001792624049599557520, 0.0003686986002124449983, 0.0005581347954649342174 ),
 ( 0.000000000000000000, 1.000000000000000000 ),
 .UNSPECIFIED. ) 
 GEOMETRIC_REPRESENTATION_ITEM ( )  RATIONAL_B_SPLINE_SURFACE ( (
 ( 1.000000000000000000, 0.9238795325112856283, 1.000000000000000000),
 ( 1.000000000000000000, 0.9229318695239514536, 1.000000000000000000),
 ( 1.000000000000000000, 0.8926288119229253137, 1.000000000000000000),
 ( 1.000000000000000000, 0.8123777807272960505, 1.000000000000000000),
 ( 1.000000000000000000, 0.7629087100930475041, 1.000000000000000000),
 ( 1.000000000000000000, 0.7071067811865475727, 1.000000000000000000) ) ) 
 REPRESENTATION_ITEM ( '' )  SURFACE ( )  );
#118309 = ORIENTED_EDGE ( 'NONE', *, *, #34428, .T. ) ;
#118310 = ORIENTED_EDGE ( 'NONE', *, *, #60038, .F. ) ;
#118311 = CARTESIAN_POINT ( 'NONE',  ( -20.93284271247462414, 64.25000000001196554, -110.0379132551783243 ) ) ;
#118312 = VECTOR ( 'NONE', #95941, 1000.000000000000000 ) ;
#118313 = CARTESIAN_POINT ( 'NONE',  ( -23.15000000000000213, 76.00000000001190870, -103.0231074845243029 ) ) ;
#118314 = CARTESIAN_POINT ( 'NONE',  ( -21.05000000000000426, 69.72991413632355773, -203.5579754875374761 ) ) ;
#118315 = CIRCLE ( 'NONE', #109909, 7.799999999999999822 ) ;
#118316 = DIRECTION ( 'NONE',  ( 0.000000000000000000, 0.2617529984165306578, 0.9651348961777082014 ) ) ;
#118317 = ADVANCED_FACE ( 'NONE', ( #19422 ), #67196, .T. ) ;
#118318 = ORIENTED_EDGE ( 'NONE', *, *, #147899, .F. ) ;
#118319 = DIRECTION ( 'NONE',  ( 1.000000000000000000, 6.938893903907222067E-15, 0.000000000000000000 ) ) ;
#118320 = VECTOR ( 'NONE', #228970, 1000.000000000000114 ) ;
#118321 = B_SPLINE_CURVE_WITH_KNOTS ( 'NONE', 3,
 ( #232692, #31934, #90580, #250933, #52742, #111442, #91875, #168891, #12369, #248389 ),
 .UNSPECIFIED., .F., .F.,
 ( 4, 2, 2, 2, 4 ),
 ( 0.000000000000000000, 0.0001584437871625036642, 0.0002376656807437575833, 0.0002772766275343837433, 0.0003168875743250099304 ),
 .UNSPECIFIED. ) ;
#118323 = CIRCLE ( 'NONE', #164303, 0.09999999999999939493 ) ;
#118322 = DIRECTION ( 'NONE',  ( 1.000000000000000000, 0.000000000000000000, 0.000000000000000000 ) ) ;
#118324 = ORIENTED_EDGE ( 'NONE', *, *, #129573, .F. ) ;
#118325 = DIRECTION ( 'NONE',  ( 0.000000000000000000, -0.4088369013363783999, 0.9126074666063545004 ) ) ;
#118326 = CIRCLE ( 'NONE', #139121, 0.1000000000000028644 ) ;
#118327 = CIRCLE ( 'NONE', #5861, 12.87500000000000000 ) ;
#118328 = PRODUCT_DEFINITION_SHAPE ( 'NONE', 'NONE',  #258128 ) ;
#118329 = DIRECTION ( 'NONE',  ( 0.000000000000000000, 0.000000000000000000, 1.000000000000000000 ) ) ;
#118330 = AXIS2_PLACEMENT_3D ( 'NONE', #246102, #50429, #49169 ) ;
#118331 = EDGE_LOOP ( 'NONE', ( #79359, #149459, #40080, #150120 ) ) ;
#118332 = CARTESIAN_POINT ( 'NONE',  ( -23.25000000000000000, 76.00000000001213607, -136.5231074845242745 ) ) ;
#118333 = VERTEX_POINT ( 'NONE', #177235 ) ;
#118334 = DIRECTION ( 'NONE',  ( 0.000000000000000000, 0.000000000000000000, -1.000000000000000000 ) ) ;
#118335 = CARTESIAN_POINT ( 'NONE',  ( 18.60000000000000142, -9.321008403361283001, -7.235938249077890738 ) ) ;
#118337 = VECTOR ( 'NONE', #142647, 1000.000000000000000 ) ;
#118336 = CARTESIAN_POINT ( 'NONE',  ( -21.05000000000000071, 74.16465844978745281, -91.36795619196134055 ) ) ;
#118338 = DIRECTION ( 'NONE',  ( 0.000000000000000000, 0.2617529984165033463, 0.9651348961777157509 ) ) ;
#118339 = DIRECTION ( 'NONE',  ( -2.978066053179066272E-16, -1.000000000000000000, -8.338584948901384773E-15 ) ) ;
#118340 = CARTESIAN_POINT ( 'NONE',  ( 21.05000000000000071, 18.75112661735452591, -228.0439950614670011 ) ) ;
#118341 = CARTESIAN_POINT ( 'NONE',  ( -23.25000000000000000, 2.000000000011154189, -188.3753780772378548 ) ) ;
#118342 = CARTESIAN_POINT ( 'NONE',  ( -18.59999999999999787, -9.480686695267820596, -107.4411151687578894 ) ) ;
#118343 = CARTESIAN_POINT ( 'NONE',  ( -20.54999999999999716, 84.66355140188063899, -45.54720860259156723 ) ) ;
#118344 = AXIS2_PLACEMENT_3D ( 'NONE', #196411, #38633, #137706 ) ;
#118345 = ADVANCED_FACE ( 'NONE', ( #106296 ), #62396, .T. ) ;
#118346 = CARTESIAN_POINT ( 'NONE',  ( 18.49505832270841310, -7.690013074335040777, -210.0420179539718504 ) ) ;
#118347 = CARTESIAN_POINT ( 'NONE',  ( -22.94999999999999929, 4.513204987021263825, 22.10000000000000142 ) ) ;
#118348 = EDGE_CURVE ( 'NONE', #100439, #42095, #187331, .T. ) ;
#118349 = CIRCLE ( 'NONE', #5884, 11.79999999999999716 ) ;
#118350 = CARTESIAN_POINT ( 'NONE',  ( 21.08804281139606474, 10.62183430185231892, -79.34999996737887784 ) ) ;
#118351 = CARTESIAN_POINT ( 'NONE',  ( 21.14999999999999858, 33.98486250090727623, -243.5821103306120108 ) ) ;
#118352 = AXIS2_PLACEMENT_3D ( 'NONE', #114927, #174956, #13270 ) ;
#118353 = AXIS2_PLACEMENT_3D ( 'NONE', #72468, #29511, #88125 ) ;
#118354 = ORIENTED_EDGE ( 'NONE', *, *, #101204, .T. ) ;
#118355 = DIRECTION ( 'NONE',  ( -4.336808689942052446E-15, 0.8660254037844445918, 0.4999999999999896194 ) ) ;
#118357 = ADVANCED_FACE ( 'NONE', ( #257974 ), #158955, .T. ) ;
#118356 = CARTESIAN_POINT ( 'NONE',  ( -17.11825945287481332, 65.95000000001152785, -48.67310748452439384 ) ) ;
#118358 = CARTESIAN_POINT ( 'NONE',  ( 20.50589344625181809, 10.48318793148705019, -41.07299497867204252 ) ) ;
#118359 = EDGE_CURVE ( 'NONE', #150841, #120381, #241041, .T. ) ;
#118360 =( BOUNDED_SURFACE ( )  B_SPLINE_SURFACE ( 3, 2, ( 
 ( #220658, #185375, #66717 ),
 ( #107114, #186674, #142391 ),
 ( #8036, #87538, #181545 ),
 ( #221904, #65421, #241501 ),
 ( #143672, #184087, #167129 ),
 ( #43306, #122849, #5421 ) ),
 .UNSPECIFIED., .F., .F., .F. ) 
 B_SPLINE_SURFACE_WITH_KNOTS ( ( 4, 2, 4 ),
 ( 3, 3 ),
 ( 0.0001792624049599680035, 0.0003686986002124869027, 0.0005581347954650057747 ),
 ( 0.000000000000000000, 1.000000000000000000 ),
 .UNSPECIFIED. ) 
 GEOMETRIC_REPRESENTATION_ITEM ( )  RATIONAL_B_SPLINE_SURFACE ( (
 ( 1.000000000000000000, 0.9238795325112821866, 1.000000000000000000),
 ( 1.000000000000000000, 0.9229318695238644121, 1.000000000000000000),
 ( 1.000000000000000000, 0.8926288119230598728, 1.000000000000000000),
 ( 1.000000000000000000, 0.8123777807271286289, 1.000000000000000000),
 ( 1.000000000000000000, 0.7629087100931351006, 1.000000000000000000),
 ( 1.000000000000000000, 0.7071067811865610064, 1.000000000000000000) ) ) 
 REPRESENTATION_ITEM ( '' )  SURFACE ( )  );
#118361 = EDGE_LOOP ( 'NONE', ( #182054, #211063, #196256, #27029 ) ) ;
#118362 = CARTESIAN_POINT ( 'NONE',  ( -23.25000000000000355, 70.35000000001232934, -160.7731074845243882 ) ) ;
#118363 = VERTEX_POINT ( 'NONE', #59796 ) ;
#118364 = FACE_OUTER_BOUND ( 'NONE', #156252, .T. ) ;
#118365 = DIRECTION ( 'NONE',  ( -1.000000000000000000, -0.000000000000000000, 0.000000000000000000 ) ) ;
#118366 = ORIENTED_EDGE ( 'NONE', *, *, #11028, .F. ) ;
#118367 = AXIS2_PLACEMENT_3D ( 'NONE', #34703, #13837, #232907 ) ;
#118368 = AXIS2_PLACEMENT_3D ( 'NONE', #105966, #40917, #100809 ) ;
#118369 = EDGE_CURVE ( 'NONE', #208842, #160579, #86732, .T. ) ;
#118370 = ORIENTED_EDGE ( 'NONE', *, *, #182440, .F. ) ;
#118371 = DIRECTION ( 'NONE',  ( 1.000000000000000000, 0.000000000000000000, 0.000000000000000000 ) ) ;
#118372 = ORIENTED_EDGE ( 'NONE', *, *, #34693, .T. ) ;
#118373 = CARTESIAN_POINT ( 'NONE',  ( -21.04999999999994387, 64.35000000001120668, -51.02310748452479316 ) ) ;
#118374 = DIRECTION ( 'NONE',  ( 0.000000000000000000, 6.982962677686266711E-15, -1.000000000000000000 ) ) ;
#118376 = DIRECTION ( 'NONE',  ( -1.000000000000000000, -3.190570557967288949E-16, -6.948722487160392945E-17 ) ) ;
#118375 = UNCERTAINTY_MEASURE_WITH_UNIT (LENGTH_MEASURE( 1.000000000000000082E-05 ), #194642, 'distance_accuracy_value', 'NONE');
#118377 = FACE_OUTER_BOUND ( 'NONE', #219879, .T. ) ;
#118378 = PLANE ( 'NONE',  #147329 ) ;
#118379 = DIRECTION ( 'NONE',  ( 0.000000000000000000, 0.9126074666063844765, 0.4088369013363114535 ) ) ;
#118380 = DIRECTION ( 'NONE',  ( -0.000000000000000000, -1.000000000000000000, -6.982962677686266711E-15 ) ) ;
#118381 = CARTESIAN_POINT ( 'NONE',  ( -18.40000000000000213, 61.34848953995435039, -212.6564661897791098 ) ) ;
#118383 = VERTEX_POINT ( 'NONE', #226234 ) ;
#118382 = CARTESIAN_POINT ( 'NONE',  ( -18.49999999999997868, -9.321008403350143467, -40.73593824907786853 ) ) ;
#118384 = ORIENTED_EDGE ( 'NONE', *, *, #130032, .T. ) ;
#118386 = CARTESIAN_POINT ( 'NONE',  ( -21.05000000000000071, 64.35000000001161879, -62.73924182154625129 ) ) ;
#118385 = LINE ( 'NONE', #42685, #70338 ) ;
#118389 = ORIENTED_EDGE ( 'NONE', *, *, #65338, .F. ) ;
#118388 = CARTESIAN_POINT ( 'NONE',  ( -16.97683810757273193, 61.09996331030407646, -220.4495434389081367 ) ) ;
#118387 = CARTESIAN_POINT ( 'NONE',  ( 21.05000000000000071, 36.65892442174935439, -249.5511627012433848 ) ) ;
#118390 = ORIENTED_EDGE ( 'NONE', *, *, #88772, .F. ) ;
#118391 = EDGE_CURVE ( 'NONE', #50939, #140576, #8262, .T. ) ;
#118392 = FACE_OUTER_BOUND ( 'NONE', #67038, .T. ) ;
#118393 = CARTESIAN_POINT ( 'NONE',  ( -23.15000000000000213, 11.75000000001115552, -88.75000000000004263 ) ) ;
#118394 = AXIS2_PLACEMENT_3D ( 'NONE', #128346, #72230, #33134 ) ;
#118395 = CARTESIAN_POINT ( 'NONE',  ( -21.04999999999994387, 83.97335046823651794, -34.66234602115918051 ) ) ;
#118396 = DIRECTION ( 'NONE',  ( 0.000000000000000000, 0.000000000000000000, -1.000000000000000000 ) ) ;
#118397 = CARTESIAN_POINT ( 'NONE',  ( -21.14999999999994174, 76.00000000001119815, -36.02310748452479316 ) ) ;
#118398 = CYLINDRICAL_SURFACE ( 'NONE', #147921, 0.09999999999999939493 ) ;
#118400 = ADVANCED_FACE ( 'NONE', ( #218879 ), #40299, .T. ) ;
#118399 = CARTESIAN_POINT ( 'NONE',  ( -20.85000000000000142, 77.16412189325286874, -61.60825939895269698 ) ) ;
#118401 = EDGE_CURVE ( 'NONE', #111741, #196055, #154052, .T. ) ;
#118402 = CARTESIAN_POINT ( 'NONE',  ( 21.00000000000000000, 14.04870287383362992, -219.6884709798077893 ) ) ;
#118403 = EDGE_LOOP ( 'NONE', ( #254368, #48938, #242614, #28589 ) ) ;
#118404 = ORIENTED_EDGE ( 'NONE', *, *, #233841, .F. ) ;
#118405 = FACE_OUTER_BOUND ( 'NONE', #13787, .T. ) ;
#118406 = AXIS2_PLACEMENT_3D ( 'NONE', #109444, #246411, #50742 ) ;
#118407 = VECTOR ( 'NONE', #157518, 1000.000000000000000 ) ;
#118408 = ORIENTED_EDGE ( 'NONE', *, *, #134569, .T. ) ;
#118409 = VERTEX_POINT ( 'NONE', #52753 ) ;
#118410 = LINE ( 'NONE', #195396, #39153 ) ;
#118411 = AXIS2_PLACEMENT_3D ( 'NONE', #96411, #13069, #213811 ) ;
#118412 = AXIS2_PLACEMENT_3D ( 'NONE', #122379, #217596, #235889 ) ;
#118413 = EDGE_CURVE ( 'NONE', #10339, #39830, #140593, .T. ) ;
#118414 = CARTESIAN_POINT ( 'NONE',  ( 21.05000000000000071, 1.115600667400684642E-11, -167.4999999999999716 ) ) ;
#118415 = PLANE ( 'NONE',  #134578 ) ;
#118416 = CARTESIAN_POINT ( 'NONE',  ( 18.54286124688534088, -9.623917578786652882, -207.7412023318626666 ) ) ;
#118417 = EDGE_CURVE ( 'NONE', #173202, #40449, #191455, .T. ) ;
#118418 = DIRECTION ( 'NONE',  ( 1.000000000000000000, -0.000000000000000000, 0.000000000000000000 ) ) ;
#118419 = ORIENTED_EDGE ( 'NONE', *, *, #161274, .F. ) ;
#118420 = ADVANCED_FACE ( 'NONE', ( #13645 ), #210564, .F. ) ;
#118421 = CARTESIAN_POINT ( 'NONE',  ( -20.85000000000000142, 87.65000000001171543, -69.52310748452423184 ) ) ;
#118422 = CARTESIAN_POINT ( 'NONE',  ( 21.14999999999999858, 6.650000000011155876, -146.1500000000000341 ) ) ;
#118423 = FACE_OUTER_BOUND ( 'NONE', #45960, .T. ) ;
#118425 = AXIS2_PLACEMENT_3D ( 'NONE', #31511, #207563, #91456 ) ;
#118424 = LINE ( 'NONE', #135391, #13031 ) ;
#118426 = EDGE_CURVE ( 'NONE', #118817, #83582, #62427, .T. ) ;
#118427 = CARTESIAN_POINT ( 'NONE',  ( -20.94999999999999929, -4.254329952141550741, -236.2118329068272260 ) ) ;
#118428 = ORIENTED_EDGE ( 'NONE', *, *, #16237, .F. ) ;
#118429 = DIRECTION ( 'NONE',  ( 0.000000000000000000, 0.000000000000000000, -1.000000000000000000 ) ) ;
#118431 = VERTEX_POINT ( 'NONE', #91888 ) ;
#118430 = AXIS2_PLACEMENT_3D ( 'NONE', #209933, #170845, #191670 ) ;
#118434 = EDGE_LOOP ( 'NONE', ( #95375, #198696, #101787, #41875 ) ) ;
#118433 = DIRECTION ( 'NONE',  ( 0.000000000000000000, 0.9887567792719329507, 0.1495327102803732933 ) ) ;
#118432 = DIRECTION ( 'NONE',  ( 0.000000000000000000, -6.938893903907222067E-15, 1.000000000000000000 ) ) ;
#118435 = DIRECTION ( 'NONE',  ( 0.000000000000000000, 1.000000000000000000, 0.000000000000000000 ) ) ;
#118436 = AXIS2_PLACEMENT_3D ( 'NONE', #58086, #257534, #159797 ) ;
#118437 = AXIS2_PLACEMENT_3D ( 'NONE', #221082, #84095, #22923 ) ;
#118438 = DIRECTION ( 'NONE',  ( -1.000000000000000000, 0.000000000000000000, 0.000000000000000000 ) ) ;
#118439 = ORIENTED_EDGE ( 'NONE', *, *, #45036, .F. ) ;
#118440 = DIRECTION ( 'NONE',  ( 0.000000000000000000, 1.000000000000000000, 0.000000000000000000 ) ) ;
#118441 = ADVANCED_FACE ( 'NONE', ( #231422 ), #28098, .F. ) ;
#118442 = CARTESIAN_POINT ( 'NONE',  ( 20.04999999999999716, 8.750000000011173285, -76.25000000000004263 ) ) ;
#118443 = DIRECTION ( 'NONE',  ( -1.000000000000000000, 0.000000000000000000, 0.000000000000000000 ) ) ;
#118445 = VERTEX_POINT ( 'NONE', #72351 ) ;
#118444 = LINE ( 'NONE', #61012, #39376 ) ;
#118446 = CIRCLE ( 'NONE', #180981, 0.5000000000000004441 ) ;
#118447 = AXIS2_PLACEMENT_3D ( 'NONE', #78246, #140804, #237341 ) ;
#118448 = CARTESIAN_POINT ( 'NONE',  ( 21.05000000000000071, 71.00000000001253397, -182.4283735034374843 ) ) ;
#118449 = VECTOR ( 'NONE', #185737, 1000.000000000000000 ) ;
#118450 = ORIENTED_EDGE ( 'NONE', *, *, #239262, .F. ) ;
#118451 = DIRECTION ( 'NONE',  ( 4.377807931758639578E-15, -0.2605042016806606298, -0.9654727137038736640 ) ) ;
#118452 = DIRECTION ( 'NONE',  ( 0.000000000000000000, 0.9876197685951252359, -0.1568667991644863424 ) ) ;
#118453 = VECTOR ( 'NONE', #187597, 1000.000000000000000 ) ;
#118454 = LINE ( 'NONE', #175867, #242026 ) ;
#118455 = B_SPLINE_CURVE_WITH_KNOTS ( 'NONE', 3,
 ( #82583, #145145, #203845, #5623, #42222, #22675, #202571, #61774, #222102, #167324, #25236, #102148, #103445, #183023, #43504, #63046, #164733, #224685, #46054 ),
 .UNSPECIFIED., .F., .F.,
 ( 4, 3, 3, 3, 3, 3, 4 ),
 ( 0.0001624081864585794055, 0.0001685232196531677375, 0.0001764526673566770378, 0.0001916878551483278104, 0.0002009890782182702088, 0.0002238845907555191150, 0.0002283406619926350520 ),
 .UNSPECIFIED. ) ;
#118456 = EDGE_LOOP ( 'NONE', ( #199103, #246427, #256588, #249734 ) ) ;
#118457 = DIRECTION ( 'NONE',  ( 0.000000000000000000, 0.9915357197604792727, -0.1298341882520475943 ) ) ;
#118458 = ORIENTED_EDGE ( 'NONE', *, *, #164619, .F. ) ;
#118459 = DIRECTION ( 'NONE',  ( -0.000000000000000000, -0.8096735173027155286, 0.5868805631290315850 ) ) ;
#118460 = CIRCLE ( 'NONE', #180996, 11.65000000000000213 ) ;
#118461 = DIRECTION ( 'NONE',  ( 0.000000000000000000, 0.9126074666063660468, 0.4088369013363524762 ) ) ;
#118462 = CARTESIAN_POINT ( 'NONE',  ( -21.65000000000000213, 12.05403912736948158, -220.1228874760914209 ) ) ;
#118463 = VERTEX_POINT ( 'NONE', #30665 ) ;
#118464 = CYLINDRICAL_SURFACE ( 'NONE', #100324, 0.1000000000000028644 ) ;
#118465 = AXIS2_PLACEMENT_3D ( 'NONE', #243504, #29630, #67434 ) ;
#118466 = AXIS2_PLACEMENT_3D ( 'NONE', #116150, #37907, #120019 ) ;
#118468 = AXIS2_PLACEMENT_3D ( 'NONE', #28239, #167743, #247236 ) ;
#118467 = CARTESIAN_POINT ( 'NONE',  ( 20.09999999999999787, 66.25000000001205080, -123.8731074845243683 ) ) ;
#118469 = CARTESIAN_POINT ( 'NONE',  ( -20.96428641294330220, 64.25000000001250555, -176.8482143065820651 ) ) ;
#118470 = B_SPLINE_CURVE_WITH_KNOTS ( 'NONE', 3,
 ( #105617, #165640, #24860, #226874, #204731, #46935, #28731, #84760, #221716, #146047, #143485, #163080, #23588 ),
 .UNSPECIFIED., .F., .F.,
 ( 4, 3, 3, 3, 4 ),
 ( 1.110764993427085326E-16, 1.946463881814652902E-05, 3.922356109943681788E-05, 4.215060953237600338E-05, 4.415117091092905685E-05 ),
 .UNSPECIFIED. ) ;
#118471 = ORIENTED_EDGE ( 'NONE', *, *, #97023, .T. ) ;
#118472 = CARTESIAN_POINT ( 'NONE',  ( -18.59999999999999787, 77.16270174995010223, -128.4231074845242802 ) ) ;
#118473 = CARTESIAN_POINT ( 'NONE',  ( 18.54999999999999716, 9.950000000011153034, -188.3500000000000227 ) ) ;
#118474 = CARTESIAN_POINT ( 'NONE',  ( 21.05000000000000071, 69.52293297888689949, -69.42310748452439384 ) ) ;
#118475 = EDGE_CURVE ( 'NONE', #226447, #137736, #208011, .T. ) ;
#118476 = VERTEX_POINT ( 'NONE', #211858 ) ;
#118477 = CARTESIAN_POINT ( 'NONE',  ( 20.94999999999999929, 1.115600667400684642E-11, -134.0000000000000284 ) ) ;
#118478 = VERTEX_POINT ( 'NONE', #228847 ) ;
#118480 = VERTEX_POINT ( 'NONE', #31950 ) ;
#118479 = CARTESIAN_POINT ( 'NONE',  ( -1.739115166359751801E-14, 11.65000000001114699, -125.3500000000000512 ) ) ;
#118481 = EDGE_CURVE ( 'NONE', #105103, #247138, #37308, .T. ) ;
#118484 = ORIENTED_EDGE ( 'NONE', *, *, #194826, .T. ) ;
#118483 = ORIENTED_EDGE ( 'NONE', *, *, #19334, .F. ) ;
#118482 = CARTESIAN_POINT ( 'NONE',  ( -21.14999999999999858, 0.000000000000000000, 6.540656951701240729 ) ) ;
#118485 = AXIS2_PLACEMENT_3D ( 'NONE', #183794, #23471, #123829 ) ;
#118486 = EDGE_CURVE ( 'NONE', #99209, #169022, #91465, .T. ) ;
#118487 = DIRECTION ( 'NONE',  ( -1.000000000000000000, -0.000000000000000000, -0.000000000000000000 ) ) ;
#118488 = EDGE_CURVE ( 'NONE', #196986, #215272, #174904, .T. ) ;
#118489 = DIRECTION ( 'NONE',  ( 1.000000000000000000, 1.186688945009009831E-16, 0.000000000000000000 ) ) ;
#118490 = AXIS2_PLACEMENT_3D ( 'NONE', #5169, #29928, #148571 ) ;
#118491 = CARTESIAN_POINT ( 'NONE',  ( -21.05000000000000071, 88.41227409416214300, -172.9231074845242802 ) ) ;
#118492 = DIRECTION ( 'NONE',  ( 0.000000000000000000, -0.1568667991644693838, -0.9876197685951279004 ) ) ;
#118493 = CARTESIAN_POINT ( 'NONE',  ( -22.50000000000000000, 7.128833340093095217, -233.7327013124392749 ) ) ;
#118494 = AXIS2_PLACEMENT_3D ( 'NONE', #131193, #171651, #210740 ) ;
#118495 = CARTESIAN_POINT ( 'NONE',  ( 21.05000000000000071, 5.000000000011153745, -155.5947339810869323 ) ) ;
#118497 = CARTESIAN_POINT ( 'NONE',  ( 18.59999999999999076, 11.65000000001115943, -192.2499999999999716 ) ) ;
#118496 = PLANE ( 'NONE',  #84381 ) ;
#118498 = ORIENTED_EDGE ( 'NONE', *, *, #64866, .F. ) ;
#118500 = EDGE_LOOP ( 'NONE', ( #33892, #84849, #143886, #210228 ) ) ;
#118499 = AXIS2_PLACEMENT_3D ( 'NONE', #104901, #68392, #29300 ) ;
#118501 = DIRECTION ( 'NONE',  ( 0.000000000000000000, 8.673617379884087537E-15, 1.000000000000000000 ) ) ;
#118502 = VECTOR ( 'NONE', #171817, 1000.000000000000000 ) ;
#118504 = ORIENTED_EDGE ( 'NONE', *, *, #192322, .T. ) ;
#118503 = DIRECTION ( 'NONE',  ( -0.000000000000000000, -0.000000000000000000, 1.000000000000000000 ) ) ;
#118505 = CARTESIAN_POINT ( 'NONE',  ( 20.94999999999999574, -10.60885044396467158, -206.2784744251879374 ) ) ;
#118506 = ORIENTED_EDGE ( 'NONE', *, *, #137583, .T. ) ;
#118507 = EDGE_CURVE ( 'NONE', #117253, #21796, #128149, .T. ) ;
#118508 = LINE ( 'NONE', #59767, #168649 ) ;
#118509 = VERTEX_POINT ( 'NONE', #179167 ) ;
#118510 = DIRECTION ( 'NONE',  ( 0.000000000000000000, 0.000000000000000000, -1.000000000000000000 ) ) ;
#118511 = CIRCLE ( 'NONE', #110102, 0.09999999999998898659 ) ;
#118512 = EDGE_CURVE ( 'NONE', #248655, #176779, #54035, .T. ) ;
#118513 = VECTOR ( 'NONE', #145579, 1000.000000000000000 ) ;
#118514 = EDGE_LOOP ( 'NONE', ( #181292, #154711, #152226, #54013 ) ) ;
#118515 = CIRCLE ( 'NONE', #114409, 0.2000000000000057288 ) ;
#118516 = DIRECTION ( 'NONE',  ( 0.000000000000000000, 0.9126074666064696306, 0.4088369013361213278 ) ) ;
#118517 = DIRECTION ( 'NONE',  ( 1.000000000000000000, 0.000000000000000000, -0.000000000000000000 ) ) ;
#118518 = AXIS2_PLACEMENT_3D ( 'NONE', #147240, #89822, #11604 ) ;
#118520 = ORIENTED_EDGE ( 'NONE', *, *, #214235, .F. ) ;
#118519 = EDGE_LOOP ( 'NONE', ( #951, #101859, #159938, #241431 ) ) ;
#118521 = ORIENTED_EDGE ( 'NONE', *, *, #251111, .F. ) ;
#118522 = CARTESIAN_POINT ( 'NONE',  ( 20.94999999999999929, 76.00000000001205080, -123.6481074845242887 ) ) ;
#118523 = EDGE_LOOP ( 'NONE', ( #124925, #200425, #205915, #151547, #160335 ) ) ;
#118524 = ORIENTED_EDGE ( 'NONE', *, *, #40939, .F. ) ;
#118525 = EDGE_CURVE ( 'NONE', #179315, #143470, #124782, .T. ) ;
#118526 = DIRECTION ( 'NONE',  ( 4.377807931758638789E-15, 0.2605042016806672911, 0.9654727137038716656 ) ) ;
#118528 = EDGE_LOOP ( 'NONE', ( #206903, #183107, #2592, #123087 ) ) ;
#118527 = CARTESIAN_POINT ( 'NONE',  ( 18.47135592147652972, -9.471088613254535105, -107.1835949398435019 ) ) ;
#118529 = EDGE_CURVE ( 'NONE', #236196, #253194, #18767, .T. ) ;
#118530 = EDGE_CURVE ( 'NONE', #98769, #195345, #166498, .T. ) ;
#118531 = CIRCLE ( 'NONE', #10379, 0.09999999999998898659 ) ;
#118533 = CARTESIAN_POINT ( 'NONE',  ( 20.95378194480896639, 65.46508800846955012, -162.4580533363765937 ) ) ;
#118532 = DIRECTION ( 'NONE',  ( 2.952720810173289112E-16, 1.000000000000000000, 6.467318590049456648E-15 ) ) ;
#118534 = CARTESIAN_POINT ( 'NONE',  ( -20.85000000000000142, -4.254329952141548965, -236.2118329068272260 ) ) ;
#118535 = CARTESIAN_POINT ( 'NONE',  ( -16.87036670365548474, 10.08494996326643189, -188.4499999999999886 ) ) ;
#118536 = DIRECTION ( 'NONE',  ( 1.000000000000000000, -0.000000000000000000, -0.000000000000000000 ) ) ;
#118537 = ORIENTED_EDGE ( 'NONE', *, *, #84302, .T. ) ;
#118538 = ORIENTED_EDGE ( 'NONE', *, *, #186594, .F. ) ;
#118539 = CARTESIAN_POINT ( 'NONE',  ( 21.00000000000000000, 66.25000000001260503, -191.1731074845244223 ) ) ;
#118540 = CIRCLE ( 'NONE', #93573, 1.899999999999997913 ) ;
#118541 = DIRECTION ( 'NONE',  ( 0.000000000000000000, 0.000000000000000000, -1.000000000000000000 ) ) ;
#118542 = CARTESIAN_POINT ( 'NONE',  ( -18.50000000000000000, 64.35000000001166143, -69.42310748452440805 ) ) ;
#118543 = EDGE_CURVE ( 'NONE', #195498, #191837, #220650, .T. ) ;
#118544 = ORIENTED_EDGE ( 'NONE', *, *, #132534, .F. ) ;
#118545 = LINE ( 'NONE', #135496, #190243 ) ;
#118546 = AXIS2_PLACEMENT_3D ( 'NONE', #145752, #204442, #207032 ) ;
#118547 = CARTESIAN_POINT ( 'NONE',  ( -20.05000000000000426, 9.250000000011157297, -179.8499999999999943 ) ) ;
#118548 = AXIS2_PLACEMENT_3D ( 'NONE', #164535, #121583, #120304 ) ;
#118549 = DIRECTION ( 'NONE',  ( -1.000000000000000000, 0.000000000000000000, 0.000000000000000000 ) ) ;
#118550 = ORIENTED_EDGE ( 'NONE', *, *, #198043, .T. ) ;
#118551 = VERTEX_POINT ( 'NONE', #253523 ) ;
#118552 = CARTESIAN_POINT ( 'NONE',  ( -21.05000000000000071, 69.34766280046808617, -247.6726305063181144 ) ) ;
#118553 = LINE ( 'NONE', #23309, #135764 ) ;
#118554 = EDGE_LOOP ( 'NONE', ( #169726, #8026, #47390, #174481 ) ) ;
#118555 = DIRECTION ( 'NONE',  ( 0.000000000000000000, 0.8814952561688438326, -0.4721928772777334582 ) ) ;
#118556 = EDGE_LOOP ( 'NONE', ( #239927, #140032, #124914 ) ) ;
#118557 = DIRECTION ( 'NONE',  ( -1.000000000000000000, 0.000000000000000000, 0.000000000000000000 ) ) ;
#118558 = CARTESIAN_POINT ( 'NONE',  ( -21.05000000000000071, -11.64999999998884483, -137.0000000000000000 ) ) ;
#118560 = CARTESIAN_POINT ( 'NONE',  ( 18.50000000000000000, 85.40000000001185754, -96.14106563635155567 ) ) ;
#118559 = CARTESIAN_POINT ( 'NONE',  ( -20.65000000000000568, 68.75000000001159606, -56.87310748452436826 ) ) ;
#118561 = CARTESIAN_POINT ( 'NONE',  ( -23.49999999999994316, 74.14873292176677921, -47.62635315998165453 ) ) ;
#118562 = EDGE_CURVE ( 'NONE', #81505, #180867, #83038, .T. ) ;
#118563 = DIRECTION ( 'NONE',  ( 0.000000000000000000, 2.891205793294679805E-16, -1.000000000000000000 ) ) ;
#118564 = AXIS2_PLACEMENT_3D ( 'NONE', #199681, #60128, #203513 ) ;
#118566 = ORIENTED_EDGE ( 'NONE', *, *, #170187, .F. ) ;
#118565 = ORIENTED_EDGE ( 'NONE', *, *, #227647, .F. ) ;
#118567 = ORIENTED_EDGE ( 'NONE', *, *, #65238, .T. ) ;
#118568 = ADVANCED_FACE ( 'NONE', ( #74931 ), #35796, .F. ) ;
#118569 = DIRECTION ( 'NONE',  ( 1.000000000000000000, 0.000000000000000000, 0.000000000000000000 ) ) ;
#118570 = VECTOR ( 'NONE', #83630, 1000.000000000000000 ) ;
#118571 = CARTESIAN_POINT ( 'NONE',  ( -21.14999999999999858, 1.115600667400684642E-11, -67.00000000000004263 ) ) ;
#118572 = CARTESIAN_POINT ( 'NONE',  ( 20.94999999999999929, 5.500000000011153745, -179.9052660189130677 ) ) ;
#118574 = CARTESIAN_POINT ( 'NONE',  ( -0.8999999999999993561, -8.250000000000005329, 23.40000000000000568 ) ) ;
#118573 = CARTESIAN_POINT ( 'NONE',  ( 20.59588692710267921, 10.36872342116900292, -7.639081094510505210 ) ) ;
#118575 = EDGE_LOOP ( 'NONE', ( #224166, #21896, #196743, #133397 ) ) ;
#118576 = CARTESIAN_POINT ( 'NONE',  ( -16.80469485234342031, 66.05784833687046387, -48.71314064059320970 ) ) ;
#118577 = VERTEX_POINT ( 'NONE', #117868 ) ;
#118578 = ADVANCED_FACE ( 'NONE', ( #215672 ), #177872, .F. ) ;
#118579 = CARTESIAN_POINT ( 'NONE',  ( -22.49533356619860669, 11.65000000631534149, -66.93487741967732063 ) ) ;
#118580 = VERTEX_POINT ( 'NONE', #477 ) ;
#118581 = ORIENTED_EDGE ( 'NONE', *, *, #146038, .F. ) ;
#118582 = CARTESIAN_POINT ( 'NONE',  ( -23.15000000000000213, -11.48912529306489994, -131.0000000000000284 ) ) ;
#118583 = CARTESIAN_POINT ( 'NONE',  ( -23.15000000000000213, -11.48912529306489994, -97.40000000000004832 ) ) ;
#118584 = CARTESIAN_POINT ( 'NONE',  ( -16.89155683852731116, 66.05000000001420801, -49.30047933406498117 ) ) ;
#118585 = CARTESIAN_POINT ( 'NONE',  ( 21.53752568622135755, 75.90102553874190505, -210.3099153590729031 ) ) ;
#118586 = EDGE_CURVE ( 'NONE', #216178, #138795, #95719, .T. ) ;
#118587 = STYLED_ITEM ( 'NONE', ( #43686 ), #103691 ) ;
#118588 = AXIS2_PLACEMENT_3D ( 'NONE', #15452, #235751, #233224 ) ;
#118589 = CARTESIAN_POINT ( 'NONE',  ( 18.49999999999999645, -1.362429037193310988, -41.38888124792119783 ) ) ;
#118590 = EDGE_CURVE ( 'NONE', #26113, #56902, #99567, .T. ) ;
#118591 = ORIENTED_EDGE ( 'NONE', *, *, #195745, .F. ) ;
#118592 = ORIENTED_EDGE ( 'NONE', *, *, #246647, .T. ) ;
#118593 = CARTESIAN_POINT ( 'NONE',  ( -20.54999999999999716, 74.00000000001151079, -49.24772940728643533 ) ) ;
#118594 = CARTESIAN_POINT ( 'NONE',  ( 21.05000000000000071, 67.22371710471958295, -124.3731074845243683 ) ) ;
#118595 = ORIENTED_EDGE ( 'NONE', *, *, #198695, .F. ) ;
#118596 = LINE ( 'NONE', #198107, #23018 ) ;
#118597 = LINE ( 'NONE', #227948, #179360 ) ;
#118598 = DIRECTION ( 'NONE',  ( -1.000000000000000000, -0.000000000000000000, 0.000000000000000000 ) ) ;
#118599 = LINE ( 'NONE', #159021, #13348 ) ;
#118601 = CARTESIAN_POINT ( 'NONE',  ( -21.14999999999999858, -11.38316329222462464, -203.4791315943886332 ) ) ;
#118600 = DIRECTION ( 'NONE',  ( 1.000000000000000000, 0.000000000000000000, 0.000000000000000000 ) ) ;
#118602 = DIRECTION ( 'NONE',  ( -0.000000000000000000, -0.2128009952263604232, 0.9770955615653316162 ) ) ;
#118603 = DIRECTION ( 'NONE',  ( 0.000000000000000000, -6.982962677686266711E-15, 1.000000000000000000 ) ) ;
#118604 = EDGE_CURVE ( 'NONE', #174346, #252190, #56584, .T. ) ;
#118605 = DIRECTION ( 'NONE',  ( 0.000000000000000000, 0.000000000000000000, 1.000000000000000000 ) ) ;
#118606 = CIRCLE ( 'NONE', #151749, 2.600000000000001421 ) ;
#118608 = EDGE_LOOP ( 'NONE', ( #138225, #31824, #136502, #39550 ) ) ;
#118607 = CARTESIAN_POINT ( 'NONE',  ( -17.29838795458461220, 10.37154985795824302, -55.60474128261655125 ) ) ;
#118609 = EDGE_CURVE ( 'NONE', #63666, #141892, #103897, .T. ) ;
#118610 = CIRCLE ( 'NONE', #201775, 11.64999999999998970 ) ;
#118611 = VECTOR ( 'NONE', #178025, 999.9999999999998863 ) ;
#118612 = ORIENTED_EDGE ( 'NONE', *, *, #246019, .T. ) ;
#118613 = ADVANCED_FACE ( 'NONE', ( #96988 ), #176589, .F. ) ;
#118614 = CARTESIAN_POINT ( 'NONE',  ( 20.95561247346651967, 10.59500736521470898, -41.09378276698163290 ) ) ;
#118615 = ORIENTED_EDGE ( 'NONE', *, *, #198057, .T. ) ;
#118616 = FACE_OUTER_BOUND ( 'NONE', #253932, .T. ) ;
#118617 = CARTESIAN_POINT ( 'NONE',  ( 23.24999999999999645, 4.775700934579428569, -11.84876810404597158 ) ) ;
#118618 = DIRECTION ( 'NONE',  ( 1.000000000000000000, -2.952720810173289112E-16, -2.061873921506763405E-30 ) ) ;
#118619 = ADVANCED_FACE ( 'NONE', ( #114012 ), #159581, .F. ) ;
#118620 = ORIENTED_EDGE ( 'NONE', *, *, #191215, .T. ) ;
#118621 = DIRECTION ( 'NONE',  ( 1.836970198721029934E-16, 0.9651348961777157509, -0.2617529984165031243 ) ) ;
#118623 = ADVANCED_FACE ( 'NONE', ( #55300 ), #115303, .T. ) ;
#118622 = DIRECTION ( 'NONE',  ( 0.000000000000000000, 0.000000000000000000, -1.000000000000000000 ) ) ;
#118624 = CARTESIAN_POINT ( 'NONE',  ( 23.24999999999999289, 11.65000000001116298, -79.15000000000004832 ) ) ;
#118625 = B_SPLINE_CURVE_WITH_KNOTS ( 'NONE', 3,
 ( #64120, #61555, #124107, #206198 ),
 .UNSPECIFIED., .F., .F.,
 ( 4, 4 ),
 ( 3.469446951953614189E-18, 0.0001058379652594568606 ),
 .UNSPECIFIED. ) ;
#118626 = AXIS2_PLACEMENT_3D ( 'NONE', #35098, #91181, #191599 ) ;
#118627 = DIRECTION ( 'NONE',  ( -1.000000000000000000, -0.000000000000000000, 0.000000000000000000 ) ) ;
#118628 = DIRECTION ( 'NONE',  ( 0.000000000000000000, 0.9126074666063804797, 0.4088369013363203908 ) ) ;
#118629 = VECTOR ( 'NONE', #39293, 1000.000000000000000 ) ;
#118630 = VECTOR ( 'NONE', #144617, 1000.000000000000227 ) ;
#118631 = ORIENTED_EDGE ( 'NONE', *, *, #197223, .T. ) ;
#118632 = DIRECTION ( 'NONE',  ( 1.186688945009010077E-16, -1.000000000000000000, -0.000000000000000000 ) ) ;
#118634 = EDGE_LOOP ( 'NONE', ( #148526, #159202, #173798, #81446 ) ) ;
#118633 = DIRECTION ( 'NONE',  ( 0.000000000000000000, -0.9126074666063773710, -0.4088369013363274962 ) ) ;
#118635 = DIRECTION ( 'NONE',  ( -0.000000000000000000, -6.982962677686266711E-15, 1.000000000000000000 ) ) ;
#118636 = CARTESIAN_POINT ( 'NONE',  ( -21.22070241538126112, 69.53005372714277144, -170.1220265150594173 ) ) ;
#118637 = ADVANCED_FACE ( 'NONE', ( #26500 ), #183006, .T. ) ;
#118638 = DIRECTION ( 'NONE',  ( -1.000000000000000000, 0.000000000000000000, 0.000000000000000000 ) ) ;
#118639 = ORIENTED_EDGE ( 'NONE', *, *, #75821, .F. ) ;
#118640 = CARTESIAN_POINT ( 'NONE',  ( 23.24999999999999289, 4.150000000011154988, -33.50000000000000000 ) ) ;
#118641 = ADVANCED_FACE ( 'NONE', ( #145126 ), #20745, .F. ) ;
#118642 = CIRCLE ( 'NONE', #6168, 0.1000000000000028644 ) ;
#118643 = APPLICATION_PROTOCOL_DEFINITION ( 'draft international standard', 'automotive_design', 1998, #203932 ) ;
#118644 = CIRCLE ( 'NONE', #247608, 0.1000000000000001027 ) ;
#118645 = AXIS2_PLACEMENT_3D ( 'NONE', #162037, #223256, #185432 ) ;
#118646 = CARTESIAN_POINT ( 'NONE',  ( 22.45380639571855497, -2.500503674154201939, -189.5187041452655592 ) ) ;
#118647 = VERTEX_POINT ( 'NONE', #104691 ) ;
#118648 = DIRECTION ( 'NONE',  ( 0.000000000000000000, 0.000000000000000000, 1.000000000000000000 ) ) ;
#118649 = CARTESIAN_POINT ( 'NONE',  ( 15.51872946208854565, 9.376580978055097049, -185.1269462470118867 ) ) ;
#118650 = AXIS2_PLACEMENT_3D ( 'NONE', #146148, #125318, #107015 ) ;
#118651 = AXIS2_PLACEMENT_3D ( 'NONE', #77687, #159830, #80234 ) ;
#118652 = CARTESIAN_POINT ( 'NONE',  ( 20.95392731769792150, 8.883061479199918509, -176.0222279795712836 ) ) ;
#118653 = ORIENTED_EDGE ( 'NONE', *, *, #34998, .T. ) ;
#118654 = VERTEX_POINT ( 'NONE', #202550 ) ;
#118655 = CARTESIAN_POINT ( 'NONE',  ( -22.45354308602371063, 75.99999978013372015, -114.7735403749838525 ) ) ;
#118656 = CIRCLE ( 'NONE', #31195, 0.1000000000000000472 ) ;
#118657 = DIRECTION ( 'NONE',  ( 2.694716079187273439E-16, 1.000000000000000000, 6.467318590049456648E-15 ) ) ;
#118658 = CIRCLE ( 'NONE', #164442, 0.1000000000000021289 ) ;
#118659 = FACE_OUTER_BOUND ( 'NONE', #134241, .T. ) ;
#118660 = CARTESIAN_POINT ( 'NONE',  ( 18.50000000000000000, -10.35479209691423996, -127.7565409830737906 ) ) ;
#118661 = CARTESIAN_POINT ( 'NONE',  ( 18.52928932304149967, 10.27928932305266407, -125.1762534328032217 ) ) ;
#118662 = DIRECTION ( 'NONE',  ( 1.186688945009010077E-16, -1.000000000000000000, -0.000000000000000000 ) ) ;
#118664 = DIRECTION ( 'NONE',  ( -7.304098846218134667E-16, 0.4088369013363281068, -0.9126074666063770380 ) ) ;
#118663 = DIRECTION ( 'NONE',  ( 0.000000000000000000, -1.000000000000000000, -6.982962677686265922E-15 ) ) ;
#118665 = CARTESIAN_POINT ( 'NONE',  ( -21.05000000000000071, 76.00000000001195133, -103.0231074845243171 ) ) ;
#118666 = DIRECTION ( 'NONE',  ( 1.000000000000000000, 1.875376730785737719E-16, 0.000000000000000000 ) ) ;
#118667 = CARTESIAN_POINT ( 'NONE',  ( -16.86337532320262156, 9.979967204235514089, -146.5510755310172044 ) ) ;
#118668 = ORIENTED_EDGE ( 'NONE', *, *, #222046, .T. ) ;
#118669 = EDGE_CURVE ( 'NONE', #243814, #228447, #23941, .T. ) ;
#118670 = EDGE_LOOP ( 'NONE', ( #82944, #107104, #106401, #137854 ) ) ;
#118671 = CARTESIAN_POINT ( 'NONE',  ( -21.07928932188134041, 1.115600667400684642E-11, -67.00000000000004263 ) ) ;
#118673 = CARTESIAN_POINT ( 'NONE',  ( 21.04999999999908411, 67.22371710472192774, -191.3651984818719143 ) ) ;
#118672 = CARTESIAN_POINT ( 'NONE',  ( -18.59999999999999787, -1.736257131597395809, -11.56865232901749785 ) ) ;
#118674 = CARTESIAN_POINT ( 'NONE',  ( 23.24999999999999289, 11.75000000001116263, -55.25000000000004974 ) ) ;
#118675 = CARTESIAN_POINT ( 'NONE',  ( -20.64999999999999858, -8.999999999988846255, -110.3939691226524786 ) ) ;
#118676 = DIRECTION ( 'NONE',  ( -0.000000000000000000, -6.982962677686266711E-15, 1.000000000000000000 ) ) ;
#118677 = ORIENTED_EDGE ( 'NONE', *, *, #118757, .F. ) ;
#118678 = ORIENTED_EDGE ( 'NONE', *, *, #185744, .T. ) ;
#118679 = AXIS2_PLACEMENT_3D ( 'NONE', #169408, #148525, #228060 ) ;
#118680 = CIRCLE ( 'NONE', #81214, 0.09999999999999543976 ) ;
#118681 = CARTESIAN_POINT ( 'NONE',  ( -23.25000000000000000, 67.23127455305841238, -235.8551265064783991 ) ) ;
#118682 = ORIENTED_EDGE ( 'NONE', *, *, #229981, .F. ) ;
#118683 = EDGE_CURVE ( 'NONE', #20561, #187685, #175078, .T. ) ;
#118684 = DIRECTION ( 'NONE',  ( -1.000000000000000000, -2.952720810173289112E-16, 0.000000000000000000 ) ) ;
#118685 = AXIS2_PLACEMENT_3D ( 'NONE', #24120, #103604, #183185 ) ;
#118686 = DIRECTION ( 'NONE',  ( -1.000000000000000000, -0.000000000000000000, -0.000000000000000000 ) ) ;
#118687 = AXIS2_PLACEMENT_3D ( 'NONE', #2955, #119075, #77353 ) ;
#118688 = AXIS2_PLACEMENT_3D ( 'NONE', #84846, #168327, #6627 ) ;
#118689 = ORIENTED_EDGE ( 'NONE', *, *, #255720, .T. ) ;
#118690 = CARTESIAN_POINT ( 'NONE',  ( -18.39999999999999858, 37.94390843806124280, -261.1300795796834109 ) ) ;
#118691 =( BOUNDED_CURVE ( )  B_SPLINE_CURVE ( 3, ( #117592, #79723, #60174, #197117 ),
 .UNSPECIFIED., .F., .F. ) 
 B_SPLINE_CURVE_WITH_KNOTS ( ( 4, 4 ),
 ( 3.752122642744613046, 4.712388980384671910 ),
 .UNSPECIFIED. ) 
 CURVE ( )  GEOMETRIC_REPRESENTATION_ITEM ( )  RATIONAL_B_SPLINE_CURVE ( ( 1.000000000000000000, 0.9246222802177266331, 0.9246222802177266331, 1.000000000000000000 ) ) 
 REPRESENTATION_ITEM ( '' )  );
#118692 = VERTEX_POINT ( 'NONE', #201258 ) ;
#118693 = DIRECTION ( 'NONE',  ( -4.239556034732056743E-17, -0.1298341882519953583, -0.9915357197604862671 ) ) ;
#118695 = AXIS2_PLACEMENT_3D ( 'NONE', #183015, #4344, #27815 ) ;
#118694 = DIRECTION ( 'NONE',  ( 1.000000000000000000, 0.000000000000000000, 0.000000000000000000 ) ) ;
#118696 = CARTESIAN_POINT ( 'NONE',  ( -23.25000000000000000, 87.65000000001235492, -166.9231074845242802 ) ) ;
#118697 = DIRECTION ( 'NONE',  ( 1.000000000000000000, 0.000000000000000000, 0.000000000000000000 ) ) ;
#118698 = CARTESIAN_POINT ( 'NONE',  ( -16.97048326478264713, 9.949999999999983302, -13.14110688012716999 ) ) ;
#118700 = DIRECTION ( 'NONE',  ( 0.000000000000000000, -0.2128009952263604232, 0.9770955615653316162 ) ) ;
#118699 = CARTESIAN_POINT ( 'NONE',  ( -18.59999999999999787, 61.95000000001191154, -97.50941241376341395 ) ) ;
#118701 = AXIS2_PLACEMENT_3D ( 'NONE', #14231, #168192, #112036 ) ;
#118702 = DIRECTION ( 'NONE',  ( 0.000000000000000000, 0.000000000000000000, 1.000000000000000000 ) ) ;
#118703 = ORIENTED_EDGE ( 'NONE', *, *, #35244, .F. ) ;
#118705 = DIRECTION ( 'NONE',  ( -1.000000000000000000, 3.151514657663852580E-16, -8.547182517843351137E-17 ) ) ;
#118704 = DIRECTION ( 'NONE',  ( 0.000000000000000000, -6.982962677686266711E-15, 1.000000000000000000 ) ) ;
#118706 = ORIENTED_EDGE ( 'NONE', *, *, #60317, .F. ) ;
#118708 = EDGE_LOOP ( 'NONE', ( #140696, #16966, #105036, #209038 ) ) ;
#118707 = DIRECTION ( 'NONE',  ( 1.000000000000000000, 0.000000000000000000, 0.000000000000000000 ) ) ;
#118709 = AXIS2_PLACEMENT_3D ( 'NONE', #256553, #254033, #195383 ) ;
#118710 = VERTEX_POINT ( 'NONE', #244227 ) ;
#118711 = CARTESIAN_POINT ( 'NONE',  ( -22.50000000000000000, 76.00000000001195133, -103.0231074845243171 ) ) ;
#118712 = CARTESIAN_POINT ( 'NONE',  ( -21.07016717457011268, 1.115542391533913547E-11, -27.17905916189910442 ) ) ;
#118713 = DIRECTION ( 'NONE',  ( 0.000000000000000000, 0.000000000000000000, -1.000000000000000000 ) ) ;
#118714 = CARTESIAN_POINT ( 'NONE',  ( -20.85000000000000142, 68.92903212821283887, -65.77654326265606244 ) ) ;
#118715 = ORIENTED_EDGE ( 'NONE', *, *, #134351, .T. ) ;
#118716 = CARTESIAN_POINT ( 'NONE',  ( 21.05000000000000071, 65.57661458509917907, -129.0310555606542664 ) ) ;
#118717 = CARTESIAN_POINT ( 'NONE',  ( 21.13461538461538680, 8.885417037985614996, -112.8500000000000369 ) ) ;
#118719 = DIRECTION ( 'NONE',  ( 0.000000000000000000, 6.853228547068871147E-15, -1.000000000000000000 ) ) ;
#118718 = AXIS2_PLACEMENT_3D ( 'NONE', #248725, #209596, #130035 ) ;
#118720 = VERTEX_POINT ( 'NONE', #181710 ) ;
#118721 = CARTESIAN_POINT ( 'NONE',  ( 18.59999999999999787, -4.317402351199911337, -229.8357552817742260 ) ) ;
#118722 = ADVANCED_FACE ( 'NONE', ( #64330 ), #3046, .F. ) ;
#118723 = DIRECTION ( 'NONE',  ( 1.000000000000000000, -7.125593699324843413E-30, 1.020425574104004196E-15 ) ) ;
#118724 = EDGE_LOOP ( 'NONE', ( #143895, #121985, #168507, #104817 ) ) ;
#118725 = ORIENTED_EDGE ( 'NONE', *, *, #111895, .F. ) ;
#118726 = DIRECTION ( 'NONE',  ( -2.952720810173289112E-16, -1.000000000000000000, -6.982962677686266711E-15 ) ) ;
#118727 = CIRCLE ( 'NONE', #164511, 12.77499999999999858 ) ;
#118728 = ORIENTED_EDGE ( 'NONE', *, *, #129265, .T. ) ;
#118729 = AXIS2_PLACEMENT_3D ( 'NONE', #190531, #28913, #170990 ) ;
#118730 = VERTEX_POINT ( 'NONE', #82565 ) ;
#118731 = CARTESIAN_POINT ( 'NONE',  ( 20.88420186297724257, 10.33025634372637391, -173.0870929282638997 ) ) ;
#118732 = EDGE_CURVE ( 'NONE', #222218, #219071, #103424, .T. ) ;
#118733 = CARTESIAN_POINT ( 'NONE',  ( -23.25000000000000000, 54.22301550979020845, -237.0256805049050115 ) ) ;
#118734 = DIRECTION ( 'NONE',  ( 0.000000000000000000, 0.1686199900910313187, -0.9856811345164828708 ) ) ;
#118735 = EDGE_CURVE ( 'NONE', #253862, #116539, #83233, .T. ) ;
#118736 = CARTESIAN_POINT ( 'NONE',  ( 20.95392731769792150, 60.88864066144310527, -225.3048589129162167 ) ) ;
#118737 = DIRECTION ( 'NONE',  ( 0.000000000000000000, 0.000000000000000000, -1.000000000000000000 ) ) ;
#118738 = EDGE_CURVE ( 'NONE', #152713, #220102, #137415, .T. ) ;
#118739 = CARTESIAN_POINT ( 'NONE',  ( -22.39999999999999858, 1.115486826172573664E-11, -88.85042919245522341 ) ) ;
#118740 = CARTESIAN_POINT ( 'NONE',  ( -21.05000000000000071, -1.851028230129704522, -78.65391326942254580 ) ) ;
#118741 = ORIENTED_EDGE ( 'NONE', *, *, #107034, .F. ) ;
#118742 = AXIS2_PLACEMENT_3D ( 'NONE', #40955, #39670, #154489 ) ;
#118744 = CARTESIAN_POINT ( 'NONE',  ( 22.39999999999999503, 11.75000000001115552, -33.40000000000000568 ) ) ;
#118743 = DIRECTION ( 'NONE',  ( -1.000000000000000000, 0.000000000000000000, 0.000000000000000000 ) ) ;
#118745 = ORIENTED_EDGE ( 'NONE', *, *, #88581, .F. ) ;
#118748 = ORIENTED_EDGE ( 'NONE', *, *, #250941, .F. ) ;
#118747 = DIRECTION ( 'NONE',  ( -1.000000000000000000, -0.000000000000000000, -0.000000000000000000 ) ) ;
#118746 = CARTESIAN_POINT ( 'NONE',  ( 21.72449340488910607, 40.89608266988597052, -236.3842060787924879 ) ) ;
#118749 = ORIENTED_EDGE ( 'NONE', *, *, #137670, .T. ) ;
#118750 = DIRECTION ( 'NONE',  ( -1.000000000000000000, 0.000000000000000000, 0.000000000000000000 ) ) ;
#118751 = CARTESIAN_POINT ( 'NONE',  ( 12.47034474403011650, 66.62446189796425244, -154.1532316035335555 ) ) ;
#118752 = CARTESIAN_POINT ( 'NONE',  ( -23.15000000000000213, 87.65000000001215597, -139.6231074845242688 ) ) ;
#118753 = CARTESIAN_POINT ( 'NONE',  ( -16.80468759584937999, 9.942153675145299019, -113.1900188662016831 ) ) ;
#118754 = AXIS2_PLACEMENT_3D ( 'NONE', #234418, #216138, #192751 ) ;
#118755 = VERTEX_POINT ( 'NONE', #25220 ) ;
#118756 = CARTESIAN_POINT ( 'NONE',  ( 20.04142135623731136, 16.72641738073392759, -222.5849938986772258 ) ) ;
#118757 = EDGE_CURVE ( 'NONE', #194584, #76104, #162164, .T. ) ;
#118758 = DIRECTION ( 'NONE',  ( 0.000000000000000000, 0.000000000000000000, 1.000000000000000000 ) ) ;
#118760 = FACE_OUTER_BOUND ( 'NONE', #91234, .T. ) ;
#118759 = CARTESIAN_POINT ( 'NONE',  ( -21.05000000000000071, 77.83534155023646406, -124.8679561919613121 ) ) ;
#118762 = ORIENTED_EDGE ( 'NONE', *, *, #48774, .F. ) ;
#118761 = DIRECTION ( 'NONE',  ( 0.000000000000000000, 0.000000000000000000, 1.000000000000000000 ) ) ;
#118763 = VERTEX_POINT ( 'NONE', #142561 ) ;
#118764 = VECTOR ( 'NONE', #167875, 1000.000000000000000 ) ;
#118765 = AXIS2_PLACEMENT_3D ( 'NONE', #121635, #64208, #240286 ) ;
#118766 = CARTESIAN_POINT ( 'NONE',  ( 12.25000000000000000, 66.15000000001155911, -52.77310748452440237 ) ) ;
#118767 = VERTEX_POINT ( 'NONE', #5605 ) ;
#118768 = DIRECTION ( 'NONE',  ( 0.000000000000000000, -0.4999999999999689138, 0.8660254037844565822 ) ) ;
#118769 = VERTEX_POINT ( 'NONE', #85133 ) ;
#118770 = CARTESIAN_POINT ( 'NONE',  ( -18.39999999999999858, 29.77885356168128794, -262.9335064780472635 ) ) ;
#118771 = CYLINDRICAL_SURFACE ( 'NONE', #178522, 0.1000000000000028644 ) ;
#118772 = ORIENTED_EDGE ( 'NONE', *, *, #108014, .T. ) ;
#118773 = DIRECTION ( 'NONE',  ( 1.000000000000000000, -0.000000000000000000, -0.000000000000000000 ) ) ;
#118774 = DIRECTION ( 'NONE',  ( 0.000000000000000000, 0.000000000000000000, -1.000000000000000000 ) ) ;
#118775 = VECTOR ( 'NONE', #147248, 999.9999999999998863 ) ;
#118776 = CIRCLE ( 'NONE', #6330, 0.1000000000000028644 ) ;
#118777 = AXIS2_PLACEMENT_3D ( 'NONE', #50865, #109570, #151300 ) ;
#118778 = EDGE_CURVE ( 'NONE', #69945, #250282, #62610, .T. ) ;
#118779 = ORIENTED_EDGE ( 'NONE', *, *, #142900, .F. ) ;
#118780 = ORIENTED_EDGE ( 'NONE', *, *, #57794, .F. ) ;
#118781 =( BOUNDED_SURFACE ( )  B_SPLINE_SURFACE ( 3, 2, ( 
 ( #6167, #167852, #188666 ),
 ( #145679, #8754, #10031 ),
 ( #225204, #169144, #248642 ),
 ( #46573, #70032, #205650 ) ),
 .UNSPECIFIED., .F., .F., .T. ) 
 B_SPLINE_SURFACE_WITH_KNOTS ( ( 4, 4 ),
 ( 3, 3 ),
 ( 0.3000847527772392831, 0.5552748953338751958 ),
 ( 0.000000000000000000, 1.000000000000000000 ),
 .UNSPECIFIED. ) 
 GEOMETRIC_REPRESENTATION_ITEM ( )  RATIONAL_B_SPLINE_SURFACE ( (
 ( 1.000000000000000000, 0.9152888060719472918, 1.000000000000000000),
 ( 1.000000000000000000, 0.9104333467450296258, 1.000000000000000000),
 ( 1.000000000000000000, 0.9035312726220154911, 1.000000000000000000),
 ( 1.000000000000000000, 0.8946697475932554600, 1.000000000000000000) ) ) 
 REPRESENTATION_ITEM ( '' )  SURFACE ( )  );
#118782 = ORIENTED_EDGE ( 'NONE', *, *, #233599, .T. ) ;
#118783 = MECHANICAL_DESIGN_GEOMETRIC_PRESENTATION_REPRESENTATION (  '', ( #1851 ), #77068 ) ;
#118784 = CARTESIAN_POINT ( 'NONE',  ( 20.94999999999999574, 74.14897176987174987, -191.8691942151018850 ) ) ;
#118785 = ORIENTED_EDGE ( 'NONE', *, *, #90257, .F. ) ;
#118787 = EDGE_LOOP ( 'NONE', ( #139841, #11032, #106607, #8587 ) ) ;
#118786 = LINE ( 'NONE', #24839, #242683 ) ;
#118788 = ADVANCED_FACE ( 'NONE', ( #65604 ), #21372, .T. ) ;
#118789 = VERTEX_POINT ( 'NONE', #141297 ) ;
#118792 = ORIENTED_EDGE ( 'NONE', *, *, #110243, .F. ) ;
#118791 = ORIENTED_EDGE ( 'NONE', *, *, #179458, .F. ) ;
#118790 = DIRECTION ( 'NONE',  ( 0.000000000000000000, 1.776356839400310418E-15, -1.000000000000000000 ) ) ;
#118793 = EDGE_CURVE ( 'NONE', #84743, #91161, #245765, .T. ) ;
#118794 = EDGE_CURVE ( 'NONE', #176232, #203476, #185557, .T. ) ;
#118795 = VERTEX_POINT ( 'NONE', #42203 ) ;
#118796 = DIRECTION ( 'NONE',  ( 0.000000000000000000, 0.000000000000000000, -1.000000000000000000 ) ) ;
#118797 = CIRCLE ( 'NONE', #93839, 11.80000000000000426 ) ;
#118798 = CYLINDRICAL_SURFACE ( 'NONE', #197059, 4.049999999999987388 ) ;
#118799 = AXIS2_PLACEMENT_3D ( 'NONE', #101445, #123637, #21976 ) ;
#118800 = FACE_OUTER_BOUND ( 'NONE', #242444, .T. ) ;
#118801 = AXIS2_PLACEMENT_3D ( 'NONE', #189867, #172918, #252385 ) ;
#118802 = ORIENTED_EDGE ( 'NONE', *, *, #96808, .T. ) ;
#118803 = DIRECTION ( 'NONE',  ( 0.000000000000000000, -0.9915357197604837136, 0.1298341882520134827 ) ) ;
#118804 = ADVANCED_FACE ( 'NONE', ( #102131 ), #68182, .F. ) ;
#118805 = ORIENTED_EDGE ( 'NONE', *, *, #15282, .F. ) ;
#118806 = FACE_OUTER_BOUND ( 'NONE', #56521, .T. ) ;
#118808 = EDGE_LOOP ( 'NONE', ( #66788, #193507, #44476, #109104 ) ) ;
#118807 = DIRECTION ( 'NONE',  ( 0.000000000000000000, 6.982962677686266711E-15, -1.000000000000000000 ) ) ;
#118809 = EDGE_CURVE ( 'NONE', #188954, #124743, #33412, .T. ) ;
#118810 = EDGE_LOOP ( 'NONE', ( #193866, #198649, #48053, #208399 ) ) ;
#118811 = AXIS2_PLACEMENT_3D ( 'NONE', #74785, #36941, #155605 ) ;
#118812 = ADVANCED_FACE ( 'NONE', ( #107298 ), #34974, .T. ) ;
#118813 = AXIS2_PLACEMENT_3D ( 'NONE', #122215, #201738, #63501 ) ;
#118814 = AXIS2_PLACEMENT_3D ( 'NONE', #18737, #115271, #37047 ) ;
#118815 = DIRECTION ( 'NONE',  ( -1.000000000000000000, -0.000000000000000000, -0.000000000000000000 ) ) ;
#118816 = DIRECTION ( 'NONE',  ( 0.000000000000000000, 1.000000000000000000, 1.265107689135680095E-16 ) ) ;
#118817 = VERTEX_POINT ( 'NONE', #111162 ) ;
#118818 = VERTEX_POINT ( 'NONE', #69485 ) ;
#118819 = CARTESIAN_POINT ( 'NONE',  ( -16.93583594267724379, 10.00862343506335961, -180.0593908393207414 ) ) ;
#118820 = CARTESIAN_POINT ( 'NONE',  ( -21.04999999999999716, 0.05132743235259914355, -161.1998166637364420 ) ) ;
#118821 = ADVANCED_FACE ( 'NONE', ( #70780 ), #70824, .T. ) ;
#118824 = ORIENTED_EDGE ( 'NONE', *, *, #211954, .F. ) ;
#118823 = ORIENTED_EDGE ( 'NONE', *, *, #194952, .F. ) ;
#118822 = AXIS2_PLACEMENT_3D ( 'NONE', #239051, #185499, #102078 ) ;
#118825 = ORIENTED_EDGE ( 'NONE', *, *, #211687, .F. ) ;
#118826 = CARTESIAN_POINT ( 'NONE',  ( 20.73486653747088582, 68.75000000001196554, -115.6731074845243512 ) ) ;
#118827 = EDGE_LOOP ( 'NONE', ( #40279, #15044, #31285, #147967 ) ) ;
#118828 = CIRCLE ( 'NONE', #223037, 0.09999999999999939493 ) ;
#118829 = EDGE_LOOP ( 'NONE', ( #40714, #189122, #19146 ) ) ;
#118830 = EDGE_CURVE ( 'NONE', #230638, #91161, #254117, .T. ) ;
#118831 = CARTESIAN_POINT ( 'NONE',  ( -21.14999999999999858, -0.09999999998884338825, -55.35042919245524473 ) ) ;
#118832 = ORIENTED_EDGE ( 'NONE', *, *, #242706, .F. ) ;
#118833 = EDGE_CURVE ( 'NONE', #49212, #235424, #228550, .T. ) ;
#118834 = CARTESIAN_POINT ( 'NONE',  ( -16.94062896051973865, 12.44566954809400627, -211.1874024072765792 ) ) ;
#118835 = ADVANCED_FACE ( 'NONE', ( #146405 ), #154231, .T. ) ;
#118836 = AXIS2_PLACEMENT_3D ( 'NONE', #180882, #244681, #26965 ) ;
#118837 = TOROIDAL_SURFACE ( 'NONE', #239626, 2.100000000000002309, 0.1000000000000000056 ) ;
#118839 = CARTESIAN_POINT ( 'NONE',  ( -21.05000000000000071, 30.90801580390628800, -252.0203440857197279 ) ) ;
#118838 = DIRECTION ( 'NONE',  ( -1.000000000000000000, -7.136802563874201079E-16, -1.554319503706925800E-16 ) ) ;
#118840 = VERTEX_POINT ( 'NONE', #150300 ) ;
#118842 = EDGE_LOOP ( 'NONE', ( #99252, #51144, #203454, #99460 ) ) ;
#118841 = ORIENTED_EDGE ( 'NONE', *, *, #202095, .T. ) ;
#118843 = CYLINDRICAL_SURFACE ( 'NONE', #173717, 0.1000000000000000472 ) ;
#118844 = FACE_OUTER_BOUND ( 'NONE', #227916, .T. ) ;
#118845 = EDGE_LOOP ( 'NONE', ( #47962, #240942, #72836, #101693 ) ) ;
#118846 = DIRECTION ( 'NONE',  ( 1.000000000000000000, 0.000000000000000000, 0.000000000000000000 ) ) ;
#118847 = ORIENTED_EDGE ( 'NONE', *, *, #3142, .F. ) ;
#118848 = ADVANCED_FACE ( 'NONE', ( #92867 ), #109857, .F. ) ;
#118849 = EDGE_LOOP ( 'NONE', ( #193103, #179976, #174298, #1041 ) ) ;
#118850 = EDGE_CURVE ( 'NONE', #204044, #81484, #12085, .T. ) ;
#118851 = DIRECTION ( 'NONE',  ( -1.000000000000000000, -0.000000000000000000, 0.000000000000000000 ) ) ;
#118852 = ORIENTED_EDGE ( 'NONE', *, *, #138589, .F. ) ;
#118853 = CARTESIAN_POINT ( 'NONE',  ( -18.50000000000000000, 1.148907358139439339E-11, -201.0000000000015064 ) ) ;
#118854 = ORIENTED_EDGE ( 'NONE', *, *, #248342, .F. ) ;
#118855 = FACE_OUTER_BOUND ( 'NONE', #52181, .T. ) ;
#118856 = CARTESIAN_POINT ( 'NONE',  ( -19.99999999999999645, 1.350000000000000089, 16.60000000000000142 ) ) ;
#118858 = CARTESIAN_POINT ( 'NONE',  ( -16.83233564386403458, 9.930221796595763095, -121.2245206634756585 ) ) ;
#118857 = CARTESIAN_POINT ( 'NONE',  ( -18.59999999999999787, -9.480686695267820596, -174.4411151687578752 ) ) ;
#118859 = CIRCLE ( 'NONE', #60378, 0.09999999999998898659 ) ;
#118860 = CARTESIAN_POINT ( 'NONE',  ( 23.14999999999999503, 69.55000000001223270, -148.8731074845244109 ) ) ;
#118861 = DIRECTION ( 'NONE',  ( 4.336808689942017736E-16, -0.000000000000000000, 1.000000000000000000 ) ) ;
#118862 = CARTESIAN_POINT ( 'NONE',  ( 23.14999999999999503, 69.35000000001180354, -81.87310748452435405 ) ) ;
#118863 = AXIS2_PLACEMENT_3D ( 'NONE', #26735, #25439, #65829 ) ;
#118864 = EDGE_CURVE ( 'NONE', #223901, #183793, #208956, .T. ) ;
#118865 = DIRECTION ( 'NONE',  ( 0.000000000000000000, -0.2128009952263603677, 0.9770955615653315052 ) ) ;
#118866 = CARTESIAN_POINT ( 'NONE',  ( 0.000000000000000000, -11.65000000000000036, 32.89999999999999858 ) ) ;
#118867 = CIRCLE ( 'NONE', #218590, 0.1000000000000028644 ) ;
#118868 = ORIENTED_EDGE ( 'NONE', *, *, #153782, .F. ) ;
#118870 = ORIENTED_EDGE ( 'NONE', *, *, #109079, .F. ) ;
#118869 = ORIENTED_EDGE ( 'NONE', *, *, #249633, .T. ) ;
#118871 = AXIS2_PLACEMENT_3D ( 'NONE', #18192, #217645, #61166 ) ;
#118872 = ORIENTED_EDGE ( 'NONE', *, *, #179533, .T. ) ;
#118873 = VERTEX_POINT ( 'NONE', #117579 ) ;
#118874 = CARTESIAN_POINT ( 'NONE',  ( 20.84999999999998721, 64.65966496992309942, -200.4475097531309586 ) ) ;
#118875 = CARTESIAN_POINT ( 'NONE',  ( 18.69999999999999929, -8.350000000000004974, 10.95857864376268864 ) ) ;
#118876 = AXIS2_PLACEMENT_3D ( 'NONE', #85109, #25198, #3025 ) ;
#118878 = CARTESIAN_POINT ( 'NONE',  ( 23.14999999999999858, 36.65892442174472876, -249.5511627012454596 ) ) ;
#118877 = DIRECTION ( 'NONE',  ( -1.000000000000000000, 0.000000000000000000, 0.000000000000000000 ) ) ;
#118880 = VERTEX_POINT ( 'NONE', #115010 ) ;
#118879 = VECTOR ( 'NONE', #70162, 1000.000000000000000 ) ;
#118881 = EDGE_CURVE ( 'NONE', #253481, #255363, #249856, .T. ) ;
#118882 = CARTESIAN_POINT ( 'NONE',  ( -0.8999999999999437339, 67.75000000001118394, -12.62310748452478926 ) ) ;
#118883 = CARTESIAN_POINT ( 'NONE',  ( 5.999999999999995559, -11.34999999999999964, 10.00000000000000178 ) ) ;
#118884 = CIRCLE ( 'NONE', #81409, 0.3999999999999994671 ) ;
#118885 = CARTESIAN_POINT ( 'NONE',  ( 20.09999999999999787, 12.21861431488691530, -211.2854491503459826 ) ) ;
#118886 = EDGE_CURVE ( 'NONE', #55636, #146352, #216679, .T. ) ;
#118887 = ORIENTED_EDGE ( 'NONE', *, *, #249637, .T. ) ;
#118888 = DIRECTION ( 'NONE',  ( 0.000000000000000000, 0.000000000000000000, 1.000000000000000000 ) ) ;
#118889 = EDGE_CURVE ( 'NONE', #206438, #1901, #237537, .T. ) ;
#118890 = DIRECTION ( 'NONE',  ( 1.000000000000000000, 0.000000000000000000, 0.000000000000000000 ) ) ;
#118891 = EDGE_CURVE ( 'NONE', #51868, #129578, #194580, .T. ) ;
#118892 = EDGE_LOOP ( 'NONE', ( #240626, #148401, #177534, #60621 ) ) ;
#118893 = DIRECTION ( 'NONE',  ( 0.000000000000000000, 0.000000000000000000, -1.000000000000000000 ) ) ;
#118894 = VECTOR ( 'NONE', #35742, 1000.000000000000000 ) ;
#118895 = CARTESIAN_POINT ( 'NONE',  ( -20.64999999999999858, 68.85000000001156195, -57.17310748452437252 ) ) ;
#118896 = DIRECTION ( 'NONE',  ( 0.000000000000000000, 0.9126074666063734853, 0.4088369013363359894 ) ) ;
#118897 = CARTESIAN_POINT ( 'NONE',  ( -20.94999999999999929, -11.48912529306490349, -103.4000000000000341 ) ) ;
#118898 = EDGE_CURVE ( 'NONE', #80585, #192885, #134551, .T. ) ;
#118899 = CARTESIAN_POINT ( 'NONE',  ( -17.29838795458705647, 10.37154985794953177, -22.10474128261738613 ) ) ;
#118900 = ORIENTED_EDGE ( 'NONE', *, *, #105723, .T. ) ;
#118901 = CARTESIAN_POINT ( 'NONE',  ( 18.46858270002951841, 47.01368633151875542, -255.2938221613214580 ) ) ;
#118902 = CARTESIAN_POINT ( 'NONE',  ( -20.94999999999994600, 64.25000000001119815, -6.123107484524794586 ) ) ;
#118903 = DIRECTION ( 'NONE',  ( -0.000000000000000000, -0.4088369013363281068, 0.9126074666063770380 ) ) ;
#118905 = LINE ( 'NONE', #19805, #187080 ) ;
#118904 = DIRECTION ( 'NONE',  ( 1.000000000000000000, 0.000000000000000000, 0.000000000000000000 ) ) ;
#118906 = DIRECTION ( 'NONE',  ( 1.000000000000000000, 0.000000000000000000, 0.000000000000000000 ) ) ;
#118907 = CARTESIAN_POINT ( 'NONE',  ( -16.91776028072577631, 9.963400393640901243, -121.3750240147021486 ) ) ;
#118908 = CARTESIAN_POINT ( 'NONE',  ( -22.50000000000000000, 1.115600667400684642E-11, -167.4999999999999716 ) ) ;
#118909 = CARTESIAN_POINT ( 'NONE',  ( 23.14999999999999858, 5.000000000011153745, -179.9052660189130677 ) ) ;
#118911 = EDGE_LOOP ( 'NONE', ( #17132, #205627, #86001, #240305 ) ) ;
#118910 = VECTOR ( 'NONE', #62721, 1000.000000000000000 ) ;
#118912 = EDGE_CURVE ( 'NONE', #139130, #183226, #96694, .T. ) ;
#118913 = TOROIDAL_SURFACE ( 'NONE', #89649, 11.65000000000000036, 0.1000000000000000056 ) ;
#118914 = EDGE_CURVE ( 'NONE', #227881, #151730, #45853, .T. ) ;
#118915 = VERTEX_POINT ( 'NONE', #212839 ) ;
#118916 = CARTESIAN_POINT ( 'NONE',  ( -23.15000000000000213, 69.09936979046463534, -247.6075824278584889 ) ) ;
#118917 = ORIENTED_EDGE ( 'NONE', *, *, #256458, .F. ) ;
#118918 = EDGE_CURVE ( 'NONE', #136073, #26265, #241663, .T. ) ;
#118919 = LINE ( 'NONE', #58895, #13637 ) ;
#118920 = CARTESIAN_POINT ( 'NONE',  ( -20.85000000000000142, 7.120270961708750512, -171.1595630418393625 ) ) ;
#118921 = EDGE_CURVE ( 'NONE', #46280, #23059, #193274, .T. ) ;
#118922 = CARTESIAN_POINT ( 'NONE',  ( 22.39999999999999503, 65.19201463318205469, -243.3742797652979277 ) ) ;
#118923 = VECTOR ( 'NONE', #241691, 1000.000000000000114 ) ;
#118924 = ORIENTED_EDGE ( 'NONE', *, *, #216186, .T. ) ;
#118925 = CARTESIAN_POINT ( 'NONE',  ( 21.07928932188134397, 0.09889514566555242248, -161.1714833436066385 ) ) ;
#118926 = CARTESIAN_POINT ( 'NONE',  ( -15.15564720441980207, 9.410708747058237122, -51.56920840584412957 ) ) ;
#118927 = CARTESIAN_POINT ( 'NONE',  ( -22.00411653889220176, 75.90096189422511941, -110.2765503521648185 ) ) ;
#118928 = EDGE_CURVE ( 'NONE', #101974, #200905, #58299, .T. ) ;
#118929 = CIRCLE ( 'NONE', #127290, 11.80000000000000426 ) ;
#118930 = CARTESIAN_POINT ( 'NONE',  ( -18.59999999999999787, -1.164121893230052995, -175.4148480855716059 ) ) ;
#118932 = ORIENTED_EDGE ( 'NONE', *, *, #100641, .T. ) ;
#118931 = CARTESIAN_POINT ( 'NONE',  ( -23.24999999999999645, 85.60000000001166143, -62.92291809330219365 ) ) ;
#118934 = DIRECTION ( 'NONE',  ( 1.000000000000000000, 2.885090398161910739E-16, 6.283419270304611573E-17 ) ) ;
#118933 = CARTESIAN_POINT ( 'NONE',  ( -16.98495255085921229, 10.00556436600593280, -146.6346172062204971 ) ) ;
#118935 = DIRECTION ( 'NONE',  ( 1.000000000000000000, -1.207181226542539700E-16, 2.694675058168174199E-16 ) ) ;
#118936 = EDGE_CURVE ( 'NONE', #29148, #113969, #41782, .T. ) ;
#118937 = DIRECTION ( 'NONE',  ( 0.000000000000000000, -0.000000000000000000, -1.000000000000000000 ) ) ;
#118938 = CYLINDRICAL_SURFACE ( 'NONE', #189682, 0.09999999999999939493 ) ;
#118939 = ORIENTED_EDGE ( 'NONE', *, *, #173872, .T. ) ;
#118940 = EDGE_CURVE ( 'NONE', #117217, #75355, #233313, .T. ) ;
#118941 = CARTESIAN_POINT ( 'NONE',  ( 0.000000000000000000, 0.000000000000000000, 0.000000000000000000 ) ) ;
#118942 = DIRECTION ( 'NONE',  ( 1.000000000000000000, -3.265361837132813093E-16, -2.280189983783949500E-30 ) ) ;
#118943 = ORIENTED_EDGE ( 'NONE', *, *, #79782, .T. ) ;
#118944 = CARTESIAN_POINT ( 'NONE',  ( -16.89146115310546392, 66.04855675435608475, -182.6682850655701884 ) ) ;
#118945 = ORIENTED_EDGE ( 'NONE', *, *, #58741, .F. ) ;
#118946 = CIRCLE ( 'NONE', #214593, 0.09999999999998898659 ) ;
#118948 = CARTESIAN_POINT ( 'NONE',  ( 18.49999999999999289, 55.01933066900991776, -229.9591340285290073 ) ) ;
#118947 = CIRCLE ( 'NONE', #152276, 0.09999999999999326095 ) ;
#118949 = FACE_OUTER_BOUND ( 'NONE', #34333, .T. ) ;
#118950 = DIRECTION ( 'NONE',  ( 1.000000000000000000, 0.000000000000000000, 0.000000000000000000 ) ) ;
#118951 = EDGE_CURVE ( 'NONE', #211036, #237980, #113725, .T. ) ;
#118952 = EDGE_LOOP ( 'NONE', ( #118450, #217518, #41462, #148645 ) ) ;
#118953 = ORIENTED_EDGE ( 'NONE', *, *, #257703, .T. ) ;
#118954 = DIRECTION ( 'NONE',  ( 0.000000000000000000, -1.000000000000000000, 0.000000000000000000 ) ) ;
#118955 = DIRECTION ( 'NONE',  ( -0.000000000000000000, -0.9770955615653313941, -0.2128009952263603677 ) ) ;
#118956 = CARTESIAN_POINT ( 'NONE',  ( -16.77308656112214891, 63.08568178456688713, -213.1278080429823092 ) ) ;
#118957 = DIRECTION ( 'NONE',  ( 0.000000000000000000, -1.000000000000000000, 0.000000000000000000 ) ) ;
#118959 = AXIS2_PLACEMENT_3D ( 'NONE', #57516, #97910, #139612 ) ;
#118958 = CYLINDRICAL_SURFACE ( 'NONE', #165866, 0.1000000000000028644 ) ;
#118960 = LINE ( 'NONE', #101918, #44120 ) ;
#118961 = AXIS2_PLACEMENT_3D ( 'NONE', #90801, #248606, #85641 ) ;
#118962 = CARTESIAN_POINT ( 'NONE',  ( 21.06280952165520759, 65.37286769941019315, -90.81905359774572162 ) ) ;
#118963 = CARTESIAN_POINT ( 'NONE',  ( -20.95000000000000284, 62.92003201576282123, -207.2439188921395896 ) ) ;
#118964 = ORIENTED_EDGE ( 'NONE', *, *, #72504, .T. ) ;
#118965 = DIRECTION ( 'NONE',  ( 0.000000000000000000, 0.2128009952263603677, -0.9770955615653313941 ) ) ;
#118967 = ORIENTED_EDGE ( 'NONE', *, *, #254731, .T. ) ;
#118966 = CYLINDRICAL_SURFACE ( 'NONE', #86368, 0.1000000000000028644 ) ;
#118968 = CARTESIAN_POINT ( 'NONE',  ( 20.94999999999999574, 65.52661458509973613, -195.9444530202758870 ) ) ;
#118969 = CARTESIAN_POINT ( 'NONE',  ( -23.25000000000000000, 7.021664781911246322, -104.3335654018973315 ) ) ;
#118971 = DIRECTION ( 'NONE',  ( 0.000000000000000000, 0.000000000000000000, -1.000000000000000000 ) ) ;
#118970 = LINE ( 'NONE', #21173, #9489 ) ;
#118972 = ADVANCED_FACE ( 'NONE', ( #197107 ), #19783, .F. ) ;
#118973 = ORIENTED_EDGE ( 'NONE', *, *, #72199, .T. ) ;
#118975 = DIRECTION ( 'NONE',  ( 0.000000000000000000, 0.9651348961777160840, -0.2617529984165015700 ) ) ;
#118974 = DIRECTION ( 'NONE',  ( 0.000000000000000000, 0.000000000000000000, -1.000000000000000000 ) ) ;
#118976 = CARTESIAN_POINT ( 'NONE',  ( 23.14999999999999858, 76.00000000001213607, -136.5231074845243313 ) ) ;
#118977 = CARTESIAN_POINT ( 'NONE',  ( 18.39999999999999503, 23.82801463864234037, -229.3483719500187306 ) ) ;
#118978 = CARTESIAN_POINT ( 'NONE',  ( -18.59999999999999787, 11.65000000001115232, -155.2500000000000284 ) ) ;
#118979 = CARTESIAN_POINT ( 'NONE',  ( -12.26136940704871847, 66.64859682587092493, -186.5435770476858863 ) ) ;
#118980 = VERTEX_POINT ( 'NONE', #253226 ) ;
#118981 = CARTESIAN_POINT ( 'NONE',  ( 23.24999999999999645, 70.40000000001199965, -115.4283735034374274 ) ) ;
#118982 = ORIENTED_EDGE ( 'NONE', *, *, #130062, .F. ) ;
#118983 = CARTESIAN_POINT ( 'NONE',  ( 23.14999999999999503, 64.35000000001249987, -177.0379132551783812 ) ) ;
#118984 = ORIENTED_EDGE ( 'NONE', *, *, #89165, .T. ) ;
#118985 = ADVANCED_FACE ( 'NONE', ( #55011 ), #18484, .T. ) ;
#118986 = CARTESIAN_POINT ( 'NONE',  ( -20.64999999999999858, 76.49733069700262433, -201.6893511817872309 ) ) ;
#118987 = CIRCLE ( 'NONE', #98090, 0.1000000000000121764 ) ;
#118988 = ORIENTED_EDGE ( 'NONE', *, *, #229821, .T. ) ;
#118989 = AXIS2_PLACEMENT_3D ( 'NONE', #107909, #130021, #247414 ) ;
#118990 = DIRECTION ( 'NONE',  ( 1.000000000000000000, -2.952720810173289112E-16, -2.061873921506763405E-30 ) ) ;
#118991 = CIRCLE ( 'NONE', #114881, 0.09999999999999939493 ) ;
#118992 = DIRECTION ( 'NONE',  ( 0.000000000000000000, 8.673617379883787770E-15, -1.000000000000000000 ) ) ;
#118994 = VERTEX_POINT ( 'NONE', #155467 ) ;
#118993 = VECTOR ( 'NONE', #195984, 1000.000000000000000 ) ;
#118995 = AXIS2_PLACEMENT_3D ( 'NONE', #10620, #90126, #169728 ) ;
#118996 = AXIS2_PLACEMENT_3D ( 'NONE', #114863, #172319, #171040 ) ;
#118998 = DIRECTION ( 'NONE',  ( 1.000000000000000000, 0.000000000000000000, 0.000000000000000000 ) ) ;
#118997 = AXIS2_PLACEMENT_3D ( 'NONE', #143808, #203789, #6872 ) ;
#118999 = CARTESIAN_POINT ( 'NONE',  ( -23.15000000000000213, 6.298909458711757559, -229.9220286223353185 ) ) ;
#119000 = DIRECTION ( 'NONE',  ( 1.000000000000000000, 0.000000000000000000, 0.000000000000000000 ) ) ;
#119001 = CARTESIAN_POINT ( 'NONE',  ( -20.54999999999999716, 36.65892442174472876, -249.5511627012454596 ) ) ;
#119002 = FACE_OUTER_BOUND ( 'NONE', #50452, .T. ) ;
#119003 = CARTESIAN_POINT ( 'NONE',  ( 22.48660254037844197, 12.58580559757026940, -223.4396719342083486 ) ) ;
#119004 = ORIENTED_EDGE ( 'NONE', *, *, #132789, .T. ) ;
#119005 = DIRECTION ( 'NONE',  ( -3.787827842127534447E-15, -0.7397360091702729346, -0.6728971962616859814 ) ) ;
#119006 = ORIENTED_EDGE ( 'NONE', *, *, #19165, .F. ) ;
#119008 = ORIENTED_EDGE ( 'NONE', *, *, #35281, .F. ) ;
#119007 = CARTESIAN_POINT ( 'NONE',  ( -16.87845715379269507, 66.04214188611484815, -90.39930683346548790 ) ) ;
#119009 = VECTOR ( 'NONE', #223972, 1000.000000000000114 ) ;
#119010 = ORIENTED_EDGE ( 'NONE', *, *, #153326, .T. ) ;
#119011 = DIRECTION ( 'NONE',  ( 0.000000000000000000, 6.982962677686266711E-15, -1.000000000000000000 ) ) ;
#119012 = CYLINDRICAL_SURFACE ( 'NONE', #24829, 0.09999999999999939493 ) ;
#119013 = CARTESIAN_POINT ( 'NONE',  ( 15.15590539855246455, 66.58931770574464792, -188.0919640425762793 ) ) ;
#119014 = AXIS2_PLACEMENT_3D ( 'NONE', #180223, #1555, #81087 ) ;
#119015 = CARTESIAN_POINT ( 'NONE',  ( 18.49999999999999289, 64.35000000001220144, -145.1731074845244507 ) ) ;
#119016 = DIRECTION ( 'NONE',  ( 0.000000000000000000, 0.000000000000000000, -1.000000000000000000 ) ) ;
#119017 = ORIENTED_EDGE ( 'NONE', *, *, #176655, .T. ) ;
#119018 = AXIS2_PLACEMENT_3D ( 'NONE', #79508, #3845, #42979 ) ;
#119019 = CARTESIAN_POINT ( 'NONE',  ( 18.59999999999998721, 6.846123162363745074, -104.2377262668499043 ) ) ;
#119020 = FACE_OUTER_BOUND ( 'NONE', #205232, .T. ) ;
#119021 = AXIS2_PLACEMENT_3D ( 'NONE', #159354, #60223, #21137 ) ;
#119022 = ORIENTED_EDGE ( 'NONE', *, *, #162615, .T. ) ;
#119024 = EDGE_LOOP ( 'NONE', ( #72560, #173351, #219332, #71819 ) ) ;
#119023 = PLANE ( 'NONE',  #5167 ) ;
#119025 = EDGE_CURVE ( 'NONE', #134210, #142111, #78443, .T. ) ;
#119026 = CYLINDRICAL_SURFACE ( 'NONE', #106572, 0.1000000000000028644 ) ;
#119027 = DIRECTION ( 'NONE',  ( -6.938893903907224433E-15, -1.000000000000000000, -6.982962677686266711E-15 ) ) ;
#119028 = EDGE_LOOP ( 'NONE', ( #182651, #64738, #77267, #92481 ) ) ;
#119029 = CARTESIAN_POINT ( 'NONE',  ( -23.25000000000000000, 87.75000000001247713, -173.1231074845242688 ) ) ;
#119030 = ORIENTED_EDGE ( 'NONE', *, *, #155424, .T. ) ;
#119031 = DIRECTION ( 'NONE',  ( 2.840903330521633255E-16, -0.8700118002898322711, 0.4930308989875231696 ) ) ;
#119032 = EDGE_CURVE ( 'NONE', #146731, #238847, #179156, .T. ) ;
#119033 = CARTESIAN_POINT ( 'NONE',  ( 15.74999999999999645, 9.850000000011137402, -83.75000000000004263 ) ) ;
#119034 = CARTESIAN_POINT ( 'NONE',  ( 23.24999999999999289, 69.55000000001206217, -124.1731074845243370 ) ) ;
#119035 = ADVANCED_FACE ( 'NONE', ( #135839 ), #99280, .F. ) ;
#119036 = DIRECTION ( 'NONE',  ( 0.000000000000000000, 0.000000000000000000, -1.000000000000000000 ) ) ;
#119037 = CIRCLE ( 'NONE', #214680, 0.09999999999999939493 ) ;
#119038 = AXIS2_PLACEMENT_3D ( 'NONE', #254696, #156956, #38275 ) ;
#119039 = AXIS2_PLACEMENT_3D ( 'NONE', #118097, #16456, #133802 ) ;
#119040 = ADVANCED_FACE ( 'NONE', ( #120192 ), #23653, .T. ) ;
#119041 = ORIENTED_EDGE ( 'NONE', *, *, #13614, .F. ) ;
#119042 = CYLINDRICAL_SURFACE ( 'NONE', #44523, 0.09999999999999939493 ) ;
#119043 = VECTOR ( 'NONE', #191297, 1000.000000000000000 ) ;
#119044 = ORIENTED_EDGE ( 'NONE', *, *, #139800, .T. ) ;
#119045 = FACE_OUTER_BOUND ( 'NONE', #9407, .T. ) ;
#119046 = CARTESIAN_POINT ( 'NONE',  ( -20.94999999999999929, -1.736257131586239844, -112.0686523290175245 ) ) ;
#119048 = ORIENTED_EDGE ( 'NONE', *, *, #14656, .F. ) ;
#119047 = CARTESIAN_POINT ( 'NONE',  ( -22.39999999999999858, 1.115600667400684642E-11, -59.20922040162664501 ) ) ;
#119049 = CARTESIAN_POINT ( 'NONE',  ( 21.09546886439543556, 67.12144688699666517, -57.28601363396898449 ) ) ;
#119050 = FACE_OUTER_BOUND ( 'NONE', #157300, .T. ) ;
#119051 = EDGE_CURVE ( 'NONE', #174644, #40125, #195722, .T. ) ;
#119052 = FACE_OUTER_BOUND ( 'NONE', #197957, .T. ) ;
#119054 = DIRECTION ( 'NONE',  ( -1.000000000000000000, -6.754466386607085130E-16, 1.507734853975053794E-15 ) ) ;
#119053 = VECTOR ( 'NONE', #24905, 1000.000000000000114 ) ;
#119055 = CARTESIAN_POINT ( 'NONE',  ( 23.24999999999999645, 11.75000000001113953, -76.25000000000004263 ) ) ;
#119056 = AXIS2_PLACEMENT_3D ( 'NONE', #43848, #60821, #120847 ) ;
#119057 = CARTESIAN_POINT ( 'NONE',  ( -18.40000000000000213, 64.66825945288736932, -182.6731074845244507 ) ) ;
#119058 = CARTESIAN_POINT ( 'NONE',  ( -18.54159361262947314, 85.46313213550527621, -129.4739852682314449 ) ) ;
#119060 = VERTEX_POINT ( 'NONE', #121466 ) ;
#119059 = FACE_OUTER_BOUND ( 'NONE', #221999, .T. ) ;
#119061 = ADVANCED_FACE ( 'NONE', ( #1474 ), #144831, .F. ) ;
#119062 = TOROIDAL_SURFACE ( 'NONE', #164845, 6.258578643762712446, 0.1000000000000000056 ) ;
#119063 = DIRECTION ( 'NONE',  ( 0.7071359030027593029, 0.7070776581709197206, 0.000000000000000000 ) ) ;
#119064 = ORIENTED_EDGE ( 'NONE', *, *, #73614, .T. ) ;
#119065 = ORIENTED_EDGE ( 'NONE', *, *, #187704, .T. ) ;
#119066 = CIRCLE ( 'NONE', #60770, 0.1000000000000004496 ) ;
#119067 = CARTESIAN_POINT ( 'NONE',  ( 23.14999999999999858, 4.813084112149524252, -11.94151775652382419 ) ) ;
#119068 = ORIENTED_EDGE ( 'NONE', *, *, #204131, .T. ) ;
#119069 = DIRECTION ( 'NONE',  ( -0.000000000000000000, 0.1350103645451876666, 0.9908441862701600211 ) ) ;
#119070 = EDGE_CURVE ( 'NONE', #9648, #114385, #83415, .T. ) ;
#119071 = DIRECTION ( 'NONE',  ( -0.7071067811865685560, -0.2890913453344204909, 0.6453109281987288171 ) ) ;
#119072 = VERTEX_POINT ( 'NONE', #21081 ) ;
#119073 = AXIS2_PLACEMENT_3D ( 'NONE', #73062, #31366, #254205 ) ;
#119074 = AXIS2_PLACEMENT_3D ( 'NONE', #150938, #68846, #209624 ) ;
#119075 = DIRECTION ( 'NONE',  ( 0.000000000000000000, 0.9651348961777157509, -0.2617529984165031243 ) ) ;
#119076 = AXIS2_PLACEMENT_3D ( 'NONE', #4184, #202399, #19929 ) ;
#119077 = VECTOR ( 'NONE', #95499, 1000.000000000000114 ) ;
#119078 = CARTESIAN_POINT ( 'NONE',  ( -16.93906926870270624, 65.98785312906605327, -190.9696551772975965 ) ) ;
#119079 = ADVANCED_FACE ( 'NONE', ( #183973 ), #203541, .T. ) ;
#119080 = ORIENTED_EDGE ( 'NONE', *, *, #190639, .T. ) ;
#119081 = FACE_OUTER_BOUND ( 'NONE', #118434, .T. ) ;
#119082 = EDGE_LOOP ( 'NONE', ( #201570, #32898, #179941, #50049 ) ) ;
#119083 = CARTESIAN_POINT ( 'NONE',  ( -22.47071067811865319, 76.00000000001195133, -103.0231074845243171 ) ) ;
#119085 = ORIENTED_EDGE ( 'NONE', *, *, #114725, .T. ) ;
#119084 = DIRECTION ( 'NONE',  ( 1.000000000000000000, -0.000000000000000000, -0.000000000000000000 ) ) ;
#119086 = ADVANCED_FACE ( 'NONE', ( #200969 ), #100548, .F. ) ;
#119087 = CARTESIAN_POINT ( 'NONE',  ( 23.25000000000000000, 85.60000000001150511, -45.91707660717669626 ) ) ;
#119088 = VERTEX_POINT ( 'NONE', #219237 ) ;
#119089 = DIRECTION ( 'NONE',  ( 2.952720810173289112E-16, 1.000000000000000000, -6.088138035986627436E-46 ) ) ;
#119090 = ORIENTED_EDGE ( 'NONE', *, *, #201323, .F. ) ;
#119092 = ORIENTED_EDGE ( 'NONE', *, *, #122709, .F. ) ;
#119091 = ORIENTED_EDGE ( 'NONE', *, *, #79657, .F. ) ;
#119093 = CARTESIAN_POINT ( 'NONE',  ( 21.05000000000000071, 69.65564095796861466, -136.5379631194182650 ) ) ;
#119094 = ORIENTED_EDGE ( 'NONE', *, *, #48001, .F. ) ;
#119095 = ADVANCED_FACE ( 'NONE', ( #40659 ), #180137, .F. ) ;
#119096 = DIRECTION ( 'NONE',  ( 1.000000000000000000, 0.000000000000000000, 0.000000000000000000 ) ) ;
#119097 = AXIS2_PLACEMENT_3D ( 'NONE', #245556, #65615, #66903 ) ;
#119098 = ORIENTED_EDGE ( 'NONE', *, *, #58668, .F. ) ;
#119099 = ADVANCED_FACE ( 'NONE', ( #101840 ), #45743, .F. ) ;
#119100 = AXIS2_PLACEMENT_3D ( 'NONE', #17624, #24091, #146557 ) ;
#119101 = EDGE_LOOP ( 'NONE', ( #150863, #234173, #57572, #211185, #40855, #199248, #4710, #129658, #245140 ) ) ;
#119102 = DIRECTION ( 'NONE',  ( 0.000000000000000000, 0.000000000000000000, -1.000000000000000000 ) ) ;
#119103 = DIRECTION ( 'NONE',  ( 1.000000000000000000, 0.000000000000000000, 0.000000000000000000 ) ) ;
#119104 = EDGE_CURVE ( 'NONE', #46909, #56627, #221784, .T. ) ;
#119106 = ORIENTED_EDGE ( 'NONE', *, *, #198635, .F. ) ;
#119105 = DIRECTION ( 'NONE',  ( -0.000000000000000000, 0.2617529984165031243, 0.9651348961777157509 ) ) ;
#119107 = CARTESIAN_POINT ( 'NONE',  ( -5.899999999999938183, 64.25000000001119815, -26.12310748452479103 ) ) ;
#119108 = ORIENTED_EDGE ( 'NONE', *, *, #203726, .T. ) ;
#119109 = CARTESIAN_POINT ( 'NONE',  ( -18.79999999999999716, 11.59510167572422112, 1.901609089591594470 ) ) ;
#119110 = CARTESIAN_POINT ( 'NONE',  ( -18.46946985241261530, -9.509317228700416180, -73.98666256549968523 ) ) ;
#119111 = FACE_OUTER_BOUND ( 'NONE', #244150, .T. ) ;
#119113 = EDGE_LOOP ( 'NONE', ( #99606, #37157, #236352, #111990, #169230 ) ) ;
#119112 = EDGE_CURVE ( 'NONE', #204366, #952, #204240, .T. ) ;
#119115 = ADVANCED_FACE ( 'NONE', ( #242652 ), #2751, .T. ) ;
#119114 = CARTESIAN_POINT ( 'NONE',  ( -20.85000000000000142, 7.021664781911246322, -137.6335654018973287 ) ) ;
#119116 = CARTESIAN_POINT ( 'NONE',  ( -18.31572283045081306, 38.18901410207342906, -261.2028819903177919 ) ) ;
#119117 = FACE_OUTER_BOUND ( 'NONE', #153408, .T. ) ;
#119118 = ORIENTED_EDGE ( 'NONE', *, *, #149528, .T. ) ;
#119119 = DIRECTION ( 'NONE',  ( 1.000000000000000000, 0.000000000000000000, 0.000000000000000000 ) ) ;
#119120 = VERTEX_POINT ( 'NONE', #82272 ) ;
#119121 = ORIENTED_EDGE ( 'NONE', *, *, #87893, .T. ) ;
#119122 = AXIS2_PLACEMENT_3D ( 'NONE', #165982, #167270, #25181 ) ;
#119123 = FACE_OUTER_BOUND ( 'NONE', #87059, .T. ) ;
#119124 = ADVANCED_FACE ( 'NONE', ( #62749 ), #202259, .F. ) ;
#119125 = VERTEX_POINT ( 'NONE', #64027 ) ;
#119126 = ORIENTED_EDGE ( 'NONE', *, *, #34340, .F. ) ;
#119127 = DIRECTION ( 'NONE',  ( 0.000000000000000000, 1.000000000000000000, 0.000000000000000000 ) ) ;
#119128 = ORIENTED_EDGE ( 'NONE', *, *, #238453, .F. ) ;
#119129 = ORIENTED_EDGE ( 'NONE', *, *, #243795, .F. ) ;
#119130 = DIRECTION ( 'NONE',  ( 0.000000000000000000, 0.000000000000000000, -1.000000000000000000 ) ) ;
#119131 = EDGE_CURVE ( 'NONE', #229236, #40931, #141879, .T. ) ;
#119132 = DIRECTION ( 'NONE',  ( 0.000000000000000000, 0.000000000000000000, -1.000000000000000000 ) ) ;
#119133 = ORIENTED_EDGE ( 'NONE', *, *, #104438, .F. ) ;
#119134 = ORIENTED_EDGE ( 'NONE', *, *, #43853, .T. ) ;
#119135 = AXIS2_PLACEMENT_3D ( 'NONE', #128623, #212019, #112906 ) ;
#119137 = AXIS2_PLACEMENT_3D ( 'NONE', #166231, #245739, #67098 ) ;
#119136 = B_SPLINE_CURVE_WITH_KNOTS ( 'NONE', 3,
 ( #57185, #237137, #199302, #96317, #42785, #217547, #38947, #138012, #40246, #2353, #160193, #136734, #98869, #197994, #218836, #181026, #200571, #175904, #62355 ),
 .UNSPECIFIED., .F., .F.,
 ( 4, 3, 3, 3, 3, 3, 4 ),
 ( -2.000416914656542534E-06, 0.000000000000000000, 4.714008503744896491E-05, 9.979203887777595382E-05, 0.0001372215519229517651, 0.0001635031576220978653, 0.0001900083748504165226 ),
 .UNSPECIFIED. ) ;
#119138 = ORIENTED_EDGE ( 'NONE', *, *, #195040, .T. ) ;
#119139 = AXIS2_PLACEMENT_3D ( 'NONE', #197818, #141696, #161288 ) ;
#119140 = VECTOR ( 'NONE', #105286, 1000.000000000000000 ) ;
#119141 =( GEOMETRIC_REPRESENTATION_CONTEXT ( 3 ) GLOBAL_UNCERTAINTY_ASSIGNED_CONTEXT ( ( #173258 ) ) GLOBAL_UNIT_ASSIGNED_CONTEXT ( ( #7251, #166378, #245884 ) ) REPRESENTATION_CONTEXT ( 'NONE', 'WORKASPACE' ) );
#119142 = CARTESIAN_POINT ( 'NONE',  ( 21.07954763557393818, 69.67070900997542537, -203.5889834031427483 ) ) ;
#119143 = ADVANCED_FACE ( 'NONE', ( #223091 ), #186497, .T. ) ;
#119144 = CARTESIAN_POINT ( 'NONE',  ( 18.45036689428337340, 85.49018414334143756, -196.5104116570379347 ) ) ;
#119145 = EDGE_CURVE ( 'NONE', #14186, #115618, #162754, .T. ) ;
#119146 = CYLINDRICAL_SURFACE ( 'NONE', #25998, 0.1000000000000000472 ) ;
#119147 = SPHERICAL_SURFACE ( 'NONE', #51498, 0.1000000000000000056 ) ;
#119148 = LINE ( 'NONE', #124288, #186821 ) ;
#119149 = DIRECTION ( 'NONE',  ( -1.000000000000000000, -0.000000000000000000, -0.000000000000000000 ) ) ;
#119150 = DIRECTION ( 'NONE',  ( 3.469446951953635015E-14, 6.982962677686266711E-15, -1.000000000000000000 ) ) ;
#119152 = LINE ( 'NONE', #117848, #137018 ) ;
#119151 = DIRECTION ( 'NONE',  ( -1.000000000000000000, -0.000000000000000000, -0.000000000000000000 ) ) ;
#119153 = FACE_OUTER_BOUND ( 'NONE', #59993, .T. ) ;
#119154 = CARTESIAN_POINT ( 'NONE',  ( -16.97683810757273193, 23.51893242087254166, -231.2247899644102631 ) ) ;
#119155 = ADVANCED_FACE ( 'NONE', ( #247798 ), #187851, .T. ) ;
#119156 = CYLINDRICAL_SURFACE ( 'NONE', #214373, 0.09999999999999950595 ) ;
#119157 = FACE_OUTER_BOUND ( 'NONE', #110176, .T. ) ;
#119158 = AXIS2_PLACEMENT_3D ( 'NONE', #67985, #105799, #47114 ) ;
#119159 = ORIENTED_EDGE ( 'NONE', *, *, #224465, .T. ) ;
#119161 = ORIENTED_EDGE ( 'NONE', *, *, #51093, .T. ) ;
#119160 = SPHERICAL_SURFACE ( 'NONE', #186517, 0.1000000000000000056 ) ;
#119162 = VECTOR ( 'NONE', #161688, 1000.000000000000114 ) ;
#119163 = CYLINDRICAL_SURFACE ( 'NONE', #128329, 0.09999999999999939493 ) ;
#119164 = CYLINDRICAL_SURFACE ( 'NONE', #190287, 0.1000000000000072220 ) ;
#119165 = CONICAL_SURFACE ( 'NONE', #219107, 4.049999999999998046, 0.7853981633974604915 ) ;
#119166 = VECTOR ( 'NONE', #208643, 1000.000000000000000 ) ;
#119167 = CARTESIAN_POINT ( 'NONE',  ( -18.50000000000000000, -1.162701749926853712, -75.10000000000003695 ) ) ;
#119168 = VERTEX_POINT ( 'NONE', #167019 ) ;
#119169 = EDGE_CURVE ( 'NONE', #227500, #185809, #209972, .T. ) ;
#119170 = DIRECTION ( 'NONE',  ( 0.5932847527679309119, -0.7865547670005532677, -0.1713032417725953160 ) ) ;
#119171 = EDGE_CURVE ( 'NONE', #237840, #196267, #169599, .T. ) ;
#119172 = CARTESIAN_POINT ( 'NONE',  ( -20.94999999999999929, 76.00000000001210765, -132.5231074845243313 ) ) ;
#119173 = ORIENTED_EDGE ( 'NONE', *, *, #197227, .F. ) ;
#119175 = CARTESIAN_POINT ( 'NONE',  ( -18.51697539158857353, 10.31565961587945957, -206.5364194119177910 ) ) ;
#119174 = AXIS2_PLACEMENT_3D ( 'NONE', #25492, #184538, #127149 ) ;
#119176 = CARTESIAN_POINT ( 'NONE',  ( -20.54999999999999716, 2.000000000011154189, -79.72462192276213955 ) ) ;
#119177 = CIRCLE ( 'NONE', #90120, 0.09999999999999939493 ) ;
#119178 = DIRECTION ( 'NONE',  ( 0.000000000000000000, 0.000000000000000000, -1.000000000000000000 ) ) ;
#119179 = CIRCLE ( 'NONE', #177657, 11.64999999999999325 ) ;
#119180 = EDGE_CURVE ( 'NONE', #47775, #156378, #150114, .T. ) ;
#119181 = CARTESIAN_POINT ( 'NONE',  ( 21.05000000000000071, 65.49732036650624423, -236.6319166190174883 ) ) ;
#119183 = VERTEX_POINT ( 'NONE', #208698 ) ;
#119182 = LINE ( 'NONE', #77448, #122793 ) ;
#119184 = CIRCLE ( 'NONE', #123460, 0.1000000000000028644 ) ;
#119186 = ORIENTED_EDGE ( 'NONE', *, *, #158121, .T. ) ;
#119185 = CARTESIAN_POINT ( 'NONE',  ( 18.49999999999999645, 46.62132166459547733, -243.0426574061995950 ) ) ;
#119188 = EDGE_CURVE ( 'NONE', #37642, #211497, #208551, .T. ) ;
#119187 = LINE ( 'NONE', #83856, #133460 ) ;
#119189 = CARTESIAN_POINT ( 'NONE',  ( -18.59999999999999787, -9.499999999988842703, -45.65000000000001279 ) ) ;
#119190 = DIRECTION ( 'NONE',  ( 0.000000000000000000, -1.000000000000000000, -6.982962677686265922E-15 ) ) ;
#119191 = CARTESIAN_POINT ( 'NONE',  ( -14.56556274378147542, 9.446557523083688679, -182.5899419543458464 ) ) ;
#119193 = CARTESIAN_POINT ( 'NONE',  ( 19.99999999999998934, 31.36165455396662693, -233.4973802202241302 ) ) ;
#119192 = CARTESIAN_POINT ( 'NONE',  ( -16.89155683852495926, 9.950000000011137047, -154.2226281504603662 ) ) ;
#119195 = EDGE_CURVE ( 'NONE', #242379, #66129, #185261, .T. ) ;
#119194 = LINE ( 'NONE', #219552, #162017 ) ;
#119196 = CARTESIAN_POINT ( 'NONE',  ( 22.60000000000000142, 0.04781839071596409585, -155.7499775809527307 ) ) ;
#119197 = CIRCLE ( 'NONE', #110809, 4.049999999999998046 ) ;
#119198 = CARTESIAN_POINT ( 'NONE',  ( -21.52071067811865746, 44.74916609337672924, -237.4025894497016225 ) ) ;
#119199 = CARTESIAN_POINT ( 'NONE',  ( 21.07928932188134397, 0.09889514566555242248, -161.1714833436066385 ) ) ;
#119200 = CARTESIAN_POINT ( 'NONE',  ( -20.94999999999999929, 7.021664781911246322, -137.8335654018973457 ) ) ;
#119201 = B_SPLINE_CURVE_WITH_KNOTS ( 'NONE', 3,
 ( #214460, #158390, #257387, #116655, #60516, #80055, #201328, #177931, #196194, #99629, #236588, #78789, #76232 ),
 .UNSPECIFIED., .F., .F.,
 ( 4, 3, 3, 3, 4 ),
 ( -3.224855718259041645E-06, 0.000000000000000000, 6.199515528676308480E-06, 4.034952380128061856E-05, 7.452715123701166987E-05 ),
 .UNSPECIFIED. ) ;
#119202 = EDGE_LOOP ( 'NONE', ( #54387, #159612, #168151, #105718 ) ) ;
#119203 = EDGE_CURVE ( 'NONE', #64247, #113685, #228250, .T. ) ;
#119204 = DIRECTION ( 'NONE',  ( 1.000000000000000000, -0.000000000000000000, -0.000000000000000000 ) ) ;
#119206 = EDGE_CURVE ( 'NONE', #166854, #19071, #37679, .T. ) ;
#119205 = EDGE_CURVE ( 'NONE', #131204, #204385, #29504, .T. ) ;
#119207 = EDGE_LOOP ( 'NONE', ( #125796, #92800, #149061, #255277 ) ) ;
#119208 = VERTEX_POINT ( 'NONE', #168313 ) ;
#119209 = DIRECTION ( 'NONE',  ( 0.000000000000000000, 1.000000000000000000, 0.000000000000000000 ) ) ;
#119210 = CARTESIAN_POINT ( 'NONE',  ( 18.49999999999999289, 11.65000000001115943, -192.3499999999999659 ) ) ;
#119211 = EDGE_LOOP ( 'NONE', ( #28628, #86380, #245575 ) ) ;
#119212 = VECTOR ( 'NONE', #246380, 1000.000000000000000 ) ;
#119213 = CIRCLE ( 'NONE', #169324, 0.1000000000000028644 ) ;
#119214 = ORIENTED_EDGE ( 'NONE', *, *, #197799, .F. ) ;
#119215 = SURFACE_STYLE_FILL_AREA ( #4379 ) ;
#119216 = AXIS2_PLACEMENT_3D ( 'NONE', #182366, #4966, #158971 ) ;
#119217 = AXIS2_PLACEMENT_3D ( 'NONE', #185775, #9697, #168828 ) ;
#119218 = ORIENTED_EDGE ( 'NONE', *, *, #171220, .F. ) ;
#119219 = EDGE_CURVE ( 'NONE', #196929, #103174, #245956, .T. ) ;
#119220 = ADVANCED_FACE ( 'NONE', ( #10484 ), #158486, .F. ) ;
#119221 = VERTEX_POINT ( 'NONE', #91303 ) ;
#119222 = CIRCLE ( 'NONE', #206878, 0.1999999999999987899 ) ;
#119223 = DIRECTION ( 'NONE',  ( 0.000000000000000000, 0.000000000000000000, -1.000000000000000000 ) ) ;
#119224 = DIRECTION ( 'NONE',  ( -1.020425574104003999E-15, -0.8814952561688430555, 0.4721928772777346239 ) ) ;
#119225 = DIRECTION ( 'NONE',  ( 0.000000000000000000, 0.000000000000000000, -1.000000000000000000 ) ) ;
#119226 = CARTESIAN_POINT ( 'NONE',  ( -20.94999999999999929, -1.162701749938009677, -8.099999999999999645 ) ) ;
#119227 = DIRECTION ( 'NONE',  ( 0.000000000000000000, -1.000000000000000000, -6.982962677686265922E-15 ) ) ;
#119228 = ADVANCED_FACE ( 'NONE', ( #52153 ), #46022, .T. ) ;
#119229 = CARTESIAN_POINT ( 'NONE',  ( 21.14999999999999503, -11.74999999998883560, -55.25000000000004974 ) ) ;
#119230 = CARTESIAN_POINT ( 'NONE',  ( 21.07928932188134397, 75.90110485435755550, -142.8516241409230076 ) ) ;
#119232 = ORIENTED_EDGE ( 'NONE', *, *, #218691, .F. ) ;
#119231 = DIRECTION ( 'NONE',  ( -0.000000000000000000, -0.000000000000000000, 1.000000000000000000 ) ) ;
#119234 = DIRECTION ( 'NONE',  ( -0.000000000000000000, -6.982962677686266711E-15, 1.000000000000000000 ) ) ;
#119233 = DIRECTION ( 'NONE',  ( -1.000000000000000000, -0.000000000000000000, 0.000000000000000000 ) ) ;
#119235 = DIRECTION ( 'NONE',  ( 0.000000000000000000, -6.982962677686267499E-15, 1.000000000000000000 ) ) ;
#119236 = CIRCLE ( 'NONE', #202612, 0.09999999999999999167 ) ;
#119237 = VERTEX_POINT ( 'NONE', #15646 ) ;
#119238 = CARTESIAN_POINT ( 'NONE',  ( 23.14999999999998437, 64.25000000001269029, -203.5231074845244166 ) ) ;
#119239 = DIRECTION ( 'NONE',  ( 0.000000000000000000, 0.000000000000000000, -1.000000000000000000 ) ) ;
#119241 = ORIENTED_EDGE ( 'NONE', *, *, #206955, .F. ) ;
#119240 = AXIS2_PLACEMENT_3D ( 'NONE', #207820, #168715, #227343 ) ;
#119242 = ADVANCED_FACE ( 'NONE', ( #95147 ), #88208, .T. ) ;
#119243 = CIRCLE ( 'NONE', #44232, 0.09999999999998898659 ) ;
#119245 = CARTESIAN_POINT ( 'NONE',  ( -16.93826681692523195, 65.98857127972429737, -115.5776490171649300 ) ) ;
#119244 = DIRECTION ( 'NONE',  ( 0.000000000000000000, 0.000000000000000000, -1.000000000000000000 ) ) ;
#119246 = B_SPLINE_CURVE_WITH_KNOTS ( 'NONE', 3,
 ( #83718, #202424, #66773, #100714, #180295, #64203, #143727, #25100, #65473, #145001 ),
 .UNSPECIFIED., .F., .F.,
 ( 4, 2, 2, 2, 4 ),
 ( 0.000000000000000000, 4.221631689688417835E-05, 8.443263379376835670E-05, 0.0001688652675874643971, 0.0003377305351749477678 ),
 .UNSPECIFIED. ) ;
#119247 = CARTESIAN_POINT ( 'NONE',  ( -20.54999999999999716, 1.115600667400684642E-11, -100.5000000000000426 ) ) ;
#119248 = DIRECTION ( 'NONE',  ( 1.000000000000000000, 0.000000000000000000, 0.000000000000000000 ) ) ;
#119249 = ORIENTED_EDGE ( 'NONE', *, *, #121745, .T. ) ;
#119250 = CARTESIAN_POINT ( 'NONE',  ( -23.25000000000000000, 77.16412189325305349, -95.10825939895268277 ) ) ;
#119251 = DIRECTION ( 'NONE',  ( 0.000000000000000000, 6.982962677686266711E-15, -1.000000000000000000 ) ) ;
#119252 = CIRCLE ( 'NONE', #77701, 0.2000000000000005107 ) ;
#119253 = CARTESIAN_POINT ( 'NONE',  ( 22.57320508075687115, 64.25000000001195133, -103.0231074845244024 ) ) ;
#119255 = EDGE_CURVE ( 'NONE', #255303, #90335, #172162, .T. ) ;
#119254 = CARTESIAN_POINT ( 'NONE',  ( -18.40000000000000213, 11.75000000001113953, -79.65000000000004832 ) ) ;
#119256 = ORIENTED_EDGE ( 'NONE', *, *, #111161, .T. ) ;
#119257 = DIRECTION ( 'NONE',  ( -1.000000000000000000, 0.000000000000000000, 0.000000000000000000 ) ) ;
#119259 = ADVANCED_FACE ( 'NONE', ( #138104 ), #37764, .T. ) ;
#119258 = CARTESIAN_POINT ( 'NONE',  ( -16.87036670365548474, 9.989418819312799513, -121.4795601173020856 ) ) ;
#119260 = DIRECTION ( 'NONE',  ( 0.000000000000000000, 0.4999999999999949485, -0.8660254037844415942 ) ) ;
#119261 = CYLINDRICAL_SURFACE ( 'NONE', #55046, 11.80000000000000426 ) ;
#119262 = CIRCLE ( 'NONE', #215118, 11.74999999999999645 ) ;
#119263 = AXIS2_PLACEMENT_3D ( 'NONE', #62109, #4671, #123366 ) ;
#119264 = DIRECTION ( 'NONE',  ( 0.000000000000000000, 0.000000000000000000, 1.000000000000000000 ) ) ;
#119265 = AXIS2_PLACEMENT_3D ( 'NONE', #242488, #100391, #102968 ) ;
#119266 = VECTOR ( 'NONE', #131370, 1000.000000000000000 ) ;
#119267 = CARTESIAN_POINT ( 'NONE',  ( -23.15000000000000213, 76.00000000001222134, -149.3981074845243313 ) ) ;
#119269 = ORIENTED_EDGE ( 'NONE', *, *, #225802, .T. ) ;
#119268 = DIRECTION ( 'NONE',  ( -1.000000000000000000, 0.000000000000000000, -0.000000000000000000 ) ) ;
#119270 = DIRECTION ( 'NONE',  ( 0.000000000000000000, 0.9126074666063622720, 0.4088369013363611360 ) ) ;
#119271 = CARTESIAN_POINT ( 'NONE',  ( 21.00000000000000000, 51.97441255244040548, -232.0063394385699667 ) ) ;
#119272 = DIRECTION ( 'NONE',  ( 0.000000000000000000, -0.000000000000000000, 1.000000000000000000 ) ) ;
#119273 = CARTESIAN_POINT ( 'NONE',  ( 21.05000000000000426, -0.01681986837452038863, -94.19257478043464005 ) ) ;
#119274 = EDGE_CURVE ( 'NONE', #148199, #236846, #191816, .T. ) ;
#119275 = DIRECTION ( 'NONE',  ( 0.000000000000000000, 0.000000000000000000, -1.000000000000000000 ) ) ;
#119276 = EDGE_LOOP ( 'NONE', ( #144090, #133433, #8095, #200990 ) ) ;
#119277 = FACE_OUTER_BOUND ( 'NONE', #257320, .T. ) ;
#119278 = FACE_OUTER_BOUND ( 'NONE', #199237, .T. ) ;
#119279 = FACE_OUTER_BOUND ( 'NONE', #171547, .T. ) ;
#119280 = VERTEX_POINT ( 'NONE', #74340 ) ;
#119281 = DIRECTION ( 'NONE',  ( 0.000000000000000000, 0.000000000000000000, 1.000000000000000000 ) ) ;
#119282 = DIRECTION ( 'NONE',  ( -0.000000000000000000, -0.9126074666063770380, -0.4088369013363281068 ) ) ;
#119283 = CIRCLE ( 'NONE', #206749, 0.09999999999998898659 ) ;
#119284 = AXIS2_PLACEMENT_3D ( 'NONE', #200987, #43201, #4062 ) ;
#119285 = CARTESIAN_POINT ( 'NONE',  ( -18.43599941264924169, 78.24390722508243812, -231.6169757740163107 ) ) ;
#119286 = CYLINDRICAL_SURFACE ( 'NONE', #238273, 0.1000000000000028644 ) ;
#119287 = ORIENTED_EDGE ( 'NONE', *, *, #240929, .T. ) ;
#119288 = VERTEX_POINT ( 'NONE', #155158 ) ;
#119290 = SPHERICAL_SURFACE ( 'NONE', #234872, 0.1000000000000000056 ) ;
#119289 = AXIS2_PLACEMENT_3D ( 'NONE', #14808, #248252, #110014 ) ;
#119291 = DIRECTION ( 'NONE',  ( 0.000000000000000000, 0.2617529984165152257, 0.9651348961777124202 ) ) ;
#119292 = DIRECTION ( 'NONE',  ( 2.952720810173288619E-16, -1.000000000000000000, 0.000000000000000000 ) ) ;
#119293 = ORIENTED_EDGE ( 'NONE', *, *, #20980, .T. ) ;
#119294 = CARTESIAN_POINT ( 'NONE',  ( 20.95512820512820440, 10.62384868372303615, -175.1649135690875880 ) ) ;
#119295 = CARTESIAN_POINT ( 'NONE',  ( 18.49999999999999645, -1.162701749938011453, -8.099999999999999645 ) ) ;
#119296 = CARTESIAN_POINT ( 'NONE',  ( -16.81095280782811230, 9.949999999999983302, -12.64999999999912639 ) ) ;
#119297 = CARTESIAN_POINT ( 'NONE',  ( 20.95561247346651967, 10.59500736521470721, -108.0937827669816755 ) ) ;
#119298 = CARTESIAN_POINT ( 'NONE',  ( -16.87683809663752399, 9.849999999999983658, -20.09763598180368405 ) ) ;
#119299 = AXIS2_PLACEMENT_3D ( 'NONE', #57540, #174990, #95401 ) ;
#119300 = ORIENTED_EDGE ( 'NONE', *, *, #207301, .F. ) ;
#119301 = CARTESIAN_POINT ( 'NONE',  ( 18.59999999999997655, 1.115600667400684642E-11, -167.5000000000000284 ) ) ;
#119302 = VERTEX_POINT ( 'NONE', #96410 ) ;
#119303 = CARTESIAN_POINT ( 'NONE',  ( 23.14999999999999858, 76.00000000001260503, -190.6481074845243597 ) ) ;
#119304 = ORIENTED_EDGE ( 'NONE', *, *, #3317, .T. ) ;
#119305 = CARTESIAN_POINT ( 'NONE',  ( -20.85000000000000142, 45.93315328338058379, -256.6017782078560003 ) ) ;
#119306 = DIRECTION ( 'NONE',  ( -0.000000000000000000, -0.8660254037844420383, 0.4999999999999943379 ) ) ;
#119307 = CARTESIAN_POINT ( 'NONE',  ( -21.05000000000000071, 75.74389420791992222, -136.5580039261965908 ) ) ;
#119308 = ORIENTED_EDGE ( 'NONE', *, *, #41453, .T. ) ;
#119309 = PLANE ( 'NONE',  #44951 ) ;
#119310 = DIRECTION ( 'NONE',  ( -1.000000000000000000, 0.000000000000000000, 0.000000000000000000 ) ) ;
#119311 = VECTOR ( 'NONE', #112513, 1000.000000000000000 ) ;
#119312 = EDGE_LOOP ( 'NONE', ( #91055, #40275, #160285, #254343 ) ) ;
#119313 = CARTESIAN_POINT ( 'NONE',  ( -15.31895204843004699, 9.396533993965073606, -151.9059397791733090 ) ) ;
#119315 = VERTEX_POINT ( 'NONE', #175993 ) ;
#119314 = LINE ( 'NONE', #39805, #96572 ) ;
#119316 = EDGE_CURVE ( 'NONE', #72318, #22952, #196801, .T. ) ;
#119317 = CARTESIAN_POINT ( 'NONE',  ( 21.05000000000000071, 11.40444339177024169, -198.6185779617709670 ) ) ;
#119318 = CARTESIAN_POINT ( 'NONE',  ( 23.14999999999999858, 7.128833340094563376, -233.7327013124401276 ) ) ;
#119319 = VECTOR ( 'NONE', #147498, 1000.000000000000000 ) ;
#119320 = CIRCLE ( 'NONE', #239950, 11.80000000000000426 ) ;
#119321 = VECTOR ( 'NONE', #119460, 1000.000000000000000 ) ;
#119322 = ORIENTED_EDGE ( 'NONE', *, *, #225967, .T. ) ;
#119323 = CARTESIAN_POINT ( 'NONE',  ( -16.77977881697927032, 9.946601933544062746, -79.66137857311510118 ) ) ;
#119324 = CARTESIAN_POINT ( 'NONE',  ( 20.94999999999999929, 71.14953271029217774, -81.55737489352601699 ) ) ;
#119325 = CARTESIAN_POINT ( 'NONE',  ( -21.05000000000000071, 1.627786319807483340, -244.0021210468063089 ) ) ;
#119326 = VERTEX_POINT ( 'NONE', #233401 ) ;
#119327 = DIRECTION ( 'NONE',  ( 1.000000000000000000, -7.166229603267617241E-16, -4.447280054184918885E-16 ) ) ;
#119328 = EDGE_CURVE ( 'NONE', #98586, #192518, #32650, .T. ) ;
#119329 = CARTESIAN_POINT ( 'NONE',  ( 12.84435279558019971, 49.30157392506335867, -233.5755204583867055 ) ) ;
#119330 = FACE_OUTER_BOUND ( 'NONE', #202246, .T. ) ;
#119331 = EDGE_CURVE ( 'NONE', #137137, #159306, #18176, .T. ) ;
#119332 = VERTEX_POINT ( 'NONE', #53456 ) ;
#119333 = ORIENTED_EDGE ( 'NONE', *, *, #217117, .T. ) ;
#119334 = TOROIDAL_SURFACE ( 'NONE', #240146, 0.4000000000000005773, 0.1000000000000000056 ) ;
#119335 = AXIS2_PLACEMENT_3D ( 'NONE', #24148, #141499, #243167 ) ;
#119336 = ORIENTED_EDGE ( 'NONE', *, *, #204273, .T. ) ;
#119337 = ADVANCED_FACE ( 'NONE', ( #192973 ), #78133, .F. ) ;
#119338 = AXIS2_PLACEMENT_3D ( 'NONE', #235264, #237843, #80015 ) ;
#119339 = EDGE_LOOP ( 'NONE', ( #221392, #117718, #34175, #115230 ) ) ;
#119340 = EDGE_CURVE ( 'NONE', #11251, #140147, #71004, .T. ) ;
#119341 = AXIS2_PLACEMENT_3D ( 'NONE', #154966, #93678, #15445 ) ;
#119342 = DIRECTION ( 'NONE',  ( 0.000000000000000000, -0.9908441862701411473, 0.1350103645453267498 ) ) ;
#119343 = CARTESIAN_POINT ( 'NONE',  ( -20.64999999999999858, 68.85000000001156195, -57.27310748452436684 ) ) ;
#119345 = ORIENTED_EDGE ( 'NONE', *, *, #223539, .T. ) ;
#119344 = CARTESIAN_POINT ( 'NONE',  ( -23.15000000000000213, 85.00000000001207923, -126.6291383618717816 ) ) ;
#119346 = CARTESIAN_POINT ( 'NONE',  ( -21.55000000000000426, 21.65523568329831505, -232.7692078405380300 ) ) ;
#119348 = AXIS2_PLACEMENT_3D ( 'NONE', #184461, #187062, #64519 ) ;
#119347 = CARTESIAN_POINT ( 'NONE',  ( 23.25000000000000000, 87.75000000001173817, -81.27310748452423184 ) ) ;
#119349 = ADVANCED_FACE ( 'NONE', ( #113427 ), #16907, .F. ) ;
#119350 = FACE_OUTER_BOUND ( 'NONE', #212979, .T. ) ;
#119351 = AXIS2_PLACEMENT_3D ( 'NONE', #253519, #55294, #214399 ) ;
#119352 = CARTESIAN_POINT ( 'NONE',  ( 18.59999999999997655, 36.65892442174935439, -249.5511627012433848 ) ) ;
#119353 = DIRECTION ( 'NONE',  ( 0.000000000000000000, -1.000000000000000000, 0.000000000000000000 ) ) ;
#119354 = DIRECTION ( 'NONE',  ( 1.186688945009010077E-16, -0.9770955615653316162, -0.2128009952263604232 ) ) ;
#119356 = ORIENTED_EDGE ( 'NONE', *, *, #116315, .T. ) ;
#119355 = DIRECTION ( 'NONE',  ( 1.000000000000000000, 0.000000000000000000, 0.000000000000000000 ) ) ;
#119358 = VERTEX_POINT ( 'NONE', #19470 ) ;
#119357 = CARTESIAN_POINT ( 'NONE',  ( -20.85000000000000142, 77.83585931145600512, -158.5186683157258187 ) ) ;
#119359 = CARTESIAN_POINT ( 'NONE',  ( -23.15000000000000213, 64.25000000001253397, -182.1731074845244507 ) ) ;
#119360 = EDGE_CURVE ( 'NONE', #155283, #133238, #129419, .T. ) ;
#119361 = VERTEX_POINT ( 'NONE', #98962 ) ;
#119362 = ORIENTED_EDGE ( 'NONE', *, *, #230229, .F. ) ;
#119363 = CARTESIAN_POINT ( 'NONE',  ( -21.05000000000000071, 6.257814610487270279, -167.4022097086911742 ) ) ;
#119364 = DIRECTION ( 'NONE',  ( -0.000000000000000000, 0.000000000000000000, 1.000000000000000000 ) ) ;
#119365 = AXIS2_PLACEMENT_3D ( 'NONE', #158304, #116575, #137405 ) ;
#119366 = AXIS2_PLACEMENT_3D ( 'NONE', #168655, #246840, #8255 ) ;
#119367 = ADVANCED_FACE ( 'NONE', ( #62447 ), #242353, .T. ) ;
#119368 = AXIS2_PLACEMENT_3D ( 'NONE', #34644, #16361, #193704 ) ;
#119369 = DIRECTION ( 'NONE',  ( 0.000000000000000000, 0.4721928772777346239, 0.8814952561688430555 ) ) ;
#119370 = DIRECTION ( 'NONE',  ( 1.000000000000000000, -2.808674667590276147E-16, -1.035613708381807261E-15 ) ) ;
#119371 = CARTESIAN_POINT ( 'NONE',  ( 22.39999999999999503, 11.75000000001115552, -167.4999999999999716 ) ) ;
#119372 = DIRECTION ( 'NONE',  ( 0.000000000000000000, -0.2128009952263601734, 0.9770955615653316162 ) ) ;
#119373 = ADVANCED_FACE ( 'NONE', ( #100249 ), #96081, .T. ) ;
#119374 = CYLINDRICAL_SURFACE ( 'NONE', #202211, 2.000000000000012879 ) ;
#119375 = ORIENTED_EDGE ( 'NONE', *, *, #108700, .F. ) ;
#119376 = ORIENTED_EDGE ( 'NONE', *, *, #237414, .F. ) ;
#119377 = CARTESIAN_POINT ( 'NONE',  ( 18.49999999999999645, 77.16270174995010223, -128.4231074845242802 ) ) ;
#119378 = CIRCLE ( 'NONE', #194234, 4.049999999999998046 ) ;
#119379 = VERTEX_POINT ( 'NONE', #182401 ) ;
#119380 = CARTESIAN_POINT ( 'NONE',  ( 23.14999999999999858, 76.00000000001244871, -170.0231074845243597 ) ) ;
#119381 = CARTESIAN_POINT ( 'NONE',  ( -17.11825945287482043, 51.61886293219122024, -231.9464690156495976 ) ) ;
#119382 = CARTESIAN_POINT ( 'NONE',  ( 21.14999999999999503, 87.75000000001234923, -167.1231074845242688 ) ) ;
#119383 = CARTESIAN_POINT ( 'NONE',  ( -18.40000000000000213, 11.47316190337362762, -146.5500000000000114 ) ) ;
#119384 = EDGE_LOOP ( 'NONE', ( #3423, #106499, #63943 ) ) ;
#119385 = CARTESIAN_POINT ( 'NONE',  ( -21.14999999999999858, 11.38316329224760359, -198.5208684056144079 ) ) ;
#119386 = ORIENTED_EDGE ( 'NONE', *, *, #99914, .F. ) ;
#119387 = CARTESIAN_POINT ( 'NONE',  ( -21.05000000000000071, -10.76604040606818025, -206.3127087229280789 ) ) ;
#119388 = ORIENTED_EDGE ( 'NONE', *, *, #9151, .F. ) ;
#119389 = CIRCLE ( 'NONE', #81746, 0.09999999999999939493 ) ;
#119390 = CARTESIAN_POINT ( 'NONE',  ( -20.54999999999999716, 0.000000000000000000, -20.62500000000000355 ) ) ;
#119391 = CIRCLE ( 'NONE', #144294, 0.09999999999999939493 ) ;
#119392 = CARTESIAN_POINT ( 'NONE',  ( -16.86422026484316916, 9.970447360871810716, -113.0822132256730299 ) ) ;
#119393 = AXIS2_PLACEMENT_3D ( 'NONE', #34236, #194592, #175051 ) ;
#119394 = AXIS2_PLACEMENT_3D ( 'NONE', #168526, #248004, #69395 ) ;
#119395 = ORIENTED_EDGE ( 'NONE', *, *, #119416, .T. ) ;
#119397 = VERTEX_POINT ( 'NONE', #239806 ) ;
#119396 = DIRECTION ( 'NONE',  ( 1.186688945009010077E-16, 1.000000000000000000, 6.982962677686266711E-15 ) ) ;
#119398 = DIRECTION ( 'NONE',  ( 0.000000000000000000, -0.5273008465188219196, 0.8496786552930077896 ) ) ;
#119399 = ORIENTED_EDGE ( 'NONE', *, *, #144929, .F. ) ;
#119400 = EDGE_CURVE ( 'NONE', #40817, #120793, #254303, .T. ) ;
#119402 = DIRECTION ( 'NONE',  ( -0.000000000000000000, -0.6132151058540604716, 0.7899159663865477077 ) ) ;
#119401 =( BOUNDED_CURVE ( )  B_SPLINE_CURVE ( 3, ( #197501, #115401, #37174, #116685 ),
 .UNSPECIFIED., .F., .F. ) 
 B_SPLINE_CURVE_WITH_KNOTS ( ( 4, 4 ),
 ( 3.141592653589793116, 4.712388980384689674 ),
 .UNSPECIFIED. ) 
 CURVE ( )  GEOMETRIC_REPRESENTATION_ITEM ( )  RATIONAL_B_SPLINE_CURVE ( ( 1.000000000000000000, 0.8047378541243649375, 0.8047378541243649375, 1.000000000000000000 ) ) 
 REPRESENTATION_ITEM ( '' )  );
#119403 = ORIENTED_EDGE ( 'NONE', *, *, #11707, .F. ) ;
#119404 = DIRECTION ( 'NONE',  ( -4.336808689942052446E-15, 0.8660254037844445918, 0.4999999999999896194 ) ) ;
#119405 = EDGE_CURVE ( 'NONE', #82203, #11722, #44174, .T. ) ;
#119406 = CARTESIAN_POINT ( 'NONE',  ( 22.42196299218230493, 26.02640355241475589, -254.3117255616162424 ) ) ;
#119408 = ADVANCED_FACE ( 'NONE', ( #80695 ), #121166, .T. ) ;
#119407 = VECTOR ( 'NONE', #77457, 1000.000000000000114 ) ;
#119409 = DIRECTION ( 'NONE',  ( 0.000000000000000000, -1.000000000000000000, -6.982962677686266711E-15 ) ) ;
#119410 = CARTESIAN_POINT ( 'NONE',  ( 20.85000000000000142, 77.13501884592155022, -28.30613060109199353 ) ) ;
#119411 = CIRCLE ( 'NONE', #186043, 0.09999999999999939493 ) ;
#119412 = DIRECTION ( 'NONE',  ( 0.000000000000000000, 0.000000000000000000, -1.000000000000000000 ) ) ;
#119413 = VECTOR ( 'NONE', #210051, 1000.000000000000000 ) ;
#119415 = EDGE_LOOP ( 'NONE', ( #93759, #26581, #19976, #167840 ) ) ;
#119414 = ADVANCED_FACE ( 'NONE', ( #123707 ), #199405, .F. ) ;
#119416 = EDGE_CURVE ( 'NONE', #217031, #163189, #196066, .T. ) ;
#119417 = CARTESIAN_POINT ( 'NONE',  ( -16.97683809663752186, 9.950000000011138823, -53.59763598180368405 ) ) ;
#119418 = CARTESIAN_POINT ( 'NONE',  ( -21.05000000000000071, -11.48912529306490349, -36.60000000000000142 ) ) ;
#119419 = CARTESIAN_POINT ( 'NONE',  ( 22.47071067811865319, 0.3704148268517115650, -229.9999874772931037 ) ) ;
#119420 = EDGE_CURVE ( 'NONE', #112737, #145941, #41959, .T. ) ;
#119421 = ORIENTED_EDGE ( 'NONE', *, *, #90042, .F. ) ;
#119422 = CARTESIAN_POINT ( 'NONE',  ( 21.07094088545303734, 6.154362662572053999, -199.5584335273501324 ) ) ;
#119424 = EDGE_CURVE ( 'NONE', #157942, #66650, #59250, .T. ) ;
#119423 = ORIENTED_EDGE ( 'NONE', *, *, #92937, .T. ) ;
#119425 = DIRECTION ( 'NONE',  ( 0.000000000000000000, 0.4721928772778128947, 0.8814952561688012000 ) ) ;
#119426 = ORIENTED_EDGE ( 'NONE', *, *, #47582, .F. ) ;
#119427 = LINE ( 'NONE', #197658, #1206 ) ;
#119428 = CARTESIAN_POINT ( 'NONE',  ( -20.94999675878240808, 10.29307482169070909, -72.45864214669403225 ) ) ;
#119429 = ADVANCED_FACE ( 'NONE', ( #160287 ), #5003, .F. ) ;
#119430 = ORIENTED_EDGE ( 'NONE', *, *, #32335, .T. ) ;
#119431 = AXIS2_PLACEMENT_3D ( 'NONE', #39639, #119150, #198674 ) ;
#119433 = VERTEX_POINT ( 'NONE', #198096 ) ;
#119432 = CARTESIAN_POINT ( 'NONE',  ( -20.65000000000000568, 7.250000000011138646, -42.75000000000000000 ) ) ;
#119434 = CARTESIAN_POINT ( 'NONE',  ( -18.45037301276669695, 8.829267269132847318, -245.4096027649236191 ) ) ;
#119435 = ORIENTED_EDGE ( 'NONE', *, *, #250632, .F. ) ;
#119437 = B_SPLINE_CURVE_WITH_KNOTS ( 'NONE', 3,
 ( #66874, #125560, #146386, #65585, #26476, #105971 ),
 .UNSPECIFIED., .F., .F.,
 ( 4, 2, 4 ),
 ( 0.000000000000000000, 0.0001891491689349542970, 0.0003782983378699085941 ),
 .UNSPECIFIED. ) ;
#119436 = DIRECTION ( 'NONE',  ( -1.000000000000000000, 0.000000000000000000, 0.000000000000000000 ) ) ;
#119438 = DIRECTION ( 'NONE',  ( 0.000000000000000000, 6.982962677686266711E-15, -1.000000000000000000 ) ) ;
#119439 = ORIENTED_EDGE ( 'NONE', *, *, #76909, .T. ) ;
#119440 = ORIENTED_EDGE ( 'NONE', *, *, #121490, .T. ) ;
#119441 = DIRECTION ( 'NONE',  ( 0.000000000000000000, 0.2617529984165031243, 0.9651348961777157509 ) ) ;
#119442 = CARTESIAN_POINT ( 'NONE',  ( -21.05000000000000071, 67.46931694187804851, -235.9558427390807083 ) ) ;
#119443 = ORIENTED_EDGE ( 'NONE', *, *, #243245, .F. ) ;
#119444 = DIRECTION ( 'NONE',  ( 0.000000000000000000, -0.01562499999996560217, -0.9998779222360102414 ) ) ;
#119445 = CIRCLE ( 'NONE', #252695, 0.1000000000000074579 ) ;
#119446 = AXIS2_PLACEMENT_3D ( 'NONE', #90485, #48795, #170085 ) ;
#119447 = VECTOR ( 'NONE', #134281, 1000.000000000000000 ) ;
#119448 = EDGE_LOOP ( 'NONE', ( #60779, #224612, #196903, #253766 ) ) ;
#119449 = VERTEX_POINT ( 'NONE', #118582 ) ;
#119450 = EDGE_CURVE ( 'NONE', #137714, #52387, #75470, .T. ) ;
#119451 = DIRECTION ( 'NONE',  ( -0.000000000000000000, 6.982962677686266711E-15, -1.000000000000000000 ) ) ;
#119452 = EDGE_CURVE ( 'NONE', #6741, #242523, #179509, .T. ) ;
#119453 = EDGE_CURVE ( 'NONE', #88893, #72605, #129609, .T. ) ;
#119455 = ORIENTED_EDGE ( 'NONE', *, *, #119656, .F. ) ;
#119454 = CARTESIAN_POINT ( 'NONE',  ( -23.15000000000000213, 64.25000000001249134, -176.8647081744214802 ) ) ;
#119456 = CARTESIAN_POINT ( 'NONE',  ( 21.14999999999999858, 69.35000000001228670, -157.7731074845243882 ) ) ;
#119457 = CARTESIAN_POINT ( 'NONE',  ( -21.29999999999995808, 76.00000000001264766, -199.4731074845243484 ) ) ;
#119458 = CARTESIAN_POINT ( 'NONE',  ( 22.47071067811865319, 76.00000000001165290, -69.52310748452431710 ) ) ;
#119459 = CIRCLE ( 'NONE', #7024, 11.75000000000001066 ) ;
#119461 = CARTESIAN_POINT ( 'NONE',  ( -22.50000000000000000, 75.90736249940297853, -181.6728046915650907 ) ) ;
#119460 = DIRECTION ( 'NONE',  ( -0.000000000000000000, -0.8814952561688430555, 0.4721928772777346239 ) ) ;
#119462 = CARTESIAN_POINT ( 'NONE',  ( -21.07954763557471267, 75.93412408139377590, -142.8523984745623636 ) ) ;
#119463 = CARTESIAN_POINT ( 'NONE',  ( -21.55000000000000071, 7.250000000011155521, -45.85000000000000142 ) ) ;
#119464 = AXIS2_PLACEMENT_3D ( 'NONE', #40364, #183694, #143266 ) ;
#119465 = AXIS2_PLACEMENT_3D ( 'NONE', #42596, #60865, #161278 ) ;
#119466 = CARTESIAN_POINT ( 'NONE',  ( 21.05000000000000071, 76.00000000001213607, -136.5231074845242745 ) ) ;
#119467 = CARTESIAN_POINT ( 'NONE',  ( 22.49999999999998579, -3.180729737797959977, -228.0957332317255180 ) ) ;
#119468 = ORIENTED_EDGE ( 'NONE', *, *, #257938, .T. ) ;
#119469 = AXIS2_PLACEMENT_3D ( 'NONE', #1946, #39837, #257508 ) ;
#119471 = ORIENTED_EDGE ( 'NONE', *, *, #158622, .F. ) ;
#119470 = CARTESIAN_POINT ( 'NONE',  ( 20.04142135623730070, 11.65000000001115943, -188.7499999999999716 ) ) ;
#119472 = ORIENTED_EDGE ( 'NONE', *, *, #237805, .T. ) ;
#119473 = CARTESIAN_POINT ( 'NONE',  ( -18.39418127959864790, 64.51609439831437953, -179.2731074845244450 ) ) ;
#119474 = ORIENTED_EDGE ( 'NONE', *, *, #203677, .F. ) ;
#119475 = DIRECTION ( 'NONE',  ( 1.000000000000000000, 0.000000000000000000, -0.000000000000000000 ) ) ;
#119476 =( BOUNDED_CURVE ( )  B_SPLINE_CURVE ( 3, ( #141568, #202826, #21636, #201538 ),
 .UNSPECIFIED., .F., .F. ) 
 B_SPLINE_CURVE_WITH_KNOTS ( ( 4, 4 ),
 ( 1.570796326794892339, 3.141592653589784678 ),
 .UNSPECIFIED. ) 
 CURVE ( )  GEOMETRIC_REPRESENTATION_ITEM ( )  RATIONAL_B_SPLINE_CURVE ( ( 1.000000000000000000, 0.8047378541243659367, 0.8047378541243659367, 1.000000000000000000 ) ) 
 REPRESENTATION_ITEM ( '' )  );
#119477 = ORIENTED_EDGE ( 'NONE', *, *, #250955, .T. ) ;
#119478 = DIRECTION ( 'NONE',  ( 0.000000000000000000, 0.9126074666063769270, 0.4088369013363282733 ) ) ;
#119481 = EDGE_LOOP ( 'NONE', ( #160831, #214514, #199651, #197734 ) ) ;
#119480 = ORIENTED_EDGE ( 'NONE', *, *, #1930, .T. ) ;
#119479 = CIRCLE ( 'NONE', #140291, 0.09999999999999939493 ) ;
#119482 = ORIENTED_EDGE ( 'NONE', *, *, #59382, .T. ) ;
#119483 = ORIENTED_EDGE ( 'NONE', *, *, #184261, .F. ) ;
#119484 = B_SPLINE_CURVE_WITH_KNOTS ( 'NONE', 3,
 ( #94965, #177107, #223883, #98779 ),
 .UNSPECIFIED., .F., .F.,
 ( 4, 4 ),
 ( 0.000000000000000000, 7.713889350928795333E-05 ),
 .UNSPECIFIED. ) ;
#119485 = CARTESIAN_POINT ( 'NONE',  ( 20.27550659511088682, 9.216043722520002035, -176.7499999999999716 ) ) ;
#119486 = DIRECTION ( 'NONE',  ( 1.000000000000000000, -0.000000000000000000, -0.000000000000000000 ) ) ;
#119487 = VERTEX_POINT ( 'NONE', #101526 ) ;
#119488 = DIRECTION ( 'NONE',  ( -0.000000000000000000, -0.000000000000000000, 1.000000000000000000 ) ) ;
#119489 = DIRECTION ( 'NONE',  ( 0.000000000000000000, 0.000000000000000000, -1.000000000000000000 ) ) ;
#119491 = ORIENTED_EDGE ( 'NONE', *, *, #44129, .F. ) ;
#119490 = DIRECTION ( 'NONE',  ( 1.000000000000000000, 0.000000000000000000, 0.000000000000000000 ) ) ;
#119492 = CARTESIAN_POINT ( 'NONE',  ( 20.04142135623731136, 11.75000000001116263, -125.1500000000000341 ) ) ;
#119493 = EDGE_LOOP ( 'NONE', ( #196375, #173370, #189717, #9590 ) ) ;
#119495 = LINE ( 'NONE', #141608, #224931 ) ;
#119494 = AXIS2_PLACEMENT_3D ( 'NONE', #216091, #136547, #115724 ) ;
#119497 = VERTEX_POINT ( 'NONE', #81963 ) ;
#119496 = DIRECTION ( 'NONE',  ( 0.000000000000000000, 0.000000000000000000, -1.000000000000000000 ) ) ;
#119498 = CARTESIAN_POINT ( 'NONE',  ( -18.50000000000000000, 77.38471025844603446, -241.6066692018393098 ) ) ;
#119500 = EDGE_CURVE ( 'NONE', #86355, #226147, #112855, .T. ) ;
#119499 = CARTESIAN_POINT ( 'NONE',  ( -12.30589683808041279, 26.71170214840295642, -233.6080780108829344 ) ) ;
#119501 = DIRECTION ( 'NONE',  ( 0.000000000000000000, 5.204170427930272346E-14, -1.000000000000000000 ) ) ;
#119502 = AXIS2_PLACEMENT_3D ( 'NONE', #9914, #129852, #222866 ) ;
#119503 = VERTEX_POINT ( 'NONE', #110543 ) ;
#119505 = LINE ( 'NONE', #19101, #79089 ) ;
#119504 = LINE ( 'NONE', #59478, #24023 ) ;
#119507 = EDGE_CURVE ( 'NONE', #114896, #4010, #154582, .T. ) ;
#119506 = CARTESIAN_POINT ( 'NONE',  ( -14.22969084473441193, 66.54399267394249762, -84.53447399037760590 ) ) ;
#119508 = B_SPLINE_CURVE_WITH_KNOTS ( 'NONE', 3,
 ( #150984, #255151, #212253, #101219, #77844, #98659, #256422, #180817, #141671, #2153, #37465, #235636, #42575, #240787 ),
 .UNSPECIFIED., .F., .F.,
 ( 4, 2, 2, 2, 2, 2, 4 ),
 ( 1.398578778534940505E-17, 0.0003823333598418207288, 0.0005735000397627034461, 0.0006690833797231245843, 0.0007168750497033337440, 0.0007407708846934382696, 0.0007646667196835427952 ),
 .UNSPECIFIED. ) ;
#119509 = CARTESIAN_POINT ( 'NONE',  ( 18.31325810956328937, 85.53638847601955320, -163.1546672782194491 ) ) ;
#119510 = CIRCLE ( 'NONE', #73729, 0.1000000000000028644 ) ;
#119511 = AXIS2_PLACEMENT_3D ( 'NONE', #195520, #239755, #215053 ) ;
#119512 = CARTESIAN_POINT ( 'NONE',  ( -20.85000000000000142, 69.38854649060172619, -247.7638912529787660 ) ) ;
#119513 = DIRECTION ( 'NONE',  ( -0.000000000000000000, 0.4721928772777346239, 0.8814952561688430555 ) ) ;
#119514 = EDGE_LOOP ( 'NONE', ( #74564, #174285, #75765, #244293 ) ) ;
#119515 = VERTEX_POINT ( 'NONE', #167994 ) ;
#119516 =( BOUNDED_SURFACE ( )  B_SPLINE_SURFACE ( 3, 2, ( 
 ( #254753, #76154, #175303 ),
 ( #119154, #77425, #137411 ),
 ( #39643, #154459, #20061 ),
 ( #59132, #235237, #98253 ),
 ( #257312, #194857, #56566 ),
 ( #233954, #139965, #219516 ),
 ( #218217, #215658, #78713 ),
 ( #99548, #179153, #74915 ),
 ( #239099, #55281, #216944 ),
 ( #462, #79986, #134826 ) ),
 .UNSPECIFIED., .F., .F., .F. ) 
 B_SPLINE_SURFACE_WITH_KNOTS ( ( 4, 2, 2, 2, 4 ),
 ( 3, 3 ),
 ( 0.002161241639767790771, 0.002579950749617455040, 0.002789305304542286958, 0.002893982582004702916, 0.002998659859467118875 ),
 ( 0.000000000000000000, 1.000000000000000000 ),
 .UNSPECIFIED. ) 
 GEOMETRIC_REPRESENTATION_ITEM ( )  RATIONAL_B_SPLINE_SURFACE ( (
 ( 1.000000000000000000, 0.7071067811864378827, 1.000000000000000000),
 ( 1.000000000000000000, 0.7632447400650679281, 1.000000000000000000),
 ( 1.000000000000000000, 0.8158073005128387845, 1.000000000000000000),
 ( 1.000000000000000000, 0.8906973462385610052, 1.000000000000000000),
 ( 1.000000000000000000, 0.9149408947793243874, 1.000000000000000000),
 ( 1.000000000000000000, 0.9493368785279177047, 1.000000000000000000),
 ( 1.000000000000000000, 0.9605194247156390031, 1.000000000000000000),
 ( 1.000000000000000000, 0.9803630264780962555, 1.000000000000000000),
 ( 1.000000000000000000, 0.9900844824271249900, 1.000000000000000000),
 ( 1.000000000000000000, 0.9894588281429297361, 1.000000000000000000) ) ) 
 REPRESENTATION_ITEM ( '' )  SURFACE ( )  );
#119517 = ORIENTED_EDGE ( 'NONE', *, *, #255425, .F. ) ;
#119518 = COLOUR_RGB ( '', 0.08235294, 0.09019608, 0.10196078) ;
#119519 = EDGE_CURVE ( 'NONE', #58899, #234175, #150285, .T. ) ;
#119520 = DIRECTION ( 'NONE',  ( -1.000000000000000000, 2.952720810173289112E-16, 2.061873921506763405E-30 ) ) ;
#119522 = EDGE_CURVE ( 'NONE', #19000, #126771, #221163, .T. ) ;
#119521 = CIRCLE ( 'NONE', #190845, 0.09999999999999240052 ) ;
#119523 = EDGE_LOOP ( 'NONE', ( #94953, #218738, #52408, #193160, #182290, #158458, #87588, #95332 ) ) ;
#119524 = DIRECTION ( 'NONE',  ( -1.000000000000000000, -7.304098846218135653E-16, -4.639676173203994055E-30 ) ) ;
#119525 = EDGE_LOOP ( 'NONE', ( #238636, #130027, #96056, #14954 ) ) ;
#119527 = DIRECTION ( 'NONE',  ( -0.000000000000000000, 0.4088369013363281623, -0.9126074666063771490 ) ) ;
#119526 = CIRCLE ( 'NONE', #57118, 0.09999999999999459321 ) ;
#119528 = DIRECTION ( 'NONE',  ( 0.000000000000000000, 0.000000000000000000, -1.000000000000000000 ) ) ;
#119529 = ORIENTED_EDGE ( 'NONE', *, *, #46488, .T. ) ;
#119530 = DIRECTION ( 'NONE',  ( 0.000000000000000000, 0.000000000000000000, -1.000000000000000000 ) ) ;
#119531 = CIRCLE ( 'NONE', #94562, 11.80000000000000426 ) ;
#119532 = EDGE_LOOP ( 'NONE', ( #218056, #198302, #87370, #188873, #184617 ) ) ;
#119533 = EDGE_CURVE ( 'NONE', #214079, #177816, #89686, .T. ) ;
#119534 = VERTEX_POINT ( 'NONE', #184951 ) ;
#119535 = EDGE_CURVE ( 'NONE', #34846, #168030, #254473, .T. ) ;
#119536 = ORIENTED_EDGE ( 'NONE', *, *, #17368, .F. ) ;
#119538 = CARTESIAN_POINT ( 'NONE',  ( -20.00857864376270001, 66.85000000001186038, -90.67310748452436542 ) ) ;
#119537 = AXIS2_PLACEMENT_3D ( 'NONE', #105705, #180154, #1490 ) ;
#119539 = CARTESIAN_POINT ( 'NONE',  ( 22.48508240969612615, 75.95372358549585101, -215.1731182160979188 ) ) ;
#119540 = CARTESIAN_POINT ( 'NONE',  ( 20.12500000000000355, 9.258049272928479567, -142.3633388371424644 ) ) ;
#119541 = DIRECTION ( 'NONE',  ( 0.000000000000000000, -0.9651348961777157509, 0.2617529984165031243 ) ) ;
#119542 = VECTOR ( 'NONE', #98143, 1000.000000000000000 ) ;
#119543 = CARTESIAN_POINT ( 'NONE',  ( 14.45963434102924339, 66.54845833862650295, -118.0692319856937900 ) ) ;
#119545 = CARTESIAN_POINT ( 'NONE',  ( -21.44999999999999929, 7.249999999999999112, -21.25000000000000000 ) ) ;
#119544 = CARTESIAN_POINT ( 'NONE',  ( -20.94999999999999929, 87.48912529308871910, -200.4231074845242802 ) ) ;
#119546 = CYLINDRICAL_SURFACE ( 'NONE', #49822, 11.74999999999999645 ) ;
#119548 = EDGE_LOOP ( 'NONE', ( #33454, #198641, #74609, #5053 ) ) ;
#119547 = CARTESIAN_POINT ( 'NONE',  ( -20.54999999999999716, -9.500000000000001776, -23.60603087734756045 ) ) ;
#119549 = CARTESIAN_POINT ( 'NONE',  ( -20.94999999999999929, 87.41227409416143246, -72.42310748452423752 ) ) ;
#119550 = ORIENTED_EDGE ( 'NONE', *, *, #22225, .T. ) ;
#119551 = CIRCLE ( 'NONE', #248710, 0.1999999999999987899 ) ;
#119552 = DIRECTION ( 'NONE',  ( -1.000000000000000000, -8.673617379884087537E-15, 0.000000000000000000 ) ) ;
#119553 = ORIENTED_EDGE ( 'NONE', *, *, #174641, .T. ) ;
#119554 = ORIENTED_EDGE ( 'NONE', *, *, #26423, .F. ) ;
#119555 = CYLINDRICAL_SURFACE ( 'NONE', #79699, 0.1000000000000124678 ) ;
#119556 = CARTESIAN_POINT ( 'NONE',  ( -18.59999999999999787, 1.637172712981537659, -145.5821533654720383 ) ) ;
#119557 = CARTESIAN_POINT ( 'NONE',  ( 20.94999999999999929, 65.17014820068582992, -222.4427298839669618 ) ) ;
#119558 = ORIENTED_EDGE ( 'NONE', *, *, #131163, .F. ) ;
#119559 = EDGE_CURVE ( 'NONE', #255460, #106654, #200337, .T. ) ;
#119560 = EDGE_CURVE ( 'NONE', #17786, #112587, #37867, .T. ) ;
#119561 = CIRCLE ( 'NONE', #236243, 0.09999999999999939493 ) ;
#119562 = CARTESIAN_POINT ( 'NONE',  ( -16.97683809663752186, 9.950000000011138823, -109.7500000000000426 ) ) ;
#119564 = ORIENTED_EDGE ( 'NONE', *, *, #4195, .F. ) ;
#119563 = CIRCLE ( 'NONE', #227866, 0.1000000000000028644 ) ;
#119565 = VERTEX_POINT ( 'NONE', #169283 ) ;
#119566 = CARTESIAN_POINT ( 'NONE',  ( -18.50000000000000711, 57.82359945636609666, -226.0354702357591350 ) ) ;
#119567 = ORIENTED_EDGE ( 'NONE', *, *, #142941, .T. ) ;
#119568 = DIRECTION ( 'NONE',  ( 1.000000000000000000, -0.000000000000000000, 0.000000000000000000 ) ) ;
#119569 = CARTESIAN_POINT ( 'NONE',  ( -20.94999999999999929, 74.16465844978765176, -124.9679561919613207 ) ) ;
#119570 = ORIENTED_EDGE ( 'NONE', *, *, #225399, .F. ) ;
#119571 = DIRECTION ( 'NONE',  ( 0.000000000000000000, 2.891205793294679805E-16, -1.000000000000000000 ) ) ;
#119572 = CARTESIAN_POINT ( 'NONE',  ( 20.94999999999999574, -11.64999999998883595, -70.00000000000004263 ) ) ;
#119574 = EDGE_CURVE ( 'NONE', #76926, #220426, #131646, .T. ) ;
#119573 = CARTESIAN_POINT ( 'NONE',  ( -23.25000000000000000, 1.115600667400684642E-11, -167.4999999999999716 ) ) ;
#119575 = ORIENTED_EDGE ( 'NONE', *, *, #51195, .F. ) ;
#119576 = EDGE_CURVE ( 'NONE', #129130, #219834, #67065, .T. ) ;
#119577 = DIRECTION ( 'NONE',  ( 1.000000000000000000, 0.000000000000000000, 0.000000000000000000 ) ) ;
#119578 = FACE_OUTER_BOUND ( 'NONE', #79425, .T. ) ;
#119579 = AXIS2_PLACEMENT_3D ( 'NONE', #252222, #73632, #108871 ) ;
#119580 = ADVANCED_FACE ( 'NONE', ( #46711 ), #162948, .T. ) ;
#119581 = DIRECTION ( 'NONE',  ( -1.000000000000000000, 0.000000000000000000, 0.000000000000000000 ) ) ;
#119582 = ORIENTED_EDGE ( 'NONE', *, *, #208543, .T. ) ;
#119583 = AXIS2_PLACEMENT_3D ( 'NONE', #106587, #47908, #25791 ) ;
#119585 = ORIENTED_EDGE ( 'NONE', *, *, #67944, .F. ) ;
#119584 = FACE_OUTER_BOUND ( 'NONE', #185231, .T. ) ;
#119586 = ORIENTED_EDGE ( 'NONE', *, *, #178943, .F. ) ;
#119587 = CARTESIAN_POINT ( 'NONE',  ( 20.46382478191414833, 18.86502014180634745, -229.9214093956406373 ) ) ;
#119588 = EDGE_CURVE ( 'NONE', #63488, #151938, #87876, .T. ) ;
#119589 = CARTESIAN_POINT ( 'NONE',  ( -23.25000000000000000, -8.999999999988846255, -143.8939691226524644 ) ) ;
#119590 = AXIS2_PLACEMENT_3D ( 'NONE', #130945, #166251, #10994 ) ;
#119591 = CARTESIAN_POINT ( 'NONE',  ( 22.50000000000000000, 68.20922040163900135, -170.1231074845244109 ) ) ;
#119592 = DIRECTION ( 'NONE',  ( 0.000000000000000000, -0.000000000000000000, 1.000000000000000000 ) ) ;
#119594 = VERTEX_POINT ( 'NONE', #88392 ) ;
#119593 = AXIS2_PLACEMENT_3D ( 'NONE', #147659, #130653, #185502 ) ;
#119595 = DIRECTION ( 'NONE',  ( 0.000000000000000000, 1.000000000000000000, 0.000000000000000000 ) ) ;
#119596 = ADVANCED_FACE ( 'NONE', ( #27200 ), #190095, .F. ) ;
#119597 = FACE_OUTER_BOUND ( 'NONE', #175672, .T. ) ;
#119598 = VECTOR ( 'NONE', #90012, 1000.000000000000000 ) ;
#119599 = VECTOR ( 'NONE', #214765, 1000.000000000000114 ) ;
#119600 = CARTESIAN_POINT ( 'NONE',  ( -18.52309608778534056, 77.30126544915781039, -241.9097476308881483 ) ) ;
#119601 = LINE ( 'NONE', #99979, #142333 ) ;
#119602 = DIRECTION ( 'NONE',  ( -1.000000000000000000, 0.000000000000000000, 0.000000000000000000 ) ) ;
#119603 = CIRCLE ( 'NONE', #7134, 0.5000000000000004441 ) ;
#119604 = ORIENTED_EDGE ( 'NONE', *, *, #76734, .T. ) ;
#119605 = ORIENTED_EDGE ( 'NONE', *, *, #1010, .F. ) ;
#119606 = CARTESIAN_POINT ( 'NONE',  ( -5.900000000000002132, -11.25000000000000000, 14.00000000000000178 ) ) ;
#119607 = CARTESIAN_POINT ( 'NONE',  ( -21.05000000000000071, 1.115600667400684642E-11, -163.5000000000000284 ) ) ;
#119608 = CARTESIAN_POINT ( 'NONE',  ( 21.11701782572533048, 10.72160911601861244, -179.7450374295111715 ) ) ;
#119609 = CARTESIAN_POINT ( 'NONE',  ( -23.25000000000000000, 76.00000000001142553, -36.02310748452432421 ) ) ;
#119610 = ORIENTED_EDGE ( 'NONE', *, *, #210391, .F. ) ;
#119611 = CYLINDRICAL_SURFACE ( 'NONE', #168059, 0.5000000000000022204 ) ;
#119612 = CIRCLE ( 'NONE', #152953, 0.09999999999999939493 ) ;
#119613 = FACE_OUTER_BOUND ( 'NONE', #61558, .T. ) ;
#119614 = AXIS2_PLACEMENT_3D ( 'NONE', #103867, #46468, #221254 ) ;
#119615 = CARTESIAN_POINT ( 'NONE',  ( 20.85000000000000142, -4.969162394454520459, -233.3995358778103935 ) ) ;
#119616 = DIRECTION ( 'NONE',  ( 1.000000000000000000, -1.207181226542539700E-16, 2.694675058168174199E-16 ) ) ;
#119617 = ORIENTED_EDGE ( 'NONE', *, *, #77922, .F. ) ;
#119618 = CARTESIAN_POINT ( 'NONE',  ( -21.05439746398122836, 12.96833403348994196, -205.3294046817250660 ) ) ;
#119619 = ORIENTED_EDGE ( 'NONE', *, *, #188597, .T. ) ;
#119620 = CARTESIAN_POINT ( 'NONE',  ( -23.39999999999994529, 82.84256550613280012, -26.34830530078816935 ) ) ;
#119621 = DIRECTION ( 'NONE',  ( 0.000000000000000000, 0.9274965247785529332, 0.3738317757009255171 ) ) ;
#119622 = CARTESIAN_POINT ( 'NONE',  ( 21.05000000000000071, 9.863005973831429074, -220.4411654715779321 ) ) ;
#119623 = CARTESIAN_POINT ( 'NONE',  ( 18.53317502108576420, 65.67736539654922012, -63.96251168765718376 ) ) ;
#119624 = CARTESIAN_POINT ( 'NONE',  ( -20.64999999999999858, 7.250000000011155521, -121.7500000000000426 ) ) ;
#119625 = CARTESIAN_POINT ( 'NONE',  ( -22.39999999999999858, 0.1000000000111554016, -100.5000000000000284 ) ) ;
#119626 = DIRECTION ( 'NONE',  ( 0.000000000000000000, 0.000000000000000000, 1.000000000000000000 ) ) ;
#119627 = CARTESIAN_POINT ( 'NONE',  ( -18.58735405345342784, -9.566478620325442606, -107.3227146462660357 ) ) ;
#119628 = CARTESIAN_POINT ( 'NONE',  ( -18.50000000000000000, 11.72137559264762174, -210.8820217676538391 ) ) ;
#119629 = DIRECTION ( 'NONE',  ( 1.000000000000000000, 0.000000000000000000, 0.000000000000000000 ) ) ;
#119630 = EDGE_CURVE ( 'NONE', #103469, #238394, #128842, .T. ) ;
#119631 = CARTESIAN_POINT ( 'NONE',  ( 22.50000000000000000, 0.000000000000000000, 0.000000000000000000 ) ) ;
#119632 = CARTESIAN_POINT ( 'NONE',  ( -23.25000000000000355, 51.48671849539696410, -231.8960919591225718 ) ) ;
#119633 = VECTOR ( 'NONE', #212587, 1000.000000000000000 ) ;
#119634 = AXIS2_PLACEMENT_3D ( 'NONE', #152285, #111858, #229243 ) ;
#119635 = TOROIDAL_SURFACE ( 'NONE', #236143, 12.77499999999999858, 0.1000000000000000056 ) ;
#119636 = CIRCLE ( 'NONE', #248819, 4.150000000000001243 ) ;
#119637 = DIRECTION ( 'NONE',  ( -3.265361837132813093E-16, 0.9770955615653316162, 0.2128009952263604232 ) ) ;
#119638 = CARTESIAN_POINT ( 'NONE',  ( 18.59999999999999787, 85.40000000001239755, -163.1410656363516125 ) ) ;
#119639 = ORIENTED_EDGE ( 'NONE', *, *, #112968, .F. ) ;
#119640 = CARTESIAN_POINT ( 'NONE',  ( 21.05000000000000071, 6.477552182493491628, -0.09999996530010009377 ) ) ;
#119641 = CARTESIAN_POINT ( 'NONE',  ( 20.85000000000000142, 77.83585931145498193, -24.51866831572578320 ) ) ;
#119643 = EDGE_CURVE ( 'NONE', #14385, #20995, #50547, .T. ) ;
#119642 = CARTESIAN_POINT ( 'NONE',  ( 20.44999100639894962, 10.43971070322319683, -41.25907572597052564 ) ) ;
#119644 = ORIENTED_EDGE ( 'NONE', *, *, #29137, .F. ) ;
#119645 = CARTESIAN_POINT ( 'NONE',  ( -18.50000000000000000, 7.021664781900089913, -37.13356540189729316 ) ) ;
#119646 = ADVANCED_FACE ( 'NONE', ( #11466 ), #67571, .F. ) ;
#119647 = EDGE_CURVE ( 'NONE', #211829, #33150, #25388, .T. ) ;
#119648 = ORIENTED_EDGE ( 'NONE', *, *, #81712, .F. ) ;
#119649 = CARTESIAN_POINT ( 'NONE',  ( 21.05000000000000071, 13.60254931771583387, -238.7443143987590304 ) ) ;
#119650 = DIRECTION ( 'NONE',  ( 0.000000000000000000, 0.000000000000000000, 1.000000000000000000 ) ) ;
#119651 = TOROIDAL_SURFACE ( 'NONE', #231906, 0.2000000000000000111, 0.1000000000000000056 ) ;
#119652 = ORIENTED_EDGE ( 'NONE', *, *, #61934, .T. ) ;
#119653 = AXIS2_PLACEMENT_3D ( 'NONE', #190460, #250400, #211285 ) ;
#119654 = ORIENTED_EDGE ( 'NONE', *, *, #201915, .F. ) ;
#119655 = CARTESIAN_POINT ( 'NONE',  ( 23.14999999999999503, 11.65000000001116298, -45.65000000000000568 ) ) ;
#119656 = EDGE_CURVE ( 'NONE', #22594, #60251, #76547, .T. ) ;
#119657 = ORIENTED_EDGE ( 'NONE', *, *, #21652, .F. ) ;
#119658 = EDGE_CURVE ( 'NONE', #200601, #175862, #12929, .T. ) ;
#119659 = DIRECTION ( 'NONE',  ( 0.000000000000000000, 0.8814952561688429444, -0.4721928772777349015 ) ) ;
#119660 = CARTESIAN_POINT ( 'NONE',  ( -23.15000000000000213, 71.65000000001228386, -157.8731074845243825 ) ) ;
#119661 = CARTESIAN_POINT ( 'NONE',  ( 18.59999999999998366, 76.00000000001142553, -36.02310748452432421 ) ) ;
#119662 = CARTESIAN_POINT ( 'NONE',  ( -18.59999999999999787, -1.835859311432484375, -112.0044391687985694 ) ) ;
#119663 = FACE_OUTER_BOUND ( 'NONE', #29164, .T. ) ;
#119664 = DIRECTION ( 'NONE',  ( 0.000000000000000000, -0.9910465087640860649, -0.1335171055202901413 ) ) ;
#119665 = CARTESIAN_POINT ( 'NONE',  ( 20.94999999999999929, -12.41227409413852811, -131.0000000000000284 ) ) ;
#119666 = CARTESIAN_POINT ( 'NONE',  ( 20.94999999999999929, 85.40000000001188596, -93.12913836187179584 ) ) ;
#119668 = ORIENTED_EDGE ( 'NONE', *, *, #215531, .F. ) ;
#119667 = CARTESIAN_POINT ( 'NONE',  ( -18.49346865148322294, -9.443073798513754724, -40.68519625531506989 ) ) ;
#119669 = ORIENTED_EDGE ( 'NONE', *, *, #98431, .F. ) ;
#119671 = DIRECTION ( 'NONE',  ( -1.000000000000000000, -0.000000000000000000, -0.000000000000000000 ) ) ;
#119670 = CARTESIAN_POINT ( 'NONE',  ( -0.8999999999999438449, 67.75000000001118394, -14.06452884076210275 ) ) ;
#119674 = EDGE_LOOP ( 'NONE', ( #183831, #237960, #16485, #220451 ) ) ;
#119673 = DIRECTION ( 'NONE',  ( 0.000000000000000000, 0.000000000000000000, 1.000000000000000000 ) ) ;
#119672 = CARTESIAN_POINT ( 'NONE',  ( -20.94999999999994600, 61.64150943397345372, -36.51839050339276582 ) ) ;
#119675 = VECTOR ( 'NONE', #137420, 1000.000000000000000 ) ;
#119676 = ORIENTED_EDGE ( 'NONE', *, *, #2245, .T. ) ;
#119677 = DIRECTION ( 'NONE',  ( -1.000000000000000000, 2.952720810173289112E-16, 2.061873921506763405E-30 ) ) ;
#119678 = CARTESIAN_POINT ( 'NONE',  ( 21.05000000000000071, 76.10000000001218723, -143.0637644362255401 ) ) ;
#119679 = ADVANCED_FACE ( 'NONE', ( #171848 ), #36166, .T. ) ;
#119680 = FACE_OUTER_BOUND ( 'NONE', #170029, .T. ) ;
#119681 = FACE_OUTER_BOUND ( 'NONE', #73308, .T. ) ;
#119683 = DIRECTION ( 'NONE',  ( -2.952720810173289112E-16, -1.000000000000000000, -6.982962677686266711E-15 ) ) ;
#119682 = CIRCLE ( 'NONE', #169613, 0.1000000000000028644 ) ;
#119684 = CARTESIAN_POINT ( 'NONE',  ( -20.64999999999999858, 85.00000000001179501, -79.41707660717668205 ) ) ;
#119685 = EDGE_CURVE ( 'NONE', #114887, #18598, #229572, .T. ) ;
#119687 = AXIS2_PLACEMENT_3D ( 'NONE', #172596, #52584, #95568 ) ;
#119686 = FACE_OUTER_BOUND ( 'NONE', #105207, .T. ) ;
#119688 = ORIENTED_EDGE ( 'NONE', *, *, #204859, .T. ) ;
#119689 = VERTEX_POINT ( 'NONE', #71445 ) ;
#119690 = CARTESIAN_POINT ( 'NONE',  ( 17.74533788810830259, 59.48958453972256422, -223.0693145980908980 ) ) ;
#119691 = VECTOR ( 'NONE', #32148, 1000.000000000000227 ) ;
#119692 = AXIS2_PLACEMENT_3D ( 'NONE', #31009, #169236, #191360 ) ;
#119693 = ORIENTED_EDGE ( 'NONE', *, *, #31781, .T. ) ;
#119694 = DIRECTION ( 'NONE',  ( -0.000000000000000000, 0.000000000000000000, 1.000000000000000000 ) ) ;
#119695 = EDGE_LOOP ( 'NONE', ( #102592, #50491, #25131, #18274 ) ) ;
#119696 = CARTESIAN_POINT ( 'NONE',  ( -13.40000000000000213, -12.25000000000000178, 15.00000000000000355 ) ) ;
#119697 = PRODUCT_DEFINITION_FORMATION_WITH_SPECIFIED_SOURCE ( 'ANY', '', #30667, .NOT_KNOWN. ) ;
#119698 = CIRCLE ( 'NONE', #107202, 0.09999999999999939493 ) ;
#119699 = CARTESIAN_POINT ( 'NONE',  ( -15.39126916658604216, 49.08063300121916939, -233.6976605013540222 ) ) ;
#119700 = CARTESIAN_POINT ( 'NONE',  ( 23.24999999999999289, 28.91254064196106910, -237.8576372133405528 ) ) ;
#119701 = CIRCLE ( 'NONE', #90632, 11.70000000000001172 ) ;
#119702 = DIRECTION ( 'NONE',  ( -0.000000000000000000, -0.000000000000000000, 1.000000000000000000 ) ) ;
#119703 = CARTESIAN_POINT ( 'NONE',  ( 21.05000000000000071, -11.74999999998883560, -164.6000000000000227 ) ) ;
#119704 = ORIENTED_EDGE ( 'NONE', *, *, #142174, .F. ) ;
#119705 = CARTESIAN_POINT ( 'NONE',  ( -20.54999999999999716, 74.05981308412420105, -123.6939882734709926 ) ) ;
#119706 = EDGE_CURVE ( 'NONE', #137538, #26118, #242021, .T. ) ;
#119707 = DIRECTION ( 'NONE',  ( 0.000000000000000000, -1.000000000000000000, 0.000000000000000000 ) ) ;
#119708 = DIRECTION ( 'NONE',  ( 0.000000000000000000, -0.2128009952263900384, 0.9770955615653251769 ) ) ;
#119709 = CARTESIAN_POINT ( 'NONE',  ( -21.14999999999999858, 55.98745301258801987, -232.8057040749261262 ) ) ;
#119710 = ORIENTED_EDGE ( 'NONE', *, *, #109894, .T. ) ;
#119711 = AXIS2_PLACEMENT_3D ( 'NONE', #59918, #40419, #179908 ) ;
#119712 = ORIENTED_EDGE ( 'NONE', *, *, #68307, .F. ) ;
#119715 = EDGE_LOOP ( 'NONE', ( #102985, #161403, #5856, #150246, #174690 ) ) ;
#119714 = DIRECTION ( 'NONE',  ( -1.000000000000000000, 0.000000000000000000, 0.000000000000000000 ) ) ;
#119713 = CARTESIAN_POINT ( 'NONE',  ( -22.50000000000000000, 64.35012909624849442, -203.6056273753975461 ) ) ;
#119716 = DIRECTION ( 'NONE',  ( 0.000000000000000000, 0.9910465087640860649, 0.1335171055202901413 ) ) ;
#119717 = VECTOR ( 'NONE', #60708, 1000.000000000000000 ) ;
#119718 = ADVANCED_FACE ( 'NONE', ( #255136 ), #150965, .T. ) ;
#119719 = AXIS2_PLACEMENT_3D ( 'NONE', #190366, #13018, #10433 ) ;
#119720 = DIRECTION ( 'NONE',  ( 1.000000000000000000, -0.000000000000000000, 0.000000000000000000 ) ) ;
#119721 = EDGE_LOOP ( 'NONE', ( #219450, #113117, #220986, #131592 ) ) ;
#119723 = EDGE_CURVE ( 'NONE', #168580, #14237, #117138, .T. ) ;
#119722 = CARTESIAN_POINT ( 'NONE',  ( 18.49362639424882104, 85.44260436790048630, -129.7586665510135049 ) ) ;
#119724 = CIRCLE ( 'NONE', #7265, 0.09999999999998712696 ) ;
#119725 = DIRECTION ( 'NONE',  ( 0.000000000000000000, -0.2617529984165031243, -0.9651348961777157509 ) ) ;
#119726 = VECTOR ( 'NONE', #166567, 1000.000000000000000 ) ;
#119727 = ADVANCED_FACE ( 'NONE', ( #114402 ), #246131, .T. ) ;
#119728 = CARTESIAN_POINT ( 'NONE',  ( 20.94999999999999574, 74.16465844978787914, -158.4679561919613775 ) ) ;
#119729 = EDGE_CURVE ( 'NONE', #201752, #82580, #79515, .T. ) ;
#119731 = ORIENTED_EDGE ( 'NONE', *, *, #106735, .F. ) ;
#119730 = CARTESIAN_POINT ( 'NONE',  ( -22.10000000000000142, -11.65000000000000036, 33.00000000000000000 ) ) ;
#119732 = CARTESIAN_POINT ( 'NONE',  ( -18.50000000000000000, 77.73625713161000306, -191.9544551555068495 ) ) ;
#119734 = EDGE_LOOP ( 'NONE', ( #108630, #173999, #73142, #53694, #140259 ) ) ;
#119733 = EDGE_CURVE ( 'NONE', #150376, #105026, #133697, .T. ) ;
#119735 = LINE ( 'NONE', #195431, #186949 ) ;
#119736 = CARTESIAN_POINT ( 'NONE',  ( -16.94165728009537375, 9.987869755934932314, -188.3910550085101363 ) ) ;
#119737 = DIRECTION ( 'NONE',  ( -0.000000000000000000, -0.1298341882520022694, -0.9915357197604853789 ) ) ;
#119738 = ADVANCED_FACE ( 'NONE', ( #173145 ), #108754, .T. ) ;
#119739 = TOROIDAL_SURFACE ( 'NONE', #115615, 0.2000000000000000111, 0.1000000000000000056 ) ;
#119740 = EDGE_LOOP ( 'NONE', ( #130887, #159898, #161138, #11267 ) ) ;
#119741 = LINE ( 'NONE', #237108, #250947 ) ;
#119745 = EDGE_CURVE ( 'NONE', #3082, #243260, #193951, .T. ) ;
#119744 = ADVANCED_FACE ( 'NONE', ( #195251 ), #153580, .T. ) ;
#119743 = EDGE_LOOP ( 'NONE', ( #10996, #228486, #187069, #94102 ) ) ;
#119742 = TOROIDAL_SURFACE ( 'NONE', #32259, 0.2000000000000000111, 0.1000000000000000056 ) ;
#119747 = VECTOR ( 'NONE', #117949, 1000.000000000000000 ) ;
#119746 = CARTESIAN_POINT ( 'NONE',  ( 20.94999999999999574, 1.162701749938009677, -7.900000000000000355 ) ) ;
#119748 = CARTESIAN_POINT ( 'NONE',  ( 18.59999999999999787, -1.263275465206102233, -208.9018646667463770 ) ) ;
#119749 = DIRECTION ( 'NONE',  ( 0.000000000000000000, 0.9908441862701782288, -0.1350103645450542456 ) ) ;
#119750 = VERTEX_POINT ( 'NONE', #230505 ) ;
#119751 = DIRECTION ( 'NONE',  ( 1.000000000000000000, -0.000000000000000000, -0.000000000000000000 ) ) ;
#119752 = LINE ( 'NONE', #137990, #138853 ) ;
#119753 = CIRCLE ( 'NONE', #178204, 0.09999999999998898659 ) ;
#119754 = EDGE_CURVE ( 'NONE', #145079, #98576, #37615, .T. ) ;
#119755 = CARTESIAN_POINT ( 'NONE',  ( -20.99142135623731065, 11.60000000001115161, -93.57179676972452853 ) ) ;
#119756 = CIRCLE ( 'NONE', #61487, 0.1000000000000028644 ) ;
#119757 = ORIENTED_EDGE ( 'NONE', *, *, #25219, .F. ) ;
#119758 = CARTESIAN_POINT ( 'NONE',  ( -23.24999999999999645, -9.599999999988845900, -207.7001893912220112 ) ) ;
#119759 = CIRCLE ( 'NONE', #73987, 0.1999999999999987899 ) ;
#119761 = ORIENTED_EDGE ( 'NONE', *, *, #200865, .F. ) ;
#119760 = EDGE_CURVE ( 'NONE', #46074, #198700, #204414, .T. ) ;
#119763 = EDGE_CURVE ( 'NONE', #23903, #191649, #62136, .T. ) ;
#119762 = CARTESIAN_POINT ( 'NONE',  ( 21.04999999999999716, 69.69554417806399726, -69.50207200798423912 ) ) ;
#119764 = ORIENTED_EDGE ( 'NONE', *, *, #15494, .F. ) ;
#119765 = AXIS2_PLACEMENT_3D ( 'NONE', #256027, #197386, #18754 ) ;
#119766 = EDGE_CURVE ( 'NONE', #80961, #134698, #202919, .T. ) ;
#119767 = DIRECTION ( 'NONE',  ( 2.952720810173289112E-16, 1.000000000000000000, 6.982962677686266711E-15 ) ) ;
#119768 = ORIENTED_EDGE ( 'NONE', *, *, #138212, .T. ) ;
#119770 = VERTEX_POINT ( 'NONE', #219916 ) ;
#119769 = DIRECTION ( 'NONE',  ( -6.938893903907222067E-15, -0.9651348961777157509, 0.2617529984165031243 ) ) ;
#119771 = EDGE_CURVE ( 'NONE', #12116, #137789, #77826, .T. ) ;
#119772 = CIRCLE ( 'NONE', #65580, 0.09999999999999939493 ) ;
#119773 = AXIS2_PLACEMENT_3D ( 'NONE', #174342, #152189, #110458 ) ;
#119776 = ORIENTED_EDGE ( 'NONE', *, *, #11284, .T. ) ;
#119775 = ORIENTED_EDGE ( 'NONE', *, *, #221841, .T. ) ;
#119774 = CYLINDRICAL_SURFACE ( 'NONE', #238615, 0.1000000000000054040 ) ;
#119777 = CARTESIAN_POINT ( 'NONE',  ( 20.94999999999999574, 8.494751065780215882, -209.2245083539370114 ) ) ;
#119778 = AXIS2_PLACEMENT_3D ( 'NONE', #16918, #56000, #155169 ) ;
#119779 = CARTESIAN_POINT ( 'NONE',  ( -21.10320863425827298, 0.02502225123826237740, -161.0997226135407345 ) ) ;
#119780 = AXIS2_PLACEMENT_3D ( 'NONE', #187219, #225014, #67246 ) ;
#119781 = CARTESIAN_POINT ( 'NONE',  ( 21.13736287352038445, 67.95335762362786625, -90.37310748452435405 ) ) ;
#119782 = AXIS2_PLACEMENT_3D ( 'NONE', #107480, #44946, #184444 ) ;
#119783 = CARTESIAN_POINT ( 'NONE',  ( 20.04142135623730070, 64.35000000001222986, -148.6731074845244507 ) ) ;
#119784 = CARTESIAN_POINT ( 'NONE',  ( -22.39999999999999858, -1.657885652111596109, -193.3876638332971254 ) ) ;
#119785 = CARTESIAN_POINT ( 'NONE',  ( -0.8999999999999437339, 67.72071067812984779, -10.02310748452479139 ) ) ;
#119786 = CARTESIAN_POINT ( 'NONE',  ( 22.39999999999999503, 76.00000000001200817, -110.8138870828976934 ) ) ;
#119788 = CARTESIAN_POINT ( 'NONE',  ( 20.27550659511088682, 66.78395627750346364, -160.7731074845244166 ) ) ;
#119787 = DIRECTION ( 'NONE',  ( -1.000000000000000000, -1.836970198721029934E-16, 0.000000000000000000 ) ) ;
#119789 = ORIENTED_EDGE ( 'NONE', *, *, #184155, .F. ) ;
#119790 = ORIENTED_EDGE ( 'NONE', *, *, #122973, .F. ) ;
#119791 = DIRECTION ( 'NONE',  ( 0.000000000000000000, 0.000000000000000000, -1.000000000000000000 ) ) ;
#119793 = ORIENTED_EDGE ( 'NONE', *, *, #80158, .T. ) ;
#119792 = DIRECTION ( 'NONE',  ( -1.000000000000000000, 0.000000000000000000, 0.000000000000000000 ) ) ;
#119794 = DIRECTION ( 'NONE',  ( 0.000000000000000000, -1.000000000000000000, 0.000000000000000000 ) ) ;
#119795 = ORIENTED_EDGE ( 'NONE', *, *, #211278, .F. ) ;
#119796 = LINE ( 'NONE', #96333, #251796 ) ;
#119797 = ORIENTED_EDGE ( 'NONE', *, *, #104125, .T. ) ;
#119798 = CARTESIAN_POINT ( 'NONE',  ( -18.50000000000000000, 7.661991824395936845, -241.5144583139544636 ) ) ;
#119799 = VECTOR ( 'NONE', #35934, 1000.000000000000000 ) ;
#119800 = ORIENTED_EDGE ( 'NONE', *, *, #244689, .F. ) ;
#119801 = CARTESIAN_POINT ( 'NONE',  ( 23.15000000000000213, 85.00000000001207923, -126.6291383618717816 ) ) ;
#119802 = DIRECTION ( 'NONE',  ( 0.000000000000000000, 0.000000000000000000, 1.000000000000000000 ) ) ;
#119803 = AXIS2_PLACEMENT_3D ( 'NONE', #253056, #154020, #92697 ) ;
#119805 = ORIENTED_EDGE ( 'NONE', *, *, #180218, .T. ) ;
#119804 = VERTEX_POINT ( 'NONE', #217328 ) ;
#119806 = EDGE_LOOP ( 'NONE', ( #160068, #48530, #141479, #241367 ) ) ;
#119807 = DIRECTION ( 'NONE',  ( 0.000000000000000000, 0.000000000000000000, 1.000000000000000000 ) ) ;
#119808 = ORIENTED_EDGE ( 'NONE', *, *, #98520, .T. ) ;
#119809 = ORIENTED_EDGE ( 'NONE', *, *, #217999, .T. ) ;
#119810 = DIRECTION ( 'NONE',  ( 0.000000000000000000, 0.6728971962617102953, -0.7397360091702507301 ) ) ;
#119812 = ORIENTED_EDGE ( 'NONE', *, *, #91580, .F. ) ;
#119811 = CARTESIAN_POINT ( 'NONE',  ( 18.54999999999999716, 67.25000000001205080, -127.2731074845243597 ) ) ;
#119814 = LINE ( 'NONE', #167599, #223509 ) ;
#119813 = DIRECTION ( 'NONE',  ( -1.000000000000000000, -0.000000000000000000, -0.000000000000000000 ) ) ;
#119815 = CARTESIAN_POINT ( 'NONE',  ( 15.74999999999999645, 9.350000000011139178, -50.25000000000000000 ) ) ;
#119816 = LINE ( 'NONE', #199345, #256917 ) ;
#119817 = CARTESIAN_POINT ( 'NONE',  ( -16.91256925476571027, 9.985731158139333985, -180.0323575109946717 ) ) ;
#119818 = ORIENTED_EDGE ( 'NONE', *, *, #199284, .T. ) ;
#119819 = ORIENTED_EDGE ( 'NONE', *, *, #131741, .T. ) ;
#119820 = DIRECTION ( 'NONE',  ( 1.000000000000000000, -0.000000000000000000, -0.000000000000000000 ) ) ;
#119821 = CARTESIAN_POINT ( 'NONE',  ( -18.59999999999999787, 1.835341550235567887, -112.0551512925630249 ) ) ;
#119823 = EDGE_CURVE ( 'NONE', #5450, #27558, #125331, .T. ) ;
#119822 = FACE_BOUND ( 'NONE', #117157, .T. ) ;
#119824 = VERTEX_POINT ( 'NONE', #23030 ) ;
#119825 = CIRCLE ( 'NONE', #74049, 0.3999999999999926392 ) ;
#119826 = AXIS2_PLACEMENT_3D ( 'NONE', #32026, #72431, #108955 ) ;
#119827 = DIRECTION ( 'NONE',  ( 1.652117596168391700E-15, 1.000000000000000000, -0.000000000000000000 ) ) ;
#119828 = EDGE_CURVE ( 'NONE', #118818, #253025, #63133, .T. ) ;
#119829 = VECTOR ( 'NONE', #133981, 1000.000000000000000 ) ;
#119830 = DIRECTION ( 'NONE',  ( 1.000000000000000000, 0.000000000000000000, 0.000000000000000000 ) ) ;
#119831 = CARTESIAN_POINT ( 'NONE',  ( -15.70407651835961360, 12.60827992760467531, -214.9270390227368352 ) ) ;
#119832 = ORIENTED_EDGE ( 'NONE', *, *, #128845, .F. ) ;
#119833 = ORIENTED_EDGE ( 'NONE', *, *, #17010, .T. ) ;
#119834 = ADVANCED_FACE ( 'NONE', ( #58262 ), #108924, .T. ) ;
#119835 = CARTESIAN_POINT ( 'NONE',  ( -18.79999999999999716, 4.513204987021263825, 22.10000000000000142 ) ) ;
#119837 = EDGE_CURVE ( 'NONE', #72929, #222045, #100530, .T. ) ;
#119836 = CARTESIAN_POINT ( 'NONE',  ( -0.8999999999999435119, 66.35000000001119247, -12.62310748452479281 ) ) ;
#119838 = ORIENTED_EDGE ( 'NONE', *, *, #5805, .T. ) ;
#119839 = CARTESIAN_POINT ( 'NONE',  ( -23.15000000000000213, 85.00000000001232081, -160.1291383618718385 ) ) ;
#119840 = ORIENTED_EDGE ( 'NONE', *, *, #257625, .F. ) ;
#119841 = CARTESIAN_POINT ( 'NONE',  ( -20.12071067811865888, 66.67928932189292368, -57.17310748452438673 ) ) ;
#119842 = CYLINDRICAL_SURFACE ( 'NONE', #174756, 0.5000000000000004441 ) ;
#119844 = CARTESIAN_POINT ( 'NONE',  ( -22.49544290803695290, 55.87396915977456047, -232.8425975917331243 ) ) ;
#119843 = CARTESIAN_POINT ( 'NONE',  ( -16.97683809663752186, 9.950000000011138823, -120.5976359818037196 ) ) ;
#119845 = CARTESIAN_POINT ( 'NONE',  ( -23.25000000000000000, 69.06610602788578035, -132.7374616501508342 ) ) ;
#119846 = CARTESIAN_POINT ( 'NONE',  ( -16.89060415895971090, 66.04877923720965782, -90.37718726025393323 ) ) ;
#119847 = CIRCLE ( 'NONE', #228158, 11.65000000000000036 ) ;
#119848 = VERTEX_POINT ( 'NONE', #98644 ) ;
#119849 = AXIS2_PLACEMENT_3D ( 'NONE', #192752, #153674, #248866 ) ;
#119850 = FACE_OUTER_BOUND ( 'NONE', #12969, .T. ) ;
#119851 =( BOUNDED_CURVE ( )  B_SPLINE_CURVE ( 3, ( #24916, #180127, #1466, #21073 ),
 .UNSPECIFIED., .F., .T. ) 
 B_SPLINE_CURVE_WITH_KNOTS ( ( 4, 4 ),
 ( 4.712388980384689674, 5.672655318024644622 ),
 .UNSPECIFIED. ) 
 CURVE ( )  GEOMETRIC_REPRESENTATION_ITEM ( )  RATIONAL_B_SPLINE_CURVE ( ( 1.000000000000000000, 0.9246222802177426203, 0.9246222802177426203, 1.000000000000000000 ) ) 
 REPRESENTATION_ITEM ( '' )  );
#119852 = ADVANCED_FACE ( 'NONE', ( #24308 ), #150632, .T. ) ;
#119854 = ORIENTED_EDGE ( 'NONE', *, *, #48330, .F. ) ;
#119853 = EDGE_LOOP ( 'NONE', ( #19910, #228188, #190370, #38361 ) ) ;
#119855 = AXIS2_PLACEMENT_3D ( 'NONE', #117231, #40294, #140630 ) ;
#119856 = ORIENTED_EDGE ( 'NONE', *, *, #240845, .T. ) ;
#119857 = ADVANCED_FACE ( 'NONE', ( #158696 ), #222452, .F. ) ;
#119858 = CARTESIAN_POINT ( 'NONE',  ( -16.91247567987038281, 66.04091731634304097, -157.3943830259870822 ) ) ;
#119859 = CARTESIAN_POINT ( 'NONE',  ( -18.50000000000000000, 0.5876173420563349792, -209.1618981382189588 ) ) ;
#119860 = DIRECTION ( 'NONE',  ( 0.000000000000000000, 0.000000000000000000, 1.000000000000000000 ) ) ;
#119861 = CARTESIAN_POINT ( 'NONE',  ( -20.90000000000000213, 1.885425182446134107, -11.59641995933507808 ) ) ;
#119862 = DIRECTION ( 'NONE',  ( 0.000000000000000000, 0.8660254037844420383, -0.4999999999999941713 ) ) ;
#119864 = LINE ( 'NONE', #198086, #140885 ) ;
#119863 = FACE_OUTER_BOUND ( 'NONE', #82922, .T. ) ;
#119865 = ORIENTED_EDGE ( 'NONE', *, *, #182744, .T. ) ;
#119866 = CARTESIAN_POINT ( 'NONE',  ( 18.49999999999999645, 1.637172712981537659, -179.0821533654719815 ) ) ;
#119867 = EDGE_LOOP ( 'NONE', ( #146308, #71308, #166653, #1489 ) ) ;
#119868 = CARTESIAN_POINT ( 'NONE',  ( 22.60000000000000142, 1.115600667400684642E-11, -167.4999999999999716 ) ) ;
#119869 = ORIENTED_EDGE ( 'NONE', *, *, #22072, .F. ) ;
#119870 = ORIENTED_EDGE ( 'NONE', *, *, #195161, .F. ) ;
#119871 = DIRECTION ( 'NONE',  ( 0.000000000000000000, -0.4721928772777346239, -0.8814952561688430555 ) ) ;
#119872 = DIRECTION ( 'NONE',  ( 0.000000000000000000, 0.2128009952263485993, -0.9770955615653341697 ) ) ;
#119873 = DIRECTION ( 'NONE',  ( -0.000000000000000000, -0.2128009952263603677, 0.9770955615653313941 ) ) ;
#119874 = EDGE_CURVE ( 'NONE', #160781, #171007, #201633, .T. ) ;
#119875 = CARTESIAN_POINT ( 'NONE',  ( 14.45204356427542081, 9.450668889178686527, -82.05554649020737656 ) ) ;
#119876 = AXIS2_PLACEMENT_3D ( 'NONE', #254485, #238814, #237533 ) ;
#119877 = EDGE_CURVE ( 'NONE', #18582, #34631, #40033, .T. ) ;
#119878 = CIRCLE ( 'NONE', #228576, 0.1000000000000000472 ) ;
#119879 = FACE_OUTER_BOUND ( 'NONE', #66557, .T. ) ;
#119880 = ORIENTED_EDGE ( 'NONE', *, *, #178612, .T. ) ;
#119881 = VERTEX_POINT ( 'NONE', #162534 ) ;
#119882 = DIRECTION ( 'NONE',  ( 0.000000000000000000, 0.9908441862701596881, -0.1350103645451904977 ) ) ;
#119883 = EDGE_LOOP ( 'NONE', ( #139325, #18712, #236792, #187058 ) ) ;
#119884 = CARTESIAN_POINT ( 'NONE',  ( -17.11825945287481332, 63.05955705323258798, -213.2241350765465882 ) ) ;
#119885 = CARTESIAN_POINT ( 'NONE',  ( 20.85000000000000142, 76.00000000001190870, -103.0231074845243029 ) ) ;
#119886 = AXIS2_PLACEMENT_3D ( 'NONE', #201366, #38442, #240497 ) ;
#119887 = FACE_OUTER_BOUND ( 'NONE', #132522, .T. ) ;
#119888 = FACE_OUTER_BOUND ( 'NONE', #136933, .T. ) ;
#119890 = ADVANCED_FACE ( 'NONE', ( #99941 ), #119555, .T. ) ;
#119889 = CARTESIAN_POINT ( 'NONE',  ( 21.40925344232283223, 0.09895018863080314031, -60.34148114060958790 ) ) ;
#119891 = CARTESIAN_POINT ( 'NONE',  ( -21.05000000000000071, -0.09999999999999939493, 6.540656951701240729 ) ) ;
#119893 = DIRECTION ( 'NONE',  ( 1.000000000000000000, 0.000000000000000000, 0.000000000000000000 ) ) ;
#119892 = CARTESIAN_POINT ( 'NONE',  ( -16.94275863006528482, 30.26173435748351537, -234.7919186320798985 ) ) ;
#119894 = DIRECTION ( 'NONE',  ( 1.000000000000000000, -7.304098846218134667E-16, 0.000000000000000000 ) ) ;
#119895 = ADVANCED_FACE ( 'NONE', ( #2138 ), #179530, .T. ) ;
#119896 = CIRCLE ( 'NONE', #65683, 0.09999999999999520384 ) ;
#119897 = CARTESIAN_POINT ( 'NONE',  ( -21.05000000000000071, 6.165100388772664530, -199.6791937419174587 ) ) ;
#119898 = DIRECTION ( 'NONE',  ( 0.000000000000000000, 0.000000000000000000, 1.000000000000000000 ) ) ;
#119899 = EDGE_CURVE ( 'NONE', #215487, #90768, #80374, .T. ) ;
#119900 = CIRCLE ( 'NONE', #11551, 0.09999999999998797351 ) ;
#119901 = DIRECTION ( 'NONE',  ( 1.000000000000000000, 0.000000000000000000, 0.000000000000000000 ) ) ;
#119902 = AXIS2_PLACEMENT_3D ( 'NONE', #144165, #165034, #127199 ) ;
#119903 = AXIS2_PLACEMENT_3D ( 'NONE', #3537, #63506, #20567 ) ;
#119904 = EDGE_CURVE ( 'NONE', #171099, #74869, #137958, .T. ) ;
#119905 = ORIENTED_EDGE ( 'NONE', *, *, #65709, .F. ) ;
#119906 = AXIS2_PLACEMENT_3D ( 'NONE', #248083, #228540, #149011 ) ;
#119907 = FACE_OUTER_BOUND ( 'NONE', #195770, .T. ) ;
#119908 = AXIS2_PLACEMENT_3D ( 'NONE', #220878, #240455, #61825 ) ;
#119909 = ORIENTED_EDGE ( 'NONE', *, *, #252232, .T. ) ;
#119910 = ADVANCED_FACE ( 'NONE', ( #68553 ), #148088, .F. ) ;
#119911 =( BOUNDED_CURVE ( )  B_SPLINE_CURVE ( 3, ( #45150, #6012, #67284, #244628 ),
 .UNSPECIFIED., .F., .F. ) 
 B_SPLINE_CURVE_WITH_KNOTS ( ( 4, 4 ),
 ( 1.570796326794908992, 2.617993877991592555 ),
 .UNSPECIFIED. ) 
 CURVE ( )  GEOMETRIC_REPRESENTATION_ITEM ( )  RATIONAL_B_SPLINE_CURVE ( ( 1.000000000000000000, 0.9106836025229446685, 0.9106836025229446685, 1.000000000000000000 ) ) 
 REPRESENTATION_ITEM ( '' )  );
#119912 = CARTESIAN_POINT ( 'NONE',  ( 18.46858270002953262, 85.47420267472266175, -129.4210855498203614 ) ) ;
#119913 = LINE ( 'NONE', #199438, #161854 ) ;
#119914 = CARTESIAN_POINT ( 'NONE',  ( 22.60000000000000142, 64.05844819680034163, -247.1686437718134073 ) ) ;
#119916 = ORIENTED_EDGE ( 'NONE', *, *, #200115, .F. ) ;
#119915 = B_SPLINE_CURVE_WITH_KNOTS ( 'NONE', 3,
 ( #234245, #119461, #195165, #59430, #138972, #176877, #156031, #133870, #16514, #255034, #235530, #17756, #198980, #56867, #179439, #214686 ),
 .UNSPECIFIED., .F., .F.,
 ( 4, 3, 3, 3, 3, 4 ),
 ( 0.000000000000000000, 2.209075297431620268E-05, 5.594258369009782919E-05, 8.979524372342005711E-05, 0.0001236472815274570580, 0.0001574990747609547690 ),
 .UNSPECIFIED. ) ;
#119917 = CARTESIAN_POINT ( 'NONE',  ( -18.59999999999999787, 64.35000000001190301, -96.00830171387039513 ) ) ;
#119918 = ADVANCED_FACE ( 'NONE', ( #9853 ), #64689, .T. ) ;
#119919 = LINE ( 'NONE', #256771, #6494 ) ;
#119920 = DIRECTION ( 'NONE',  ( 0.000000000000000000, -0.8700118002898321601, 0.4930308989875230030 ) ) ;
#119921 = AXIS2_PLACEMENT_3D ( 'NONE', #134673, #16066, #194702 ) ;
#119922 = DIRECTION ( 'NONE',  ( 1.000000000000000000, 0.000000000000000000, 0.000000000000000000 ) ) ;
#119923 = AXIS2_PLACEMENT_3D ( 'NONE', #103378, #199956, #237783 ) ;
#119924 = DIRECTION ( 'NONE',  ( -0.000000000000000000, -0.000000000000000000, -1.000000000000000000 ) ) ;
#119925 = FACE_OUTER_BOUND ( 'NONE', #50439, .T. ) ;
#119926 = ADVANCED_BREP_SHAPE_REPRESENTATION ( '', ( #25248, #2425 ), #227278 ) ;
#119927 = AXIS2_PLACEMENT_3D ( 'NONE', #212179, #192603, #231739 ) ;
#119928 = CIRCLE ( 'NONE', #48961, 0.09999999999999939493 ) ;
#119929 = ORIENTED_EDGE ( 'NONE', *, *, #238694, .T. ) ;
#119930 = CARTESIAN_POINT ( 'NONE',  ( 20.94999999999999574, 77.83534155023627932, -91.46795619196132066 ) ) ;
#119933 = EDGE_LOOP ( 'NONE', ( #169246, #213083, #188268, #133744 ) ) ;
#119932 = CARTESIAN_POINT ( 'NONE',  ( -22.50000000000000000, 76.00000000001165290, -69.62310748452432563 ) ) ;
#119931 = AXIS2_PLACEMENT_3D ( 'NONE', #9049, #248959, #246382 ) ;
#119934 = PLANE ( 'NONE',  #163385 ) ;
#119935 = ADVANCED_FACE ( 'NONE', ( #244608 ), #5986, .F. ) ;
#119936 = CARTESIAN_POINT ( 'NONE',  ( -16.77732147262506146, 9.945966932629788815, -188.3364912432758445 ) ) ;
#119937 = AXIS2_PLACEMENT_3D ( 'NONE', #188662, #89552, #107842 ) ;
#119938 = DIRECTION ( 'NONE',  ( 1.000000000000000000, 0.000000000000000000, 0.000000000000000000 ) ) ;
#119939 = ORIENTED_EDGE ( 'NONE', *, *, #160265, .F. ) ;
#119940 = CARTESIAN_POINT ( 'NONE',  ( -22.50000000000000000, 75.90000000001222702, -148.1726782920690937 ) ) ;
#119941 = SHAPE_DEFINITION_REPRESENTATION ( #153648, #241717 ) ;
#119942 = LINE ( 'NONE', #25949, #217188 ) ;
#119943 = VERTEX_POINT ( 'NONE', #223751 ) ;
#119944 = CARTESIAN_POINT ( 'NONE',  ( -18.50000000000000000, 64.35000000001259934, -191.2731074845244450 ) ) ;
#119945 = TOROIDAL_SURFACE ( 'NONE', #86552, 0.4000000000000012990, 0.1000000000000000056 ) ;
#119946 = AXIS2_PLACEMENT_3D ( 'NONE', #82643, #146486, #223458 ) ;
#119947 = DIRECTION ( 'NONE',  ( -1.000000000000000000, 0.000000000000000000, 0.000000000000000000 ) ) ;
#119948 = ORIENTED_EDGE ( 'NONE', *, *, #214977, .T. ) ;
#119949 = ORIENTED_EDGE ( 'NONE', *, *, #87625, .F. ) ;
#119950 = DIRECTION ( 'NONE',  ( 0.000000000000000000, -0.000000000000000000, -1.000000000000000000 ) ) ;
#119951 = DIRECTION ( 'NONE',  ( -1.000000000000000000, -0.000000000000000000, -0.000000000000000000 ) ) ;
#119953 = AXIS2_PLACEMENT_3D ( 'NONE', #148075, #67244, #165064 ) ;
#119952 = LINE ( 'NONE', #199476, #31947 ) ;
#119954 = CARTESIAN_POINT ( 'NONE',  ( 18.58143601961908331, 10.43572941510574026, -125.2500000000000568 ) ) ;
#119955 = DIRECTION ( 'NONE',  ( 0.000000000000000000, -0.9770955615653316162, -0.2128009952263604232 ) ) ;
#119956 = CIRCLE ( 'NONE', #215581, 0.5000000000000004441 ) ;
#119958 = LINE ( 'NONE', #199481, #45424 ) ;
#119957 = CARTESIAN_POINT ( 'NONE',  ( 18.52928932188134326, 65.72071067813041623, -78.31452884076169596 ) ) ;
#119959 = CARTESIAN_POINT ( 'NONE',  ( 20.84999999999998721, 65.66751761918619934, -30.42826094061123854 ) ) ;
#119960 = DIRECTION ( 'NONE',  ( 0.000000000000000000, 6.982962677686266711E-15, -1.000000000000000000 ) ) ;
#119961 = CARTESIAN_POINT ( 'NONE',  ( -20.54999999999999716, 23.45160524131172508, -253.2535058871250726 ) ) ;
#119962 = FACE_OUTER_BOUND ( 'NONE', #252292, .T. ) ;
#119963 = ORIENTED_EDGE ( 'NONE', *, *, #168909, .F. ) ;
#119964 = ORIENTED_EDGE ( 'NONE', *, *, #210955, .F. ) ;
#119965 = DIRECTION ( 'NONE',  ( 0.000000000000000000, 0.008583690987124100932, -0.9999631594459055250 ) ) ;
#119967 = CARTESIAN_POINT ( 'NONE',  ( 20.84999999999998721, 65.66751761918722252, -164.4282609406112670 ) ) ;
#119966 = CARTESIAN_POINT ( 'NONE',  ( -21.05000000000000071, 69.45934304831071415, -102.9231074845243512 ) ) ;
#119968 = CIRCLE ( 'NONE', #194958, 0.09999999999999939493 ) ;
#119969 = DIRECTION ( 'NONE',  ( 0.000000000000000000, -1.000000000000000000, 2.771150684185008344E-14 ) ) ;
#119970 = DIRECTION ( 'NONE',  ( -1.000000000000000000, 3.854941057726231589E-15, 0.000000000000000000 ) ) ;
#119972 = EDGE_CURVE ( 'NONE', #77258, #144320, #44837, .T. ) ;
#119971 = FACE_OUTER_BOUND ( 'NONE', #166565, .T. ) ;
#119973 = EDGE_LOOP ( 'NONE', ( #208927, #243696, #104089, #232179 ) ) ;
#119974 = AXIS2_PLACEMENT_3D ( 'NONE', #246114, #24513, #205679 ) ;
#119975 = FACE_OUTER_BOUND ( 'NONE', #132992, .T. ) ;
#119976 = VERTEX_POINT ( 'NONE', #166398 ) ;
#119977 = ADVANCED_FACE ( 'NONE', ( #168977 ), #88076, .T. ) ;
#119979 = EDGE_CURVE ( 'NONE', #228001, #166580, #149950, .T. ) ;
#119978 = CIRCLE ( 'NONE', #136480, 0.09999999999999939493 ) ;
#119980 = CIRCLE ( 'NONE', #253209, 0.09999999999999749367 ) ;
#119981 = CARTESIAN_POINT ( 'NONE',  ( -12.68215100488889924, 9.396630376317714806, -17.90705739281830589 ) ) ;
#119982 = VECTOR ( 'NONE', #29281, 1000.000000000000000 ) ;
#119983 = ORIENTED_EDGE ( 'NONE', *, *, #128372, .F. ) ;
#119984 = CARTESIAN_POINT ( 'NONE',  ( 23.24999999999999645, 76.00000000001244871, -170.0231074845243597 ) ) ;
#119985 = AXIS2_PLACEMENT_3D ( 'NONE', #174358, #236836, #60759 ) ;
#119986 = CARTESIAN_POINT ( 'NONE',  ( 18.40916198585728836, 85.50000000001136868, -29.42291785270129623 ) ) ;
#119987 = ORIENTED_EDGE ( 'NONE', *, *, #47963, .F. ) ;
#119988 = FACE_OUTER_BOUND ( 'NONE', #130193, .T. ) ;
#119989 = EDGE_CURVE ( 'NONE', #179663, #58814, #52798, .T. ) ;
#119990 = ORIENTED_EDGE ( 'NONE', *, *, #54571, .F. ) ;
#119991 = LINE ( 'NONE', #159108, #87042 ) ;
#119993 = AXIS2_PLACEMENT_3D ( 'NONE', #147871, #48748, #221596 ) ;
#119992 = DIRECTION ( 'NONE',  ( -0.000000000000000000, -0.000000000000000000, -1.000000000000000000 ) ) ;
#119994 = DIRECTION ( 'NONE',  ( 0.000000000000000000, 0.9908441862701605762, -0.1350103645451835310 ) ) ;
#119995 = CARTESIAN_POINT ( 'NONE',  ( 18.59999999999999432, -1.835859311432484375, -78.50443916879852679 ) ) ;
#119997 = DIRECTION ( 'NONE',  ( -0.000000000000000000, 0.8660254037844411501, 0.4999999999999956701 ) ) ;
#119996 = PLANE ( 'NONE',  #141439 ) ;
#119998 = DIRECTION ( 'NONE',  ( -1.000000000000000000, -0.000000000000000000, -0.000000000000000000 ) ) ;
#120000 = ORIENTED_EDGE ( 'NONE', *, *, #195409, .T. ) ;
#119999 = DIRECTION ( 'NONE',  ( -1.000000000000000000, -0.000000000000000000, -0.000000000000000000 ) ) ;
#120002 = CARTESIAN_POINT ( 'NONE',  ( 20.94999999999999929, 45.16048418391989117, -238.5653317536036582 ) ) ;
#120001 = DIRECTION ( 'NONE',  ( -0.000000000000000000, -6.982962677686266711E-15, 1.000000000000000000 ) ) ;
#120003 = VERTEX_POINT ( 'NONE', #247169 ) ;
#120005 = ORIENTED_EDGE ( 'NONE', *, *, #28390, .F. ) ;
#120004 = CARTESIAN_POINT ( 'NONE',  ( -18.59999999999999787, 64.35000000001222986, -148.6731074845244507 ) ) ;
#120006 = AXIS2_PLACEMENT_3D ( 'NONE', #120008, #140826, #121300 ) ;
#120007 = ORIENTED_EDGE ( 'NONE', *, *, #167048, .T. ) ;
#120008 = CARTESIAN_POINT ( 'NONE',  ( -6.000000000000003553, -11.25000000000000000, 10.00000000000000178 ) ) ;
#120009 = FACE_OUTER_BOUND ( 'NONE', #123373, .T. ) ;
#120010 = FACE_OUTER_BOUND ( 'NONE', #75837, .T. ) ;
#120011 = ORIENTED_EDGE ( 'NONE', *, *, #86774, .F. ) ;
#120012 = EDGE_CURVE ( 'NONE', #40935, #4681, #114905, .T. ) ;
#120014 = EDGE_CURVE ( 'NONE', #11610, #133529, #183957, .T. ) ;
#120013 = DIRECTION ( 'NONE',  ( 0.000000000000000000, -0.4999999999999348299, 0.8660254037844762331 ) ) ;
#120015 = CARTESIAN_POINT ( 'NONE',  ( 21.14999999999999858, 64.35000000001214460, -136.4231074845243938 ) ) ;
#120016 = DIRECTION ( 'NONE',  ( 0.000000000000000000, 0.9908441862701596881, -0.1350103645451904977 ) ) ;
#120017 = CARTESIAN_POINT ( 'NONE',  ( -16.92973740335288824, 9.992503814478434165, -154.9060590352028441 ) ) ;
#120018 = EDGE_CURVE ( 'NONE', #52387, #140944, #178914, .T. ) ;
#120019 = DIRECTION ( 'NONE',  ( -1.000000000000000000, 0.000000000000000000, 0.000000000000000000 ) ) ;
#120020 = CIRCLE ( 'NONE', #174194, 0.09999999999999681366 ) ;
#120021 = ORIENTED_EDGE ( 'NONE', *, *, #223594, .T. ) ;
#120023 = VERTEX_POINT ( 'NONE', #153256 ) ;
#120022 = AXIS2_PLACEMENT_3D ( 'NONE', #168689, #108661, #109935 ) ;
#120024 = TOROIDAL_SURFACE ( 'NONE', #187206, 14.20833333333334103, 0.1000000000000000056 ) ;
#120025 = DIRECTION ( 'NONE',  ( -1.000000000000000000, -1.836970198721029934E-16, 0.000000000000000000 ) ) ;
#120026 = AXIS2_PLACEMENT_3D ( 'NONE', #51533, #170284, #210644 ) ;
#120027 = EDGE_LOOP ( 'NONE', ( #183469, #6433, #81946 ) ) ;
#120028 = CARTESIAN_POINT ( 'NONE',  ( -16.94107738177415357, 10.01423928513661998, -12.54999999999999361 ) ) ;
#120029 = VERTEX_POINT ( 'NONE', #150653 ) ;
#120030 = CARTESIAN_POINT ( 'NONE',  ( 20.91682497891422798, 10.32263460347359363, -173.0605957968672328 ) ) ;
#120031 = LINE ( 'NONE', #177439, #23139 ) ;
#120032 = PLANE ( 'NONE',  #85056 ) ;
#120033 = CARTESIAN_POINT ( 'NONE',  ( -18.59999999999999787, 64.35000000001198828, -115.2731074845243739 ) ) ;
#120034 = EDGE_CURVE ( 'NONE', #146995, #13313, #17366, .T. ) ;
#120035 = AXIS2_PLACEMENT_3D ( 'NONE', #86507, #248190, #163514 ) ;
#120037 = CIRCLE ( 'NONE', #111627, 0.1999999999999987899 ) ;
#120036 = DIRECTION ( 'NONE',  ( -0.000000000000000000, -6.982962677686266711E-15, 1.000000000000000000 ) ) ;
#120038 = CYLINDRICAL_SURFACE ( 'NONE', #186291, 0.09999999999999892308 ) ;
#120039 = ORIENTED_EDGE ( 'NONE', *, *, #127167, .F. ) ;
#120041 = FACE_OUTER_BOUND ( 'NONE', #134880, .T. ) ;
#120040 = DIRECTION ( 'NONE',  ( 0.000000000000000000, 0.000000000000000000, -1.000000000000000000 ) ) ;
#120042 = ORIENTED_EDGE ( 'NONE', *, *, #134585, .T. ) ;
#120045 = ORIENTED_EDGE ( 'NONE', *, *, #142070, .F. ) ;
#120044 = SURFACE_STYLE_USAGE ( .BOTH. , #44339 ) ;
#120043 = DIRECTION ( 'NONE',  ( 1.000000000000000000, 0.000000000000000000, 0.000000000000000000 ) ) ;
#120046 = VERTEX_POINT ( 'NONE', #133651 ) ;
#120047 = CIRCLE ( 'NONE', #7582, 0.09999999999999939493 ) ;
#120048 = CARTESIAN_POINT ( 'NONE',  ( 23.14999999999999858, 76.00000000001141132, -34.02310748452431710 ) ) ;
#120049 = CARTESIAN_POINT ( 'NONE',  ( 21.04999999999999716, 0.01471785653530480707, -60.65527659590978260 ) ) ;
#120050 = CYLINDRICAL_SURFACE ( 'NONE', #48536, 0.1000000000000028644 ) ;
#120051 = ADVANCED_FACE ( 'NONE', ( #79748 ), #172830, .F. ) ;
#120052 = CARTESIAN_POINT ( 'NONE',  ( 18.39999999999999858, -9.499999999988842703, -74.03206939669971121 ) ) ;
#120053 = ORIENTED_EDGE ( 'NONE', *, *, #163278, .F. ) ;
#120054 = CARTESIAN_POINT ( 'NONE',  ( 20.27550659511089037, 66.78395627750340680, -149.1731074845244223 ) ) ;
#120055 = FACE_OUTER_BOUND ( 'NONE', #7162, .T. ) ;
#120056 = EDGE_CURVE ( 'NONE', #201690, #255841, #251008, .T. ) ;
#120058 = CARTESIAN_POINT ( 'NONE',  ( 20.94999999999999574, 10.47338541491290442, -7.578654464248542943 ) ) ;
#120057 = DIRECTION ( 'NONE',  ( 0.000000000000000000, 0.9910827722268055195, -0.1332476588733540468 ) ) ;
#120059 = EDGE_CURVE ( 'NONE', #118267, #159944, #125506, .T. ) ;
#120061 = VERTEX_POINT ( 'NONE', #189779 ) ;
#120060 = CARTESIAN_POINT ( 'NONE',  ( 18.49999999999998934, 69.45000000001206786, -126.5060803140843291 ) ) ;
#120062 = ORIENTED_EDGE ( 'NONE', *, *, #5812, .F. ) ;
#120063 = CIRCLE ( 'NONE', #32582, 0.09999999999999724387 ) ;
#120064 = VECTOR ( 'NONE', #5544, 1000.000000000000000 ) ;
#120065 = TOROIDAL_SURFACE ( 'NONE', #132505, 0.4000000000000005773, 0.1000000000000000056 ) ;
#120066 = EDGE_CURVE ( 'NONE', #201612, #100761, #230183, .T. ) ;
#120067 = DIRECTION ( 'NONE',  ( 0.000000000000000000, -1.000000000000000000, 0.000000000000000000 ) ) ;
#120069 = ADVANCED_FACE ( 'NONE', ( #52817 ), #98116, .T. ) ;
#120068 = ORIENTED_EDGE ( 'NONE', *, *, #142620, .T. ) ;
#120070 = SPHERICAL_SURFACE ( 'NONE', #14576, 0.1000000000000000056 ) ;
#120071 = EDGE_LOOP ( 'NONE', ( #106037, #28567, #79027, #36040 ) ) ;
#120072 = CARTESIAN_POINT ( 'NONE',  ( 21.05000000000000071, -1.162701749926853712, -175.3999999999999773 ) ) ;
#120073 = CARTESIAN_POINT ( 'NONE',  ( -23.25000000000000000, -11.74999999998884448, -100.5000000000000284 ) ) ;
#120074 = CARTESIAN_POINT ( 'NONE',  ( -18.39999999999999858, 85.60000000001139142, -29.42291809330221142 ) ) ;
#120075 = CIRCLE ( 'NONE', #20086, 12.87500000000000178 ) ;
#120076 = EDGE_CURVE ( 'NONE', #181631, #242144, #121451, .T. ) ;
#120077 = ORIENTED_EDGE ( 'NONE', *, *, #108358, .T. ) ;
#120078 = FACE_OUTER_BOUND ( 'NONE', #20701, .T. ) ;
#120079 = ADVANCED_FACE ( 'NONE', ( #18522 ), #238853, .T. ) ;
#120080 = AXIS2_PLACEMENT_3D ( 'NONE', #174935, #155350, #135737 ) ;
#120081 = CIRCLE ( 'NONE', #207551, 0.1000000000000028644 ) ;
#120082 = CARTESIAN_POINT ( 'NONE',  ( -16.87683809663752399, 9.850000000011144508, -53.59763598180369826 ) ) ;
#120083 = EDGE_CURVE ( 'NONE', #186823, #169023, #146339, .T. ) ;
#120084 = EDGE_CURVE ( 'NONE', #194623, #148114, #50654, .T. ) ;
#120085 = CIRCLE ( 'NONE', #57672, 0.09999999999999939493 ) ;
#120086 = VERTEX_POINT ( 'NONE', #141044 ) ;
#120087 = ORIENTED_EDGE ( 'NONE', *, *, #3682, .T. ) ;
#120088 = ORIENTED_EDGE ( 'NONE', *, *, #86594, .F. ) ;
#120089 = EDGE_CURVE ( 'NONE', #146041, #207925, #199749, .T. ) ;
#120090 = CYLINDRICAL_SURFACE ( 'NONE', #104061, 0.09999999999999609201 ) ;
#120091 = ORIENTED_EDGE ( 'NONE', *, *, #202271, .F. ) ;
#120093 = EDGE_LOOP ( 'NONE', ( #81632, #171274, #90015, #59071 ) ) ;
#120092 = CARTESIAN_POINT ( 'NONE',  ( -23.25000000000000000, 71.65000000001207070, -124.2731074845243313 ) ) ;
#120095 = EDGE_CURVE ( 'NONE', #238954, #111525, #181462, .T. ) ;
#120094 = ORIENTED_EDGE ( 'NONE', *, *, #113180, .T. ) ;
#120096 = CIRCLE ( 'NONE', #3520, 4.000000000000003553 ) ;
#120097 = EDGE_CURVE ( 'NONE', #46294, #173457, #146106, .T. ) ;
#120100 = ORIENTED_EDGE ( 'NONE', *, *, #143546, .T. ) ;
#120099 = ORIENTED_EDGE ( 'NONE', *, *, #90950, .F. ) ;
#120098 = DIRECTION ( 'NONE',  ( 0.000000000000000000, -0.9126074666063660468, -0.4088369013363524762 ) ) ;
#120101 = EDGE_CURVE ( 'NONE', #250243, #226600, #241428, .T. ) ;
#120103 = ORIENTED_EDGE ( 'NONE', *, *, #217690, .T. ) ;
#120102 = TOROIDAL_SURFACE ( 'NONE', #57695, 0.6000000000000017542, 0.1000000000000000056 ) ;
#120104 = CARTESIAN_POINT ( 'NONE',  ( -21.05000000000000071, 86.27712145182582049, -209.5223386573213702 ) ) ;
#120105 = AXIS2_PLACEMENT_3D ( 'NONE', #155407, #152838, #94100 ) ;
#120106 = CARTESIAN_POINT ( 'NONE',  ( -23.25000000000000000, 4.350000000011156054, -54.64999999999999858 ) ) ;
#120107 = AXIS2_PLACEMENT_3D ( 'NONE', #229811, #154181, #55004 ) ;
#120108 = CARTESIAN_POINT ( 'NONE',  ( -16.84981964351492323, 14.08033693763356986, -219.0474555060754085 ) ) ;
#120109 = CIRCLE ( 'NONE', #7656, 0.09999999999999892308 ) ;
#120110 = CIRCLE ( 'NONE', #153438, 0.09999999999998898659 ) ;
#120111 = ORIENTED_EDGE ( 'NONE', *, *, #135403, .T. ) ;
#120112 = AXIS2_PLACEMENT_3D ( 'NONE', #206493, #169985, #89109 ) ;
#120113 = CARTESIAN_POINT ( 'NONE',  ( -18.50000000000000000, 64.35000000001180354, -81.67310748452439384 ) ) ;
#120115 = ORIENTED_EDGE ( 'NONE', *, *, #238665, .F. ) ;
#120114 = DIRECTION ( 'NONE',  ( 0.000000000000000000, -0.9651348961777157509, 0.2617529984165031243 ) ) ;
#120116 = CARTESIAN_POINT ( 'NONE',  ( 21.14999999999999858, 6.093673009692411213, -199.5727803633481301 ) ) ;
#120118 = ORIENTED_EDGE ( 'NONE', *, *, #136119, .F. ) ;
#120117 = DIRECTION ( 'NONE',  ( 1.000000000000000000, 0.000000000000000000, 0.000000000000000000 ) ) ;
#120119 = EDGE_CURVE ( 'NONE', #17892, #9372, #1509, .T. ) ;
#120120 = VECTOR ( 'NONE', #188404, 1000.000000000000000 ) ;
#120121 = ORIENTED_EDGE ( 'NONE', *, *, #83477, .F. ) ;
#120122 = DIRECTION ( 'NONE',  ( 1.000000000000000000, 0.000000000000000000, 0.000000000000000000 ) ) ;
#120123 = FACE_OUTER_BOUND ( 'NONE', #175871, .T. ) ;
#120124 = EDGE_LOOP ( 'NONE', ( #150239, #150192, #50530, #155595 ) ) ;
#120125 = VERTEX_POINT ( 'NONE', #184006 ) ;
#120126 = CARTESIAN_POINT ( 'NONE',  ( 17.74533788810830615, 10.81849979148195118, -77.31362267494763785 ) ) ;
#120128 = DIRECTION ( 'NONE',  ( 0.000000000000000000, -0.6728971962617172897, 0.7397360091702445128 ) ) ;
#120127 = B_SPLINE_CURVE_WITH_KNOTS ( 'NONE', 3,
 ( #158529, #238030, #124522, #99783, #102343, #25426, #1979, #239330, #140197, #4549, #41150, #101038, #81498, #44980, #142767, #123231 ),
 .UNSPECIFIED., .F., .F.,
 ( 4, 3, 3, 3, 3, 4 ),
 ( 0.000000000000000000, 1.810570668010599751E-05, 2.740575833570006129E-05, 4.256816319434536945E-05, 5.213463471025743496E-05, 6.641585710718904932E-05 ),
 .UNSPECIFIED. ) ;
#120129 = AXIS2_PLACEMENT_3D ( 'NONE', #244130, #64225, #227143 ) ;
#120130 = AXIS2_PLACEMENT_3D ( 'NONE', #116668, #141364, #18848 ) ;
#120132 = ORIENTED_EDGE ( 'NONE', *, *, #168383, .T. ) ;
#120131 = ORIENTED_EDGE ( 'NONE', *, *, #28530, .T. ) ;
#120134 = ORIENTED_EDGE ( 'NONE', *, *, #12557, .F. ) ;
#120133 = CLOSED_SHELL ( 'NONE', ( #192124, #214677, #24678, #60923, #250528, #120275, #75359, #145926, #10296, #217970, #137890, #233437, #94708, #23212, #63912, #208947, #242782, #187570, #16119, #225237, #146263, #251595, #103189, #16277, #20754, #4516, #107907, #152826, #129796, #52915, #167817, #86253, #165663, #19818, #9454, #101507, #160571, #185699, #242946, #171942, #41874, #120397, #23584, #76193, #110253, #173743, #159294, #41512, #2944, #190451, #251624, #222701, #115176, #35948, #233720, #122629, #37795, #22854, #228360, #246002, #151160, #33850, #129422, #74292, #232787, #213334, #256885, #108666, #26704, #30179, #67948, #186849, #143225, #256756, #190129, #22538, #142632, #126210, #33490, #53165, #150572, #86250, #165958, #150282, #53156, #30321, #29919, #124442, #197624, #205308, #75646, #133957, #161144, #202147, #110598, #114329, #109744, #106702, #145141, #175658, #177688, #139687, #198769, #72215, #248117, #94448, #65388, #143566, #187419, #15907, #105875, #5684, #252319, #119079, #195033, #141484, #156234, #60748, #136538, #25726, #168429, #38382, #219936, #128931, #2652, #73685, #40117, #154808, #89716, #197704, #172256, #194766, #15249, #42991, #214083, #110539, #159872, #197638, #144538, #74053, #95357, #125087, #97563, #2845, #16225, #175759, #143824, #241775, #82384, #78230, #42505, #20200, #187848, #180326, #191586, #98995, #231843, #238711, #147208, #188151, #124986, #95856, #137317, #230603, #2518, #136209, #29707, #113010, #36335, #184528, #102773, #92053, #233190, #93781, #139484, #96001, #60344, #228301, #153484, #212394, #252217, #45483, #70760, #76322, #65239, #138764, #203996, #67805, #114995, #14368, #120654, #106415, #180499, #246811, #43478, #247178, #91487, #219899, #170420, #172466, #52608, #92000, #24149, #131500, #239278, #21974, #116034, #81546, #135535, #156711, #18679, #210529, #114803, #136446, #60732, #80601, #252705, #21490, #172825, #2511, #160433, #110018, #39505, #180452, #219128, #88874, #25981, #26110, #233180, #140791, #31725, #144359, #8129, #231043, #248965, #27785, #229737, #58669, #82515, #218406, #50214, #255045, #198971, #139116, #89631, #86127, #74488, #56578, #31113, #174763, #65781, #231768, #112862, #165433, #90698, #136974, #91821, #5089, #225760, #210724, #55946, #257746, #195462, #178655, #51473, #76757, #77619, #202726, #256889, #228689, #236914, #220273, #220460, #201716, #174767, #154473, #44437, #118264, #112920, #216051, #75660, #39984, #63416, #13715, #235386, #154223, #111291, #18850, #42138, #156811, #200204, #229207, #36216, #4502, #217795, #54198, #63218, #102730, #55512, #49297, #61046, #202447, #78220, #50178, #86384, #59316, #130670, #87391, #68224, #117438, #134943, #14903, #178989, #141757, #40291, #9945, #220268, #202956, #127476, #36830, #140290, #157896, #125355, #123097, #113678, #24716, #133828, #46026, #89594, #248491, #198691, #181733, #235156, #104264, #102004, #202046, #58324, #226838, #81745, #115344, #129991, #135894, #108904, #223030, #62900, #39254, #3603, #26130, #193146, #83429, #62094, #221174, #64543, #89693, #110432, #32594, #212988, #197657, #103800, #76256, #190737, #237976, #181346, #59902, #156174, #213322, #232025, #150899, #186342, #216300, #92926, #107847, #245542, #151857, #199902, #95992, #59816, #150083, #62621, #210218, #205839, #204897, #25954, #205264, #132463, #257791, #744, #22575, #136906, #125093, #15285, #115042, #153212, #232139, #239581, #233749, #126948, #151991, #257973, #247967, #89058, #127701, #153686, #163241, #79062, #145949, #41589, #255756, #28796, #7025, #172238, #149799, #46662, #23712, #151257, #119408, #128062, #227441, #75982, #40758, #127480, #245742, #126915, #191768, #55394, #154861, #106234, #74597, #217941, #231856, #14911, #236434, #250155, #170249, #49044, #156243, #231695, #192863, #112011, #96306, #216350, #88457, #35109, #77653, #18684, #117979, #23759, #217439, #145572, #91714, #173575, #41103, #84304, #75852, #165584, #75921, #194016, #237798, #158233, #122919, #174375, #110315, #96509, #183622, #175681, #173715, #103585, #91952, #195439, #223642, #115948, #69126, #102130, #6922, #201079, #129179, #71207, #127314 ) ) ;
#120135 = CARTESIAN_POINT ( 'NONE',  ( -23.15000000000000213, 76.00000000001126921, -203.5231074845248997 ) ) ;
#120136 = VERTEX_POINT ( 'NONE', #41957 ) ;
#120137 = ORIENTED_EDGE ( 'NONE', *, *, #114650, .T. ) ;
#120138 = CARTESIAN_POINT ( 'NONE',  ( -23.15000000000000213, 71.75000000001180922, -81.87310748452433984 ) ) ;
#120139 = ORIENTED_EDGE ( 'NONE', *, *, #172983, .F. ) ;
#120140 = DIRECTION ( 'NONE',  ( -0.000000000000000000, -1.000000000000000000, 0.000000000000000000 ) ) ;
#120142 = DIRECTION ( 'NONE',  ( 0.000000000000000000, 0.000000000000000000, -1.000000000000000000 ) ) ;
#120141 = DIRECTION ( 'NONE',  ( -1.000000000000000000, 0.000000000000000000, 0.000000000000000000 ) ) ;
#120143 = ORIENTED_EDGE ( 'NONE', *, *, #56179, .T. ) ;
#120144 = CIRCLE ( 'NONE', #74357, 0.09999999999998898659 ) ;
#120145 = CIRCLE ( 'NONE', #36946, 0.1000000000000000472 ) ;
#120147 = EDGE_LOOP ( 'NONE', ( #152954, #127177, #77855, #36905 ) ) ;
#120146 = VERTEX_POINT ( 'NONE', #243977 ) ;
#120148 = DIRECTION ( 'NONE',  ( 1.000000000000000000, -0.000000000000000000, -0.000000000000000000 ) ) ;
#120150 = EDGE_CURVE ( 'NONE', #61430, #146933, #584, .T. ) ;
#120149 = CARTESIAN_POINT ( 'NONE',  ( 18.59999999999999432, -1.162701749938009677, -8.000000000000000000 ) ) ;
#120151 = CIRCLE ( 'NONE', #36757, 0.1000000000000106498 ) ;
#120152 = ORIENTED_EDGE ( 'NONE', *, *, #175028, .F. ) ;
#120153 = EDGE_CURVE ( 'NONE', #178237, #212838, #90211, .T. ) ;
#120154 = CARTESIAN_POINT ( 'NONE',  ( -21.05000000000000071, 1.148907358139439339E-11, -201.0000000000015064 ) ) ;
#120155 = VERTEX_POINT ( 'NONE', #224411 ) ;
#120156 = ORIENTED_EDGE ( 'NONE', *, *, #12566, .T. ) ;
#120157 = CARTESIAN_POINT ( 'NONE',  ( -22.39999999999999858, 7.790779598384560245, -134.0000000000000000 ) ) ;
#120158 = ORIENTED_EDGE ( 'NONE', *, *, #222922, .F. ) ;
#120159 = CARTESIAN_POINT ( 'NONE',  ( -23.15000000000000213, 11.65000000000000036, -12.25000000000000000 ) ) ;
#120160 = CARTESIAN_POINT ( 'NONE',  ( 21.05000000000000071, 76.10000000001198828, -109.5637644362255543 ) ) ;
#120161 = EDGE_LOOP ( 'NONE', ( #83303, #35152, #15200, #69068 ) ) ;
#120162 = AXIS2_PLACEMENT_3D ( 'NONE', #181554, #45872, #201095 ) ;
#120163 = CARTESIAN_POINT ( 'NONE',  ( 22.50000000000000000, 36.65892442174472876, -249.5511627012454596 ) ) ;
#120164 = DIRECTION ( 'NONE',  ( 0.000000000000000000, -7.026728003956683390E-15, 1.000000000000000000 ) ) ;
#120166 = CARTESIAN_POINT ( 'NONE',  ( -16.77180007708460607, 9.950000000011137047, -121.3643858810452087 ) ) ;
#120165 = CARTESIAN_POINT ( 'NONE',  ( 23.24999999999999645, 71.00000000001180922, -81.92837350343744163 ) ) ;
#120167 = CYLINDRICAL_SURFACE ( 'NONE', #239858, 0.1000000000000124678 ) ;
#120168 = DIRECTION ( 'NONE',  ( 0.000000000000000000, -1.000000000000000000, -8.717686153663073805E-15 ) ) ;
#120170 = CIRCLE ( 'NONE', #95182, 0.1000000000000059591 ) ;
#120169 = DIRECTION ( 'NONE',  ( -5.603264701231743991E-32, -7.172728831056617961E-15, 1.000000000000000000 ) ) ;
#120171 = AXIS2_PLACEMENT_3D ( 'NONE', #101882, #181468, #202301 ) ;
#120172 = DIRECTION ( 'NONE',  ( -0.7071067811865475727, 0.7071067811865475727, 4.937700262164531476E-15 ) ) ;
#120173 = DIRECTION ( 'NONE',  ( 5.421010862427554711E-16, 1.000000000000000000, 1.023556919514279895E-14 ) ) ;
#120175 = CARTESIAN_POINT ( 'NONE',  ( 23.14999999999999858, 76.00000000001242029, -166.0231074845243597 ) ) ;
#120174 = VECTOR ( 'NONE', #11005, 1000.000000000000000 ) ;
#120176 = ADVANCED_FACE ( 'NONE', ( #124052 ), #122776, .T. ) ;
#120178 = ORIENTED_EDGE ( 'NONE', *, *, #106889, .F. ) ;
#120177 = AXIS2_PLACEMENT_3D ( 'NONE', #118493, #41528, #178477 ) ;
#120180 = ORIENTED_EDGE ( 'NONE', *, *, #240113, .T. ) ;
#120179 = ORIENTED_EDGE ( 'NONE', *, *, #15160, .T. ) ;
#120181 = ORIENTED_EDGE ( 'NONE', *, *, #180100, .T. ) ;
#120182 = EDGE_LOOP ( 'NONE', ( #125021, #174784 ) ) ;
#120183 = CARTESIAN_POINT ( 'NONE',  ( 20.85000000000000142, 77.36242903720516040, -95.13422623660308375 ) ) ;
#120184 = DIRECTION ( 'NONE',  ( -1.000000000000000000, 0.000000000000000000, 0.000000000000000000 ) ) ;
#120186 = DIRECTION ( 'NONE',  ( 1.000000000000000000, 0.000000000000000000, 0.000000000000000000 ) ) ;
#120185 = DIRECTION ( 'NONE',  ( -3.265361837132813093E-16, -1.000000000000000000, 7.445645354460596589E-46 ) ) ;
#120187 = DIRECTION ( 'NONE',  ( 0.000000000000000000, -6.853228547068871147E-15, 1.000000000000000000 ) ) ;
#120188 = EDGE_LOOP ( 'NONE', ( #223704, #112026, #200357, #76396 ) ) ;
#120189 = VECTOR ( 'NONE', #197888, 1000.000000000000000 ) ;
#120190 = FACE_OUTER_BOUND ( 'NONE', #13295, .T. ) ;
#120191 = FILL_AREA_STYLE_COLOUR ( '', #2038 ) ;
#120192 = FACE_OUTER_BOUND ( 'NONE', #133554, .T. ) ;
#120193 = CARTESIAN_POINT ( 'NONE',  ( -21.10000000000000142, 6.322468214605804882, 12.11686199900910310 ) ) ;
#120194 = DIRECTION ( 'NONE',  ( -0.000000000000000000, -0.2617529984165031243, -0.9651348961777157509 ) ) ;
#120195 = ORIENTED_EDGE ( 'NONE', *, *, #86162, .F. ) ;
#120196 = SPHERICAL_SURFACE ( 'NONE', #213790, 0.1000000000000000056 ) ;
#120197 = CARTESIAN_POINT ( 'NONE',  ( -21.05000000000011795, -0.01771943329734000649, -94.05891531152838070 ) ) ;
#120198 = EDGE_LOOP ( 'NONE', ( #52146, #58464, #29397, #29173, #172378, #226334, #21256, #157128, #202063, #13059 ) ) ;
#120199 = CARTESIAN_POINT ( 'NONE',  ( -16.87487986503753845, 66.04999244492597654, -56.87313274483766179 ) ) ;
#120200 = FACE_OUTER_BOUND ( 'NONE', #30358, .T. ) ;
#120201 = DIRECTION ( 'NONE',  ( -0.7071067811865388020, 0.7071067811865561215, 0.000000000000000000 ) ) ;
#120202 = FACE_OUTER_BOUND ( 'NONE', #193192, .T. ) ;
#120203 = SPHERICAL_SURFACE ( 'NONE', #66747, 0.1000000000000000056 ) ;
#120204 = EDGE_LOOP ( 'NONE', ( #90531, #234277, #117994, #7819 ) ) ;
#120205 = CARTESIAN_POINT ( 'NONE',  ( -20.64999999999999858, 76.00000000001143974, -37.92310748452432989 ) ) ;
#120207 = ADVANCED_FACE ( 'NONE', ( #61504 ), #24964, .T. ) ;
#120206 = LINE ( 'NONE', #23669, #117391 ) ;
#120208 = DIRECTION ( 'NONE',  ( 0.000000000000000000, -1.000000000000000000, 0.000000000000000000 ) ) ;
#120210 = DIRECTION ( 'NONE',  ( 0.000000000000000000, 0.000000000000000000, 1.000000000000000000 ) ) ;
#120209 = LINE ( 'NONE', #159317, #224093 ) ;
#120211 = DIRECTION ( 'NONE',  ( 1.000000000000000000, -0.000000000000000000, -0.000000000000000000 ) ) ;
#120212 = EDGE_CURVE ( 'NONE', #36652, #127250, #179684, .T. ) ;
#120213 = PLANE ( 'NONE',  #53975 ) ;
#120214 = VECTOR ( 'NONE', #168886, 1000.000000000000000 ) ;
#120215 = CARTESIAN_POINT ( 'NONE',  ( -21.45000000000000284, 65.32753222054176945, -213.4247798787853867 ) ) ;
#120216 = CARTESIAN_POINT ( 'NONE',  ( 22.48508240969612615, 75.95372358549511205, -114.6731182160978761 ) ) ;
#120217 = AXIS2_PLACEMENT_3D ( 'NONE', #22738, #205186, #142641 ) ;
#120218 = ORIENTED_EDGE ( 'NONE', *, *, #205976, .F. ) ;
#120219 = ORIENTED_EDGE ( 'NONE', *, *, #196779, .T. ) ;
#120220 = EDGE_CURVE ( 'NONE', #148469, #115416, #70522, .T. ) ;
#120221 = VECTOR ( 'NONE', #9531, 1000.000000000000114 ) ;
#120222 = VERTEX_POINT ( 'NONE', #9220 ) ;
#120223 = ADVANCED_FACE ( 'NONE', ( #10523 ), #11826, .T. ) ;
#120224 = DIRECTION ( 'NONE',  ( -1.000000000000000000, -0.000000000000000000, -0.000000000000000000 ) ) ;
#120225 = DIRECTION ( 'NONE',  ( 0.000000000000000000, 0.000000000000000000, -1.000000000000000000 ) ) ;
#120226 = AXIS2_PLACEMENT_3D ( 'NONE', #201203, #141234, #83779 ) ;
#120227 = AXIS2_PLACEMENT_3D ( 'NONE', #129133, #252918, #130403 ) ;
#120228 = CARTESIAN_POINT ( 'NONE',  ( -23.25000000000000000, -11.74999999998884448, -100.5000000000000284 ) ) ;
#120230 = ADVANCED_FACE ( 'NONE', ( #168351 ), #27549, .T. ) ;
#120229 = B_SPLINE_CURVE_WITH_KNOTS ( 'NONE', 3,
 ( #32489, #66445, #225487, #169435, #7761, #209810, #112002, #31212, #166864, #46858, #110703, #246367, #67727, #247645, #147258, #10336 ),
 .UNSPECIFIED., .F., .F.,
 ( 4, 3, 3, 3, 3, 4 ),
 ( 0.000000000000000000, 2.209075297431048351E-05, 5.594258369009902181E-05, 8.979524372342336392E-05, 0.0001236472815274606630, 0.0001574990747609576150 ),
 .UNSPECIFIED. ) ;
#120231 = DIRECTION ( 'NONE',  ( 0.000000000000000000, 0.000000000000000000, 1.000000000000000000 ) ) ;
#120232 = ORIENTED_EDGE ( 'NONE', *, *, #97952, .F. ) ;
#120233 = CIRCLE ( 'NONE', #7781, 0.1000000000000070832 ) ;
#120234 = CARTESIAN_POINT ( 'NONE',  ( -18.59999999999999787, 64.25000000001277556, -215.2731074845244450 ) ) ;
#120235 = DIRECTION ( 'NONE',  ( -3.265361837132813586E-16, 0.9770955615653313941, 0.2128009952263610893 ) ) ;
#120236 = CARTESIAN_POINT ( 'NONE',  ( -21.53752568622130781, 75.90102553874135083, -109.8099153590727894 ) ) ;
#120237 = CARTESIAN_POINT ( 'NONE',  ( -23.25000000000000000, 7.128833340093095217, -233.7327013124392749 ) ) ;
#120239 = ORIENTED_EDGE ( 'NONE', *, *, #4588, .F. ) ;
#120238 = CARTESIAN_POINT ( 'NONE',  ( -16.85722902420149083, 9.950000000011076651, -188.2344525262296600 ) ) ;
#120241 = CARTESIAN_POINT ( 'NONE',  ( -17.78241384944000103, 10.85557575281363896, -157.2509623275143724 ) ) ;
#120240 = FACE_OUTER_BOUND ( 'NONE', #158518, .T. ) ;
#120242 = EDGE_CURVE ( 'NONE', #155996, #229458, #67237, .T. ) ;
#120243 = FACE_OUTER_BOUND ( 'NONE', #88953, .T. ) ;
#120244 =( BOUNDED_SURFACE ( )  B_SPLINE_SURFACE ( 3, 2, ( 
 ( #84160, #163767, #226268 ),
 ( #42518, #47636, #141622 ),
 ( #243278, #221148, #144173 ),
 ( #201593, #131045, #31978 ) ),
 .UNSPECIFIED., .F., .F., .F. ) 
 B_SPLINE_SURFACE_WITH_KNOTS ( ( 4, 4 ),
 ( 3, 3 ),
 ( 4.712388980384689674, 5.765869716888459173 ),
 ( 0.000000000000000000, 1.000000000000000000 ),
 .UNSPECIFIED. ) 
 GEOMETRIC_REPRESENTATION_ITEM ( )  RATIONAL_B_SPLINE_SURFACE ( (
 ( 1.000000000000000000, 0.7071067811865497932, 1.000000000000000000),
 ( 1.000000000000000000, 0.7953136715912831889, 1.000000000000000000),
 ( 1.000000000000000000, 0.8646876308615263351, 1.000000000000000000),
 ( 1.000000000000000000, 0.8984936768950678720, 1.000000000000000000) ) ) 
 REPRESENTATION_ITEM ( '' )  SURFACE ( )  );
#120245 = DIRECTION ( 'NONE',  ( -0.000000000000000000, 0.2128009952263603677, -0.9770955615653313941 ) ) ;
#120246 = EDGE_LOOP ( 'NONE', ( #9798, #30372, #92857, #32575 ) ) ;
#120247 = DIRECTION ( 'NONE',  ( 0.000000000000000000, 0.000000000000000000, 1.000000000000000000 ) ) ;
#120248 = DIRECTION ( 'NONE',  ( 0.000000000000000000, 0.000000000000000000, -1.000000000000000000 ) ) ;
#120249 = FACE_OUTER_BOUND ( 'NONE', #40195, .T. ) ;
#120250 = ORIENTED_EDGE ( 'NONE', *, *, #92253, .F. ) ;
#120251 = CARTESIAN_POINT ( 'NONE',  ( -18.50000000000000000, 74.16465844978745281, -91.46795619196133487 ) ) ;
#120252 = STYLED_ITEM ( 'NONE', ( #33303 ), #107142 ) ;
#120253 = CARTESIAN_POINT ( 'NONE',  ( -23.25000000000000000, 87.65000000001266756, -200.4231074845242802 ) ) ;
#120254 = VERTEX_POINT ( 'NONE', #150043 ) ;
#120256 = B_SPLINE_CURVE_WITH_KNOTS ( 'NONE', 3,
 ( #28593, #108083, #7704, #165494, #105466, #127644, #45533, #125083, #66383, #5085, #248875, #70264, #123792, #168095, #225430, #207189, #187629, #88481, #8972, #228024, #205882, #203327, #186338, #204594, #166799, #148493, #208481, #183763, #67660, #224157 ),
 .UNSPECIFIED., .F., .F.,
 ( 4, 2, 2, 2, 2, 2, 2, 2, 2, 2, 2, 2, 2, 2, 4 ),
 ( 0.000000000000000000, 0.0003422764154113365422, 0.0006845528308226730843, 0.001026829246234009464, 0.001369105661645346169, 0.002053658492468014591, 0.002738211323290683230, 0.003080487738702017333, 0.003422764154113351436, 0.003765040569524685538, 0.004107316984936019641, 0.004449593400347353310, 0.004791869815758687846, 0.005134146231170021515, 0.005476422646581355184 ),
 .UNSPECIFIED. ) ;
#120255 = AXIS2_PLACEMENT_3D ( 'NONE', #14583, #231060, #234899 ) ;
#120257 = CIRCLE ( 'NONE', #57653, 0.2000000000000058675 ) ;
#120258 = CARTESIAN_POINT ( 'NONE',  ( 20.27550659511089037, 9.216043722520002035, -113.1500000000000483 ) ) ;
#120259 = CARTESIAN_POINT ( 'NONE',  ( -23.25000000000000000, 70.60814576644823148, -215.7631455941064189 ) ) ;
#120260 = DIRECTION ( 'NONE',  ( 0.000000000000000000, 0.000000000000000000, -1.000000000000000000 ) ) ;
#120261 = ORIENTED_EDGE ( 'NONE', *, *, #77261, .T. ) ;
#120262 = ORIENTED_EDGE ( 'NONE', *, *, #221868, .T. ) ;
#120263 = DIRECTION ( 'NONE',  ( 0.000000000000000000, 0.000000000000000000, -1.000000000000000000 ) ) ;
#120264 = DIRECTION ( 'NONE',  ( 0.000000000000000000, 0.000000000000000000, 1.000000000000000000 ) ) ;
#120265 = CARTESIAN_POINT ( 'NONE',  ( -16.80891096016324227, 63.09035564583723499, -213.1105745952694690 ) ) ;
#120266 = DIRECTION ( 'NONE',  ( 0.000000000000000000, -0.000000000000000000, 1.000000000000000000 ) ) ;
#120267 = VECTOR ( 'NONE', #153445, 999.9999999999998863 ) ;
#120269 = CARTESIAN_POINT ( 'NONE',  ( -21.05000000000000071, 76.10000000001222986, -148.1726782920690937 ) ) ;
#120268 = AXIS2_PLACEMENT_3D ( 'NONE', #233418, #13085, #114735 ) ;
#120270 = LINE ( 'NONE', #82351, #77032 ) ;
#120271 = CARTESIAN_POINT ( 'NONE',  ( 18.49505816908823874, -9.437872553199980530, -107.2776572016709480 ) ) ;
#120272 = VECTOR ( 'NONE', #147263, 1000.000000000000000 ) ;
#120273 = ORIENTED_EDGE ( 'NONE', *, *, #50303, .F. ) ;
#120274 = LINE ( 'NONE', #220623, #110794 ) ;
#120275 = ADVANCED_FACE ( 'NONE', ( #229570 ), #42307, .T. ) ;
#120277 = ORIENTED_EDGE ( 'NONE', *, *, #83027, .F. ) ;
#120276 = FACE_OUTER_BOUND ( 'NONE', #122882, .T. ) ;
#120278 = CARTESIAN_POINT ( 'NONE',  ( 20.95539060131842746, 65.37613784235699654, -195.8693736708682422 ) ) ;
#120279 = VECTOR ( 'NONE', #245001, 1000.000000000000000 ) ;
#120280 = FACE_OUTER_BOUND ( 'NONE', #210261, .T. ) ;
#120282 = DIRECTION ( 'NONE',  ( -0.000000000000000000, 1.000000000000000000, 6.982962677686266711E-15 ) ) ;
#120281 = DIRECTION ( 'NONE',  ( 0.000000000000000000, 1.000000000000000000, 0.000000000000000000 ) ) ;
#120283 = ORIENTED_EDGE ( 'NONE', *, *, #166119, .T. ) ;
#120285 = CARTESIAN_POINT ( 'NONE',  ( -18.40000000000000213, 11.47316190336248809, -24.17405393319204876 ) ) ;
#120284 = CARTESIAN_POINT ( 'NONE',  ( -18.50000000000000711, 11.65000000001115232, -107.5148057706540357 ) ) ;
#120286 = DIRECTION ( 'NONE',  ( -1.000000000000000000, -0.000000000000000000, -0.000000000000000000 ) ) ;
#120287 = FACE_OUTER_BOUND ( 'NONE', #240459, .T. ) ;
#120288 = CARTESIAN_POINT ( 'NONE',  ( -20.94999999999999929, 1.115650877919449575E-11, -138.1000000000000227 ) ) ;
#120290 = EDGE_CURVE ( 'NONE', #214613, #85598, #109102, .T. ) ;
#120289 = CARTESIAN_POINT ( 'NONE',  ( -14.77538296656413586, 66.56333706821347107, -185.2000707522295784 ) ) ;
#120291 = ORIENTED_EDGE ( 'NONE', *, *, #165227, .T. ) ;
#120292 = DIRECTION ( 'NONE',  ( 1.000000000000000000, 0.000000000000000000, 0.000000000000000000 ) ) ;
#120293 = AXIS2_PLACEMENT_3D ( 'NONE', #181731, #244251, #46060 ) ;
#120294 = AXIS2_PLACEMENT_3D ( 'NONE', #186321, #144597, #25965 ) ;
#120295 = ORIENTED_EDGE ( 'NONE', *, *, #69756, .T. ) ;
#120296 = ADVANCED_FACE ( 'NONE', ( #69226 ), #210008, .F. ) ;
#120297 = EDGE_CURVE ( 'NONE', #101453, #159861, #25733, .T. ) ;
#120298 = DIRECTION ( 'NONE',  ( 0.000000000000000000, -0.8096735173027155286, 0.5868805631290315850 ) ) ;
#120299 = CIRCLE ( 'NONE', #207752, 0.09999999999999691080 ) ;
#120300 = EDGE_LOOP ( 'NONE', ( #204947, #124612, #251248 ) ) ;
#120301 = CARTESIAN_POINT ( 'NONE',  ( -18.50000000000000000, -9.400000000000005684, -40.41465834296965909 ) ) ;
#120302 = ORIENTED_EDGE ( 'NONE', *, *, #122800, .T. ) ;
#120303 = AXIS2_PLACEMENT_3D ( 'NONE', #82264, #142268, #121461 ) ;
#120304 = DIRECTION ( 'NONE',  ( 0.000000000000000000, 0.8814952561688446098, -0.4721928772777316263 ) ) ;
#120305 = STYLED_ITEM ( 'NONE', ( #206186 ), #22252 ) ;
#120306 = VECTOR ( 'NONE', #14313, 1000.000000000000000 ) ;
#120307 = FACE_OUTER_BOUND ( 'NONE', #98482, .T. ) ;
#120308 = EDGE_LOOP ( 'NONE', ( #168976, #202677 ) ) ;
#120309 = EDGE_CURVE ( 'NONE', #179646, #72929, #250399, .T. ) ;
#120310 = VECTOR ( 'NONE', #245523, 999.9999999999998863 ) ;
#120311 = EDGE_CURVE ( 'NONE', #121060, #177802, #167051, .T. ) ;
#120312 = DIRECTION ( 'NONE',  ( 1.000000000000000000, 0.000000000000000000, -0.000000000000000000 ) ) ;
#120313 = CARTESIAN_POINT ( 'NONE',  ( -22.60000000000080789, 75.95218301954666629, -114.7731299156770461 ) ) ;
#120314 = CYLINDRICAL_SURFACE ( 'NONE', #70017, 11.80000000000000426 ) ;
#120315 = DIRECTION ( 'NONE',  ( 0.000000000000000000, 0.000000000000000000, -1.000000000000000000 ) ) ;
#120316 = CARTESIAN_POINT ( 'NONE',  ( -23.15000000000000213, 11.75000000001115552, -45.65000000000000568 ) ) ;
#120317 = CARTESIAN_POINT ( 'NONE',  ( 22.49231231312462853, 12.57605540120662191, -223.4344661467465016 ) ) ;
#120318 = EDGE_LOOP ( 'NONE', ( #26185, #13995, #131608, #231021 ) ) ;
#120320 = CIRCLE ( 'NONE', #170207, 0.09999999999998898659 ) ;
#120319 = CYLINDRICAL_SURFACE ( 'NONE', #178475, 0.09999999999998898659 ) ;
#120321 = VECTOR ( 'NONE', #57347, 1000.000000000000000 ) ;
#120322 = ORIENTED_EDGE ( 'NONE', *, *, #54994, .T. ) ;
#120323 = VERTEX_POINT ( 'NONE', #151328 ) ;
#120324 = ORIENTED_EDGE ( 'NONE', *, *, #52031, .T. ) ;
#120325 = CARTESIAN_POINT ( 'NONE',  ( 23.14999999999999858, 76.00000000001189449, -101.0231074845243029 ) ) ;
#120326 = CIRCLE ( 'NONE', #118518, 1.749999999999999778 ) ;
#120327 = DIRECTION ( 'NONE',  ( -1.000000000000000000, -0.000000000000000000, -0.000000000000000000 ) ) ;
#120328 = LINE ( 'NONE', #77291, #59015 ) ;
#120329 = CARTESIAN_POINT ( 'NONE',  ( 21.14999999999999503, -11.64999999998883595, -69.90000000000004832 ) ) ;
#120330 = EDGE_CURVE ( 'NONE', #141624, #145447, #109598, .T. ) ;
#120331 = DIRECTION ( 'NONE',  ( 1.000000000000000000, 0.000000000000000000, 0.000000000000000000 ) ) ;
#120332 = ORIENTED_EDGE ( 'NONE', *, *, #247196, .T. ) ;
#120333 = EDGE_CURVE ( 'NONE', #190389, #34228, #42472, .T. ) ;
#120334 = ADVANCED_FACE ( 'NONE', ( #49634 ), #92365, .T. ) ;
#120335 = CARTESIAN_POINT ( 'NONE',  ( 21.05000000000000071, 77.84908441863932183, -158.3670969630772163 ) ) ;
#120336 = DIRECTION ( 'NONE',  ( 1.000000000000000000, -0.000000000000000000, 0.000000000000000000 ) ) ;
#120337 = TOROIDAL_SURFACE ( 'NONE', #7880, 11.65000000000000036, 0.1000000000000000056 ) ;
#120338 = ORIENTED_EDGE ( 'NONE', *, *, #103012, .T. ) ;
#120339 = CIRCLE ( 'NONE', #178589, 3.970710678118657189 ) ;
#120340 = DIRECTION ( 'NONE',  ( 0.000000000000000000, 0.8814952561688476074, -0.4721928772777262417 ) ) ;
#120341 = AXIS2_PLACEMENT_3D ( 'NONE', #187627, #188894, #28591 ) ;
#120342 = VERTEX_POINT ( 'NONE', #251687 ) ;
#120343 = AXIS2_PLACEMENT_3D ( 'NONE', #205119, #29124, #164737 ) ;
#120344 = CARTESIAN_POINT ( 'NONE',  ( 22.60000000000000142, 75.89914163091405896, -215.2726746080137445 ) ) ;
#120345 = ORIENTED_EDGE ( 'NONE', *, *, #235756, .T. ) ;
#120346 = DIRECTION ( 'NONE',  ( 1.000000000000000000, 0.000000000000000000, 0.000000000000000000 ) ) ;
#120347 =( BOUNDED_CURVE ( )  B_SPLINE_CURVE ( 3, ( #114133, #249809, #50300, #69909 ),
 .UNSPECIFIED., .F., .T. ) 
 B_SPLINE_CURVE_WITH_KNOTS ( ( 4, 4 ),
 ( 5.733388419619900311, 5.983100554402347449 ),
 .UNSPECIFIED. ) 
 CURVE ( )  GEOMETRIC_REPRESENTATION_ITEM ( )  RATIONAL_B_SPLINE_CURVE ( ( 1.000000000000000000, 0.9948104011409416580, 0.9948104011409416580, 1.000000000000000000 ) ) 
 REPRESENTATION_ITEM ( '' )  );
#120348 = CARTESIAN_POINT ( 'NONE',  ( 21.14999999999999858, 9.028068219309963283, -211.6732836666006961 ) ) ;
#120349 = CARTESIAN_POINT ( 'NONE',  ( 13.88638282980484107, 66.54257354752263609, -51.02306561612434876 ) ) ;
#120350 = CARTESIAN_POINT ( 'NONE',  ( -13.39999999999994529, 66.35000000001119247, -21.02310748452479316 ) ) ;
#120351 = AXIS2_PLACEMENT_3D ( 'NONE', #196853, #256782, #35263 ) ;
#120352 = AXIS2_PLACEMENT_3D ( 'NONE', #133681, #72447, #32046 ) ;
#120353 = EDGE_CURVE ( 'NONE', #129511, #3044, #63313, .T. ) ;
#120354 = AXIS2_PLACEMENT_3D ( 'NONE', #20015, #23878, #22577 ) ;
#120355 = VERTEX_POINT ( 'NONE', #211284 ) ;
#120356 = CARTESIAN_POINT ( 'NONE',  ( 18.59999999999999076, 51.96945017402672562, -231.5060697639786440 ) ) ;
#120357 = ORIENTED_EDGE ( 'NONE', *, *, #205372, .F. ) ;
#120358 = CYLINDRICAL_SURFACE ( 'NONE', #139447, 0.1000000000000028644 ) ;
#120359 = ADVANCED_FACE ( 'NONE', ( #92598, #32692 ), #112204, .T. ) ;
#120360 = CARTESIAN_POINT ( 'NONE',  ( 20.02499999999999858, 66.25000000001151079, -48.27310748452438816 ) ) ;
#120362 = VERTEX_POINT ( 'NONE', #157781 ) ;
#120361 = FACE_OUTER_BOUND ( 'NONE', #122300, .T. ) ;
#120363 = CARTESIAN_POINT ( 'NONE',  ( -18.49513951962167013, 85.43772502668979030, -129.7450349094951605 ) ) ;
#120364 = CARTESIAN_POINT ( 'NONE',  ( -18.79999999999999716, 6.841561409100513025, 9.675512259591560138 ) ) ;
#120365 = FACE_OUTER_BOUND ( 'NONE', #113173, .T. ) ;
#120366 = CARTESIAN_POINT ( 'NONE',  ( -16.79139129368504157, 9.944944162472836524, -79.67024463282588442 ) ) ;
#120367 = AXIS2_PLACEMENT_3D ( 'NONE', #21538, #643, #158496 ) ;
#120368 = EDGE_CURVE ( 'NONE', #232638, #146711, #209084, .T. ) ;
#120369 = DIRECTION ( 'NONE',  ( 0.000000000000000000, 1.000000000000000000, 0.000000000000000000 ) ) ;
#120370 = CARTESIAN_POINT ( 'NONE',  ( 18.39999999999999503, 11.47316190337363828, -146.6500000000000341 ) ) ;
#120372 = VERTEX_POINT ( 'NONE', #255488 ) ;
#120371 = DIRECTION ( 'NONE',  ( -1.000000000000000000, 0.000000000000000000, 0.000000000000000000 ) ) ;
#120373 = ADVANCED_FACE ( 'NONE', ( #97718 ), #71552, .T. ) ;
#120375 = ADVANCED_FACE ( 'NONE', ( #178604 ), #56026, .T. ) ;
#120374 = DIRECTION ( 'NONE',  ( 1.000000000000000000, 0.000000000000000000, 0.000000000000000000 ) ) ;
#120377 = ADVANCED_FACE ( 'NONE', ( #196838 ), #237271, .T. ) ;
#120376 = ORIENTED_EDGE ( 'NONE', *, *, #134920, .T. ) ;
#120378 = ORIENTED_EDGE ( 'NONE', *, *, #231421, .T. ) ;
#120379 = CARTESIAN_POINT ( 'NONE',  ( -18.59999999999999787, -1.249999999988843369, -74.80048075441509070 ) ) ;
#120380 = CARTESIAN_POINT ( 'NONE',  ( 21.07016717456946253, 69.67905916191168103, -103.0231074845243455 ) ) ;
#120381 = VERTEX_POINT ( 'NONE', #156482 ) ;
#120382 = CARTESIAN_POINT ( 'NONE',  ( -18.40000000000000213, 64.51332499825484490, -179.2731074845244450 ) ) ;
#120383 = AXIS2_PLACEMENT_3D ( 'NONE', #97459, #177056, #37532 ) ;
#120384 = AXIS2_PLACEMENT_3D ( 'NONE', #176272, #53723, #74617 ) ;
#120385 = ORIENTED_EDGE ( 'NONE', *, *, #162986, .T. ) ;
#120386 = AXIS2_PLACEMENT_3D ( 'NONE', #140113, #196251, #81411 ) ;
#120387 = VECTOR ( 'NONE', #71745, 1000.000000000000000 ) ;
#120389 = EDGE_CURVE ( 'NONE', #28807, #52494, #217242, .T. ) ;
#120388 = DIRECTION ( 'NONE',  ( 1.000000000000000000, 0.000000000000000000, 0.000000000000000000 ) ) ;
#120390 = ADVANCED_FACE ( 'NONE', ( #194313 ), #258064, .F. ) ;
#120391 = CYLINDRICAL_SURFACE ( 'NONE', #47194, 0.09999999999999939493 ) ;
#120392 = ORIENTED_EDGE ( 'NONE', *, *, #132292, .T. ) ;
#120393 = CIRCLE ( 'NONE', #116275, 0.09999999999999864553 ) ;
#120394 = VERTEX_POINT ( 'NONE', #113458 ) ;
#120395 = DIRECTION ( 'NONE',  ( 0.000000000000000000, 0.000000000000000000, -1.000000000000000000 ) ) ;
#120396 = EDGE_LOOP ( 'NONE', ( #224603, #33241, #22790, #257259 ) ) ;
#120397 = ADVANCED_FACE ( 'NONE', ( #233435 ), #121623, .F. ) ;
#120398 = FACE_OUTER_BOUND ( 'NONE', #202120, .T. ) ;
#120399 = EDGE_LOOP ( 'NONE', ( #207274, #120007, #85701, #101767, #45257, #209298 ) ) ;
#120401 = ORIENTED_EDGE ( 'NONE', *, *, #171954, .T. ) ;
#120400 = CARTESIAN_POINT ( 'NONE',  ( 18.59999999999999076, 7.120270961708750512, -137.6595630418393625 ) ) ;
#120402 = CARTESIAN_POINT ( 'NONE',  ( -14.00000000000000178, 66.15000000001185754, -86.27310748452437394 ) ) ;
#120403 = ORIENTED_EDGE ( 'NONE', *, *, #95679, .F. ) ;
#120404 = CARTESIAN_POINT ( 'NONE',  ( -21.07016717457010557, 1.116512752478288073E-11, -94.17905916189914706 ) ) ;
#120405 = VECTOR ( 'NONE', #41638, 1000.000000000000000 ) ;
#120407 = ORIENTED_EDGE ( 'NONE', *, *, #155539, .F. ) ;
#120406 = EDGE_CURVE ( 'NONE', #32328, #40297, #67420, .T. ) ;
#120409 = VERTEX_POINT ( 'NONE', #15680 ) ;
#120408 = VERTEX_POINT ( 'NONE', #152622 ) ;
#120411 = CARTESIAN_POINT ( 'NONE',  ( 21.05000000000000071, 69.55891531154095730, -136.5053880512155331 ) ) ;
#120410 = AXIS2_PLACEMENT_3D ( 'NONE', #27004, #28295, #123511 ) ;
#120412 = EDGE_CURVE ( 'NONE', #207794, #8721, #100707, .T. ) ;
#120413 = CYLINDRICAL_SURFACE ( 'NONE', #156480, 0.09999999999998898659 ) ;
#120414 = ORIENTED_EDGE ( 'NONE', *, *, #244569, .T. ) ;
#120415 = VECTOR ( 'NONE', #65611, 999.9999999999998863 ) ;
#120416 = EDGE_CURVE ( 'NONE', #115602, #9223, #96443, .T. ) ;
#120417 = VERTEX_POINT ( 'NONE', #136875 ) ;
#120418 = CARTESIAN_POINT ( 'NONE',  ( 17.23472005113827876, 42.89716137982957633, -235.4615306384476128 ) ) ;
#120419 = FACE_OUTER_BOUND ( 'NONE', #125887, .T. ) ;
#120421 = ORIENTED_EDGE ( 'NONE', *, *, #115668, .T. ) ;
#120420 = DIRECTION ( 'NONE',  ( 0.000000000000000000, 1.000000000000000000, 0.000000000000000000 ) ) ;
#120422 = FACE_OUTER_BOUND ( 'NONE', #192151, .T. ) ;
#120423 = EDGE_LOOP ( 'NONE', ( #229210, #9511, #64808, #243541 ) ) ;
#120424 = CARTESIAN_POINT ( 'NONE',  ( -20.64999999999999858, 25.94586868676353575, -241.5435999122864530 ) ) ;
#120425 = DIRECTION ( 'NONE',  ( 1.000000000000000000, 0.000000000000000000, 0.000000000000000000 ) ) ;
#120426 = EDGE_CURVE ( 'NONE', #183798, #202859, #216409, .T. ) ;
#120427 = ORIENTED_EDGE ( 'NONE', *, *, #250348, .F. ) ;
#120428 = CARTESIAN_POINT ( 'NONE',  ( -18.59999999999999787, 76.00000000001237765, -170.0231074845243597 ) ) ;
#120429 = DIRECTION ( 'NONE',  ( 0.000000000000000000, -7.116814260417660624E-15, 1.000000000000000000 ) ) ;
#120430 = CARTESIAN_POINT ( 'NONE',  ( 21.05000000000000071, 84.66355140188105111, -93.49900636645693908 ) ) ;
#120431 = ORIENTED_EDGE ( 'NONE', *, *, #93916, .T. ) ;
#120432 = CARTESIAN_POINT ( 'NONE',  ( 20.94999999999999929, 65.70729864261056719, -164.5657455973725121 ) ) ;
#120433 = VERTEX_POINT ( 'NONE', #95185 ) ;
#120434 = TOROIDAL_SURFACE ( 'NONE', #195255, 0.2000000000000000111, 0.1000000000000000056 ) ;
#120435 = VERTEX_POINT ( 'NONE', #117318 ) ;
#120436 = CIRCLE ( 'NONE', #116319, 0.09999999999999843736 ) ;
#120437 = DIRECTION ( 'NONE',  ( 0.000000000000000000, 0.2128009952263595073, -0.9770955615653317272 ) ) ;
#120438 = ORIENTED_EDGE ( 'NONE', *, *, #241465, .F. ) ;
#120439 = ORIENTED_EDGE ( 'NONE', *, *, #235228, .F. ) ;
#120440 = CARTESIAN_POINT ( 'NONE',  ( 20.94999999999999929, -3.363022478626109368, -226.2703567425896267 ) ) ;
#120441 = DIRECTION ( 'NONE',  ( 0.000000000000000000, 0.9908441862701596881, -0.1350103645451904977 ) ) ;
#120442 = ORIENTED_EDGE ( 'NONE', *, *, #69625, .T. ) ;
#120443 = CIRCLE ( 'NONE', #70551, 0.2000000000000057288 ) ;
#120444 = ORIENTED_EDGE ( 'NONE', *, *, #148042, .F. ) ;
#120445 = DIRECTION ( 'NONE',  ( -1.000000000000000000, -0.000000000000000000, 0.000000000000000000 ) ) ;
#120446 = DIRECTION ( 'NONE',  ( 0.000000000000000000, -0.000000000000000000, -1.000000000000000000 ) ) ;
#120447 = ORIENTED_EDGE ( 'NONE', *, *, #152740, .T. ) ;
#120448 = VERTEX_POINT ( 'NONE', #58605 ) ;
#120449 = CIRCLE ( 'NONE', #107938, 0.1000000000000028644 ) ;
#120450 = ORIENTED_EDGE ( 'NONE', *, *, #6187, .T. ) ;
#120451 = CIRCLE ( 'NONE', #228761, 0.1000000000000084294 ) ;
#120452 = ADVANCED_FACE ( 'NONE', ( #173496 ), #138139, .T. ) ;
#120453 = CARTESIAN_POINT ( 'NONE',  ( -16.89797118371545182, 66.02361927736747305, -82.08581411696629004 ) ) ;
#120454 = CARTESIAN_POINT ( 'NONE',  ( 21.05000000000000071, 64.58471289989986985, -237.0407535203538316 ) ) ;
#120455 = DIRECTION ( 'NONE',  ( -3.265361837132813093E-16, -1.000000000000000000, -6.982962677686266711E-15 ) ) ;
#120456 = CARTESIAN_POINT ( 'NONE',  ( -20.96428641294275153, 11.75000000001149481, -127.1748931779423089 ) ) ;
#120457 = AXIS2_PLACEMENT_3D ( 'NONE', #138419, #75911, #133319 ) ;
#120459 = VECTOR ( 'NONE', #35935, 1000.000000000000000 ) ;
#120458 = CARTESIAN_POINT ( 'NONE',  ( 21.14999999999999858, 1.363275264940682741, -230.6442496871288483 ) ) ;
#120460 = CARTESIAN_POINT ( 'NONE',  ( 20.73486653747088582, 7.250000000011182166, -121.3500000000000227 ) ) ;
#120461 = CARTESIAN_POINT ( 'NONE',  ( -16.98495255085918032, 65.99443563401784729, -190.8884902783039195 ) ) ;
#120463 = DIRECTION ( 'NONE',  ( 0.000000000000000000, 1.000000000000000000, 0.000000000000000000 ) ) ;
#120462 = DIRECTION ( 'NONE',  ( 0.000000000000000000, -0.1495327102803586661, -0.9887567792719350601 ) ) ;
#120464 = DIRECTION ( 'NONE',  ( -1.000000000000000000, 0.000000000000000000, 0.000000000000000000 ) ) ;
#120465 = CARTESIAN_POINT ( 'NONE',  ( 18.49999999999999289, 11.75000000000000355, 11.75000000000000000 ) ) ;
#120466 = DIRECTION ( 'NONE',  ( 1.000000000000000000, -0.000000000000000000, 0.000000000000000000 ) ) ;
#120467 = EDGE_CURVE ( 'NONE', #97170, #213795, #155376, .T. ) ;
#120468 = CARTESIAN_POINT ( 'NONE',  ( -18.40000000000000213, 11.75000000001113953, -180.1499999999999773 ) ) ;
#120469 = ORIENTED_EDGE ( 'NONE', *, *, #248664, .T. ) ;
#120470 = AXIS2_PLACEMENT_3D ( 'NONE', #210926, #208380, #131382 ) ;
#120471 = AXIS2_PLACEMENT_3D ( 'NONE', #77463, #157046, #95752 ) ;
#120472 = CIRCLE ( 'NONE', #237151, 12.87499999999999822 ) ;
#120474 = ORIENTED_EDGE ( 'NONE', *, *, #38892, .T. ) ;
#120473 = CYLINDRICAL_SURFACE ( 'NONE', #194902, 14.30833333333333890 ) ;
#120475 = VECTOR ( 'NONE', #254467, 1000.000000000000000 ) ;
#120476 = DIRECTION ( 'NONE',  ( 0.000000000000000000, 0.000000000000000000, 1.000000000000000000 ) ) ;
#120477 = DIRECTION ( 'NONE',  ( 0.000000000000000000, 0.01562500000001262185, 0.9998779222360095753 ) ) ;
#120478 = FILL_AREA_STYLE ('',( #237823 ) ) ;
#120479 = ORIENTED_EDGE ( 'NONE', *, *, #32657, .F. ) ;
#120480 = DIRECTION ( 'NONE',  ( 1.000000000000000000, 0.000000000000000000, 0.000000000000000000 ) ) ;
#120481 = PRODUCT_DEFINITION_SHAPE ( 'NONE', 'NONE',  #258132 ) ;
#120482 = CARTESIAN_POINT ( 'NONE',  ( 20.94999999999999929, 69.15387683765952431, -132.7853812176745407 ) ) ;
#120483 = AXIS2_PLACEMENT_3D ( 'NONE', #12505, #172887, #52876 ) ;
#120484 = ORIENTED_EDGE ( 'NONE', *, *, #134131, .F. ) ;
#120485 = CARTESIAN_POINT ( 'NONE',  ( 23.14999999999998437, 76.00000000001192291, -98.97310748452431994 ) ) ;
#120486 = FACE_OUTER_BOUND ( 'NONE', #184473, .T. ) ;
#120487 = PLANE ( 'NONE',  #192953 ) ;
#120488 = LINE ( 'NONE', #3055, #253452 ) ;
#120490 = ORIENTED_EDGE ( 'NONE', *, *, #141257, .F. ) ;
#120489 = CARTESIAN_POINT ( 'NONE',  ( -20.94788355080264353, 67.49401193140447219, -195.5283494629371432 ) ) ;
#120492 = EDGE_LOOP ( 'NONE', ( #120781, #56210, #202897, #62657 ) ) ;
#120491 = CARTESIAN_POINT ( 'NONE',  ( -18.33981767444241484, 85.56957578981651125, -96.20394564079951749 ) ) ;
#120493 = TOROIDAL_SURFACE ( 'NONE', #66315, 0.2000000000000000111, 0.1000000000000000056 ) ;
#120494 = B_SPLINE_CURVE_WITH_KNOTS ( 'NONE', 3,
 ( #173886, #254628, #214253, #94288, #133429, #51286, #175170, #153031, #171324, #35647 ),
 .UNSPECIFIED., .F., .F.,
 ( 4, 2, 2, 2, 4 ),
 ( 0.000000000000000000, 0.0001584437871624302908, 0.0002376656807436914470, 0.0002772766275343568009, 0.0003168875743250221277 ),
 .UNSPECIFIED. ) ;
#120495 = CARTESIAN_POINT ( 'NONE',  ( -23.15000000000000213, 1.115600667400684642E-11, -37.54999999999999716 ) ) ;
#120496 = FACE_OUTER_BOUND ( 'NONE', #184560, .T. ) ;
#120497 = AXIS2_PLACEMENT_3D ( 'NONE', #147260, #44327, #106840 ) ;
#120498 = CARTESIAN_POINT ( 'NONE',  ( -14.87779219673428521, 9.430633469083948839, -182.7317657948240424 ) ) ;
#120500 = DIRECTION ( 'NONE',  ( 0.000000000000000000, -0.8814952561688476074, 0.4721928772777262417 ) ) ;
#120499 = CARTESIAN_POINT ( 'NONE',  ( -18.44085059012131822, 64.48598750652799083, -78.78280216540285608 ) ) ;
#120501 = LINE ( 'NONE', #257345, #132968 ) ;
#120502 = TOROIDAL_SURFACE ( 'NONE', #149535, 11.65000000000000036, 0.1000000000000000056 ) ;
#120504 = EDGE_CURVE ( 'NONE', #231042, #74054, #122463, .T. ) ;
#120503 = CYLINDRICAL_SURFACE ( 'NONE', #86756, 0.9000000000000014655 ) ;
#120505 = CARTESIAN_POINT ( 'NONE',  ( -21.05000000000000071, 64.25000000001233502, -163.2392418215462726 ) ) ;
#120506 = FACE_OUTER_BOUND ( 'NONE', #178549, .T. ) ;
#120507 = CARTESIAN_POINT ( 'NONE',  ( 21.08078803292165659, 10.04943488157321774, -228.1127893679160650 ) ) ;
#120508 = ORIENTED_EDGE ( 'NONE', *, *, #223015, .F. ) ;
#120509 = DIRECTION ( 'NONE',  ( 1.000000000000000000, -0.000000000000000000, -0.000000000000000000 ) ) ;
#120510 = EDGE_LOOP ( 'NONE', ( #204931, #158724, #149244, #132003 ) ) ;
#120511 = ORIENTED_EDGE ( 'NONE', *, *, #98770, .T. ) ;
#120512 = ADVANCED_FACE ( 'NONE', ( #201991 ), #75808, .F. ) ;
#120513 = CARTESIAN_POINT ( 'NONE',  ( -20.00857864376270001, 66.85000000001150511, -48.27310748452438816 ) ) ;
#120514 = DIRECTION ( 'NONE',  ( 0.000000000000000000, -0.2617529984164955192, -0.9651348961777178603 ) ) ;
#120515 = ORIENTED_EDGE ( 'NONE', *, *, #79637, .T. ) ;
#120516 = EDGE_CURVE ( 'NONE', #5450, #64377, #179876, .T. ) ;
#120517 = AXIS2_PLACEMENT_3D ( 'NONE', #191464, #92316, #171901 ) ;
#120518 = EDGE_LOOP ( 'NONE', ( #162993, #23292, #212070, #146063 ) ) ;
#120519 = VECTOR ( 'NONE', #221713, 1000.000000000000227 ) ;
#120520 = PRESENTATION_STYLE_ASSIGNMENT (( #102172 ) ) ;
#120521 = EDGE_CURVE ( 'NONE', #194521, #114130, #46557, .T. ) ;
#120522 = EDGE_LOOP ( 'NONE', ( #250331, #81027, #141673, #90328 ) ) ;
#120523 = ORIENTED_EDGE ( 'NONE', *, *, #138148, .F. ) ;
#120524 = CARTESIAN_POINT ( 'NONE',  ( -21.05000000000000071, 1.115600667400684642E-11, -88.70000000000004547 ) ) ;
#120525 = CARTESIAN_POINT ( 'NONE',  ( -22.00411653889209518, 0.09903810578596834724, 7.253442867640404579 ) ) ;
#120526 = LINE ( 'NONE', #142605, #76072 ) ;
#120527 = CARTESIAN_POINT ( 'NONE',  ( 20.94999999999999929, 60.99662849158838895, -205.1669373764474642 ) ) ;
#120528 = DIRECTION ( 'NONE',  ( 0.000000000000000000, -6.982962677686266711E-15, 1.000000000000000000 ) ) ;
#120529 = DIRECTION ( 'NONE',  ( 0.000000000000000000, 0.8814952561688476074, -0.4721928772777262417 ) ) ;
#120530 = CARTESIAN_POINT ( 'NONE',  ( -20.94999999999999929, 76.00000000001190870, -103.0231074845243029 ) ) ;
#120532 = VERTEX_POINT ( 'NONE', #203267 ) ;
#120531 = CARTESIAN_POINT ( 'NONE',  ( 23.24999999999999645, 4.999999999999997335, -12.40526601891309788 ) ) ;
#120534 = DIRECTION ( 'NONE',  ( 1.000000000000000000, 0.000000000000000000, -0.000000000000000000 ) ) ;
#120533 = CARTESIAN_POINT ( 'NONE',  ( -18.41431012584568094, 62.49790673650496586, -209.4212991392053311 ) ) ;
#120535 = ADVANCED_FACE ( 'NONE', ( #121204 ), #241137, .T. ) ;
#120536 = DIRECTION ( 'NONE',  ( 0.000000000000000000, -1.000000000000000000, 0.000000000000000000 ) ) ;
#120537 = ORIENTED_EDGE ( 'NONE', *, *, #38698, .F. ) ;
#120538 =( LENGTH_UNIT ( ) NAMED_UNIT ( * ) SI_UNIT ( .MILLI., .METRE. ) );
#120539 = ORIENTED_EDGE ( 'NONE', *, *, #55452, .F. ) ;
#120541 = CARTESIAN_POINT ( 'NONE',  ( -33.72168855820451938, 63.08573235307422777, -213.1276215869287398 ) ) ;
#120540 = FACE_OUTER_BOUND ( 'NONE', #109497, .T. ) ;
#120542 = CARTESIAN_POINT ( 'NONE',  ( -18.50000000000000000, 85.40000000001187175, -96.14106563635156988 ) ) ;
#120543 = CARTESIAN_POINT ( 'NONE',  ( 22.48660254037844197, 64.35000000001164722, -69.57310748452439952 ) ) ;
#120544 = ORIENTED_EDGE ( 'NONE', *, *, #52346, .T. ) ;
#120545 = CARTESIAN_POINT ( 'NONE',  ( -21.65000000000000213, 68.75000000001161027, -60.27310748452437394 ) ) ;
#120546 = DIRECTION ( 'NONE',  ( 1.000000000000000000, 0.000000000000000000, -0.000000000000000000 ) ) ;
#120547 = CARTESIAN_POINT ( 'NONE',  ( -22.60000000000094289, 0.1008583691096561485, -21.75043287651059387 ) ) ;
#120548 = LINE ( 'NONE', #56658, #257396 ) ;
#120549 = ORIENTED_EDGE ( 'NONE', *, *, #240139, .T. ) ;
#120550 = EDGE_CURVE ( 'NONE', #27581, #100505, #254808, .T. ) ;
#120551 = CARTESIAN_POINT ( 'NONE',  ( -1.739115166359751801E-14, 64.35000000001252829, -178.6731074845244507 ) ) ;
#120552 = AXIS2_PLACEMENT_3D ( 'NONE', #197542, #127008, #26646 ) ;
#120553 = LINE ( 'NONE', #215762, #257477 ) ;
#120555 = DIRECTION ( 'NONE',  ( 1.000000000000000000, -2.824170522722115425E-14, 2.841386468225606068E-14 ) ) ;
#120554 = CIRCLE ( 'NONE', #49794, 0.5000000000000004441 ) ;
#120556 = CIRCLE ( 'NONE', #191300, 2.000000000000003109 ) ;
#120557 = CIRCLE ( 'NONE', #249716, 11.74999999999999645 ) ;
#120558 = DIRECTION ( 'NONE',  ( 0.000000000000000000, 0.8814952561688418342, -0.4721928772777368444 ) ) ;
#120559 = DIRECTION ( 'NONE',  ( 0.000000000000000000, 0.000000000000000000, 1.000000000000000000 ) ) ;
#120560 = ADVANCED_FACE ( 'NONE', ( #63754 ), #224106, .F. ) ;
#120562 = ORIENTED_EDGE ( 'NONE', *, *, #171310, .T. ) ;
#120561 = DIRECTION ( 'NONE',  ( 0.000000000000000000, -0.4721928772777346239, -0.8814952561688430555 ) ) ;
#120563 = CIRCLE ( 'NONE', #66385, 0.1000000000000054040 ) ;
#120564 = DIRECTION ( 'NONE',  ( 0.000000000000000000, -1.000000000000000000, 0.000000000000000000 ) ) ;
#120565 = DIRECTION ( 'NONE',  ( -1.000000000000000000, 0.000000000000000000, 0.000000000000000000 ) ) ;
#120566 = DIRECTION ( 'NONE',  ( 0.000000000000000000, 0.000000000000000000, -1.000000000000000000 ) ) ;
#120567 = CARTESIAN_POINT ( 'NONE',  ( 21.05000000000084626, 10.60832956796496696, -175.0916850132954323 ) ) ;
#120569 = VERTEX_POINT ( 'NONE', #101566 ) ;
#120568 = DIRECTION ( 'NONE',  ( 0.000000000000000000, -1.000000000000000000, 0.000000000000000000 ) ) ;
#120570 = CARTESIAN_POINT ( 'NONE',  ( -20.64999999999999858, -9.399999999988846611, -191.1060308773475356 ) ) ;
#120571 = CARTESIAN_POINT ( 'NONE',  ( -23.25000000000000000, 28.42524210734032053, -258.3567845160494585 ) ) ;
#120572 = CARTESIAN_POINT ( 'NONE',  ( 20.91682497891423154, 67.49276774653023381, -195.4544018784149841 ) ) ;
#120573 = EDGE_CURVE ( 'NONE', #60123, #231379, #59013, .T. ) ;
#120574 = ORIENTED_EDGE ( 'NONE', *, *, #36357, .F. ) ;
#120575 = CARTESIAN_POINT ( 'NONE',  ( -18.50000000000000000, 76.00000000001213607, -136.5231074845243313 ) ) ;
#120576 = DIRECTION ( 'NONE',  ( 1.000000000000000000, 0.000000000000000000, 0.000000000000000000 ) ) ;
#120577 = AXIS2_PLACEMENT_3D ( 'NONE', #55577, #98546, #176873 ) ;
#120578 = SPHERICAL_SURFACE ( 'NONE', #25276, 0.1000000000000000056 ) ;
#120579 = AXIS2_PLACEMENT_3D ( 'NONE', #153386, #109067, #33435 ) ;
#120580 = EDGE_CURVE ( 'NONE', #278, #180772, #163299, .T. ) ;
#120581 = DIRECTION ( 'NONE',  ( 1.000000000000000000, 0.000000000000000000, 0.000000000000000000 ) ) ;
#120582 = FACE_OUTER_BOUND ( 'NONE', #66218, .T. ) ;
#120583 = VECTOR ( 'NONE', #223099, 1000.000000000000114 ) ;
#120584 = VERTEX_POINT ( 'NONE', #181157 ) ;
#120585 = ORIENTED_EDGE ( 'NONE', *, *, #90867, .F. ) ;
#120586 = LINE ( 'NONE', #115418, #189077 ) ;
#120587 = DIRECTION ( 'NONE',  ( 0.000000000000000000, 7.056502275159894776E-15, -1.000000000000000000 ) ) ;
#120588 = EDGE_CURVE ( 'NONE', #55457, #85029, #129942, .T. ) ;
#120589 = CARTESIAN_POINT ( 'NONE',  ( 21.05000000000000071, 63.43511439055885148, -224.4466865888566360 ) ) ;
#120590 = EDGE_LOOP ( 'NONE', ( #50426, #25322 ) ) ;
#120591 = CARTESIAN_POINT ( 'NONE',  ( 20.95052659398289308, 10.47982436779105875, -175.0752387558655698 ) ) ;
#120592 = ADVANCED_FACE ( 'NONE', ( #184995 ), #24667, .T. ) ;
#120594 = EDGE_CURVE ( 'NONE', #20729, #128969, #199445, .T. ) ;
#120593 = CARTESIAN_POINT ( 'NONE',  ( 20.72390388899165714, 11.94582835298777468, -206.0857503901398786 ) ) ;
#120595 = CARTESIAN_POINT ( 'NONE',  ( -20.64999999999999858, 85.00000000001179501, -79.01707660717669057 ) ) ;
#120596 = CARTESIAN_POINT ( 'NONE',  ( 23.14999999999999503, 64.35000000001201670, -114.7731074845243882 ) ) ;
#120598 = CARTESIAN_POINT ( 'NONE',  ( -16.89935556175703368, 9.949999999999985079, -20.36032363711476734 ) ) ;
#120597 = AXIS2_PLACEMENT_3D ( 'NONE', #7723, #224179, #85929 ) ;
#120599 = ORIENTED_EDGE ( 'NONE', *, *, #104933, .F. ) ;
#120601 = ORIENTED_EDGE ( 'NONE', *, *, #103117, .F. ) ;
#120600 = CARTESIAN_POINT ( 'NONE',  ( 21.05000000000000071, 1.115600667400684642E-11, -167.5000000000000284 ) ) ;
#120602 = ADVANCED_FACE ( 'NONE', ( #62488 ), #142005, .F. ) ;
#120603 = ORIENTED_EDGE ( 'NONE', *, *, #47339, .T. ) ;
#120604 = CARTESIAN_POINT ( 'NONE',  ( 23.24999999999999645, 11.75000000001113953, -176.7499999999999716 ) ) ;
#120605 = VERTEX_POINT ( 'NONE', #100293 ) ;
#120606 = CARTESIAN_POINT ( 'NONE',  ( -21.05000000000000071, 0.09843750001115432469, -27.20076908991313047 ) ) ;
#120607 = DIRECTION ( 'NONE',  ( 0.000000000000000000, 0.2128009952263605342, -0.9770955615653315052 ) ) ;
#120608 = DIRECTION ( 'NONE',  ( 0.000000000000000000, -0.1350103645451945777, 0.9908441862701590219 ) ) ;
#120609 = TOROIDAL_SURFACE ( 'NONE', #170713, 12.77499999999999858, 0.1000000000000000056 ) ;
#120610 = EDGE_LOOP ( 'NONE', ( #29763, #189819, #82475, #245650, #182817 ) ) ;
#120611 = EDGE_CURVE ( 'NONE', #219486, #130620, #5043, .T. ) ;
#120612 = EDGE_CURVE ( 'NONE', #101165, #89005, #184124, .T. ) ;
#120613 = CARTESIAN_POINT ( 'NONE',  ( -23.25000000000000000, 64.65966496992309942, -200.4475097531309586 ) ) ;
#120614 = CARTESIAN_POINT ( 'NONE',  ( -21.10000000000000142, -11.64999999999999858, 11.89999999999999680 ) ) ;
#120615 = ORIENTED_EDGE ( 'NONE', *, *, #118285, .T. ) ;
#120616 = CARTESIAN_POINT ( 'NONE',  ( -16.89268316805465986, 9.951721813253337601, -54.35575247854554704 ) ) ;
#120618 = ORIENTED_EDGE ( 'NONE', *, *, #228975, .F. ) ;
#120617 = CARTESIAN_POINT ( 'NONE',  ( -21.14999999999999858, 12.82677665681128687, -205.1493534351658354 ) ) ;
#120619 = CARTESIAN_POINT ( 'NONE',  ( -18.50000000000000000, 66.85000000001222986, -148.8731074845244393 ) ) ;
#120620 = DIRECTION ( 'NONE',  ( -1.000000000000000000, -1.387778780781454006E-13, 0.000000000000000000 ) ) ;
#120621 = VECTOR ( 'NONE', #58653, 1000.000000000000000 ) ;
#120622 = AXIS2_PLACEMENT_3D ( 'NONE', #32764, #247911, #112279 ) ;
#120623 = ORIENTED_EDGE ( 'NONE', *, *, #78124, .F. ) ;
#120624 = LINE ( 'NONE', #257481, #68521 ) ;
#120625 = DIRECTION ( 'NONE',  ( 0.000000000000000000, -6.467318590049456648E-15, 1.000000000000000000 ) ) ;
#120626 = CARTESIAN_POINT ( 'NONE',  ( -18.39999999999999858, 11.47316190337362762, -143.3259460668079726 ) ) ;
#120627 = ORIENTED_EDGE ( 'NONE', *, *, #149898, .T. ) ;
#120628 = CARTESIAN_POINT ( 'NONE',  ( 21.05000000000000071, 5.849999999999949019, -10.13249722427797117 ) ) ;
#120629 = EDGE_CURVE ( 'NONE', #68492, #59785, #5221, .T. ) ;
#120630 = ADVANCED_FACE ( 'NONE', ( #32375 ), #205838, .F. ) ;
#120631 = LINE ( 'NONE', #3207, #109896 ) ;
#120632 = DIRECTION ( 'NONE',  ( 1.000000000000000000, 3.265361837132813093E-16, -0.000000000000000000 ) ) ;
#120633 = CIRCLE ( 'NONE', #145539, 0.09999999999999749367 ) ;
#120634 = AXIS2_PLACEMENT_3D ( 'NONE', #20532, #100011, #179605 ) ;
#120635 = ORIENTED_EDGE ( 'NONE', *, *, #186719, .T. ) ;
#120636 = ADVANCED_FACE ( 'NONE', ( #46751 ), #230547, .T. ) ;
#120637 = AXIS2_PLACEMENT_3D ( 'NONE', #52808, #210612, #91945 ) ;
#120638 = AXIS2_PLACEMENT_3D ( 'NONE', #141733, #221259, #143002 ) ;
#120639 = AXIS2_PLACEMENT_3D ( 'NONE', #192031, #246830, #32979 ) ;
#120640 = VERTEX_POINT ( 'NONE', #130142 ) ;
#120641 = AXIS2_PLACEMENT_3D ( 'NONE', #94785, #137747, #59473 ) ;
#120642 = CIRCLE ( 'NONE', #133106, 0.09999999999999939493 ) ;
#120643 = ORIENTED_EDGE ( 'NONE', *, *, #87834, .F. ) ;
#120644 = CARTESIAN_POINT ( 'NONE',  ( -16.87786941232800686, 9.958154714156124854, -87.87718579979406286 ) ) ;
#120645 = AXIS2_PLACEMENT_3D ( 'NONE', #86759, #62092, #161195 ) ;
#120646 = CARTESIAN_POINT ( 'NONE',  ( 21.08804582317324616, 8.878166167103060502, -45.84999982940517071 ) ) ;
#120648 = ORIENTED_EDGE ( 'NONE', *, *, #160574, .F. ) ;
#120647 = CARTESIAN_POINT ( 'NONE',  ( 12.25000000000000000, 26.10747769360537873, -233.2920644364425300 ) ) ;
#120649 = CARTESIAN_POINT ( 'NONE',  ( 21.05000000000000071, 11.75000000001115907, -127.1583993101029790 ) ) ;
#120650 = DIRECTION ( 'NONE',  ( -1.000000000000000000, 2.952720810173289112E-16, 2.061873921506763405E-30 ) ) ;
#120651 = DIRECTION ( 'NONE',  ( -0.000000000000000000, -6.982962677686266711E-15, 1.000000000000000000 ) ) ;
#120652 = CARTESIAN_POINT ( 'NONE',  ( 23.14999999999999858, 0.000000000000000000, -33.50000000000000000 ) ) ;
#120653 = CARTESIAN_POINT ( 'NONE',  ( -18.49499033040906326, 85.43814877175674383, -129.3249542586007976 ) ) ;
#120654 = ADVANCED_FACE ( 'NONE', ( #209693 ), #111889, .T. ) ;
#120655 = DIRECTION ( 'NONE',  ( -0.000000000000000000, 1.000000000000000000, -0.000000000000000000 ) ) ;
#120657 = ORIENTED_EDGE ( 'NONE', *, *, #239482, .F. ) ;
#120656 = CARTESIAN_POINT ( 'NONE',  ( 23.25000000000000000, -8.999999999988844479, -43.39396912265245021 ) ) ;
#120659 = ORIENTED_EDGE ( 'NONE', *, *, #255995, .T. ) ;
#120658 = DIRECTION ( 'NONE',  ( 0.000000000000000000, -1.000000000000000000, -0.000000000000000000 ) ) ;
#120660 = CARTESIAN_POINT ( 'NONE',  ( -16.92570016628984675, 60.92319296112430749, -221.0677532620695160 ) ) ;
#120661 = VERTEX_POINT ( 'NONE', #87158 ) ;
#120662 = ADVANCED_FACE ( 'NONE', ( #49329 ), #88432, .F. ) ;
#120663 = EDGE_LOOP ( 'NONE', ( #39073, #73299, #167531, #109686 ) ) ;
#120664 = DIRECTION ( 'NONE',  ( 1.000000000000000000, 0.000000000000000000, 0.000000000000000000 ) ) ;
#120665 = AXIS2_PLACEMENT_3D ( 'NONE', #123991, #88673, #44456 ) ;
#120666 = FACE_OUTER_BOUND ( 'NONE', #144615, .T. ) ;
#120667 = DIRECTION ( 'NONE',  ( 0.000000000000000000, 0.000000000000000000, -1.000000000000000000 ) ) ;
#120668 = DIRECTION ( 'NONE',  ( -0.000000000000000000, 0.8660254037844424824, 0.4999999999999934497 ) ) ;
#120669 = ADVANCED_FACE ( 'NONE', ( #85856 ), #188407, .T. ) ;
#120670 = CARTESIAN_POINT ( 'NONE',  ( 23.25000000000000000, 69.16514130714681130, -247.7543978865853660 ) ) ;
#120671 = CARTESIAN_POINT ( 'NONE',  ( 22.47071067811865319, 65.11488425470513164, -243.2801022963548405 ) ) ;
#120672 = EDGE_CURVE ( 'NONE', #165976, #141132, #128882, .T. ) ;
#120673 = AXIS2_PLACEMENT_3D ( 'NONE', #214936, #234493, #157578 ) ;
#120674 = DIRECTION ( 'NONE',  ( -0.000000000000000000, 6.982962677686266711E-15, -1.000000000000000000 ) ) ;
#120675 = ORIENTED_EDGE ( 'NONE', *, *, #156473, .F. ) ;
#120676 = ORIENTED_EDGE ( 'NONE', *, *, #219485, .T. ) ;
#120677 = EDGE_CURVE ( 'NONE', #188830, #111286, #50595, .T. ) ;
#120678 = CARTESIAN_POINT ( 'NONE',  ( 21.05000000000005400, 64.35000000001120668, -5.923107484524795296 ) ) ;
#120679 = CIRCLE ( 'NONE', #108194, 4.049999999999998046 ) ;
#120680 = ORIENTED_EDGE ( 'NONE', *, *, #186557, .F. ) ;
#120681 = CYLINDRICAL_SURFACE ( 'NONE', #72124, 1.749999999999999778 ) ;
#120682 = CARTESIAN_POINT ( 'NONE',  ( 18.50016250449482413, 68.01715840423111104, -224.2192812407674580 ) ) ;
#120683 = VECTOR ( 'NONE', #183996, 1000.000000000000000 ) ;
#120685 = EDGE_CURVE ( 'NONE', #70872, #9918, #151009, .T. ) ;
#120684 = DIRECTION ( 'NONE',  ( 0.000000000000000000, 0.000000000000000000, -1.000000000000000000 ) ) ;
#120687 = ADVANCED_FACE ( 'NONE', ( #226675 ), #159214, .F. ) ;
#120686 = EDGE_CURVE ( 'NONE', #86183, #30145, #250934, .T. ) ;
#120688 = DIRECTION ( 'NONE',  ( -1.000000000000000000, 0.000000000000000000, 0.000000000000000000 ) ) ;
#120689 = ORIENTED_EDGE ( 'NONE', *, *, #50571, .F. ) ;
#120690 = CARTESIAN_POINT ( 'NONE',  ( -20.94999999999999929, 67.23127455305835554, -235.8551265064784559 ) ) ;
#120691 = VERTEX_POINT ( 'NONE', #68920 ) ;
#120692 = CARTESIAN_POINT ( 'NONE',  ( -18.59999999999999787, 62.42744096235649920, -225.1319887738535499 ) ) ;
#120693 = ORIENTED_EDGE ( 'NONE', *, *, #183670, .F. ) ;
#120694 = LINE ( 'NONE', #101043, #189943 ) ;
#120695 = AXIS2_PLACEMENT_3D ( 'NONE', #79335, #57197, #101433 ) ;
#120696 = CARTESIAN_POINT ( 'NONE',  ( -21.14999999999999858, 44.06843597547145208, -258.9974126733344519 ) ) ;
#120697 = ORIENTED_EDGE ( 'NONE', *, *, #22946, .T. ) ;
#120698 = CARTESIAN_POINT ( 'NONE',  ( 18.54999999999999716, 41.52322060116084401, -237.7841060310786077 ) ) ;
#120700 = VERTEX_POINT ( 'NONE', #170624 ) ;
#120699 = CARTESIAN_POINT ( 'NONE',  ( 21.05000000000000071, 67.23127455305835554, -235.8551265064784559 ) ) ;
#120701 = ADVANCED_FACE ( 'NONE', ( #187586 ), #234181, .F. ) ;
#120702 = CARTESIAN_POINT ( 'NONE',  ( 20.94999999999999929, 38.43293829866423295, -234.5626268121764895 ) ) ;
#120704 = EDGE_CURVE ( 'NONE', #129546, #223130, #42659, .T. ) ;
#120703 = TOROIDAL_SURFACE ( 'NONE', #3969, 0.6000000000000013101, 0.1000000000000000056 ) ;
#120705 = ORIENTED_EDGE ( 'NONE', *, *, #60257, .F. ) ;
#120706 = EDGE_CURVE ( 'NONE', #166775, #209272, #10223, .T. ) ;
#120707 = EDGE_LOOP ( 'NONE', ( #117951, #60828, #51854, #48550 ) ) ;
#120708 = CARTESIAN_POINT ( 'NONE',  ( -21.05000000000000071, 74.75000000001189449, -95.02310748452431710 ) ) ;
#120709 = LINE ( 'NONE', #138919, #117933 ) ;
#120711 = EDGE_CURVE ( 'NONE', #217161, #257895, #248830, .T. ) ;
#120710 = DIRECTION ( 'NONE',  ( 1.000000000000000000, 0.000000000000000000, 0.000000000000000000 ) ) ;
#120712 = CARTESIAN_POINT ( 'NONE',  ( -18.59999999999999787, -1.135018845899022466, -74.71697688343232358 ) ) ;
#120713 = CARTESIAN_POINT ( 'NONE',  ( -13.22483237240080101, 66.56332574816974557, -188.3462455535252218 ) ) ;
#120714 = EDGE_CURVE ( 'NONE', #168971, #74036, #180047, .T. ) ;
#120715 = ORIENTED_EDGE ( 'NONE', *, *, #223332, .T. ) ;
#120716 = LINE ( 'NONE', #43721, #161090 ) ;
#120717 = B_SPLINE_CURVE_WITH_KNOTS ( 'NONE', 3,
 ( #101806, #219207, #4018, #5275, #84806, #121438 ),
 .UNSPECIFIED., .F., .F.,
 ( 4, 2, 4 ),
 ( 0.000000000000000000, 0.0001895189928937367218, 0.0003790379857874734437 ),
 .UNSPECIFIED. ) ;
#120718 = AXIS2_PLACEMENT_3D ( 'NONE', #11265, #9974, #208192 ) ;
#120719 = FACE_OUTER_BOUND ( 'NONE', #155332, .T. ) ;
#120720 = VECTOR ( 'NONE', #245416, 1000.000000000000000 ) ;
#120721 = ORIENTED_EDGE ( 'NONE', *, *, #122278, .T. ) ;
#120722 = CARTESIAN_POINT ( 'NONE',  ( 18.49999999999998934, 10.29288807859941457, -105.9580020160122018 ) ) ;
#120723 = VERTEX_POINT ( 'NONE', #210981 ) ;
#120724 = DIRECTION ( 'NONE',  ( 0.000000000000000000, 0.2128009952263602012, -0.9770955615653315052 ) ) ;
#120725 = ORIENTED_EDGE ( 'NONE', *, *, #180645, .T. ) ;
#120726 = CARTESIAN_POINT ( 'NONE',  ( 18.59999999999998721, 69.15387683765983695, -166.2853812176745691 ) ) ;
#120727 = CARTESIAN_POINT ( 'NONE',  ( -17.22767730082141213, 65.65075578754381525, -181.3806787939495848 ) ) ;
#120728 = EDGE_LOOP ( 'NONE', ( #90635, #193520, #178260, #232854 ) ) ;
#120729 = B_SPLINE_CURVE_WITH_KNOTS ( 'NONE', 3,
 ( #249237, #108434, #105837, #69321, #146262, #70622, #185401, #228390, #229668, #49738, #225785, #31495, #111001 ),
 .UNSPECIFIED., .F., .F.,
 ( 4, 3, 3, 3, 4 ),
 ( -3.224855718284247652E-06, 4.235164736271501695E-22, 6.199515528661409170E-06, 4.034952380126323066E-05, 7.452715123697944196E-05 ),
 .UNSPECIFIED. ) ;
#120731 = ORIENTED_EDGE ( 'NONE', *, *, #54954, .T. ) ;
#120730 = DIRECTION ( 'NONE',  ( 0.000000000000000000, 1.000000000000000000, 0.000000000000000000 ) ) ;
#120732 = ADVANCED_FACE ( 'NONE', ( #74065 ), #92301, .T. ) ;
#120733 = CARTESIAN_POINT ( 'NONE',  ( 22.60000000000000142, 64.25043287652275126, -136.6239658536230763 ) ) ;
#120734 = EDGE_LOOP ( 'NONE', ( #238119, #161297, #65225, #77366 ) ) ;
#120735 = EDGE_CURVE ( 'NONE', #178254, #50042, #138315, .T. ) ;
#120736 = DIRECTION ( 'NONE',  ( 1.000000000000000000, -0.000000000000000000, -0.000000000000000000 ) ) ;
#120737 = CYLINDRICAL_SURFACE ( 'NONE', #93618, 0.09999999999999868716 ) ;
#120738 = ORIENTED_EDGE ( 'NONE', *, *, #222631, .F. ) ;
#120740 = VERTEX_POINT ( 'NONE', #76589 ) ;
#120739 = EDGE_CURVE ( 'NONE', #148838, #93175, #58293, .T. ) ;
#120741 = CIRCLE ( 'NONE', #74950, 0.5000000000000023315 ) ;
#120743 = AXIS2_PLACEMENT_3D ( 'NONE', #13661, #174062, #73663 ) ;
#120742 = CARTESIAN_POINT ( 'NONE',  ( -21.14999999999999503, 11.75000000001115197, -174.4191472459587544 ) ) ;
#120744 = CYLINDRICAL_SURFACE ( 'NONE', #156852, 0.1000000000000028644 ) ;
#120745 = ORIENTED_EDGE ( 'NONE', *, *, #112051, .T. ) ;
#120746 = CIRCLE ( 'NONE', #149787, 0.09999999999999939493 ) ;
#120748 = CARTESIAN_POINT ( 'NONE',  ( -16.87368910959167678, 66.03872618332066224, -123.9106143878837827 ) ) ;
#120747 = TOROIDAL_SURFACE ( 'NONE', #4188, 0.2000000000000000111, 0.1000000000000000056 ) ;
#120749 = EDGE_LOOP ( 'NONE', ( #176780, #36307, #10630, #153632 ) ) ;
#120750 = ORIENTED_EDGE ( 'NONE', *, *, #78739, .T. ) ;
#120751 = VECTOR ( 'NONE', #226685, 1000.000000000000000 ) ;
#120752 = FACE_OUTER_BOUND ( 'NONE', #86814, .T. ) ;
#120753 = EDGE_CURVE ( 'NONE', #252932, #26421, #71906, .T. ) ;
#120755 = EDGE_LOOP ( 'NONE', ( #88435, #149630, #13540, #160518, #17172 ) ) ;
#120754 = CARTESIAN_POINT ( 'NONE',  ( -16.85939591225058720, 9.905226478399001167, -46.46006824646904931 ) ) ;
#120756 = LINE ( 'NONE', #183271, #228327 ) ;
#120757 = AXIS2_PLACEMENT_3D ( 'NONE', #139083, #218639, #200383 ) ;
#120758 = DIRECTION ( 'NONE',  ( 0.000000000000000000, 1.000000000000000000, 0.000000000000000000 ) ) ;
#120759 = CARTESIAN_POINT ( 'NONE',  ( 21.00000000000000000, 6.841561409100513025, 9.675512259591560138 ) ) ;
#120760 = AXIS2_PLACEMENT_3D ( 'NONE', #202734, #7099, #204018 ) ;
#120762 = CARTESIAN_POINT ( 'NONE',  ( -21.45000000000000284, 68.29142135624910281, -81.77310748452435973 ) ) ;
#120761 = CARTESIAN_POINT ( 'NONE',  ( -16.93255653858138388, 66.00154854603471222, -90.44146411653470352 ) ) ;
#120763 = DIRECTION ( 'NONE',  ( 0.000000000000000000, 0.008583690987128220901, 0.9999631594459055250 ) ) ;
#120764 = CARTESIAN_POINT ( 'NONE',  ( 21.14999999999999503, 4.136903274969363942, -245.4596299165286268 ) ) ;
#120765 = DIRECTION ( 'NONE',  ( -1.000000000000000000, 0.000000000000000000, 0.000000000000000000 ) ) ;
#120766 = ADVANCED_FACE ( 'NONE', ( #152315 ), #246638, .T. ) ;
#120767 = FACE_OUTER_BOUND ( 'NONE', #84807, .T. ) ;
#120768 = AXIS2_PLACEMENT_3D ( 'NONE', #122103, #162528, #222445 ) ;
#120769 = ORIENTED_EDGE ( 'NONE', *, *, #141937, .F. ) ;
#120770 = ORIENTED_EDGE ( 'NONE', *, *, #176310, .T. ) ;
#120771 = ORIENTED_EDGE ( 'NONE', *, *, #53787, .F. ) ;
#120772 = DIRECTION ( 'NONE',  ( 1.000000000000000000, 0.000000000000000000, 0.000000000000000000 ) ) ;
#120773 = ORIENTED_EDGE ( 'NONE', *, *, #91834, .T. ) ;
#120774 = DIRECTION ( 'NONE',  ( 0.000000000000000000, 0.000000000000000000, 1.000000000000000000 ) ) ;
#120775 = ORIENTED_EDGE ( 'NONE', *, *, #250769, .T. ) ;
#120776 =( LENGTH_UNIT ( ) NAMED_UNIT ( * ) SI_UNIT ( .MILLI., .METRE. ) );
#120777 = DIRECTION ( 'NONE',  ( 0.000000000000000000, 0.9126074666063804797, 0.4088369013363203908 ) ) ;
#120778 = AXIS2_PLACEMENT_3D ( 'NONE', #257814, #196604, #60941 ) ;
#120780 = ORIENTED_EDGE ( 'NONE', *, *, #200680, .T. ) ;
#120779 = ORIENTED_EDGE ( 'NONE', *, *, #120467, .T. ) ;
#120781 = ORIENTED_EDGE ( 'NONE', *, *, #71196, .T. ) ;
#120782 = ORIENTED_EDGE ( 'NONE', *, *, #94519, .F. ) ;
#120783 = LINE ( 'NONE', #222386, #150469 ) ;
#120784 = DIRECTION ( 'NONE',  ( 1.000000000000000000, -0.000000000000000000, -0.000000000000000000 ) ) ;
#120786 = VERTEX_POINT ( 'NONE', #36209 ) ;
#120785 = CARTESIAN_POINT ( 'NONE',  ( 21.00000000000000000, 9.750000000011153745, -188.6499999999999488 ) ) ;
#120787 = AXIS2_PLACEMENT_3D ( 'NONE', #135543, #97686, #16910 ) ;
#120788 = CARTESIAN_POINT ( 'NONE',  ( 20.22894356738407851, 40.41144770130940600, -237.7030586605688711 ) ) ;
#120789 = DIRECTION ( 'NONE',  ( 0.000000000000000000, 0.000000000000000000, -1.000000000000000000 ) ) ;
#120791 = ORIENTED_EDGE ( 'NONE', *, *, #229568, .F. ) ;
#120790 = CARTESIAN_POINT ( 'NONE',  ( 20.95556889135987788, 10.62194358774625336, -141.6423942218575291 ) ) ;
#120792 = CARTESIAN_POINT ( 'NONE',  ( 19.99999999738043144, 11.75000000001116263, -125.1871719496315905 ) ) ;
#120793 = VERTEX_POINT ( 'NONE', #33675 ) ;
#120794 = CIRCLE ( 'NONE', #124869, 0.2000000000000057288 ) ;
#120796 = ORIENTED_EDGE ( 'NONE', *, *, #24146, .T. ) ;
#120795 = DIRECTION ( 'NONE',  ( 1.000000000000000000, 0.000000000000000000, 0.000000000000000000 ) ) ;
#120797 = DIRECTION ( 'NONE',  ( 0.000000000000000000, -0.2617529984165031243, -0.9651348961777157509 ) ) ;
#120798 = CARTESIAN_POINT ( 'NONE',  ( -23.15000000000000213, 64.25000000001145395, -39.12310748452440379 ) ) ;
#120799 = EDGE_CURVE ( 'NONE', #33205, #181057, #56029, .T. ) ;
#120800 = DIRECTION ( 'NONE',  ( 0.000000000000000000, 0.000000000000000000, -1.000000000000000000 ) ) ;
#120801 = EDGE_LOOP ( 'NONE', ( #177944, #230086, #180710, #234823 ) ) ;
#120803 = CARTESIAN_POINT ( 'NONE',  ( -21.06715728752538652, 64.25000000001190870, -96.00830171387038092 ) ) ;
#120802 = CARTESIAN_POINT ( 'NONE',  ( 23.14999999999999147, 63.22596473392088967, -234.7688515630498785 ) ) ;
#120804 = CARTESIAN_POINT ( 'NONE',  ( 20.85000000000000142, 36.65892442174935439, -249.5511627012433848 ) ) ;
#120805 = CIRCLE ( 'NONE', #45945, 7.800000000000001599 ) ;
#120806 = CARTESIAN_POINT ( 'NONE',  ( 21.30000000000002558, 1.115650265596050101E-11, -37.54999999999999716 ) ) ;
#120807 = CARTESIAN_POINT ( 'NONE',  ( 23.14999999999999858, -2.100000000000002309, -33.50000000000000000 ) ) ;
#120808 = CARTESIAN_POINT ( 'NONE',  ( -21.05000000000000071, 77.25000000001232081, -162.0231074845243313 ) ) ;
#120809 = CIRCLE ( 'NONE', #249960, 12.87499999999999822 ) ;
#120810 = ORIENTED_EDGE ( 'NONE', *, *, #72261, .T. ) ;
#120811 = EDGE_LOOP ( 'NONE', ( #215953, #122213, #111468, #105996 ) ) ;
#120812 = ORIENTED_EDGE ( 'NONE', *, *, #58053, .F. ) ;
#120813 = DIRECTION ( 'NONE',  ( 1.000000000000000000, 0.000000000000000000, 0.000000000000000000 ) ) ;
#120814 = ORIENTED_EDGE ( 'NONE', *, *, #151538, .F. ) ;
#120816 = DIRECTION ( 'NONE',  ( -1.000000000000000000, -0.000000000000000000, 0.000000000000000000 ) ) ;
#120815 = AXIS2_PLACEMENT_3D ( 'NONE', #44827, #103492, #183065 ) ;
#120817 = VERTEX_POINT ( 'NONE', #114443 ) ;
#120818 = EDGE_CURVE ( 'NONE', #201773, #70810, #25933, .T. ) ;
#120819 = DIRECTION ( 'NONE',  ( -1.000000000000000000, -0.000000000000000000, -0.000000000000000000 ) ) ;
#120820 = CARTESIAN_POINT ( 'NONE',  ( -21.07016717457010557, 76.00000000001243450, -176.3440483226252411 ) ) ;
#120821 = CIRCLE ( 'NONE', #29262, 0.1000000000000028644 ) ;
#120822 = AXIS2_PLACEMENT_3D ( 'NONE', #256845, #177399, #78252 ) ;
#120823 = EDGE_CURVE ( 'NONE', #229414, #10431, #77864, .T. ) ;
#120824 = ORIENTED_EDGE ( 'NONE', *, *, #58873, .F. ) ;
#120825 = CARTESIAN_POINT ( 'NONE',  ( 18.39999999999999858, 37.94390843806124991, -261.1300795796834109 ) ) ;
#120826 = ADVANCED_FACE ( 'NONE', ( #38762 ), #195290, .T. ) ;
#120827 = B_SPLINE_CURVE_WITH_KNOTS ( 'NONE', 3,
 ( #30229, #109733, #15481, #77985, #234496, #237076, #55834, #214940 ),
 .UNSPECIFIED., .F., .F.,
 ( 4, 2, 2, 4 ),
 ( 0.000000000000000000, 0.0001094981963948513511, 0.0002189963927897027021, 0.0004379927855794011216 ),
 .UNSPECIFIED. ) ;
#120828 = EDGE_LOOP ( 'NONE', ( #30337, #201936, #51804, #95369, #223052 ) ) ;
#120829 = ORIENTED_EDGE ( 'NONE', *, *, #3999, .F. ) ;
#120830 = CIRCLE ( 'NONE', #245699, 0.5000000000000004441 ) ;
#120831 = VECTOR ( 'NONE', #187872, 1000.000000000000000 ) ;
#120832 = ORIENTED_EDGE ( 'NONE', *, *, #79950, .F. ) ;
#120833 = AXIS2_PLACEMENT_3D ( 'NONE', #10794, #169913, #249412 ) ;
#120834 = AXIS2_PLACEMENT_3D ( 'NONE', #35227, #155174, #194294 ) ;
#120835 = ADVANCED_FACE ( 'NONE', ( #236955 ), #75995, .F. ) ;
#120836 = DIRECTION ( 'NONE',  ( -1.000000000000000000, 0.000000000000000000, -0.000000000000000000 ) ) ;
#120837 = CARTESIAN_POINT ( 'NONE',  ( -22.39999999999999858, 1.115600667400684642E-11, -55.35042919245524473 ) ) ;
#120838 = DIRECTION ( 'NONE',  ( 0.000000000000000000, -1.000000000000000000, -6.352154140967427193E-15 ) ) ;
#120840 = ADVANCED_FACE ( 'NONE', ( #60872 ), #180840, .T. ) ;
#120839 = DIRECTION ( 'NONE',  ( -0.000000000000000000, -6.982962677686266711E-15, 1.000000000000000000 ) ) ;
#120841 = DIRECTION ( 'NONE',  ( 1.284012543211123464E-15, 0.1480365673253023762, -0.9889818879709281196 ) ) ;
#120842 = DIRECTION ( 'NONE',  ( 0.000000000000000000, -1.000000000000000000, 0.000000000000000000 ) ) ;
#120843 = AXIS2_PLACEMENT_3D ( 'NONE', #242975, #42225, #219551 ) ;
#120845 = DIRECTION ( 'NONE',  ( 1.000000000000000000, 0.000000000000000000, 0.000000000000000000 ) ) ;
#120844 = CARTESIAN_POINT ( 'NONE',  ( 21.04999999999999716, -0.01759718699757174473, -161.0592291063375967 ) ) ;
#120846 = CARTESIAN_POINT ( 'NONE',  ( -16.89268316805466341, 9.951721813253341153, -46.14424752145445296 ) ) ;
#120848 = VERTEX_POINT ( 'NONE', #99975 ) ;
#120847 = DIRECTION ( 'NONE',  ( 1.000000000000000000, 0.000000000000000000, 0.000000000000000000 ) ) ;
#120849 = CARTESIAN_POINT ( 'NONE',  ( 21.09813707148777340, 69.61493789427544243, -103.0544589840538663 ) ) ;
#120850 = EDGE_CURVE ( 'NONE', #196680, #45647, #197817, .T. ) ;
#120851 = DIRECTION ( 'NONE',  ( -1.000000000000000000, -0.000000000000000000, -0.000000000000000000 ) ) ;
#120852 = ORIENTED_EDGE ( 'NONE', *, *, #19339, .T. ) ;
#120853 = VERTEX_POINT ( 'NONE', #179569 ) ;
#120854 = CARTESIAN_POINT ( 'NONE',  ( 23.24999999999997513, 62.82351852614503684, -207.2177435922979214 ) ) ;
#120855 = DIRECTION ( 'NONE',  ( 0.000000000000000000, 0.000000000000000000, 1.000000000000000000 ) ) ;
#120856 = DIRECTION ( 'NONE',  ( -0.7071067811865473507, -0.3338907855510733769, -0.6233112732207618523 ) ) ;
#120857 = ORIENTED_EDGE ( 'NONE', *, *, #54484, .F. ) ;
#120858 = ADVANCED_FACE ( 'NONE', ( #877 ), #109291, .T. ) ;
#120859 = CARTESIAN_POINT ( 'NONE',  ( 20.85000000000000142, 1.115600667400684642E-11, -141.9000000000000341 ) ) ;
#120860 = ORIENTED_EDGE ( 'NONE', *, *, #134171, .F. ) ;
#120861 = ORIENTED_EDGE ( 'NONE', *, *, #49561, .F. ) ;
#120862 = CARTESIAN_POINT ( 'NONE',  ( -16.92570016628984675, 9.958788957739859171, -12.62065067003899088 ) ) ;
#120863 = EDGE_LOOP ( 'NONE', ( #100476, #19127, #97957, #177716 ) ) ;
#120864 = CARTESIAN_POINT ( 'NONE',  ( -16.93255653858138388, 60.87470302366463670, -221.0950187931682649 ) ) ;
#120865 = LINE ( 'NONE', #178269, #227774 ) ;
#120866 = CARTESIAN_POINT ( 'NONE',  ( -21.05000000000000071, 74.16465844978745281, -91.36795619196134055 ) ) ;
#120867 = DIRECTION ( 'NONE',  ( 1.000000000000000000, 0.000000000000000000, 0.000000000000000000 ) ) ;
#120868 = CARTESIAN_POINT ( 'NONE',  ( -18.59999999999999787, 11.75000000001115552, -100.5000000000000426 ) ) ;
#120869 = ORIENTED_EDGE ( 'NONE', *, *, #94315, .T. ) ;
#120870 = VECTOR ( 'NONE', #22543, 1000.000000000000000 ) ;
#120871 = EDGE_CURVE ( 'NONE', #203964, #169815, #13462, .T. ) ;
#120872 = DIRECTION ( 'NONE',  ( 0.000000000000000000, 0.000000000000000000, -1.000000000000000000 ) ) ;
#120873 = DIRECTION ( 'NONE',  ( 0.000000000000000000, -0.8700118002898359348, 0.4930308989875165082 ) ) ;
#120874 = AXIS2_PLACEMENT_3D ( 'NONE', #72951, #76758, #190310 ) ;
#120875 = CYLINDRICAL_SURFACE ( 'NONE', #61547, 0.1000000000000028644 ) ;
#120876 = CIRCLE ( 'NONE', #8420, 0.1000000000000065836 ) ;
#120877 = EDGE_LOOP ( 'NONE', ( #192316, #141628, #109889, #102421 ) ) ;
#120878 = EDGE_CURVE ( 'NONE', #244178, #179546, #80037, .T. ) ;
#120880 = ORIENTED_EDGE ( 'NONE', *, *, #45433, .T. ) ;
#120879 = DIRECTION ( 'NONE',  ( 1.000000000000000000, 0.000000000000000000, 0.000000000000000000 ) ) ;
#120881 = DIRECTION ( 'NONE',  ( 1.000000000000000000, 0.000000000000000000, 0.000000000000000000 ) ) ;
#120882 = CARTESIAN_POINT ( 'NONE',  ( -20.85000000000000142, 77.83585931145546510, -91.51866831572576189 ) ) ;
#120883 = CARTESIAN_POINT ( 'NONE',  ( -20.94999999999999929, 87.48912529308779540, -72.42310748452423752 ) ) ;
#120884 = DIRECTION ( 'NONE',  ( 0.000000000000000000, -7.056502275159890832E-15, 1.000000000000000000 ) ) ;
#120885 = LINE ( 'NONE', #99972, #225734 ) ;
#120886 = FACE_OUTER_BOUND ( 'NONE', #208076, .T. ) ;
#120887 = AXIS2_PLACEMENT_3D ( 'NONE', #9593, #147848, #65726 ) ;
#120888 = ORIENTED_EDGE ( 'NONE', *, *, #213307, .T. ) ;
#120889 = DIRECTION ( 'NONE',  ( 0.000000000000000000, 1.224646799147358384E-16, 1.000000000000000000 ) ) ;
#120890 = VECTOR ( 'NONE', #150877, 1000.000000000000000 ) ;
#120891 = CARTESIAN_POINT ( 'NONE',  ( -16.79814274880124358, 9.949272542688458287, -146.6524330370480413 ) ) ;
#120892 = DIRECTION ( 'NONE',  ( 0.000000000000000000, 0.2617529984165152257, 0.9651348961777124202 ) ) ;
#120893 = CARTESIAN_POINT ( 'NONE',  ( 21.07094088545304089, 6.320167221927651013, -133.9011062974477966 ) ) ;
#120895 = AXIS2_PLACEMENT_3D ( 'NONE', #240107, #161870, #41924 ) ;
#120894 = DIRECTION ( 'NONE',  ( 1.000000000000000000, 0.000000000000000000, 0.000000000000000000 ) ) ;
#120896 = CARTESIAN_POINT ( 'NONE',  ( 20.13684514580103624, 66.50414460725895083, -61.38007579883958442 ) ) ;
#120897 = EDGE_CURVE ( 'NONE', #236113, #44305, #46755, .T. ) ;
#120898 = CIRCLE ( 'NONE', #175081, 0.09999999999999553690 ) ;
#120899 = ORIENTED_EDGE ( 'NONE', *, *, #185009, .F. ) ;
#120900 = EDGE_LOOP ( 'NONE', ( #46664, #105621, #155330, #222871, #129108 ) ) ;
#120901 = LINE ( 'NONE', #82986, #279 ) ;
#120902 = SPHERICAL_SURFACE ( 'NONE', #155221, 0.1000000000000000056 ) ;
#120903 = CARTESIAN_POINT ( 'NONE',  ( 20.94560253601876809, 17.12224500340141731, -224.4024732428971731 ) ) ;
#120904 = EDGE_CURVE ( 'NONE', #126428, #178010, #80465, .T. ) ;
#120905 = ORIENTED_EDGE ( 'NONE', *, *, #120014, .T. ) ;
#120906 = FACE_OUTER_BOUND ( 'NONE', #34699, .T. ) ;
#120907 = EDGE_CURVE ( 'NONE', #104329, #205524, #239529, .T. ) ;
#120909 = ADVANCED_FACE ( 'NONE', ( #158734 ), #78328, .T. ) ;
#120908 = DIRECTION ( 'NONE',  ( 1.000000000000000000, 0.000000000000000000, 0.000000000000000000 ) ) ;
#120910 = AXIS2_PLACEMENT_3D ( 'NONE', #161175, #217266, #179469 ) ;
#120911 = AXIS2_PLACEMENT_3D ( 'NONE', #46882, #163017, #220417 ) ;
#120912 = CARTESIAN_POINT ( 'NONE',  ( -21.05000000000000071, 11.65000000001115232, -140.7838656629781724 ) ) ;
#120913 = EDGE_CURVE ( 'NONE', #194507, #240371, #125853, .T. ) ;
#120914 = ORIENTED_EDGE ( 'NONE', *, *, #194663, .T. ) ;
#120915 = DIRECTION ( 'NONE',  ( -0.7071067811865463515, 0.7071067811865487940, 4.178957128135655137E-15 ) ) ;
#120916 = ADVANCED_FACE ( 'NONE', ( #182123 ), #142598, .F. ) ;
#120917 = ORIENTED_EDGE ( 'NONE', *, *, #186509, .T. ) ;
#120918 = DIRECTION ( 'NONE',  ( 0.000000000000000000, 0.2128009952263678062, -0.9770955615653298398 ) ) ;
#120919 = CARTESIAN_POINT ( 'NONE',  ( 21.04999999999999716, 69.50331341424582376, -170.0084513660146683 ) ) ;
#120920 = DIRECTION ( 'NONE',  ( 0.000000000000000000, 0.2128009952263603399, -0.9770955615653315052 ) ) ;
#120921 = CARTESIAN_POINT ( 'NONE',  ( 18.59117750673696179, 65.66751761918648356, -63.92826094061123143 ) ) ;
#120922 = DIRECTION ( 'NONE',  ( 0.000000000000000000, 0.000000000000000000, -1.000000000000000000 ) ) ;
#120923 = LINE ( 'NONE', #200431, #164434 ) ;
#120924 = FACE_OUTER_BOUND ( 'NONE', #169168, .T. ) ;
#120925 = DIRECTION ( 'NONE',  ( 0.000000000000000000, -0.9770955615653551529, -0.2128009952262517601 ) ) ;
#120926 = DIRECTION ( 'NONE',  ( 0.000000000000000000, -6.982962677686266711E-15, 1.000000000000000000 ) ) ;
#120927 = VECTOR ( 'NONE', #84301, 1000.000000000000000 ) ;
#120928 = CARTESIAN_POINT ( 'NONE',  ( 23.14999999999999858, 67.92720994251783395, -214.1870976236629929 ) ) ;
#120929 = VECTOR ( 'NONE', #236255, 1000.000000000000000 ) ;
#120930 = DIRECTION ( 'NONE',  ( 0.000000000000000000, 0.000000000000000000, 1.000000000000000000 ) ) ;
#120932 = CARTESIAN_POINT ( 'NONE',  ( 23.25000000000000000, -11.74999999998883560, -122.2500000000000284 ) ) ;
#120931 = TOROIDAL_SURFACE ( 'NONE', #179193, 12.77499999999999858, 0.1000000000000000056 ) ;
#120933 = AXIS2_PLACEMENT_3D ( 'NONE', #49947, #68239, #166088 ) ;
#120934 = DIRECTION ( 'NONE',  ( 0.000000000000000000, 0.9126074666063768159, 0.4088369013363282178 ) ) ;
#120935 = DIRECTION ( 'NONE',  ( 0.000000000000000000, -0.6728971962617102953, 0.7397360091702507301 ) ) ;
#120936 = EDGE_CURVE ( 'NONE', #84905, #51335, #34330, .T. ) ;
#120937 = CIRCLE ( 'NONE', #16873, 0.1000000000000028644 ) ;
#120938 = ORIENTED_EDGE ( 'NONE', *, *, #166481, .T. ) ;
#120939 = CARTESIAN_POINT ( 'NONE',  ( 20.94999999999999929, 76.00000000001237765, -170.0231074845243597 ) ) ;
#120940 = CARTESIAN_POINT ( 'NONE',  ( 21.05000000000000071, 1.115600667400684642E-11, -104.6000000000000512 ) ) ;
#120941 = EDGE_CURVE ( 'NONE', #73222, #195640, #30210, .T. ) ;
#120942 = EDGE_CURVE ( 'NONE', #226810, #79078, #221500, .T. ) ;
#120943 = EDGE_LOOP ( 'NONE', ( #55977, #182824, #20972, #30053 ) ) ;
#120944 = DIRECTION ( 'NONE',  ( 0.000000000000000000, 2.081668171172181135E-13, -1.000000000000000000 ) ) ;
#120945 = AXIS2_PLACEMENT_3D ( 'NONE', #108362, #249164, #168377 ) ;
#120947 = AXIS2_PLACEMENT_3D ( 'NONE', #29407, #209279, #7218 ) ;
#120946 = LINE ( 'NONE', #183464, #101466 ) ;
#120948 = ORIENTED_EDGE ( 'NONE', *, *, #196, .F. ) ;
#120949 = CARTESIAN_POINT ( 'NONE',  ( -16.86337532320261090, 9.979967204235514089, -188.4489244689827956 ) ) ;
#120950 = DIRECTION ( 'NONE',  ( 1.000000000000000000, 0.000000000000000000, -0.000000000000000000 ) ) ;
#120951 = VERTEX_POINT ( 'NONE', #227649 ) ;
#120952 = ORIENTED_EDGE ( 'NONE', *, *, #187380, .T. ) ;
#120953 =( BOUNDED_SURFACE ( )  B_SPLINE_SURFACE ( 3, 2, ( 
 ( #13158, #92679, #251757 ),
 ( #210079, #133103, #233503 ),
 ( #31464, #54824, #213912 ),
 ( #110965, #35321, #114816 ) ),
 .UNSPECIFIED., .F., .F., .F. ) 
 B_SPLINE_SURFACE_WITH_KNOTS ( ( 4, 4 ),
 ( 3, 3 ),
 ( 0.0002700421466196751283, 0.0004789321604330810467 ),
 ( 0.000000000000000000, 1.000000000000000000 ),
 .UNSPECIFIED. ) 
 GEOMETRIC_REPRESENTATION_ITEM ( )  RATIONAL_B_SPLINE_SURFACE ( (
 ( 1.000000000000000000, 0.7071067811865475727, 1.000000000000000000),
 ( 1.000000000000000000, 0.7163411249511765222, 1.000000000000000000),
 ( 1.000000000000000000, 0.7221957104841898456, 1.000000000000000000),
 ( 1.000000000000000000, 0.7250110520819876836, 1.000000000000000000) ) ) 
 REPRESENTATION_ITEM ( '' )  SURFACE ( )  );
#120954 = ORIENTED_EDGE ( 'NONE', *, *, #80500, .T. ) ;
#120955 = CARTESIAN_POINT ( 'NONE',  ( 21.05000000000000071, 0.03201369318779723888, 6.258842723537621389 ) ) ;
#120956 = DIRECTION ( 'NONE',  ( -1.000000000000000000, -7.304098846218163263E-16, 4.217023435051627211E-16 ) ) ;
#120958 = CARTESIAN_POINT ( 'NONE',  ( 21.09316766718127667, 34.01873860631857838, -243.7537655525922276 ) ) ;
#120957 = UNCERTAINTY_MEASURE_WITH_UNIT (LENGTH_MEASURE( 1.000000000000000082E-05 ), #180467, 'distance_accuracy_value', 'NONE');
#120959 = CARTESIAN_POINT ( 'NONE',  ( -21.65000000000000213, 11.52084357182974195, -219.8296352432475942 ) ) ;
#120960 = SPHERICAL_SURFACE ( 'NONE', #151643, 0.1000000000000000056 ) ;
#120961 = EDGE_CURVE ( 'NONE', #56891, #251948, #167590, .T. ) ;
#120962 = CARTESIAN_POINT ( 'NONE',  ( -20.64999999999999858, -3.444512620907437039, -226.2123967847655592 ) ) ;
#120963 = DIRECTION ( 'NONE',  ( 0.000000000000000000, -0.000000000000000000, -1.000000000000000000 ) ) ;
#120964 = CARTESIAN_POINT ( 'NONE',  ( 21.07094088545369104, 1.604332817732096572, -230.6611890373810638 ) ) ;
#120966 = EDGE_LOOP ( 'NONE', ( #126907, #171387, #22554, #30512, #253849, #78310, #224801, #88251, #114933, #221790, #124150 ) ) ;
#120965 = CARTESIAN_POINT ( 'NONE',  ( 21.14999999999999858, 6.540656951712400691, -33.60000000000000142 ) ) ;
#120967 = VERTEX_POINT ( 'NONE', #124716 ) ;
#120969 = DIRECTION ( 'NONE',  ( 0.000000000000000000, -1.000000000000000000, 0.000000000000000000 ) ) ;
#120968 = CARTESIAN_POINT ( 'NONE',  ( -20.94999999999999929, -11.48912529306489994, -131.1000000000000227 ) ) ;
#120971 = ORIENTED_EDGE ( 'NONE', *, *, #137954, .F. ) ;
#120970 = CARTESIAN_POINT ( 'NONE',  ( -16.79270642812307557, 60.94587935087318442, -221.0320299440186318 ) ) ;
#120972 = AXIS2_PLACEMENT_3D ( 'NONE', #63195, #3221, #162337 ) ;
#120973 = ADVANCED_FACE ( 'NONE', ( #9888 ), #169014, .T. ) ;
#120974 = VERTEX_POINT ( 'NONE', #228951 ) ;
#120975 = LINE ( 'NONE', #19279, #208132 ) ;
#120976 = CARTESIAN_POINT ( 'NONE',  ( -21.64999999999999858, 14.23543104469003673, -219.1360829004572395 ) ) ;
#120977 = DIRECTION ( 'NONE',  ( 1.000000000000000000, 0.000000000000000000, 0.000000000000000000 ) ) ;
#120978 = DIRECTION ( 'NONE',  ( 0.000000000000000000, 0.000000000000000000, 1.000000000000000000 ) ) ;
#120979 = CIRCLE ( 'NONE', #241747, 0.1000000000000065836 ) ;
#120980 = DIRECTION ( 'NONE',  ( 0.000000000000000000, -8.881784197001272834E-15, 1.000000000000000000 ) ) ;
#120981 = EDGE_CURVE ( 'NONE', #224623, #975, #17701, .T. ) ;
#120982 = LINE ( 'NONE', #139203, #12460 ) ;
#120983 = LINE ( 'NONE', #964, #244565 ) ;
#120984 = EDGE_CURVE ( 'NONE', #183920, #211645, #125984, .T. ) ;
#120985 = DIRECTION ( 'NONE',  ( 1.000000000000000000, 0.000000000000000000, 0.000000000000000000 ) ) ;
#120986 = ORIENTED_EDGE ( 'NONE', *, *, #71494, .T. ) ;
#120987 = ORIENTED_EDGE ( 'NONE', *, *, #194627, .T. ) ;
#120988 = EDGE_CURVE ( 'NONE', #201532, #97383, #92722, .T. ) ;
#120989 = DIRECTION ( 'NONE',  ( 0.000000000000000000, -0.8814952561688429444, 0.4721928772777345684 ) ) ;
#120990 = CIRCLE ( 'NONE', #241755, 11.70000000000000284 ) ;
#120991 = EDGE_LOOP ( 'NONE', ( #244369, #31906, #126199, #239064 ) ) ;
#120992 = CARTESIAN_POINT ( 'NONE',  ( 21.05000000000000071, 1.115486826172573664E-11, -26.95934304829875572 ) ) ;
#120994 = ORIENTED_EDGE ( 'NONE', *, *, #45632, .T. ) ;
#120993 = CIRCLE ( 'NONE', #91750, 4.000000000000003553 ) ;
#120995 = CARTESIAN_POINT ( 'NONE',  ( -20.94999999999999929, 68.49522935589659767, -224.1230159437372436 ) ) ;
#120996 = ADVANCED_FACE ( 'NONE', ( #110269 ), #184672, .F. ) ;
#120997 = EDGE_CURVE ( 'NONE', #251640, #41250, #85540, .T. ) ;
#120998 = AXIS2_PLACEMENT_3D ( 'NONE', #90049, #125344, #87479 ) ;
#120999 = DIRECTION ( 'NONE',  ( 0.000000000000000000, 6.982962677686266711E-15, -1.000000000000000000 ) ) ;
#121000 = DIRECTION ( 'NONE',  ( 0.000000000000000000, 0.8814952561688428334, -0.4721928772777349570 ) ) ;
#121001 = DIRECTION ( 'NONE',  ( 0.000000000000000000, 0.9126074666063771490, 0.4088369013363281623 ) ) ;
#121002 = CARTESIAN_POINT ( 'NONE',  ( -21.05000000000000071, 1.115600667400684642E-11, -138.2999999999999829 ) ) ;
#121003 = VERTEX_POINT ( 'NONE', #149429 ) ;
#121004 = CIRCLE ( 'NONE', #71107, 0.09999999999999459321 ) ;
#121006 = AXIS2_PLACEMENT_3D ( 'NONE', #32449, #231916, #132813 ) ;
#121005 = CARTESIAN_POINT ( 'NONE',  ( -20.54999999999999361, 64.35000000001254250, -182.1731074845244507 ) ) ;
#121007 = ORIENTED_EDGE ( 'NONE', *, *, #96677, .T. ) ;
#121008 = CARTESIAN_POINT ( 'NONE',  ( 22.43288208788031568, 0.004899854896538679595, -122.3503481562809441 ) ) ;
#121009 = PLANE ( 'NONE',  #114568 ) ;
#121010 = CARTESIAN_POINT ( 'NONE',  ( -23.15000000000000213, 11.65000000001115588, -67.00000000000004263 ) ) ;
#121011 = DIRECTION ( 'NONE',  ( 0.000000000000000000, -1.000000000000000000, -6.982962677686265922E-15 ) ) ;
#121012 = VERTEX_POINT ( 'NONE', #106402 ) ;
#121013 = CARTESIAN_POINT ( 'NONE',  ( -20.97625342178413277, 64.39999999919203333, -96.09490425472216657 ) ) ;
#121014 = EDGE_LOOP ( 'NONE', ( #21414, #138794, #104028, #29324 ) ) ;
#121017 = ORIENTED_EDGE ( 'NONE', *, *, #102570, .F. ) ;
#121016 = CARTESIAN_POINT ( 'NONE',  ( 21.04999999999999716, 6.304455821958818262, -67.02103547654014903 ) ) ;
#121015 = CARTESIAN_POINT ( 'NONE',  ( 18.50000000000000355, 47.11985028124983899, -255.1884644111641194 ) ) ;
#121018 = ADVANCED_FACE ( 'NONE', ( #89421 ), #130319, .F. ) ;
#121019 = DIRECTION ( 'NONE',  ( 2.827886303505249259E-16, -0.8660254037844411501, -0.4999999999999956701 ) ) ;
#121021 = ADVANCED_FACE ( 'NONE', ( #66017 ), #185966, .T. ) ;
#121020 = CIRCLE ( 'NONE', #41908, 0.09999999999999108213 ) ;
#121022 = AXIS2_PLACEMENT_3D ( 'NONE', #175700, #255154, #34927 ) ;
#121023 = CIRCLE ( 'NONE', #4456, 0.1000000000000043771 ) ;
#121024 = DIRECTION ( 'NONE',  ( 0.000000000000000000, 0.000000000000000000, -1.000000000000000000 ) ) ;
#121025 = ORIENTED_EDGE ( 'NONE', *, *, #10517, .F. ) ;
#121026 = DIRECTION ( 'NONE',  ( 0.000000000000000000, 1.000000000000000000, 6.982962677686266711E-15 ) ) ;
#121027 = CARTESIAN_POINT ( 'NONE',  ( -16.81744102076748959, 30.20632856012693424, -234.8070450048000737 ) ) ;
#121028 = CYLINDRICAL_SURFACE ( 'NONE', #209334, 0.1000000000000002554 ) ;
#121030 = ORIENTED_EDGE ( 'NONE', *, *, #130205, .F. ) ;
#121029 = DIRECTION ( 'NONE',  ( 1.000000000000000000, 2.952720810173289112E-16, -0.000000000000000000 ) ) ;
#121031 = FACE_OUTER_BOUND ( 'NONE', #75610, .T. ) ;
#121032 = EDGE_CURVE ( 'NONE', #227071, #109970, #196957, .T. ) ;
#121033 = CIRCLE ( 'NONE', #179292, 0.09999999999998898659 ) ;
#121034 = EDGE_LOOP ( 'NONE', ( #247926, #32065, #31162, #84345 ) ) ;
#121036 = EDGE_CURVE ( 'NONE', #104140, #137094, #159396, .T. ) ;
#121035 = SPHERICAL_SURFACE ( 'NONE', #24450, 0.1000000000000000056 ) ;
#121037 = DIRECTION ( 'NONE',  ( -4.336808689942053235E-15, -0.8660254037844482555, -0.4999999999999836797 ) ) ;
#121038 = CARTESIAN_POINT ( 'NONE',  ( -18.40904629823842953, -9.499999999988851584, -140.6001895624823135 ) ) ;
#121039 = ORIENTED_EDGE ( 'NONE', *, *, #129744, .T. ) ;
#121040 = FACE_OUTER_BOUND ( 'NONE', #88456, .T. ) ;
#121041 = VERTEX_POINT ( 'NONE', #68594 ) ;
#121042 = DIRECTION ( 'NONE',  ( 0.000000000000000000, 0.000000000000000000, 1.000000000000000000 ) ) ;
#121043 = CARTESIAN_POINT ( 'NONE',  ( -0.8999999999999986899, -12.25000000000000355, 26.00000000000000355 ) ) ;
#121044 = DIRECTION ( 'NONE',  ( 0.000000000000000000, 0.000000000000000000, -1.000000000000000000 ) ) ;
#121045 = EDGE_LOOP ( 'NONE', ( #44382, #221073 ) ) ;
#121046 = EDGE_CURVE ( 'NONE', #250592, #31642, #192706, .T. ) ;
#121047 = DIRECTION ( 'NONE',  ( 1.000000000000000000, -0.000000000000000000, -0.000000000000000000 ) ) ;
#121048 = VECTOR ( 'NONE', #116213, 1000.000000000000000 ) ;
#121049 = DIRECTION ( 'NONE',  ( 0.000000000000000000, 0.2617529984165039569, 0.9651348961777155289 ) ) ;
#121050 = CARTESIAN_POINT ( 'NONE',  ( -21.05315837477644436, 64.25000000001249134, -176.8647514783578742 ) ) ;
#121051 = AXIS2_PLACEMENT_3D ( 'NONE', #106575, #107875, #226517 ) ;
#121052 = EDGE_LOOP ( 'NONE', ( #27699, #96079, #55895, #157842 ) ) ;
#121053 = EDGE_CURVE ( 'NONE', #21362, #55330, #165122, .T. ) ;
#121054 = CARTESIAN_POINT ( 'NONE',  ( 20.94999999999999929, -1.835341550213257733, -145.5551512925629822 ) ) ;
#121055 = DIRECTION ( 'NONE',  ( 0.000000000000000000, 0.8814952561688428334, -0.4721928772777350125 ) ) ;
#121056 = ORIENTED_EDGE ( 'NONE', *, *, #209129, .F. ) ;
#121057 = DIRECTION ( 'NONE',  ( 1.000000000000000000, 0.000000000000000000, 0.000000000000000000 ) ) ;
#121058 = AXIS2_PLACEMENT_3D ( 'NONE', #170602, #128866, #70191 ) ;
#121059 = ORIENTED_EDGE ( 'NONE', *, *, #132589, .T. ) ;
#121060 = VERTEX_POINT ( 'NONE', #167716 ) ;
#121061 =( BOUNDED_SURFACE ( )  B_SPLINE_SURFACE ( 3, 2, ( 
 ( #232788, #171543, #168987 ),
 ( #54119, #208093, #34587 ),
 ( #213189, #251027, #167688 ),
 ( #247185, #68568, #128535 ) ),
 .UNSPECIFIED., .F., .F., .F. ) 
 B_SPLINE_SURFACE_WITH_KNOTS ( ( 4, 4 ),
 ( 3, 3 ),
 ( 5.727910411845712702, 5.983100554402349225 ),
 ( 0.000000000000000000, 1.000000000000000000 ),
 .UNSPECIFIED. ) 
 GEOMETRIC_REPRESENTATION_ITEM ( )  RATIONAL_B_SPLINE_SURFACE ( (
 ( 1.000000000000000000, 0.8946697475932141597, 1.000000000000000000),
 ( 1.000000000000000000, 0.9035312726220726676, 1.000000000000000000),
 ( 1.000000000000000000, 0.9104333467450284045, 1.000000000000000000),
 ( 1.000000000000000000, 0.9152888060719485130, 1.000000000000000000) ) ) 
 REPRESENTATION_ITEM ( '' )  SURFACE ( )  );
#121063 = CARTESIAN_POINT ( 'NONE',  ( 22.47071067811865319, 0.09909245471376171288, -159.7799252555019223 ) ) ;
#121062 = CIRCLE ( 'NONE', #162738, 0.1000000000000028644 ) ;
#121064 = VERTEX_POINT ( 'NONE', #29498 ) ;
#121066 = VERTEX_POINT ( 'NONE', #108983 ) ;
#121065 = LINE ( 'NONE', #44062, #113880 ) ;
#121067 = EDGE_CURVE ( 'NONE', #213820, #149564, #154577, .T. ) ;
#121070 = ORIENTED_EDGE ( 'NONE', *, *, #235639, .F. ) ;
#121069 = ORIENTED_EDGE ( 'NONE', *, *, #207716, .F. ) ;
#121068 = CYLINDRICAL_SURFACE ( 'NONE', #234511, 0.5000000000000004441 ) ;
#121071 = AXIS2_PLACEMENT_3D ( 'NONE', #176265, #254456, #36765 ) ;
#121072 = LINE ( 'NONE', #160192, #195405 ) ;
#121073 = CARTESIAN_POINT ( 'NONE',  ( -21.14999999999999858, 87.65000000001214175, -136.5231074845242176 ) ) ;
#121075 = LINE ( 'NONE', #182316, #91925 ) ;
#121074 = CARTESIAN_POINT ( 'NONE',  ( 20.91682497891422798, 46.43483777265581836, -243.0774829958280918 ) ) ;
#121076 = DIRECTION ( 'NONE',  ( -1.000000000000000000, -0.000000000000000000, -0.000000000000000000 ) ) ;
#121077 = AXIS2_PLACEMENT_3D ( 'NONE', #4046, #83557, #163144 ) ;
#121078 = CARTESIAN_POINT ( 'NONE',  ( -16.94389599338512298, 44.07998477742863486, -235.2786503815312074 ) ) ;
#121079 = VECTOR ( 'NONE', #180774, 1000.000000000000000 ) ;
#121080 = CARTESIAN_POINT ( 'NONE',  ( 20.04142135623730070, 64.35000000001198828, -115.1731074845243796 ) ) ;
#121082 = CARTESIAN_POINT ( 'NONE',  ( -23.15000000000000213, 71.65000000001259650, -191.3731074845243825 ) ) ;
#121081 = DIRECTION ( 'NONE',  ( -1.000000000000000000, -9.012599976027990443E-15, -6.882867235861669241E-14 ) ) ;
#121084 = VERTEX_POINT ( 'NONE', #111569 ) ;
#121083 = AXIS2_PLACEMENT_3D ( 'NONE', #150878, #15240, #92183 ) ;
#121085 = EDGE_LOOP ( 'NONE', ( #229738, #46362, #130226, #244735 ) ) ;
#121086 = CARTESIAN_POINT ( 'NONE',  ( -18.59999999999999787, 1.261786168576181755, -75.08649896354552311 ) ) ;
#121088 = ORIENTED_EDGE ( 'NONE', *, *, #34948, .T. ) ;
#121087 = DIRECTION ( 'NONE',  ( -1.836970198721029934E-16, -1.000000000000000000, -6.982962677686266711E-15 ) ) ;
#121089 = CARTESIAN_POINT ( 'NONE',  ( 20.94999999999999929, 76.00000000001213607, -136.5231074845243313 ) ) ;
#121090 = ORIENTED_EDGE ( 'NONE', *, *, #157249, .T. ) ;
#121091 = FACE_OUTER_BOUND ( 'NONE', #91933, .T. ) ;
#121092 = VERTEX_POINT ( 'NONE', #191129 ) ;
#121093 = CARTESIAN_POINT ( 'NONE',  ( -18.59999999999999787, -1.835859311432481045, -112.0044391687985694 ) ) ;
#121094 = ORIENTED_EDGE ( 'NONE', *, *, #227902, .F. ) ;
#121095 = AXIS2_PLACEMENT_3D ( 'NONE', #117148, #95004, #173319 ) ;
#121096 = FACE_OUTER_BOUND ( 'NONE', #121599, .T. ) ;
#121097 = CARTESIAN_POINT ( 'NONE',  ( 21.05000000000000071, 87.48912529308749697, -38.92310748452424463 ) ) ;
#121098 = B_SPLINE_CURVE_WITH_KNOTS ( 'NONE', 3,
 ( #93252, #194949, #94530, #232792, #16314, #253600, #154554, #252317, #211938, #95804, #73724, #254839, #150672, #72435, #230201, #136201, #54122, #76253, #52837, #171549, #33330, #251032, #133670, #155825, #235330, #215757 ),
 .UNSPECIFIED., .F., .F.,
 ( 4, 2, 2, 2, 2, 2, 2, 2, 2, 2, 2, 2, 4 ),
 ( 0.005476422646581340439, 0.006160811967703548782, 0.006845201288825757124, 0.007187395949386861729, 0.007529590609947966334, 0.007871785270509069204, 0.008213979931070173809, 0.008556174591631278414, 0.008898369252192381285, 0.009240563912753487624, 0.009582758573314590494, 0.01026714789443680491, 0.01095153721555902106 ),
 .UNSPECIFIED. ) ;
#121100 = ORIENTED_EDGE ( 'NONE', *, *, #249136, .F. ) ;
#121099 = ORIENTED_EDGE ( 'NONE', *, *, #16551, .F. ) ;
#121101 = VERTEX_POINT ( 'NONE', #33355 ) ;
#121102 = DIRECTION ( 'NONE',  ( 1.000000000000000000, 0.000000000000000000, 0.000000000000000000 ) ) ;
#121103 = EDGE_LOOP ( 'NONE', ( #212017, #39104, #200868, #143505 ) ) ;
#121104 = EDGE_LOOP ( 'NONE', ( #164609, #33400, #203630, #223733 ) ) ;
#121105 = CYLINDRICAL_SURFACE ( 'NONE', #134490, 0.09999999999999939493 ) ;
#121107 = ORIENTED_EDGE ( 'NONE', *, *, #213571, .F. ) ;
#121106 = LINE ( 'NONE', #119811, #164324 ) ;
#121109 = DIRECTION ( 'NONE',  ( 1.000000000000000000, -0.000000000000000000, -0.000000000000000000 ) ) ;
#121108 = DIRECTION ( 'NONE',  ( 1.000000000000000000, 0.000000000000000000, 0.000000000000000000 ) ) ;
#121110 = DIRECTION ( 'NONE',  ( 0.000000000000000000, 0.9126074666063545004, 0.4088369013363783999 ) ) ;
#121111 = DIRECTION ( 'NONE',  ( 0.000000000000000000, 0.2128009952263604232, -0.9770955615653316162 ) ) ;
#121112 = CARTESIAN_POINT ( 'NONE',  ( 23.24999999999999289, 10.74948822439028895, -222.3968794097801549 ) ) ;
#121113 = ORIENTED_EDGE ( 'NONE', *, *, #38088, .T. ) ;
#121114 = VERTEX_POINT ( 'NONE', #256137 ) ;
#121115 = DIRECTION ( 'NONE',  ( 0.000000000000000000, 0.9964539953858966292, 0.08413937888696132461 ) ) ;
#121117 = VECTOR ( 'NONE', #220989, 1000.000000000000000 ) ;
#121116 = CYLINDRICAL_SURFACE ( 'NONE', #214098, 0.1000000000000028644 ) ;
#121118 = DIRECTION ( 'NONE',  ( 0.000000000000000000, -0.9999631594459057471, 0.008583690987121077309 ) ) ;
#121119 = AXIS2_PLACEMENT_3D ( 'NONE', #104124, #88407, #84532 ) ;
#121120 = ADVANCED_FACE ( 'NONE', ( #133692 ), #234070, .F. ) ;
#121121 = AXIS2_PLACEMENT_3D ( 'NONE', #22407, #101891, #2802 ) ;
#121122 = ORIENTED_EDGE ( 'NONE', *, *, #211038, .T. ) ;
#121123 = CARTESIAN_POINT ( 'NONE',  ( 22.39999999999999503, 76.10000000001174669, -81.17267829206912211 ) ) ;
#121124 = DIRECTION ( 'NONE',  ( 0.000000000000000000, -0.2128009952263734406, 0.9770955615653287296 ) ) ;
#121125 = AXIS2_PLACEMENT_3D ( 'NONE', #250755, #72144, #151700 ) ;
#121126 = DIRECTION ( 'NONE',  ( 0.000000000000000000, 6.982962677686266711E-15, -1.000000000000000000 ) ) ;
#121127 = ORIENTED_EDGE ( 'NONE', *, *, #243642, .T. ) ;
#121128 = ORIENTED_EDGE ( 'NONE', *, *, #165052, .F. ) ;
#121129 = DIRECTION ( 'NONE',  ( 0.000000000000000000, 1.897661533703519897E-16, -1.000000000000000000 ) ) ;
#121130 = CARTESIAN_POINT ( 'NONE',  ( -20.64999999999999858, 76.00000000001186606, -90.14810748452431710 ) ) ;
#121131 = ORIENTED_EDGE ( 'NONE', *, *, #244222, .F. ) ;
#121132 = CARTESIAN_POINT ( 'NONE',  ( 20.94999999999999929, 36.65892442174935439, -249.5511627012433848 ) ) ;
#121133 = ORIENTED_EDGE ( 'NONE', *, *, #58445, .T. ) ;
#121134 = CARTESIAN_POINT ( 'NONE',  ( 21.00000000000000000, 9.750000000011153745, -179.8499999999999943 ) ) ;
#121135 = CARTESIAN_POINT ( 'NONE',  ( -16.84419801905645997, 9.950000000011140600, -87.83051015377803594 ) ) ;
#121137 = FACE_OUTER_BOUND ( 'NONE', #89700, .T. ) ;
#121136 = DIRECTION ( 'NONE',  ( -1.000000000000000000, 0.000000000000000000, 0.000000000000000000 ) ) ;
#121139 = EDGE_CURVE ( 'NONE', #125280, #225321, #193675, .T. ) ;
#121138 = AXIS2_PLACEMENT_3D ( 'NONE', #92626, #213871, #57342 ) ;
#121140 = DIRECTION ( 'NONE',  ( 1.000000000000000000, 0.000000000000000000, 0.000000000000000000 ) ) ;
#121141 = DIRECTION ( 'NONE',  ( -1.000000000000000000, -0.000000000000000000, 0.000000000000000000 ) ) ;
#121142 = ORIENTED_EDGE ( 'NONE', *, *, #82678, .T. ) ;
#121143 = CARTESIAN_POINT ( 'NONE',  ( -20.94999999999999929, 76.00000000001267608, -203.5231074845243597 ) ) ;
#121145 = ORIENTED_EDGE ( 'NONE', *, *, #219897, .F. ) ;
#121144 = VERTEX_POINT ( 'NONE', #115407 ) ;
#121146 = ORIENTED_EDGE ( 'NONE', *, *, #32652, .T. ) ;
#121147 = ORIENTED_EDGE ( 'NONE', *, *, #206594, .F. ) ;
#121148 = EDGE_CURVE ( 'NONE', #239047, #7145, #134404, .T. ) ;
#121149 = CARTESIAN_POINT ( 'NONE',  ( 18.49999999999999289, 54.98105481382776816, -230.1569079895687366 ) ) ;
#121150 = DIRECTION ( 'NONE',  ( 0.7071067811865475727, 0.7071067811865475727, 2.044391222244500083E-16 ) ) ;
#121151 = CARTESIAN_POINT ( 'NONE',  ( -21.05000000000000071, 69.74218538953603286, -136.6208977758331287 ) ) ;
#121153 = EDGE_CURVE ( 'NONE', #254405, #170816, #26112, .T. ) ;
#121152 = DIRECTION ( 'NONE',  ( 0.000000000000000000, 0.000000000000000000, -1.000000000000000000 ) ) ;
#121154 = CARTESIAN_POINT ( 'NONE',  ( -18.50000000000000000, -1.687074390080403941, -20.68542703345834965 ) ) ;
#121155 = AXIS2_PLACEMENT_3D ( 'NONE', #215783, #116699, #77545 ) ;
#121157 = DIRECTION ( 'NONE',  ( 0.000000000000000000, 0.000000000000000000, -1.000000000000000000 ) ) ;
#121156 = CARTESIAN_POINT ( 'NONE',  ( 20.52683494730037239, 8.980530818301453166, -8.505252722537006704 ) ) ;
#121159 = ORIENTED_EDGE ( 'NONE', *, *, #55702, .F. ) ;
#121158 = CARTESIAN_POINT ( 'NONE',  ( 18.54271179734040942, 77.31781020912761448, -241.8821825064762834 ) ) ;
#121160 = FACE_OUTER_BOUND ( 'NONE', #227852, .T. ) ;
#121161 = EDGE_LOOP ( 'NONE', ( #186429, #58049, #238443, #112696 ) ) ;
#121162 = EDGE_CURVE ( 'NONE', #166364, #232094, #213216, .T. ) ;
#121163 = CARTESIAN_POINT ( 'NONE',  ( 13.99999999999999822, 9.850000000011137402, -83.75000000000004263 ) ) ;
#121164 = VERTEX_POINT ( 'NONE', #76275 ) ;
#121165 = EDGE_LOOP ( 'NONE', ( #158740, #204396, #48171, #196946 ) ) ;
#121166 = CYLINDRICAL_SURFACE ( 'NONE', #166876, 0.09999999999999939493 ) ;
#121167 = AXIS2_PLACEMENT_3D ( 'NONE', #123418, #118289, #101228 ) ;
#121168 = CARTESIAN_POINT ( 'NONE',  ( 18.39999999999999503, 11.75000000001113953, -158.2500000000000284 ) ) ;
#121169 = CARTESIAN_POINT ( 'NONE',  ( -23.15000000000000213, 6.757359537351773859, -220.2789794402637824 ) ) ;
#121170 = CARTESIAN_POINT ( 'NONE',  ( 15.75000000000000000, 9.350000000011139178, -83.51856895740272080 ) ) ;
#121171 = EDGE_CURVE ( 'NONE', #94374, #72992, #16337, .T. ) ;
#121172 = CIRCLE ( 'NONE', #112747, 0.09999999999999939493 ) ;
#121173 = CARTESIAN_POINT ( 'NONE',  ( 18.39999999999999503, 11.47316190337363828, -113.1500000000000341 ) ) ;
#121174 = ORIENTED_EDGE ( 'NONE', *, *, #73390, .T. ) ;
#121176 = VERTEX_POINT ( 'NONE', #35901 ) ;
#121175 = ADVANCED_FACE ( 'NONE', ( #51553 ), #114120, .T. ) ;
#121177 = VECTOR ( 'NONE', #109901, 1000.000000000000000 ) ;
#121178 = FACE_OUTER_BOUND ( 'NONE', #125469, .T. ) ;
#121179 = ORIENTED_EDGE ( 'NONE', *, *, #66108, .F. ) ;
#121180 = FACE_OUTER_BOUND ( 'NONE', #19703, .T. ) ;
#121181 = CYLINDRICAL_SURFACE ( 'NONE', #44462, 0.09999999999999939493 ) ;
#121182 = FACE_OUTER_BOUND ( 'NONE', #220418, .T. ) ;
#121183 = DIRECTION ( 'NONE',  ( 0.000000000000000000, -6.467318590049456648E-15, 1.000000000000000000 ) ) ;
#121184 = CARTESIAN_POINT ( 'NONE',  ( -18.59999999999999787, 68.97833521811179480, -99.18954208262705663 ) ) ;
#121185 = CARTESIAN_POINT ( 'NONE',  ( -21.05000000000000071, 74.63912941281955682, -61.45010955743337178 ) ) ;
#121186 = DIRECTION ( 'NONE',  ( 0.000000000000000000, -0.2617529984165031243, -0.9651348961777157509 ) ) ;
#121187 = DIRECTION ( 'NONE',  ( 0.000000000000000000, -0.8127272543710951647, 0.5826443254700256480 ) ) ;
#121188 = ADVANCED_FACE ( 'NONE', ( #175420 ), #138670, .T. ) ;
#121189 = CARTESIAN_POINT ( 'NONE',  ( 21.05000000000000071, 87.29603075034701476, -72.57100664418810254 ) ) ;
#121190 = CARTESIAN_POINT ( 'NONE',  ( -20.54999999999999716, 71.65000000001225544, -153.2731074845243882 ) ) ;
#121191 = AXIS2_PLACEMENT_3D ( 'NONE', #214555, #17634, #217107 ) ;
#121192 = SPHERICAL_SURFACE ( 'NONE', #28068, 0.1000000000000000056 ) ;
#121193 = CIRCLE ( 'NONE', #29595, 2.000000000000001776 ) ;
#121194 = ORIENTED_EDGE ( 'NONE', *, *, #14122, .T. ) ;
#121195 = AXIS2_PLACEMENT_3D ( 'NONE', #196854, #213865, #93910 ) ;
#121196 = CARTESIAN_POINT ( 'NONE',  ( 20.95496329884391784, 10.56743320610419445, -41.07430993228482663 ) ) ;
#121197 = ORIENTED_EDGE ( 'NONE', *, *, #62428, .F. ) ;
#121198 = AXIS2_PLACEMENT_3D ( 'NONE', #25790, #66206, #144423 ) ;
#121199 = TOROIDAL_SURFACE ( 'NONE', #21242, 11.90000000000000213, 0.1000000000000000056 ) ;
#121200 = LINE ( 'NONE', #98997, #166623 ) ;
#121201 = CARTESIAN_POINT ( 'NONE',  ( 18.59999999999999076, 6.550000000011156231, -177.5170271704400022 ) ) ;
#121202 = CARTESIAN_POINT ( 'NONE',  ( 22.39999999999999503, 64.25313205997782973, -247.2214437328673853 ) ) ;
#121203 = VERTEX_POINT ( 'NONE', #176692 ) ;
#121204 = FACE_OUTER_BOUND ( 'NONE', #155192, .T. ) ;
#121205 = FACE_OUTER_BOUND ( 'NONE', #217832, .T. ) ;
#121206 = CARTESIAN_POINT ( 'NONE',  ( -21.05000000000000071, -11.64999999998884483, -170.4999999999999716 ) ) ;
#121207 = VECTOR ( 'NONE', #236625, 1000.000000000000000 ) ;
#121208 = CARTESIAN_POINT ( 'NONE',  ( -23.30000000000000426, 3.332938107839114927, 33.00000000000000000 ) ) ;
#121209 = AXIS2_PLACEMENT_3D ( 'NONE', #193141, #97846, #15809 ) ;
#121210 = CIRCLE ( 'NONE', #8745, 12.97499999999999964 ) ;
#121211 = DIRECTION ( 'NONE',  ( 0.000000000000000000, 0.000000000000000000, -1.000000000000000000 ) ) ;
#121212 = CARTESIAN_POINT ( 'NONE',  ( -21.05000000000000071, 69.74218538953553548, -69.62089777583315708 ) ) ;
#121213 = VECTOR ( 'NONE', #226311, 1000.000000000000000 ) ;
#121214 = CIRCLE ( 'NONE', #187837, 0.1000000000000028644 ) ;
#121215 = ADVANCED_FACE ( 'NONE', ( #94556 ), #230225, .T. ) ;
#121216 = EDGE_CURVE ( 'NONE', #143771, #8746, #46922, .T. ) ;
#121217 = VERTEX_POINT ( 'NONE', #251059 ) ;
#121218 = CARTESIAN_POINT ( 'NONE',  ( -18.59999999999999787, 77.73670573947921980, -58.00568489690056850 ) ) ;
#121220 = ORIENTED_EDGE ( 'NONE', *, *, #161177, .T. ) ;
#121219 = DIRECTION ( 'NONE',  ( 0.000000000000000000, 1.776356839400254803E-15, -1.000000000000000000 ) ) ;
#121221 = CARTESIAN_POINT ( 'NONE',  ( -20.00857864376270001, 66.75000000001185185, -90.67310748452436542 ) ) ;
#121222 = CARTESIAN_POINT ( 'NONE',  ( -22.39999999999999858, 11.65000000000000036, -0.1000000000000028644 ) ) ;
#121224 = EDGE_CURVE ( 'NONE', #75284, #15820, #238484, .T. ) ;
#121223 = CARTESIAN_POINT ( 'NONE',  ( 21.05000000000000071, 87.48912529308779540, -72.62310748452422615 ) ) ;
#121225 = EDGE_CURVE ( 'NONE', #171894, #90093, #34501, .T. ) ;
#121226 = VERTEX_POINT ( 'NONE', #231525 ) ;
#121227 = DIRECTION ( 'NONE',  ( 0.000000000000000000, 0.8660254037844420383, -0.4999999999999943379 ) ) ;
#121228 = APPLICATION_PROTOCOL_DEFINITION ( 'draft international standard', 'automotive_design', 1998, #99186 ) ;
#121229 = CIRCLE ( 'NONE', #25349, 0.1000000000000000472 ) ;
#121230 = DIRECTION ( 'NONE',  ( 0.000000000000000000, -0.4930308989874980785, -0.8700118002898462599 ) ) ;
#121231 = EDGE_CURVE ( 'NONE', #146973, #238921, #255175, .T. ) ;
#121232 = VERTEX_POINT ( 'NONE', #52861 ) ;
#121233 = LINE ( 'NONE', #40409, #233727 ) ;
#121234 = FACE_OUTER_BOUND ( 'NONE', #80705, .T. ) ;
#121235 = EDGE_CURVE ( 'NONE', #143067, #135417, #54147, .T. ) ;
#121237 = EDGE_CURVE ( 'NONE', #167682, #174804, #17898, .T. ) ;
#121236 = EDGE_CURVE ( 'NONE', #204466, #200569, #81384, .T. ) ;
#121238 = DIRECTION ( 'NONE',  ( -1.000000000000000000, 0.000000000000000000, 0.000000000000000000 ) ) ;
#121239 = ORIENTED_EDGE ( 'NONE', *, *, #251543, .F. ) ;
#121240 = EDGE_CURVE ( 'NONE', #80321, #257571, #251110, .T. ) ;
#121241 = VERTEX_POINT ( 'NONE', #197507 ) ;
#121242 = CARTESIAN_POINT ( 'NONE',  ( -22.45437739390953169, 76.00000000001203659, -114.6726782961207505 ) ) ;
#121243 = DIRECTION ( 'NONE',  ( 0.000000000000000000, 0.000000000000000000, 1.000000000000000000 ) ) ;
#121244 = VECTOR ( 'NONE', #228138, 1000.000000000000000 ) ;
#121245 = DIRECTION ( 'NONE',  ( 1.000000000000000000, -0.000000000000000000, -0.000000000000000000 ) ) ;
#121246 = DIRECTION ( 'NONE',  ( 1.000000000000000000, 0.000000000000000000, 0.000000000000000000 ) ) ;
#121247 = EDGE_CURVE ( 'NONE', #253379, #249805, #234380, .T. ) ;
#121248 = CARTESIAN_POINT ( 'NONE',  ( 18.49999999999999289, 10.49142135624846439, -125.3500000000000512 ) ) ;
#121249 = CARTESIAN_POINT ( 'NONE',  ( 20.94999999999999929, -1.349153571964892606, -175.2874973355899044 ) ) ;
#121251 = DIRECTION ( 'NONE',  ( 1.000000000000000000, 0.000000000000000000, 0.000000000000000000 ) ) ;
#121250 = CARTESIAN_POINT ( 'NONE',  ( 21.00023020733438273, 6.390869245267715826, -6.911788849595090767E-16 ) ) ;
#121252 = CYLINDRICAL_SURFACE ( 'NONE', #140317, 1.749999999999999778 ) ;
#121254 = EDGE_CURVE ( 'NONE', #3745, #203569, #167777, .T. ) ;
#121253 = CYLINDRICAL_SURFACE ( 'NONE', #193737, 11.74999999999999645 ) ;
#121255 = CARTESIAN_POINT ( 'NONE',  ( 22.45301702632625762, 0.01521087972134078925, -155.8502077757395625 ) ) ;
#121257 = EDGE_CURVE ( 'NONE', #114377, #115375, #246843, .T. ) ;
#121256 = CARTESIAN_POINT ( 'NONE',  ( 23.24999999999997513, 64.25000000001146816, -43.03791325517834565 ) ) ;
#121258 = VERTEX_POINT ( 'NONE', #157133 ) ;
#121259 = AXIS2_PLACEMENT_3D ( 'NONE', #120428, #1710, #179116 ) ;
#121260 = ORIENTED_EDGE ( 'NONE', *, *, #79273, .F. ) ;
#121261 = CARTESIAN_POINT ( 'NONE',  ( 21.14999999999999503, -11.74999999998883560, -69.90000000000004832 ) ) ;
#121263 = CARTESIAN_POINT ( 'NONE',  ( 21.05095171578076574, 67.22382012124155892, -191.3572342078865347 ) ) ;
#121262 = CARTESIAN_POINT ( 'NONE',  ( -21.14999999999999858, 76.00000000001271871, -210.0637644362255969 ) ) ;
#121264 = EDGE_CURVE ( 'NONE', #221530, #177661, #55282, .T. ) ;
#121265 = AXIS2_PLACEMENT_3D ( 'NONE', #43839, #123375, #98626 ) ;
#121266 = CYLINDRICAL_SURFACE ( 'NONE', #31161, 7.899999999999990585 ) ;
#121267 = DIRECTION ( 'NONE',  ( 0.000000000000000000, 0.4721928772776973204, 0.8814952561688629284 ) ) ;
#121268 = DIRECTION ( 'NONE',  ( 1.000000000000000000, 0.000000000000000000, 0.000000000000000000 ) ) ;
#121269 = ADVANCED_FACE ( 'NONE', ( #82670 ), #236633, .T. ) ;
#121270 = ORIENTED_EDGE ( 'NONE', *, *, #247845, .T. ) ;
#121271 = EDGE_CURVE ( 'NONE', #223519, #6309, #219639, .T. ) ;
#121272 = CARTESIAN_POINT ( 'NONE',  ( 18.49999999999996803, 68.92903212821283887, -65.77654326265606244 ) ) ;
#121273 = ORIENTED_EDGE ( 'NONE', *, *, #102097, .F. ) ;
#121274 = CARTESIAN_POINT ( 'NONE',  ( -16.90202395485708919, 51.66072493185733805, -231.9102439397140358 ) ) ;
#121275 = EDGE_LOOP ( 'NONE', ( #158392, #151551, #30967, #243332 ) ) ;
#121276 = DIRECTION ( 'NONE',  ( -1.000000000000000000, 0.000000000000000000, 0.000000000000000000 ) ) ;
#121277 = AXIS2_PLACEMENT_3D ( 'NONE', #37451, #214777, #174428 ) ;
#121278 = VECTOR ( 'NONE', #185860, 1000.000000000000000 ) ;
#121279 = PLANE ( 'NONE',  #254603 ) ;
#121280 = CIRCLE ( 'NONE', #17202, 0.09999999999999982514 ) ;
#121281 = ORIENTED_EDGE ( 'NONE', *, *, #24410, .F. ) ;
#121282 = DIRECTION ( 'NONE',  ( 1.000000000000000000, -0.000000000000000000, -0.000000000000000000 ) ) ;
#121283 = VERTEX_POINT ( 'NONE', #4444 ) ;
#121284 = CARTESIAN_POINT ( 'NONE',  ( 18.59999999999999787, 77.25000000001239187, -162.2226267301092832 ) ) ;
#121285 = DIRECTION ( 'NONE',  ( 0.000000000000000000, 6.577889128801576950E-15, -1.000000000000000000 ) ) ;
#121286 = DIRECTION ( 'NONE',  ( 0.000000000000000000, 0.000000000000000000, 1.000000000000000000 ) ) ;
#121287 = DIRECTION ( 'NONE',  ( -1.000000000000000000, 0.000000000000000000, 0.000000000000000000 ) ) ;
#121288 = DIRECTION ( 'NONE',  ( 1.000000000000000000, 0.000000000000000000, 0.000000000000000000 ) ) ;
#121289 = CARTESIAN_POINT ( 'NONE',  ( 18.58222699835054570, 65.66799936921553638, -130.9299399888601272 ) ) ;
#121290 = VECTOR ( 'NONE', #251852, 1000.000000000000000 ) ;
#121291 = DIRECTION ( 'NONE',  ( 0.000000000000000000, -0.4999999999999689138, 0.8660254037844565822 ) ) ;
#121293 = VERTEX_POINT ( 'NONE', #41040 ) ;
#121292 = CARTESIAN_POINT ( 'NONE',  ( 20.72390388899090041, 65.41003688158804152, -129.0117591887780577 ) ) ;
#121295 = DIRECTION ( 'NONE',  ( 3.469446951953609771E-14, -0.7899159663865552572, -0.6132151058540507016 ) ) ;
#121294 = CARTESIAN_POINT ( 'NONE',  ( 20.94999999999999929, -1.835341550213257733, -112.0551512925630249 ) ) ;
#121296 = ORIENTED_EDGE ( 'NONE', *, *, #13424, .T. ) ;
#121298 = ORIENTED_EDGE ( 'NONE', *, *, #210346, .F. ) ;
#121297 = DIRECTION ( 'NONE',  ( 7.304098846218134667E-16, -0.9651348961777158619, 0.2617529984165031243 ) ) ;
#121299 = EDGE_LOOP ( 'NONE', ( #248784, #94565, #133857, #181494 ) ) ;
#121300 = DIRECTION ( 'NONE',  ( -2.168404344971008868E-16, 0.000000000000000000, -1.000000000000000000 ) ) ;
#121301 = CARTESIAN_POINT ( 'NONE',  ( -22.14074124539699895, 29.87418771707450205, -252.4821028181641225 ) ) ;
#121302 = VERTEX_POINT ( 'NONE', #21473 ) ;
#121303 = CARTESIAN_POINT ( 'NONE',  ( 23.24999999999999645, 23.82801463864234393, -229.3483719500187306 ) ) ;
#121304 = CARTESIAN_POINT ( 'NONE',  ( 23.15000000000000213, 49.61306877027904250, -254.2671747026441551 ) ) ;
#121305 = CARTESIAN_POINT ( 'NONE',  ( 18.49505816908825651, 38.17690089667952691, -261.0709640404842844 ) ) ;
#121306 = FACE_OUTER_BOUND ( 'NONE', #188390, .T. ) ;
#121307 = CARTESIAN_POINT ( 'NONE',  ( -18.50211644919735932, 46.36250628750309488, -243.0620573837409779 ) ) ;
#121308 = VECTOR ( 'NONE', #86602, 1000.000000000000000 ) ;
#121309 = EDGE_CURVE ( 'NONE', #124703, #64997, #30395, .T. ) ;
#121310 = CIRCLE ( 'NONE', #42171, 0.1999999999999987899 ) ;
#121311 = AXIS2_PLACEMENT_3D ( 'NONE', #62232, #63494, #179625 ) ;
#121313 = AXIS2_PLACEMENT_3D ( 'NONE', #83602, #178929, #60213 ) ;
#121312 = CARTESIAN_POINT ( 'NONE',  ( -20.85000000000000142, 1.115600667400684642E-11, -167.5000000000000284 ) ) ;
#121314 = ORIENTED_EDGE ( 'NONE', *, *, #76410, .T. ) ;
#121315 = VERTEX_POINT ( 'NONE', #100932 ) ;
#121316 = EDGE_CURVE ( 'NONE', #152840, #40817, #176149, .T. ) ;
#121317 = LINE ( 'NONE', #83395, #256067 ) ;
#121318 = EDGE_LOOP ( 'NONE', ( #164880, #73287, #73516, #10352 ) ) ;
#121319 = CARTESIAN_POINT ( 'NONE',  ( 23.25000000000000000, 85.00000000001159606, -59.62913836187181715 ) ) ;
#121320 = ORIENTED_EDGE ( 'NONE', *, *, #224447, .T. ) ;
#121321 = CARTESIAN_POINT ( 'NONE',  ( -23.30000000000000426, -11.79999999999999893, -347.0000000000001137 ) ) ;
#121322 = EDGE_CURVE ( 'NONE', #152104, #76073, #209432, .T. ) ;
#121323 = EDGE_CURVE ( 'NONE', #232013, #196307, #245403, .T. ) ;
#121324 = DIRECTION ( 'NONE',  ( 0.000000000000000000, 0.000000000000000000, 1.000000000000000000 ) ) ;
#121325 = DIRECTION ( 'NONE',  ( 0.7071067811865462405, 0.2890913453342134898, -0.6453109281988460566 ) ) ;
#121326 = DIRECTION ( 'NONE',  ( 1.000000000000000000, -0.000000000000000000, -0.000000000000000000 ) ) ;
#121327 = ORIENTED_EDGE ( 'NONE', *, *, #41876, .T. ) ;
#121328 = CIRCLE ( 'NONE', #175470, 0.1000000000000054040 ) ;
#121329 = CARTESIAN_POINT ( 'NONE',  ( 23.15000000000000213, -8.999999999988844479, -143.8939691226524644 ) ) ;
#121330 = DIRECTION ( 'NONE',  ( 0.000000000000000000, 0.000000000000000000, 1.000000000000000000 ) ) ;
#121331 = CARTESIAN_POINT ( 'NONE',  ( 20.94999999999999929, 76.00000000001185185, -90.04810748452430857 ) ) ;
#121332 = CARTESIAN_POINT ( 'NONE',  ( -2.995603634470891112E-16, 66.37537870982728805, -213.6053525232321704 ) ) ;
#121333 = ORIENTED_EDGE ( 'NONE', *, *, #97114, .F. ) ;
#121335 = CARTESIAN_POINT ( 'NONE',  ( 22.48660254037844197, 64.35000000001213039, -136.5731074845243995 ) ) ;
#121334 = DIRECTION ( 'NONE',  ( 0.000000000000000000, 0.000000000000000000, -1.000000000000000000 ) ) ;
#121336 = ORIENTED_EDGE ( 'NONE', *, *, #172116, .T. ) ;
#121339 = ORIENTED_EDGE ( 'NONE', *, *, #247152, .T. ) ;
#121338 = CARTESIAN_POINT ( 'NONE',  ( -21.05000000000000071, 1.115600667400684642E-11, -200.9999999999999432 ) ) ;
#121337 = CARTESIAN_POINT ( 'NONE',  ( 18.79999999999999716, -11.65000000000000036, 32.89999999999999858 ) ) ;
#121340 = EDGE_CURVE ( 'NONE', #136008, #253318, #85240, .T. ) ;
#121341 = ORIENTED_EDGE ( 'NONE', *, *, #31314, .T. ) ;
#121342 = CARTESIAN_POINT ( 'NONE',  ( 18.59999999999999076, 69.55000000001187743, -93.00608031408432907 ) ) ;
#121343 = EDGE_CURVE ( 'NONE', #32310, #208014, #125684, .T. ) ;
#121344 = CARTESIAN_POINT ( 'NONE',  ( 22.60000000000000142, 0.000000000000000000, 0.000000000000000000 ) ) ;
#121345 = CARTESIAN_POINT ( 'NONE',  ( 21.05000000000000071, 8.776282895303632259, -79.15000000000004832 ) ) ;
#121346 = ORIENTED_EDGE ( 'NONE', *, *, #253111, .T. ) ;
#121347 = CARTESIAN_POINT ( 'NONE',  ( -16.86337532320260735, 66.02003279578765671, -115.5741830155415499 ) ) ;
#121348 = CIRCLE ( 'NONE', #216952, 0.09999999999999939493 ) ;
#121349 = DIRECTION ( 'NONE',  ( -1.000000000000000000, -1.734723475976817507E-14, 0.000000000000000000 ) ) ;
#121351 = CARTESIAN_POINT ( 'NONE',  ( -16.87331047859651179, 44.13548170601895038, -235.2989316066074821 ) ) ;
#121350 = DIRECTION ( 'NONE',  ( 0.000000000000000000, -0.9126074666063771490, -0.4088369013363281623 ) ) ;
#121353 = VERTEX_POINT ( 'NONE', #168722 ) ;
#121352 = CARTESIAN_POINT ( 'NONE',  ( 21.59780538579342135, 0.09897866959798530540, 6.847090529943256065 ) ) ;
#121354 = CIRCLE ( 'NONE', #150362, 12.87500000000000178 ) ;
#121355 = ADVANCED_FACE ( 'NONE', ( #108698 ), #13807, .F. ) ;
#121356 = EDGE_LOOP ( 'NONE', ( #97625, #72839, #33306, #172798 ) ) ;
#121357 = AXIS2_PLACEMENT_3D ( 'NONE', #187379, #243480, #105208 ) ;
#121358 = ADVANCED_FACE ( 'NONE', ( #129553 ), #186977, .T. ) ;
#121359 = CARTESIAN_POINT ( 'NONE',  ( -21.14999999999999858, -11.65000000000000036, 3.469446951953614189E-15 ) ) ;
#121360 = CARTESIAN_POINT ( 'NONE',  ( 23.14999999999999858, 1.115600667400684642E-11, -167.5000000000000284 ) ) ;
#121362 = ORIENTED_EDGE ( 'NONE', *, *, #206794, .T. ) ;
#121361 = AXIS2_PLACEMENT_3D ( 'NONE', #90352, #5660, #244289 ) ;
#121363 = FACE_OUTER_BOUND ( 'NONE', #231050, .T. ) ;
#121364 = ORIENTED_EDGE ( 'NONE', *, *, #232577, .F. ) ;
#121365 = FACE_OUTER_BOUND ( 'NONE', #212245, .T. ) ;
#121366 = AXIS2_PLACEMENT_3D ( 'NONE', #135579, #176035, #215135 ) ;
#121367 = CARTESIAN_POINT ( 'NONE',  ( 21.05000000000000071, 77.84908441863962025, -191.8670969630772163 ) ) ;
#121368 = DIRECTION ( 'NONE',  ( 0.000000000000000000, 0.000000000000000000, -1.000000000000000000 ) ) ;
#121369 = EDGE_LOOP ( 'NONE', ( #132613, #236467, #235584, #22875, #184612 ) ) ;
#121370 = EDGE_CURVE ( 'NONE', #209835, #2822, #192884, .T. ) ;
#121371 = CIRCLE ( 'NONE', #664, 0.1000000000000017680 ) ;
#121372 = EDGE_CURVE ( 'NONE', #86923, #127210, #197143, .T. ) ;
#121374 = EDGE_CURVE ( 'NONE', #201532, #18598, #86530, .T. ) ;
#121373 = CIRCLE ( 'NONE', #175516, 11.75000000000000000 ) ;
#121375 = DIRECTION ( 'NONE',  ( 0.000000000000000000, 0.000000000000000000, -1.000000000000000000 ) ) ;
#121376 = AXIS2_PLACEMENT_3D ( 'NONE', #239648, #139227, #140524 ) ;
#121377 = EDGE_LOOP ( 'NONE', ( #15251, #49516, #122871, #172797 ) ) ;
#121378 = EDGE_LOOP ( 'NONE', ( #212412, #161038 ) ) ;
#121379 = AXIS2_PLACEMENT_3D ( 'NONE', #228513, #54970, #49853 ) ;
#121380 = VERTEX_POINT ( 'NONE', #166139 ) ;
#121381 = FACE_OUTER_BOUND ( 'NONE', #140584, .T. ) ;
#121382 = EDGE_LOOP ( 'NONE', ( #206049, #71770, #239148, #74389 ) ) ;
#121384 = ORIENTED_EDGE ( 'NONE', *, *, #23673, .F. ) ;
#121383 = LINE ( 'NONE', #58770, #155244 ) ;
#121385 = EDGE_CURVE ( 'NONE', #68445, #71022, #227350, .T. ) ;
#121386 = ORIENTED_EDGE ( 'NONE', *, *, #28810, .F. ) ;
#121389 = ORIENTED_EDGE ( 'NONE', *, *, #26719, .T. ) ;
#121388 = EDGE_LOOP ( 'NONE', ( #137241, #133519, #84246, #70677 ) ) ;
#121387 = CARTESIAN_POINT ( 'NONE',  ( -16.77683809663752257, 9.945835743215301505, -113.1639490191042512 ) ) ;
#121390 = EDGE_CURVE ( 'NONE', #97776, #222832, #46147, .T. ) ;
#121391 = EDGE_LOOP ( 'NONE', ( #36110, #201507, #18449, #219911 ) ) ;
#121392 = DIRECTION ( 'NONE',  ( 0.000000000000000000, 0.000000000000000000, 1.000000000000000000 ) ) ;
#121393 = CIRCLE ( 'NONE', #229689, 0.1000000000000002554 ) ;
#121394 = CIRCLE ( 'NONE', #179630, 11.65000000000001457 ) ;
#121395 = AXIS2_PLACEMENT_3D ( 'NONE', #189180, #108360, #31420 ) ;
#121396 =( BOUNDED_SURFACE ( )  B_SPLINE_SURFACE ( 3, 2, ( 
 ( #129201, #165774, #47067 ),
 ( #186615, #7973, #127918 ),
 ( #90051, #207462, #108355 ),
 ( #50906, #167071, #187896 ),
 ( #67931, #249159, #208747 ),
 ( #9239, #30115, #150065 ),
 ( #130470, #75663, #74395 ),
 ( #177346, #93913, #134307 ),
 ( #152643, #232164, #53508 ),
 ( #16967, #235987, #35268 ) ),
 .UNSPECIFIED., .F., .F., .T. ) 
 B_SPLINE_SURFACE_WITH_KNOTS ( ( 4, 2, 2, 2, 4 ),
 ( 3, 3 ),
 ( 0.002161241639767812889, 0.002579950749617465015, 0.002789305304542291294, 0.002893982582004704217, 0.002998659859467117141 ),
 ( 0.000000000000000000, 1.000000000000000000 ),
 .UNSPECIFIED. ) 
 GEOMETRIC_REPRESENTATION_ITEM ( )  RATIONAL_B_SPLINE_SURFACE ( (
 ( 1.000000000000000000, 0.7071067811864985009, 1.000000000000000000),
 ( 1.000000000000000000, 0.7632447400666618753, 1.000000000000000000),
 ( 1.000000000000000000, 0.8158073005106054598, 1.000000000000000000),
 ( 1.000000000000000000, 0.8906973462397409502, 1.000000000000000000),
 ( 1.000000000000000000, 0.9149408947796440206, 1.000000000000000000),
 ( 1.000000000000000000, 0.9493368785277611632, 1.000000000000000000),
 ( 1.000000000000000000, 0.9605194247158402865, 1.000000000000000000),
 ( 1.000000000000000000, 0.9803630264779391590, 1.000000000000000000),
 ( 1.000000000000000000, 0.9900844824272457823, 1.000000000000000000),
 ( 1.000000000000000000, 0.9894588281429252952, 1.000000000000000000) ) ) 
 REPRESENTATION_ITEM ( '' )  SURFACE ( )  );
#121397 = AXIS2_PLACEMENT_3D ( 'NONE', #115764, #177047, #213575 ) ;
#121398 = CARTESIAN_POINT ( 'NONE',  ( -16.85697194749124250, 14.05784564333523079, -218.9854180901164113 ) ) ;
#121399 = ORIENTED_EDGE ( 'NONE', *, *, #197841, .F. ) ;
#121400 = PLANE ( 'NONE',  #112148 ) ;
#121402 = ORIENTED_EDGE ( 'NONE', *, *, #249609, .F. ) ;
#121401 = CYLINDRICAL_SURFACE ( 'NONE', #161753, 11.80000000000000604 ) ;
#121403 = SPHERICAL_SURFACE ( 'NONE', #229807, 0.1000000000000000056 ) ;
#121405 = ORIENTED_EDGE ( 'NONE', *, *, #5801, .F. ) ;
#121404 = CARTESIAN_POINT ( 'NONE',  ( -18.59999999999999787, 76.00000000001237765, -170.0231074845243597 ) ) ;
#121406 = ORIENTED_EDGE ( 'NONE', *, *, #227403, .F. ) ;
#121407 = CARTESIAN_POINT ( 'NONE',  ( 18.39999999999999858, -9.499999999999998224, -40.10018939122204529 ) ) ;
#121408 = LINE ( 'NONE', #237465, #232534 ) ;
#121409 = ORIENTED_EDGE ( 'NONE', *, *, #30170, .F. ) ;
#121410 = ORIENTED_EDGE ( 'NONE', *, *, #77344, .T. ) ;
#121411 = CARTESIAN_POINT ( 'NONE',  ( -16.93710578446423654, 9.950000000011137047, -180.4188039837998474 ) ) ;
#121412 = CARTESIAN_POINT ( 'NONE',  ( -21.05000000000000071, -0.02110330804802081767, -161.1954836707355128 ) ) ;
#121414 = VERTEX_POINT ( 'NONE', #205207 ) ;
#121413 = EDGE_LOOP ( 'NONE', ( #123765, #58705, #36806, #236587 ) ) ;
#121415 = ORIENTED_EDGE ( 'NONE', *, *, #87850, .F. ) ;
#121416 = LINE ( 'NONE', #1412, #152857 ) ;
#121417 = ORIENTED_EDGE ( 'NONE', *, *, #23159, .F. ) ;
#121418 = VERTEX_POINT ( 'NONE', #26612 ) ;
#121419 = CARTESIAN_POINT ( 'NONE',  ( 18.49505816908824229, 85.43787255322352792, -163.2454502828533975 ) ) ;
#121420 = ORIENTED_EDGE ( 'NONE', *, *, #3958, .F. ) ;
#121421 = LINE ( 'NONE', #123964, #19010 ) ;
#121423 = CARTESIAN_POINT ( 'NONE',  ( 18.42595409746858692, -9.499999812553779677, -107.4993623517473793 ) ) ;
#121422 = CARTESIAN_POINT ( 'NONE',  ( -18.59999999999999787, 2.859758780633683273, -208.6670499591424459 ) ) ;
#121424 = AXIS2_PLACEMENT_3D ( 'NONE', #68749, #188682, #51715 ) ;
#121425 = EDGE_LOOP ( 'NONE', ( #7812, #182609, #62100, #34493 ) ) ;
#121427 = ORIENTED_EDGE ( 'NONE', *, *, #172148, .F. ) ;
#121426 = ORIENTED_EDGE ( 'NONE', *, *, #33763, .T. ) ;
#121428 = FACE_OUTER_BOUND ( 'NONE', #237981, .T. ) ;
#121429 = ORIENTED_EDGE ( 'NONE', *, *, #201878, .F. ) ;
#121430 = CIRCLE ( 'NONE', #142236, 0.1000000000000028644 ) ;
#121431 = DIRECTION ( 'NONE',  ( 0.000000000000000000, 0.000000000000000000, -1.000000000000000000 ) ) ;
#121432 = VERTEX_POINT ( 'NONE', #167410 ) ;
#121433 = ORIENTED_EDGE ( 'NONE', *, *, #170319, .T. ) ;
#121434 = DIRECTION ( 'NONE',  ( -0.000000000000000000, -0.000000000000000000, 1.000000000000000000 ) ) ;
#121435 = ADVANCED_FACE ( 'NONE', ( #124416 ), #189532, .F. ) ;
#121436 = EDGE_LOOP ( 'NONE', ( #223200, #251598, #198502, #226541 ) ) ;
#121437 = DIRECTION ( 'NONE',  ( -1.000000000000000000, -0.000000000000000000, 0.000000000000000000 ) ) ;
#121438 = CARTESIAN_POINT ( 'NONE',  ( 21.05000000000000071, 34.01125473725045367, -243.8802146427659352 ) ) ;
#121439 = EDGE_LOOP ( 'NONE', ( #233278, #178938, #220434, #141693 ) ) ;
#121440 = CARTESIAN_POINT ( 'NONE',  ( -21.04999999999994387, 77.16254490893143725, -44.02310748452479316 ) ) ;
#121441 = LINE ( 'NONE', #221759, #70510 ) ;
#121443 = CARTESIAN_POINT ( 'NONE',  ( 18.59999999999999076, 6.650000000011155876, -155.3500000000000227 ) ) ;
#121442 = DIRECTION ( 'NONE',  ( 0.000000000000000000, 0.000000000000000000, 1.000000000000000000 ) ) ;
#121444 = CARTESIAN_POINT ( 'NONE',  ( -20.94999999999999929, -1.162701749926853712, -175.3999999999999773 ) ) ;
#121445 = ADVANCED_FACE ( 'NONE', ( #244340 ), #238255, .T. ) ;
#121447 = ADVANCED_FACE ( 'NONE', ( #210376 ), #53863, .F. ) ;
#121446 = CARTESIAN_POINT ( 'NONE',  ( 21.13507111622889667, 65.28231661301390432, -157.7739388981636353 ) ) ;
#121448 = CARTESIAN_POINT ( 'NONE',  ( -23.25000000000000355, 70.35000000001232934, -160.7731074845243882 ) ) ;
#121449 = CARTESIAN_POINT ( 'NONE',  ( -23.15000000000000213, 76.00000000001142553, -36.02310748452432421 ) ) ;
#121450 = DIRECTION ( 'NONE',  ( -0.000000000000000000, 0.000000000000000000, 1.000000000000000000 ) ) ;
#121451 = CIRCLE ( 'NONE', #38222, 0.1000000000000029476 ) ;
#121452 = ORIENTED_EDGE ( 'NONE', *, *, #5902, .F. ) ;
#121453 = AXIS2_PLACEMENT_3D ( 'NONE', #146410, #63032, #123029 ) ;
#121454 = AXIS2_PLACEMENT_3D ( 'NONE', #226724, #27290, #127643 ) ;
#121456 = ORIENTED_EDGE ( 'NONE', *, *, #116010, .F. ) ;
#121455 = VERTEX_POINT ( 'NONE', #55108 ) ;
#121457 = VERTEX_POINT ( 'NONE', #152998 ) ;
#121458 = ORIENTED_EDGE ( 'NONE', *, *, #16144, .T. ) ;
#121459 = ADVANCED_FACE ( 'NONE', ( #130823 ), #192108, .T. ) ;
#121460 = DIRECTION ( 'NONE',  ( 1.000000000000000000, 0.000000000000000000, 0.000000000000000000 ) ) ;
#121462 = CARTESIAN_POINT ( 'NONE',  ( -14.23072895065543264, 9.455987233612740184, -15.01153116689783040 ) ) ;
#121461 = DIRECTION ( 'NONE',  ( -1.000000000000000000, 0.000000000000000000, 0.000000000000000000 ) ) ;
#121463 = CARTESIAN_POINT ( 'NONE',  ( 20.95512820512820440, 67.12384868372420499, -161.4644784893834810 ) ) ;
#121464 = ORIENTED_EDGE ( 'NONE', *, *, #170160, .T. ) ;
#121465 = CARTESIAN_POINT ( 'NONE',  ( -20.92356734117541706, 10.31973158071402175, -106.0505334713354841 ) ) ;
#121466 = CARTESIAN_POINT ( 'NONE',  ( -23.25000000000000000, 87.48912529308779540, -72.62310748452422615 ) ) ;
#121468 = AXIS2_PLACEMENT_3D ( 'NONE', #250137, #211012, #111923 ) ;
#121467 = DIRECTION ( 'NONE',  ( 1.000000000000000000, -3.265361837132813093E-16, -2.280189983783949500E-30 ) ) ;
#121469 = DIRECTION ( 'NONE',  ( 0.000000000000000000, 0.2128009952263485993, -0.9770955615653341697 ) ) ;
#121470 = ORIENTED_EDGE ( 'NONE', *, *, #117914, .F. ) ;
#121471 = CARTESIAN_POINT ( 'NONE',  ( -20.94999999999999929, -1.249999999988843369, -75.00000000000004263 ) ) ;
#121472 = CARTESIAN_POINT ( 'NONE',  ( -23.15000000000000213, 71.65000000001180069, -81.77310748452433131 ) ) ;
#121473 = ORIENTED_EDGE ( 'NONE', *, *, #186340, .T. ) ;
#121474 = EDGE_CURVE ( 'NONE', #52350, #156064, #1319, .T. ) ;
#121475 = DIRECTION ( 'NONE',  ( 1.000000000000000000, 0.000000000000000000, 0.000000000000000000 ) ) ;
#121476 = EDGE_CURVE ( 'NONE', #229005, #8823, #250768, .T. ) ;
#121477 = DIRECTION ( 'NONE',  ( -1.073024830501117725E-15, 6.982962677686266711E-15, -1.000000000000000000 ) ) ;
#121478 = CYLINDRICAL_SURFACE ( 'NONE', #114389, 0.1000000000000028644 ) ;
#121479 = CARTESIAN_POINT ( 'NONE',  ( 22.94999999999999929, 0.000000000000000000, -3.900000000000000355 ) ) ;
#121480 = DIRECTION ( 'NONE',  ( -1.836970198721029934E-16, -1.000000000000000000, -6.982962677686266711E-15 ) ) ;
#121481 = ORIENTED_EDGE ( 'NONE', *, *, #146395, .T. ) ;
#121482 = LINE ( 'NONE', #161886, #161222 ) ;
#121483 = CARTESIAN_POINT ( 'NONE',  ( -20.54999999999999716, 85.00000000001251976, -179.5170766071767332 ) ) ;
#121484 = CARTESIAN_POINT ( 'NONE',  ( -21.05000000000000071, 77.83534155023670564, -158.4679561919613491 ) ) ;
#121487 = CARTESIAN_POINT ( 'NONE',  ( 20.94999999999999929, 74.95298800634525094, -207.3836470692357636 ) ) ;
#121486 = VECTOR ( 'NONE', #26345, 1000.000000000000000 ) ;
#121485 = FACE_OUTER_BOUND ( 'NONE', #16156, .T. ) ;
#121489 = LINE ( 'NONE', #200998, #228819 ) ;
#121488 = VECTOR ( 'NONE', #51177, 1000.000000000000000 ) ;
#121490 = EDGE_CURVE ( 'NONE', #83182, #160572, #205319, .T. ) ;
#121491 = CIRCLE ( 'NONE', #254517, 0.09999999999999553690 ) ;
#121492 = LINE ( 'NONE', #61488, #133104 ) ;
#121493 = DIRECTION ( 'NONE',  ( -0.000000000000000000, -0.000000000000000000, 1.000000000000000000 ) ) ;
#121494 = DIRECTION ( 'NONE',  ( 0.000000000000000000, 0.9910465087640866200, 0.1335171055202873380 ) ) ;
#121496 = ORIENTED_EDGE ( 'NONE', *, *, #210388, .F. ) ;
#121495 = CARTESIAN_POINT ( 'NONE',  ( -17.80356949364094277, 10.87673139701457536, -144.2869269757789823 ) ) ;
#121497 = EDGE_LOOP ( 'NONE', ( #216239, #73116, #188065, #191299 ) ) ;
#121498 = AXIS2_PLACEMENT_3D ( 'NONE', #145873, #225404, #126317 ) ;
#121499 = FILL_AREA_STYLE ('',( #41953 ) ) ;
#121500 = EDGE_CURVE ( 'NONE', #256585, #17954, #172265, .T. ) ;
#121501 = DIRECTION ( 'NONE',  ( 0.000000000000000000, 0.9908441862701791170, -0.1350103645450472789 ) ) ;
#121502 = DIRECTION ( 'NONE',  ( 1.000000000000000000, -3.265361837132813093E-16, -2.280189983783949500E-30 ) ) ;
#121503 = ORIENTED_EDGE ( 'NONE', *, *, #154463, .T. ) ;
#121504 = LINE ( 'NONE', #100589, #221976 ) ;
#121505 = CARTESIAN_POINT ( 'NONE',  ( 23.24999999999999289, 53.42432843990430058, -234.7536552047824330 ) ) ;
#121506 = CYLINDRICAL_SURFACE ( 'NONE', #140255, 0.1000000000000101918 ) ;
#121507 = ADVANCED_FACE ( 'NONE', ( #170003 ), #233794, .F. ) ;
#121508 = ADVANCED_FACE ( 'NONE', ( #70886 ), #95547, .T. ) ;
#121509 = CARTESIAN_POINT ( 'NONE',  ( 18.59999999999999076, 1.835341550224411922, -11.55515129256298046 ) ) ;
#121511 = ORIENTED_EDGE ( 'NONE', *, *, #150017, .T. ) ;
#121510 = DIRECTION ( 'NONE',  ( -1.000000000000000000, 0.000000000000000000, -0.000000000000000000 ) ) ;
#121513 = CARTESIAN_POINT ( 'NONE',  ( -17.22767730082509630, 10.34924421247947102, -156.1424286905735528 ) ) ;
#121512 = CYLINDRICAL_SURFACE ( 'NONE', #158937, 0.09999999999999939493 ) ;
#121514 = CARTESIAN_POINT ( 'NONE',  ( 20.22894356738409627, 66.72150177717459485, -161.7545845782749154 ) ) ;
#121516 = EDGE_CURVE ( 'NONE', #75834, #83901, #249504, .T. ) ;
#121515 = CARTESIAN_POINT ( 'NONE',  ( -16.77683809663752257, 66.05416425680844839, -190.8591584654202222 ) ) ;
#121517 = ADVANCED_FACE ( 'NONE', ( #254599 ), #155564, .T. ) ;
#121518 = ORIENTED_EDGE ( 'NONE', *, *, #224602, .F. ) ;
#121519 = AXIS2_PLACEMENT_3D ( 'NONE', #176010, #75625, #116026 ) ;
#121520 = DIRECTION ( 'NONE',  ( 1.000000000000000000, 0.000000000000000000, 0.000000000000000000 ) ) ;
#121521 = DIRECTION ( 'NONE',  ( -7.304098846218134667E-16, 0.9651348961777158619, -0.2617529984165031243 ) ) ;
#121522 = DIRECTION ( 'NONE',  ( 0.000000000000000000, 0.4999999999999608646, 0.8660254037844612451 ) ) ;
#121523 = VERTEX_POINT ( 'NONE', #14764 ) ;
#121524 = AXIS2_PLACEMENT_3D ( 'NONE', #87493, #187908, #143627 ) ;
#121525 = DIRECTION ( 'NONE',  ( -1.000000000000000000, 0.000000000000000000, 0.000000000000000000 ) ) ;
#121526 = DIRECTION ( 'NONE',  ( 1.000000000000000000, -0.000000000000000000, -0.000000000000000000 ) ) ;
#121527 = ORIENTED_EDGE ( 'NONE', *, *, #7938, .T. ) ;
#121528 = ADVANCED_FACE ( 'NONE', ( #52559 ), #173860, .F. ) ;
#121529 = CARTESIAN_POINT ( 'NONE',  ( 18.59999999999999787, 76.00000000001267608, -203.5231074845243597 ) ) ;
#121531 = ADVANCED_FACE ( 'NONE', ( #172579 ), #74750, .T. ) ;
#121530 = CIRCLE ( 'NONE', #79776, 7.900000000000003908 ) ;
#121533 = CARTESIAN_POINT ( 'NONE',  ( -20.64999999999999858, 2.400000000011155432, -154.2753780772379173 ) ) ;
#121532 = VECTOR ( 'NONE', #252655, 1000.000000000000114 ) ;
#121534 = CARTESIAN_POINT ( 'NONE',  ( -18.40000000000000213, 16.38400329561159907, -222.2501914957450424 ) ) ;
#121535 = EDGE_LOOP ( 'NONE', ( #120697, #148856, #132658, #28910 ) ) ;
#121536 = EDGE_CURVE ( 'NONE', #93645, #129320, #163845, .T. ) ;
#121537 = ORIENTED_EDGE ( 'NONE', *, *, #230112, .T. ) ;
#121538 = AXIS2_PLACEMENT_3D ( 'NONE', #188785, #12749, #70157 ) ;
#121540 = AXIS2_PLACEMENT_3D ( 'NONE', #257379, #142611, #240451 ) ;
#121539 = DIRECTION ( 'NONE',  ( -1.020425574104004196E-15, 0.000000000000000000, 1.000000000000000000 ) ) ;
#121541 = DIRECTION ( 'NONE',  ( 0.000000000000000000, 0.000000000000000000, -1.000000000000000000 ) ) ;
#121542 = EDGE_CURVE ( 'NONE', #71501, #100213, #167969, .T. ) ;
#121543 = LINE ( 'NONE', #181500, #86999 ) ;
#121544 = FACE_OUTER_BOUND ( 'NONE', #236228, .T. ) ;
#121546 = FACE_OUTER_BOUND ( 'NONE', #175351, .T. ) ;
#121545 = DIRECTION ( 'NONE',  ( 0.000000000000000000, -0.9915357197604971473, 0.1298341882519111479 ) ) ;
#121547 = TOROIDAL_SURFACE ( 'NONE', #138243, 0.2000000000000000111, 0.1000000000000000056 ) ;
#121548 = DIRECTION ( 'NONE',  ( 0.000000000000000000, -0.9126074666063913599, -0.4088369013362965210 ) ) ;
#121550 = EDGE_CURVE ( 'NONE', #149698, #146995, #138498, .T. ) ;
#121549 = FACE_OUTER_BOUND ( 'NONE', #129791, .T. ) ;
#121553 = ADVANCED_FACE ( 'NONE', ( #176397 ), #80408, .T. ) ;
#121552 = DIRECTION ( 'NONE',  ( 0.000000000000000000, -0.9994937237965558774, -0.03181660087586650476 ) ) ;
#121551 = AXIS2_PLACEMENT_3D ( 'NONE', #186088, #246069, #122266 ) ;
#121554 = ORIENTED_EDGE ( 'NONE', *, *, #147470, .F. ) ;
#121555 = CARTESIAN_POINT ( 'NONE',  ( -20.64999999999999858, 7.150000000000000355, -21.25000000000000000 ) ) ;
#121556 = ORIENTED_EDGE ( 'NONE', *, *, #114700, .F. ) ;
#121557 = CARTESIAN_POINT ( 'NONE',  ( -20.94999999999999929, 64.40000000001208491, -129.5949042542488314 ) ) ;
#121558 = CARTESIAN_POINT ( 'NONE',  ( -18.40000000000000213, 11.33174054712517886, -20.85000000000000142 ) ) ;
#121560 = DIRECTION ( 'NONE',  ( -3.265361837132813093E-16, -1.000000000000000000, -6.982962677686266711E-15 ) ) ;
#121559 = CARTESIAN_POINT ( 'NONE',  ( -20.54999999999999716, 73.50000000001205080, -123.2984855617622202 ) ) ;
#121561 = AXIS2_PLACEMENT_3D ( 'NONE', #170619, #233131, #212272 ) ;
#121562 = ADVANCED_FACE ( 'NONE', ( #255861, #218041, #197214 ), #219339, .T. ) ;
#121563 = ORIENTED_EDGE ( 'NONE', *, *, #43180, .F. ) ;
#121565 = CARTESIAN_POINT ( 'NONE',  ( 20.94999999999999929, 1.115600667400684642E-11, -167.4999999999999716 ) ) ;
#121564 = CARTESIAN_POINT ( 'NONE',  ( -16.85697194749126382, 66.09145628588788668, -56.58810321691077405 ) ) ;
#121566 = DIRECTION ( 'NONE',  ( 0.7071067811865474617, -0.6824534298470372740, 0.1850873201762208153 ) ) ;
#121567 = CYLINDRICAL_SURFACE ( 'NONE', #13926, 0.09999999999998898659 ) ;
#121568 = CARTESIAN_POINT ( 'NONE',  ( 20.94999999999999929, 11.65000000001115943, -93.71613433702195550 ) ) ;
#121570 = CARTESIAN_POINT ( 'NONE',  ( -13.77083647240105257, 66.54258906972242471, -185.0231915757781564 ) ) ;
#121569 = AXIS2_PLACEMENT_3D ( 'NONE', #18019, #153744, #213661 ) ;
#121571 = VERTEX_POINT ( 'NONE', #81105 ) ;
#121572 = CARTESIAN_POINT ( 'NONE',  ( 20.94999999999999929, 76.00000000001244871, -170.0231074845243597 ) ) ;
#121573 = ADVANCED_FACE ( 'NONE', ( #77259 ), #158143, .F. ) ;
#121574 = ORIENTED_EDGE ( 'NONE', *, *, #185943, .F. ) ;
#121575 = EDGE_CURVE ( 'NONE', #63408, #224607, #217974, .T. ) ;
#121576 = CARTESIAN_POINT ( 'NONE',  ( 15.74999999999999645, 9.850000000011137402, -184.2499999999999716 ) ) ;
#121577 = ORIENTED_EDGE ( 'NONE', *, *, #156178, .T. ) ;
#121579 = DIRECTION ( 'NONE',  ( 0.000000000000000000, -0.4088369013362398441, 0.9126074666064164509 ) ) ;
#121578 = VECTOR ( 'NONE', #94607, 1000.000000000000000 ) ;
#121580 = CIRCLE ( 'NONE', #9112, 0.1000000000000028644 ) ;
#121581 = ORIENTED_EDGE ( 'NONE', *, *, #61789, .F. ) ;
#121582 = CIRCLE ( 'NONE', #9114, 0.1000000000000124678 ) ;
#121583 = DIRECTION ( 'NONE',  ( -1.000000000000000000, -0.000000000000000000, -0.000000000000000000 ) ) ;
#121584 = CIRCLE ( 'NONE', #104746, 4.049999999999998046 ) ;
#121585 = CARTESIAN_POINT ( 'NONE',  ( -21.05000000000000071, -11.48912529306490349, -170.4999999999999716 ) ) ;
#121586 = VERTEX_POINT ( 'NONE', #257139 ) ;
#121587 = EDGE_CURVE ( 'NONE', #251907, #177565, #133152, .T. ) ;
#121588 = FACE_OUTER_BOUND ( 'NONE', #224510, .T. ) ;
#121589 = CARTESIAN_POINT ( 'NONE',  ( 21.30740335185485890, 69.44334207798414127, -136.6220420103001914 ) ) ;
#121590 = DIRECTION ( 'NONE',  ( 0.000000000000000000, 6.982962677686266711E-15, -1.000000000000000000 ) ) ;
#121591 = CARTESIAN_POINT ( 'NONE',  ( -20.94999999999999929, 0.5876173420563349792, -209.1618981382189588 ) ) ;
#121592 = CARTESIAN_POINT ( 'NONE',  ( 19.81427058490550053, 62.44792297811893178, -208.9137562170004117 ) ) ;
#121593 = ORIENTED_EDGE ( 'NONE', *, *, #249887, .F. ) ;
#121594 = TOROIDAL_SURFACE ( 'NONE', #96586, 11.65000000000000036, 0.1000000000000000056 ) ;
#121595 = CARTESIAN_POINT ( 'NONE',  ( -22.59999999999999787, 31.80488924422933295, -238.9605610896540213 ) ) ;
#121596 = ORIENTED_EDGE ( 'NONE', *, *, #121810, .F. ) ;
#121598 = ORIENTED_EDGE ( 'NONE', *, *, #174907, .F. ) ;
#121597 = CARTESIAN_POINT ( 'NONE',  ( -16.89268316805466341, 66.04827818676967865, -90.37885996306994230 ) ) ;
#121599 = EDGE_LOOP ( 'NONE', ( #126442, #71696, #75493, #183352 ) ) ;
#121600 = CARTESIAN_POINT ( 'NONE',  ( 18.46921299892753510, -9.509378177823768041, -6.986578709370435014 ) ) ;
#121601 = CARTESIAN_POINT ( 'NONE',  ( 20.94999999999999574, 74.75000000001189449, -95.12310748452432563 ) ) ;
#121602 = FACE_OUTER_BOUND ( 'NONE', #148546, .T. ) ;
#121603 = SPHERICAL_SURFACE ( 'NONE', #116795, 0.1000000000000000056 ) ;
#121604 = ORIENTED_EDGE ( 'NONE', *, *, #154200, .T. ) ;
#121605 = CARTESIAN_POINT ( 'NONE',  ( -14.00000000000000178, 47.91805600923872532, -233.7139610577891631 ) ) ;
#121606 = DIRECTION ( 'NONE',  ( 0.000000000000000000, 6.769652589177795712E-15, -1.000000000000000000 ) ) ;
#121607 = EDGE_LOOP ( 'NONE', ( #17834, #220643, #83003, #136247, #219491, #164469 ) ) ;
#121608 = DIRECTION ( 'NONE',  ( -1.000000000000000000, 0.000000000000000000, -0.000000000000000000 ) ) ;
#121609 = EDGE_CURVE ( 'NONE', #111978, #237934, #67979, .T. ) ;
#121610 = CARTESIAN_POINT ( 'NONE',  ( -21.05000000000000071, -11.64999999998884306, -64.10000000000000853 ) ) ;
#121611 = VERTEX_POINT ( 'NONE', #118981 ) ;
#121612 = EDGE_CURVE ( 'NONE', #188436, #120661, #159392, .T. ) ;
#121613 = CARTESIAN_POINT ( 'NONE',  ( -16.88705144915419964, 9.950000000011137047, -146.9309785947120304 ) ) ;
#121614 = VECTOR ( 'NONE', #145176, 1000.000000000000000 ) ;
#121615 = FACE_OUTER_BOUND ( 'NONE', #235043, .T. ) ;
#121616 = VERTEX_POINT ( 'NONE', #21184 ) ;
#121617 = ADVANCED_FACE ( 'NONE', ( #61566, #98084 ), #79814, .T. ) ;
#121618 = EDGE_CURVE ( 'NONE', #89573, #58384, #109659, .T. ) ;
#121619 = CARTESIAN_POINT ( 'NONE',  ( 23.14999999999999858, 4.999999999999997335, -12.40526601891309788 ) ) ;
#121620 = FACE_OUTER_BOUND ( 'NONE', #31568, .T. ) ;
#121621 = CARTESIAN_POINT ( 'NONE',  ( -21.64999999999999858, 44.09459801588531036, -235.2076708599468020 ) ) ;
#121622 = B_SPLINE_CURVE_WITH_KNOTS ( 'NONE', 3,
 ( #207264, #3910, #221649, #143415, #202113, #67732, #182565, #44330, #82130, #104268 ),
 .UNSPECIFIED., .F., .F.,
 ( 4, 3, 3, 4 ),
 ( 7.632826238681267430E-06, 4.756916949875584252E-05, 9.484459048148792613E-05, 0.0001435500935099677739 ),
 .UNSPECIFIED. ) ;
#121623 = CONICAL_SURFACE ( 'NONE', #9173, 4.050000000000006040, 0.7853981633974604915 ) ;
#121624 = DIRECTION ( 'NONE',  ( 1.000000000000000000, 0.000000000000000000, 0.000000000000000000 ) ) ;
#121625 = CARTESIAN_POINT ( 'NONE',  ( 20.85000000000000142, -1.835859311432481045, -78.50443916879852679 ) ) ;
#121627 = ORIENTED_EDGE ( 'NONE', *, *, #67939, .T. ) ;
#121626 = CIRCLE ( 'NONE', #175783, 0.1000000000000008937 ) ;
#121628 = DIRECTION ( 'NONE',  ( -1.000000000000000000, -0.000000000000000000, -0.000000000000000000 ) ) ;
#121629 = ORIENTED_EDGE ( 'NONE', *, *, #203589, .T. ) ;
#121630 = DIRECTION ( 'NONE',  ( 0.000000000000000000, 0.2605042016806672911, -0.9654727137038716656 ) ) ;
#121631 = CARTESIAN_POINT ( 'NONE',  ( -16.98495255085919098, 60.88170416505755611, -221.0420300672591623 ) ) ;
#121633 = ORIENTED_EDGE ( 'NONE', *, *, #164804, .T. ) ;
#121632 = DIRECTION ( 'NONE',  ( -0.000000000000000000, -6.982962677686266711E-15, 1.000000000000000000 ) ) ;
#121634 = CARTESIAN_POINT ( 'NONE',  ( -23.25000000000000355, 64.25000000001210765, -127.2731074845243882 ) ) ;
#121635 = CARTESIAN_POINT ( 'NONE',  ( -21.05000000000000071, 87.29603075034744109, -139.5710066441881452 ) ) ;
#121636 = CARTESIAN_POINT ( 'NONE',  ( 21.09610168723072832, 75.96641049312049176, -109.4020631997490796 ) ) ;
#121637 = CARTESIAN_POINT ( 'NONE',  ( -16.83794237512074687, 9.926359221118632448, -79.80354215869901680 ) ) ;
#121638 = DIRECTION ( 'NONE',  ( -1.000000000000000000, 0.000000000000000000, -0.000000000000000000 ) ) ;
#121640 = EDGE_LOOP ( 'NONE', ( #135753, #20423, #77738, #154415 ) ) ;
#121639 = DIRECTION ( 'NONE',  ( -0.000000000000000000, 6.982962677686266711E-15, -1.000000000000000000 ) ) ;
#121641 = AXIS2_PLACEMENT_3D ( 'NONE', #212147, #154752, #15235 ) ;
#121642 = ADVANCED_FACE ( 'NONE', ( #237974 ), #201240, .T. ) ;
#121643 = CARTESIAN_POINT ( 'NONE',  ( -19.89999999999999858, 5.488301202077012775, 16.40000000000000213 ) ) ;
#121644 = ORIENTED_EDGE ( 'NONE', *, *, #1853, .T. ) ;
#121645 = ORIENTED_EDGE ( 'NONE', *, *, #80618, .T. ) ;
#121646 = B_SPLINE_CURVE_WITH_KNOTS ( 'NONE', 3,
 ( #28882, #103208, #62821, #86206 ),
 .UNSPECIFIED., .F., .F.,
 ( 4, 4 ),
 ( 0.000000000000000000, 0.0001048066582182356256 ),
 .UNSPECIFIED. ) ;
#121647 = CARTESIAN_POINT ( 'NONE',  ( -20.64999999999999858, 6.703231349641842307, -231.7785101893094577 ) ) ;
#121648 = ORIENTED_EDGE ( 'NONE', *, *, #24938, .T. ) ;
#121649 = EDGE_CURVE ( 'NONE', #111810, #188971, #122152, .T. ) ;
#121650 = DIRECTION ( 'NONE',  ( 0.000000000000000000, -0.1575844902526687130, -0.9875055080513762684 ) ) ;
#121651 = AXIS2_PLACEMENT_3D ( 'NONE', #37914, #157886, #59999 ) ;
#121652 = VECTOR ( 'NONE', #69591, 1000.000000000000000 ) ;
#121653 = ADVANCED_FACE ( 'NONE', ( #95891 ), #77600, .T. ) ;
#121654 = DIRECTION ( 'NONE',  ( 1.000000000000000000, -0.000000000000000000, 0.000000000000000000 ) ) ;
#121655 = CIRCLE ( 'NONE', #163169, 0.1000000000000028644 ) ;
#121656 = ORIENTED_EDGE ( 'NONE', *, *, #130200, .F. ) ;
#121657 = DIRECTION ( 'NONE',  ( 1.000000000000000000, 0.000000000000000000, 0.000000000000000000 ) ) ;
#121658 = PLANE ( 'NONE',  #230575 ) ;
#121659 = EDGE_CURVE ( 'NONE', #99817, #138284, #34678, .T. ) ;
#121660 = ORIENTED_EDGE ( 'NONE', *, *, #44668, .F. ) ;
#121661 = ORIENTED_EDGE ( 'NONE', *, *, #99036, .T. ) ;
#121662 = PLANE ( 'NONE',  #215197 ) ;
#121663 = VERTEX_POINT ( 'NONE', #37235 ) ;
#121664 = CARTESIAN_POINT ( 'NONE',  ( 20.85000000000000142, -1.135018845899022466, -208.7169768834322952 ) ) ;
#121665 = ORIENTED_EDGE ( 'NONE', *, *, #220452, .F. ) ;
#121667 = ORIENTED_EDGE ( 'NONE', *, *, #16936, .T. ) ;
#121666 = CARTESIAN_POINT ( 'NONE',  ( -21.05000000000000071, 68.22930980752001062, -227.7331931781284879 ) ) ;
#121668 = EDGE_CURVE ( 'NONE', #256377, #145620, #9701, .T. ) ;
#121669 = EDGE_CURVE ( 'NONE', #199005, #61045, #30583, .T. ) ;
#121670 = AXIS2_PLACEMENT_3D ( 'NONE', #86858, #169030, #208140 ) ;
#121671 = CARTESIAN_POINT ( 'NONE',  ( 21.05000000000000071, 7.128833340094563376, -233.7327013124401276 ) ) ;
#121672 = VERTEX_POINT ( 'NONE', #235404 ) ;
#121673 = DIRECTION ( 'NONE',  ( 1.000000000000000000, 0.000000000000000000, 0.000000000000000000 ) ) ;
#121674 = ORIENTED_EDGE ( 'NONE', *, *, #228823, .T. ) ;
#121676 = ORIENTED_EDGE ( 'NONE', *, *, #101129, .T. ) ;
#121675 = ORIENTED_EDGE ( 'NONE', *, *, #257492, .T. ) ;
#121677 = CYLINDRICAL_SURFACE ( 'NONE', #11441, 0.09999999999999990841 ) ;
#121678 = EDGE_CURVE ( 'NONE', #201031, #98769, #55456, .T. ) ;
#121679 = CARTESIAN_POINT ( 'NONE',  ( -20.95000000000002416, 56.23643450586806125, -227.9054833905874773 ) ) ;
#121680 = ORIENTED_EDGE ( 'NONE', *, *, #20948, .F. ) ;
#121681 = AXIS2_PLACEMENT_3D ( 'NONE', #77127, #174998, #75848 ) ;
#121682 = ORIENTED_EDGE ( 'NONE', *, *, #102335, .T. ) ;
#121683 = DIRECTION ( 'NONE',  ( -3.035766082959430717E-14, 0.000000000000000000, -1.000000000000000000 ) ) ;
#121684 = ADVANCED_FACE ( 'NONE', ( #178033 ), #97343, .T. ) ;
#121686 = DIRECTION ( 'NONE',  ( 0.000000000000000000, 0.000000000000000000, -1.000000000000000000 ) ) ;
#121685 = AXIS2_PLACEMENT_3D ( 'NONE', #1075, #117206, #18096 ) ;
#121688 = EDGE_LOOP ( 'NONE', ( #79662, #3337, #41598, #159145 ) ) ;
#121687 = DIRECTION ( 'NONE',  ( 0.000000000000000000, 0.000000000000000000, 1.000000000000000000 ) ) ;
#121689 = DIRECTION ( 'NONE',  ( 1.000000000000000000, 0.000000000000000000, -0.000000000000000000 ) ) ;
#121690 = ORIENTED_EDGE ( 'NONE', *, *, #210611, .T. ) ;
#121691 = DIRECTION ( 'NONE',  ( 0.000000000000000000, 6.982962677686266711E-15, -1.000000000000000000 ) ) ;
#121692 = DIRECTION ( 'NONE',  ( 0.000000000000000000, 0.5000000000000729417, 0.8660254037843965191 ) ) ;
#121693 = AXIS2_PLACEMENT_3D ( 'NONE', #154856, #12776, #51853 ) ;
#121694 = ORIENTED_EDGE ( 'NONE', *, *, #143138, .F. ) ;
#121695 = CARTESIAN_POINT ( 'NONE',  ( 20.94999999999999929, 69.56804783242856161, -248.4091712263733882 ) ) ;
#121696 = DIRECTION ( 'NONE',  ( -0.000000000000000000, -1.000000000000000000, -6.982962677686266711E-15 ) ) ;
#121697 = CYLINDRICAL_SURFACE ( 'NONE', #24053, 0.09999999999999939493 ) ;
#121698 = AXIS2_PLACEMENT_3D ( 'NONE', #80764, #237304, #57351 ) ;
#121700 = VERTEX_POINT ( 'NONE', #39820 ) ;
#121699 = CIRCLE ( 'NONE', #9251, 0.1000000000000028644 ) ;
#121701 = FACE_OUTER_BOUND ( 'NONE', #141249, .T. ) ;
#121702 = ORIENTED_EDGE ( 'NONE', *, *, #221293, .T. ) ;
#121703 = ORIENTED_EDGE ( 'NONE', *, *, #154025, .T. ) ;
#121704 = VECTOR ( 'NONE', #6356, 1000.000000000000000 ) ;
#121705 = EDGE_LOOP ( 'NONE', ( #112165, #123916, #81972, #102063, #250044, #223590, #252019 ) ) ;
#121706 = VERTEX_POINT ( 'NONE', #180586 ) ;
#121707 = DIRECTION ( 'NONE',  ( 0.000000000000000000, -0.8814952561688449428, 0.4721928772777310157 ) ) ;
#121708 = ORIENTED_EDGE ( 'NONE', *, *, #12893, .F. ) ;
#121709 = DIRECTION ( 'NONE',  ( 0.000000000000000000, 0.000000000000000000, 1.000000000000000000 ) ) ;
#121710 = ORIENTED_EDGE ( 'NONE', *, *, #100915, .T. ) ;
#121711 = DIRECTION ( 'NONE',  ( 0.000000000000000000, 6.982962677686266711E-15, -1.000000000000000000 ) ) ;
#121712 = AXIS2_PLACEMENT_3D ( 'NONE', #238168, #156115, #139043 ) ;
#121713 = DIRECTION ( 'NONE',  ( 0.000000000000000000, 0.8814952561688476074, -0.4721928772777262417 ) ) ;
#121714 = ORIENTED_EDGE ( 'NONE', *, *, #16147, .F. ) ;
#121715 = EDGE_LOOP ( 'NONE', ( #248721, #110441, #73386, #241967 ) ) ;
#121716 = AXIS2_PLACEMENT_3D ( 'NONE', #178068, #99765, #20270 ) ;
#121717 = VECTOR ( 'NONE', #59807, 1000.000000000000000 ) ;
#121718 = AXIS2_PLACEMENT_3D ( 'NONE', #243315, #85494, #217641 ) ;
#121719 = ORIENTED_EDGE ( 'NONE', *, *, #132347, .F. ) ;
#121720 = ADVANCED_FACE ( 'NONE', ( #119330 ), #20237, .T. ) ;
#121721 = CIRCLE ( 'NONE', #105092, 0.1000000000000035305 ) ;
#121722 = CARTESIAN_POINT ( 'NONE',  ( 21.05000000000000071, 69.52244781751886649, -203.4231075192253115 ) ) ;
#121724 = ADVANCED_FACE ( 'NONE', ( #1920 ), #56742, .T. ) ;
#121723 = AXIS2_PLACEMENT_3D ( 'NONE', #25727, #67415, #127397 ) ;
#121725 = LINE ( 'NONE', #216936, #126106 ) ;
#121726 = CARTESIAN_POINT ( 'NONE',  ( -20.85000000106584750, 11.75000000001115197, -127.1555046564734113 ) ) ;
#121727 = CARTESIAN_POINT ( 'NONE',  ( 21.05000000000000071, 65.49746832288732890, -162.4642776674505171 ) ) ;
#121728 = CYLINDRICAL_SURFACE ( 'NONE', #131828, 0.09999999999999939493 ) ;
#121729 = CARTESIAN_POINT ( 'NONE',  ( -5.899999999999938183, 64.25000000001119815, -21.92310748452479174 ) ) ;
#121730 = EDGE_CURVE ( 'NONE', #19594, #229988, #175469, .T. ) ;
#121732 = CARTESIAN_POINT ( 'NONE',  ( 21.08884785362045378, 6.357193367436396514, -100.4502169049331997 ) ) ;
#121731 = DIRECTION ( 'NONE',  ( -1.000000000000000000, -0.000000000000000000, -0.000000000000000000 ) ) ;
#121734 = ADVANCED_FACE ( 'NONE', ( #179323 ), #222248, .T. ) ;
#121733 = DIRECTION ( 'NONE',  ( -1.000000000000000000, 0.000000000000000000, 0.000000000000000000 ) ) ;
#121735 = FACE_OUTER_BOUND ( 'NONE', #33864, .T. ) ;
#121736 = CARTESIAN_POINT ( 'NONE',  ( -20.94999999999999929, 87.48912529308842068, -167.0231074845242745 ) ) ;
#121737 = CARTESIAN_POINT ( 'NONE',  ( -20.94999999999999929, -11.48912529306489994, -198.0999999999999659 ) ) ;
#121738 = CIRCLE ( 'NONE', #238234, 0.5000000000000004441 ) ;
#121740 = EDGE_LOOP ( 'NONE', ( #30987, #90681, #94407, #231324 ) ) ;
#121739 = AXIS2_PLACEMENT_3D ( 'NONE', #18915, #56725, #38494 ) ;
#121741 = VECTOR ( 'NONE', #45447, 1000.000000000000227 ) ;
#121743 = ORIENTED_EDGE ( 'NONE', *, *, #244793, .F. ) ;
#121742 = CARTESIAN_POINT ( 'NONE',  ( 21.05000000000000426, 10.72371710471867701, -108.0944173916131774 ) ) ;
#121744 = ORIENTED_EDGE ( 'NONE', *, *, #64860, .T. ) ;
#121745 = EDGE_CURVE ( 'NONE', #180641, #8118, #256193, .T. ) ;
#121746 = DIRECTION ( 'NONE',  ( 0.000000000000000000, 0.000000000000000000, -1.000000000000000000 ) ) ;
#121747 =( BOUNDED_CURVE ( )  B_SPLINE_CURVE ( 3, ( #218412, #254929, #16405, #217122 ),
 .UNSPECIFIED., .F., .T. ) 
 B_SPLINE_CURVE_WITH_KNOTS ( ( 4, 4 ),
 ( 3.141592653589791784, 4.712388980384688786 ),
 .UNSPECIFIED. ) 
 CURVE ( )  GEOMETRIC_REPRESENTATION_ITEM ( )  RATIONAL_B_SPLINE_CURVE ( ( 1.000000000000000000, 0.8047378541243649375, 0.8047378541243649375, 1.000000000000000000 ) ) 
 REPRESENTATION_ITEM ( '' )  );
#121748 = EDGE_CURVE ( 'NONE', #54519, #205409, #14006, .T. ) ;
#121749 = DIRECTION ( 'NONE',  ( 1.000000000000000000, 0.000000000000000000, 0.000000000000000000 ) ) ;
#121750 = ORIENTED_EDGE ( 'NONE', *, *, #128961, .F. ) ;
#121751 = FILL_AREA_STYLE_COLOUR ( '', #255908 ) ;
#121752 = PRODUCT_DEFINITION ( 'UNKNOWN', '', #90450, #84306 ) ;
#121753 = DIRECTION ( 'NONE',  ( -1.000000000000000000, 0.000000000000000000, 0.000000000000000000 ) ) ;
#121754 = CYLINDRICAL_SURFACE ( 'NONE', #170335, 0.09999999999999939493 ) ;
#121755 = AXIS2_PLACEMENT_3D ( 'NONE', #138101, #178565, #139382 ) ;
#121756 = ORIENTED_EDGE ( 'NONE', *, *, #159921, .F. ) ;
#121757 = CARTESIAN_POINT ( 'NONE',  ( -18.59999999999999787, 10.33248238083634440, -206.5948465439131496 ) ) ;
#121758 = CARTESIAN_POINT ( 'NONE',  ( -20.85000000000000142, 7.021664781900089913, -37.33356540189728889 ) ) ;
#121759 = CARTESIAN_POINT ( 'NONE',  ( -18.59999999999999787, 59.16775194334852728, -221.0793150863668473 ) ) ;
#121760 =( BOUNDED_SURFACE ( )  B_SPLINE_SURFACE ( 3, 2, ( 
 ( #113373, #174682, #192916 ),
 ( #177226, #237177, #93797 ),
 ( #213751, #35159, #114654 ),
 ( #194220, #254146, #75553 ),
 ( #155099, #234596, #44104 ),
 ( #164058, #181064, #158943 ),
 ( #118527, #203169, #101455 ),
 ( #102763, #238451, #61092 ),
 ( #222721, #81904, #182344 ),
 ( #3680, #104045, #199338 ) ),
 .UNSPECIFIED., .F., .F., .F. ) 
 B_SPLINE_SURFACE_WITH_KNOTS ( ( 4, 2, 2, 2, 4 ),
 ( 3, 3 ),
 ( 0.0001701955120502369480, 0.0002247052511886141093, 0.0002792149903269912706, 0.0003882344686037456473, 0.0006062734251572542924 ),
 ( 0.000000000000000000, 1.000000000000000000 ),
 .UNSPECIFIED. ) 
 GEOMETRIC_REPRESENTATION_ITEM ( )  RATIONAL_B_SPLINE_SURFACE ( (
 ( 1.000000000000000000, 0.2966190024561626837, 1.000000000000000000),
 ( 1.000000000000000000, 0.2964522492704476098, 1.000000000000000000),
 ( 1.000000000000000000, 0.3059923531893983806, 1.000000000000000000),
 ( 1.000000000000000000, 0.3355751146934523033, 1.000000000000000000),
 ( 1.000000000000000000, 0.3550672384964473349, 1.000000000000000000),
 ( 1.000000000000000000, 0.4157034672179019674, 1.000000000000000000),
 ( 1.000000000000000000, 0.4588031877652369306, 1.000000000000000000),
 ( 1.000000000000000000, 0.5771441759665676408, 1.000000000000000000),
 ( 1.000000000000000000, 0.6469377121768183914, 1.000000000000000000),
 ( 1.000000000000000000, 0.7071067811865376918, 1.000000000000000000) ) ) 
 REPRESENTATION_ITEM ( '' )  SURFACE ( )  );
#121761 = EDGE_CURVE ( 'NONE', #242144, #3656, #115461, .T. ) ;
#121762 = EDGE_CURVE ( 'NONE', #137271, #6219, #135874, .T. ) ;
#121763 = CARTESIAN_POINT ( 'NONE',  ( 18.55857864376268296, 15.39652800355464279, -222.9769737602899227 ) ) ;
#121765 = ORIENTED_EDGE ( 'NONE', *, *, #107818, .F. ) ;
#121764 = CARTESIAN_POINT ( 'NONE',  ( -20.90851465518105812, 67.49261718274587452, -195.4446851895584416 ) ) ;
#121766 = EDGE_CURVE ( 'NONE', #187076, #43421, #5770, .T. ) ;
#121767 = FACE_OUTER_BOUND ( 'NONE', #184868, .T. ) ;
#121769 = VERTEX_POINT ( 'NONE', #104853 ) ;
#121768 = DIRECTION ( 'NONE',  ( 0.000000000000000000, -6.938893903907222067E-15, 1.000000000000000000 ) ) ;
#121770 = DIRECTION ( 'NONE',  ( 0.000000000000000000, 0.8814952561688438326, -0.4721928772777331806 ) ) ;
#121771 = CARTESIAN_POINT ( 'NONE',  ( -23.15000000000000213, 87.48912529308852015, -173.0231074845243029 ) ) ;
#121772 = CARTESIAN_POINT ( 'NONE',  ( -18.39999999999999858, 11.47316190337362762, -76.32594606680801519 ) ) ;
#121773 = CARTESIAN_POINT ( 'NONE',  ( -12.84409460144753901, 9.410682294279109072, -182.9311434419482225 ) ) ;
#121775 = CARTESIAN_POINT ( 'NONE',  ( 18.79999999999999716, -1.467286812112899463, 28.00000000000000000 ) ) ;
#121774 = CARTESIAN_POINT ( 'NONE',  ( -21.14999999999999858, 11.75000000001115552, -100.5000000000000284 ) ) ;
#121776 = DIRECTION ( 'NONE',  ( 4.026293107431335996E-15, -0.8700118002898359348, 0.4930308989875165082 ) ) ;
#121777 = EDGE_CURVE ( 'NONE', #178174, #15176, #202707, .T. ) ;
#121778 = CARTESIAN_POINT ( 'NONE',  ( -20.85000000000000142, 68.97833521811179480, -99.18954208262705663 ) ) ;
#121779 = DIRECTION ( 'NONE',  ( 0.000000000000000000, 0.000000000000000000, 1.000000000000000000 ) ) ;
#121780 = ORIENTED_EDGE ( 'NONE', *, *, #9684, .T. ) ;
#121782 = AXIS2_PLACEMENT_3D ( 'NONE', #110276, #34627, #11191 ) ;
#121781 = CARTESIAN_POINT ( 'NONE',  ( 23.24999999999999289, 69.35000000001200249, -115.1731074845243512 ) ) ;
#121783 = ORIENTED_EDGE ( 'NONE', *, *, #250512, .F. ) ;
#121784 = ORIENTED_EDGE ( 'NONE', *, *, #150347, .F. ) ;
#121785 = CARTESIAN_POINT ( 'NONE',  ( 20.94999999999999929, 6.450000000000001066, -10.01702717044001822 ) ) ;
#121786 = CARTESIAN_POINT ( 'NONE',  ( -23.15000000000000213, 1.115600667400684642E-11, -167.5000000000000284 ) ) ;
#121787 = VERTEX_POINT ( 'NONE', #67062 ) ;
#121789 = EDGE_CURVE ( 'NONE', #64899, #184752, #103587, .T. ) ;
#121788 = EDGE_LOOP ( 'NONE', ( #247317, #89517, #143510, #112374 ) ) ;
#121790 = AXIS2_PLACEMENT_3D ( 'NONE', #11508, #250106, #131430 ) ;
#121791 = ORIENTED_EDGE ( 'NONE', *, *, #33898, .T. ) ;
#121792 = CARTESIAN_POINT ( 'NONE',  ( 20.95443524775735256, 8.878554263883966513, -75.53372227560019780 ) ) ;
#121793 = ORIENTED_EDGE ( 'NONE', *, *, #142941, .F. ) ;
#121794 = AXIS2_PLACEMENT_3D ( 'NONE', #249226, #90121, #190551 ) ;
#121795 = DIRECTION ( 'NONE',  ( 0.000000000000000000, 1.000000000000000000, -0.000000000000000000 ) ) ;
#121796 = CARTESIAN_POINT ( 'NONE',  ( -22.47071067811865319, 0.09909245470260577560, 7.720074744498064412 ) ) ;
#121797 = DIRECTION ( 'NONE',  ( 1.000000000000000000, 0.000000000000000000, 0.000000000000000000 ) ) ;
#121798 = DIRECTION ( 'NONE',  ( 1.000000000000000000, 0.000000000000000000, 0.000000000000000000 ) ) ;
#121799 = CIRCLE ( 'NONE', #76003, 0.1000000000000028644 ) ;
#121800 = EDGE_CURVE ( 'NONE', #140759, #159539, #93090, .T. ) ;
#121801 = CARTESIAN_POINT ( 'NONE',  ( 21.05000000000000071, 7.128833340093095217, -233.7327013124392749 ) ) ;
#121802 = LINE ( 'NONE', #83895, #132656 ) ;
#121803 = ORIENTED_EDGE ( 'NONE', *, *, #108019, .T. ) ;
#121805 = CARTESIAN_POINT ( 'NONE',  ( 18.47149038651511432, 85.67145715801805750, -29.35032114978585227 ) ) ;
#121804 = CARTESIAN_POINT ( 'NONE',  ( -17.80356949363990182, 62.80985299201304173, -210.6043626271361973 ) ) ;
#121806 = DIRECTION ( 'NONE',  ( -1.000000000000000000, -0.000000000000000000, -0.000000000000000000 ) ) ;
#121807 = ORIENTED_EDGE ( 'NONE', *, *, #51760, .T. ) ;
#121808 = DIRECTION ( 'NONE',  ( 1.000000000000000000, 3.265361837132813093E-16, -0.000000000000000000 ) ) ;
#121810 = EDGE_CURVE ( 'NONE', #76759, #193899, #213906, .T. ) ;
#121809 = DIRECTION ( 'NONE',  ( 0.000000000000000000, 6.982962677686266711E-15, -1.000000000000000000 ) ) ;
#121811 = ORIENTED_EDGE ( 'NONE', *, *, #233913, .F. ) ;
#121812 = AXIS2_PLACEMENT_3D ( 'NONE', #187154, #106282, #7190 ) ;
#121815 = CARTESIAN_POINT ( 'NONE',  ( 21.46681500598040415, 76.00000000001170974, -76.38061864395039890 ) ) ;
#121814 = AXIS2_PLACEMENT_3D ( 'NONE', #234530, #254084, #35096 ) ;
#121813 = CARTESIAN_POINT ( 'NONE',  ( -20.64999999999999858, 2.500000000000000444, -13.22462192276210224 ) ) ;
#121816 = CARTESIAN_POINT ( 'NONE',  ( -21.76363531954647357, 75.90099812571254745, -110.0360440323960631 ) ) ;
#121817 = ORIENTED_EDGE ( 'NONE', *, *, #3911, .T. ) ;
#121818 = EDGE_CURVE ( 'NONE', #136044, #216000, #106159, .T. ) ;
#121819 = DIRECTION ( 'NONE',  ( 1.000000000000000000, 0.000000000000000000, 0.000000000000000000 ) ) ;
#121821 = ADVANCED_FACE ( 'NONE', ( #42359 ), #8377, .F. ) ;
#121820 = DIRECTION ( 'NONE',  ( -0.000000000000000000, 1.000000000000000000, -0.000000000000000000 ) ) ;
#121822 = AXIS2_PLACEMENT_3D ( 'NONE', #100405, #3899, #221638 ) ;
#121823 = CARTESIAN_POINT ( 'NONE',  ( -22.45437739390953880, 1.115488181425289271E-11, -21.85042918840543535 ) ) ;
#121824 = CARTESIAN_POINT ( 'NONE',  ( -22.50047199487803695, 0.04490605193026415975, -122.2499525810811321 ) ) ;
#121825 = ORIENTED_EDGE ( 'NONE', *, *, #137120, .F. ) ;
#121826 = AXIS2_PLACEMENT_3D ( 'NONE', #202635, #117961, #123114 ) ;
#121827 = B_SPLINE_CURVE_WITH_KNOTS ( 'NONE', 3,
 ( #154592, #94573, #252356, #170321, #11203, #230241, #249814, #35918, #76290, #235367 ),
 .UNSPECIFIED., .F., .F.,
 ( 4, 3, 3, 4 ),
 ( 0.000000000000000000, 0.0002000000000008585893, 0.001000000000082977483, 0.001967863649483336721 ),
 .UNSPECIFIED. ) ;
#121828 = CIRCLE ( 'NONE', #105191, 11.64999999999999325 ) ;
#121829 = CIRCLE ( 'NONE', #9378, 0.09999999999999939493 ) ;
#121830 = DIRECTION ( 'NONE',  ( -0.000000000000000000, 0.4721928772777345684, 0.8814952561688429444 ) ) ;
#121831 = LINE ( 'NONE', #201348, #254916 ) ;
#121832 = FACE_OUTER_BOUND ( 'NONE', #138510, .T. ) ;
#121834 = ADVANCED_FACE ( 'NONE', ( #85302 ), #47470, .T. ) ;
#121833 = CARTESIAN_POINT ( 'NONE',  ( 22.10000000000000142, -1.467286812112899463, 28.00000000000000000 ) ) ;
#121836 = ORIENTED_EDGE ( 'NONE', *, *, #48546, .T. ) ;
#121835 = CARTESIAN_POINT ( 'NONE',  ( -21.37071067811865532, 8.070710678129811910, -121.7500000000000426 ) ) ;
#121837 = DIRECTION ( 'NONE',  ( 2.952720810173289112E-16, -1.000000000000000000, 0.000000000000000000 ) ) ;
#121838 = LINE ( 'NONE', #219627, #194777 ) ;
#121839 = CARTESIAN_POINT ( 'NONE',  ( -21.07928932188134041, 75.90110485435729970, -75.85162414091762173 ) ) ;
#121840 = CARTESIAN_POINT ( 'NONE',  ( 21.05000000000000426, 6.413826288824131971, -167.5857409370333926 ) ) ;
#121841 = ADVANCED_FACE ( 'NONE', ( #244400 ), #181873, .F. ) ;
#121843 = ORIENTED_EDGE ( 'NONE', *, *, #139163, .T. ) ;
#121842 = CARTESIAN_POINT ( 'NONE',  ( -13.39999999999994529, 67.75000000001118394, -21.02310748452479316 ) ) ;
#121844 = DIRECTION ( 'NONE',  ( -1.000000000000000000, 0.000000000000000000, 0.000000000000000000 ) ) ;
#121845 = DIRECTION ( 'NONE',  ( 0.000000000000000000, 0.000000000000000000, 1.000000000000000000 ) ) ;
#121846 = CARTESIAN_POINT ( 'NONE',  ( 23.24999999999999289, 4.150000000011154988, -167.4999999999999716 ) ) ;
#121847 = ORIENTED_EDGE ( 'NONE', *, *, #123775, .F. ) ;
#121848 = DIRECTION ( 'NONE',  ( -1.000000000000000000, 0.000000000000000000, 0.000000000000000000 ) ) ;
#121849 = CARTESIAN_POINT ( 'NONE',  ( 21.05000000000000071, 76.08559286337477090, -176.4367702193935656 ) ) ;
#121850 = ADVANCED_FACE ( 'NONE', ( #86588 ), #87874, .F. ) ;
#121851 = DIRECTION ( 'NONE',  ( 0.000000000000000000, 0.9893560106964510714, -0.1455152366551481502 ) ) ;
#121852 = EDGE_CURVE ( 'NONE', #13038, #196986, #126418, .T. ) ;
#121853 = AXIS2_PLACEMENT_3D ( 'NONE', #151760, #14820, #115177 ) ;
#121854 = DIRECTION ( 'NONE',  ( 0.000000000000000000, -1.000000000000000000, 0.000000000000000000 ) ) ;
#121855 = AXIS2_PLACEMENT_3D ( 'NONE', #146083, #169560, #5268 ) ;
#121856 = CARTESIAN_POINT ( 'NONE',  ( -16.83558968593875349, 9.950000000011137047, -87.83769481238333299 ) ) ;
#121857 = ORIENTED_EDGE ( 'NONE', *, *, #211614, .F. ) ;
#121858 = ORIENTED_EDGE ( 'NONE', *, *, #198268, .F. ) ;
#121859 = FACE_OUTER_BOUND ( 'NONE', #197364, .T. ) ;
#121860 = CARTESIAN_POINT ( 'NONE',  ( 23.14999999999999503, 69.35000000001200249, -115.3731074845243398 ) ) ;
#121861 = CARTESIAN_POINT ( 'NONE',  ( -20.54999999999999716, 70.71284696581484752, -215.3770916356353382 ) ) ;
#121862 = DIRECTION ( 'NONE',  ( 0.000000000000000000, 1.000000000000000000, 0.000000000000000000 ) ) ;
#121863 = VERTEX_POINT ( 'NONE', #124476 ) ;
#121864 = EDGE_CURVE ( 'NONE', #88270, #105026, #64060, .T. ) ;
#121865 = EDGE_CURVE ( 'NONE', #40848, #76927, #65769, .T. ) ;
#121866 = CARTESIAN_POINT ( 'NONE',  ( 20.95203847575071521, 10.50106053928516303, -175.0670713486235002 ) ) ;
#121867 = AXIS2_PLACEMENT_3D ( 'NONE', #103812, #106381, #43871 ) ;
#121868 = DIRECTION ( 'NONE',  ( 0.000000000000000000, -1.000000000000000000, 0.000000000000000000 ) ) ;
#121869 = CIRCLE ( 'NONE', #163553, 1.749999999999999778 ) ;
#121870 = CYLINDRICAL_SURFACE ( 'NONE', #4008, 0.1000000000000028644 ) ;
#121871 = CIRCLE ( 'NONE', #142682, 0.1999999999999996503 ) ;
#121872 = AXIS2_PLACEMENT_3D ( 'NONE', #123960, #84782, #203489 ) ;
#121873 = DIRECTION ( 'NONE',  ( 0.000000000000000000, -6.982962677686266711E-15, 1.000000000000000000 ) ) ;
#121874 = DIRECTION ( 'NONE',  ( -1.000000000000000000, 0.000000000000000000, 0.000000000000000000 ) ) ;
#121876 = DIRECTION ( 'NONE',  ( -0.000000000000000000, -0.000000000000000000, 1.000000000000000000 ) ) ;
#121875 = AXIS2_PLACEMENT_3D ( 'NONE', #36222, #209706, #11519 ) ;
#121877 = ORIENTED_EDGE ( 'NONE', *, *, #44358, .F. ) ;
#121879 = ORIENTED_EDGE ( 'NONE', *, *, #224218, .F. ) ;
#121878 = CARTESIAN_POINT ( 'NONE',  ( 18.69999999999999574, -9.849999999999990763, 31.50000000000000000 ) ) ;
#121880 = CIRCLE ( 'NONE', #221793, 0.1000000000000028644 ) ;
#121881 = ORIENTED_EDGE ( 'NONE', *, *, #118912, .F. ) ;
#121882 = DIRECTION ( 'NONE',  ( 0.000000000000000000, 0.5859227990963362664, 0.8103668758649469339 ) ) ;
#121883 = EDGE_LOOP ( 'NONE', ( #196462, #197904, #77150, #247257, #44150, #2149, #72203, #27835 ) ) ;
#121884 = CARTESIAN_POINT ( 'NONE',  ( -17.04295772865474490, 10.02489942527111388, -154.8500000000000227 ) ) ;
#121885 = CARTESIAN_POINT ( 'NONE',  ( -21.05000000000000071, 6.258842723548828424, -100.4679863068123211 ) ) ;
#121886 = FACE_OUTER_BOUND ( 'NONE', #54560, .T. ) ;
#121887 = ORIENTED_EDGE ( 'NONE', *, *, #31842, .F. ) ;
#121888 = DIRECTION ( 'NONE',  ( 0.000000000000000000, -6.982962677686266711E-15, 1.000000000000000000 ) ) ;
#121889 = CARTESIAN_POINT ( 'NONE',  ( 21.05000000000000071, 1.115600667400684642E-11, -46.47500000000000142 ) ) ;
#121890 = VECTOR ( 'NONE', #167356, 1000.000000000000000 ) ;
#121891 = ORIENTED_EDGE ( 'NONE', *, *, #128003, .T. ) ;
#121892 = LINE ( 'NONE', #99713, #8384 ) ;
#121893 = CIRCLE ( 'NONE', #146976, 12.97499999999998899 ) ;
#121895 = ORIENTED_EDGE ( 'NONE', *, *, #130199, .F. ) ;
#121894 = CARTESIAN_POINT ( 'NONE',  ( -20.65000000000000568, 68.75000000001256240, -182.6731074845244223 ) ) ;
#121896 = DIRECTION ( 'NONE',  ( 1.000000000000000000, 0.000000000000000000, 0.000000000000000000 ) ) ;
#121897 = DIRECTION ( 'NONE',  ( 0.000000000000000000, 6.982962677686266711E-15, -1.000000000000000000 ) ) ;
#121898 = AXIS2_PLACEMENT_3D ( 'NONE', #164387, #243904, #66571 ) ;
#121899 = ADVANCED_FACE ( 'NONE', ( #245695 ), #27968, .T. ) ;
#121900 = VERTEX_POINT ( 'NONE', #127029 ) ;
#121901 = AXIS2_PLACEMENT_3D ( 'NONE', #126971, #13454, #66994 ) ;
#121902 = CARTESIAN_POINT ( 'NONE',  ( -16.77828822508139694, 9.946229374931901290, -79.66262825137400228 ) ) ;
#121903 = CARTESIAN_POINT ( 'NONE',  ( -20.54999999999999716, 73.50000000001180922, -82.74772940728642823 ) ) ;
#121904 = LINE ( 'NONE', #97139, #193090 ) ;
#121905 = ORIENTED_EDGE ( 'NONE', *, *, #37964, .T. ) ;
#121906 = CARTESIAN_POINT ( 'NONE',  ( -20.54999999999999716, 85.00000000001222134, -146.4170766071767389 ) ) ;
#121907 = AXIS2_PLACEMENT_3D ( 'NONE', #67202, #47615, #249696 ) ;
#121908 = CARTESIAN_POINT ( 'NONE',  ( 23.25000000000000000, -11.64999999998883595, -164.4000000000000057 ) ) ;
#121909 = CARTESIAN_POINT ( 'NONE',  ( -21.05000000000000071, 70.56573376625485139, -228.3808404818380779 ) ) ;
#121910 = ORIENTED_EDGE ( 'NONE', *, *, #95299, .F. ) ;
#121911 = ADVANCED_FACE ( 'NONE', ( #149186 ), #91759, .F. ) ;
#121912 = VECTOR ( 'NONE', #106417, 1000.000000000000000 ) ;
#121913 = AXIS2_PLACEMENT_3D ( 'NONE', #151745, #195995, #56450 ) ;
#121914 = AXIS2_PLACEMENT_3D ( 'NONE', #71143, #193640, #55366 ) ;
#121915 = ORIENTED_EDGE ( 'NONE', *, *, #26907, .T. ) ;
#121916 = EDGE_LOOP ( 'NONE', ( #129090, #255862, #16670, #69083 ) ) ;
#121917 = LINE ( 'NONE', #201432, #151785 ) ;
#121918 = DIRECTION ( 'NONE',  ( 0.000000000000000000, -1.000000000000000000, 0.000000000000000000 ) ) ;
#121920 = ORIENTED_EDGE ( 'NONE', *, *, #111377, .F. ) ;
#121919 = PLANE ( 'NONE',  #120972 ) ;
#121921 = CYLINDRICAL_SURFACE ( 'NONE', #7632, 0.09999999999999892308 ) ;
#121922 = CARTESIAN_POINT ( 'NONE',  ( -22.57320508075686050, 11.48087284840414490, -198.4995883060918231 ) ) ;
#121923 = CARTESIAN_POINT ( 'NONE',  ( -16.89208623190940273, 51.62302926044408480, -231.9428734964056389 ) ) ;
#121924 = CARTESIAN_POINT ( 'NONE',  ( 23.14999999999999503, 11.65000000000000746, -26.48519422934606027 ) ) ;
#121925 = FACE_OUTER_BOUND ( 'NONE', #128045, .T. ) ;
#121927 = ORIENTED_EDGE ( 'NONE', *, *, #66715, .T. ) ;
#121926 = CARTESIAN_POINT ( 'NONE',  ( 20.94999999999999574, 69.60000000001261355, -193.5926828544628222 ) ) ;
#121929 = VERTEX_POINT ( 'NONE', #207883 ) ;
#121928 = CARTESIAN_POINT ( 'NONE',  ( -21.05000000000000071, 70.53171716061257257, -228.4612385850772682 ) ) ;
#121930 = CARTESIAN_POINT ( 'NONE',  ( 22.45305468355010348, -0.1008583690885486023, -55.25043287651032387 ) ) ;
#121931 = ORIENTED_EDGE ( 'NONE', *, *, #249591, .F. ) ;
#121932 = ORIENTED_EDGE ( 'NONE', *, *, #162515, .T. ) ;
#121933 = DIRECTION ( 'NONE',  ( 0.000000000000000000, -1.000000000000000000, 0.000000000000000000 ) ) ;
#121934 = CARTESIAN_POINT ( 'NONE',  ( -21.05000000000000071, 76.00000000001142553, -36.02310748452432421 ) ) ;
#121935 = TOROIDAL_SURFACE ( 'NONE', #76131, 0.6000000000000013101, 0.1000000000000000056 ) ;
#121936 = SPHERICAL_SURFACE ( 'NONE', #52690, 0.1000000000000000056 ) ;
#121937 = CARTESIAN_POINT ( 'NONE',  ( 20.94999999999999929, 0.000000000000000000, 0.000000000000000000 ) ) ;
#121938 = CARTESIAN_POINT ( 'NONE',  ( -18.59999999999999787, 7.128833340094563376, -233.7327013124401276 ) ) ;
#121939 = VERTEX_POINT ( 'NONE', #48772 ) ;
#121940 = DIRECTION ( 'NONE',  ( 0.000000000000000000, -0.9887567792719351711, 0.1495327102803594987 ) ) ;
#121941 = VERTEX_POINT ( 'NONE', #33115 ) ;
#121942 = ORIENTED_EDGE ( 'NONE', *, *, #45412, .F. ) ;
#121943 = ADVANCED_FACE ( 'NONE', ( #29261 ), #8292, .T. ) ;
#121944 = ORIENTED_EDGE ( 'NONE', *, *, #73310, .F. ) ;
#121945 = FACE_OUTER_BOUND ( 'NONE', #80172, .T. ) ;
#121946 = AXIS2_PLACEMENT_3D ( 'NONE', #195962, #18596, #237645 ) ;
#121947 = CARTESIAN_POINT ( 'NONE',  ( -18.39999999999999858, 86.89640087696872683, -199.6396878666313341 ) ) ;
#121948 = EDGE_CURVE ( 'NONE', #126189, #88113, #155679, .T. ) ;
#121949 = ORIENTED_EDGE ( 'NONE', *, *, #129135, .T. ) ;
#121950 = CARTESIAN_POINT ( 'NONE',  ( 21.05000000000000071, 70.15000000001211333, -126.3906102602463619 ) ) ;
#121951 = VERTEX_POINT ( 'NONE', #69643 ) ;
#121952 = CARTESIAN_POINT ( 'NONE',  ( -12.60206096961792532, 9.389686005666810331, -49.17284350635132029 ) ) ;
#121953 = ORIENTED_EDGE ( 'NONE', *, *, #237634, .F. ) ;
#121954 = EDGE_CURVE ( 'NONE', #40045, #125547, #248265, .T. ) ;
#121955 = DIRECTION ( 'NONE',  ( 0.000000000000000000, 0.000000000000000000, 1.000000000000000000 ) ) ;
#121956 = FACE_OUTER_BOUND ( 'NONE', #255790, .T. ) ;
#121957 = ORIENTED_EDGE ( 'NONE', *, *, #136993, .F. ) ;
#121958 = CARTESIAN_POINT ( 'NONE',  ( 18.59999999999999076, 43.00579525902548994, -254.2551217332645876 ) ) ;
#121959 = ADVANCED_FACE ( 'NONE', ( #210438 ), #192164, .T. ) ;
#121961 = VERTEX_POINT ( 'NONE', #188282 ) ;
#121960 = CARTESIAN_POINT ( 'NONE',  ( -23.15000000000000213, 48.31748480764120046, -244.3282712866738962 ) ) ;
#121962 = CARTESIAN_POINT ( 'NONE',  ( 18.49999999999999645, 64.18627039993180006, -224.3513032416919089 ) ) ;
#121963 = EDGE_LOOP ( 'NONE', ( #175429, #7866, #108689, #215476 ) ) ;
#121964 = AXIS2_PLACEMENT_3D ( 'NONE', #60963, #144328, #140493 ) ;
#121965 = CARTESIAN_POINT ( 'NONE',  ( 21.05000000000000071, 0.000000000000000000, 0.000000000000000000 ) ) ;
#121966 = ORIENTED_EDGE ( 'NONE', *, *, #83450, .F. ) ;
#121967 = CARTESIAN_POINT ( 'NONE',  ( 23.40000000000005542, 74.83745509109094485, -43.92310748452479885 ) ) ;
#121968 = ADVANCED_FACE ( 'NONE', ( #133451 ), #172632, .F. ) ;
#121969 = CARTESIAN_POINT ( 'NONE',  ( 22.49806830649813350, 25.99547786654754589, -254.2433729751658120 ) ) ;
#121970 = DIRECTION ( 'NONE',  ( 1.186688945009010077E-16, 1.000000000000000000, 6.982962677686266711E-15 ) ) ;
#121971 = CARTESIAN_POINT ( 'NONE',  ( -16.88460203013675454, 9.954759003246872240, -121.3658918095382546 ) ) ;
#121972 = DIRECTION ( 'NONE',  ( -1.073024830501117725E-15, -0.2128009952263604232, 0.9770955615653316162 ) ) ;
#121973 = DIRECTION ( 'NONE',  ( 0.000000000000000000, 0.000000000000000000, -1.000000000000000000 ) ) ;
#121974 = AXIS2_PLACEMENT_3D ( 'NONE', #3700, #160246, #221444 ) ;
#121975 = ORIENTED_EDGE ( 'NONE', *, *, #168028, .T. ) ;
#121976 = AXIS2_PLACEMENT_3D ( 'NONE', #58125, #56833, #235495 ) ;
#121977 = CARTESIAN_POINT ( 'NONE',  ( 18.39999999999999858, -9.599999999988845900, -107.2001893912220964 ) ) ;
#121978 = DIRECTION ( 'NONE',  ( 0.000000000000000000, -0.2128009952265059457, 0.9770955615652998638 ) ) ;
#121979 = DIRECTION ( 'NONE',  ( 1.000000000000000000, 0.000000000000000000, 0.000000000000000000 ) ) ;
#121980 = SPHERICAL_SURFACE ( 'NONE', #101155, 0.1000000000000000056 ) ;
#121981 = ORIENTED_EDGE ( 'NONE', *, *, #36091, .F. ) ;
#121982 = CARTESIAN_POINT ( 'NONE',  ( -21.05000000000000071, 76.08579911628599746, -109.4370863660127497 ) ) ;
#121983 = ORIENTED_EDGE ( 'NONE', *, *, #89531, .F. ) ;
#121984 = CARTESIAN_POINT ( 'NONE',  ( 21.14999999999999858, 11.65000000001116298, -112.7500000000000284 ) ) ;
#121985 = ORIENTED_EDGE ( 'NONE', *, *, #125328, .F. ) ;
#121986 = CARTESIAN_POINT ( 'NONE',  ( 18.50000000000000000, 65.76686835164943545, -247.8575435273897938 ) ) ;
#121987 = CARTESIAN_POINT ( 'NONE',  ( -20.94999999999999929, 10.29288807859936661, -72.45800201601217339 ) ) ;
#121989 = EDGE_LOOP ( 'NONE', ( #56513, #128044, #20297, #88361 ) ) ;
#121988 = CIRCLE ( 'NONE', #101080, 12.97499999999999787 ) ;
#121991 = VERTEX_POINT ( 'NONE', #110030 ) ;
#121990 = DIRECTION ( 'NONE',  ( -1.000000000000000000, 0.000000000000000000, 0.000000000000000000 ) ) ;
#121992 = DIRECTION ( 'NONE',  ( 0.000000000000000000, 0.000000000000000000, -1.000000000000000000 ) ) ;
#121993 = VERTEX_POINT ( 'NONE', #73510 ) ;
#121994 = DIRECTION ( 'NONE',  ( -0.000000000000000000, 1.000000000000000000, 6.982962677686266711E-15 ) ) ;
#121995 = CIRCLE ( 'NONE', #5449, 0.1000000000000024342 ) ;
#121996 = AXIS2_PLACEMENT_3D ( 'NONE', #97189, #37287, #157244 ) ;
#121997 = VECTOR ( 'NONE', #239904, 1000.000000000000000 ) ;
#121998 = CARTESIAN_POINT ( 'NONE',  ( -21.05000000000000071, 1.162701749949165642, -75.00000000000004263 ) ) ;
#121999 = ORIENTED_EDGE ( 'NONE', *, *, #162024, .F. ) ;
#122000 = AXIS2_PLACEMENT_3D ( 'NONE', #81910, #107930, #150910 ) ;
#122001 = EDGE_LOOP ( 'NONE', ( #38685, #181338, #245633 ) ) ;
#122002 = CARTESIAN_POINT ( 'NONE',  ( 23.14999999999999858, 4.813084112160680661, -112.4415177565238650 ) ) ;
#122003 = CARTESIAN_POINT ( 'NONE',  ( -16.86445178670650691, 14.17961099607968833, -219.2923173631047860 ) ) ;
#122004 = DIRECTION ( 'NONE',  ( -1.000000000000000000, 0.000000000000000000, 0.000000000000000000 ) ) ;
#122005 = ORIENTED_EDGE ( 'NONE', *, *, #101289, .F. ) ;
#122006 = VERTEX_POINT ( 'NONE', #89178 ) ;
#122007 = EDGE_CURVE ( 'NONE', #192936, #181336, #113939, .T. ) ;
#122008 = CARTESIAN_POINT ( 'NONE',  ( -20.94999999999999929, 0.000000000000000000, -33.50000000000000000 ) ) ;
#122009 = EDGE_CURVE ( 'NONE', #225207, #125758, #226352, .T. ) ;
#122011 = EDGE_LOOP ( 'NONE', ( #213181, #64584, #116947 ) ) ;
#122010 = DIRECTION ( 'NONE',  ( 1.000000000000000000, -1.207181226542539700E-16, 2.694675058168174199E-16 ) ) ;
#122012 = FACE_OUTER_BOUND ( 'NONE', #181921, .T. ) ;
#122013 = CARTESIAN_POINT ( 'NONE',  ( -22.49756042579671700, 75.92195366299456794, -81.17297244562665526 ) ) ;
#122014 = DIRECTION ( 'NONE',  ( 0.000000000000000000, 0.7397360091702777085, -0.6728971962616808744 ) ) ;
#122016 = CARTESIAN_POINT ( 'NONE',  ( -16.92507428761701860, 9.950000000011138823, -188.2866025403783965 ) ) ;
#122015 = CARTESIAN_POINT ( 'NONE',  ( -16.93226657140833069, 66.00045617728744674, -90.44439437355075029 ) ) ;
#122018 = EDGE_CURVE ( 'NONE', #85340, #14237, #209127, .T. ) ;
#122017 = CARTESIAN_POINT ( 'NONE',  ( -21.11833042828144613, 75.99289949095295071, -142.9687521783799014 ) ) ;
#122019 = CARTESIAN_POINT ( 'NONE',  ( 21.05000000000000071, 8.876614585098254295, -108.8850804788447135 ) ) ;
#122020 = AXIS2_PLACEMENT_3D ( 'NONE', #121759, #82572, #100842 ) ;
#122021 = CARTESIAN_POINT ( 'NONE',  ( -18.39999999999999858, 47.00127771169579916, -255.4372249185379928 ) ) ;
#122022 = FACE_OUTER_BOUND ( 'NONE', #42152, .T. ) ;
#122023 = ORIENTED_EDGE ( 'NONE', *, *, #15667, .T. ) ;
#122024 = CIRCLE ( 'NONE', #155382, 0.09999999999999134581 ) ;
#122025 = ORIENTED_EDGE ( 'NONE', *, *, #63270, .T. ) ;
#122027 = DIRECTION ( 'NONE',  ( -1.000000000000000000, 0.000000000000000000, 0.000000000000000000 ) ) ;
#122026 = AXIS2_PLACEMENT_3D ( 'NONE', #49864, #228524, #129408 ) ;
#122028 = ADVANCED_FACE ( 'NONE', ( #72212 ), #104947, .T. ) ;
#122029 = ORIENTED_EDGE ( 'NONE', *, *, #137616, .T. ) ;
#122030 = DIRECTION ( 'NONE',  ( 0.2834754621636439431, 0.2834754621636471628, 0.9161240771326858434 ) ) ;
#122031 = CIRCLE ( 'NONE', #246924, 1.749999999999998002 ) ;
#122032 = EDGE_CURVE ( 'NONE', #29489, #149997, #22391, .T. ) ;
#122033 = ADVANCED_FACE ( 'NONE', ( #199865 ), #154349, .F. ) ;
#122034 = ORIENTED_EDGE ( 'NONE', *, *, #39688, .T. ) ;
#122035 = CIRCLE ( 'NONE', #217873, 0.09999999999999820144 ) ;
#122036 = CARTESIAN_POINT ( 'NONE',  ( 16.87683809663749557, 30.20632856012693068, -234.8070450048000737 ) ) ;
#122038 = EDGE_LOOP ( 'NONE', ( #238361, #189044, #156967, #256574 ) ) ;
#122037 = VERTEX_POINT ( 'NONE', #60321 ) ;
#122039 = FACE_OUTER_BOUND ( 'NONE', #76667, .T. ) ;
#122040 = ORIENTED_EDGE ( 'NONE', *, *, #241559, .T. ) ;
#122041 = EDGE_LOOP ( 'NONE', ( #238105, #172228, #135519, #81135 ) ) ;
#122042 = VECTOR ( 'NONE', #138894, 1000.000000000000114 ) ;
#122043 = EDGE_CURVE ( 'NONE', #68437, #47344, #176452, .T. ) ;
#122044 = FACE_OUTER_BOUND ( 'NONE', #109924, .T. ) ;
#122046 = ORIENTED_EDGE ( 'NONE', *, *, #190468, .T. ) ;
#122045 = CARTESIAN_POINT ( 'NONE',  ( -23.25000000000000355, 28.17589918783267322, -238.5974746063260739 ) ) ;
#122047 = CARTESIAN_POINT ( 'NONE',  ( 20.97250901189795513, 39.30993059825905078, -236.7215534631462788 ) ) ;
#122048 = EDGE_CURVE ( 'NONE', #67817, #133612, #147265, .T. ) ;
#122049 = CARTESIAN_POINT ( 'NONE',  ( 19.90621891164687440, 11.75000000001116263, -158.8284452778770230 ) ) ;
#122051 = ORIENTED_EDGE ( 'NONE', *, *, #45812, .T. ) ;
#122050 = CARTESIAN_POINT ( 'NONE',  ( 20.95545211741311320, 10.58641331155510379, -141.5861468595883252 ) ) ;
#122052 = CARTESIAN_POINT ( 'NONE',  ( 19.80993210785715775, 11.75000000001116263, -125.2671177488815175 ) ) ;
#122054 = EDGE_CURVE ( 'NONE', #207209, #40580, #218101, .T. ) ;
#122053 = ORIENTED_EDGE ( 'NONE', *, *, #207633, .F. ) ;
#122055 = DIRECTION ( 'NONE',  ( 0.000000000000000000, 0.000000000000000000, -1.000000000000000000 ) ) ;
#122056 = CIRCLE ( 'NONE', #234285, 0.09999999999999939493 ) ;
#122058 = VERTEX_POINT ( 'NONE', #137290 ) ;
#122057 = CARTESIAN_POINT ( 'NONE',  ( 18.49999999999999289, 64.35000000001171827, -69.52310748452438816 ) ) ;
#122059 = VECTOR ( 'NONE', #246041, 1000.000000000000000 ) ;
#122060 = CARTESIAN_POINT ( 'NONE',  ( -18.59999999999999787, 12.87592094156238609, -205.3750039893633073 ) ) ;
#122061 = CARTESIAN_POINT ( 'NONE',  ( -14.87770893841226894, 27.68529808098225686, -234.0457819887453468 ) ) ;
#122062 = CARTESIAN_POINT ( 'NONE',  ( 18.49999999999999645, 74.83729825007360148, -61.42310748452432989 ) ) ;
#122063 = ORIENTED_EDGE ( 'NONE', *, *, #213114, .T. ) ;
#122065 = CARTESIAN_POINT ( 'NONE',  ( -23.25000000000000355, 5.649999999999983480, -20.85000000000000142 ) ) ;
#122064 = PLANE ( 'NONE',  #169979 ) ;
#122066 = CARTESIAN_POINT ( 'NONE',  ( -15.69373346032659455, 66.64320997496594146, -85.81828097591048277 ) ) ;
#122067 = CARTESIAN_POINT ( 'NONE',  ( 23.24999999999999289, 11.65000000001116298, -155.7499999999999716 ) ) ;
#122068 = CARTESIAN_POINT ( 'NONE',  ( -23.15000000000000213, 36.65892442174935439, -249.5511627012433848 ) ) ;
#122069 = DIRECTION ( 'NONE',  ( 0.7071067811865127117, 0.7071067811865821007, 0.000000000000000000 ) ) ;
#122071 = ORIENTED_EDGE ( 'NONE', *, *, #177385, .T. ) ;
#122070 = VECTOR ( 'NONE', #62346, 1000.000000000000000 ) ;
#122072 = ORIENTED_EDGE ( 'NONE', *, *, #187799, .T. ) ;
#122073 = CIRCLE ( 'NONE', #9641, 7.899999999999990585 ) ;
#122075 = ORIENTED_EDGE ( 'NONE', *, *, #82887, .T. ) ;
#122074 = AXIS2_PLACEMENT_3D ( 'NONE', #95955, #116821, #254974 ) ;
#122076 = LINE ( 'NONE', #182050, #5442 ) ;
#122077 = AXIS2_PLACEMENT_3D ( 'NONE', #134617, #255825, #194650 ) ;
#122079 = EDGE_LOOP ( 'NONE', ( #45642, #107207, #80241, #60930 ) ) ;
#122078 = EDGE_CURVE ( 'NONE', #91508, #2351, #154885, .T. ) ;
#122080 = DIRECTION ( 'NONE',  ( 0.000000000000000000, 0.000000000000000000, -1.000000000000000000 ) ) ;
#122081 = VERTEX_POINT ( 'NONE', #119034 ) ;
#122082 = EDGE_CURVE ( 'NONE', #25855, #4376, #198552, .T. ) ;
#122083 = CARTESIAN_POINT ( 'NONE',  ( -21.53752568617674612, 6.786807874515071504, -100.4010255387293284 ) ) ;
#122084 = CARTESIAN_POINT ( 'NONE',  ( 18.52130828395271678, -9.481395502614633486, -40.52450672388363984 ) ) ;
#122085 = B_SPLINE_CURVE_WITH_KNOTS ( 'NONE', 3,
 ( #88192, #52940, #231600, #206890, #150768, #229031, #50353, #47791, #209449, #226424, #191207, #12562, #166508 ),
 .UNSPECIFIED., .F., .F.,
 ( 4, 3, 3, 3, 4 ),
 ( 1.075528555105620399E-16, 1.946463881814325270E-05, 3.922356109943460204E-05, 4.215060953239334383E-05, 4.415117091092807429E-05 ),
 .UNSPECIFIED. ) ;
#122087 = EDGE_CURVE ( 'NONE', #251940, #219844, #130693, .T. ) ;
#122086 = ORIENTED_EDGE ( 'NONE', *, *, #121575, .F. ) ;
#122088 =( NAMED_UNIT ( * ) SI_UNIT ( $, .STERADIAN. ) SOLID_ANGLE_UNIT ( ) );
#122089 = VECTOR ( 'NONE', #159178, 1000.000000000000114 ) ;
#122090 = VECTOR ( 'NONE', #106474, 1000.000000000000000 ) ;
#122091 = EDGE_LOOP ( 'NONE', ( #256973, #180174, #144106, #128063 ) ) ;
#122092 = AXIS2_PLACEMENT_3D ( 'NONE', #234184, #254977, #195101 ) ;
#122094 = ORIENTED_EDGE ( 'NONE', *, *, #160028, .T. ) ;
#122093 = CIRCLE ( 'NONE', #134540, 0.1000000000000028644 ) ;
#122095 = VERTEX_POINT ( 'NONE', #4197 ) ;
#122096 = DIRECTION ( 'NONE',  ( 0.000000000000000000, -0.000000000000000000, -1.000000000000000000 ) ) ;
#122097 = CARTESIAN_POINT ( 'NONE',  ( -40.23850191057533010, 66.15000000001120384, -4.623107484524796362 ) ) ;
#122098 = DIRECTION ( 'NONE',  ( 1.000000000000000000, 0.000000000000000000, 0.000000000000000000 ) ) ;
#122099 = LINE ( 'NONE', #105045, #85703 ) ;
#122100 = CARTESIAN_POINT ( 'NONE',  ( 18.39999999999999503, 64.25000000001261924, -190.8731074845244393 ) ) ;
#122102 = CARTESIAN_POINT ( 'NONE',  ( 21.05000000000000071, 70.60000000001151932, -48.42837350343745584 ) ) ;
#122101 = CYLINDRICAL_SURFACE ( 'NONE', #253876, 0.1000000000000028644 ) ;
#122103 = CARTESIAN_POINT ( 'NONE',  ( -23.15000000000000213, 1.115600667400684642E-11, -136.1000000000000227 ) ) ;
#122105 = VERTEX_POINT ( 'NONE', #64191 ) ;
#122104 = FACE_OUTER_BOUND ( 'NONE', #78117, .T. ) ;
#122106 = LINE ( 'NONE', #102498, #179194 ) ;
#122107 = DIRECTION ( 'NONE',  ( -0.7071067811865475727, -0.7071067811865475727, -0.000000000000000000 ) ) ;
#122108 = ORIENTED_EDGE ( 'NONE', *, *, #25466, .T. ) ;
#122109 = CARTESIAN_POINT ( 'NONE',  ( 13.40000000000005898, 67.75000000001118394, -25.06452884076209742 ) ) ;
#122110 = DIRECTION ( 'NONE',  ( 0.000000000000000000, 0.9167729611565434977, -0.3994087351226345284 ) ) ;
#122112 = ADVANCED_FACE ( 'NONE', ( #182874 ), #172442, .T. ) ;
#122111 = LINE ( 'NONE', #142923, #8747 ) ;
#122113 = ORIENTED_EDGE ( 'NONE', *, *, #78524, .T. ) ;
#122114 = ADVANCED_FACE ( 'NONE', ( #103287 ), #100703, .F. ) ;
#122115 = DIRECTION ( 'NONE',  ( 0.000000000000000000, 6.982962677686266711E-15, -1.000000000000000000 ) ) ;
#122116 = DIRECTION ( 'NONE',  ( -0.000000000000000000, 0.3427706569149420734, -0.9394191166663041770 ) ) ;
#122117 = ORIENTED_EDGE ( 'NONE', *, *, #56858, .T. ) ;
#122118 = ORIENTED_EDGE ( 'NONE', *, *, #113758, .T. ) ;
#122119 = ADVANCED_FACE ( 'NONE', ( #2909 ), #22512, .F. ) ;
#122120 = AXIS2_PLACEMENT_3D ( 'NONE', #121889, #205243, #146548 ) ;
#122122 = EDGE_CURVE ( 'NONE', #249092, #184776, #181582, .T. ) ;
#122121 = CARTESIAN_POINT ( 'NONE',  ( -16.92973740335356680, 9.992503814467269763, -12.59394096479777048 ) ) ;
#122123 = ORIENTED_EDGE ( 'NONE', *, *, #3552, .T. ) ;
#122124 = DIRECTION ( 'NONE',  ( 0.000000000000000000, 0.9910465087640860649, -0.1335171055202901413 ) ) ;
#122125 = CARTESIAN_POINT ( 'NONE',  ( 20.94999999999999929, 64.08993991385487732, -222.4142553782910454 ) ) ;
#122126 = CARTESIAN_POINT ( 'NONE',  ( 20.94999999999999574, 36.65892442174472876, -249.5511627012454596 ) ) ;
#122127 = LINE ( 'NONE', #196512, #192587 ) ;
#122128 = ORIENTED_EDGE ( 'NONE', *, *, #172636, .F. ) ;
#122129 = ADVANCED_FACE ( 'NONE', ( #162023 ), #82429, .F. ) ;
#122130 = DIRECTION ( 'NONE',  ( 0.000000000000000000, -0.4088369013363281623, 0.9126074666063771490 ) ) ;
#122131 = CARTESIAN_POINT ( 'NONE',  ( -18.50000000000000000, 77.16412189325305349, -95.10825939895268277 ) ) ;
#122132 = CARTESIAN_POINT ( 'NONE',  ( 18.49999999999999289, 10.23906162413259402, -192.2543974345975926 ) ) ;
#122133 = CARTESIAN_POINT ( 'NONE',  ( -22.39999999999999858, 26.02743912001966464, -254.3139371321002216 ) ) ;
#122134 = EDGE_CURVE ( 'NONE', #241009, #151179, #84868, .T. ) ;
#122136 = ORIENTED_EDGE ( 'NONE', *, *, #29547, .F. ) ;
#122135 = CIRCLE ( 'NONE', #126402, 0.1000000000000078465 ) ;
#122137 = EDGE_CURVE ( 'NONE', #3155, #226069, #155853, .T. ) ;
#122139 = EDGE_LOOP ( 'NONE', ( #187641, #102535 ) ) ;
#122138 = DIRECTION ( 'NONE',  ( 7.304098846218134667E-16, 0.9651348961777158619, -0.2617529984165031243 ) ) ;
#122140 = CARTESIAN_POINT ( 'NONE',  ( 22.50000000000000000, 11.64957080755595520, -66.90000000000004832 ) ) ;
#122141 = LINE ( 'NONE', #180833, #69592 ) ;
#122142 = EDGE_CURVE ( 'NONE', #29396, #25296, #141536, .T. ) ;
#122143 = CARTESIAN_POINT ( 'NONE',  ( -16.92570016628983254, 9.958788957751014692, -87.87934932996105886 ) ) ;
#122144 = CARTESIAN_POINT ( 'NONE',  ( 21.05000000000000071, 74.83729825007388570, -94.92310748452432279 ) ) ;
#122145 = DIRECTION ( 'NONE',  ( 0.5000000000001141309, 0.000000000000000000, -0.8660254037843729824 ) ) ;
#122146 = DIRECTION ( 'NONE',  ( -0.000000000000000000, 0.1350103645451945777, -0.9908441862701590219 ) ) ;
#122147 = ORIENTED_EDGE ( 'NONE', *, *, #94659, .F. ) ;
#122148 = CARTESIAN_POINT ( 'NONE',  ( -16.90202395485715314, 63.08422021722274309, -213.0722826622215678 ) ) ;
#122149 = CARTESIAN_POINT ( 'NONE',  ( -21.05000000000000071, 36.65892442174935439, -249.5511627012433848 ) ) ;
#122150 = CARTESIAN_POINT ( 'NONE',  ( -22.50875500270928953, -0.1008579137753043697, 11.74956712739789211 ) ) ;
#122151 = CARTESIAN_POINT ( 'NONE',  ( -21.65000000000000213, 62.98921886345645760, -213.1014462870871569 ) ) ;
#122152 = CIRCLE ( 'NONE', #138848, 7.900000000000000355 ) ;
#122153 = EDGE_CURVE ( 'NONE', #151457, #152968, #43402, .T. ) ;
#122154 = CARTESIAN_POINT ( 'NONE',  ( -23.25000000000000000, 0.8618440306782485516, -204.9572370243411115 ) ) ;
#122156 = FACE_OUTER_BOUND ( 'NONE', #125476, .T. ) ;
#122155 = CIRCLE ( 'NONE', #134593, 0.1999999999999945155 ) ;
#122157 = ORIENTED_EDGE ( 'NONE', *, *, #150092, .T. ) ;
#122158 = ORIENTED_EDGE ( 'NONE', *, *, #102918, .T. ) ;
#122159 = DIRECTION ( 'NONE',  ( -1.000000000000000000, 0.000000000000000000, -0.000000000000000000 ) ) ;
#122161 = FACE_OUTER_BOUND ( 'NONE', #150876, .T. ) ;
#122160 = VECTOR ( 'NONE', #195447, 999.9999999999998863 ) ;
#122162 = ADVANCED_FACE ( 'NONE', ( #143713 ), #26349, .T. ) ;
#122163 = FACE_OUTER_BOUND ( 'NONE', #195904, .T. ) ;
#122164 = CARTESIAN_POINT ( 'NONE',  ( 20.85000000000000142, 17.16609282392354174, -224.6038045889790453 ) ) ;
#122165 = ORIENTED_EDGE ( 'NONE', *, *, #39991, .F. ) ;
#122167 = EDGE_CURVE ( 'NONE', #79511, #70872, #244092, .T. ) ;
#122166 = CARTESIAN_POINT ( 'NONE',  ( 23.24999999999999645, 76.00000000001126921, -203.5231074845248997 ) ) ;
#122168 = EDGE_CURVE ( 'NONE', #81419, #142144, #139228, .T. ) ;
#122169 = CARTESIAN_POINT ( 'NONE',  ( -20.64999999999999858, 48.50000630096246823, -244.2465039064066161 ) ) ;
#122170 = CIRCLE ( 'NONE', #76342, 12.87499999999999822 ) ;
#122171 = TOROIDAL_SURFACE ( 'NONE', #180425, 0.2000000000000000111, 0.1000000000000000056 ) ;
#122172 = DIRECTION ( 'NONE',  ( 8.673617379884087537E-15, 6.982962677686266711E-15, -1.000000000000000000 ) ) ;
#122173 = VECTOR ( 'NONE', #17343, 1000.000000000000227 ) ;
#122174 = CARTESIAN_POINT ( 'NONE',  ( -21.14999999999999858, 1.580567032079710055, -244.0902705724231794 ) ) ;
#122175 = B_SPLINE_CURVE_WITH_KNOTS ( 'NONE', 3,
 ( #73392, #152933, #232457, #253266, #74685, #49935, #129489, #12129, #52492, #233731 ),
 .UNSPECIFIED., .F., .F.,
 ( 4, 3, 3, 4 ),
 ( 0.000000000000000000, 0.0002000000000002884074, 0.001000000000045112589, 0.001967863649472103085 ),
 .UNSPECIFIED. ) ;
#122176 = ORIENTED_EDGE ( 'NONE', *, *, #112094, .F. ) ;
#122177 = DIRECTION ( 'NONE',  ( -1.000000000000000000, -0.000000000000000000, -0.000000000000000000 ) ) ;
#122178 = AXIS2_PLACEMENT_3D ( 'NONE', #7239, #25550, #86770 ) ;
#122179 = EDGE_LOOP ( 'NONE', ( #47274, #196487, #240180, #26133 ) ) ;
#122180 = EDGE_CURVE ( 'NONE', #238921, #217031, #130878, .T. ) ;
#122181 = LINE ( 'NONE', #25641, #39194 ) ;
#122182 = DIRECTION ( 'NONE',  ( 0.000000000000000000, 0.000000000000000000, 1.000000000000000000 ) ) ;
#122183 = CARTESIAN_POINT ( 'NONE',  ( -21.07928932188134041, 10.02993822722537942, -228.1074463178628662 ) ) ;
#122184 = CARTESIAN_POINT ( 'NONE',  ( 18.51697539158856642, 65.68434038414336840, -63.98668807260654745 ) ) ;
#122186 = AXIS2_PLACEMENT_3D ( 'NONE', #241176, #138183, #62525 ) ;
#122185 = CARTESIAN_POINT ( 'NONE',  ( -23.15000000000000213, 76.00000000001126921, -203.5231074845248997 ) ) ;
#122187 = DIRECTION ( 'NONE',  ( 0.000000000000000000, -1.000000000000000000, 0.000000000000000000 ) ) ;
#122189 = CARTESIAN_POINT ( 'NONE',  ( -21.14999999999999858, 69.74218538953657287, -203.6208977758331855 ) ) ;
#122188 = VECTOR ( 'NONE', #256924, 1000.000000000000114 ) ;
#122190 = TOROIDAL_SURFACE ( 'NONE', #159786, 11.70000000000000107, 0.1000000000000000056 ) ;
#122191 = FACE_OUTER_BOUND ( 'NONE', #199742, .T. ) ;
#122193 = FACE_OUTER_BOUND ( 'NONE', #23793, .T. ) ;
#122192 = TOROIDAL_SURFACE ( 'NONE', #230318, 0.9750000000000019762, 0.1000000000000000056 ) ;
#122194 = EDGE_CURVE ( 'NONE', #215594, #80413, #35067, .T. ) ;
#122195 = FACE_OUTER_BOUND ( 'NONE', #153601, .T. ) ;
#122196 = FACE_OUTER_BOUND ( 'NONE', #124452, .T. ) ;
#122197 = LINE ( 'NONE', #201717, #231270 ) ;
#122198 = CARTESIAN_POINT ( 'NONE',  ( 20.99780126800934354, 56.17802974602408739, -228.0901074916681353 ) ) ;
#122199 = EDGE_LOOP ( 'NONE', ( #53139, #6448, #181942, #178198 ) ) ;
#122200 = CARTESIAN_POINT ( 'NONE',  ( -22.39999999999999858, 68.20922040163873135, -136.6231074845243540 ) ) ;
#122201 = DIRECTION ( 'NONE',  ( 1.000000000000000000, 0.000000000000000000, 0.000000000000000000 ) ) ;
#122202 = EDGE_CURVE ( 'NONE', #140944, #192232, #126604, .T. ) ;
#122203 = ORIENTED_EDGE ( 'NONE', *, *, #134649, .T. ) ;
#122204 = LINE ( 'NONE', #4787, #22429 ) ;
#122205 = CIRCLE ( 'NONE', #201302, 0.9750000000000036415 ) ;
#122206 = VERTEX_POINT ( 'NONE', #126725 ) ;
#122207 = CARTESIAN_POINT ( 'NONE',  ( 20.94999999999999574, 74.16465844978787914, -158.4679561919613775 ) ) ;
#122208 = DIRECTION ( 'NONE',  ( 0.000000000000000000, 5.204170427930272346E-14, 1.000000000000000000 ) ) ;
#122209 = CIRCLE ( 'NONE', #230552, 0.09999999999998898659 ) ;
#122210 = ADVANCED_FACE ( 'NONE', ( #121620 ), #208832, .F. ) ;
#122212 = ORIENTED_EDGE ( 'NONE', *, *, #114112, .F. ) ;
#122211 = AXIS2_PLACEMENT_3D ( 'NONE', #213926, #35330, #194390 ) ;
#122213 = ORIENTED_EDGE ( 'NONE', *, *, #29979, .F. ) ;
#122215 = CARTESIAN_POINT ( 'NONE',  ( 20.94999999999999929, 1.115600667400684642E-11, -67.00000000000004263 ) ) ;
#122214 = VECTOR ( 'NONE', #168862, 1000.000000000000000 ) ;
#122216 = AXIS2_PLACEMENT_3D ( 'NONE', #110819, #252900, #155128 ) ;
#122217 = ORIENTED_EDGE ( 'NONE', *, *, #174890, .T. ) ;
#122218 = CARTESIAN_POINT ( 'NONE',  ( -20.64999999999999858, -8.663551401858001100, -90.97589888193274987 ) ) ;
#122220 = AXIS2_PLACEMENT_3D ( 'NONE', #70231, #186306, #205854 ) ;
#122219 = CARTESIAN_POINT ( 'NONE',  ( -18.40000000000000213, 5.650000000011139001, -87.85000000000003695 ) ) ;
#122221 = DIRECTION ( 'NONE',  ( 0.000000000000000000, 0.8814952561688449428, -0.4721928772777310157 ) ) ;
#122222 = DIRECTION ( 'NONE',  ( 0.000000000000000000, 0.000000000000000000, 1.000000000000000000 ) ) ;
#122223 = DIRECTION ( 'NONE',  ( 0.000000000000000000, 0.000000000000000000, -1.000000000000000000 ) ) ;
#122224 = AXIS2_PLACEMENT_3D ( 'NONE', #254704, #93103, #111397 ) ;
#122225 = CARTESIAN_POINT ( 'NONE',  ( 23.14999999999999147, -4.149999999988843058, -100.5000000000000284 ) ) ;
#122227 = CYLINDRICAL_SURFACE ( 'NONE', #212105, 10.00000000000000178 ) ;
#122226 = AXIS2_PLACEMENT_3D ( 'NONE', #57550, #171147, #54974 ) ;
#122228 = AXIS2_PLACEMENT_3D ( 'NONE', #174656, #37681, #153809 ) ;
#122229 = ORIENTED_EDGE ( 'NONE', *, *, #215592, .F. ) ;
#122230 = ORIENTED_EDGE ( 'NONE', *, *, #143842, .F. ) ;
#122232 = DIRECTION ( 'NONE',  ( 0.000000000000000000, 0.000000000000000000, -1.000000000000000000 ) ) ;
#122231 = CARTESIAN_POINT ( 'NONE',  ( -18.50000000000000000, 70.65875701002008213, -79.32975769101238939 ) ) ;
#122233 = VECTOR ( 'NONE', #17197, 1000.000000000000227 ) ;
#122235 = ORIENTED_EDGE ( 'NONE', *, *, #41985, .F. ) ;
#122234 = CARTESIAN_POINT ( 'NONE',  ( 21.10642757222115051, 10.72315628916975250, -146.2406975237852294 ) ) ;
#122236 = ORIENTED_EDGE ( 'NONE', *, *, #191910, .T. ) ;
#122237 = CARTESIAN_POINT ( 'NONE',  ( 20.00000000000000000, 5.474129339729826960, 16.54142135623731136 ) ) ;
#122238 = CARTESIAN_POINT ( 'NONE',  ( 20.86036036209915423, 10.62104277658212048, -175.1663484185077095 ) ) ;
#122239 = CIRCLE ( 'NONE', #205410, 0.1000000000000028644 ) ;
#122240 = CARTESIAN_POINT ( 'NONE',  ( -20.94999999999999929, 1.115600667400684642E-11, -167.5000000000000284 ) ) ;
#122241 = CARTESIAN_POINT ( 'NONE',  ( 18.50000000000000000, -9.399999999999998579, -40.38204184817267617 ) ) ;
#122242 = DIRECTION ( 'NONE',  ( 1.186688945009010324E-16, -0.4721928772777346239, -0.8814952561688430555 ) ) ;
#122243 = CIRCLE ( 'NONE', #9801, 2.000000000000001776 ) ;
#122244 = CYLINDRICAL_SURFACE ( 'NONE', #115388, 0.1000000000000008105 ) ;
#122245 = ADVANCED_FACE ( 'NONE', ( #30208 ), #76704, .T. ) ;
#122246 = DIRECTION ( 'NONE',  ( 1.387778780781405791E-13, 0.9999176327611370985, 0.01283462868040226822 ) ) ;
#122247 = AXIS2_PLACEMENT_3D ( 'NONE', #109473, #14264, #189032 ) ;
#122248 = ORIENTED_EDGE ( 'NONE', *, *, #197000, .F. ) ;
#122249 = ORIENTED_EDGE ( 'NONE', *, *, #257096, .F. ) ;
#122250 = CARTESIAN_POINT ( 'NONE',  ( -21.05000000000000071, 63.65372963998873246, -224.5957079722776655 ) ) ;
#122251 = VERTEX_POINT ( 'NONE', #147573 ) ;
#122252 = CARTESIAN_POINT ( 'NONE',  ( 20.85000000000000142, 76.00000000001170974, -69.52310748452431710 ) ) ;
#122253 = VERTEX_POINT ( 'NONE', #27665 ) ;
#122254 = DIRECTION ( 'NONE',  ( 0.000000000000000000, 0.2617529984165071766, 0.9651348961777145297 ) ) ;
#122255 = AXIS2_PLACEMENT_3D ( 'NONE', #236454, #94365, #117794 ) ;
#122256 = CIRCLE ( 'NONE', #226277, 0.09999999999999971412 ) ;
#122257 = CARTESIAN_POINT ( 'NONE',  ( -12.42749937872396693, 48.82262352862033339, -233.8339354177745975 ) ) ;
#122258 = ADVANCED_FACE ( 'NONE', ( #109711 ), #107153, .F. ) ;
#122259 = CARTESIAN_POINT ( 'NONE',  ( 21.13461538461538325, 10.61458296203669249, -146.3500000000000227 ) ) ;
#122260 = DIRECTION ( 'NONE',  ( 1.000000000000000000, -0.000000000000000000, -0.000000000000000000 ) ) ;
#122261 = ORIENTED_EDGE ( 'NONE', *, *, #197530, .F. ) ;
#122262 = CARTESIAN_POINT ( 'NONE',  ( -18.79999999999999716, -1.885425182446133885, -11.49641995933507843 ) ) ;
#122263 = EDGE_LOOP ( 'NONE', ( #65978, #142496, #214332, #190402 ) ) ;
#122264 = EDGE_CURVE ( 'NONE', #111853, #103081, #189278, .T. ) ;
#122265 = CARTESIAN_POINT ( 'NONE',  ( -22.00356870067735215, 30.03864867784057680, -252.5169646700133796 ) ) ;
#122266 = DIRECTION ( 'NONE',  ( -1.000000000000000000, 0.000000000000000000, 0.000000000000000000 ) ) ;
#122267 = CARTESIAN_POINT ( 'NONE',  ( -23.15000000000000213, 76.00000000001141132, -34.02310748452431710 ) ) ;
#122268 = VERTEX_POINT ( 'NONE', #71901 ) ;
#122269 = CARTESIAN_POINT ( 'NONE',  ( -23.15000000000000213, 74.00000000001223555, -149.7477294072864709 ) ) ;
#122270 = EDGE_CURVE ( 'NONE', #217247, #170976, #22566, .T. ) ;
#122271 = VERTEX_POINT ( 'NONE', #8074 ) ;
#122274 = ORIENTED_EDGE ( 'NONE', *, *, #182710, .T. ) ;
#122273 = CARTESIAN_POINT ( 'NONE',  ( 18.58719872626880232, -9.566644397587486637, -107.3224781963970571 ) ) ;
#122272 = CARTESIAN_POINT ( 'NONE',  ( -20.64999999999999858, 76.00000000001190870, -103.0231074845243029 ) ) ;
#122275 = CIRCLE ( 'NONE', #55586, 0.1000000000000106498 ) ;
#122276 = TOROIDAL_SURFACE ( 'NONE', #59706, 11.70000000000000107, 0.1000000000000000056 ) ;
#122277 = ORIENTED_EDGE ( 'NONE', *, *, #147720, .F. ) ;
#122278 = EDGE_CURVE ( 'NONE', #130839, #245547, #20933, .T. ) ;
#122279 = DIRECTION ( 'NONE',  ( -3.890533409366484652E-14, -0.1298341882520124002, -0.9915357197604841577 ) ) ;
#122280 = ORIENTED_EDGE ( 'NONE', *, *, #168521, .F. ) ;
#122281 = DIRECTION ( 'NONE',  ( 1.000000000000000000, 0.000000000000000000, 0.000000000000000000 ) ) ;
#122282 = EDGE_CURVE ( 'NONE', #113546, #115854, #210129, .T. ) ;
#122283 = CARTESIAN_POINT ( 'NONE',  ( -16.94445028196807002, 9.992063609708893068, -54.39266982158155628 ) ) ;
#122284 = ADVANCED_FACE ( 'NONE', ( #171041 ), #51003, .F. ) ;
#122285 = CARTESIAN_POINT ( 'NONE',  ( -22.43310005002225438, -3.137626837017164938, -228.2268448955577469 ) ) ;
#122286 = LINE ( 'NONE', #162704, #76746 ) ;
#122287 = DIRECTION ( 'NONE',  ( 0.000000000000000000, 1.000000000000000000, 0.000000000000000000 ) ) ;
#122288 = ADVANCED_FACE ( 'NONE', ( #190571 ), #32799, .F. ) ;
#122289 = ORIENTED_EDGE ( 'NONE', *, *, #24106, .F. ) ;
#122290 = CARTESIAN_POINT ( 'NONE',  ( 21.15000000000005542, 74.94272479589878344, -3.123107484524795474 ) ) ;
#122291 = DIRECTION ( 'NONE',  ( -0.7071067811865475727, -0.7071067811865475727, 0.000000000000000000 ) ) ;
#122292 = CARTESIAN_POINT ( 'NONE',  ( -18.52309608778520555, -9.642476320044044868, -140.7145963411697096 ) ) ;
#122293 = ORIENTED_EDGE ( 'NONE', *, *, #14471, .F. ) ;
#122294 = CARTESIAN_POINT ( 'NONE',  ( 13.40000000000005898, 67.75000000001118394, -25.06452884076209742 ) ) ;
#122295 = ORIENTED_EDGE ( 'NONE', *, *, #206763, .T. ) ;
#122296 = DIRECTION ( 'NONE',  ( 0.000000000000000000, 0.000000000000000000, -1.000000000000000000 ) ) ;
#122297 = DIRECTION ( 'NONE',  ( -0.000000000000000000, 1.000000000000000000, 0.000000000000000000 ) ) ;
#122298 = CARTESIAN_POINT ( 'NONE',  ( 20.99749315643148151, 36.02367272165624712, -235.8812521217649305 ) ) ;
#122300 = EDGE_LOOP ( 'NONE', ( #230756, #41485, #89087, #63880 ) ) ;
#122299 = CARTESIAN_POINT ( 'NONE',  ( 23.24999999999999645, 64.25000000001233502, -160.7731074845244450 ) ) ;
#122301 = DIRECTION ( 'NONE',  ( 1.000000000000000000, 0.000000000000000000, -0.000000000000000000 ) ) ;
#122302 = EDGE_CURVE ( 'NONE', #63115, #40557, #226526, .T. ) ;
#122303 = CARTESIAN_POINT ( 'NONE',  ( 18.59999999999999432, 1.736257131608553550, -145.5686523290175387 ) ) ;
#122304 = DIRECTION ( 'NONE',  ( -1.000000000000000000, 0.000000000000000000, -0.000000000000000000 ) ) ;
#122305 = ORIENTED_EDGE ( 'NONE', *, *, #201297, .F. ) ;
#122306 = CARTESIAN_POINT ( 'NONE',  ( -23.15000000000000213, 4.350000000011156054, -54.75000000000000000 ) ) ;
#122307 = DIRECTION ( 'NONE',  ( -1.000000000000000000, 0.000000000000000000, 0.000000000000000000 ) ) ;
#122308 = ORIENTED_EDGE ( 'NONE', *, *, #234032, .F. ) ;
#122310 = CARTESIAN_POINT ( 'NONE',  ( 22.49999999999999645, 64.25043287652299284, -170.1239658536231616 ) ) ;
#122309 = VECTOR ( 'NONE', #107495, 1000.000000000000114 ) ;
#122311 = CIRCLE ( 'NONE', #26659, 0.09999999999999609201 ) ;
#122312 = VERTEX_POINT ( 'NONE', #9336 ) ;
#122313 = CIRCLE ( 'NONE', #51538, 3.899999999999999467 ) ;
#122314 = EDGE_CURVE ( 'NONE', #17731, #176425, #60138, .T. ) ;
#122315 = CARTESIAN_POINT ( 'NONE',  ( 21.05000000000000071, 1.115600667400684642E-11, -100.5000000000000426 ) ) ;
#122316 = ORIENTED_EDGE ( 'NONE', *, *, #179802, .T. ) ;
#122318 = ORIENTED_EDGE ( 'NONE', *, *, #107112, .T. ) ;
#122317 = CARTESIAN_POINT ( 'NONE',  ( -21.05000000000000071, 11.62071067812980907, -107.3684166523410823 ) ) ;
#122321 = VERTEX_POINT ( 'NONE', #169742 ) ;
#122320 = ORIENTED_EDGE ( 'NONE', *, *, #130745, .F. ) ;
#122319 = DIRECTION ( 'NONE',  ( 0.000000000000000000, -1.000000000000000000, 0.000000000000000000 ) ) ;
#122322 = CARTESIAN_POINT ( 'NONE',  ( 20.94999999999999574, 68.49765435822607174, -224.1215006111142714 ) ) ;
#122323 = DIRECTION ( 'NONE',  ( 1.000000000000000000, 0.000000000000000000, -0.000000000000000000 ) ) ;
#122324 = DIRECTION ( 'NONE',  ( 1.000000000000000000, 0.000000000000000000, 0.000000000000000000 ) ) ;
#122325 = VECTOR ( 'NONE', #83701, 1000.000000000000000 ) ;
#122327 = CARTESIAN_POINT ( 'NONE',  ( 21.05000000000000071, 5.000000000011153745, -88.09473398108696074 ) ) ;
#122326 = CARTESIAN_POINT ( 'NONE',  ( -23.25000000000000000, -1.835859311432481045, -179.0044391687985410 ) ) ;
#122329 = EDGE_CURVE ( 'NONE', #85197, #86058, #49753, .T. ) ;
#122328 = FACE_OUTER_BOUND ( 'NONE', #150816, .T. ) ;
#122330 = CIRCLE ( 'NONE', #193081, 0.5000000000000014433 ) ;
#122331 = EDGE_CURVE ( 'NONE', #215804, #27481, #80791, .T. ) ;
#122332 = CARTESIAN_POINT ( 'NONE',  ( -20.64999999999999858, 76.00000000001126921, -203.5231074845248997 ) ) ;
#122333 = DIRECTION ( 'NONE',  ( 0.000000000000000000, -0.000000000000000000, 1.000000000000000000 ) ) ;
#122334 = AXIS2_PLACEMENT_3D ( 'NONE', #107815, #127385, #85645 ) ;
#122335 = ORIENTED_EDGE ( 'NONE', *, *, #169932, .F. ) ;
#122336 = EDGE_LOOP ( 'NONE', ( #149637, #132389, #215449, #114236, #137916 ) ) ;
#122337 = CIRCLE ( 'NONE', #109844, 0.09999999999999939493 ) ;
#122338 = DIRECTION ( 'NONE',  ( -1.000000000000000000, 0.000000000000000000, 0.000000000000000000 ) ) ;
#122340 = ORIENTED_EDGE ( 'NONE', *, *, #35118, .T. ) ;
#122339 = DIRECTION ( 'NONE',  ( 0.000000000000000000, 0.000000000000000000, -1.000000000000000000 ) ) ;
#122341 = EDGE_LOOP ( 'NONE', ( #69431, #243034, #202172, #56835 ) ) ;
#122342 = CARTESIAN_POINT ( 'NONE',  ( -22.39999999999999503, 7.790779598373400283, -1.558540622947912624E-15 ) ) ;
#122343 = ADVANCED_FACE ( 'NONE', ( #191867 ), #172320, .F. ) ;
#122344 = ORIENTED_EDGE ( 'NONE', *, *, #25314, .F. ) ;
#122345 = CYLINDRICAL_SURFACE ( 'NONE', #58626, 0.09999999999999939493 ) ;
#122346 = CIRCLE ( 'NONE', #18288, 11.80000000000000426 ) ;
#122347 = EDGE_CURVE ( 'NONE', #73589, #101099, #97528, .T. ) ;
#122348 = VECTOR ( 'NONE', #199311, 1000.000000000000000 ) ;
#122349 = ADVANCED_FACE ( 'NONE', ( #116164 ), #154043, .T. ) ;
#122350 = ORIENTED_EDGE ( 'NONE', *, *, #132698, .T. ) ;
#122351 = CIRCLE ( 'NONE', #247413, 0.1000000000000028644 ) ;
#122352 = DIRECTION ( 'NONE',  ( 1.000000000000000000, 0.000000000000000000, 0.000000000000000000 ) ) ;
#122353 = CARTESIAN_POINT ( 'NONE',  ( -21.14999999999999858, 11.75000000000000000, -6.726130636059191481 ) ) ;
#122355 = ORIENTED_EDGE ( 'NONE', *, *, #46765, .T. ) ;
#122354 = ORIENTED_EDGE ( 'NONE', *, *, #180666, .F. ) ;
#122356 = ORIENTED_EDGE ( 'NONE', *, *, #208734, .F. ) ;
#122357 = DIRECTION ( 'NONE',  ( -0.000000000000000000, 1.000000000000000000, 6.352154140967427193E-15 ) ) ;
#122358 = VERTEX_POINT ( 'NONE', #177440 ) ;
#122359 = ORIENTED_EDGE ( 'NONE', *, *, #88852, .T. ) ;
#122360 = EDGE_CURVE ( 'NONE', #248548, #58858, #19625, .T. ) ;
#122362 = CARTESIAN_POINT ( 'NONE',  ( -20.90000000000000213, -1.311673547813416718, -7.986648289447971116 ) ) ;
#122361 = AXIS2_PLACEMENT_3D ( 'NONE', #224700, #66922, #86455 ) ;
#122364 = ORIENTED_EDGE ( 'NONE', *, *, #9939, .T. ) ;
#122363 = DIRECTION ( 'NONE',  ( -3.265361837132812600E-16, -0.4088369013363267745, 0.9126074666063774821 ) ) ;
#122366 = CYLINDRICAL_SURFACE ( 'NONE', #152834, 7.900000000000000355 ) ;
#122365 = CYLINDRICAL_SURFACE ( 'NONE', #161613, 0.09999999999999230338 ) ;
#122367 = CARTESIAN_POINT ( 'NONE',  ( 20.94999999999999574, 8.926614585098251453, -108.9716830192231498 ) ) ;
#122368 = DIRECTION ( 'NONE',  ( 0.000000000000000000, 0.9061079809440786281, 0.4230464831072883181 ) ) ;
#122369 = CARTESIAN_POINT ( 'NONE',  ( -13.40000000000000213, -8.279289321881350361, 18.97071067811866030 ) ) ;
#122370 = ORIENTED_EDGE ( 'NONE', *, *, #151440, .F. ) ;
#122371 = CIRCLE ( 'NONE', #184900, 3.999999999999998224 ) ;
#122372 = ORIENTED_EDGE ( 'NONE', *, *, #69252, .F. ) ;
#122373 = CONICAL_SURFACE ( 'NONE', #209677, 4.299999999999956302, 0.7853981633974466137 ) ;
#122374 = FACE_OUTER_BOUND ( 'NONE', #45051, .T. ) ;
#122375 = CARTESIAN_POINT ( 'NONE',  ( 18.39999999999999858, -9.399999999988843058, -122.2500000000000284 ) ) ;
#122376 = ORIENTED_EDGE ( 'NONE', *, *, #18429, .T. ) ;
#122377 = CARTESIAN_POINT ( 'NONE',  ( -23.15000000000000213, 2.000000000011154189, -180.7246219227620543 ) ) ;
#122378 = DIRECTION ( 'NONE',  ( 0.000000000000000000, -0.9915357197604971473, 0.1298341882519111479 ) ) ;
#122379 = CARTESIAN_POINT ( 'NONE',  ( -21.14999999999999858, -0.09999999998884338825, -21.85042919245519855 ) ) ;
#122380 = ORIENTED_EDGE ( 'NONE', *, *, #157507, .F. ) ;
#122381 = ORIENTED_EDGE ( 'NONE', *, *, #98490, .T. ) ;
#122382 = CARTESIAN_POINT ( 'NONE',  ( 18.39999999999999858, 85.50000000001209344, -129.4910380878245633 ) ) ;
#122383 = DIRECTION ( 'NONE',  ( 1.000000000000000000, -0.000000000000000000, -0.000000000000000000 ) ) ;
#122385 = EDGE_CURVE ( 'NONE', #172249, #65541, #39334, .T. ) ;
#122384 = ORIENTED_EDGE ( 'NONE', *, *, #171966, .T. ) ;
#122386 = CARTESIAN_POINT ( 'NONE',  ( 18.59999999999999076, 6.450000000011156587, -110.5170271704400591 ) ) ;
#122387 = ORIENTED_EDGE ( 'NONE', *, *, #52250, .T. ) ;
#122388 = EDGE_CURVE ( 'NONE', #116802, #97945, #8436, .T. ) ;
#122389 = CARTESIAN_POINT ( 'NONE',  ( 20.94999999999999574, -11.74999999998883560, -137.1000000000000227 ) ) ;
#122390 = CARTESIAN_POINT ( 'NONE',  ( -18.59999999999999787, 11.64999999999999680, -12.15000000000000036 ) ) ;
#122392 = CARTESIAN_POINT ( 'NONE',  ( -20.94999675878240808, 68.00468331834514402, -224.2298952291173464 ) ) ;
#122391 = CARTESIAN_POINT ( 'NONE',  ( -21.51976009735018991, 10.39190259496836610, -227.6411649781647384 ) ) ;
#122393 = DIRECTION ( 'NONE',  ( 1.000000000000000000, 3.265361837132813093E-16, -0.000000000000000000 ) ) ;
#122394 = DIRECTION ( 'NONE',  ( -0.000000000000000000, 1.000000000000000000, -0.000000000000000000 ) ) ;
#122395 = VECTOR ( 'NONE', #204283, 1000.000000000000000 ) ;
#122396 = AXIS2_PLACEMENT_3D ( 'NONE', #65798, #181902, #184456 ) ;
#122398 = EDGE_CURVE ( 'NONE', #135773, #150875, #105912, .T. ) ;
#122397 = ORIENTED_EDGE ( 'NONE', *, *, #218753, .T. ) ;
#122399 = DIRECTION ( 'NONE',  ( -1.000000000000000000, 0.000000000000000000, 0.000000000000000000 ) ) ;
#122401 = ORIENTED_EDGE ( 'NONE', *, *, #44759, .F. ) ;
#122400 = ORIENTED_EDGE ( 'NONE', *, *, #204528, .T. ) ;
#122402 = ORIENTED_EDGE ( 'NONE', *, *, #172270, .T. ) ;
#122403 = EDGE_LOOP ( 'NONE', ( #45976, #105822, #61090, #10464, #68787 ) ) ;
#122404 = AXIS2_PLACEMENT_3D ( 'NONE', #8081, #87582, #221946 ) ;
#122405 = LINE ( 'NONE', #237220, #103153 ) ;
#122406 = AXIS2_PLACEMENT_3D ( 'NONE', #42846, #126221, #67537 ) ;
#122407 = DIRECTION ( 'NONE',  ( 0.000000000000000000, -0.2128009952263603677, 0.9770955615653313941 ) ) ;
#122408 = DIRECTION ( 'NONE',  ( 0.000000000000000000, 0.000000000000000000, 1.000000000000000000 ) ) ;
#122409 = CARTESIAN_POINT ( 'NONE',  ( 20.94999999999999929, 1.115600667400684642E-11, -200.9999999999999432 ) ) ;
#122411 = CARTESIAN_POINT ( 'NONE',  ( 18.59999999999999787, 77.83534155023627932, -91.46795619196132066 ) ) ;
#122410 = CARTESIAN_POINT ( 'NONE',  ( 21.76363531954645936, 68.98706345213993529, -69.62210935882382046 ) ) ;
#122413 = ORIENTED_EDGE ( 'NONE', *, *, #45496, .F. ) ;
#122412 = CARTESIAN_POINT ( 'NONE',  ( 20.94999999999999929, 70.15000000001252545, -180.1556047088023149 ) ) ;
#122414 = CARTESIAN_POINT ( 'NONE',  ( -21.14999999999999858, 1.115600667400684642E-11, -100.5000000000000284 ) ) ;
#122415 = ORIENTED_EDGE ( 'NONE', *, *, #167361, .T. ) ;
#122416 = VECTOR ( 'NONE', #84255, 1000.000000000000000 ) ;
#122417 = DIRECTION ( 'NONE',  ( -0.000000000000000000, 1.000000000000000000, -0.000000000000000000 ) ) ;
#122418 = ORIENTED_EDGE ( 'NONE', *, *, #167268, .T. ) ;
#122419 = VERTEX_POINT ( 'NONE', #195713 ) ;
#122420 = CARTESIAN_POINT ( 'NONE',  ( -18.59999999999999787, -1.835341550213255957, -179.0551512925629538 ) ) ;
#122421 = AXIS2_PLACEMENT_3D ( 'NONE', #105320, #184896, #32272 ) ;
#122422 = CARTESIAN_POINT ( 'NONE',  ( -23.15000000000000213, 11.65000000001115588, -155.7499999999999716 ) ) ;
#122423 = DIRECTION ( 'NONE',  ( 1.000000000000000000, -1.836970198721029934E-16, -1.601412966608202925E-30 ) ) ;
#122424 = CARTESIAN_POINT ( 'NONE',  ( 14.87567385445976953, 9.430764995433476017, -82.23053739475051316 ) ) ;
#122425 = AXIS2_PLACEMENT_3D ( 'NONE', #15279, #227891, #167948 ) ;
#122426 = EDGE_CURVE ( 'NONE', #219071, #201185, #126789, .T. ) ;
#122427 = VECTOR ( 'NONE', #174626, 1000.000000000000000 ) ;
#122428 = CARTESIAN_POINT ( 'NONE',  ( -20.65000000000000568, 5.650000000011139001, -42.75000000000000000 ) ) ;
#122429 = ORIENTED_EDGE ( 'NONE', *, *, #95490, .T. ) ;
#122430 = ORIENTED_EDGE ( 'NONE', *, *, #226784, .T. ) ;
#122431 = ADVANCED_FACE ( 'NONE', ( #234812 ), #251686, .F. ) ;
#122432 = ORIENTED_EDGE ( 'NONE', *, *, #202771, .F. ) ;
#122433 = DIRECTION ( 'NONE',  ( -1.000000000000000000, 0.000000000000000000, 0.000000000000000000 ) ) ;
#122434 = DIRECTION ( 'NONE',  ( 0.000000000000000000, 0.000000000000000000, 1.000000000000000000 ) ) ;
#122436 = CIRCLE ( 'NONE', #43141, 0.09999999999999939493 ) ;
#122435 = CARTESIAN_POINT ( 'NONE',  ( -23.25000000000000000, -8.999999999988844479, -191.7060308773475299 ) ) ;
#122437 = DIRECTION ( 'NONE',  ( 0.000000000000000000, 0.2128009952263485993, -0.9770955615653341697 ) ) ;
#122438 = CARTESIAN_POINT ( 'NONE',  ( 22.01447462590973458, 0.09903700007069084210, -59.73619979877013719 ) ) ;
#122439 = LINE ( 'NONE', #143271, #137713 ) ;
#122440 = EDGE_CURVE ( 'NONE', #236406, #56169, #55837, .T. ) ;
#122441 = FACE_OUTER_BOUND ( 'NONE', #73208, .T. ) ;
#122442 = LINE ( 'NONE', #24651, #79307 ) ;
#122443 = CARTESIAN_POINT ( 'NONE',  ( -21.04999999999959570, 6.351302579977191165, -199.6316406787433664 ) ) ;
#122444 = VECTOR ( 'NONE', #158911, 1000.000000000000000 ) ;
#122446 = ADVANCED_FACE ( 'NONE', ( #14509 ), #237382, .T. ) ;
#122445 = CARTESIAN_POINT ( 'NONE',  ( -22.59066674512252249, 11.75000000001115552, -133.9694958763695070 ) ) ;
#122447 = DIRECTION ( 'NONE',  ( 0.000000000000000000, 0.2617529984165036239, 0.9651348961777156399 ) ) ;
#122448 = B_SPLINE_CURVE_WITH_KNOTS ( 'NONE', 3,
 ( #251379, #175724, #17894, #77865, #111890, #214817, #94867, #16641, #96142, #233138, #235658, #256446, #216095, #131431, #210982, #32376 ),
 .UNSPECIFIED., .F., .F.,
 ( 4, 3, 3, 3, 3, 4 ),
 ( 0.000000000000000000, 2.372700795693547977E-05, 5.739057815866958510E-05, 9.073899019179559378E-05, 0.0001243544287365697066, 0.0001585386695601189160 ),
 .UNSPECIFIED. ) ;
#122449 = CIRCLE ( 'NONE', #80901, 0.1999999999999997335 ) ;
#122450 = AXIS2_PLACEMENT_3D ( 'NONE', #251857, #215304, #155369 ) ;
#122451 = EDGE_CURVE ( 'NONE', #173825, #18380, #176145, .T. ) ;
#122452 = ORIENTED_EDGE ( 'NONE', *, *, #252051, .T. ) ;
#122453 = CIRCLE ( 'NONE', #26597, 0.09999999999998898659 ) ;
#122455 = ADVANCED_FACE ( 'NONE', ( #155307 ), #151487, .F. ) ;
#122454 = EDGE_CURVE ( 'NONE', #30076, #70167, #97832, .T. ) ;
#122456 = CARTESIAN_POINT ( 'NONE',  ( 18.39999999999999503, 64.25000000001230660, -157.3731074845244393 ) ) ;
#122457 = ORIENTED_EDGE ( 'NONE', *, *, #133347, .T. ) ;
#122458 =( REPRESENTATION_RELATIONSHIP ('NONE','NONE', #36900, #224939 ) REPRESENTATION_RELATIONSHIP_WITH_TRANSFORMATION ( #171904 )SHAPE_REPRESENTATION_RELATIONSHIP( ) );
#122459 = CARTESIAN_POINT ( 'NONE',  ( 20.94999999999999574, 11.62071067812981795, -93.63158334765908819 ) ) ;
#122460 = DIRECTION ( 'NONE',  ( 0.000000000000000000, 0.000000000000000000, -1.000000000000000000 ) ) ;
#122461 = LINE ( 'NONE', #3786, #222972 ) ;
#122462 = ORIENTED_EDGE ( 'NONE', *, *, #52908, .T. ) ;
#122463 = LINE ( 'NONE', #41655, #242391 ) ;
#122464 = CARTESIAN_POINT ( 'NONE',  ( 19.75857864376268935, 34.44688795055758135, -235.1500552906961730 ) ) ;
#122465 = LINE ( 'NONE', #121206, #175505 ) ;
#122466 = CIRCLE ( 'NONE', #226477, 0.2000000000000057288 ) ;
#122468 = EDGE_CURVE ( 'NONE', #116858, #5127, #40, .T. ) ;
#122467 = MECHANICAL_DESIGN_GEOMETRIC_PRESENTATION_REPRESENTATION (  '', ( #22518 ), #196898 ) ;
#122470 = DIRECTION ( 'NONE',  ( 0.000000000000000000, -0.8660254037844420383, 0.4999999999999942824 ) ) ;
#122469 = VECTOR ( 'NONE', #154451, 1000.000000000000000 ) ;
#122471 = ADVANCED_FACE ( 'NONE', ( #85971 ), #120032, .F. ) ;
#122472 = DIRECTION ( 'NONE',  ( 0.000000000000000000, 0.4088369013363281068, -0.9126074666063770380 ) ) ;
#122473 = ORIENTED_EDGE ( 'NONE', *, *, #210214, .F. ) ;
#122474 = FACE_OUTER_BOUND ( 'NONE', #72791, .T. ) ;
#122476 = ORIENTED_EDGE ( 'NONE', *, *, #122991, .T. ) ;
#122475 = CARTESIAN_POINT ( 'NONE',  ( -23.25000000000000000, -11.65000000000000036, 3.469446951953614189E-15 ) ) ;
#122477 = CARTESIAN_POINT ( 'NONE',  ( 18.49999999999999645, 72.10920423909969657, -225.0008277277438822 ) ) ;
#122478 = EDGE_CURVE ( 'NONE', #45529, #101453, #6460, .T. ) ;
#122479 =( BOUNDED_SURFACE ( )  B_SPLINE_SURFACE ( 3, 2, ( 
 ( #165023, #221128, #84141 ),
 ( #125882, #22976, #102442 ),
 ( #241987, #64633, #122049 ),
 ( #124618, #104998, #245847 ),
 ( #65926, #63336, #224970 ),
 ( #21671, #205415, #26827 ) ),
 .UNSPECIFIED., .F., .F., .F. ) 
 B_SPLINE_SURFACE_WITH_KNOTS ( ( 4, 2, 4 ),
 ( 3, 3 ),
 ( 4.712388980384689674, 5.497787143782137953, 6.283185307179586232 ),
 ( 0.000000000000000000, 1.000000000000000000 ),
 .UNSPECIFIED. ) 
 GEOMETRIC_REPRESENTATION_ITEM ( )  RATIONAL_B_SPLINE_SURFACE ( (
 ( 1.000000000000000000, 0.7071067811865536790, 1.000000000000000000),
 ( 1.000000000000000000, 0.7727932973495903468, 1.000000000000000000),
 ( 1.000000000000000000, 0.8282379607643433062, 1.000000000000000000),
 ( 1.000000000000000000, 0.9038128468045532049, 1.000000000000000000),
 ( 1.000000000000000000, 0.9240297172239071433, 1.000000000000000000),
 ( 1.000000000000000000, 0.9238795325112914014, 1.000000000000000000) ) ) 
 REPRESENTATION_ITEM ( '' )  SURFACE ( )  );
#122480 = DIRECTION ( 'NONE',  ( -0.000000000000000000, -1.000000000000000000, 6.308085367188393199E-16 ) ) ;
#122481 = CARTESIAN_POINT ( 'NONE',  ( -18.50000000000000000, 77.68707439010330518, -82.33768045106596389 ) ) ;
#122482 = EDGE_LOOP ( 'NONE', ( #22964, #108099, #159908, #36324 ) ) ;
#122483 = DIRECTION ( 'NONE',  ( 1.000000000000000000, -0.000000000000000000, -0.000000000000000000 ) ) ;
#122484 = CONTEXT_DEPENDENT_SHAPE_REPRESENTATION ( #50826, #22659 ) ;
#122485 = ADVANCED_FACE ( 'NONE', ( #60004 ), #10074, .T. ) ;
#122486 = DIRECTION ( 'NONE',  ( 0.000000000000000000, -0.2128009952263601456, 0.9770955615653316162 ) ) ;
#122487 = ORIENTED_EDGE ( 'NONE', *, *, #249071, .T. ) ;
#122488 = CARTESIAN_POINT ( 'NONE',  ( 23.15000000000000213, -11.74999999998883737, -155.3500000000000227 ) ) ;
#122489 = DIRECTION ( 'NONE',  ( 0.000000000000000000, -6.982962677686266711E-15, 1.000000000000000000 ) ) ;
#122490 = EDGE_CURVE ( 'NONE', #76904, #250592, #47473, .T. ) ;
#122491 = VECTOR ( 'NONE', #213946, 1000.000000000000000 ) ;
#122492 = CARTESIAN_POINT ( 'NONE',  ( -18.59999999999999787, -1.162701749926853712, -108.6000000000000227 ) ) ;
#122493 = EDGE_LOOP ( 'NONE', ( #27933, #56293, #215995, #193608 ) ) ;
#122494 = EDGE_LOOP ( 'NONE', ( #190929, #231045, #204310, #227791, #144926, #36122, #232256, #142837, #157084, #44130 ) ) ;
#122495 = ADVANCED_FACE ( 'NONE', ( #82123 ), #101680, .F. ) ;
#122496 = DIRECTION ( 'NONE',  ( 0.000000000000000000, 0.000000000000000000, -1.000000000000000000 ) ) ;
#122497 = DIRECTION ( 'NONE',  ( 0.000000000000000000, -0.1455152366551721865, -0.9893560106964475187 ) ) ;
#122498 = DIRECTION ( 'NONE',  ( 0.000000000000000000, 1.000000000000000000, -6.308085367188393199E-16 ) ) ;
#122499 = CARTESIAN_POINT ( 'NONE',  ( -16.92507428761700794, 14.14551054555384901, -219.1931271797256784 ) ) ;
#122500 = CARTESIAN_POINT ( 'NONE',  ( 20.94999999999999574, 6.400000000011158541, -76.93042463006162279 ) ) ;
#122501 = CARTESIAN_POINT ( 'NONE',  ( 18.59999999999999076, 8.366615838327078336, -209.3410474610450365 ) ) ;
#122503 = SPHERICAL_SURFACE ( 'NONE', #82787, 0.1000000000000000056 ) ;
#122502 = CARTESIAN_POINT ( 'NONE',  ( 18.59999999999999076, 14.05000000001116689, -39.01369507076098841 ) ) ;
#122504 = EDGE_CURVE ( 'NONE', #33201, #59064, #204651, .T. ) ;
#122505 = LINE ( 'NONE', #51576, #161017 ) ;
#122506 = FACE_OUTER_BOUND ( 'NONE', #96300, .T. ) ;
#122507 = DIRECTION ( 'NONE',  ( 1.000000000000000000, -2.952720810173289112E-16, -2.061873921506763405E-30 ) ) ;
#122509 = DIRECTION ( 'NONE',  ( -1.000000000000000000, -0.000000000000000000, 1.073024830501117725E-15 ) ) ;
#122508 = CIRCLE ( 'NONE', #5759, 0.1999999999999996503 ) ;
#122510 = EDGE_LOOP ( 'NONE', ( #9126, #178178, #158437, #191919 ) ) ;
#122511 = CIRCLE ( 'NONE', #126768, 0.09999999999998898659 ) ;
#122512 = ORIENTED_EDGE ( 'NONE', *, *, #100180, .F. ) ;
#122513 = DIRECTION ( 'NONE',  ( -1.000000000000000000, 7.510212038922846022E-17, -1.676432719286211941E-16 ) ) ;
#122514 = DIRECTION ( 'NONE',  ( 0.000000000000000000, 6.982962677686267499E-15, -1.000000000000000000 ) ) ;
#122517 = CARTESIAN_POINT ( 'NONE',  ( -21.51976009735018991, 6.910458441659202755, 1.166362318020024071E-16 ) ) ;
#122516 = CARTESIAN_POINT ( 'NONE',  ( -18.59999999999999787, 1.115600667400684642E-11, -67.00000000000000000 ) ) ;
#122515 = AXIS2_PLACEMENT_3D ( 'NONE', #60163, #223093, #238819 ) ;
#122518 = CIRCLE ( 'NONE', #55823, 0.09999999999999939493 ) ;
#122519 = CYLINDRICAL_SURFACE ( 'NONE', #122731, 14.30833333333333535 ) ;
#122520 = LINE ( 'NONE', #165498, #166598 ) ;
#122521 = ADVANCED_FACE ( 'NONE', ( #143407 ), #62598, .T. ) ;
#122522 = PLANE ( 'NONE',  #227323 ) ;
#122523 = ORIENTED_EDGE ( 'NONE', *, *, #233973, .F. ) ;
#122524 = FACE_OUTER_BOUND ( 'NONE', #94091, .T. ) ;
#122525 = EDGE_LOOP ( 'NONE', ( #184174, #176700, #61643, #162364 ) ) ;
#122527 = AXIS2_PLACEMENT_3D ( 'NONE', #52298, #130564, #227095 ) ;
#122526 = CARTESIAN_POINT ( 'NONE',  ( -12.25000000000000355, 9.349999999999981881, -16.86574316727392286 ) ) ;
#122528 = ORIENTED_EDGE ( 'NONE', *, *, #101414, .T. ) ;
#122529 = DIRECTION ( 'NONE',  ( 1.836970198721029934E-16, 1.000000000000000000, 6.982962677686266711E-15 ) ) ;
#122530 = VECTOR ( 'NONE', #145534, 1000.000000000000000 ) ;
#122532 = DIRECTION ( 'NONE',  ( 1.000000000000000000, 0.000000000000000000, 0.000000000000000000 ) ) ;
#122531 = VECTOR ( 'NONE', #232304, 1000.000000000000114 ) ;
#122533 = AXIS2_PLACEMENT_3D ( 'NONE', #152166, #135118, #193840 ) ;
#122534 = AXIS2_PLACEMENT_3D ( 'NONE', #18583, #51563, #57685 ) ;
#122535 = ORIENTED_EDGE ( 'NONE', *, *, #17216, .F. ) ;
#122536 = CARTESIAN_POINT ( 'NONE',  ( -17.04295772865477687, 65.97510057475108169, -190.8731074845244109 ) ) ;
#122537 = EDGE_LOOP ( 'NONE', ( #78021, #27982, #87829, #39534 ) ) ;
#122538 = CARTESIAN_POINT ( 'NONE',  ( -20.94999999999999929, 77.16270174995010223, -128.5231074845242745 ) ) ;
#122539 = CARTESIAN_POINT ( 'NONE',  ( -21.00023020733438628, 69.60913075474394418, -69.52310748452435973 ) ) ;
#122540 = DIRECTION ( 'NONE',  ( 1.000000000000000000, 0.000000000000000000, 0.000000000000000000 ) ) ;
#122541 = AXIS2_PLACEMENT_3D ( 'NONE', #193305, #35540, #231161 ) ;
#122543 = DIRECTION ( 'NONE',  ( 0.000000000000000000, 0.000000000000000000, -1.000000000000000000 ) ) ;
#122542 = AXIS2_PLACEMENT_3D ( 'NONE', #63182, #26665, #7070 ) ;
#122544 = DIRECTION ( 'NONE',  ( 0.000000000000000000, 0.9964539953858966292, 0.08413937888696132461 ) ) ;
#122547 = CARTESIAN_POINT ( 'NONE',  ( 21.05000000000000071, 62.04503132991427350, -248.4786563706009588 ) ) ;
#122546 = VECTOR ( 'NONE', #256199, 1000.000000000000000 ) ;
#122545 = CARTESIAN_POINT ( 'NONE',  ( -21.05000000000000071, 76.00000000001168132, -73.82310748452428584 ) ) ;
#122548 = FACE_OUTER_BOUND ( 'NONE', #192892, .T. ) ;
#122551 = ORIENTED_EDGE ( 'NONE', *, *, #92749, .F. ) ;
#122550 = CARTESIAN_POINT ( 'NONE',  ( 21.05000000000000071, 85.00000000001232081, -160.1291383618718385 ) ) ;
#122549 = B_SPLINE_CURVE_WITH_KNOTS ( 'NONE', 3,
 ( #84186, #202911, #243312, #205469 ),
 .UNSPECIFIED., .F., .F.,
 ( 4, 4 ),
 ( 0.000000000000000000, 0.0002118541922231950789 ),
 .UNSPECIFIED. ) ;
#122553 = CARTESIAN_POINT ( 'NONE',  ( -21.14999999999994174, 83.80000000001119531, -34.86056257560453986 ) ) ;
#122552 = CARTESIAN_POINT ( 'NONE',  ( -21.05000000000000071, 6.540656951712397138, -33.60000000000000142 ) ) ;
#122554 = EDGE_LOOP ( 'NONE', ( #227314, #38019, #196420, #97690 ) ) ;
#122556 = ORIENTED_EDGE ( 'NONE', *, *, #160420, .F. ) ;
#122555 = FACE_OUTER_BOUND ( 'NONE', #2929, .T. ) ;
#122557 = ORIENTED_EDGE ( 'NONE', *, *, #162400, .F. ) ;
#122558 = DIRECTION ( 'NONE',  ( 0.000000000000000000, 0.9126074666063769270, 0.4088369013363282733 ) ) ;
#122559 = DIRECTION ( 'NONE',  ( -0.000000000000000000, -0.1686199900910463068, 0.9856811345164802063 ) ) ;
#122560 = DIRECTION ( 'NONE',  ( 0.000000000000000000, 0.000000000000000000, -1.000000000000000000 ) ) ;
#122561 = AXIS2_PLACEMENT_3D ( 'NONE', #118114, #135090, #214635 ) ;
#122562 = EDGE_LOOP ( 'NONE', ( #99466, #7911, #121574 ) ) ;
#122563 = CARTESIAN_POINT ( 'NONE',  ( 21.14999999999999503, 1.115488181425289271E-11, -127.4593430482987912 ) ) ;
#122564 = CARTESIAN_POINT ( 'NONE',  ( 21.05000005001280172, 8.871279691782062216, -112.6779475882458570 ) ) ;
#122565 = DIRECTION ( 'NONE',  ( -1.000000000000000000, 0.000000000000000000, -0.000000000000000000 ) ) ;
#122566 = VECTOR ( 'NONE', #202134, 1000.000000000000000 ) ;
#122567 = ORIENTED_EDGE ( 'NONE', *, *, #124882, .T. ) ;
#122568 = AXIS2_PLACEMENT_3D ( 'NONE', #126397, #122572, #82112 ) ;
#122569 = CARTESIAN_POINT ( 'NONE',  ( -18.58222699835055280, 46.46797214202639736, -243.0846070113367716 ) ) ;
#122570 = CIRCLE ( 'NONE', #51591, 12.87499999999999822 ) ;
#122571 = EDGE_CURVE ( 'NONE', #45940, #130445, #84678, .T. ) ;
#122572 = DIRECTION ( 'NONE',  ( 0.000000000000000000, 6.982962677686266711E-15, -1.000000000000000000 ) ) ;
#122573 = VERTEX_POINT ( 'NONE', #165555 ) ;
#122574 = EDGE_LOOP ( 'NONE', ( #250695, #17706, #220449, #181767 ) ) ;
#122575 = DIRECTION ( 'NONE',  ( 1.000000000000000000, 0.000000000000000000, 0.000000000000000000 ) ) ;
#122576 = ORIENTED_EDGE ( 'NONE', *, *, #161823, .T. ) ;
#122577 = FACE_OUTER_BOUND ( 'NONE', #207183, .T. ) ;
#122578 = ORIENTED_EDGE ( 'NONE', *, *, #245727, .T. ) ;
#122579 = CARTESIAN_POINT ( 'NONE',  ( -23.15000000000000213, 74.00000000001151079, -49.24772940728643533 ) ) ;
#122580 =( BOUNDED_CURVE ( )  B_SPLINE_CURVE ( 3, ( #247612, #127674, #28622, #128958 ),
 .UNSPECIFIED., .F., .F. ) 
 B_SPLINE_CURVE_WITH_KNOTS ( ( 4, 4 ),
 ( 0.5235987755983128045, 1.570796326794896558 ),
 .UNSPECIFIED. ) 
 CURVE ( )  GEOMETRIC_REPRESENTATION_ITEM ( )  RATIONAL_B_SPLINE_CURVE ( ( 1.000000000000000000, 0.9106836025229614329, 0.9106836025229614329, 1.000000000000000000 ) ) 
 REPRESENTATION_ITEM ( '' )  );
#122581 = CARTESIAN_POINT ( 'NONE',  ( 23.25000000000000000, -11.64999999998883595, -63.89999999999999858 ) ) ;
#122582 = DIRECTION ( 'NONE',  ( -1.000000000000000000, 0.000000000000000000, -0.000000000000000000 ) ) ;
#122583 = EDGE_CURVE ( 'NONE', #112231, #154754, #122721, .T. ) ;
#122584 = DIRECTION ( 'NONE',  ( 0.000000000000000000, -0.2128009952263485993, 0.9770955615653341697 ) ) ;
#122585 = ORIENTED_EDGE ( 'NONE', *, *, #149885, .F. ) ;
#122586 = ADVANCED_FACE ( 'NONE', ( #185106 ), #142122, .T. ) ;
#122587 = DIRECTION ( 'NONE',  ( 1.000000000000000000, 0.000000000000000000, 0.000000000000000000 ) ) ;
#122588 = AXIS2_PLACEMENT_3D ( 'NONE', #78457, #172488, #52465 ) ;
#122589 = AXIS2_PLACEMENT_3D ( 'NONE', #191881, #34100, #11951 ) ;
#122590 = DIRECTION ( 'NONE',  ( 1.000000000000000000, 0.000000000000000000, 0.000000000000000000 ) ) ;
#122591 = CARTESIAN_POINT ( 'NONE',  ( -21.07933241753356413, 0.09337959043042065588, -27.17135405162026274 ) ) ;
#122592 = CARTESIAN_POINT ( 'NONE',  ( -11.59999999999994458, 67.75000000001118394, -18.42310748452479174 ) ) ;
#122593 = CIRCLE ( 'NONE', #10152, 0.1000000000000002831 ) ;
#122594 = VERTEX_POINT ( 'NONE', #239958 ) ;
#122596 = CARTESIAN_POINT ( 'NONE',  ( 23.14999999999999503, 61.57587952878035509, -212.2000740415318774 ) ) ;
#122595 = CARTESIAN_POINT ( 'NONE',  ( 20.94999999999999929, 14.05000000001115623, -94.98630492923912527 ) ) ;
#122597 = ORIENTED_EDGE ( 'NONE', *, *, #186447, .T. ) ;
#122600 = ORIENTED_EDGE ( 'NONE', *, *, #136896, .F. ) ;
#122599 = CARTESIAN_POINT ( 'NONE',  ( -23.15000000000000213, 15.92646454033039660, -219.3818586450342707 ) ) ;
#122598 = DIRECTION ( 'NONE',  ( 0.000000000000000000, -0.7397360091702823714, 0.6728971962616756564 ) ) ;
#122601 = VERTEX_POINT ( 'NONE', #43037 ) ;
#122602 = FACE_OUTER_BOUND ( 'NONE', #195747, .T. ) ;
#122603 = AXIS2_PLACEMENT_3D ( 'NONE', #61320, #224231, #5159 ) ;
#122604 = CARTESIAN_POINT ( 'NONE',  ( 23.14999999999999858, 5.000000000011153745, -189.0947339810868755 ) ) ;
#122605 = EDGE_CURVE ( 'NONE', #8700, #215032, #114307, .T. ) ;
#122606 = VECTOR ( 'NONE', #97337, 1000.000000000000000 ) ;
#122607 = ORIENTED_EDGE ( 'NONE', *, *, #199004, .T. ) ;
#122608 = LINE ( 'NONE', #242531, #196910 ) ;
#122609 = EDGE_CURVE ( 'NONE', #159875, #7826, #219082, .T. ) ;
#122610 = CARTESIAN_POINT ( 'NONE',  ( -18.59999999999999787, -1.835341550213255957, -145.5551512925629822 ) ) ;
#122611 = AXIS2_PLACEMENT_3D ( 'NONE', #126987, #164839, #142673 ) ;
#122612 = EDGE_CURVE ( 'NONE', #185818, #132466, #30564, .T. ) ;
#122614 = FACE_OUTER_BOUND ( 'NONE', #60414, .T. ) ;
#122613 = DIRECTION ( 'NONE',  ( 1.000000000000000000, 0.000000000000000000, 0.000000000000000000 ) ) ;
#122616 = ORIENTED_EDGE ( 'NONE', *, *, #208445, .T. ) ;
#122615 = CARTESIAN_POINT ( 'NONE',  ( -18.59999999999999787, 57.82359945636609666, -226.0354702357591350 ) ) ;
#122617 = AXIS2_PLACEMENT_3D ( 'NONE', #311, #79832, #12523 ) ;
#122618 = ADVANCED_FACE ( 'NONE', ( #220394 ), #15132, .F. ) ;
#122619 = AXIS2_PLACEMENT_3D ( 'NONE', #201289, #44793, #46064 ) ;
#122620 = PRODUCT ( 'Snap Open Cable Crossbars 4', 'Snap Open Cable Crossbars 4', '', ( #7671 ) ) ;
#122621 = VERTEX_POINT ( 'NONE', #9035 ) ;
#122622 = DIRECTION ( 'NONE',  ( -1.000000000000000000, 2.952720810173289112E-16, 2.061873921506763405E-30 ) ) ;
#122623 = CARTESIAN_POINT ( 'NONE',  ( -20.94999999999999929, -10.60885044396467336, -206.2784744251879090 ) ) ;
#122624 = CIRCLE ( 'NONE', #147547, 0.1000000000000028644 ) ;
#122625 = CARTESIAN_POINT ( 'NONE',  ( -20.85000000000000142, 6.846123162363745074, -104.2377262668499043 ) ) ;
#122626 = ORIENTED_EDGE ( 'NONE', *, *, #116948, .T. ) ;
#122627 = CYLINDRICAL_SURFACE ( 'NONE', #60326, 0.09999999999999939493 ) ;
#122629 = ADVANCED_FACE ( 'NONE', ( #87268 ), #51990, .F. ) ;
#122628 = B_SPLINE_CURVE_WITH_KNOTS ( 'NONE', 3,
 ( #30105, #249149, #170932, #27555, #246547, #107030 ),
 .UNSPECIFIED., .F., .F.,
 ( 4, 2, 4 ),
 ( 0.000000000000000000, 0.0001891491689349539989, 0.0003782983378699079978 ),
 .UNSPECIFIED. ) ;
#122630 = VERTEX_POINT ( 'NONE', #131548 ) ;
#122631 = CARTESIAN_POINT ( 'NONE',  ( -23.15000000000000213, -11.64999999998884483, -63.89999999999999858 ) ) ;
#122632 = CARTESIAN_POINT ( 'NONE',  ( -20.54999999999999716, 85.50000000001251976, -179.9170766071767389 ) ) ;
#122633 = CARTESIAN_POINT ( 'NONE',  ( 21.46681500593265213, 6.857511159395769162, -33.50000000000000711 ) ) ;
#122634 = AXIS2_PLACEMENT_3D ( 'NONE', #174139, #234057, #66984 ) ;
#122635 = VERTEX_POINT ( 'NONE', #126409 ) ;
#122636 = CARTESIAN_POINT ( 'NONE',  ( 23.14999999999999858, 79.90000000001214175, -136.5231074845243029 ) ) ;
#122637 = ADVANCED_FACE ( 'NONE', ( #250216 ), #63868, .F. ) ;
#122638 = AXIS2_PLACEMENT_3D ( 'NONE', #247394, #150872, #30963 ) ;
#122639 = DIRECTION ( 'NONE',  ( 1.000000000000000000, 0.000000000000000000, 0.000000000000000000 ) ) ;
#122640 = CIRCLE ( 'NONE', #39446, 0.1000000000000021844 ) ;
#122641 = VECTOR ( 'NONE', #227851, 1000.000000000000000 ) ;
#122642 = ORIENTED_EDGE ( 'NONE', *, *, #131358, .T. ) ;
#122643 = CIRCLE ( 'NONE', #18577, 0.09999999999999939493 ) ;
#122644 = ORIENTED_EDGE ( 'NONE', *, *, #16707, .F. ) ;
#122645 = EDGE_LOOP ( 'NONE', ( #213445, #118984, #10135 ) ) ;
#122646 = DIRECTION ( 'NONE',  ( 1.000000000000000000, 0.000000000000000000, 0.000000000000000000 ) ) ;
#122647 = ORIENTED_EDGE ( 'NONE', *, *, #44, .F. ) ;
#122649 = ORIENTED_EDGE ( 'NONE', *, *, #170777, .T. ) ;
#122648 = DIRECTION ( 'NONE',  ( 0.000000000000000000, -1.000000000000000000, 0.000000000000000000 ) ) ;
#122650 = EDGE_LOOP ( 'NONE', ( #111816, #219570 ) ) ;
#122653 = ORIENTED_EDGE ( 'NONE', *, *, #100993, .F. ) ;
#122652 = ORIENTED_EDGE ( 'NONE', *, *, #26090, .T. ) ;
#122651 = CARTESIAN_POINT ( 'NONE',  ( -16.78055652883087134, 9.946776916136505164, -113.1607918375924697 ) ) ;
#122654 = ORIENTED_EDGE ( 'NONE', *, *, #89119, .T. ) ;
#122655 = CARTESIAN_POINT ( 'NONE',  ( -1.739115166359751801E-14, 64.35000000001221565, -145.1731074845244507 ) ) ;
#122656 = CIRCLE ( 'NONE', #126732, 0.09999999999998898659 ) ;
#122657 = CARTESIAN_POINT ( 'NONE',  ( 20.94999999999999574, 77.26178616857734482, -161.9366085209788650 ) ) ;
#122658 = ADVANCED_FACE ( 'NONE', ( #29910 ), #228096, .F. ) ;
#122659 = CARTESIAN_POINT ( 'NONE',  ( -16.77180007708460252, 14.16206291785975857, -219.2691289366548517 ) ) ;
#122660 = ORIENTED_EDGE ( 'NONE', *, *, #51312, .T. ) ;
#122661 = DIRECTION ( 'NONE',  ( 0.000000000000000000, 0.2128009952263604232, -0.9770955615653316162 ) ) ;
#122662 = CIRCLE ( 'NONE', #214784, 0.3999999999999975797 ) ;
#122664 = ORIENTED_EDGE ( 'NONE', *, *, #142246, .F. ) ;
#122663 = DIRECTION ( 'NONE',  ( 0.000000000000000000, -6.938893903907222067E-15, 1.000000000000000000 ) ) ;
#122665 = CARTESIAN_POINT ( 'NONE',  ( -18.59999999999999787, -1.135018845899022466, -208.7169768834322952 ) ) ;
#122667 = ORIENTED_EDGE ( 'NONE', *, *, #37225, .F. ) ;
#122666 = DIRECTION ( 'NONE',  ( -1.000000000000000000, -0.000000000000000000, -0.000000000000000000 ) ) ;
#122668 = EDGE_CURVE ( 'NONE', #8823, #59550, #76312, .T. ) ;
#122669 = EDGE_CURVE ( 'NONE', #185482, #162306, #120229, .T. ) ;
#122670 = EDGE_LOOP ( 'NONE', ( #144748, #30075, #203667, #56405 ) ) ;
#122671 = DIRECTION ( 'NONE',  ( -1.000000000000000000, 0.000000000000000000, -0.000000000000000000 ) ) ;
#122672 = EDGE_CURVE ( 'NONE', #175831, #163280, #47651, .T. ) ;
#122673 = EDGE_CURVE ( 'NONE', #220305, #74961, #109403, .T. ) ;
#122674 = ORIENTED_EDGE ( 'NONE', *, *, #96598, .T. ) ;
#122675 = ORIENTED_EDGE ( 'NONE', *, *, #11084, .F. ) ;
#122676 = CYLINDRICAL_SURFACE ( 'NONE', #172811, 0.1000000000000000472 ) ;
#122678 = EDGE_CURVE ( 'NONE', #75171, #96108, #207256, .T. ) ;
#122677 = CARTESIAN_POINT ( 'NONE',  ( -21.64999999999999858, 11.58468387039765801, -220.1227639117171861 ) ) ;
#122679 = ADVANCED_FACE ( 'NONE', ( #91137 ), #149851, .T. ) ;
#122681 = ORIENTED_EDGE ( 'NONE', *, *, #141157, .T. ) ;
#122680 = ORIENTED_EDGE ( 'NONE', *, *, #52177, .F. ) ;
#122682 = CIRCLE ( 'NONE', #76861, 0.1000000000000002554 ) ;
#122683 = ORIENTED_EDGE ( 'NONE', *, *, #241128, .F. ) ;
#122684 = CARTESIAN_POINT ( 'NONE',  ( 21.05281448260627641, 61.94770618465719991, -221.8088539820179506 ) ) ;
#122685 = ORIENTED_EDGE ( 'NONE', *, *, #31914, .F. ) ;
#122686 = ORIENTED_EDGE ( 'NONE', *, *, #51019, .T. ) ;
#122687 = EDGE_CURVE ( 'NONE', #7520, #121164, #245078, .T. ) ;
#122688 = LINE ( 'NONE', #23604, #188496 ) ;
#122690 = ORIENTED_EDGE ( 'NONE', *, *, #204784, .F. ) ;
#122689 = DIRECTION ( 'NONE',  ( 1.000000000000000000, -0.000000000000000000, -0.000000000000000000 ) ) ;
#122691 = CARTESIAN_POINT ( 'NONE',  ( 21.05000000000000071, 53.86595165227826243, -236.3638196928718855 ) ) ;
#122693 = DIRECTION ( 'NONE',  ( -1.000000000000000000, -0.000000000000000000, -0.000000000000000000 ) ) ;
#122692 = CARTESIAN_POINT ( 'NONE',  ( -16.94275863009466576, 22.95996116793751085, -230.8805586247883639 ) ) ;
#122694 = ORIENTED_EDGE ( 'NONE', *, *, #197365, .T. ) ;
#122696 = VERTEX_POINT ( 'NONE', #187695 ) ;
#122695 = ORIENTED_EDGE ( 'NONE', *, *, #202284, .F. ) ;
#122697 = FACE_OUTER_BOUND ( 'NONE', #17597, .T. ) ;
#122698 = ORIENTED_EDGE ( 'NONE', *, *, #147342, .T. ) ;
#122699 = AXIS2_PLACEMENT_3D ( 'NONE', #232258, #52288, #108440 ) ;
#122700 = TOROIDAL_SURFACE ( 'NONE', #126769, 0.4000000000000005773, 0.1000000000000000056 ) ;
#122701 = VECTOR ( 'NONE', #127023, 1000.000000000000227 ) ;
#122702 = EDGE_CURVE ( 'NONE', #230038, #251252, #168157, .T. ) ;
#122703 = DIRECTION ( 'NONE',  ( 1.000000000000000000, 2.952720810173289112E-16, -0.000000000000000000 ) ) ;
#122704 = ORIENTED_EDGE ( 'NONE', *, *, #71366, .F. ) ;
#122705 = ORIENTED_EDGE ( 'NONE', *, *, #217003, .T. ) ;
#122706 = MECHANICAL_DESIGN_GEOMETRIC_PRESENTATION_REPRESENTATION (  '', ( #51925 ), #168520 ) ;
#122707 = CARTESIAN_POINT ( 'NONE',  ( 18.59999999999999076, 69.55000000001261640, -193.5060803140843859 ) ) ;
#122709 = EDGE_CURVE ( 'NONE', #197247, #182665, #147635, .T. ) ;
#122708 = ORIENTED_EDGE ( 'NONE', *, *, #78769, .F. ) ;
#122710 = DIRECTION ( 'NONE',  ( 0.000000000000000000, -1.000000000000000000, 0.000000000000000000 ) ) ;
#122711 = DIRECTION ( 'NONE',  ( 0.000000000000000000, 0.9893560106964510714, -0.1455152366551481502 ) ) ;
#122712 = ORIENTED_EDGE ( 'NONE', *, *, #86220, .F. ) ;
#122713 = ADVANCED_FACE ( 'NONE', ( #177120 ), #132848, .T. ) ;
#122714 = CARTESIAN_POINT ( 'NONE',  ( -20.64999999999999858, 2.400000000011155432, -180.7246219227620543 ) ) ;
#122715 = CARTESIAN_POINT ( 'NONE',  ( 5.900000000000060751, 64.65000000001120384, -22.02310748452479316 ) ) ;
#122717 = DIRECTION ( 'NONE',  ( 0.000000000000000000, -1.000000000000000000, 0.000000000000000000 ) ) ;
#122716 = CARTESIAN_POINT ( 'NONE',  ( 23.24999999999999289, 66.34920340998563404, -213.7018660128499334 ) ) ;
#122718 = FACE_OUTER_BOUND ( 'NONE', #31008, .T. ) ;
#122719 = CARTESIAN_POINT ( 'NONE',  ( -16.94107738177414291, 65.98576071487489969, -48.57310748452439952 ) ) ;
#122720 = DIRECTION ( 'NONE',  ( -1.000000000000000000, 0.000000000000000000, 0.000000000000000000 ) ) ;
#122721 = CIRCLE ( 'NONE', #43030, 0.09999999999998898659 ) ;
#122722 = DIRECTION ( 'NONE',  ( 0.000000000000000000, 0.000000000000000000, -1.000000000000000000 ) ) ;
#122723 = DIRECTION ( 'NONE',  ( 0.000000000000000000, -0.1350103645451904977, 0.9908441862701596881 ) ) ;
#122724 = VECTOR ( 'NONE', #113074, 1000.000000000000000 ) ;
#122725 = ORIENTED_EDGE ( 'NONE', *, *, #198067, .F. ) ;
#122726 = AXIS2_PLACEMENT_3D ( 'NONE', #243827, #166903, #229415 ) ;
#122727 = AXIS2_PLACEMENT_3D ( 'NONE', #65871, #129701, #28062 ) ;
#122729 = ORIENTED_EDGE ( 'NONE', *, *, #209158, .F. ) ;
#122728 = ORIENTED_EDGE ( 'NONE', *, *, #104546, .T. ) ;
#122730 = ORIENTED_EDGE ( 'NONE', *, *, #189806, .T. ) ;
#122731 = AXIS2_PLACEMENT_3D ( 'NONE', #82058, #101614, #140785 ) ;
#122732 = CARTESIAN_POINT ( 'NONE',  ( 21.05000000000000071, 76.10000000001198828, -109.5637644362255543 ) ) ;
#122733 = DIRECTION ( 'NONE',  ( -1.836970198721029934E-16, -1.000000000000000000, -6.982962677686266711E-15 ) ) ;
#122735 = CARTESIAN_POINT ( 'NONE',  ( -14.11697426661281618, 9.457410944767410399, -15.00008397379002822 ) ) ;
#122734 = CARTESIAN_POINT ( 'NONE',  ( -18.59999999999999787, 64.35000000001190301, -96.00830171387039513 ) ) ;
#122736 = DIRECTION ( 'NONE',  ( -1.000000000000000000, -2.952720810173289112E-16, 0.000000000000000000 ) ) ;
#122737 = ORIENTED_EDGE ( 'NONE', *, *, #121766, .T. ) ;
#122738 = VECTOR ( 'NONE', #87857, 1000.000000000000000 ) ;
#122739 = DIRECTION ( 'NONE',  ( 1.000000000000000000, -7.304098846218133681E-16, 0.000000000000000000 ) ) ;
#122740 = TOROIDAL_SURFACE ( 'NONE', #222641, 4.149999999999999467, 0.1000000000000000056 ) ;
#122742 = AXIS2_PLACEMENT_3D ( 'NONE', #130888, #133465, #229991 ) ;
#122741 = CARTESIAN_POINT ( 'NONE',  ( 20.94999999999999929, 76.00000000001142553, -36.02310748452432421 ) ) ;
#122743 = DIRECTION ( 'NONE',  ( -1.000000000000000000, -0.000000000000000000, -0.000000000000000000 ) ) ;
#122744 = DIRECTION ( 'NONE',  ( 1.000000000000000000, -0.000000000000000000, -0.000000000000000000 ) ) ;
#122746 = EDGE_LOOP ( 'NONE', ( #179364, #211112, #60050, #28714 ) ) ;
#122745 = AXIS2_PLACEMENT_3D ( 'NONE', #207595, #210156, #87607 ) ;
#122747 = DIRECTION ( 'NONE',  ( 0.000000000000000000, 6.982962677686266711E-15, -1.000000000000000000 ) ) ;
#122748 = CIRCLE ( 'NONE', #39554, 0.5000000000000076605 ) ;
#122749 = CARTESIAN_POINT ( 'NONE',  ( -21.05000000000000426, 0.09843750001115451898, -94.20076908991316600 ) ) ;
#122750 = EDGE_LOOP ( 'NONE', ( #246197, #55766, #17613, #243204 ) ) ;
#122751 = DIRECTION ( 'NONE',  ( -0.000000000000000000, 0.000000000000000000, -1.000000000000000000 ) ) ;
#122752 = CARTESIAN_POINT ( 'NONE',  ( 20.94999999999999929, 36.65892442174472876, -249.5511627012454596 ) ) ;
#122753 = CARTESIAN_POINT ( 'NONE',  ( 21.00000000000000000, 9.750000000011153745, -188.6499999999999488 ) ) ;
#122754 = VECTOR ( 'NONE', #79281, 1000.000000000000000 ) ;
#122755 = CARTESIAN_POINT ( 'NONE',  ( 20.94999999999999929, 76.00000000001165290, -69.52310748452431710 ) ) ;
#122757 = ORIENTED_EDGE ( 'NONE', *, *, #74740, .F. ) ;
#122756 = CIRCLE ( 'NONE', #10323, 0.09999999999999939493 ) ;
#122758 = CARTESIAN_POINT ( 'NONE',  ( 18.39999999999999858, 46.96039402156216624, -255.3459641718773128 ) ) ;
#122759 = CARTESIAN_POINT ( 'NONE',  ( -20.64999999999999858, -8.999999999988844479, -157.6060308773475924 ) ) ;
#122760 = CARTESIAN_POINT ( 'NONE',  ( -21.05000000000000071, -0.09999996528894432302, -60.52244781750656699 ) ) ;
#122761 = ADVANCED_FACE ( 'NONE', ( #37600 ), #113270, .F. ) ;
#122763 = DIRECTION ( 'NONE',  ( 1.000000000000000000, 0.000000000000000000, 0.000000000000000000 ) ) ;
#122762 = CARTESIAN_POINT ( 'NONE',  ( 19.58285714285715073, 65.61500148966017321, -61.89342281713445004 ) ) ;
#122764 = DIRECTION ( 'NONE',  ( -1.000000000000000000, 0.000000000000000000, 0.000000000000000000 ) ) ;
#122765 = CARTESIAN_POINT ( 'NONE',  ( 21.05000000000000071, 62.08148826970417389, -247.6553521922769221 ) ) ;
#122767 = EDGE_CURVE ( 'NONE', #167954, #13968, #201788, .T. ) ;
#122766 = FACE_OUTER_BOUND ( 'NONE', #87648, .T. ) ;
#122768 = DIRECTION ( 'NONE',  ( -3.469446951953679822E-14, -0.9770955615653551529, -0.2128009952262517601 ) ) ;
#122770 = VERTEX_POINT ( 'NONE', #75456 ) ;
#122769 = CYLINDRICAL_SURFACE ( 'NONE', #206920, 0.1000000000000038219 ) ;
#122771 = ORIENTED_EDGE ( 'NONE', *, *, #36632, .T. ) ;
#122772 = EDGE_CURVE ( 'NONE', #194221, #189304, #255288, .T. ) ;
#122773 = ADVANCED_FACE ( 'NONE', ( #195400 ), #172007, .T. ) ;
#122774 = AXIS2_PLACEMENT_3D ( 'NONE', #216176, #58368, #37571 ) ;
#122775 = AXIS2_PLACEMENT_3D ( 'NONE', #93723, #173318, #211108 ) ;
#122776 = CYLINDRICAL_SURFACE ( 'NONE', #196410, 0.09999999999999939493 ) ;
#122777 = VECTOR ( 'NONE', #224853, 1000.000000000000000 ) ;
#122778 = CARTESIAN_POINT ( 'NONE',  ( 15.06592377766031454, 9.417789466963359502, -149.3573845439768775 ) ) ;
#122779 = ORIENTED_EDGE ( 'NONE', *, *, #203827, .T. ) ;
#122780 = EDGE_CURVE ( 'NONE', #105518, #200975, #94981, .T. ) ;
#122781 = DIRECTION ( 'NONE',  ( 0.000000000000000000, 2.664535259100315349E-15, -1.000000000000000000 ) ) ;
#122782 = EDGE_CURVE ( 'NONE', #31617, #168244, #137945, .T. ) ;
#122783 = DIRECTION ( 'NONE',  ( 0.000000000000000000, -1.000000000000000000, 0.000000000000000000 ) ) ;
#122784 = CARTESIAN_POINT ( 'NONE',  ( -18.39999999999999858, -9.599999999988845900, -73.70018939122203960 ) ) ;
#122785 = AXIS2_PLACEMENT_3D ( 'NONE', #124517, #145343, #8421 ) ;
#122786 = AXIS2_PLACEMENT_3D ( 'NONE', #211896, #33283, #128492 ) ;
#122787 = VERTEX_POINT ( 'NONE', #234490 ) ;
#122788 = LINE ( 'NONE', #81046, #232806 ) ;
#122790 = ORIENTED_EDGE ( 'NONE', *, *, #80581, .T. ) ;
#122789 = DIRECTION ( 'NONE',  ( 0.000000000000000000, -0.8814952561688425003, 0.4721928772777359007 ) ) ;
#122791 = DIRECTION ( 'NONE',  ( 0.000000000000000000, 0.9126074666063771490, 0.4088369013363281623 ) ) ;
#122792 = VERTEX_POINT ( 'NONE', #252764 ) ;
#122793 = VECTOR ( 'NONE', #37096, 1000.000000000000114 ) ;
#122794 = LINE ( 'NONE', #81057, #79253 ) ;
#122795 = VECTOR ( 'NONE', #163263, 1000.000000000000000 ) ;
#122796 = EDGE_CURVE ( 'NONE', #218186, #99277, #88782, .T. ) ;
#122797 = DIRECTION ( 'NONE',  ( -1.000000000000000000, 0.000000000000000000, 0.000000000000000000 ) ) ;
#122798 = ORIENTED_EDGE ( 'NONE', *, *, #80233, .F. ) ;
#122799 = DIRECTION ( 'NONE',  ( 2.952720810173289112E-16, 1.000000000000000000, 6.982962677686266711E-15 ) ) ;
#122800 = EDGE_CURVE ( 'NONE', #139895, #199876, #56025, .T. ) ;
#122801 = DIRECTION ( 'NONE',  ( 0.5000000000001141309, -6.047423072554455661E-15, 0.8660254037843729824 ) ) ;
#122802 = CARTESIAN_POINT ( 'NONE',  ( -20.64999999999999858, 74.00000000001223555, -149.2477294072864709 ) ) ;
#122803 = CARTESIAN_POINT ( 'NONE',  ( -22.50000000000000000, 1.115600667400684642E-11, -134.0000000000000000 ) ) ;
#122804 = ORIENTED_EDGE ( 'NONE', *, *, #155117, .F. ) ;
#122805 = VECTOR ( 'NONE', #207814, 1000.000000000000114 ) ;
#122806 = ORIENTED_EDGE ( 'NONE', *, *, #37072, .F. ) ;
#122807 = EDGE_CURVE ( 'NONE', #120433, #140343, #197924, .T. ) ;
#122808 = CARTESIAN_POINT ( 'NONE',  ( 21.14999999999999503, 76.10000000001222986, -148.1726782920690937 ) ) ;
#122809 = EDGE_CURVE ( 'NONE', #34777, #172898, #97134, .T. ) ;
#122810 = CARTESIAN_POINT ( 'NONE',  ( 23.24999999999999645, 5.600000000011153389, -21.75000000000000355 ) ) ;
#122811 = DIRECTION ( 'NONE',  ( -3.265361837132813093E-16, -0.4088369013363053472, 0.9126074666063872520 ) ) ;
#122812 = CARTESIAN_POINT ( 'NONE',  ( 21.05000000000000071, 10.56271494673980271, -141.4568021056454654 ) ) ;
#122813 = CYLINDRICAL_SURFACE ( 'NONE', #128424, 0.09999999999999939493 ) ;
#122814 = ADVANCED_FACE ( 'NONE', ( #256572 ), #153738, .T. ) ;
#122815 = LINE ( 'NONE', #47087, #52654 ) ;
#122816 = CARTESIAN_POINT ( 'NONE',  ( -16.80100426158789872, 66.05684947961542264, -56.84016173169033692 ) ) ;
#122817 = CARTESIAN_POINT ( 'NONE',  ( 22.50927854361892244, 76.10085807354001020, -148.2726746105511779 ) ) ;
#122818 = ORIENTED_EDGE ( 'NONE', *, *, #99946, .F. ) ;
#122819 = DIRECTION ( 'NONE',  ( -4.408576920032448588E-17, 0.1350103645451876944, -0.9908441862701601321 ) ) ;
#122820 = AXIS2_PLACEMENT_3D ( 'NONE', #104982, #165001, #758 ) ;
#122822 = ORIENTED_EDGE ( 'NONE', *, *, #194042, .F. ) ;
#122821 = CARTESIAN_POINT ( 'NONE',  ( -20.54999999999999716, 76.00000000001189449, -101.0231074845243029 ) ) ;
#122823 = CIRCLE ( 'NONE', #243602, 0.09999999999998898659 ) ;
#122824 = DIRECTION ( 'NONE',  ( 0.000000000000000000, 0.000000000000000000, 1.000000000000000000 ) ) ;
#122825 = CYLINDRICAL_SURFACE ( 'NONE', #61658, 3.999999999999996447 ) ;
#122827 = FACE_OUTER_BOUND ( 'NONE', #97636, .T. ) ;
#122826 = CARTESIAN_POINT ( 'NONE',  ( 21.46681500597710013, 76.00000000001200817, -109.8806186439539516 ) ) ;
#122828 = ORIENTED_EDGE ( 'NONE', *, *, #189155, .F. ) ;
#122830 = CARTESIAN_POINT ( 'NONE',  ( -18.60000000000000142, -8.150000000000005684, 33.00000000000000000 ) ) ;
#122829 = CARTESIAN_POINT ( 'NONE',  ( -18.50000000000000000, 66.75000000001199396, -115.3731074845243683 ) ) ;
#122831 = CARTESIAN_POINT ( 'NONE',  ( 20.94999999999999929, 1.115600667400684642E-11, -167.5000000000000284 ) ) ;
#122832 = EDGE_CURVE ( 'NONE', #28459, #141595, #54570, .T. ) ;
#122833 = FACE_OUTER_BOUND ( 'NONE', #176460, .T. ) ;
#122834 = DIRECTION ( 'NONE',  ( 1.000000000000000000, 0.000000000000000000, 0.000000000000000000 ) ) ;
#122835 = CARTESIAN_POINT ( 'NONE',  ( -21.05000000000000071, 77.85102823015243700, -57.86919421510181394 ) ) ;
#122836 = ORIENTED_EDGE ( 'NONE', *, *, #111463, .F. ) ;
#122837 = VERTEX_POINT ( 'NONE', #214932 ) ;
#122838 = ADVANCED_FACE ( 'NONE', ( #212386 ), #19302, .T. ) ;
#122839 = CARTESIAN_POINT ( 'NONE',  ( 21.15000000000005187, 77.25000000001119815, -43.92310748452479885 ) ) ;
#122840 = ORIENTED_EDGE ( 'NONE', *, *, #255162, .F. ) ;
#122841 = FACE_OUTER_BOUND ( 'NONE', #159805, .T. ) ;
#122842 = AXIS2_PLACEMENT_3D ( 'NONE', #135181, #20402, #38669 ) ;
#122843 = ORIENTED_EDGE ( 'NONE', *, *, #23246, .T. ) ;
#122844 = DIRECTION ( 'NONE',  ( 0.000000000000000000, 0.9126074666063770380, 0.4088369013363281068 ) ) ;
#122845 = VECTOR ( 'NONE', #113506, 1000.000000000000000 ) ;
#122846 = CARTESIAN_POINT ( 'NONE',  ( -18.59999999999999787, 77.73625713161000306, -191.9544551555068495 ) ) ;
#122847 = ORIENTED_EDGE ( 'NONE', *, *, #249123, .T. ) ;
#122848 = CARTESIAN_POINT ( 'NONE',  ( -16.80469485234341676, 9.942151663152195340, -87.80996684393123530 ) ) ;
#122849 = CARTESIAN_POINT ( 'NONE',  ( -21.05000000000000782, 65.51923798433685420, -242.1677427744925808 ) ) ;
#122850 = DIRECTION ( 'NONE',  ( 0.000000000000000000, 0.000000000000000000, -1.000000000000000000 ) ) ;
#122851 = CARTESIAN_POINT ( 'NONE',  ( -21.14999999999994174, 76.00000000001119815, -36.02310748452479316 ) ) ;
#122852 = DIRECTION ( 'NONE',  ( 0.000000000000000000, 6.982962677686266711E-15, -1.000000000000000000 ) ) ;
#122853 = DIRECTION ( 'NONE',  ( 0.000000000000000000, 0.000000000000000000, -1.000000000000000000 ) ) ;
#122854 = CARTESIAN_POINT ( 'NONE',  ( 20.04142135391667168, 62.35689476345314119, -208.9382773759953409 ) ) ;
#122855 = VERTEX_POINT ( 'NONE', #18011 ) ;
#122857 = DIRECTION ( 'NONE',  ( 0.000000000000000000, 0.1290532225515364506, 0.9916376685811525427 ) ) ;
#122856 = FACE_OUTER_BOUND ( 'NONE', #212221, .T. ) ;
#122858 = VERTEX_POINT ( 'NONE', #97516 ) ;
#122860 = EDGE_LOOP ( 'NONE', ( #215295, #152542, #102476 ) ) ;
#122859 = LINE ( 'NONE', #160724, #160709 ) ;
#122861 = AXIS2_PLACEMENT_3D ( 'NONE', #190925, #52652, #111361 ) ;
#122862 = ORIENTED_EDGE ( 'NONE', *, *, #14937, .F. ) ;
#122863 = MECHANICAL_DESIGN_GEOMETRIC_PRESENTATION_REPRESENTATION (  '', ( #218487 ), #110362 ) ;
#122864 = DIRECTION ( 'NONE',  ( 1.000000000000000000, -0.000000000000000000, -0.000000000000000000 ) ) ;
#122865 = CARTESIAN_POINT ( 'NONE',  ( -18.40000000000000213, 8.822561741677553471, -76.25000000000004263 ) ) ;
#122866 = DIRECTION ( 'NONE',  ( 0.000000000000000000, 0.8660254037844420383, -0.4999999999999943379 ) ) ;
#122867 = CARTESIAN_POINT ( 'NONE',  ( -21.14999999999999858, -1.236118717437885595, -194.8647072476926496 ) ) ;
#122868 = ORIENTED_EDGE ( 'NONE', *, *, #140521, .T. ) ;
#122869 = DIRECTION ( 'NONE',  ( 0.000000000000000000, 0.5000000000000078826, -0.8660254037844340447 ) ) ;
#122870 = LINE ( 'NONE', #184106, #214640 ) ;
#122871 = ORIENTED_EDGE ( 'NONE', *, *, #167574, .T. ) ;
#122872 = FACE_OUTER_BOUND ( 'NONE', #46977, .T. ) ;
#122873 = EDGE_CURVE ( 'NONE', #243788, #131621, #115836, .T. ) ;
#122875 = AXIS2_PLACEMENT_3D ( 'NONE', #150839, #126125, #131275 ) ;
#122874 = DIRECTION ( 'NONE',  ( 0.000000000000000000, 0.000000000000000000, -1.000000000000000000 ) ) ;
#122876 = ORIENTED_EDGE ( 'NONE', *, *, #82777, .F. ) ;
#122878 = DIRECTION ( 'NONE',  ( 0.000000000000000000, 0.000000000000000000, 1.000000000000000000 ) ) ;
#122877 = AXIS2_PLACEMENT_3D ( 'NONE', #5142, #160431, #239949 ) ;
#122879 = CIRCLE ( 'NONE', #43751, 0.09999999999999897859 ) ;
#122880 = AXIS2_PLACEMENT_3D ( 'NONE', #88711, #7930, #105699 ) ;
#122881 = CARTESIAN_POINT ( 'NONE',  ( 18.59999999999999076, 1.750000000011155743, -78.66951155790169992 ) ) ;
#122882 = EDGE_LOOP ( 'NONE', ( #197044, #71573, #92453, #209621 ) ) ;
#122883 = DIRECTION ( 'NONE',  ( -1.000000000000000000, 0.000000000000000000, -0.000000000000000000 ) ) ;
#122884 = COLOUR_RGB ( '', 0.08235294, 0.09019608, 0.10196078) ;
#122885 = ADVANCED_FACE ( 'NONE', ( #157574 ), #118415, .F. ) ;
#122886 = CARTESIAN_POINT ( 'NONE',  ( -21.45000000000000284, 7.708578643773852157, -155.2500000000000284 ) ) ;
#122887 = CARTESIAN_POINT ( 'NONE',  ( 19.88284271247463053, 16.69046054743353125, -222.6951690485254858 ) ) ;
#122888 = CARTESIAN_POINT ( 'NONE',  ( 23.14999999999999503, 69.45000000001222418, -148.8731074845244109 ) ) ;
#122889 = ADVANCED_FACE ( 'NONE', ( #257858 ), #110204, .F. ) ;
#122890 = EDGE_CURVE ( 'NONE', #115133, #22692, #127068, .T. ) ;
#122891 = CYLINDRICAL_SURFACE ( 'NONE', #224734, 11.74999999999999645 ) ;
#122892 = DIRECTION ( 'NONE',  ( 1.000000000000000000, -0.000000000000000000, -0.000000000000000000 ) ) ;
#122893 = CARTESIAN_POINT ( 'NONE',  ( 21.05000000000003979, 83.90000000001120384, -37.18565239344504647 ) ) ;
#122894 = TOROIDAL_SURFACE ( 'NONE', #10287, 4.900000000000003020, 0.1000000000000000056 ) ;
#122895 = ORIENTED_EDGE ( 'NONE', *, *, #124046, .F. ) ;
#122897 = DIRECTION ( 'NONE',  ( 0.000000000000000000, 1.000000000000000000, 0.000000000000000000 ) ) ;
#122896 = CARTESIAN_POINT ( 'NONE',  ( 17.74533788810829904, 10.81849979147079210, -23.18637732505242610 ) ) ;
#122898 = VECTOR ( 'NONE', #166955, 1000.000000000000000 ) ;
#122899 = AXIS2_PLACEMENT_3D ( 'NONE', #92354, #171943, #231895 ) ;
#122900 = EDGE_LOOP ( 'NONE', ( #189118, #193198, #227379, #254982 ) ) ;
#122901 = FACE_OUTER_BOUND ( 'NONE', #141790, .T. ) ;
#122902 = EDGE_CURVE ( 'NONE', #181206, #122058, #167947, .T. ) ;
#122903 = CARTESIAN_POINT ( 'NONE',  ( -23.15000000000000213, -8.999999999988844479, -157.6060308773475924 ) ) ;
#122905 = ORIENTED_EDGE ( 'NONE', *, *, #246825, .F. ) ;
#122904 = CARTESIAN_POINT ( 'NONE',  ( -18.50000000000000000, 76.00000000001142553, -36.02310748452432421 ) ) ;
#122907 = ORIENTED_EDGE ( 'NONE', *, *, #20571, .T. ) ;
#122906 = CARTESIAN_POINT ( 'NONE',  ( -18.41418431465368144, 85.50000000001233502, -129.9229180933028829 ) ) ;
#122908 = DIRECTION ( 'NONE',  ( 1.000000000000000000, 0.000000000000000000, 0.000000000000000000 ) ) ;
#122909 = LINE ( 'NONE', #82452, #109032 ) ;
#122910 = LINE ( 'NONE', #79883, #176951 ) ;
#122911 = CARTESIAN_POINT ( 'NONE',  ( 20.85000000000000142, 78.48087866980282001, -232.8271061603568910 ) ) ;
#122912 = AXIS2_PLACEMENT_3D ( 'NONE', #187332, #45235, #7385 ) ;
#122913 = AXIS2_PLACEMENT_3D ( 'NONE', #52717, #13611, #74894 ) ;
#122915 = ORIENTED_EDGE ( 'NONE', *, *, #216461, .T. ) ;
#122914 = DIRECTION ( 'NONE',  ( 0.000000000000000000, 0.000000000000000000, -1.000000000000000000 ) ) ;
#122916 = VECTOR ( 'NONE', #146294, 1000.000000000000000 ) ;
#122917 = CARTESIAN_POINT ( 'NONE',  ( 21.14999999999999858, 78.47509609352879068, -238.9045489380306435 ) ) ;
#122918 = ORIENTED_EDGE ( 'NONE', *, *, #94026, .T. ) ;
#122919 = ADVANCED_FACE ( 'NONE', ( #59684 ), #79248, .T. ) ;
#122920 = ORIENTED_EDGE ( 'NONE', *, *, #208124, .T. ) ;
#122921 = TOROIDAL_SURFACE ( 'NONE', #10495, 0.2000000000000000111, 0.1000000000000000056 ) ;
#122922 = CARTESIAN_POINT ( 'NONE',  ( -18.42637059832564361, 85.49694546190107758, -29.41403017472442727 ) ) ;
#122923 = FACE_OUTER_BOUND ( 'NONE', #402, .T. ) ;
#122924 = CIRCLE ( 'NONE', #81192, 12.77499999999999503 ) ;
#122926 = ORIENTED_EDGE ( 'NONE', *, *, #103790, .F. ) ;
#122925 = AXIS2_PLACEMENT_3D ( 'NONE', #101334, #23166, #162660 ) ;
#122927 = DIRECTION ( 'NONE',  ( 0.000000000000000000, 0.000000000000000000, -1.000000000000000000 ) ) ;
#122929 = EDGE_CURVE ( 'NONE', #61597, #201908, #55447, .T. ) ;
#122928 = CARTESIAN_POINT ( 'NONE',  ( 21.05000000000000071, 18.71171618620643429, -229.8673829423568691 ) ) ;
#122930 = ORIENTED_EDGE ( 'NONE', *, *, #109358, .T. ) ;
#122931 = DIRECTION ( 'NONE',  ( 0.000000000000000000, -0.8660254037844412611, -0.4999999999999956701 ) ) ;
#122932 = CARTESIAN_POINT ( 'NONE',  ( -21.14999999999994174, 77.83551161375991967, -47.52760213295649550 ) ) ;
#122933 = ORIENTED_EDGE ( 'NONE', *, *, #12921, .F. ) ;
#122934 = VERTEX_POINT ( 'NONE', #227440 ) ;
#122935 = FACE_OUTER_BOUND ( 'NONE', #33699, .T. ) ;
#122936 = ORIENTED_EDGE ( 'NONE', *, *, #12892, .F. ) ;
#122937 = SPHERICAL_SURFACE ( 'NONE', #50478, 0.1000000000000000056 ) ;
#122938 = VERTEX_POINT ( 'NONE', #46233 ) ;
#122940 = EDGE_LOOP ( 'NONE', ( #251800, #156499, #244288, #61101 ) ) ;
#122939 = DIRECTION ( 'NONE',  ( 1.000000000000000000, 6.938893903907222067E-15, 0.000000000000000000 ) ) ;
#122941 = DIRECTION ( 'NONE',  ( 0.000000000000000000, -1.776356839400254803E-15, 1.000000000000000000 ) ) ;
#122942 = ORIENTED_EDGE ( 'NONE', *, *, #16658, .T. ) ;
#122943 = AXIS2_PLACEMENT_3D ( 'NONE', #206271, #44634, #62905 ) ;
#122944 = CARTESIAN_POINT ( 'NONE',  ( 22.50927854361889047, -0.1008580735143608520, -88.75043287397312497 ) ) ;
#122945 = ORIENTED_EDGE ( 'NONE', *, *, #107567, .T. ) ;
#122946 = CIRCLE ( 'NONE', #143770, 0.09999999999999938105 ) ;
#122948 = ORIENTED_EDGE ( 'NONE', *, *, #8973, .F. ) ;
#122947 = ORIENTED_EDGE ( 'NONE', *, *, #205642, .T. ) ;
#122949 = CARTESIAN_POINT ( 'NONE',  ( 21.07928932188134397, 69.67148334361883144, -136.6220026301787698 ) ) ;
#122950 = AXIS2_PLACEMENT_3D ( 'NONE', #23828, #242837, #244116 ) ;
#122951 = CARTESIAN_POINT ( 'NONE',  ( -16.94275863006528482, 14.20646624631278065, -219.2874100846283625 ) ) ;
#122952 = ORIENTED_EDGE ( 'NONE', *, *, #110695, .T. ) ;
#122953 = AXIS2_PLACEMENT_3D ( 'NONE', #186762, #66798, #203742 ) ;
#122954 = EDGE_CURVE ( 'NONE', #9026, #136054, #164909, .T. ) ;
#122955 = CIRCLE ( 'NONE', #10531, 0.1000000000000088318 ) ;
#122956 = ADVANCED_FACE ( 'NONE', ( #128359 ), #125770, .T. ) ;
#122957 = ORIENTED_EDGE ( 'NONE', *, *, #131679, .T. ) ;
#122958 = DIRECTION ( 'NONE',  ( 1.000000000000000000, -2.952720810173289112E-16, -2.061873921506763405E-30 ) ) ;
#122959 = LINE ( 'NONE', #163367, #147163 ) ;
#122961 = ORIENTED_EDGE ( 'NONE', *, *, #232181, .F. ) ;
#122960 = DIRECTION ( 'NONE',  ( 0.000000000000000000, 0.1686199900910463068, -0.9856811345164802063 ) ) ;
#122962 = DIRECTION ( 'NONE',  ( 1.000000000000000000, 0.000000000000000000, 0.000000000000000000 ) ) ;
#122963 = EDGE_LOOP ( 'NONE', ( #118058, #244920, #22223, #249385 ) ) ;
#122964 = EDGE_CURVE ( 'NONE', #208058, #215605, #143130, .T. ) ;
#122966 = EDGE_CURVE ( 'NONE', #109224, #97478, #126401, .T. ) ;
#122965 = CARTESIAN_POINT ( 'NONE',  ( -18.50596464788227635, 65.69367753730678317, -131.0189238066348594 ) ) ;
#122967 = DIRECTION ( 'NONE',  ( 0.000000000000000000, 0.000000000000000000, -1.000000000000000000 ) ) ;
#122968 = AXIS2_PLACEMENT_3D ( 'NONE', #27193, #229219, #230497 ) ;
#122969 = EDGE_LOOP ( 'NONE', ( #202850, #59738, #68070, #55521, #242880, #222124 ) ) ;
#122970 = CARTESIAN_POINT ( 'NONE',  ( 21.14999999999999858, 69.45000000001259366, -191.3731074845244109 ) ) ;
#122971 = CARTESIAN_POINT ( 'NONE',  ( -18.59999999999999787, 66.65000000001198543, -115.3731074845243683 ) ) ;
#122972 = CIRCLE ( 'NONE', #248229, 11.75000000000001066 ) ;
#122973 = EDGE_CURVE ( 'NONE', #156274, #220426, #100089, .T. ) ;
#122974 = ORIENTED_EDGE ( 'NONE', *, *, #215929, .F. ) ;
#122975 = CARTESIAN_POINT ( 'NONE',  ( -18.50000000000000000, 0.000000000000000000, -33.50000000000000000 ) ) ;
#122976 = ORIENTED_EDGE ( 'NONE', *, *, #146611, .F. ) ;
#122977 = ADVANCED_FACE ( 'NONE', ( #20607 ), #151371, .T. ) ;
#122979 = EDGE_CURVE ( 'NONE', #241189, #257982, #155660, .T. ) ;
#122978 = ADVANCED_FACE ( 'NONE', ( #28000 ), #38932, .T. ) ;
#122981 = ORIENTED_EDGE ( 'NONE', *, *, #66071, .T. ) ;
#122980 = EDGE_LOOP ( 'NONE', ( #37016, #199838, #117833, #190598 ) ) ;
#122982 = ORIENTED_EDGE ( 'NONE', *, *, #150886, .T. ) ;
#122983 = FACE_OUTER_BOUND ( 'NONE', #166563, .T. ) ;
#122984 = ORIENTED_EDGE ( 'NONE', *, *, #219145, .F. ) ;
#122985 = DIRECTION ( 'NONE',  ( 0.000000000000000000, -1.000000000000000000, 0.000000000000000000 ) ) ;
#122986 = VECTOR ( 'NONE', #72677, 1000.000000000000000 ) ;
#122987 = EDGE_LOOP ( 'NONE', ( #36802, #162000 ) ) ;
#122988 = CARTESIAN_POINT ( 'NONE',  ( -16.87036670365548474, 66.01058118070986325, -48.54354736722234520 ) ) ;
#122989 = CARTESIAN_POINT ( 'NONE',  ( -18.59999999999999787, 23.34004772283014972, -229.2004250369967338 ) ) ;
#122990 = ORIENTED_EDGE ( 'NONE', *, *, #67170, .F. ) ;
#122991 = EDGE_CURVE ( 'NONE', #142111, #103006, #59734, .T. ) ;
#122992 = VERTEX_POINT ( 'NONE', #104892 ) ;
#122993 = EDGE_CURVE ( 'NONE', #49603, #118225, #85339, .T. ) ;
#122994 = ADVANCED_FACE ( 'NONE', ( #147925 ), #48806, .T. ) ;
#122995 = VERTEX_POINT ( 'NONE', #232613 ) ;
#122996 = CIRCLE ( 'NONE', #206191, 0.1999999999999987899 ) ;
#122997 = CIRCLE ( 'NONE', #247884, 0.09999999999999939493 ) ;
#122998 = ADVANCED_FACE ( 'NONE', ( #31848 ), #154375, .T. ) ;
#122999 = CARTESIAN_POINT ( 'NONE',  ( 21.05000000000000426, 69.69981666374641804, -203.5744349168663518 ) ) ;
#123000 = ORIENTED_EDGE ( 'NONE', *, *, #246110, .F. ) ;
#123001 = DIRECTION ( 'NONE',  ( 0.000000000000000000, 0.8814952561688439436, -0.4721928772777330696 ) ) ;
#123002 = DIRECTION ( 'NONE',  ( -1.000000000000000000, 0.000000000000000000, 0.000000000000000000 ) ) ;
#123003 = DIRECTION ( 'NONE',  ( 1.000000000000000000, 0.000000000000000000, 0.000000000000000000 ) ) ;
#123004 = EDGE_CURVE ( 'NONE', #86293, #203870, #111357, .T. ) ;
#123005 = LINE ( 'NONE', #180405, #127747 ) ;
#123006 = PLANE ( 'NONE',  #118876 ) ;
#123008 = CARTESIAN_POINT ( 'NONE',  ( 21.09096482362050651, 34.02127186812258941, -243.7598725113532794 ) ) ;
#123007 = CARTESIAN_POINT ( 'NONE',  ( -23.15000000000000213, 1.910280373842930812, -121.3686321448010972 ) ) ;
#123009 = CARTESIAN_POINT ( 'NONE',  ( 23.40000000000005542, 77.83551161375991967, -47.52760213295649550 ) ) ;
#123011 = ADVANCED_FACE ( 'NONE', ( #52648 ), #190922, .T. ) ;
#123010 = CARTESIAN_POINT ( 'NONE',  ( 20.00000000000000711, 4.528782138689105174, 21.95447128030238915 ) ) ;
#123012 = CARTESIAN_POINT ( 'NONE',  ( -20.85000000000000142, 68.97833521811233481, -166.1895420826271277 ) ) ;
#123013 = CYLINDRICAL_SURFACE ( 'NONE', #234394, 0.09999999999999804878 ) ;
#123014 = ORIENTED_EDGE ( 'NONE', *, *, #227116, .F. ) ;
#123015 = TOROIDAL_SURFACE ( 'NONE', #10594, 0.2000000000000000111, 0.1000000000000000056 ) ;
#123017 = ORIENTED_EDGE ( 'NONE', *, *, #31919, .F. ) ;
#123016 = CARTESIAN_POINT ( 'NONE',  ( -21.14999999999999858, 87.75000000001213607, -136.5231074845242176 ) ) ;
#123018 = ORIENTED_EDGE ( 'NONE', *, *, #33100, .T. ) ;
#123019 = EDGE_CURVE ( 'NONE', #189058, #112680, #192193, .T. ) ;
#123020 = DIRECTION ( 'NONE',  ( 0.000000000000000000, 1.000000000000000000, 0.000000000000000000 ) ) ;
#123021 = CARTESIAN_POINT ( 'NONE',  ( 20.87631937322888120, 10.47149503677486138, -141.5797458745818460 ) ) ;
#123022 = FACE_OUTER_BOUND ( 'NONE', #184839, .T. ) ;
#123023 = ORIENTED_EDGE ( 'NONE', *, *, #224893, .F. ) ;
#123024 =( LENGTH_UNIT ( ) NAMED_UNIT ( * ) SI_UNIT ( .MILLI., .METRE. ) );
#123025 = DIRECTION ( 'NONE',  ( -2.952720810173289112E-16, -1.000000000000000000, -6.982962677686266711E-15 ) ) ;
#123026 = CARTESIAN_POINT ( 'NONE',  ( 21.05000000000000071, 65.49889199258218753, -241.8691648588935266 ) ) ;
#123027 = EDGE_LOOP ( 'NONE', ( #87425, #193532, #152794, #190063 ) ) ;
#123029 = DIRECTION ( 'NONE',  ( 0.000000000000000000, 0.000000000000000000, 1.000000000000000000 ) ) ;
#123028 = CIRCLE ( 'NONE', #160473, 0.1000000000000056677 ) ;
#123030 = AXIS2_PLACEMENT_3D ( 'NONE', #204545, #25927, #100294 ) ;
#123031 = DIRECTION ( 'NONE',  ( -1.000000000000000000, 0.000000000000000000, -0.000000000000000000 ) ) ;
#123032 = DIRECTION ( 'NONE',  ( 0.000000000000000000, 5.329070518200751394E-15, -1.000000000000000000 ) ) ;
#123033 = SPHERICAL_SURFACE ( 'NONE', #53739, 0.1000000000000000056 ) ;
#123035 = ORIENTED_EDGE ( 'NONE', *, *, #4536, .F. ) ;
#123034 = CARTESIAN_POINT ( 'NONE',  ( -16.94225986326249611, 66.05000000001228955, -157.0763881089165181 ) ) ;
#123036 = DIRECTION ( 'NONE',  ( -1.000000000000000000, 0.000000000000000000, 0.000000000000000000 ) ) ;
#123038 = ORIENTED_EDGE ( 'NONE', *, *, #110834, .T. ) ;
#123037 = DIRECTION ( 'NONE',  ( 0.000000000000000000, -1.000000000000000000, 0.000000000000000000 ) ) ;
#123039 = DIRECTION ( 'NONE',  ( 0.000000000000000000, 0.000000000000000000, 1.000000000000000000 ) ) ;
#123040 = CARTESIAN_POINT ( 'NONE',  ( -22.50000000000000000, 76.00000000001195133, -103.0231074845243171 ) ) ;
#123041 = CARTESIAN_POINT ( 'NONE',  ( 20.94999999999999929, 70.15000000001211333, -126.3906102602463619 ) ) ;
#123042 = DIRECTION ( 'NONE',  ( 1.186688945009010077E-16, -1.000000000000000000, -0.000000000000000000 ) ) ;
#123043 = EDGE_CURVE ( 'NONE', #29239, #197260, #151792, .T. ) ;
#123045 = DIRECTION ( 'NONE',  ( 0.000000000000000000, 0.4088369013363283289, -0.9126074666063768159 ) ) ;
#123044 = CARTESIAN_POINT ( 'NONE',  ( -23.15000000000000213, 84.59626168225530307, -160.5729799673740104 ) ) ;
#123046 = DIRECTION ( 'NONE',  ( 0.000000000000000000, 0.000000000000000000, -1.000000000000000000 ) ) ;
#123047 = FACE_OUTER_BOUND ( 'NONE', #7499, .T. ) ;
#123048 = CIRCLE ( 'NONE', #152296, 0.1000000000000028644 ) ;
#123049 =( NAMED_UNIT ( * ) PLANE_ANGLE_UNIT ( ) SI_UNIT ( $, .RADIAN. ) );
#123050 = CYLINDRICAL_SURFACE ( 'NONE', #152024, 0.09999999999999609201 ) ;
#123051 = EDGE_CURVE ( 'NONE', #70381, #177774, #176489, .T. ) ;
#123052 = VECTOR ( 'NONE', #148223, 1000.000000000000000 ) ;
#123053 = CARTESIAN_POINT ( 'NONE',  ( 20.94999999999999574, 74.83729825007431202, -162.1231074845243540 ) ) ;
#123054 = VERTEX_POINT ( 'NONE', #129633 ) ;
#123055 = CIRCLE ( 'NONE', #156403, 0.1999999999999987899 ) ;
#123056 = FACE_OUTER_BOUND ( 'NONE', #49078, .T. ) ;
#123057 = ORIENTED_EDGE ( 'NONE', *, *, #84595, .T. ) ;
#123059 = VERTEX_POINT ( 'NONE', #113916 ) ;
#123058 = PRESENTATION_LAYER_ASSIGNMENT (  '', '', ( #89720 ) ) ;
#123060 = EDGE_CURVE ( 'NONE', #198432, #65850, #14849, .T. ) ;
#123061 = CARTESIAN_POINT ( 'NONE',  ( 22.50000000000000000, 64.35042919246788529, -203.6231074845244393 ) ) ;
#123062 = EDGE_CURVE ( 'NONE', #102833, #210821, #243106, .T. ) ;
#123063 = DIRECTION ( 'NONE',  ( 0.000000000000000000, -6.308085367188393199E-16, -1.000000000000000000 ) ) ;
#123064 = ORIENTED_EDGE ( 'NONE', *, *, #207278, .F. ) ;
#123065 = ORIENTED_EDGE ( 'NONE', *, *, #124392, .T. ) ;
#123066 =( NAMED_UNIT ( * ) PLANE_ANGLE_UNIT ( ) SI_UNIT ( $, .RADIAN. ) );
#123067 = EDGE_LOOP ( 'NONE', ( #214773, #27749, #129325, #123023 ) ) ;
#123068 = LINE ( 'NONE', #66934, #150193 ) ;
#123069 = AXIS2_PLACEMENT_3D ( 'NONE', #197968, #41493, #40218 ) ;
#123070 = EDGE_LOOP ( 'NONE', ( #142337, #196325, #102256, #226280 ) ) ;
#123071 = CIRCLE ( 'NONE', #173192, 0.1000000000000054040 ) ;
#123072 = ADVANCED_FACE ( 'NONE', ( #188321 ), #73543, .T. ) ;
#123073 = CARTESIAN_POINT ( 'NONE',  ( -21.44999999999999929, 7.350000000011155166, -188.7499999999999716 ) ) ;
#123074 = DIRECTION ( 'NONE',  ( -1.000000000000000000, -0.000000000000000000, 0.000000000000000000 ) ) ;
#123075 = PLANE ( 'NONE',  #217710 ) ;
#123076 = CIRCLE ( 'NONE', #6726, 0.09999999999999939493 ) ;
#123077 = CARTESIAN_POINT ( 'NONE',  ( -16.85939681242906474, 29.91185388629861563, -234.7000971468440298 ) ) ;
#123078 = FACE_OUTER_BOUND ( 'NONE', #51931, .T. ) ;
#123079 = CARTESIAN_POINT ( 'NONE',  ( 5.899999999999996803, -11.34999999999999964, 14.00000000000000178 ) ) ;
#123080 = DIRECTION ( 'NONE',  ( 1.020425574104004196E-15, 1.210927747993693964E-31, -1.000000000000000000 ) ) ;
#123083 = ORIENTED_EDGE ( 'NONE', *, *, #158026, .F. ) ;
#123082 = CARTESIAN_POINT ( 'NONE',  ( -18.50000000000000000, 59.16775194334852728, -221.0793150863668473 ) ) ;
#123081 = VECTOR ( 'NONE', #151414, 1000.000000000000000 ) ;
#123085 = DIRECTION ( 'NONE',  ( -0.000000000000000000, -0.000000000000000000, -1.000000000000000000 ) ) ;
#123084 = CARTESIAN_POINT ( 'NONE',  ( 20.95035502843362707, 65.52236167323513882, -61.94680777578801667 ) ) ;
#123086 = DIRECTION ( 'NONE',  ( 1.000000000000000000, 0.000000000000000000, 0.000000000000000000 ) ) ;
#123087 = ORIENTED_EDGE ( 'NONE', *, *, #250244, .T. ) ;
#123088 = VECTOR ( 'NONE', #53594, 1000.000000000000000 ) ;
#123089 = CARTESIAN_POINT ( 'NONE',  ( -20.54999999999999716, 74.00000000001205080, -123.2984855617622060 ) ) ;
#123090 = DIRECTION ( 'NONE',  ( 0.000000000000000000, 0.000000000000000000, 1.000000000000000000 ) ) ;
#123091 = VECTOR ( 'NONE', #116163, 1000.000000000000000 ) ;
#123093 = VERTEX_POINT ( 'NONE', #12278 ) ;
#123092 = CIRCLE ( 'NONE', #118997, 0.09999999999998898659 ) ;
#123095 = DIRECTION ( 'NONE',  ( 2.879366945564059217E-14, -0.9875055080513751582, 0.1575844902526747915 ) ) ;
#123094 = CARTESIAN_POINT ( 'NONE',  ( -33.72168855820452649, 52.34166666667851331, -86.27310748452447342 ) ) ;
#123096 = CARTESIAN_POINT ( 'NONE',  ( -21.53551880898957904, 75.90103026544032616, -109.8079052459406597 ) ) ;
#123097 = ADVANCED_FACE ( 'NONE', ( #130915 ), #22382, .T. ) ;
#123098 = ORIENTED_EDGE ( 'NONE', *, *, #177768, .F. ) ;
#123099 = AXIS2_PLACEMENT_3D ( 'NONE', #38288, #232651, #197342 ) ;
#123100 = FACE_OUTER_BOUND ( 'NONE', #95271, .T. ) ;
#123101 = TOROIDAL_SURFACE ( 'NONE', #60532, 2.699999999999999734, 0.1000000000000000056 ) ;
#123102 = CARTESIAN_POINT ( 'NONE',  ( -20.85000000000000142, -0.3238857010703366512, -33.45758958931398297 ) ) ;
#123103 = CARTESIAN_POINT ( 'NONE',  ( -18.39999999999999858, 46.93047535494665823, -255.3593673659106855 ) ) ;
#123104 = ORIENTED_EDGE ( 'NONE', *, *, #134239, .T. ) ;
#123105 = CIRCLE ( 'NONE', #156459, 0.09999999999999609201 ) ;
#123106 = AXIS2_PLACEMENT_3D ( 'NONE', #240593, #163636, #84034 ) ;
#123107 = EDGE_CURVE ( 'NONE', #41808, #30729, #33146, .T. ) ;
#123108 = ADVANCED_FACE ( 'NONE', ( #9679 ), #133484, .T. ) ;
#123109 = CARTESIAN_POINT ( 'NONE',  ( 21.09546886439534674, 67.12144688699692097, -90.78601363396897739 ) ) ;
#123110 = DIRECTION ( 'NONE',  ( 0.000000000000000000, 0.9126074666063660468, 0.4088369013363524762 ) ) ;
#123111 = PLANE ( 'NONE',  #45335 ) ;
#123112 = FACE_OUTER_BOUND ( 'NONE', #9774, .T. ) ;
#123113 = CARTESIAN_POINT ( 'NONE',  ( 23.25000000000000355, -22.45632476061176774, -107.2938984477316353 ) ) ;
#123114 = DIRECTION ( 'NONE',  ( 0.000000000000000000, 0.9126074666063641594, 0.4088369013363568061 ) ) ;
#123115 = EDGE_CURVE ( 'NONE', #176041, #229965, #10972, .T. ) ;
#123116 = ORIENTED_EDGE ( 'NONE', *, *, #110298, .F. ) ;
#123117 = CARTESIAN_POINT ( 'NONE',  ( 20.04142135623730070, 11.75000000001115907, -121.8500000000000369 ) ) ;
#123118 = CYLINDRICAL_SURFACE ( 'NONE', #115646, 11.74999999999999645 ) ;
#123119 = CARTESIAN_POINT ( 'NONE',  ( 23.14999999999999858, 74.00000000001244871, -170.0231074845243882 ) ) ;
#123120 = LINE ( 'NONE', #162258, #34720 ) ;
#123121 = DIRECTION ( 'NONE',  ( 1.000000000000000000, 0.000000000000000000, 0.000000000000000000 ) ) ;
#123122 = EDGE_CURVE ( 'NONE', #243534, #87303, #94342, .T. ) ;
#123124 = ORIENTED_EDGE ( 'NONE', *, *, #169480, .T. ) ;
#123123 = CARTESIAN_POINT ( 'NONE',  ( 21.07964655665547582, 67.22511038503301961, -57.30119090156032513 ) ) ;
#123125 = CARTESIAN_POINT ( 'NONE',  ( -18.59999999999999787, 77.25000000001165290, -61.72262673010922640 ) ) ;
#123126 = EDGE_CURVE ( 'NONE', #15594, #108958, #168148, .T. ) ;
#123127 = DIRECTION ( 'NONE',  ( -0.000000000000000000, -0.9126074666063770380, -0.4088369013363282178 ) ) ;
#123128 = CARTESIAN_POINT ( 'NONE',  ( -23.15000000000000213, 76.00000000001126921, -203.5231074845248997 ) ) ;
#123129 = ORIENTED_EDGE ( 'NONE', *, *, #18212, .F. ) ;
#123130 = DIRECTION ( 'NONE',  ( -1.000000000000000000, 0.000000000000000000, 0.000000000000000000 ) ) ;
#123131 = FACE_OUTER_BOUND ( 'NONE', #77377, .T. ) ;
#123132 = CIRCLE ( 'NONE', #131490, 0.1000000000000124678 ) ;
#123133 = ADVANCED_FACE ( 'NONE', ( #168810 ), #41811, .T. ) ;
#123134 = AXIS2_PLACEMENT_3D ( 'NONE', #11302, #189938, #86952 ) ;
#123135 = DIRECTION ( 'NONE',  ( 1.000000000000000000, 0.000000000000000000, 0.000000000000000000 ) ) ;
#123136 = ORIENTED_EDGE ( 'NONE', *, *, #252746, .T. ) ;
#123137 = DIRECTION ( 'NONE',  ( 0.000000000000000000, 0.000000000000000000, -1.000000000000000000 ) ) ;
#123138 = EDGE_LOOP ( 'NONE', ( #146669, #160710, #232513, #4394 ) ) ;
#123139 = AXIS2_PLACEMENT_3D ( 'NONE', #221690, #101732, #165613 ) ;
#123140 = DIRECTION ( 'NONE',  ( -1.000000000000000000, -0.000000000000000000, 0.000000000000000000 ) ) ;
#123141 = CARTESIAN_POINT ( 'NONE',  ( -21.12230431290519306, 34.01407833148830662, -243.6600691369628180 ) ) ;
#123142 = ADVANCED_FACE ( 'NONE', ( #254667 ), #147249, .T. ) ;
#123143 = PRESENTATION_STYLE_ASSIGNMENT (( #186989 ) ) ;
#123144 = CARTESIAN_POINT ( 'NONE',  ( 23.14999999999999858, 35.97645343225767789, -235.9694016464868298 ) ) ;
#123145 = ORIENTED_EDGE ( 'NONE', *, *, #47322, .T. ) ;
#123146 = AXIS2_PLACEMENT_3D ( 'NONE', #121444, #125270, #44457 ) ;
#123147 = VECTOR ( 'NONE', #105051, 1000.000000000000000 ) ;
#123148 = CARTESIAN_POINT ( 'NONE',  ( 21.05000000000000071, 5.000000000011153745, -122.0947339810869465 ) ) ;
#123149 = CARTESIAN_POINT ( 'NONE',  ( -22.57320508075687115, 64.25000000001195133, -103.0231074845244024 ) ) ;
#123150 = LINE ( 'NONE', #143975, #70569 ) ;
#123151 = CARTESIAN_POINT ( 'NONE',  ( -21.14999999999999858, 76.10000000001222986, -148.1726782920690937 ) ) ;
#123152 = CARTESIAN_POINT ( 'NONE',  ( 18.54148534481894117, 10.32532329027886853, -206.5699343018359286 ) ) ;
#123153 = VERTEX_POINT ( 'NONE', #117770 ) ;
#123155 = ORIENTED_EDGE ( 'NONE', *, *, #185225, .F. ) ;
#123154 = LINE ( 'NONE', #121878, #169479 ) ;
#123156 = EDGE_LOOP ( 'NONE', ( #113235, #18635, #2042, #205754 ) ) ;
#123157 = FACE_OUTER_BOUND ( 'NONE', #19504, .T. ) ;
#123158 = EDGE_LOOP ( 'NONE', ( #102933, #256794, #74545, #193727 ) ) ;
#123159 = DIRECTION ( 'NONE',  ( -1.000000000000000000, -0.000000000000000000, 0.000000000000000000 ) ) ;
#123160 = CARTESIAN_POINT ( 'NONE',  ( -21.07954640115341505, 6.329287696035425625, -100.4339922928603102 ) ) ;
#123161 = FACE_OUTER_BOUND ( 'NONE', #169250, .T. ) ;
#123163 = ORIENTED_EDGE ( 'NONE', *, *, #103292, .T. ) ;
#123162 = AXIS2_PLACEMENT_3D ( 'NONE', #170798, #95051, #174650 ) ;
#123164 = CARTESIAN_POINT ( 'NONE',  ( -16.94878442675512531, 66.00827089702058004, -56.91132706016227871 ) ) ;
#123165 = DIRECTION ( 'NONE',  ( 1.000000000000000000, -0.000000000000000000, -0.000000000000000000 ) ) ;
#123166 = VERTEX_POINT ( 'NONE', #215577 ) ;
#123167 = CARTESIAN_POINT ( 'NONE',  ( 22.49533356619863156, 11.65000000631534149, -100.4348774196772638 ) ) ;
#123169 = ORIENTED_EDGE ( 'NONE', *, *, #196047, .T. ) ;
#123168 = CARTESIAN_POINT ( 'NONE',  ( 20.94999999999999929, 36.65892442174472876, -249.5511627012454596 ) ) ;
#123170 = LINE ( 'NONE', #188273, #144197 ) ;
#123171 = DIRECTION ( 'NONE',  ( -0.000000000000000000, 6.982962677686266711E-15, -1.000000000000000000 ) ) ;
#123172 = AXIS2_PLACEMENT_3D ( 'NONE', #150014, #93862, #155163 ) ;
#123173 = CIRCLE ( 'NONE', #227210, 0.9000000000000014655 ) ;
#123174 = AXIS2_PLACEMENT_3D ( 'NONE', #53904, #212977, #115163 ) ;
#123175 = VECTOR ( 'NONE', #113132, 1000.000000000000114 ) ;
#123176 = VERTEX_POINT ( 'NONE', #36984 ) ;
#123177 = CARTESIAN_POINT ( 'NONE',  ( -21.55000000000000071, 7.249999999999999112, -12.34999999999999964 ) ) ;
#123178 = CARTESIAN_POINT ( 'NONE',  ( 21.05193202509564898, 10.72393601970834354, -79.17253460332581483 ) ) ;
#123179 = CARTESIAN_POINT ( 'NONE',  ( 23.14999999999999858, 76.00000000001190870, -103.0231074845243029 ) ) ;
#123180 = VERTEX_POINT ( 'NONE', #76071 ) ;
#123181 = CARTESIAN_POINT ( 'NONE',  ( -20.54999999999999716, 4.350000000011156054, -179.8499999999999943 ) ) ;
#123182 = EDGE_CURVE ( 'NONE', #56184, #150108, #17393, .T. ) ;
#123183 = DIRECTION ( 'NONE',  ( 0.000000000000000000, -7.109473446599835262E-15, 1.000000000000000000 ) ) ;
#123184 = EDGE_CURVE ( 'NONE', #155798, #16790, #218134, .T. ) ;
#123185 = ORIENTED_EDGE ( 'NONE', *, *, #131449, .F. ) ;
#123186 = EDGE_CURVE ( 'NONE', #189932, #118769, #159480, .T. ) ;
#123187 = CIRCLE ( 'NONE', #202298, 0.6000000000000015321 ) ;
#123188 = ORIENTED_EDGE ( 'NONE', *, *, #120942, .F. ) ;
#123189 = AXIS2_PLACEMENT_3D ( 'NONE', #187308, #109021, #149470 ) ;
#123190 = ORIENTED_EDGE ( 'NONE', *, *, #235438, .F. ) ;
#123191 = CARTESIAN_POINT ( 'NONE',  ( -20.94999999999999929, 1.835341550235569663, -78.55515129256303908 ) ) ;
#123192 = EDGE_CURVE ( 'NONE', #210115, #183119, #201410, .T. ) ;
#123193 = CARTESIAN_POINT ( 'NONE',  ( -16.80070461187868247, 66.05000000001255955, -182.6700713136814045 ) ) ;
#123195 = ORIENTED_EDGE ( 'NONE', *, *, #9516, .T. ) ;
#123194 = CARTESIAN_POINT ( 'NONE',  ( -20.64999999999999858, 71.75000000001205080, -124.1731074845243228 ) ) ;
#123196 = CARTESIAN_POINT ( 'NONE',  ( 20.94560253601876809, 11.75000000001115907, -127.0100835125151093 ) ) ;
#123197 = CYLINDRICAL_SURFACE ( 'NONE', #228106, 0.09999999999999938105 ) ;
#123198 = CYLINDRICAL_SURFACE ( 'NONE', #233791, 0.09999999999999939493 ) ;
#123199 = DIRECTION ( 'NONE',  ( 0.000000000000000000, -0.2617529984165052337, -0.9651348961777151958 ) ) ;
#123200 = FACE_OUTER_BOUND ( 'NONE', #146488, .T. ) ;
#123201 = DIRECTION ( 'NONE',  ( 0.000000000000000000, 0.000000000000000000, -1.000000000000000000 ) ) ;
#123203 = VERTEX_POINT ( 'NONE', #219419 ) ;
#123202 = CARTESIAN_POINT ( 'NONE',  ( -16.92973740335360588, 66.00749618554401366, -182.6170484493211461 ) ) ;
#123205 = ORIENTED_EDGE ( 'NONE', *, *, #87278, .T. ) ;
#123204 = CARTESIAN_POINT ( 'NONE',  ( 23.14999999999999503, 64.35000000001195986, -109.9379132551783158 ) ) ;
#123206 = CARTESIAN_POINT ( 'NONE',  ( 22.59999999999999787, 0.04781839071596413748, -55.24997758095282308 ) ) ;
#123207 = ORIENTED_EDGE ( 'NONE', *, *, #139590, .F. ) ;
#123208 = DIRECTION ( 'NONE',  ( 1.000000000000000000, 0.000000000000000000, 0.000000000000000000 ) ) ;
#123209 = VECTOR ( 'NONE', #251903, 1000.000000000000114 ) ;
#123210 = CARTESIAN_POINT ( 'NONE',  ( -18.39999999999999858, 64.52683809665015247, -194.1971614177164724 ) ) ;
#123211 = LINE ( 'NONE', #198892, #202545 ) ;
#123212 = EDGE_CURVE ( 'NONE', #97122, #67614, #193058, .T. ) ;
#123213 = ADVANCED_FACE ( 'NONE', ( #40838 ), #61595, .F. ) ;
#123214 = DIRECTION ( 'NONE',  ( 0.000000000000000000, -0.9887567792719341719, -0.1495327102803664099 ) ) ;
#123215 = DIRECTION ( 'NONE',  ( 1.000000000000000000, 0.000000000000000000, 0.000000000000000000 ) ) ;
#123216 = ORIENTED_EDGE ( 'NONE', *, *, #67178, .F. ) ;
#123217 = B_SPLINE_CURVE_WITH_KNOTS ( 'NONE', 3,
 ( #236338, #57686, #232515, #135937 ),
 .UNSPECIFIED., .F., .F.,
 ( 4, 4 ),
 ( 0.000000000000000000, 7.713889350927600000E-05 ),
 .UNSPECIFIED. ) ;
#123218 = DIRECTION ( 'NONE',  ( 1.000000000000000000, 0.000000000000000000, 0.000000000000000000 ) ) ;
#123219 = ORIENTED_EDGE ( 'NONE', *, *, #156734, .F. ) ;
#123220 = CARTESIAN_POINT ( 'NONE',  ( -0.000000000000000000, -11.25000000000000000, 13.90000000000000213 ) ) ;
#123221 = EDGE_CURVE ( 'NONE', #5211, #19570, #101404, .T. ) ;
#123222 = VECTOR ( 'NONE', #141085, 1000.000000000000000 ) ;
#123223 = CIRCLE ( 'NONE', #248123, 0.09999999999999993616 ) ;
#123224 = VERTEX_POINT ( 'NONE', #244127 ) ;
#123225 = VECTOR ( 'NONE', #199113, 1000.000000000000000 ) ;
#123226 = AXIS2_PLACEMENT_3D ( 'NONE', #81873, #126154, #181029 ) ;
#123227 = CARTESIAN_POINT ( 'NONE',  ( 21.04999999999999716, 76.01454569058479649, -210.0201252709573794 ) ) ;
#123228 = CYLINDRICAL_SURFACE ( 'NONE', #143059, 0.09999999999999530098 ) ;
#123229 = MECHANICAL_DESIGN_GEOMETRIC_PRESENTATION_REPRESENTATION (  '', ( #89896 ), #14917 ) ;
#123230 = ORIENTED_EDGE ( 'NONE', *, *, #105279, .F. ) ;
#123231 = CARTESIAN_POINT ( 'NONE',  ( -16.94445028196807002, 66.00793639031451221, -149.1304376629428816 ) ) ;
#123232 = ORIENTED_EDGE ( 'NONE', *, *, #208856, .T. ) ;
#123233 = CARTESIAN_POINT ( 'NONE',  ( -12.47155713865592652, 9.375669526436931633, -49.36779000938595630 ) ) ;
#123234 = ORIENTED_EDGE ( 'NONE', *, *, #63235, .F. ) ;
#123235 = LINE ( 'NONE', #179378, #81390 ) ;
#123236 = EDGE_CURVE ( 'NONE', #147354, #169820, #80579, .T. ) ;
#123237 = DIRECTION ( 'NONE',  ( 0.7071067811865486830, 0.1504730267678053013, -0.6909108974501224631 ) ) ;
#123238 = VERTEX_POINT ( 'NONE', #121647 ) ;
#123240 = ORIENTED_EDGE ( 'NONE', *, *, #57217, .F. ) ;
#123239 = CARTESIAN_POINT ( 'NONE',  ( -23.15000000000000213, 11.75000000000000000, 11.75000000000000000 ) ) ;
#123241 = CARTESIAN_POINT ( 'NONE',  ( 21.13461538461538325, 67.11458296203812779, -191.2731074845244166 ) ) ;
#123242 = ORIENTED_EDGE ( 'NONE', *, *, #107989, .T. ) ;
#123243 = AXIS2_PLACEMENT_3D ( 'NONE', #205623, #227762, #230328 ) ;
#123244 = EDGE_CURVE ( 'NONE', #110820, #92834, #47201, .T. ) ;
#123245 = ORIENTED_EDGE ( 'NONE', *, *, #21696, .F. ) ;
#123246 = AXIS2_PLACEMENT_3D ( 'NONE', #56122, #130539, #172292 ) ;
#123247 = DIRECTION ( 'NONE',  ( 0.000000000000000000, -0.6728971962617388280, 0.7397360091702248619 ) ) ;
#123248 = CARTESIAN_POINT ( 'NONE',  ( -20.94999999999999929, 44.55458850188623643, -247.3966190010231969 ) ) ;
#123249 =( BOUNDED_SURFACE ( )  B_SPLINE_SURFACE ( 3, 2, ( 
 ( #197045, #237477, #240049 ),
 ( #198341, #61401, #185203 ),
 ( #66545, #224324, #125233 ),
 ( #26141, #206050, #105635 ) ),
 .UNSPECIFIED., .F., .F., .F. ) 
 B_SPLINE_SURFACE_WITH_KNOTS ( ( 4, 4 ),
 ( 3, 3 ),
 ( -1.341700188450811737E-18, 0.0003124336117481280473 ),
 ( 0.000000000000000000, 1.000000000000000000 ),
 .UNSPECIFIED. ) 
 GEOMETRIC_REPRESENTATION_ITEM ( )  RATIONAL_B_SPLINE_SURFACE ( (
 ( 1.000000000000000000, 0.7040654476016059427, 1.000000000000000000),
 ( 1.000000000000000000, 0.7039193538780386117, 1.000000000000000000),
 ( 1.000000000000000000, 0.7089171279146311289, 1.000000000000000000),
 ( 1.000000000000000000, 0.7071067811865457964, 1.000000000000000000) ) ) 
 REPRESENTATION_ITEM ( '' )  SURFACE ( )  );
#123250 = DIRECTION ( 'NONE',  ( 0.000000000000000000, 1.000000000000000000, 0.000000000000000000 ) ) ;
#123251 = CIRCLE ( 'NONE', #98267, 0.09999999999998898659 ) ;
#123252 = EDGE_CURVE ( 'NONE', #231172, #95681, #51348, .T. ) ;
#123253 = EDGE_CURVE ( 'NONE', #142144, #63069, #164009, .T. ) ;
#123254 = VECTOR ( 'NONE', #153837, 1000.000000000000000 ) ;
#123255 = DIRECTION ( 'NONE',  ( 0.000000000000000000, 0.000000000000000000, 1.000000000000000000 ) ) ;
#123256 = DIRECTION ( 'NONE',  ( 1.000000000000000000, 0.000000000000000000, -0.000000000000000000 ) ) ;
#123257 = ORIENTED_EDGE ( 'NONE', *, *, #102963, .T. ) ;
#123258 = DIRECTION ( 'NONE',  ( 0.000000000000000000, 0.000000000000000000, -1.000000000000000000 ) ) ;
#123259 = DIRECTION ( 'NONE',  ( 1.000000000000000000, 0.000000000000000000, 0.000000000000000000 ) ) ;
#123260 = CARTESIAN_POINT ( 'NONE',  ( -16.87036670365549895, 44.00112830765706917, -235.3159266546824995 ) ) ;
#123261 = LINE ( 'NONE', #184503, #221813 ) ;
#123262 = ORIENTED_EDGE ( 'NONE', *, *, #95303, .F. ) ;
#123263 = CARTESIAN_POINT ( 'NONE',  ( -21.05000000000000426, 76.01771943332086323, -109.4641921729955243 ) ) ;
#123264 = EDGE_LOOP ( 'NONE', ( #49550, #74, #233072, #100879 ) ) ;
#123265 = CARTESIAN_POINT ( 'NONE',  ( 15.15590539855246099, 9.410682294279107296, -115.9311434419482936 ) ) ;
#123266 = VERTEX_POINT ( 'NONE', #242852 ) ;
#123267 = ADVANCED_FACE ( 'NONE', ( #104593 ), #42111, .T. ) ;
#123268 = AXIS2_PLACEMENT_3D ( 'NONE', #156348, #158906, #221394 ) ;
#123269 = EDGE_CURVE ( 'NONE', #191683, #53873, #141193, .T. ) ;
#123271 =( BOUNDED_SURFACE ( )  B_SPLINE_SURFACE ( 3, 2, ( 
 ( #225827, #45939, #4227 ),
 ( #125481, #245439, #66791 ),
 ( #246700, #124209, #102034 ),
 ( #181614, #203733, #2945 ),
 ( #5504, #68072, #151489 ),
 ( #28992, #148908, #111050 ) ),
 .UNSPECIFIED., .F., .F., .F. ) 
 B_SPLINE_SURFACE_WITH_KNOTS ( ( 4, 2, 4 ),
 ( 3, 3 ),
 ( 4.712388980384689674, 5.497787143782137953, 6.283185307179586232 ),
 ( 0.000000000000000000, 1.000000000000000000 ),
 .UNSPECIFIED. ) 
 GEOMETRIC_REPRESENTATION_ITEM ( )  RATIONAL_B_SPLINE_SURFACE ( (
 ( 1.000000000000000000, 0.7071067811865706654, 1.000000000000000000),
 ( 1.000000000000000000, 0.7727932973487074975, 1.000000000000000000),
 ( 1.000000000000000000, 0.8282379607655521170, 1.000000000000000000),
 ( 1.000000000000000000, 0.9038128468033841401, 1.000000000000000000),
 ( 1.000000000000000000, 0.9240297172248549407, 1.000000000000000000),
 ( 1.000000000000000000, 0.9238795325112804102, 1.000000000000000000) ) ) 
 REPRESENTATION_ITEM ( '' )  SURFACE ( )  );
#123270 = AXIS2_PLACEMENT_3D ( 'NONE', #165806, #143639, #146203 ) ;
#123272 = DIRECTION ( 'NONE',  ( 0.000000000000000000, 1.224646799142015331E-16, 1.000000000000000000 ) ) ;
#123273 = CARTESIAN_POINT ( 'NONE',  ( 20.85000000000000142, 77.83585931145600512, -158.5186683157258187 ) ) ;
#123274 = ORIENTED_EDGE ( 'NONE', *, *, #78606, .T. ) ;
#123276 = ORIENTED_EDGE ( 'NONE', *, *, #24931, .T. ) ;
#123275 = CARTESIAN_POINT ( 'NONE',  ( -21.14999999999999858, 76.10085836911117951, -181.7726746080137445 ) ) ;
#123277 = LINE ( 'NONE', #67153, #88028 ) ;
#123278 = ORIENTED_EDGE ( 'NONE', *, *, #205397, .F. ) ;
#123279 = AXIS2_PLACEMENT_3D ( 'NONE', #58655, #221578, #182501 ) ;
#123280 = EDGE_CURVE ( 'NONE', #96167, #116233, #162054, .T. ) ;
#123281 = AXIS2_PLACEMENT_3D ( 'NONE', #112222, #134310, #161294 ) ;
#123282 = CARTESIAN_POINT ( 'NONE',  ( -22.49510344025093644, 0.06712767820541534758, -21.85002989488574343 ) ) ;
#123283 = CARTESIAN_POINT ( 'NONE',  ( -21.05000000000000071, -11.64999999998884306, -164.6000000000000227 ) ) ;
#123284 = VERTEX_POINT ( 'NONE', #6812 ) ;
#123285 = ORIENTED_EDGE ( 'NONE', *, *, #68482, .T. ) ;
#123286 = ADVANCED_FACE ( 'NONE', ( #122923 ), #164613, .T. ) ;
#123287 = FACE_BOUND ( 'NONE', #179687, .T. ) ;
#123288 = CARTESIAN_POINT ( 'NONE',  ( 21.05000000000000071, 76.08561306081669784, -209.9368672183346405 ) ) ;
#123289 = DIRECTION ( 'NONE',  ( -0.000000000000000000, -0.9770955615653316162, -0.2128009952263604232 ) ) ;
#123290 = ADVANCED_FACE ( 'NONE', ( #23838 ), #27704, .T. ) ;
#123291 = ADVANCED_FACE ( 'NONE', ( #182899 ), #43377, .F. ) ;
#123292 = ORIENTED_EDGE ( 'NONE', *, *, #8150, .T. ) ;
#123293 = EDGE_LOOP ( 'NONE', ( #109952, #29145, #83605, #1464 ) ) ;
#123294 =( BOUNDED_SURFACE ( )  B_SPLINE_SURFACE ( 3, 2, ( 
 ( #47225, #227158, #126781 ),
 ( #128072, #45959, #125497 ),
 ( #184176, #26417, #48524 ),
 ( #206326, #66813, #105905 ),
 ( #188050, #165935, #107212 ),
 ( #88921, #186773, #8127 ) ),
 .UNSPECIFIED., .F., .F., .F. ) 
 B_SPLINE_SURFACE_WITH_KNOTS ( ( 4, 2, 4 ),
 ( 3, 3 ),
 ( 1.570796326794895448, 2.356194490192343505, 3.141592653589791784 ),
 ( 0.000000000000000000, 1.000000000000000000 ),
 .UNSPECIFIED. ) 
 GEOMETRIC_REPRESENTATION_ITEM ( )  RATIONAL_B_SPLINE_SURFACE ( (
 ( 1.000000000000000000, 0.7071067811865352493, 1.000000000000000000),
 ( 1.000000000000000000, 0.6611148371780189992, 1.000000000000000000),
 ( 1.000000000000000000, 0.6092287576694327411, 1.000000000000000000),
 ( 1.000000000000000000, 0.5278258667059284592, 1.000000000000000000),
 ( 1.000000000000000000, 0.4993418825333061917, 1.000000000000000000),
 ( 1.000000000000000000, 0.4999999999999960587, 1.000000000000000000) ) ) 
 REPRESENTATION_ITEM ( '' )  SURFACE ( )  );
#123295 = DIRECTION ( 'NONE',  ( -0.000000000000000000, -6.982962677686266711E-15, 1.000000000000000000 ) ) ;
#123296 = EDGE_CURVE ( 'NONE', #185310, #171186, #8109, .T. ) ;
#123298 = VERTEX_POINT ( 'NONE', #186754 ) ;
#123297 = DIRECTION ( 'NONE',  ( 0.000000000000000000, 0.8814952561688476074, -0.4721928772777262417 ) ) ;
#123299 = ADVANCED_FACE ( 'NONE', ( #103326 ), #123271, .T. ) ;
#123300 = VECTOR ( 'NONE', #229394, 1000.000000000000000 ) ;
#123301 = CARTESIAN_POINT ( 'NONE',  ( -16.97683809663752186, 9.950000000011138823, -180.9023640181964652 ) ) ;
#123302 = CARTESIAN_POINT ( 'NONE',  ( 20.94999999999999574, 74.73821383144657204, -61.43660852097884373 ) ) ;
#123303 = EDGE_CURVE ( 'NONE', #81295, #113518, #10675, .T. ) ;
#123304 = AXIS2_PLACEMENT_3D ( 'NONE', #169148, #170448, #209521 ) ;
#123305 = PLANE ( 'NONE',  #15198 ) ;
#123307 = FACE_OUTER_BOUND ( 'NONE', #203360, .T. ) ;
#123306 = CARTESIAN_POINT ( 'NONE',  ( -21.14999999999994174, 64.35000000001120668, -51.02310748452479316 ) ) ;
#123309 = AXIS2_PLACEMENT_3D ( 'NONE', #225303, #187511, #71414 ) ;
#123308 = DIRECTION ( 'NONE',  ( 0.000000000000000000, -1.000000000000000000, 0.000000000000000000 ) ) ;
#123310 = CIRCLE ( 'NONE', #206516, 0.5000000000000004441 ) ;
#123312 = ADVANCED_FACE ( 'NONE', ( #91493 ), #133188, .T. ) ;
#123311 = CARTESIAN_POINT ( 'NONE',  ( 21.05000000000000071, 8.815452279208699338, -108.9203925526142882 ) ) ;
#123313 = DIRECTION ( 'NONE',  ( 0.000000000000000000, -1.000000000000000000, 0.000000000000000000 ) ) ;
#123314 = DIRECTION ( 'NONE',  ( 0.000000000000000000, 0.000000000000000000, 1.000000000000000000 ) ) ;
#123316 = ORIENTED_EDGE ( 'NONE', *, *, #176352, .T. ) ;
#123315 = AXIS2_PLACEMENT_3D ( 'NONE', #4893, #44053, #239690 ) ;
#123317 = ORIENTED_EDGE ( 'NONE', *, *, #19455, .T. ) ;
#123318 = CARTESIAN_POINT ( 'NONE',  ( -21.14999999999999858, -0.09999999998884338825, -127.4593430482987912 ) ) ;
#123319 = EDGE_LOOP ( 'NONE', ( #193215, #247719, #113164, #154487 ) ) ;
#123320 = EDGE_CURVE ( 'NONE', #120569, #48243, #72438, .T. ) ;
#123321 = AXIS2_PLACEMENT_3D ( 'NONE', #233984, #253542, #30689 ) ;
#123322 = EDGE_CURVE ( 'NONE', #241487, #20464, #239015, .T. ) ;
#123323 = CARTESIAN_POINT ( 'NONE',  ( 18.59999999999999076, 70.05000000001193428, -92.71740517948948934 ) ) ;
#123324 = ORIENTED_EDGE ( 'NONE', *, *, #227497, .F. ) ;
#123325 = AXIS2_PLACEMENT_3D ( 'NONE', #164501, #65382, #108372 ) ;
#123326 = CARTESIAN_POINT ( 'NONE',  ( 18.49999999999999645, 43.57568952063339651, -245.1784935019914826 ) ) ;
#123327 = VERTEX_POINT ( 'NONE', #128052 ) ;
#123328 = DIRECTION ( 'NONE',  ( 1.000000000000000000, -0.000000000000000000, -0.000000000000000000 ) ) ;
#123329 = ORIENTED_EDGE ( 'NONE', *, *, #97713, .T. ) ;
#123330 = ORIENTED_EDGE ( 'NONE', *, *, #139843, .T. ) ;
#123331 = CARTESIAN_POINT ( 'NONE',  ( 21.05000000000000071, 23.49882452903949570, -253.1653563615082305 ) ) ;
#123332 = DIRECTION ( 'NONE',  ( 0.000000000000000000, 0.000000000000000000, -1.000000000000000000 ) ) ;
#123334 = ORIENTED_EDGE ( 'NONE', *, *, #16060, .F. ) ;
#123333 = DIRECTION ( 'NONE',  ( 0.000000000000000000, -0.000000000000000000, 1.000000000000000000 ) ) ;
#123335 = CIRCLE ( 'NONE', #194094, 0.09999999999998898659 ) ;
#123336 = CARTESIAN_POINT ( 'NONE',  ( -1.739115166359751801E-14, 11.65000000001114699, -121.8500000000000369 ) ) ;
#123338 = VERTEX_POINT ( 'NONE', #51039 ) ;
#123337 = CARTESIAN_POINT ( 'NONE',  ( 20.95566103547454517, 10.61824765095822087, -141.6318401929806043 ) ) ;
#123339 = CARTESIAN_POINT ( 'NONE',  ( 19.75857864376269291, 11.75000000001116263, -125.3500000000000512 ) ) ;
#123340 = VERTEX_POINT ( 'NONE', #11977 ) ;
#123341 = LINE ( 'NONE', #204137, #241525 ) ;
#123343 = VERTEX_POINT ( 'NONE', #188031 ) ;
#123342 = DIRECTION ( 'NONE',  ( 0.000000000000000000, -0.9998779222360104635, -0.01562499999996343723 ) ) ;
#123344 = LINE ( 'NONE', #211552, #151379 ) ;
#123345 = CARTESIAN_POINT ( 'NONE',  ( -12.48127053791145258, 27.09445758862755227, -233.7906081272070082 ) ) ;
#123346 = CARTESIAN_POINT ( 'NONE',  ( 21.04999999999999716, 10.68430915749624077, -74.52669679032690908 ) ) ;
#123347 = ORIENTED_EDGE ( 'NONE', *, *, #53433, .T. ) ;
#123348 = EDGE_CURVE ( 'NONE', #138064, #59138, #131900, .T. ) ;
#123350 = DIRECTION ( 'NONE',  ( 0.000000000000000000, -0.7280513885558860254, 0.6855225566105367374 ) ) ;
#123349 = DIRECTION ( 'NONE',  ( 1.224646799147353207E-16, -1.000000000000000000, -6.982962677686266711E-15 ) ) ;
#123351 = DIRECTION ( 'NONE',  ( 0.000000000000000000, 1.000000000000000000, 0.000000000000000000 ) ) ;
#123352 = CARTESIAN_POINT ( 'NONE',  ( 18.54999999999999716, 8.750000000000024869, -12.65000000000000213 ) ) ;
#123353 = AXIS2_PLACEMENT_3D ( 'NONE', #201623, #25570, #243307 ) ;
#123354 = CONICAL_SURFACE ( 'NONE', #189987, 4.049999999999998046, 0.7853981633974604915 ) ;
#123355 = EDGE_CURVE ( 'NONE', #117652, #134581, #178127, .T. ) ;
#123356 = CARTESIAN_POINT ( 'NONE',  ( 22.57320508075688537, 12.62988036037870643, -223.4632815780722410 ) ) ;
#123357 = CIRCLE ( 'NONE', #31809, 0.09999999999999971412 ) ;
#123358 = DIRECTION ( 'NONE',  ( 0.000000000000000000, 0.000000000000000000, 1.000000000000000000 ) ) ;
#123359 = ORIENTED_EDGE ( 'NONE', *, *, #112310, .T. ) ;
#123360 = VERTEX_POINT ( 'NONE', #9371 ) ;
#123361 = ORIENTED_EDGE ( 'NONE', *, *, #11399, .F. ) ;
#123362 = CARTESIAN_POINT ( 'NONE',  ( -20.64999999999999858, 65.49732036650624423, -236.6319166190174883 ) ) ;
#123363 = ORIENTED_EDGE ( 'NONE', *, *, #146667, .F. ) ;
#123364 = CARTESIAN_POINT ( 'NONE',  ( -18.50000000000000000, 9.150000000011157653, -112.8500000000000369 ) ) ;
#123365 = ORIENTED_EDGE ( 'NONE', *, *, #248484, .T. ) ;
#123366 = DIRECTION ( 'NONE',  ( -0.7071067811865127117, -0.7071067811865821007, 0.000000000000000000 ) ) ;
#123367 = ORIENTED_EDGE ( 'NONE', *, *, #155904, .T. ) ;
#123368 = AXIS2_PLACEMENT_3D ( 'NONE', #6639, #4072, #125319 ) ;
#123369 = DIRECTION ( 'NONE',  ( -0.1538461538461510236, 0.9880948137434718559, 0.000000000000000000 ) ) ;
#123370 = EDGE_CURVE ( 'NONE', #193883, #141135, #55815, .T. ) ;
#123371 = AXIS2_PLACEMENT_3D ( 'NONE', #147432, #27528, #88714 ) ;
#123372 = ORIENTED_EDGE ( 'NONE', *, *, #167462, .F. ) ;
#123373 = EDGE_LOOP ( 'NONE', ( #182653, #95081, #84768, #60045 ) ) ;
#123374 = ORIENTED_EDGE ( 'NONE', *, *, #53564, .T. ) ;
#123375 = DIRECTION ( 'NONE',  ( 1.000000000000000000, 0.000000000000000000, 0.000000000000000000 ) ) ;
#123376 = DIRECTION ( 'NONE',  ( -1.000000000000000000, -0.000000000000000000, -0.000000000000000000 ) ) ;
#123377 = TOROIDAL_SURFACE ( 'NONE', #231536, 3.899999999999999467, 0.1000000000000000056 ) ;
#123378 = DIRECTION ( 'NONE',  ( 0.000000000000000000, 0.000000000000000000, -1.000000000000000000 ) ) ;
#123379 = CARTESIAN_POINT ( 'NONE',  ( 15.74999999999999645, 26.41090933635396354, -233.4546044608430577 ) ) ;
#123380 = CARTESIAN_POINT ( 'NONE',  ( 20.94999999999999574, 44.09392520544991356, -258.8097135244738638 ) ) ;
#123381 = CARTESIAN_POINT ( 'NONE',  ( 12.25000000000000000, 66.65000000001204228, -119.7731074845243739 ) ) ;
#123383 = CARTESIAN_POINT ( 'NONE',  ( -18.69999999999999929, -11.65000000000000036, -15.00000000000000000 ) ) ;
#123382 = LINE ( 'NONE', #240767, #53974 ) ;
#123384 = CARTESIAN_POINT ( 'NONE',  ( -20.94999999999999929, 7.021664781900089913, -37.33356540189728889 ) ) ;
#123386 = ORIENTED_EDGE ( 'NONE', *, *, #201092, .F. ) ;
#123385 = DIRECTION ( 'NONE',  ( 0.000000000000000000, 0.000000000000000000, -1.000000000000000000 ) ) ;
#123388 = CARTESIAN_POINT ( 'NONE',  ( 21.11927991906888025, 69.55150688152053817, -103.0321911639982488 ) ) ;
#123387 = CARTESIAN_POINT ( 'NONE',  ( -21.05000000000000071, 1.115600667400684642E-11, -134.0000000000000000 ) ) ;
#123389 = LINE ( 'NONE', #24306, #3140 ) ;
#123390 = ORIENTED_EDGE ( 'NONE', *, *, #27988, .F. ) ;
#123391 = CARTESIAN_POINT ( 'NONE',  ( -18.59999999999999787, 72.02722222756958104, -225.1832529173024398 ) ) ;
#123392 = LINE ( 'NONE', #105058, #31321 ) ;
#123393 = CARTESIAN_POINT ( 'NONE',  ( -23.25000000000000355, 66.05000000001190585, -93.77310748452438816 ) ) ;
#123394 = ORIENTED_EDGE ( 'NONE', *, *, #242385, .T. ) ;
#123395 = CIRCLE ( 'NONE', #10968, 12.87499999999999822 ) ;
#123396 = CARTESIAN_POINT ( 'NONE',  ( 21.08078803292166015, 69.66698703557557337, -203.6022934716821737 ) ) ;
#123397 = LINE ( 'NONE', #183376, #213476 ) ;
#123398 = VERTEX_POINT ( 'NONE', #229718 ) ;
#123399 = ORIENTED_EDGE ( 'NONE', *, *, #208768, .F. ) ;
#123400 = CARTESIAN_POINT ( 'NONE',  ( -23.15000000000000213, 42.98415524044398950, -233.9519173640447889 ) ) ;
#123401 = ORIENTED_EDGE ( 'NONE', *, *, #108378, .F. ) ;
#123402 = CYLINDRICAL_SURFACE ( 'NONE', #100836, 2.000000000000001776 ) ;
#123403 = CARTESIAN_POINT ( 'NONE',  ( -18.50000000000000000, -9.421290279513540256, -174.3238821790264410 ) ) ;
#123404 = FACE_OUTER_BOUND ( 'NONE', #141219, .T. ) ;
#123405 = DIRECTION ( 'NONE',  ( -1.000000000000000000, 0.000000000000000000, 0.000000000000000000 ) ) ;
#123406 = ORIENTED_EDGE ( 'NONE', *, *, #53537, .T. ) ;
#123407 = EDGE_CURVE ( 'NONE', #210905, #20887, #184836, .T. ) ;
#123408 = LINE ( 'NONE', #141675, #25501 ) ;
#123409 = CARTESIAN_POINT ( 'NONE',  ( -21.05000000000000071, -11.64999999998884306, -97.50000000000004263 ) ) ;
#123410 = ADVANCED_FACE ( 'NONE', ( #112351 ), #150195, .F. ) ;
#123411 = VECTOR ( 'NONE', #80771, 1000.000000000000000 ) ;
#123412 = CARTESIAN_POINT ( 'NONE',  ( 18.52928932304149967, 10.27928932305266407, -192.1762534328030938 ) ) ;
#123413 = DIRECTION ( 'NONE',  ( 0.000000000000000000, 1.000000000000000000, 6.982962677686266711E-15 ) ) ;
#123414 = VECTOR ( 'NONE', #210664, 1000.000000000000227 ) ;
#123415 = AXIS2_PLACEMENT_3D ( 'NONE', #234244, #77729, #176876 ) ;
#123416 = VERTEX_POINT ( 'NONE', #32843 ) ;
#123417 = EDGE_CURVE ( 'NONE', #200908, #252901, #35048, .T. ) ;
#123419 = EDGE_LOOP ( 'NONE', ( #20723, #158044, #65633, #31344 ) ) ;
#123418 = CARTESIAN_POINT ( 'NONE',  ( 20.94999999999999574, 1.162701749949165642, -41.60000000000000142 ) ) ;
#123420 = CARTESIAN_POINT ( 'NONE',  ( 18.52928932188133970, 10.27928932189250411, -121.8500000000000369 ) ) ;
#123421 = CARTESIAN_POINT ( 'NONE',  ( 18.46082813848008897, 78.23583199935188759, -231.4993683512706752 ) ) ;
#123422 = CYLINDRICAL_SURFACE ( 'NONE', #13053, 0.1000000000000000472 ) ;
#123423 = ADVANCED_FACE ( 'NONE', ( #53649 ), #130611, .T. ) ;
#123424 = DIRECTION ( 'NONE',  ( 0.000000000000000000, -0.4088369013363281068, 0.9126074666063770380 ) ) ;
#123425 = DIRECTION ( 'NONE',  ( 0.000000000000000000, -0.3427706569149662763, 0.9394191166662954062 ) ) ;
#123426 = CARTESIAN_POINT ( 'NONE',  ( 21.05000000000000071, 64.35000000001186038, -90.87310748452438247 ) ) ;
#123427 = ORIENTED_EDGE ( 'NONE', *, *, #152153, .F. ) ;
#123428 = DIRECTION ( 'NONE',  ( 1.000000000000000000, 0.000000000000000000, 0.000000000000000000 ) ) ;
#123429 = PLANE ( 'NONE',  #198235 ) ;
#123430 = CYLINDRICAL_SURFACE ( 'NONE', #235625, 0.1000000000000124678 ) ;
#123431 = CARTESIAN_POINT ( 'NONE',  ( 23.14999999999999503, 61.57587952878035509, -212.2000740415318774 ) ) ;
#123432 = ADVANCED_FACE ( 'NONE', ( #189314 ), #247985, .T. ) ;
#123433 = CARTESIAN_POINT ( 'NONE',  ( 21.14999999999999503, 76.10000000001203091, -114.6726782920691079 ) ) ;
#123434 = AXIS2_PLACEMENT_3D ( 'NONE', #75015, #235331, #256120 ) ;
#123435 = DIRECTION ( 'NONE',  ( 0.000000000000000000, -0.9908441862701791170, 0.1350103645450472789 ) ) ;
#123436 = CIRCLE ( 'NONE', #77605, 0.9000000000000014655 ) ;
#123437 = EDGE_LOOP ( 'NONE', ( #109543, #226428, #180123, #113525 ) ) ;
#123438 = ORIENTED_EDGE ( 'NONE', *, *, #42364, .F. ) ;
#123439 = CARTESIAN_POINT ( 'NONE',  ( 21.15000000000005187, 76.00000000001119815, -40.17310748452479174 ) ) ;
#123440 = CARTESIAN_POINT ( 'NONE',  ( 21.05000000000000071, 7.128833340094563376, -233.7327013124401276 ) ) ;
#123441 = FACE_OUTER_BOUND ( 'NONE', #41183, .T. ) ;
#123442 = CARTESIAN_POINT ( 'NONE',  ( -21.29999999999995808, 1.115600667400684642E-11, -134.0000000000000000 ) ) ;
#123443 = VECTOR ( 'NONE', #113550, 1000.000000000000000 ) ;
#123444 = EDGE_CURVE ( 'NONE', #126771, #253449, #249294, .T. ) ;
#123445 = ORIENTED_EDGE ( 'NONE', *, *, #96959, .F. ) ;
#123446 = CARTESIAN_POINT ( 'NONE',  ( 20.94999999999999574, 13.60254931771583387, -238.7443143987590304 ) ) ;
#123447 = CIRCLE ( 'NONE', #219295, 0.1000000000000028644 ) ;
#123448 = AXIS2_PLACEMENT_3D ( 'NONE', #79998, #177866, #239110 ) ;
#123449 = CARTESIAN_POINT ( 'NONE',  ( 21.14999999999999858, -0.09999999998884338825, -60.45934304829879835 ) ) ;
#123450 = CARTESIAN_POINT ( 'NONE',  ( 21.05000000000000071, 65.17014820068582992, -222.4427298839669618 ) ) ;
#123451 = CARTESIAN_POINT ( 'NONE',  ( 0.9000000000000547562, 67.75000000001118394, -10.02310748452479139 ) ) ;
#123452 = AXIS2_PLACEMENT_3D ( 'NONE', #158597, #120758, #239398 ) ;
#123453 = PRESENTATION_LAYER_ASSIGNMENT (  '', '', ( #11027 ) ) ;
#123454 = ORIENTED_EDGE ( 'NONE', *, *, #150075, .T. ) ;
#123455 = DIRECTION ( 'NONE',  ( 1.000000000000000000, 0.000000000000000000, 0.000000000000000000 ) ) ;
#123456 = ORIENTED_EDGE ( 'NONE', *, *, #56872, .F. ) ;
#123457 = CARTESIAN_POINT ( 'NONE',  ( -22.39999999999999858, 0.000000000000000000, 0.1000000000000028644 ) ) ;
#123458 = LINE ( 'NONE', #24377, #4006 ) ;
#123459 = DIRECTION ( 'NONE',  ( 1.000000000000000000, 0.000000000000000000, 0.000000000000000000 ) ) ;
#123460 = AXIS2_PLACEMENT_3D ( 'NONE', #229106, #175567, #50437 ) ;
#123461 = CARTESIAN_POINT ( 'NONE',  ( -21.05000000000000071, 1.749999999999999778, -11.66951155790164307 ) ) ;
#123462 = DIRECTION ( 'NONE',  ( 0.000000000000000000, 0.8814952561688444987, -0.4721928772777320149 ) ) ;
#123463 = CYLINDRICAL_SURFACE ( 'NONE', #110424, 0.09999999999999939493 ) ;
#123464 = DIRECTION ( 'NONE',  ( -1.000000000000000000, 0.000000000000000000, 0.000000000000000000 ) ) ;
#123465 = CARTESIAN_POINT ( 'NONE',  ( -18.43707690579160641, -9.682403433465239573, -107.1568433774128266 ) ) ;
#123466 = CARTESIAN_POINT ( 'NONE',  ( -21.00023020733438273, 6.390869245278866018, -67.00000000000004263 ) ) ;
#123467 = CARTESIAN_POINT ( 'NONE',  ( 18.59999999999999076, 64.35000000001147669, -44.77310748452440237 ) ) ;
#123468 = DIRECTION ( 'NONE',  ( 0.000000000000000000, 0.000000000000000000, 1.000000000000000000 ) ) ;
#123469 = VECTOR ( 'NONE', #218520, 1000.000000000000000 ) ;
#123470 = CARTESIAN_POINT ( 'NONE',  ( 18.47688499308725341, -9.464855950284134067, -40.20134775313739794 ) ) ;
#123471 = CARTESIAN_POINT ( 'NONE',  ( 21.05000000000000071, 84.66355140188112216, -112.5472086025915388 ) ) ;
#123472 = CARTESIAN_POINT ( 'NONE',  ( 21.05000000000085336, 8.894723818387976877, -175.9870843231449555 ) ) ;
#123473 = EDGE_CURVE ( 'NONE', #40222, #97414, #85036, .T. ) ;
#123474 = ORIENTED_EDGE ( 'NONE', *, *, #235472, .T. ) ;
#123475 = DIRECTION ( 'NONE',  ( 0.000000000000000000, -0.9126074666063770380, -0.4088369013363281068 ) ) ;
#123476 = DIRECTION ( 'NONE',  ( 1.000000000000000000, 0.000000000000000000, 0.000000000000000000 ) ) ;
#123477 = EDGE_CURVE ( 'NONE', #180362, #33688, #56193, .T. ) ;
#123478 = ORIENTED_EDGE ( 'NONE', *, *, #145722, .T. ) ;
#123479 = CARTESIAN_POINT ( 'NONE',  ( 20.95512820512820440, 30.87711321140620413, -234.4019277376435184 ) ) ;
#123480 = DIRECTION ( 'NONE',  ( -6.938893903907222067E-15, 1.000000000000000000, 0.000000000000000000 ) ) ;
#123481 = CIRCLE ( 'NONE', #252648, 0.1000000000000090955 ) ;
#123482 = DIRECTION ( 'NONE',  ( 1.000000000000000000, 0.000000000000000000, 0.000000000000000000 ) ) ;
#123483 = EDGE_CURVE ( 'NONE', #64423, #55402, #134925, .T. ) ;
#123484 = EDGE_LOOP ( 'NONE', ( #44098, #23971, #137553, #206421 ) ) ;
#123487 = ADVANCED_FACE ( 'NONE', ( #157933 ), #20971, .F. ) ;
#123486 = CIRCLE ( 'NONE', #210983, 0.09999999999999939493 ) ;
#123485 = DIRECTION ( 'NONE',  ( 1.000000000000000000, 0.000000000000000000, 0.000000000000000000 ) ) ;
#123488 = DIRECTION ( 'NONE',  ( 1.000000000000000000, 0.000000000000000000, 0.000000000000000000 ) ) ;
#123489 = CIRCLE ( 'NONE', #48468, 0.1000000000000028644 ) ;
#123490 = ORIENTED_EDGE ( 'NONE', *, *, #206678, .F. ) ;
#123491 = CIRCLE ( 'NONE', #102605, 4.000000000000003553 ) ;
#123492 = ORIENTED_EDGE ( 'NONE', *, *, #247931, .T. ) ;
#123493 = DIRECTION ( 'NONE',  ( 0.000000000000000000, 0.000000000000000000, 1.000000000000000000 ) ) ;
#123494 = ORIENTED_EDGE ( 'NONE', *, *, #35571, .F. ) ;
#123495 = EDGE_CURVE ( 'NONE', #224755, #198610, #159927, .T. ) ;
#123497 = AXIS2_PLACEMENT_3D ( 'NONE', #70797, #111182, #129458 ) ;
#123496 = FACE_OUTER_BOUND ( 'NONE', #216116, .T. ) ;
#123498 = DIRECTION ( 'NONE',  ( -1.000000000000000000, -0.000000000000000000, -0.000000000000000000 ) ) ;
#123500 = DIRECTION ( 'NONE',  ( 0.000000000000000000, 0.2128009952263602844, -0.9770955615653315052 ) ) ;
#123499 = PRODUCT_DEFINITION_CONTEXT ( 'detailed design', #125842, 'design' ) ;
#123501 = ADVANCED_FACE ( 'NONE', ( #15838 ), #18372, .T. ) ;
#123502 = LINE ( 'NONE', #220033, #75403 ) ;
#123503 = AXIS2_PLACEMENT_3D ( 'NONE', #236626, #43582, #180529 ) ;
#123504 = CARTESIAN_POINT ( 'NONE',  ( -17.11825945287481332, 10.05000000001113847, -87.85000000000003695 ) ) ;
#123505 = CIRCLE ( 'NONE', #11075, 4.300000000000025580 ) ;
#123506 = CYLINDRICAL_SURFACE ( 'NONE', #226104, 0.8750000000000007772 ) ;
#123507 = DIRECTION ( 'NONE',  ( -3.265361837132813093E-16, -0.9651348961777146407, 0.2617529984165072321 ) ) ;
#123509 = EDGE_LOOP ( 'NONE', ( #153939, #199366, #236135, #243633 ) ) ;
#123508 = CARTESIAN_POINT ( 'NONE',  ( 18.43630871534871574, 87.08575402747911198, -199.6284159481674010 ) ) ;
#123510 = ORIENTED_EDGE ( 'NONE', *, *, #75459, .T. ) ;
#123512 = CARTESIAN_POINT ( 'NONE',  ( 22.39999999999999858, 0.1000000000111554016, -126.2092204016266379 ) ) ;
#123511 = DIRECTION ( 'NONE',  ( -1.000000000000000000, 0.000000000000000000, 0.000000000000000000 ) ) ;
#123514 = EDGE_LOOP ( 'NONE', ( #20403, #65210, #213511, #206127 ) ) ;
#123513 = CARTESIAN_POINT ( 'NONE',  ( -16.88705144915410017, 61.01290475571573779, -220.7705454887500593 ) ) ;
#123515 = VERTEX_POINT ( 'NONE', #138294 ) ;
#123516 = CARTESIAN_POINT ( 'NONE',  ( -18.40000000000000213, 65.08943781962308606, -222.1672656287770451 ) ) ;
#123517 = CARTESIAN_POINT ( 'NONE',  ( 20.72390388899090752, 10.58996311843487348, -175.0113482957463020 ) ) ;
#123519 = ADVANCED_FACE ( 'NONE', ( #219122 ), #40548, .F. ) ;
#123518 = FACE_OUTER_BOUND ( 'NONE', #84871, .T. ) ;
#123521 = CARTESIAN_POINT ( 'NONE',  ( 20.95512820512820440, 8.876151316299271343, -109.0586289951409924 ) ) ;
#123520 = CIRCLE ( 'NONE', #11090, 0.5000000000000004441 ) ;
#123522 = ADVANCED_FACE ( 'NONE', ( #214012 ), #74543, .T. ) ;
#123523 = ADVANCED_FACE ( 'NONE', ( #234859 ), #238703, .T. ) ;
#123524 = CARTESIAN_POINT ( 'NONE',  ( 21.00000000000000000, 30.46448808713892831, -235.1722212069449256 ) ) ;
#123525 = CARTESIAN_POINT ( 'NONE',  ( 18.59999999999999076, 5.949999999999945111, -10.30570230503485973 ) ) ;
#123526 = EDGE_LOOP ( 'NONE', ( #82354, #42860, #204496 ) ) ;
#123527 = EDGE_LOOP ( 'NONE', ( #79441, #37933, #217193, #89390 ) ) ;
#123528 = DIRECTION ( 'NONE',  ( 0.000000000000000000, -1.000000000000000000, 0.000000000000000000 ) ) ;
#123529 = CIRCLE ( 'NONE', #77521, 11.75000000000000000 ) ;
#123530 = AXIS2_PLACEMENT_3D ( 'NONE', #8549, #9825, #151935 ) ;
#123531 = VERTEX_POINT ( 'NONE', #156641 ) ;
#123532 = CIRCLE ( 'NONE', #235959, 0.2000000000000057288 ) ;
#123534 = SPHERICAL_SURFACE ( 'NONE', #55148, 0.1000000000000000056 ) ;
#123533 = AXIS2_PLACEMENT_3D ( 'NONE', #96389, #139364, #217613 ) ;
#123535 = ORIENTED_EDGE ( 'NONE', *, *, #164466, .T. ) ;
#123536 = CARTESIAN_POINT ( 'NONE',  ( 21.05000000000000071, 4.999999999999997335, -21.09473398108690390 ) ) ;
#123537 = EDGE_CURVE ( 'NONE', #21929, #80413, #251478, .T. ) ;
#123538 = DIRECTION ( 'NONE',  ( 0.000000000000000000, 0.000000000000000000, -1.000000000000000000 ) ) ;
#123539 = CARTESIAN_POINT ( 'NONE',  ( 21.05000000000000071, 1.115600667400684642E-11, -100.5000000000000426 ) ) ;
#123540 = CARTESIAN_POINT ( 'NONE',  ( -21.11927991906891222, 75.99091632053885803, -209.9716006030158724 ) ) ;
#123541 = ORIENTED_EDGE ( 'NONE', *, *, #169557, .T. ) ;
#123542 = EDGE_LOOP ( 'NONE', ( #70100, #239036, #246192, #117818 ) ) ;
#123543 = CARTESIAN_POINT ( 'NONE',  ( 22.47809213839789066, 0.03753706763967752658, -122.3500266652122264 ) ) ;
#123544 = LINE ( 'NONE', #204349, #93714 ) ;
#123545 = EDGE_CURVE ( 'NONE', #239074, #8048, #18438, .T. ) ;
#123546 = DIRECTION ( 'NONE',  ( -1.073024830501117528E-15, 0.8814952561688430555, -0.4721928772777346239 ) ) ;
#123547 = AXIS2_PLACEMENT_3D ( 'NONE', #231493, #15016, #254831 ) ;
#123548 = DIRECTION ( 'NONE',  ( -0.000000000000000000, 1.000000000000000000, 7.525063763929033127E-15 ) ) ;
#123549 = ORIENTED_EDGE ( 'NONE', *, *, #180656, .F. ) ;
#123550 = VECTOR ( 'NONE', #65012, 1000.000000000000000 ) ;
#123552 = CARTESIAN_POINT ( 'NONE',  ( -14.00000000000000178, 66.15000000001185754, -86.27310748452437394 ) ) ;
#123551 = CIRCLE ( 'NONE', #111079, 0.09999999999999609201 ) ;
#123553 = ORIENTED_EDGE ( 'NONE', *, *, #30708, .F. ) ;
#123556 = EDGE_LOOP ( 'NONE', ( #102857, #159773, #114415, #249608, #73237, #64466, #8846, #20302, #54652, #115939, #218832, #171024 ) ) ;
#123555 = LINE ( 'NONE', #242205, #117991 ) ;
#123554 = DIRECTION ( 'NONE',  ( 0.000000000000000000, 0.000000000000000000, -1.000000000000000000 ) ) ;
#123557 = SPHERICAL_SURFACE ( 'NONE', #102061, 0.1000000000000000056 ) ;
#123558 = ORIENTED_EDGE ( 'NONE', *, *, #9721, .T. ) ;
#123559 = CARTESIAN_POINT ( 'NONE',  ( -1.739115166359751170E-14, 11.65000000001114699, -155.3500000000000227 ) ) ;
#123560 = VECTOR ( 'NONE', #45565, 1000.000000000000000 ) ;
#123561 = EDGE_LOOP ( 'NONE', ( #64030, #217213, #211394, #57723 ) ) ;
#123562 = DIRECTION ( 'NONE',  ( 0.000000000000000000, -2.775557561563196798E-13, -1.000000000000000000 ) ) ;
#123563 = EDGE_CURVE ( 'NONE', #107956, #256826, #139013, .T. ) ;
#123564 = DIRECTION ( 'NONE',  ( 1.000000000000000000, 0.000000000000000000, 0.000000000000000000 ) ) ;
#123565 = DIRECTION ( 'NONE',  ( -1.000000000000000000, 0.000000000000000000, 0.000000000000000000 ) ) ;
#123566 = CARTESIAN_POINT ( 'NONE',  ( -18.58671080940899856, -9.406932858815459042, -74.12415446490474835 ) ) ;
#123567 = EDGE_CURVE ( 'NONE', #160419, #70041, #177484, .T. ) ;
#123568 = FACE_OUTER_BOUND ( 'NONE', #72960, .T. ) ;
#123569 = ORIENTED_EDGE ( 'NONE', *, *, #242423, .F. ) ;
#123570 = EDGE_CURVE ( 'NONE', #184831, #54640, #174937, .T. ) ;
#123571 = CARTESIAN_POINT ( 'NONE',  ( 23.14999999999999858, 78.10000000001214460, -136.5231074845243029 ) ) ;
#123572 = CARTESIAN_POINT ( 'NONE',  ( 22.47071067811865319, 59.75442326890422606, -233.9300113800879046 ) ) ;
#123573 = CARTESIAN_POINT ( 'NONE',  ( -18.33682934331484304, -9.511185591082512047, -140.9056547686735428 ) ) ;
#123574 = AXIS2_PLACEMENT_3D ( 'NONE', #95094, #195507, #19416 ) ;
#123575 = ORIENTED_EDGE ( 'NONE', *, *, #134138, .F. ) ;
#123576 = FACE_OUTER_BOUND ( 'NONE', #245284, .T. ) ;
#123577 = ORIENTED_EDGE ( 'NONE', *, *, #123477, .T. ) ;
#123578 = DIRECTION ( 'NONE',  ( -0.000000000000000000, -0.000000000000000000, -1.000000000000000000 ) ) ;
#123579 = EDGE_CURVE ( 'NONE', #197139, #246280, #159195, .T. ) ;
#123580 = ADVANCED_FACE ( 'NONE', ( #57477 ), #197487, .T. ) ;
#123581 = DIRECTION ( 'NONE',  ( 0.000000000000000000, -0.9651348961777157509, 0.2617529984165027912 ) ) ;
#123583 = ORIENTED_EDGE ( 'NONE', *, *, #103284, .F. ) ;
#123582 = CARTESIAN_POINT ( 'NONE',  ( -16.87683809663749557, 44.82209472663102900, -234.9913374327310862 ) ) ;
#123584 = DIRECTION ( 'NONE',  ( 0.000000000000000000, -0.9908441862701605762, -0.1350103645451835310 ) ) ;
#123585 = AXIS2_PLACEMENT_3D ( 'NONE', #236291, #118935, #116366 ) ;
#123586 = CARTESIAN_POINT ( 'NONE',  ( -15.57281606413133979, 62.77476515014583924, -216.4875458411299860 ) ) ;
#123587 = DIRECTION ( 'NONE',  ( -1.000000000000000000, 0.000000000000000000, 0.000000000000000000 ) ) ;
#123588 = VERTEX_POINT ( 'NONE', #114907 ) ;
#123589 = AXIS2_PLACEMENT_3D ( 'NONE', #251081, #191150, #73772 ) ;
#123590 = CARTESIAN_POINT ( 'NONE',  ( 20.95512820512820440, 8.876151316288115822, -12.15000000000000036 ) ) ;
#123591 = DIRECTION ( 'NONE',  ( 0.000000000000000000, 0.000000000000000000, 1.000000000000000000 ) ) ;
#123592 = ORIENTED_EDGE ( 'NONE', *, *, #130836, .F. ) ;
#123593 = CARTESIAN_POINT ( 'NONE',  ( 20.94999999999999929, 5.500000000011153745, -88.09473398108696074 ) ) ;
#123594 = AXIS2_PLACEMENT_3D ( 'NONE', #128140, #188108, #47282 ) ;
#123595 = EDGE_CURVE ( 'NONE', #184931, #163009, #215286, .T. ) ;
#123596 = EDGE_CURVE ( 'NONE', #95409, #13934, #6501, .T. ) ;
#123597 = ORIENTED_EDGE ( 'NONE', *, *, #5488, .T. ) ;
#123598 = AXIS2_PLACEMENT_3D ( 'NONE', #167072, #165776, #67933 ) ;
#123599 = CARTESIAN_POINT ( 'NONE',  ( -15.55912972643741199, 67.50912972644930221, -90.47310748452437679 ) ) ;
#123601 = ORIENTED_EDGE ( 'NONE', *, *, #23186, .T. ) ;
#123600 = DIRECTION ( 'NONE',  ( -6.938893903907225222E-15, -0.4088369013363281068, 0.9126074666063770380 ) ) ;
#123602 = B_SPLINE_CURVE_WITH_KNOTS ( 'NONE', 3,
 ( #116540, #132242, #211792, #100772, #163373, #219468, #139927, #82510, #198631, #218172, #2989, #180366, #122965, #43418, #202493, #4272, #40880, #162101, #179113 ),
 .UNSPECIFIED., .F., .F.,
 ( 4, 3, 3, 3, 3, 3, 4 ),
 ( 0.000000000000000000, 2.646747978908353324E-05, 5.271166642128909460E-05, 9.008788829885495768E-05, 0.0001426648776561096547, 0.0001897378458659754511, 0.0001917382627806486133 ),
 .UNSPECIFIED. ) ;
#123603 = ADVANCED_FACE ( 'NONE', ( #3944 ), #5197, .F. ) ;
#123604 = AXIS2_PLACEMENT_3D ( 'NONE', #165412, #210952, #50562 ) ;
#123607 = EDGE_LOOP ( 'NONE', ( #202870, #17200, #180814, #160762 ) ) ;
#123606 = EDGE_LOOP ( 'NONE', ( #239695, #197026, #29558, #153609 ) ) ;
#123605 = CARTESIAN_POINT ( 'NONE',  ( 18.49999999999999289, 14.55853075413893194, -219.6797800383511401 ) ) ;
#123608 = CARTESIAN_POINT ( 'NONE',  ( -16.87036670365549895, 9.989418819312803066, -79.52043988269799968 ) ) ;
#123609 = DIRECTION ( 'NONE',  ( 0.000000000000000000, 1.000000000000000000, 1.387778780781444413E-14 ) ) ;
#123610 = ADVANCED_FACE ( 'NONE', ( #224266 ), #209997, .T. ) ;
#123611 = CARTESIAN_POINT ( 'NONE',  ( 13.99999999999999822, 66.15000000001204228, -119.7731074845243739 ) ) ;
#123613 = CARTESIAN_POINT ( 'NONE',  ( 23.14999999999999858, 4.775700934590584090, -112.3487681040460160 ) ) ;
#123612 = CARTESIAN_POINT ( 'NONE',  ( 22.40736611211992368, 1.115600667400684642E-11, -88.85042919245522341 ) ) ;
#123614 = LINE ( 'NONE', #181031, #36786 ) ;
#123615 = EDGE_CURVE ( 'NONE', #22343, #239112, #146013, .T. ) ;
#123616 = CIRCLE ( 'NONE', #156957, 0.1000000000000028644 ) ;
#123617 = CARTESIAN_POINT ( 'NONE',  ( -16.94333152886236959, 44.08063011399070774, -235.2792992266545298 ) ) ;
#123618 = DIRECTION ( 'NONE',  ( -0.000000000000000000, -0.000000000000000000, -1.000000000000000000 ) ) ;
#123619 = DIRECTION ( 'NONE',  ( -0.000000000000000000, 1.000000000000000000, 6.982962677686266711E-15 ) ) ;
#123620 = VECTOR ( 'NONE', #144393, 1000.000000000000000 ) ;
#123621 = EDGE_LOOP ( 'NONE', ( #220813, #79238, #36089, #199616 ) ) ;
#123622 = EDGE_LOOP ( 'NONE', ( #187800, #123832, #88291, #64813 ) ) ;
#123623 = EDGE_CURVE ( 'NONE', #78078, #180142, #68439, .T. ) ;
#123625 = CARTESIAN_POINT ( 'NONE',  ( -20.87155475150660777, 64.25000000001175238, -76.42752095536712886 ) ) ;
#123624 = CIRCLE ( 'NONE', #102739, 0.09999999999999939493 ) ;
#123627 = ORIENTED_EDGE ( 'NONE', *, *, #132689, .F. ) ;
#123626 = DIRECTION ( 'NONE',  ( 0.000000000000000000, 0.000000000000000000, -1.000000000000000000 ) ) ;
#123628 = CIRCLE ( 'NONE', #140158, 11.64999999999999325 ) ;
#123629 = VERTEX_POINT ( 'NONE', #239999 ) ;
#123630 = CARTESIAN_POINT ( 'NONE',  ( -21.93340585971863277, 7.324147022855313161, -1.264184810800004045E-15 ) ) ;
#123631 = EDGE_LOOP ( 'NONE', ( #68402, #254173, #197663, #187132 ) ) ;
#123632 = CARTESIAN_POINT ( 'NONE',  ( -21.05000000000000071, 38.48566838331611706, -234.6475946777057970 ) ) ;
#123633 = CIRCLE ( 'NONE', #86180, 0.09999999999999761857 ) ;
#123634 = AXIS2_PLACEMENT_3D ( 'NONE', #118875, #177588, #139680 ) ;
#123635 = EDGE_CURVE ( 'NONE', #19295, #3179, #89166, .T. ) ;
#123636 = VERTEX_POINT ( 'NONE', #225528 ) ;
#123637 = DIRECTION ( 'NONE',  ( -0.000000000000000000, -0.000000000000000000, 1.000000000000000000 ) ) ;
#123638 = LINE ( 'NONE', #225269, #19829 ) ;
#123641 = VERTEX_POINT ( 'NONE', #125185 ) ;
#123640 = EDGE_LOOP ( 'NONE', ( #61135, #132904, #216084, #44681 ) ) ;
#123639 = CIRCLE ( 'NONE', #198462, 1.900000000000012790 ) ;
#123642 = EDGE_LOOP ( 'NONE', ( #122654, #245785, #80181, #179406 ) ) ;
#123643 = CARTESIAN_POINT ( 'NONE',  ( 21.14999999999999858, 10.71339244341104013, -45.75000000000000711 ) ) ;
#123644 = VECTOR ( 'NONE', #190765, 1000.000000000000000 ) ;
#123645 = VERTEX_POINT ( 'NONE', #204694 ) ;
#123646 = AXIS2_PLACEMENT_3D ( 'NONE', #111595, #191152, #188554 ) ;
#123647 = ORIENTED_EDGE ( 'NONE', *, *, #90042, .T. ) ;
#123648 = CARTESIAN_POINT ( 'NONE',  ( 20.94999999999999929, 1.115600667400684642E-11, -134.0000000000000284 ) ) ;
#123649 = CYLINDRICAL_SURFACE ( 'NONE', #19970, 0.09999999999998898659 ) ;
#123651 = ORIENTED_EDGE ( 'NONE', *, *, #102347, .F. ) ;
#123650 = DIRECTION ( 'NONE',  ( 1.000000000000000000, -7.304098846218133681E-16, -4.639676173203992654E-30 ) ) ;
#123653 = CARTESIAN_POINT ( 'NONE',  ( -16.87383368123029825, 60.93935776605891164, -221.0417277355860790 ) ) ;
#123652 = CARTESIAN_POINT ( 'NONE',  ( 18.59999999999999432, 62.13039908340535078, -248.0610840288475174 ) ) ;
#123654 = CARTESIAN_POINT ( 'NONE',  ( 21.07928932188134397, 0.09889514566555242248, -60.67148334360673800 ) ) ;
#123656 = ORIENTED_EDGE ( 'NONE', *, *, #257505, .F. ) ;
#123655 = CARTESIAN_POINT ( 'NONE',  ( -0.8999999999999437339, 64.25000000001119815, -10.02310748452479139 ) ) ;
#123657 = LINE ( 'NONE', #64944, #221931 ) ;
#123658 = VERTEX_POINT ( 'NONE', #26091 ) ;
#123659 = EDGE_LOOP ( 'NONE', ( #112940, #203782, #168048, #49896, #251862, #43247, #134056, #142403, #27046 ) ) ;
#123660 = CARTESIAN_POINT ( 'NONE',  ( -21.03571358705827166, 18.69339893459851254, -226.5978988804882874 ) ) ;
#123661 = LINE ( 'NONE', #6252, #28917 ) ;
#123662 = VECTOR ( 'NONE', #30333, 1000.000000000000000 ) ;
#123663 = ORIENTED_EDGE ( 'NONE', *, *, #30014, .F. ) ;
#123664 = CARTESIAN_POINT ( 'NONE',  ( 21.59780538579342135, 0.09897866960914131207, -26.65290947005674482 ) ) ;
#123665 = DIRECTION ( 'NONE',  ( -1.000000000000000000, 0.000000000000000000, 0.000000000000000000 ) ) ;
#123666 = CARTESIAN_POINT ( 'NONE',  ( -18.59999999999999787, 77.83585931145570669, -124.9186683157258244 ) ) ;
#123667 = VERTEX_POINT ( 'NONE', #62644 ) ;
#123668 = ORIENTED_EDGE ( 'NONE', *, *, #234840, .F. ) ;
#123669 = DIRECTION ( 'NONE',  ( -0.000000000000000000, -6.982962677686266711E-15, 1.000000000000000000 ) ) ;
#123670 = EDGE_CURVE ( 'NONE', #182341, #139599, #122508, .T. ) ;
#123671 = DIRECTION ( 'NONE',  ( 1.000000000000000000, 0.000000000000000000, 0.000000000000000000 ) ) ;
#123672 = ORIENTED_EDGE ( 'NONE', *, *, #172627, .T. ) ;
#123673 = DIRECTION ( 'NONE',  ( 0.000000000000000000, 0.9999631594459055250, 0.008583690987131395445 ) ) ;
#123674 = ORIENTED_EDGE ( 'NONE', *, *, #24096, .T. ) ;
#123675 = LINE ( 'NONE', #84487, #81611 ) ;
#123676 = DIRECTION ( 'NONE',  ( 1.000000000000000000, 0.000000000000000000, -0.000000000000000000 ) ) ;
#123677 = DIRECTION ( 'NONE',  ( 0.000000000000000000, -0.8814952561688476074, 0.4721928772777262417 ) ) ;
#123678 = VECTOR ( 'NONE', #113940, 1000.000000000000000 ) ;
#123679 = CARTESIAN_POINT ( 'NONE',  ( 22.41477678272288188, 0.0008238657741001866345, -55.35041471548464642 ) ) ;
#123680 = TOROIDAL_SURFACE ( 'NONE', #219509, 7.791421356237335338, 0.1000000000000000056 ) ;
#123681 = DIRECTION ( 'NONE',  ( -1.000000000000000000, -2.952720810173289112E-16, 0.000000000000000000 ) ) ;
#123682 = CIRCLE ( 'NONE', #211152, 0.09999999999998898659 ) ;
#123683 = AXIS2_PLACEMENT_3D ( 'NONE', #75292, #154826, #231783 ) ;
#123684 = ORIENTED_EDGE ( 'NONE', *, *, #136889, .F. ) ;
#123685 = FACE_OUTER_BOUND ( 'NONE', #136177, .T. ) ;
#123686 = ADVANCED_FACE ( 'NONE', ( #2648 ), #231432, .F. ) ;
#123687 = VECTOR ( 'NONE', #221726, 1000.000000000000000 ) ;
#123689 = ORIENTED_EDGE ( 'NONE', *, *, #50112, .F. ) ;
#123688 = ORIENTED_EDGE ( 'NONE', *, *, #160313, .T. ) ;
#123690 = VERTEX_POINT ( 'NONE', #44372 ) ;
#123691 = ORIENTED_EDGE ( 'NONE', *, *, #208940, .F. ) ;
#123692 = DIRECTION ( 'NONE',  ( 1.000000000000000000, 0.000000000000000000, 0.000000000000000000 ) ) ;
#123693 = CARTESIAN_POINT ( 'NONE',  ( -23.39999999999994529, 74.83745509109094485, -44.02310748452479316 ) ) ;
#123694 = CARTESIAN_POINT ( 'NONE',  ( -20.64999999999999858, 73.60000000001254250, -183.2477294072864709 ) ) ;
#123695 = LINE ( 'NONE', #28479, #256893 ) ;
#123696 = CARTESIAN_POINT ( 'NONE',  ( 21.05000000000000071, 1.115600667400684642E-11, -100.5000000000000284 ) ) ;
#123698 = DIRECTION ( 'NONE',  ( -3.265361837132813093E-16, -1.000000000000000000, -7.026728003956683390E-15 ) ) ;
#123697 = DIRECTION ( 'NONE',  ( -1.000000000000000000, -0.000000000000000000, -0.000000000000000000 ) ) ;
#123700 = VERTEX_POINT ( 'NONE', #61350 ) ;
#123699 = CARTESIAN_POINT ( 'NONE',  ( 18.59999999999999432, 77.83585931145570669, -125.0186683157258045 ) ) ;
#123701 = CYLINDRICAL_SURFACE ( 'NONE', #137282, 11.75000000000001066 ) ;
#123702 = ORIENTED_EDGE ( 'NONE', *, *, #209373, .T. ) ;
#123703 = CARTESIAN_POINT ( 'NONE',  ( -22.59999985501179154, 11.74986979301414181, -66.93440133020057203 ) ) ;
#123704 = AXIS2_PLACEMENT_3D ( 'NONE', #113818, #53855, #172571 ) ;
#123705 = VERTEX_POINT ( 'NONE', #104304 ) ;
#123706 = EDGE_LOOP ( 'NONE', ( #110422, #246729, #221115, #164069, #61892, #65946, #74567, #200134, #211507, #28348, #95787 ) ) ;
#123707 = FACE_OUTER_BOUND ( 'NONE', #41149, .T. ) ;
#123708 = CYLINDRICAL_SURFACE ( 'NONE', #185038, 0.09999999999999939493 ) ;
#123709 = CARTESIAN_POINT ( 'NONE',  ( -16.83233564386398129, 66.06977820342696361, -48.79858682104877943 ) ) ;
#123710 = LINE ( 'NONE', #24632, #137494 ) ;
#123711 = VECTOR ( 'NONE', #43620, 1000.000000000000114 ) ;
#123712 = CARTESIAN_POINT ( 'NONE',  ( 18.59999999999999076, 65.79142135624952914, -148.6731074845244223 ) ) ;
#123713 = ORIENTED_EDGE ( 'NONE', *, *, #252808, .F. ) ;
#123714 = ORIENTED_EDGE ( 'NONE', *, *, #256031, .T. ) ;
#123715 = DIRECTION ( 'NONE',  ( 0.000000000000000000, 0.000000000000000000, -1.000000000000000000 ) ) ;
#123716 = ORIENTED_EDGE ( 'NONE', *, *, #213948, .F. ) ;
#123717 = CARTESIAN_POINT ( 'NONE',  ( -22.14074124539699540, 0.09905289585522827900, -126.6099221489562439 ) ) ;
#123718 = CARTESIAN_POINT ( 'NONE',  ( -20.64999999999999858, 52.99650480578122824, -234.2878581050858884 ) ) ;
#123719 = CARTESIAN_POINT ( 'NONE',  ( 21.05000000000000071, 69.35000000001228670, -157.8731074845244109 ) ) ;
#123720 = DIRECTION ( 'NONE',  ( 1.000000000000000000, 0.000000000000000000, 0.000000000000000000 ) ) ;
#123721 = CARTESIAN_POINT ( 'NONE',  ( -23.25000000000000000, 85.00000000001223555, -145.8170766071767446 ) ) ;
#123722 = DIRECTION ( 'NONE',  ( -0.000000000000000000, 1.000000000000000000, 8.717686153663073805E-15 ) ) ;
#123723 = CYLINDRICAL_SURFACE ( 'NONE', #137521, 0.09999999999999939493 ) ;
#123725 = EDGE_CURVE ( 'NONE', #75286, #57574, #142167, .T. ) ;
#123724 = DIRECTION ( 'NONE',  ( 0.000000000000000000, 0.000000000000000000, 1.000000000000000000 ) ) ;
#123726 = B_SPLINE_CURVE_WITH_KNOTS ( 'NONE', 3,
 ( #82324, #182760, #4103, #163191, #242705, #64077, #143612, #223142 ),
 .UNSPECIFIED., .F., .F.,
 ( 4, 2, 2, 4 ),
 ( 0.000000000000000000, 0.0001306511400391334671, 0.0001959767100587002007, 0.0002613022800782669342 ),
 .UNSPECIFIED. ) ;
#123727 = CARTESIAN_POINT ( 'NONE',  ( 18.49999999999999289, 65.79142135392936552, -178.8206006188949004 ) ) ;
#123728 = DIRECTION ( 'NONE',  ( 0.000000000000000000, -7.147358527629766941E-15, 1.000000000000000000 ) ) ;
#123729 = AXIS2_PLACEMENT_3D ( 'NONE', #43231, #21123, #237582 ) ;
#123731 = AXIS2_PLACEMENT_3D ( 'NONE', #17248, #172505, #173791 ) ;
#123730 = CARTESIAN_POINT ( 'NONE',  ( -18.59999999999999787, 64.35000000001214460, -136.5231074845244166 ) ) ;
#123732 = VECTOR ( 'NONE', #216854, 1000.000000000000000 ) ;
#123733 = CIRCLE ( 'NONE', #227756, 7.799999999999992717 ) ;
#123734 = ORIENTED_EDGE ( 'NONE', *, *, #144141, .F. ) ;
#123735 = EDGE_CURVE ( 'NONE', #136422, #149532, #10057, .T. ) ;
#123736 = CARTESIAN_POINT ( 'NONE',  ( 20.95520789717937404, 10.57693059939611224, -41.08023297387485684 ) ) ;
#123737 = ORIENTED_EDGE ( 'NONE', *, *, #210026, .F. ) ;
#123738 = DIRECTION ( 'NONE',  ( 1.000000000000000000, 0.000000000000000000, 0.000000000000000000 ) ) ;
#123739 = ADVANCED_FACE ( 'NONE', ( #82164 ), #221684, .F. ) ;
#123740 = DIRECTION ( 'NONE',  ( 0.000000000000000000, 0.2605042016806672911, -0.9654727137038716656 ) ) ;
#123741 = DIRECTION ( 'NONE',  ( 1.000000000000000000, 0.000000000000000000, 0.000000000000000000 ) ) ;
#123742 = ORIENTED_EDGE ( 'NONE', *, *, #123567, .F. ) ;
#123743 = DIRECTION ( 'NONE',  ( 0.000000000000000000, 0.000000000000000000, -1.000000000000000000 ) ) ;
#123744 = CARTESIAN_POINT ( 'NONE',  ( -19.89999999999999858, 5.586869315528661062, 16.41686199900910736 ) ) ;
#123745 = DIRECTION ( 'NONE',  ( 0.000000000000000000, 1.000000000000000000, -0.000000000000000000 ) ) ;
#123746 = DIRECTION ( 'NONE',  ( 0.000000000000000000, 0.9651348961777157509, -0.2617529984165031243 ) ) ;
#123747 = TOROIDAL_SURFACE ( 'NONE', #127848, 0.4000000000000012990, 0.1000000000000000056 ) ;
#123748 = AXIS2_PLACEMENT_3D ( 'NONE', #190275, #11645, #205970 ) ;
#123749 = EDGE_CURVE ( 'NONE', #219135, #104039, #151562, .T. ) ;
#123750 = FACE_OUTER_BOUND ( 'NONE', #181880, .T. ) ;
#123751 = CARTESIAN_POINT ( 'NONE',  ( 20.94999999999999929, 11.65000000001115943, -60.21613433702191287 ) ) ;
#123752 = TOROIDAL_SURFACE ( 'NONE', #11313, 7.800000000000000711, 0.1000000000000000056 ) ;
#123753 = ORIENTED_EDGE ( 'NONE', *, *, #8605, .F. ) ;
#123754 = DIRECTION ( 'NONE',  ( -1.000000000000000000, 0.000000000000000000, 1.927470528863115795E-15 ) ) ;
#123756 = ORIENTED_EDGE ( 'NONE', *, *, #185527, .T. ) ;
#123755 = DIRECTION ( 'NONE',  ( 0.000000000000000000, 0.000000000000000000, 1.000000000000000000 ) ) ;
#123757 = CARTESIAN_POINT ( 'NONE',  ( -20.54999999999999716, 9.350000000000001421, -12.25000000000000000 ) ) ;
#123758 = DIRECTION ( 'NONE',  ( 0.000000000000000000, 0.9126074666063660468, 0.4088369013363524762 ) ) ;
#123759 = EDGE_CURVE ( 'NONE', #228170, #142241, #131588, .T. ) ;
#123760 = CARTESIAN_POINT ( 'NONE',  ( 23.14999999999999503, 59.16775194334852017, -221.0793150863668473 ) ) ;
#123761 = ORIENTED_EDGE ( 'NONE', *, *, #207785, .T. ) ;
#123762 = CYLINDRICAL_SURFACE ( 'NONE', #151470, 0.1000000000000013933 ) ;
#123763 = PRODUCT_CONTEXT ( 'NONE', #180708, 'mechanical' ) ;
#123764 = LINE ( 'NONE', #100315, #175542 ) ;
#123765 = ORIENTED_EDGE ( 'NONE', *, *, #242913, .F. ) ;
#123766 = DIRECTION ( 'NONE',  ( 0.000000000000000000, 0.2128009952263605065, -0.9770955615653315052 ) ) ;
#123767 = DIRECTION ( 'NONE',  ( -1.000000000000000000, 0.000000000000000000, 0.000000000000000000 ) ) ;
#123768 = AXIS2_PLACEMENT_3D ( 'NONE', #214110, #251945, #72041 ) ;
#123769 = DIRECTION ( 'NONE',  ( 0.000000000000000000, 0.000000000000000000, 1.000000000000000000 ) ) ;
#123770 = ORIENTED_EDGE ( 'NONE', *, *, #45063, .T. ) ;
#123771 = ORIENTED_EDGE ( 'NONE', *, *, #17357, .T. ) ;
#123772 = CARTESIAN_POINT ( 'NONE',  ( -18.50000000000000000, 10.29270135741298375, -139.4573618871519614 ) ) ;
#123773 = DIRECTION ( 'NONE',  ( 0.000000000000000000, 1.000000000000000000, -0.000000000000000000 ) ) ;
#123774 = DIRECTION ( 'NONE',  ( -1.000000000000000000, 0.000000000000000000, 0.000000000000000000 ) ) ;
#123775 = EDGE_CURVE ( 'NONE', #246341, #219596, #12954, .T. ) ;
#123776 = CYLINDRICAL_SURFACE ( 'NONE', #148941, 2.000000000000001776 ) ;
#123777 = DIRECTION ( 'NONE',  ( -0.000000000000000000, 0.8660254037844377084, 0.5000000000000016653 ) ) ;
#123778 = CARTESIAN_POINT ( 'NONE',  ( -16.87036670365548474, 65.91505003675672469, -115.5731074845243711 ) ) ;
#123779 = CARTESIAN_POINT ( 'NONE',  ( 22.60000000000000497, -3.206176178680899991, -228.1422727337474896 ) ) ;
#123781 = CIRCLE ( 'NONE', #111315, 11.70000000000001528 ) ;
#123780 = DIRECTION ( 'NONE',  ( 0.000000000000000000, 0.4999999999999088507, -0.8660254037844913322 ) ) ;
#123782 = CARTESIAN_POINT ( 'NONE',  ( -22.39999999999999858, 31.85509083104287598, -238.8280249686205536 ) ) ;
#123783 = LINE ( 'NONE', #203320, #6285 ) ;
#123784 = CARTESIAN_POINT ( 'NONE',  ( -33.72168855820452649, 23.65833333333332433, -16.75000000000000000 ) ) ;
#123785 = AXIS2_PLACEMENT_3D ( 'NONE', #134085, #213634, #75441 ) ;
#123786 = ORIENTED_EDGE ( 'NONE', *, *, #157424, .T. ) ;
#123787 = AXIS2_PLACEMENT_3D ( 'NONE', #127508, #115644, #256367 ) ;
#123788 = ORIENTED_EDGE ( 'NONE', *, *, #226660, .T. ) ;
#123789 = CARTESIAN_POINT ( 'NONE',  ( -20.94999999999999929, 67.85909929089923764, -227.8797997985275856 ) ) ;
#123790 = CARTESIAN_POINT ( 'NONE',  ( -20.00857864376270001, 9.250000000011157297, -121.6500000000000341 ) ) ;
#123792 = CARTESIAN_POINT ( 'NONE',  ( -13.77083647240106323, 13.17759476088265203, -217.0636392655389102 ) ) ;
#123791 = CARTESIAN_POINT ( 'NONE',  ( -13.39999999999994351, 63.75000000001119815, -21.02310748452479316 ) ) ;
#123793 = PRODUCT_DEFINITION_FORMATION_WITH_SPECIFIED_SOURCE ( 'ANY', '', #26382, .NOT_KNOWN. ) ;
#123794 = EDGE_CURVE ( 'NONE', #6262, #17415, #131042, .T. ) ;
#123795 = AXIS2_PLACEMENT_3D ( 'NONE', #178502, #199334, #256671 ) ;
#123796 = DIRECTION ( 'NONE',  ( 0.000000000000000000, -0.9609271840673806464, 0.2768012769485257429 ) ) ;
#123797 = CARTESIAN_POINT ( 'NONE',  ( 23.15000000000000213, 87.65000000001165859, -69.52310748452424605 ) ) ;
#123798 = CIRCLE ( 'NONE', #11179, 11.70000000000001528 ) ;
#123799 = FACE_OUTER_BOUND ( 'NONE', #236085, .T. ) ;
#123800 = CARTESIAN_POINT ( 'NONE',  ( -21.44999999999999929, 44.92467540951147953, -237.7943620901849613 ) ) ;
#123801 = EDGE_CURVE ( 'NONE', #145080, #255597, #108188, .T. ) ;
#123802 = ORIENTED_EDGE ( 'NONE', *, *, #126280, .T. ) ;
#123803 = LINE ( 'NONE', #61255, #109515 ) ;
#123804 = ORIENTED_EDGE ( 'NONE', *, *, #167276, .T. ) ;
#123805 = ADVANCED_FACE ( 'NONE', ( #89883 ), #48198, .F. ) ;
#123806 = CARTESIAN_POINT ( 'NONE',  ( -18.59999999999999787, 11.65000000001115232, -174.5148057706539930 ) ) ;
#123807 = CIRCLE ( 'NONE', #32236, 0.09999999999998898659 ) ;
#123808 = AXIS2_PLACEMENT_3D ( 'NONE', #149280, #8471, #249654 ) ;
#123809 = DIRECTION ( 'NONE',  ( 1.000000000000000000, 3.265361837132813093E-16, -0.000000000000000000 ) ) ;
#123811 = EDGE_LOOP ( 'NONE', ( #5403, #81892, #47845, #27239 ) ) ;
#123810 = CIRCLE ( 'NONE', #40455, 12.77500000000000036 ) ;
#123812 = CARTESIAN_POINT ( 'NONE',  ( -18.50000972452446035, 18.34807417603271418, -236.8765254748879556 ) ) ;
#123813 = ADVANCED_FACE ( 'NONE', ( #87315 ), #5938, .T. ) ;
#123814 = VERTEX_POINT ( 'NONE', #247688 ) ;
#123815 = VECTOR ( 'NONE', #9059, 1000.000000000000000 ) ;
#123816 = DIRECTION ( 'NONE',  ( 0.000000000000000000, 7.116814260417668513E-15, -1.000000000000000000 ) ) ;
#123817 = CARTESIAN_POINT ( 'NONE',  ( -21.93340585972066137, 68.67585297715831416, -69.52310748452435973 ) ) ;
#123818 = DIRECTION ( 'NONE',  ( 2.952720810173289112E-16, -1.000000000000000000, 0.000000000000000000 ) ) ;
#123819 = EDGE_CURVE ( 'NONE', #19771, #105588, #226716, .T. ) ;
#123820 = CARTESIAN_POINT ( 'NONE',  ( 20.94999999999999929, 78.50726470275242264, -228.6618886302502176 ) ) ;
#123821 = ADVANCED_FACE ( 'NONE', ( #189004 ), #186444, .T. ) ;
#123822 = CARTESIAN_POINT ( 'NONE',  ( -21.14999999999999858, 1.115600667400684642E-11, -93.95934304829879125 ) ) ;
#123823 = CARTESIAN_POINT ( 'NONE',  ( 23.04999999999999716, 67.17743825834509153, -45.27310748452438816 ) ) ;
#123824 = DIRECTION ( 'NONE',  ( 0.000000000000000000, 6.982962677686267499E-15, -1.000000000000000000 ) ) ;
#123825 = CARTESIAN_POINT ( 'NONE',  ( 23.15000000000000213, 23.45160524131172153, -253.2535058871250726 ) ) ;
#123827 = EDGE_LOOP ( 'NONE', ( #151875, #211790, #204438, #233375, #57494, #2100, #6199, #167364, #119477, #182015 ) ) ;
#123826 = CARTESIAN_POINT ( 'NONE',  ( -20.54999999999999716, 76.00000000001141132, -34.02310748452431710 ) ) ;
#123829 = DIRECTION ( 'NONE',  ( -0.7071067811865388020, 0.7071067811865561215, 0.000000000000000000 ) ) ;
#123828 = CARTESIAN_POINT ( 'NONE',  ( -20.94999999999999929, 86.52890073500824997, -209.5906233940697234 ) ) ;
#123830 = ORIENTED_EDGE ( 'NONE', *, *, #208566, .T. ) ;
#123832 = ORIENTED_EDGE ( 'NONE', *, *, #223017, .F. ) ;
#123831 = CARTESIAN_POINT ( 'NONE',  ( -23.15000000000000213, 11.65000000001115588, -122.2500000000000284 ) ) ;
#123833 = AXIS2_PLACEMENT_3D ( 'NONE', #68154, #29070, #94132 ) ;
#123834 = ORIENTED_EDGE ( 'NONE', *, *, #29435, .F. ) ;
#123835 = DIRECTION ( 'NONE',  ( -1.000000000000000000, 0.000000000000000000, 0.000000000000000000 ) ) ;
#123836 = AXIS2_PLACEMENT_3D ( 'NONE', #221506, #242366, #122437 ) ;
#123837 = DIRECTION ( 'NONE',  ( 0.000000000000000000, 0.9910465087640860649, -0.1335171055202901413 ) ) ;
#123838 = EDGE_CURVE ( 'NONE', #138100, #21468, #72624, .T. ) ;
#123839 = ORIENTED_EDGE ( 'NONE', *, *, #50197, .F. ) ;
#123840 = CARTESIAN_POINT ( 'NONE',  ( -20.64999999999999858, 68.85000000001259934, -191.2731074845244166 ) ) ;
#123841 = CARTESIAN_POINT ( 'NONE',  ( 23.24999999999999289, 64.25000000001244871, -181.7731074845244450 ) ) ;
#123842 = CARTESIAN_POINT ( 'NONE',  ( 18.50000000000000000, 38.28679861725831302, -261.0868692510649680 ) ) ;
#123843 = EDGE_CURVE ( 'NONE', #21650, #171420, #214267, .T. ) ;
#123844 = ADVANCED_FACE ( 'NONE', ( #149894 ), #148602, .F. ) ;
#123845 = ORIENTED_EDGE ( 'NONE', *, *, #79987, .T. ) ;
#123846 = CARTESIAN_POINT ( 'NONE',  ( 21.05000000000000071, 1.162701749949165642, -175.5999999999999659 ) ) ;
#123847 = CIRCLE ( 'NONE', #70269, 0.09999999999999939493 ) ;
#123848 = AXIS2_PLACEMENT_3D ( 'NONE', #151264, #230807, #89975 ) ;
#123849 = CARTESIAN_POINT ( 'NONE',  ( -18.59999999999999787, 36.65892442174472876, -249.5511627012454596 ) ) ;
#123850 = ORIENTED_EDGE ( 'NONE', *, *, #244045, .T. ) ;
#123851 = EDGE_LOOP ( 'NONE', ( #29345, #235083, #107386, #25592, #125398 ) ) ;
#123852 = DIRECTION ( 'NONE',  ( 0.000000000000000000, 0.2617529984164955192, 0.9651348961777177493 ) ) ;
#123853 = VERTEX_POINT ( 'NONE', #230707 ) ;
#123854 = LINE ( 'NONE', #101675, #9206 ) ;
#123855 = ORIENTED_EDGE ( 'NONE', *, *, #17070, .F. ) ;
#123856 = CARTESIAN_POINT ( 'NONE',  ( -20.85000000000000142, 46.02130280899747561, -256.6489974955837852 ) ) ;
#123857 = TOROIDAL_SURFACE ( 'NONE', #48817, 11.65000000000000036, 0.1000000000000000056 ) ;
#123858 = EDGE_CURVE ( 'NONE', #131694, #130891, #64415, .T. ) ;
#123859 = CARTESIAN_POINT ( 'NONE',  ( -22.47071067811865319, 68.27992525551387359, -103.1221999392269595 ) ) ;
#123860 = ADVANCED_FACE ( 'NONE', ( #172043 ), #139210, .T. ) ;
#123861 = CARTESIAN_POINT ( 'NONE',  ( -21.07933241753356413, 30.84517785335011908, -252.0533277889904866 ) ) ;
#123862 = CARTESIAN_POINT ( 'NONE',  ( -23.15000000000000213, -8.663551401858004652, -43.02410111806730697 ) ) ;
#123863 = VERTEX_POINT ( 'NONE', #10378 ) ;
#123864 = CIRCLE ( 'NONE', #7321, 0.2000000000000057288 ) ;
#123865 = TOROIDAL_SURFACE ( 'NONE', #73806, 0.6000000000000013101, 0.1000000000000000056 ) ;
#123866 = DIRECTION ( 'NONE',  ( 0.000000000000000000, -6.853228547068871147E-15, 1.000000000000000000 ) ) ;
#123867 = AXIS2_PLACEMENT_3D ( 'NONE', #10497, #112177, #13077 ) ;
#123868 = AXIS2_PLACEMENT_3D ( 'NONE', #40022, #76536, #56945 ) ;
#123869 = EDGE_CURVE ( 'NONE', #16854, #106553, #175887, .T. ) ;
#123870 = CARTESIAN_POINT ( 'NONE',  ( 21.14999999999999858, 65.28660755661216797, -124.2731074845243739 ) ) ;
#123871 = SPHERICAL_SURFACE ( 'NONE', #57256, 0.1000000000000000056 ) ;
#123872 = FACE_OUTER_BOUND ( 'NONE', #249455, .T. ) ;
#123873 = ORIENTED_EDGE ( 'NONE', *, *, #164723, .T. ) ;
#123875 = DIRECTION ( 'NONE',  ( 3.469446951953646374E-14, -0.7899159663865635839, -0.6132151058540398214 ) ) ;
#123874 = DIRECTION ( 'NONE',  ( 1.000000000000000000, 0.000000000000000000, 0.000000000000000000 ) ) ;
#123876 = EDGE_LOOP ( 'NONE', ( #125566, #25136, #165358, #232280 ) ) ;
#123878 = ORIENTED_EDGE ( 'NONE', *, *, #176764, .F. ) ;
#123877 = SURFACE_STYLE_FILL_AREA ( #83419 ) ;
#123879 = CIRCLE ( 'NONE', #69712, 11.90000000000000036 ) ;
#123880 = EDGE_LOOP ( 'NONE', ( #228461, #51547, #190300, #154938 ) ) ;
#123881 = DIRECTION ( 'NONE',  ( 0.000000000000000000, 0.4999999999999088507, -0.8660254037844913322 ) ) ;
#123882 = DIRECTION ( 'NONE',  ( 0.000000000000000000, 0.000000000000000000, 1.000000000000000000 ) ) ;
#123883 = FACE_OUTER_BOUND ( 'NONE', #224964, .T. ) ;
#123884 = ORIENTED_EDGE ( 'NONE', *, *, #250943, .F. ) ;
#123885 = CYLINDRICAL_SURFACE ( 'NONE', #26240, 0.09999999999998898659 ) ;
#123886 = CARTESIAN_POINT ( 'NONE',  ( -18.59999999999999787, 7.120270961708750512, -104.1595630418393768 ) ) ;
#123888 = CARTESIAN_POINT ( 'NONE',  ( 21.05000000000000071, -8.999999999988842703, -157.6060308773475640 ) ) ;
#123887 = CYLINDRICAL_SURFACE ( 'NONE', #13927, 0.1000000000000052097 ) ;
#123890 = EDGE_LOOP ( 'NONE', ( #130977, #141225, #108838, #129235 ) ) ;
#123889 = DIRECTION ( 'NONE',  ( 1.000000000000000000, 0.000000000000000000, 0.000000000000000000 ) ) ;
#123891 = AXIS2_PLACEMENT_3D ( 'NONE', #214853, #77901, #75377 ) ;
#123892 = EDGE_CURVE ( 'NONE', #77493, #81484, #101792, .T. ) ;
#123893 = ORIENTED_EDGE ( 'NONE', *, *, #41408, .F. ) ;
#123894 = EDGE_CURVE ( 'NONE', #26209, #227798, #173340, .T. ) ;
#123895 = CARTESIAN_POINT ( 'NONE',  ( -16.89268316805466341, 9.951721813253341153, -79.64424752145448849 ) ) ;
#123896 = CYLINDRICAL_SURFACE ( 'NONE', #106187, 0.5000000000000004441 ) ;
#123897 = CIRCLE ( 'NONE', #36620, 0.1000000000000035305 ) ;
#123898 = CARTESIAN_POINT ( 'NONE',  ( -22.39999999999999858, 0.09999999999999939493, 7.790779598373403836 ) ) ;
#123899 = VERTEX_POINT ( 'NONE', #74225 ) ;
#123900 = CARTESIAN_POINT ( 'NONE',  ( -14.00000000000000178, 62.10905854918435409, -217.1108499610990918 ) ) ;
#123901 = VERTEX_POINT ( 'NONE', #59726 ) ;
#123902 = CYLINDRICAL_SURFACE ( 'NONE', #68380, 4.000000000000003553 ) ;
#123903 = EDGE_CURVE ( 'NONE', #198122, #250577, #97565, .T. ) ;
#123904 = CARTESIAN_POINT ( 'NONE',  ( -18.50000000000000000, 1.115600667400684642E-11, -100.5000000000000426 ) ) ;
#123905 = DIRECTION ( 'NONE',  ( 1.000000000000000000, -0.000000000000000000, -0.000000000000000000 ) ) ;
#123906 = ORIENTED_EDGE ( 'NONE', *, *, #31082, .T. ) ;
#123907 = LINE ( 'NONE', #187738, #183563 ) ;
#123908 = EDGE_CURVE ( 'NONE', #181190, #109505, #118606, .T. ) ;
#123909 = EDGE_CURVE ( 'NONE', #206936, #161742, #15522, .T. ) ;
#123910 = AXIS2_PLACEMENT_3D ( 'NONE', #171893, #231847, #109294 ) ;
#123911 = CIRCLE ( 'NONE', #236320, 0.09999999999999939493 ) ;
#123912 = DIRECTION ( 'NONE',  ( 1.000000000000000000, 0.000000000000000000, 0.000000000000000000 ) ) ;
#123913 = AXIS2_PLACEMENT_3D ( 'NONE', #123730, #63745, #104137 ) ;
#123914 = EDGE_CURVE ( 'NONE', #150331, #232336, #60116, .T. ) ;
#123915 = EDGE_LOOP ( 'NONE', ( #245458, #97165, #224529, #61788 ) ) ;
#123916 = ORIENTED_EDGE ( 'NONE', *, *, #215531, .T. ) ;
#123918 = EDGE_CURVE ( 'NONE', #126778, #134853, #235815, .T. ) ;
#123917 = EDGE_CURVE ( 'NONE', #199100, #214956, #156015, .T. ) ;
#123919 = VERTEX_POINT ( 'NONE', #118462 ) ;
#123920 = CARTESIAN_POINT ( 'NONE',  ( -22.47071067811865319, 0.09909245471376171288, -126.2799252555019649 ) ) ;
#123921 = VERTEX_POINT ( 'NONE', #252810 ) ;
#123923 = EDGE_LOOP ( 'NONE', ( #202467, #183842, #138248 ) ) ;
#123922 = CARTESIAN_POINT ( 'NONE',  ( 15.74999999999999289, 66.65000000001258229, -186.6573643172504831 ) ) ;
#123924 = ORIENTED_EDGE ( 'NONE', *, *, #206618, .T. ) ;
#123927 = VERTEX_POINT ( 'NONE', #98841 ) ;
#123926 = ORIENTED_EDGE ( 'NONE', *, *, #137109, .T. ) ;
#123925 = CARTESIAN_POINT ( 'NONE',  ( -18.50000000000000000, 70.22659352830977753, -197.9852579278363578 ) ) ;
#123928 = VECTOR ( 'NONE', #60010, 1000.000000000000000 ) ;
#123929 = DIRECTION ( 'NONE',  ( 0.000000000000000000, -6.454785026890489601E-15, 1.000000000000000000 ) ) ;
#123930 = VECTOR ( 'NONE', #157819, 1000.000000000000000 ) ;
#123931 = ORIENTED_EDGE ( 'NONE', *, *, #81030, .F. ) ;
#123932 = DIRECTION ( 'NONE',  ( 0.000000000000000000, -6.938893903907234689E-15, 1.000000000000000000 ) ) ;
#123933 = ADVANCED_FACE ( 'NONE', ( #35101 ), #157615, .F. ) ;
#123934 = EDGE_CURVE ( 'NONE', #108723, #15940, #176858, .T. ) ;
#123935 = CARTESIAN_POINT ( 'NONE',  ( 21.05000000000000071, 67.07338541492552508, -195.0514244653012952 ) ) ;
#123936 = DIRECTION ( 'NONE',  ( 0.000000000000000000, -7.056502275159894776E-15, 1.000000000000000000 ) ) ;
#123937 = EDGE_LOOP ( 'NONE', ( #120952, #227555, #106253, #153685 ) ) ;
#123938 = ADVANCED_FACE ( 'NONE', ( #33823 ), #95085, .T. ) ;
#123939 = CARTESIAN_POINT ( 'NONE',  ( 18.59999999999999076, 15.51794587355511545, -222.9505302427971003 ) ) ;
#123941 = ORIENTED_EDGE ( 'NONE', *, *, #74069, .T. ) ;
#123940 = DIRECTION ( 'NONE',  ( -1.000000000000000000, -0.000000000000000000, -0.000000000000000000 ) ) ;
#123942 = CARTESIAN_POINT ( 'NONE',  ( -16.89268316805465986, 14.16190809729244648, -219.2603268738197073 ) ) ;
#123944 = EDGE_LOOP ( 'NONE', ( #253769, #92898, #29666, #211048 ) ) ;
#123943 = FACE_OUTER_BOUND ( 'NONE', #120308, .T. ) ;
#123945 = ORIENTED_EDGE ( 'NONE', *, *, #218085, .F. ) ;
#123946 = ADVANCED_FACE ( 'NONE', ( #115885 ), #135428, .T. ) ;
#123947 = EDGE_CURVE ( 'NONE', #93920, #215460, #1840, .T. ) ;
#123948 = ORIENTED_EDGE ( 'NONE', *, *, #159548, .F. ) ;
#123949 = ORIENTED_EDGE ( 'NONE', *, *, #251012, .T. ) ;
#123950 = CARTESIAN_POINT ( 'NONE',  ( -18.50000000000000000, 69.15387683765952431, -132.7853812176745407 ) ) ;
#123951 = DIRECTION ( 'NONE',  ( 1.000000000000000000, 0.000000000000000000, 0.000000000000000000 ) ) ;
#123952 = AXIS2_PLACEMENT_3D ( 'NONE', #159289, #56300, #141007 ) ;
#123953 = CIRCLE ( 'NONE', #116151, 0.6000000000000033085 ) ;
#123955 = ORIENTED_EDGE ( 'NONE', *, *, #15796, .T. ) ;
#123954 = VERTEX_POINT ( 'NONE', #37647 ) ;
#123956 = ORIENTED_EDGE ( 'NONE', *, *, #48648, .F. ) ;
#123957 = FACE_OUTER_BOUND ( 'NONE', #230919, .T. ) ;
#123958 = ORIENTED_EDGE ( 'NONE', *, *, #137688, .T. ) ;
#123959 = ORIENTED_EDGE ( 'NONE', *, *, #227212, .T. ) ;
#123960 = CARTESIAN_POINT ( 'NONE',  ( 11.60000000000000142, -11.65000000000000036, 17.70000000000000284 ) ) ;
#123962 = ORIENTED_EDGE ( 'NONE', *, *, #34338, .F. ) ;
#123961 = DIRECTION ( 'NONE',  ( 1.000000000000000000, 0.000000000000000000, 0.000000000000000000 ) ) ;
#123963 = EDGE_CURVE ( 'NONE', #110507, #176941, #22774, .T. ) ;
#123964 = CARTESIAN_POINT ( 'NONE',  ( 23.14999999999999503, 61.95000000001248708, -175.5368025552853624 ) ) ;
#123965 = TOROIDAL_SURFACE ( 'NONE', #36688, 0.2000000000000000111, 0.1000000000000000056 ) ;
#123967 = DIRECTION ( 'NONE',  ( -0.000000000000000000, -0.000000000000000000, 1.000000000000000000 ) ) ;
#123966 = CARTESIAN_POINT ( 'NONE',  ( -21.05000000000000071, 64.40000000001249703, -176.9513107147999449 ) ) ;
#123968 = ORIENTED_EDGE ( 'NONE', *, *, #97896, .F. ) ;
#123970 = EDGE_LOOP ( 'NONE', ( #151410, #134184, #87181 ) ) ;
#123969 = ORIENTED_EDGE ( 'NONE', *, *, #9279, .F. ) ;
#123971 = AXIS2_PLACEMENT_3D ( 'NONE', #168443, #208803, #75717 ) ;
#123972 = EDGE_CURVE ( 'NONE', #36199, #29274, #10261, .T. ) ;
#123973 = DIRECTION ( 'NONE',  ( 0.000000000000000000, 7.056502275159890832E-15, -1.000000000000000000 ) ) ;
#123974 = DIRECTION ( 'NONE',  ( 0.000000000000000000, -0.1455152366551522025, -0.9893560106964505163 ) ) ;
#123975 = ORIENTED_EDGE ( 'NONE', *, *, #182377, .T. ) ;
#123976 = AXIS2_PLACEMENT_3D ( 'NONE', #116496, #34416, #193473 ) ;
#123977 = CIRCLE ( 'NONE', #257187, 0.1000000000000043493 ) ;
#123978 = CARTESIAN_POINT ( 'NONE',  ( 18.79999999999999716, 1.250000000000000000, 16.60000000000000142 ) ) ;
#123979 = AXIS2_PLACEMENT_3D ( 'NONE', #222069, #220815, #142553 ) ;
#123980 = ORIENTED_EDGE ( 'NONE', *, *, #231751, .F. ) ;
#123981 = ORIENTED_EDGE ( 'NONE', *, *, #142319, .T. ) ;
#123982 = DIRECTION ( 'NONE',  ( 0.000000000000000000, 0.000000000000000000, 1.000000000000000000 ) ) ;
#123983 = ADVANCED_FACE ( 'NONE', ( #244795 ), #213129, .T. ) ;
#123984 = VECTOR ( 'NONE', #253584, 1000.000000000000000 ) ;
#123985 = ORIENTED_EDGE ( 'NONE', *, *, #166934, .T. ) ;
#123986 = CARTESIAN_POINT ( 'NONE',  ( -21.00250684356851849, 11.75000000001115197, -107.5148057687598566 ) ) ;
#123987 = ORIENTED_EDGE ( 'NONE', *, *, #49983, .T. ) ;
#123988 = CARTESIAN_POINT ( 'NONE',  ( -20.54999999999999716, 73.60000000001151932, -49.24772940728643533 ) ) ;
#123989 = CARTESIAN_POINT ( 'NONE',  ( 20.85000000000000142, 77.83585931145498193, -24.51866831572578675 ) ) ;
#123991 = CARTESIAN_POINT ( 'NONE',  ( 21.05000000000000071, -11.64999999998883595, -164.6000000000000227 ) ) ;
#123990 = LINE ( 'NONE', #242628, #244432 ) ;
#123992 = CYLINDRICAL_SURFACE ( 'NONE', #248227, 0.8750000000000007772 ) ;
#123993 = DIRECTION ( 'NONE',  ( 0.000000000000000000, -0.9691069652679039637, 0.2466408114429434750 ) ) ;
#123994 = DIRECTION ( 'NONE',  ( -0.000000000000000000, -6.982962677686266711E-15, 1.000000000000000000 ) ) ;
#123995 = FACE_OUTER_BOUND ( 'NONE', #175960, .T. ) ;
#123996 = CIRCLE ( 'NONE', #207203, 0.09999999999999824307 ) ;
#123997 = ORIENTED_EDGE ( 'NONE', *, *, #24359, .T. ) ;
#123998 = ADVANCED_FACE ( 'NONE', ( #144392 ), #223946, .F. ) ;
#123999 = AXIS2_PLACEMENT_3D ( 'NONE', #125535, #172411, #113670 ) ;
#124002 = VERTEX_POINT ( 'NONE', #162720 ) ;
#124001 = ORIENTED_EDGE ( 'NONE', *, *, #146406, .T. ) ;
#124000 = AXIS2_PLACEMENT_3D ( 'NONE', #166654, #145754, #83195 ) ;
#124003 = EDGE_LOOP ( 'NONE', ( #172559, #83028, #183727, #17782 ) ) ;
#124004 = VECTOR ( 'NONE', #190967, 1000.000000000000000 ) ;
#124005 = DIRECTION ( 'NONE',  ( 0.000000000000000000, 1.000000000000000000, 0.000000000000000000 ) ) ;
#124006 =( BOUNDED_SURFACE ( )  B_SPLINE_SURFACE ( 3, 2, ( 
 ( #193011, #247751, #40914 ),
 ( #126524, #100807, #139957 ),
 ( #198666, #66555, #125243 ),
 ( #79975, #27470, #46963 ),
 ( #144778, #159556, #146072 ),
 ( #180400, #119144, #26152 ),
 ( #206059, #246466, #207358 ),
 ( #239088, #106943, #224334 ) ),
 .UNSPECIFIED., .F., .F., .F. ) 
 B_SPLINE_SURFACE_WITH_KNOTS ( ( 4, 2, 2, 4 ),
 ( 3, 3 ),
 ( 0.0001704874539069695018, 0.0003809798300636461129, 0.0004862260181419844184, 0.0005914722062203227240 ),
 ( 0.000000000000000000, 1.000000000000000000 ),
 .UNSPECIFIED. ) 
 GEOMETRIC_REPRESENTATION_ITEM ( )  RATIONAL_B_SPLINE_SURFACE ( (
 ( 1.000000000000000000, 0.7071067811865302533, 1.000000000000000000),
 ( 1.000000000000000000, 0.7670648383570790596, 1.000000000000000000),
 ( 1.000000000000000000, 0.8204820770259678708, 1.000000000000000000),
 ( 1.000000000000000000, 0.8877218296110218620, 1.000000000000000000),
 ( 1.000000000000000000, 0.9080815932661593370, 1.000000000000000000),
 ( 1.000000000000000000, 0.9395541505865371290, 1.000000000000000000),
 ( 1.000000000000000000, 0.9506520335376564823, 1.000000000000000000),
 ( 1.000000000000000000, 0.9504532311154358926, 1.000000000000000000) ) ) 
 REPRESENTATION_ITEM ( '' )  SURFACE ( )  );
#124007 = CARTESIAN_POINT ( 'NONE',  ( -16.89268316805465986, 66.04827818676963602, -82.16735500597883401 ) ) ;
#124008 = AXIS2_PLACEMENT_3D ( 'NONE', #3604, #21900, #45308 ) ;
#124010 = CARTESIAN_POINT ( 'NONE',  ( 21.33487959338958362, 6.725558151911193328, -1.166372555419950539E-16 ) ) ;
#124009 = DIRECTION ( 'NONE',  ( -1.000000000000000000, 5.751876041739926423E-15, -1.546394132359972529E-14 ) ) ;
#124011 = CARTESIAN_POINT ( 'NONE',  ( -18.40000000000000213, 11.48667500176882328, -109.7500000000000426 ) ) ;
#124012 = ORIENTED_EDGE ( 'NONE', *, *, #255549, .F. ) ;
#124013 = CARTESIAN_POINT ( 'NONE',  ( -21.55000000000000071, 65.89281126173843006, -213.4744760240239145 ) ) ;
#124014 = CARTESIAN_POINT ( 'NONE',  ( -13.40000000000000036, -8.350000000000004974, 19.04142135623731491 ) ) ;
#124015 = DIRECTION ( 'NONE',  ( 1.000000000000000000, 0.000000000000000000, 0.000000000000000000 ) ) ;
#124016 = CARTESIAN_POINT ( 'NONE',  ( -16.94052228080551359, 9.986279733109993728, -87.89037550266947108 ) ) ;
#124017 = ORIENTED_EDGE ( 'NONE', *, *, #24690, .F. ) ;
#124018 = CIRCLE ( 'NONE', #7470, 0.09999999999999939493 ) ;
#124019 = CIRCLE ( 'NONE', #182278, 0.09999999999999742428 ) ;
#124020 = CARTESIAN_POINT ( 'NONE',  ( 21.70464131381650219, 7.095358018979006864, -134.0000000000000000 ) ) ;
#124021 = CARTESIAN_POINT ( 'NONE',  ( -21.07928932188134041, 0.09889514566555070163, -94.17148334360673800 ) ) ;
#124022 = ORIENTED_EDGE ( 'NONE', *, *, #19615, .F. ) ;
#124023 = DIRECTION ( 'NONE',  ( 1.875376730785737719E-16, -0.9770955615653315052, -0.2128009952263603954 ) ) ;
#124024 = CARTESIAN_POINT ( 'NONE',  ( -22.14074124539699895, 0.6612868435708807446, -230.1558445308521073 ) ) ;
#124025 = CARTESIAN_POINT ( 'NONE',  ( -20.94999999999999929, 77.83534155023598089, -57.96795619196132776 ) ) ;
#124026 = DIRECTION ( 'NONE',  ( -0.000000000000000000, -2.891205793294679805E-16, 1.000000000000000000 ) ) ;
#124027 = DIRECTION ( 'NONE',  ( -1.000000000000000000, -0.000000000000000000, -0.000000000000000000 ) ) ;
#124028 = CARTESIAN_POINT ( 'NONE',  ( 20.94999999999999574, 87.65000000001163016, -66.62310748452424036 ) ) ;
#124029 = ORIENTED_EDGE ( 'NONE', *, *, #137848, .T. ) ;
#124030 = DIRECTION ( 'NONE',  ( 0.000000000000000000, 1.000000000000000000, 0.000000000000000000 ) ) ;
#124031 = FACE_OUTER_BOUND ( 'NONE', #72591, .T. ) ;
#124032 = CARTESIAN_POINT ( 'NONE',  ( -21.04999999999999716, 0.09843750001115433856, -60.70076908991315889 ) ) ;
#124033 = AXIS2_PLACEMENT_3D ( 'NONE', #62434, #141953, #198080 ) ;
#124035 = CARTESIAN_POINT ( 'NONE',  ( 20.85000000000000142, 36.65892442174935439, -249.5511627012433848 ) ) ;
#124034 = CARTESIAN_POINT ( 'NONE',  ( 18.39999999999999503, 11.75000000001113953, -79.65000000000004832 ) ) ;
#124037 = ADVANCED_FACE ( 'NONE', ( #180999 ), #20647, .T. ) ;
#124036 = DIRECTION ( 'NONE',  ( 0.000000000000000000, -1.000000000000000000, 0.000000000000000000 ) ) ;
#124038 = AXIS2_PLACEMENT_3D ( 'NONE', #62422, #143218, #102793 ) ;
#124039 = CARTESIAN_POINT ( 'NONE',  ( -20.00857864376270001, 44.18876898710608003, -236.1516686502934590 ) ) ;
#124040 = CARTESIAN_POINT ( 'NONE',  ( 21.05000000000000071, 1.115600667400684642E-11, -67.00000000000000000 ) ) ;
#124042 = DIRECTION ( 'NONE',  ( 1.000000000000000000, 0.000000000000000000, 0.000000000000000000 ) ) ;
#124041 = CIRCLE ( 'NONE', #19983, 1.500000000000001332 ) ;
#124044 = EDGE_LOOP ( 'NONE', ( #170684, #112364, #68360, #53848 ) ) ;
#124043 = CARTESIAN_POINT ( 'NONE',  ( -17.29838795458769596, 10.37154985796132500, -145.3952587173806705 ) ) ;
#124045 = CIRCLE ( 'NONE', #40687, 0.09999999999999939493 ) ;
#124046 = EDGE_CURVE ( 'NONE', #110094, #256921, #100132, .T. ) ;
#124047 = AXIS2_PLACEMENT_3D ( 'NONE', #85702, #62338, #226513 ) ;
#124048 = DIRECTION ( 'NONE',  ( 0.000000000000000000, 1.000000000000000000, 0.000000000000000000 ) ) ;
#124049 = ADVANCED_FACE ( 'NONE', ( #222657, #140561 ), #44043, .T. ) ;
#124050 = CIRCLE ( 'NONE', #24109, 4.099999999999998757 ) ;
#124051 = CIRCLE ( 'NONE', #190708, 0.1000000000000002554 ) ;
#124052 = FACE_OUTER_BOUND ( 'NONE', #206788, .T. ) ;
#124053 = VECTOR ( 'NONE', #114749, 1000.000000000000000 ) ;
#124054 = CARTESIAN_POINT ( 'NONE',  ( 12.29592348164039706, 9.355806591641284697, -150.2911025315461586 ) ) ;
#124055 = ADVANCED_FACE ( 'NONE', ( #4881 ), #160110, .T. ) ;
#124056 = ORIENTED_EDGE ( 'NONE', *, *, #228179, .F. ) ;
#124057 = VECTOR ( 'NONE', #16532, 1000.000000000000000 ) ;
#124058 = LINE ( 'NONE', #224417, #147177 ) ;
#124059 = CYLINDRICAL_SURFACE ( 'NONE', #203338, 0.09999999999998898659 ) ;
#124060 = DIRECTION ( 'NONE',  ( 0.000000000000000000, -0.2128009952263603677, 0.9770955615653313941 ) ) ;
#124061 = EDGE_CURVE ( 'NONE', #75474, #88270, #193433, .T. ) ;
#124063 = EDGE_LOOP ( 'NONE', ( #160727, #64996, #141280, #61361 ) ) ;
#124062 = ADVANCED_FACE ( 'NONE', ( #45323 ), #35235, .T. ) ;
#124064 = CYLINDRICAL_SURFACE ( 'NONE', #99478, 0.5000000000000004441 ) ;
#124066 = ORIENTED_EDGE ( 'NONE', *, *, #19046, .F. ) ;
#124065 = DIRECTION ( 'NONE',  ( -1.000000000000000000, 7.304098846218134667E-16, 2.111765289898285610E-31 ) ) ;
#124068 = DIRECTION ( 'NONE',  ( 0.000000000000000000, 0.000000000000000000, 1.000000000000000000 ) ) ;
#124067 = CARTESIAN_POINT ( 'NONE',  ( 23.24999999999999645, -3.899999999988843502, -100.5000000000000426 ) ) ;
#124069 = ADVANCED_FACE ( 'NONE', ( #80569 ), #161442, .F. ) ;
#124070 = CARTESIAN_POINT ( 'NONE',  ( -23.49999999999994316, 77.75000000001119815, -47.64205752314703801 ) ) ;
#124071 = ORIENTED_EDGE ( 'NONE', *, *, #157656, .F. ) ;
#124072 = CARTESIAN_POINT ( 'NONE',  ( -18.59999999999999787, 11.74999999999999645, 11.75000000000000000 ) ) ;
#124073 = CIRCLE ( 'NONE', #19843, 0.09999999999999939493 ) ;
#124074 = DIRECTION ( 'NONE',  ( 0.000000000000000000, 0.000000000000000000, 1.000000000000000000 ) ) ;
#124075 = CARTESIAN_POINT ( 'NONE',  ( -18.50000000000000000, 9.350000000011156942, -112.8500000000000369 ) ) ;
#124076 = CARTESIAN_POINT ( 'NONE',  ( -21.64999999999999858, 29.92301283376028920, -235.3359421585013820 ) ) ;
#124078 = ADVANCED_FACE ( 'NONE', ( #81841 ), #221369, .F. ) ;
#124077 = DIRECTION ( 'NONE',  ( 0.000000000000000000, -0.5954378521545836689, -0.8034013718071036925 ) ) ;
#124079 = ORIENTED_EDGE ( 'NONE', *, *, #104340, .T. ) ;
#124080 = DIRECTION ( 'NONE',  ( 0.000000000000000000, -0.4088369013363281068, 0.9126074666063770380 ) ) ;
#124081 = CIRCLE ( 'NONE', #32527, 0.09999999999999939493 ) ;
#124082 = CARTESIAN_POINT ( 'NONE',  ( 18.59999999999999432, 54.95667902235472013, -229.8578999281555468 ) ) ;
#124083 = LINE ( 'NONE', #24992, #23944 ) ;
#124084 = PLANE ( 'NONE',  #61836 ) ;
#124085 = ORIENTED_EDGE ( 'NONE', *, *, #92462, .F. ) ;
#124086 = EDGE_CURVE ( 'NONE', #217669, #17731, #97706, .T. ) ;
#124087 = EDGE_LOOP ( 'NONE', ( #110467, #184984, #241627, #58412 ) ) ;
#124088 = CARTESIAN_POINT ( 'NONE',  ( 22.50927854361893310, 76.10085807353952703, -81.27267461055122055 ) ) ;
#124089 = EDGE_CURVE ( 'NONE', #202644, #47237, #50430, .T. ) ;
#124090 = LINE ( 'NONE', #122810, #44700 ) ;
#124091 = DIRECTION ( 'NONE',  ( 0.000000000000000000, 0.000000000000000000, -1.000000000000000000 ) ) ;
#124092 = DIRECTION ( 'NONE',  ( 1.000000000000000000, 0.000000000000000000, 0.000000000000000000 ) ) ;
#124093 = CARTESIAN_POINT ( 'NONE',  ( 22.60000000000000142, 64.25043287652299284, -170.1239658536231616 ) ) ;
#124095 = CARTESIAN_POINT ( 'NONE',  ( -21.45000000000000284, 62.99793053463489656, -222.0144804547670390 ) ) ;
#124094 = PLANE ( 'NONE',  #115971 ) ;
#124096 = AXIS2_PLACEMENT_3D ( 'NONE', #118307, #197822, #107715 ) ;
#124097 = CIRCLE ( 'NONE', #153164, 0.09999999999999939493 ) ;
#124098 = CARTESIAN_POINT ( 'NONE',  ( 18.59999999999999432, 77.26178616857691850, -94.93660852097882241 ) ) ;
#124099 = CARTESIAN_POINT ( 'NONE',  ( -23.25000000000000000, 7.882824859404637508, -245.3558965132535832 ) ) ;
#124100 = VECTOR ( 'NONE', #222482, 1000.000000000000000 ) ;
#124101 = CARTESIAN_POINT ( 'NONE',  ( -18.51991288638587463, 47.01789743104386332, -255.2023397431154592 ) ) ;
#124102 = CARTESIAN_POINT ( 'NONE',  ( -23.25000000000000000, 46.02130280899747561, -256.6489974955837852 ) ) ;
#124104 = EDGE_LOOP ( 'NONE', ( #217851, #238753, #180094, #99148, #63321 ) ) ;
#124103 = DIRECTION ( 'NONE',  ( 0.000000000000000000, 0.9126074666063770380, 0.4088369013363281068 ) ) ;
#124105 = CARTESIAN_POINT ( 'NONE',  ( 20.95576188350343116, 65.39101945504923208, -195.9118737617701242 ) ) ;
#124106 = FACE_OUTER_BOUND ( 'NONE', #23574, .T. ) ;
#124108 = DIRECTION ( 'NONE',  ( 1.000000000000000000, 3.190570557967288949E-16, 6.948722487160392945E-17 ) ) ;
#124107 = CARTESIAN_POINT ( 'NONE',  ( 22.59999999999999432, 64.25012875563544412, -103.0885370755380706 ) ) ;
#124109 =( BOUNDED_SURFACE ( )  B_SPLINE_SURFACE ( 3, 2, ( 
 ( #204495, #143242, #141961 ),
 ( #201952, #222773, #183676 ),
 ( #25891, #186240, #126246 ),
 ( #205788, #23339, #104100 ),
 ( #182395, #27195, #80689 ),
 ( #102817, #3739, #162840 ) ),
 .UNSPECIFIED., .F., .F., .F. ) 
 B_SPLINE_SURFACE_WITH_KNOTS ( ( 4, 2, 4 ),
 ( 3, 3 ),
 ( 0.0001300404313046710908, 0.0003183318589266656714, 0.0005066232865486602248 ),
 ( 0.000000000000000000, 1.000000000000000000 ),
 .UNSPECIFIED. ) 
 GEOMETRIC_REPRESENTATION_ITEM ( )  RATIONAL_B_SPLINE_SURFACE ( (
 ( 1.000000000000000000, 0.7071067811865475727, 1.000000000000000000),
 ( 1.000000000000000000, 0.7625113560545213609, 1.000000000000000000),
 ( 1.000000000000000000, 0.8126073484681893833, 1.000000000000000000),
 ( 1.000000000000000000, 0.8923049332738569595, 1.000000000000000000),
 ( 1.000000000000000000, 0.9231914937764841289, 1.000000000000000000),
 ( 1.000000000000000000, 0.9238795325112909573, 1.000000000000000000) ) ) 
 REPRESENTATION_ITEM ( '' )  SURFACE ( )  );
#124110 = EDGE_CURVE ( 'NONE', #118231, #18113, #85217, .T. ) ;
#124111 = ORIENTED_EDGE ( 'NONE', *, *, #104147, .F. ) ;
#124112 = CARTESIAN_POINT ( 'NONE',  ( -16.80621392010910498, 66.05779742250381048, -56.83351551910742927 ) ) ;
#124113 = DIRECTION ( 'NONE',  ( 0.000000000000000000, 0.000000000000000000, -1.000000000000000000 ) ) ;
#124114 = CARTESIAN_POINT ( 'NONE',  ( 23.14999999999999147, 76.00000000001267608, -203.5231074845243597 ) ) ;
#124115 = CYLINDRICAL_SURFACE ( 'NONE', #157681, 11.74999999999999645 ) ;
#124116 = LINE ( 'NONE', #182813, #220028 ) ;
#124117 = ORIENTED_EDGE ( 'NONE', *, *, #25968, .F. ) ;
#124118 = ORIENTED_EDGE ( 'NONE', *, *, #2358, .F. ) ;
#124119 = AXIS2_PLACEMENT_3D ( 'NONE', #242199, #123548, #64844 ) ;
#124121 = AXIS2_PLACEMENT_3D ( 'NONE', #98108, #119005, #318 ) ;
#124120 = CARTESIAN_POINT ( 'NONE',  ( -23.25000000000000000, 1.115600667400684642E-11, -70.90000000000000568 ) ) ;
#124122 = VERTEX_POINT ( 'NONE', #166585 ) ;
#124123 = FACE_OUTER_BOUND ( 'NONE', #132368, .T. ) ;
#124124 = VERTEX_POINT ( 'NONE', #208264 ) ;
#124125 = ADVANCED_FACE ( 'NONE', ( #111718 ), #86985, .F. ) ;
#124127 = LINE ( 'NONE', #224483, #72773 ) ;
#124126 = CIRCLE ( 'NONE', #228166, 0.1000000000000028644 ) ;
#124128 = CARTESIAN_POINT ( 'NONE',  ( 21.05000000000000071, 76.00000000001156764, -57.37310748452432563 ) ) ;
#124129 = DIRECTION ( 'NONE',  ( -0.000000000000000000, -0.4088369013363296611, 0.9126074666063764829 ) ) ;
#124130 = ORIENTED_EDGE ( 'NONE', *, *, #51860, .T. ) ;
#124131 = EDGE_CURVE ( 'NONE', #182139, #255967, #68694, .T. ) ;
#124132 = CARTESIAN_POINT ( 'NONE',  ( 21.05000000000005400, 66.15000000001120384, -6.023107484524798494 ) ) ;
#124133 = FACE_OUTER_BOUND ( 'NONE', #232944, .T. ) ;
#124134 = DIRECTION ( 'NONE',  ( -0.000000000000000000, -0.000000000000000000, 1.000000000000000000 ) ) ;
#124135 = EDGE_CURVE ( 'NONE', #73708, #38660, #10441, .T. ) ;
#124136 = CARTESIAN_POINT ( 'NONE',  ( -20.54999999999999716, 1.115600667400684642E-11, -100.5000000000000426 ) ) ;
#124137 = ADVANCED_FACE ( 'NONE', ( #90859 ), #158335, .T. ) ;
#124138 = CARTESIAN_POINT ( 'NONE',  ( -22.50000000000000000, 0.1000000000111554016, -55.35042919245524473 ) ) ;
#124139 = DIRECTION ( 'NONE',  ( 0.000000000000000000, 1.000000000000000000, 0.000000000000000000 ) ) ;
#124140 = DIRECTION ( 'NONE',  ( 0.000000000000000000, -7.147358527629766941E-15, 1.000000000000000000 ) ) ;
#124141 = AXIS2_PLACEMENT_3D ( 'NONE', #96093, #113110, #118243 ) ;
#124142 = ORIENTED_EDGE ( 'NONE', *, *, #94560, .T. ) ;
#124144 = EDGE_CURVE ( 'NONE', #154872, #1294, #189973, .T. ) ;
#124143 = DIRECTION ( 'NONE',  ( -0.000000000000000000, 0.000000000000000000, 1.000000000000000000 ) ) ;
#124146 = ORIENTED_EDGE ( 'NONE', *, *, #92994, .T. ) ;
#124145 = CIRCLE ( 'NONE', #61588, 11.80000000000000426 ) ;
#124148 = ORIENTED_EDGE ( 'NONE', *, *, #228314, .F. ) ;
#124147 = CARTESIAN_POINT ( 'NONE',  ( -16.86337532320261801, 66.02003279578751460, -90.47203195350718374 ) ) ;
#124149 = AXIS2_PLACEMENT_3D ( 'NONE', #186317, #7684, #87184 ) ;
#124150 = ORIENTED_EDGE ( 'NONE', *, *, #248751, .T. ) ;
#124151 = CARTESIAN_POINT ( 'NONE',  ( 21.05000000000000071, 71.00000000001260503, -191.1178414656112921 ) ) ;
#124152 = PLANE ( 'NONE',  #26116 ) ;
#124153 = EDGE_CURVE ( 'NONE', #239230, #44201, #151921, .T. ) ;
#124154 = CARTESIAN_POINT ( 'NONE',  ( 21.14999999999999858, 64.14229051353817113, -222.2212283990554624 ) ) ;
#124155 = ORIENTED_EDGE ( 'NONE', *, *, #40530, .F. ) ;
#124156 = CARTESIAN_POINT ( 'NONE',  ( 20.95512820512820440, 10.62384868372303615, -155.2500000000000284 ) ) ;
#124157 = CIRCLE ( 'NONE', #228386, 0.5000000000000004441 ) ;
#124158 = CARTESIAN_POINT ( 'NONE',  ( -20.94999999999999929, 76.00000000001213607, -136.5231074845243313 ) ) ;
#124159 = ORIENTED_EDGE ( 'NONE', *, *, #250545, .T. ) ;
#124160 = DIRECTION ( 'NONE',  ( 0.000000000000000000, 0.000000000000000000, -1.000000000000000000 ) ) ;
#124161 = CARTESIAN_POINT ( 'NONE',  ( -18.59999999999999787, 11.65000000001115232, -21.75000000000000355 ) ) ;
#124162 = TOROIDAL_SURFACE ( 'NONE', #132518, 12.97499999999999609, 0.1000000000000000056 ) ;
#124163 = VERTEX_POINT ( 'NONE', #29644 ) ;
#124164 = VECTOR ( 'NONE', #171490, 1000.000000000000000 ) ;
#124165 = CARTESIAN_POINT ( 'NONE',  ( -16.87333278164158656, 9.882609784590076885, -147.1331678061536365 ) ) ;
#124166 = EDGE_CURVE ( 'NONE', #76960, #221695, #239383, .T. ) ;
#124167 = ORIENTED_EDGE ( 'NONE', *, *, #174718, .F. ) ;
#124168 = CARTESIAN_POINT ( 'NONE',  ( -17.78043020864321022, 65.14640788800653581, -146.8600583188042208 ) ) ;
#124170 = VERTEX_POINT ( 'NONE', #12638 ) ;
#124169 = VECTOR ( 'NONE', #62819, 999.9999999999998863 ) ;
#124171 = CARTESIAN_POINT ( 'NONE',  ( 21.05000000000000071, 76.03753606329811987, -176.3553797584600318 ) ) ;
#124172 = EDGE_CURVE ( 'NONE', #137285, #126094, #227802, .T. ) ;
#124173 = CARTESIAN_POINT ( 'NONE',  ( -21.14999999999999858, 1.115600667400684642E-11, -127.4593430482987912 ) ) ;
#124174 = DIRECTION ( 'NONE',  ( 1.000000000000000000, 0.000000000000000000, 0.000000000000000000 ) ) ;
#124175 = ADVANCED_FACE ( 'NONE', ( #47873 ), #235269, .F. ) ;
#124176 = CARTESIAN_POINT ( 'NONE',  ( -21.93340585971934331, 7.156391548294640970, -199.4414142243538777 ) ) ;
#124177 = EDGE_CURVE ( 'NONE', #129212, #65906, #256065, .T. ) ;
#124178 = AXIS2_PLACEMENT_3D ( 'NONE', #78564, #254619, #235092 ) ;
#124179 = CARTESIAN_POINT ( 'NONE',  ( 18.39999999999999503, 5.649999999999983480, -12.65000000000000213 ) ) ;
#124180 = FACE_OUTER_BOUND ( 'NONE', #219116, .T. ) ;
#124182 = CARTESIAN_POINT ( 'NONE',  ( -23.15000000000000213, 64.25000000001227818, -157.8731074845244393 ) ) ;
#124181 = CIRCLE ( 'NONE', #123999, 0.09999999999998898659 ) ;
#124183 = ORIENTED_EDGE ( 'NONE', *, *, #194535, .F. ) ;
#124185 = CARTESIAN_POINT ( 'NONE',  ( -21.05000000000000071, 79.03091752131670944, -235.9469187808398942 ) ) ;
#124184 = DIRECTION ( 'NONE',  ( -3.890533409366484652E-14, -0.1298341882520124002, -0.9915357197604841577 ) ) ;
#124186 = AXIS2_PLACEMENT_3D ( 'NONE', #153525, #127493, #28435 ) ;
#124187 = ORIENTED_EDGE ( 'NONE', *, *, #148172, .T. ) ;
#124188 = VECTOR ( 'NONE', #162685, 1000.000000000000000 ) ;
#124189 = DIRECTION ( 'NONE',  ( 2.952720810173288126E-16, -0.9770955615653313941, -0.2128009952263603677 ) ) ;
#124190 = CARTESIAN_POINT ( 'NONE',  ( -20.54999999999999716, 2.000000000011154189, -53.77537807723790309 ) ) ;
#124192 = ORIENTED_EDGE ( 'NONE', *, *, #73227, .F. ) ;
#124191 = DIRECTION ( 'NONE',  ( 1.000000000000000000, -2.952720810173289112E-16, -2.061873921506763405E-30 ) ) ;
#124194 = ORIENTED_EDGE ( 'NONE', *, *, #1862, .F. ) ;
#124193 = CARTESIAN_POINT ( 'NONE',  ( -18.42637059832564006, 85.49694546190180233, -129.9140301747244450 ) ) ;
#124195 = CARTESIAN_POINT ( 'NONE',  ( -21.64999999999999858, 65.79629777212066699, -213.4483007241822747 ) ) ;
#124196 = CARTESIAN_POINT ( 'NONE',  ( 20.94999999999999929, 8.776282895303632259, -54.75000000000000000 ) ) ;
#124197 = CARTESIAN_POINT ( 'NONE',  ( 21.05000000000000071, 76.00000000001237765, -170.0231074845243597 ) ) ;
#124198 = LINE ( 'NONE', #203722, #18224 ) ;
#124201 = EDGE_CURVE ( 'NONE', #163039, #180993, #214422, .T. ) ;
#124200 = ORIENTED_EDGE ( 'NONE', *, *, #41213, .T. ) ;
#124199 = DIRECTION ( 'NONE',  ( 0.000000000000000000, 0.000000000000000000, -1.000000000000000000 ) ) ;
#124202 = PRODUCT_DEFINITION_SHAPE ( 'NONE', 'NONE',  #182404 ) ;
#124203 = AXIS2_PLACEMENT_3D ( 'NONE', #162058, #224568, #43380 ) ;
#124204 = AXIS2_PLACEMENT_3D ( 'NONE', #181786, #162241, #226005 ) ;
#124205 = DIRECTION ( 'NONE',  ( 0.000000000000000000, 0.000000000000000000, -1.000000000000000000 ) ) ;
#124206 = EDGE_LOOP ( 'NONE', ( #222928, #83463, #84470, #231257 ) ) ;
#124207 = EDGE_LOOP ( 'NONE', ( #254411, #225132, #161651, #149419 ) ) ;
#124208 = CARTESIAN_POINT ( 'NONE',  ( -21.65000000000000213, 51.57797924205760864, -231.8552082689889460 ) ) ;
#124209 = CARTESIAN_POINT ( 'NONE',  ( 19.87657994472041878, 34.50802439524682086, -235.0693608050739556 ) ) ;
#124210 = ORIENTED_EDGE ( 'NONE', *, *, #126003, .T. ) ;
#124211 = EDGE_CURVE ( 'NONE', #37046, #110542, #143701, .T. ) ;
#124212 = CARTESIAN_POINT ( 'NONE',  ( -16.89268316805466341, 9.951721813253341153, -180.1442475214544174 ) ) ;
#124213 = ADVANCED_FACE ( 'NONE', ( #76427 ), #33508, .T. ) ;
#124215 = ORIENTED_EDGE ( 'NONE', *, *, #21985, .T. ) ;
#124214 = AXIS2_PLACEMENT_3D ( 'NONE', #81093, #198487, #95535 ) ;
#124216 = CARTESIAN_POINT ( 'NONE',  ( 21.08376601933332495, 6.183116931858830156, -199.5881120517869078 ) ) ;
#124218 = DIRECTION ( 'NONE',  ( 3.265361837132813093E-16, 1.000000000000000000, 6.982962677686266711E-15 ) ) ;
#124217 = AXIS2_PLACEMENT_3D ( 'NONE', #186532, #223071, #86100 ) ;
#124219 = ADVANCED_FACE ( 'NONE', ( #234215 ), #39514, .F. ) ;
#124220 = ORIENTED_EDGE ( 'NONE', *, *, #197931, .T. ) ;
#124221 = EDGE_LOOP ( 'NONE', ( #186513, #96128, #75033, #41497, #52567, #118823 ) ) ;
#124223 = EDGE_CURVE ( 'NONE', #51521, #11973, #58130, .T. ) ;
#124222 = CARTESIAN_POINT ( 'NONE',  ( -21.13435531349827201, 60.96395774854146765, -234.1553755472027945 ) ) ;
#124224 = ORIENTED_EDGE ( 'NONE', *, *, #217770, .T. ) ;
#124225 = CARTESIAN_POINT ( 'NONE',  ( 18.58719872626880232, -0.7668622897694893359, -242.4347059258014383 ) ) ;
#124226 = VERTEX_POINT ( 'NONE', #137673 ) ;
#124228 = ORIENTED_EDGE ( 'NONE', *, *, #37698, .T. ) ;
#124227 = DIRECTION ( 'NONE',  ( 2.952720810173289112E-16, -1.000000000000000000, 0.000000000000000000 ) ) ;
#124229 = VECTOR ( 'NONE', #65431, 1000.000000000000000 ) ;
#124230 = DIRECTION ( 'NONE',  ( 0.000000000000000000, 6.982962677686266711E-15, -1.000000000000000000 ) ) ;
#124231 = ORIENTED_EDGE ( 'NONE', *, *, #11543, .T. ) ;
#124232 = CARTESIAN_POINT ( 'NONE',  ( -23.15000000000000213, 7.128833340094563376, -233.7327013124401276 ) ) ;
#124233 = VECTOR ( 'NONE', #43560, 1000.000000000000114 ) ;
#124234 = VECTOR ( 'NONE', #146165, 1000.000000000000114 ) ;
#124235 = ORIENTED_EDGE ( 'NONE', *, *, #57839, .F. ) ;
#124237 = ORIENTED_EDGE ( 'NONE', *, *, #19953, .T. ) ;
#124236 = ORIENTED_EDGE ( 'NONE', *, *, #209238, .F. ) ;
#124238 = CARTESIAN_POINT ( 'NONE',  ( -18.59999999999999787, 1.835341550235567887, -179.1551512925629197 ) ) ;
#124239 = CIRCLE ( 'NONE', #240933, 0.09999999999999939493 ) ;
#124240 = CARTESIAN_POINT ( 'NONE',  ( -16.91776028072577631, 14.17742018842817942, -219.2766717927335378 ) ) ;
#124241 = ORIENTED_EDGE ( 'NONE', *, *, #213724, .T. ) ;
#124242 = VECTOR ( 'NONE', #157645, 1000.000000000000000 ) ;
#124243 = EDGE_CURVE ( 'NONE', #91096, #58706, #38599, .T. ) ;
#124244 = EDGE_CURVE ( 'NONE', #160946, #14833, #235502, .T. ) ;
#124245 = ORIENTED_EDGE ( 'NONE', *, *, #235407, .F. ) ;
#124246 = CARTESIAN_POINT ( 'NONE',  ( 20.94999999999999929, 1.115600667400684642E-11, -100.5000000000000426 ) ) ;
#124247 = CARTESIAN_POINT ( 'NONE',  ( 21.05000000000005400, 76.00000000001119815, -36.02310748452479316 ) ) ;
#124249 = ORIENTED_EDGE ( 'NONE', *, *, #234340, .T. ) ;
#124248 = CARTESIAN_POINT ( 'NONE',  ( -20.94999999999999929, 67.75954444190071513, -227.8703747234148693 ) ) ;
#124250 = DIRECTION ( 'NONE',  ( -1.000000000000000000, -1.836970198721029934E-16, -3.186635328391151676E-31 ) ) ;
#124251 = ORIENTED_EDGE ( 'NONE', *, *, #138659, .F. ) ;
#124252 = CARTESIAN_POINT ( 'NONE',  ( -21.05000000000000071, 69.45934304831089889, -136.4231074845243654 ) ) ;
#124253 = CARTESIAN_POINT ( 'NONE',  ( 20.94999999999999929, 1.115600667400684642E-11, -67.00000000000000000 ) ) ;
#124254 = AXIS2_PLACEMENT_3D ( 'NONE', #36608, #95257, #128307 ) ;
#124255 = ORIENTED_EDGE ( 'NONE', *, *, #91718, .T. ) ;
#124257 = EDGE_CURVE ( 'NONE', #119302, #118551, #217211, .T. ) ;
#124256 = CARTESIAN_POINT ( 'NONE',  ( 23.14999999999999858, 3.900000000011155432, -200.9999999999999432 ) ) ;
#124258 = CARTESIAN_POINT ( 'NONE',  ( -23.15000000000000213, 1.910280373842936141, -180.1313678551989028 ) ) ;
#124259 = ORIENTED_EDGE ( 'NONE', *, *, #156547, .F. ) ;
#124260 = EDGE_CURVE ( 'NONE', #79239, #127125, #73906, .T. ) ;
#124261 = DIRECTION ( 'NONE',  ( 1.000000000000000000, 0.000000000000000000, 0.000000000000000000 ) ) ;
#124262 = ORIENTED_EDGE ( 'NONE', *, *, #148542, .F. ) ;
#124264 = EDGE_LOOP ( 'NONE', ( #181926, #164408, #167232, #20705, #174448, #230433, #187624, #202881, #203209, #126701, #251871, #97818 ) ) ;
#124263 = ORIENTED_EDGE ( 'NONE', *, *, #91808, .T. ) ;
#124265 = EDGE_LOOP ( 'NONE', ( #131896, #136362 ) ) ;
#124266 = DIRECTION ( 'NONE',  ( -1.000000000000000000, 0.000000000000000000, -0.000000000000000000 ) ) ;
#124267 = ORIENTED_EDGE ( 'NONE', *, *, #27222, .T. ) ;
#124268 = CARTESIAN_POINT ( 'NONE',  ( -16.97092634996639759, 65.99911103366341081, -48.65325025082221799 ) ) ;
#124269 = ORIENTED_EDGE ( 'NONE', *, *, #194850, .F. ) ;
#124270 = EDGE_CURVE ( 'NONE', #195862, #67969, #195133, .T. ) ;
#124271 = CARTESIAN_POINT ( 'NONE',  ( -16.89318236219975589, 66.04846474213637464, -48.66797785241853802 ) ) ;
#124272 = DIRECTION ( 'NONE',  ( 1.000000000000000000, 0.000000000000000000, -0.000000000000000000 ) ) ;
#124273 = ORIENTED_EDGE ( 'NONE', *, *, #223183, .T. ) ;
#124274 = ORIENTED_EDGE ( 'NONE', *, *, #193888, .T. ) ;
#124275 = EDGE_CURVE ( 'NONE', #200421, #204355, #35412, .T. ) ;
#124276 = AXIS2_PLACEMENT_3D ( 'NONE', #138489, #218030, #228337 ) ;
#124277 = CIRCLE ( 'NONE', #186636, 0.1000000000000124678 ) ;
#124278 = CIRCLE ( 'NONE', #165987, 12.87499999999999822 ) ;
#124279 = CIRCLE ( 'NONE', #32730, 0.09999999999999939493 ) ;
#124280 = ORIENTED_EDGE ( 'NONE', *, *, #79648, .T. ) ;
#124281 = CARTESIAN_POINT ( 'NONE',  ( 21.05000000000000071, 88.41227409416215721, -173.0231074845242745 ) ) ;
#124282 = ORIENTED_EDGE ( 'NONE', *, *, #81722, .F. ) ;
#124283 = CARTESIAN_POINT ( 'NONE',  ( -20.94999999999999929, 87.48912529308871910, -200.6231074845242688 ) ) ;
#124284 = EDGE_CURVE ( 'NONE', #148169, #42365, #72822, .T. ) ;
#124285 = CARTESIAN_POINT ( 'NONE',  ( 20.90000000000000213, -11.75000000000000178, 0.000000000000000000 ) ) ;
#124286 = DIRECTION ( 'NONE',  ( 0.000000000000000000, -1.000000000000000000, -2.891205793294679805E-16 ) ) ;
#124287 = CARTESIAN_POINT ( 'NONE',  ( 23.15000000000000213, -12.41227409413852811, -63.89999999999999858 ) ) ;
#124288 = CARTESIAN_POINT ( 'NONE',  ( -23.15000000000000213, 21.13195309841794867, -243.6318585593224100 ) ) ;
#124289 = CARTESIAN_POINT ( 'NONE',  ( -22.39999999999999858, 68.20922040163897293, -170.1231074845244109 ) ) ;
#124290 = CARTESIAN_POINT ( 'NONE',  ( -18.49499033040906681, 85.43814877175731226, -196.3249542586008829 ) ) ;
#124292 = CARTESIAN_POINT ( 'NONE',  ( 20.94999999999999929, 58.88775506787933978, -225.6504858384382999 ) ) ;
#124291 = CARTESIAN_POINT ( 'NONE',  ( -16.79363873026997922, 66.05114977059379555, -149.1769537030789650 ) ) ;
#124293 = CARTESIAN_POINT ( 'NONE',  ( -23.15000000000000213, 7.128833340093095217, -233.7327013124392749 ) ) ;
#124294 = CARTESIAN_POINT ( 'NONE',  ( -21.29999999999995808, -0.8618440306552707098, -197.0427629756619297 ) ) ;
#124295 = AXIS2_PLACEMENT_3D ( 'NONE', #95267, #52267, #233516 ) ;
#124296 = DIRECTION ( 'NONE',  ( 0.000000000000000000, 0.4558084472153119959, -0.8900778951570285091 ) ) ;
#124297 = CARTESIAN_POINT ( 'NONE',  ( 21.11747605621531321, 44.24434441712620014, -236.5336189637216933 ) ) ;
#124298 = ORIENTED_EDGE ( 'NONE', *, *, #17247, .F. ) ;
#124299 = AXIS2_PLACEMENT_3D ( 'NONE', #169224, #128788, #170529 ) ;
#124301 = ORIENTED_EDGE ( 'NONE', *, *, #88169, .F. ) ;
#124300 = CARTESIAN_POINT ( 'NONE',  ( 20.94999999999999929, -11.48912529306489994, -63.89999999999999858 ) ) ;
#124302 = ORIENTED_EDGE ( 'NONE', *, *, #205455, .F. ) ;
#124303 = CARTESIAN_POINT ( 'NONE',  ( -22.94999999999999929, 6.841561409100513025, 9.675512259591560138 ) ) ;
#124304 = DIRECTION ( 'NONE',  ( 1.000000000000000000, 0.000000000000000000, 0.000000000000000000 ) ) ;
#124305 = ORIENTED_EDGE ( 'NONE', *, *, #138285, .F. ) ;
#124306 = CARTESIAN_POINT ( 'NONE',  ( -22.59999999999999787, 11.64957080755595520, -133.9000000000000057 ) ) ;
#124307 = AXIS2_PLACEMENT_3D ( 'NONE', #245901, #72409, #30726 ) ;
#124308 = LINE ( 'NONE', #203831, #103984 ) ;
#124309 = VERTEX_POINT ( 'NONE', #34779 ) ;
#124310 = AXIS2_PLACEMENT_3D ( 'NONE', #96624, #154116, #195789 ) ;
#124311 = AXIS2_PLACEMENT_3D ( 'NONE', #8645, #230251, #51583 ) ;
#124312 = LINE ( 'NONE', #25225, #154751 ) ;
#124313 = CARTESIAN_POINT ( 'NONE',  ( 20.85000000000000142, -1.835859311443637010, -45.00443916879852679 ) ) ;
#124314 = CARTESIAN_POINT ( 'NONE',  ( 21.04999999999987637, 65.39167043205816299, -61.93142247122878530 ) ) ;
#124315 = DIRECTION ( 'NONE',  ( 0.000000000000000000, 0.9915357197604804940, -0.1298341882520397950 ) ) ;
#124317 = ORIENTED_EDGE ( 'NONE', *, *, #195618, .F. ) ;
#124316 = CARTESIAN_POINT ( 'NONE',  ( -16.97683809663752186, 66.05000000001230376, -156.6207434663279514 ) ) ;
#124318 = AXIS2_PLACEMENT_3D ( 'NONE', #6714, #107093, #244034 ) ;
#124319 = LINE ( 'NONE', #46049, #198504 ) ;
#124321 = ORIENTED_EDGE ( 'NONE', *, *, #209770, .F. ) ;
#124320 = CARTESIAN_POINT ( 'NONE',  ( -22.50000000000000000, 0.1000000000111554016, -126.2092204016266379 ) ) ;
#124322 = DIRECTION ( 'NONE',  ( 0.000000000000000000, 1.000000000000000000, 0.000000000000000000 ) ) ;
#124323 = CARTESIAN_POINT ( 'NONE',  ( -23.25000000000000355, 5.650000000011139001, -143.2500000000000284 ) ) ;
#124324 = EDGE_LOOP ( 'NONE', ( #8370, #55265 ) ) ;
#124325 = LINE ( 'NONE', #225949, #115237 ) ;
#124326 = FACE_OUTER_BOUND ( 'NONE', #216144, .T. ) ;
#124328 = DIRECTION ( 'NONE',  ( 1.000000000000000000, 0.000000000000000000, 0.000000000000000000 ) ) ;
#124327 = CARTESIAN_POINT ( 'NONE',  ( -18.50000000000000000, 76.00000000001195133, -103.0231074845243171 ) ) ;
#124330 = ADVANCED_FACE ( 'NONE', ( #157286 ), #75182, .T. ) ;
#124329 = DIRECTION ( 'NONE',  ( -1.000000000000000000, 0.000000000000000000, 0.000000000000000000 ) ) ;
#124331 = CARTESIAN_POINT ( 'NONE',  ( -21.64999999999999858, 62.98921886345645760, -213.1014462870871569 ) ) ;
#124332 = SURFACE_STYLE_USAGE ( .BOTH. , #61781 ) ;
#124333 = LINE ( 'NONE', #203855, #239304 ) ;
#124334 = VECTOR ( 'NONE', #177483, 1000.000000000000000 ) ;
#124335 = VECTOR ( 'NONE', #53772, 1000.000000000000000 ) ;
#124336 = DIRECTION ( 'NONE',  ( 0.000000000000000000, 1.000000000000000000, 2.891205793294679805E-16 ) ) ;
#124337 = CIRCLE ( 'NONE', #70379, 4.049999999999998934 ) ;
#124338 = ORIENTED_EDGE ( 'NONE', *, *, #246686, .T. ) ;
#124339 = CYLINDRICAL_SURFACE ( 'NONE', #143183, 2.000000000000001776 ) ;
#124340 = ORIENTED_EDGE ( 'NONE', *, *, #67579, .T. ) ;
#124341 = ORIENTED_EDGE ( 'NONE', *, *, #149885, .T. ) ;
#124342 = DIRECTION ( 'NONE',  ( -1.000000000000000000, 0.000000000000000000, 0.000000000000000000 ) ) ;
#124343 = ADVANCED_FACE ( 'NONE', ( #133841 ), #36044, .F. ) ;
#124344 = CARTESIAN_POINT ( 'NONE',  ( 21.30000000000002558, 1.115600667400684642E-11, -62.95000000000004547 ) ) ;
#124345 = ORIENTED_EDGE ( 'NONE', *, *, #77961, .F. ) ;
#124346 = AXIS2_PLACEMENT_3D ( 'NONE', #150084, #229603, #130485 ) ;
#124347 = EDGE_CURVE ( 'NONE', #174398, #1620, #152156, .T. ) ;
#124348 = ORIENTED_EDGE ( 'NONE', *, *, #95556, .F. ) ;
#124349 = VECTOR ( 'NONE', #82391, 1000.000000000000114 ) ;
#124350 = ORIENTED_EDGE ( 'NONE', *, *, #225856, .F. ) ;
#124351 = DIRECTION ( 'NONE',  ( -1.000000000000000000, 0.000000000000000000, 0.000000000000000000 ) ) ;
#124352 = EDGE_LOOP ( 'NONE', ( #228919, #253224, #245833, #68374 ) ) ;
#124354 = CARTESIAN_POINT ( 'NONE',  ( -23.15000000000000213, 76.00000000001267608, -203.5231074845243597 ) ) ;
#124353 = AXIS2_PLACEMENT_3D ( 'NONE', #38062, #117573, #100543 ) ;
#124355 = CARTESIAN_POINT ( 'NONE',  ( 5.900000000000060751, 64.35000000001120668, -22.12310748452479103 ) ) ;
#124356 = FACE_OUTER_BOUND ( 'NONE', #217172, .T. ) ;
#124357 = CIRCLE ( 'NONE', #149315, 0.1000000000000028644 ) ;
#124358 = AXIS2_PLACEMENT_3D ( 'NONE', #46989, #88678, #229512 ) ;
#124359 = CARTESIAN_POINT ( 'NONE',  ( -20.85000000000000142, 76.00000000001142553, -36.02310748452432421 ) ) ;
#124360 = CARTESIAN_POINT ( 'NONE',  ( -16.94107738177414291, 65.98576071487592287, -182.5731074845244279 ) ) ;
#124361 = CIRCLE ( 'NONE', #11954, 0.1000000000000055844 ) ;
#124362 = EDGE_CURVE ( 'NONE', #128423, #130315, #135311, .T. ) ;
#124363 = LINE ( 'NONE', #203880, #141638 ) ;
#124364 = ADVANCED_FACE ( 'NONE', ( #174309 ), #253773, .F. ) ;
#124365 = DIRECTION ( 'NONE',  ( -0.7071067811865301422, 0.7071067811865648922, 0.000000000000000000 ) ) ;
#124367 = ORIENTED_EDGE ( 'NONE', *, *, #111360, .F. ) ;
#124366 = DIRECTION ( 'NONE',  ( -1.000000000000000000, -0.000000000000000000, -0.000000000000000000 ) ) ;
#124369 = DIRECTION ( 'NONE',  ( 0.000000000000000000, -1.000000000000000000, -0.000000000000000000 ) ) ;
#124368 = CARTESIAN_POINT ( 'NONE',  ( -16.97048361161166952, 66.05000000001223270, -149.6642231400940091 ) ) ;
#124370 = AXIS2_PLACEMENT_3D ( 'NONE', #159390, #241485, #141104 ) ;
#124371 = CARTESIAN_POINT ( 'NONE',  ( 21.05000000000000071, 76.00000000001267608, -203.5231074845243597 ) ) ;
#124372 = ORIENTED_EDGE ( 'NONE', *, *, #40008, .F. ) ;
#124374 = EDGE_CURVE ( 'NONE', #8351, #159790, #27025, .T. ) ;
#124373 = CARTESIAN_POINT ( 'NONE',  ( -14.87779219673429409, 9.430633469083950615, -115.7317657948241560 ) ) ;
#124375 = DIRECTION ( 'NONE',  ( -0.000000000000000000, 0.2128009952263603677, -0.9770955615653313941 ) ) ;
#124376 = VERTEX_POINT ( 'NONE', #37332 ) ;
#124378 = DIRECTION ( 'NONE',  ( 0.000000000000000000, -0.1495327102803283015, -0.9887567792719397231 ) ) ;
#124377 = DIRECTION ( 'NONE',  ( 1.000000000000000000, -7.304098846218135653E-16, 0.000000000000000000 ) ) ;
#124379 = CARTESIAN_POINT ( 'NONE',  ( -16.77180007708460963, 66.05000000001182059, -82.15872160347920783 ) ) ;
#124380 = AXIS2_PLACEMENT_3D ( 'NONE', #119418, #121979, #21604 ) ;
#124382 = ORIENTED_EDGE ( 'NONE', *, *, #183233, .F. ) ;
#124381 = TOROIDAL_SURFACE ( 'NONE', #140950, 0.6000000000000004219, 0.1000000000000000056 ) ;
#124383 = FACE_OUTER_BOUND ( 'NONE', #208542, .T. ) ;
#124384 = CARTESIAN_POINT ( 'NONE',  ( 21.05000000000000071, -10.86374996222470379, -206.3339888224507206 ) ) ;
#124385 = EDGE_CURVE ( 'NONE', #216892, #156398, #16487, .T. ) ;
#124386 = DIRECTION ( 'NONE',  ( -1.000000000000000000, -0.000000000000000000, -0.000000000000000000 ) ) ;
#124387 = DIRECTION ( 'NONE',  ( -1.000000000000000000, 0.000000000000000000, 0.000000000000000000 ) ) ;
#124388 = ORIENTED_EDGE ( 'NONE', *, *, #187832, .F. ) ;
#124389 = ORIENTED_EDGE ( 'NONE', *, *, #235484, .T. ) ;
#124390 = AXIS2_PLACEMENT_3D ( 'NONE', #33297, #234015, #129783 ) ;
#124391 = VECTOR ( 'NONE', #16791, 1000.000000000000000 ) ;
#124392 = EDGE_CURVE ( 'NONE', #127698, #36453, #223632, .T. ) ;
#124393 = CARTESIAN_POINT ( 'NONE',  ( 20.85000000000000142, 77.83585931145498193, -24.41866831572578178 ) ) ;
#124394 = CARTESIAN_POINT ( 'NONE',  ( 23.14999999999999858, 79.76402609510435582, -204.5439441783492498 ) ) ;
#124395 = DIRECTION ( 'NONE',  ( 0.000000000000000000, 0.000000000000000000, 1.000000000000000000 ) ) ;
#124396 = FACE_OUTER_BOUND ( 'NONE', #122494, .T. ) ;
#124397 = VECTOR ( 'NONE', #99055, 1000.000000000000000 ) ;
#124398 = DIRECTION ( 'NONE',  ( -1.000000000000000000, 1.476360405086644309E-16, -0.000000000000000000 ) ) ;
#124399 = CARTESIAN_POINT ( 'NONE',  ( -20.94788355080264353, 65.69792220476320210, -97.53355541284612684 ) ) ;
#124400 = AXIS2_PLACEMENT_3D ( 'NONE', #251632, #232088, #113405 ) ;
#124402 = ORIENTED_EDGE ( 'NONE', *, *, #57912, .F. ) ;
#124401 = CARTESIAN_POINT ( 'NONE',  ( -23.25000000000000000, 4.150000000011156764, -54.64999999999999858 ) ) ;
#124403 = CARTESIAN_POINT ( 'NONE',  ( -21.05000000000000071, 6.257814610492678398, -33.40220970869076922 ) ) ;
#124404 = DIRECTION ( 'NONE',  ( -0.000000000000000000, 1.000000000000000000, -0.000000000000000000 ) ) ;
#124405 = DIRECTION ( 'NONE',  ( 1.000000000000000000, 0.000000000000000000, -0.000000000000000000 ) ) ;
#124406 = DIRECTION ( 'NONE',  ( 2.952720810173289112E-16, 1.000000000000000000, 6.938893903907222067E-15 ) ) ;
#124407 = DIRECTION ( 'NONE',  ( 0.000000000000000000, 0.9654727137038815465, -0.2605042016806309868 ) ) ;
#124409 = ORIENTED_EDGE ( 'NONE', *, *, #36762, .T. ) ;
#124408 = CARTESIAN_POINT ( 'NONE',  ( 23.14999999999999858, 7.128833340094563376, -233.7327013124401276 ) ) ;
#124410 = CARTESIAN_POINT ( 'NONE',  ( -20.94999999999999929, 77.16412189325330928, -128.8082593989527425 ) ) ;
#124411 = DIRECTION ( 'NONE',  ( 0.000000000000000000, 0.000000000000000000, 1.000000000000000000 ) ) ;
#124412 = AXIS2_PLACEMENT_3D ( 'NONE', #83548, #141003, #161861 ) ;
#124413 = CARTESIAN_POINT ( 'NONE',  ( -16.91049119928362998, 63.09403526110288141, -213.0970071285398433 ) ) ;
#124414 = CYLINDRICAL_SURFACE ( 'NONE', #253114, 0.1000000000000070832 ) ;
#124415 = ORIENTED_EDGE ( 'NONE', *, *, #44939, .F. ) ;
#124416 = FACE_OUTER_BOUND ( 'NONE', #167426, .T. ) ;
#124417 = CARTESIAN_POINT ( 'NONE',  ( -16.88783316861808359, 66.05000000001201954, -115.7753715265041308 ) ) ;
#124418 = AXIS2_PLACEMENT_3D ( 'NONE', #85873, #126307, #123758 ) ;
#124419 = CIRCLE ( 'NONE', #232748, 11.65000000000000036 ) ;
#124420 = DIRECTION ( 'NONE',  ( -0.000000000000000000, -0.000000000000000000, -1.000000000000000000 ) ) ;
#124421 = AXIS2_PLACEMENT_3D ( 'NONE', #236468, #173985, #134780 ) ;
#124422 = LINE ( 'NONE', #201372, #34369 ) ;
#124423 = EDGE_LOOP ( 'NONE', ( #72824, #123390, #186518, #179345 ) ) ;
#124424 = CARTESIAN_POINT ( 'NONE',  ( -16.97683810757273193, 9.950000000011137047, -87.23642328753973629 ) ) ;
#124425 = ORIENTED_EDGE ( 'NONE', *, *, #201985, .F. ) ;
#124426 = EDGE_CURVE ( 'NONE', #92976, #174229, #93636, .T. ) ;
#124427 = DIRECTION ( 'NONE',  ( -0.000000000000000000, -0.2128009952263603677, 0.9770955615653313941 ) ) ;
#124429 = EDGE_CURVE ( 'NONE', #35701, #156136, #56197, .T. ) ;
#124428 = CARTESIAN_POINT ( 'NONE',  ( -20.64999999999999858, 67.23127455305841238, -235.8551265064783991 ) ) ;
#124430 = DIRECTION ( 'NONE',  ( 4.408576920032447355E-17, 0.9594490217226103734, 0.2818822000686205254 ) ) ;
#124431 = DIRECTION ( 'NONE',  ( -0.000000000000000000, 0.000000000000000000, 1.000000000000000000 ) ) ;
#124432 = VERTEX_POINT ( 'NONE', #42442 ) ;
#124433 = EDGE_CURVE ( 'NONE', #210786, #174802, #126953, .T. ) ;
#124434 = EDGE_CURVE ( 'NONE', #11158, #149638, #240646, .T. ) ;
#124435 = DIRECTION ( 'NONE',  ( 0.000000000000000000, 0.000000000000000000, 1.000000000000000000 ) ) ;
#124436 = EDGE_CURVE ( 'NONE', #189565, #251301, #210352, .T. ) ;
#124437 = SPHERICAL_SURFACE ( 'NONE', #199559, 0.1000000000000000056 ) ;
#124438 = DIRECTION ( 'NONE',  ( 0.000000000000000000, -0.000000000000000000, -1.000000000000000000 ) ) ;
#124439 = EDGE_CURVE ( 'NONE', #213275, #23820, #104949, .T. ) ;
#124442 = ADVANCED_FACE ( 'NONE', ( #103675 ), #4587, .T. ) ;
#124441 = EDGE_CURVE ( 'NONE', #68319, #210177, #59400, .T. ) ;
#124440 = CARTESIAN_POINT ( 'NONE',  ( 21.04999999999998650, 6.650000000011155876, -112.7500000000000284 ) ) ;
#124443 = ORIENTED_EDGE ( 'NONE', *, *, #185083, .F. ) ;
#124445 = ORIENTED_EDGE ( 'NONE', *, *, #48442, .F. ) ;
#124444 = CARTESIAN_POINT ( 'NONE',  ( -20.90000000000000213, 7.900000000000000355, 1.212568896937007867 ) ) ;
#124446 = ORIENTED_EDGE ( 'NONE', *, *, #87881, .F. ) ;
#124447 = CARTESIAN_POINT ( 'NONE',  ( -18.59999999999999787, -1.164121893230052995, -175.3148480855716400 ) ) ;
#124448 = EDGE_LOOP ( 'NONE', ( #52354, #111956, #125747, #132101 ) ) ;
#124449 = DIRECTION ( 'NONE',  ( 0.000000000000000000, 0.000000000000000000, -1.000000000000000000 ) ) ;
#124450 = CYLINDRICAL_SURFACE ( 'NONE', #1347, 0.1000000000000028644 ) ;
#124451 = CARTESIAN_POINT ( 'NONE',  ( 18.79999999999999361, -11.75000000000000000, 30.09999999999999787 ) ) ;
#124452 = EDGE_LOOP ( 'NONE', ( #168239, #130326, #188423, #128175 ) ) ;
#124453 = PLANE ( 'NONE',  #82328 ) ;
#124454 = FACE_OUTER_BOUND ( 'NONE', #32191, .T. ) ;
#124455 = CARTESIAN_POINT ( 'NONE',  ( 20.97250901189795513, 10.62456803371303593, -41.16454571696699816 ) ) ;
#124456 = ORIENTED_EDGE ( 'NONE', *, *, #213571, .T. ) ;
#124457 = CARTESIAN_POINT ( 'NONE',  ( -23.25000000000000000, 64.35000000001150511, -48.27310748452440237 ) ) ;
#124458 = ADVANCED_FACE ( 'NONE', ( #718 ), #204750, .T. ) ;
#124460 = ORIENTED_EDGE ( 'NONE', *, *, #187492, .T. ) ;
#124459 = DIRECTION ( 'NONE',  ( -1.000000000000000000, 0.000000000000000000, 0.000000000000000000 ) ) ;
#124461 = FACE_OUTER_BOUND ( 'NONE', #2531, .T. ) ;
#124462 = B_SPLINE_CURVE_WITH_KNOTS ( 'NONE', 3,
 ( #172739, #95706, #215650, #34491, #91865, #211828, #94424, #76146, #55273, #235230 ),
 .UNSPECIFIED., .F., .F.,
 ( 4, 3, 3, 4 ),
 ( 1.957469226477651626E-15, 8.145022132832446376E-06, 1.905645951092409121E-05, 2.061107371225752961E-05 ),
 .UNSPECIFIED. ) ;
#124463 = CARTESIAN_POINT ( 'NONE',  ( 18.59999999999997655, 7.128833340094563376, -233.7327013124401276 ) ) ;
#124464 = VECTOR ( 'NONE', #39139, 1000.000000000000000 ) ;
#124465 = EDGE_CURVE ( 'NONE', #43292, #58399, #13523, .T. ) ;
#124466 = AXIS2_PLACEMENT_3D ( 'NONE', #167091, #67952, #134017 ) ;
#124467 = EDGE_CURVE ( 'NONE', #123641, #70529, #160308, .T. ) ;
#124468 = ORIENTED_EDGE ( 'NONE', *, *, #146894, .F. ) ;
#124469 = DIRECTION ( 'NONE',  ( 1.000000000000000000, -7.304098846218134667E-16, 4.607487905232622991E-31 ) ) ;
#124471 = ADVANCED_FACE ( 'NONE', ( #249651 ), #145389, .T. ) ;
#124470 = DIRECTION ( 'NONE',  ( 0.000000000000000000, 0.8814952561688430555, -0.4721928772777346239 ) ) ;
#124472 = VECTOR ( 'NONE', #183057, 1000.000000000000114 ) ;
#124473 = DIRECTION ( 'NONE',  ( -1.000000000000000000, 0.000000000000000000, -0.000000000000000000 ) ) ;
#124474 = ORIENTED_EDGE ( 'NONE', *, *, #169635, .F. ) ;
#124475 = DIRECTION ( 'NONE',  ( 0.000000000000000000, -0.1568667991644863147, 0.9876197685951252359 ) ) ;
#124476 = CARTESIAN_POINT ( 'NONE',  ( 21.05000000000000071, 87.48912529308842068, -167.1231074845242688 ) ) ;
#124477 = EDGE_CURVE ( 'NONE', #18466, #102678, #114483, .T. ) ;
#124478 = ORIENTED_EDGE ( 'NONE', *, *, #175901, .T. ) ;
#124479 = AXIS2_PLACEMENT_3D ( 'NONE', #132092, #211641, #236474 ) ;
#124480 = AXIS2_PLACEMENT_3D ( 'NONE', #221777, #122733, #243928 ) ;
#124481 = AXIS2_PLACEMENT_3D ( 'NONE', #48125, #208512, #46827 ) ;
#124482 = AXIS2_PLACEMENT_3D ( 'NONE', #210572, #31959, #247111 ) ;
#124483 = VERTEX_POINT ( 'NONE', #85385 ) ;
#124484 = CARTESIAN_POINT ( 'NONE',  ( 21.04116576186320486, 65.37533692126123697, -191.1945257158966740 ) ) ;
#124485 = VERTEX_POINT ( 'NONE', #187119 ) ;
#124486 = CARTESIAN_POINT ( 'NONE',  ( 21.14999999999999858, 64.35000000001173248, -81.27310748452440237 ) ) ;
#124487 = DIRECTION ( 'NONE',  ( 1.000000000000000000, -0.000000000000000000, -0.000000000000000000 ) ) ;
#124489 = ORIENTED_EDGE ( 'NONE', *, *, #96295, .T. ) ;
#124488 = CARTESIAN_POINT ( 'NONE',  ( -16.87683809663752399, 9.850000000011144508, -147.4023640181963515 ) ) ;
#124490 = CYLINDRICAL_SURFACE ( 'NONE', #253314, 0.1000000000000028644 ) ;
#124491 = CARTESIAN_POINT ( 'NONE',  ( -20.65000000000000568, 5.650000000011139001, -109.7500000000000426 ) ) ;
#124492 = CARTESIAN_POINT ( 'NONE',  ( 21.09610168723073187, 75.96641049312022176, -75.90206319974912219 ) ) ;
#124493 = DIRECTION ( 'NONE',  ( -1.000000000000000000, 0.000000000000000000, 0.000000000000000000 ) ) ;
#124494 = CARTESIAN_POINT ( 'NONE',  ( -20.64999999999999858, 74.00000000001180922, -82.74772940728641402 ) ) ;
#124495 = CARTESIAN_POINT ( 'NONE',  ( 18.59999999999999432, -3.391987963166880338, -191.5331142350599691 ) ) ;
#124497 = ORIENTED_EDGE ( 'NONE', *, *, #161626, .F. ) ;
#124496 = DIRECTION ( 'NONE',  ( -0.000000000000000000, -0.8660254037844420383, 0.4999999999999943379 ) ) ;
#124498 = DIRECTION ( 'NONE',  ( 1.734723475976817507E-14, -6.982962677686266711E-15, 1.000000000000000000 ) ) ;
#124499 = ORIENTED_EDGE ( 'NONE', *, *, #6574, .F. ) ;
#124500 = CARTESIAN_POINT ( 'NONE',  ( -23.25000000000000000, 11.65000000001115588, -122.2500000000000284 ) ) ;
#124501 = AXIS2_PLACEMENT_3D ( 'NONE', #222697, #223989, #45363 ) ;
#124502 = AXIS2_PLACEMENT_3D ( 'NONE', #88813, #168435, #69295 ) ;
#124503 = PLANE ( 'NONE',  #30139 ) ;
#124504 = CARTESIAN_POINT ( 'NONE',  ( -20.85000000000000142, 76.32388570108224712, -103.0655178952103199 ) ) ;
#124505 = AXIS2_PLACEMENT_3D ( 'NONE', #114354, #92209, #190043 ) ;
#124506 = CARTESIAN_POINT ( 'NONE',  ( 20.94999999999999574, 77.16270174995064224, -195.5231074845243313 ) ) ;
#124507 = ORIENTED_EDGE ( 'NONE', *, *, #140128, .F. ) ;
#124508 = LINE ( 'NONE', #204030, #139637 ) ;
#124509 = EDGE_CURVE ( 'NONE', #255132, #150150, #123048, .T. ) ;
#124510 = CARTESIAN_POINT ( 'NONE',  ( 20.94999999999999929, 87.48912529308779540, -72.62310748452422615 ) ) ;
#124511 = B_SPLINE_CURVE_WITH_KNOTS ( 'NONE', 3,
 ( #4363, #86445, #66917, #25245 ),
 .UNSPECIFIED., .F., .F.,
 ( 4, 4 ),
 ( 0.000000000000000000, 7.713889350930799751E-05 ),
 .UNSPECIFIED. ) ;
#124512 = TOROIDAL_SURFACE ( 'NONE', #103629, 4.149999999999999467, 0.1000000000000000056 ) ;
#124513 = CIRCLE ( 'NONE', #241047, 0.1000000000000052097 ) ;
#124514 = EDGE_CURVE ( 'NONE', #190169, #184818, #69734, .T. ) ;
#124515 = ORIENTED_EDGE ( 'NONE', *, *, #96077, .T. ) ;
#124516 = AXIS2_PLACEMENT_3D ( 'NONE', #241250, #222940, #183825 ) ;
#124517 = CARTESIAN_POINT ( 'NONE',  ( -20.85000000000000142, 7.021664781911246322, -104.3335654018973315 ) ) ;
#124518 = AXIS2_PLACEMENT_3D ( 'NONE', #151728, #233812, #69606 ) ;
#124519 = CARTESIAN_POINT ( 'NONE',  ( -18.47690164073606311, 86.88895830507721030, -199.5328223242795787 ) ) ;
#124520 = ADVANCED_FACE ( 'NONE', ( #184511 ), #206661, .T. ) ;
#124521 = ORIENTED_EDGE ( 'NONE', *, *, #135832, .F. ) ;
#124523 = EDGE_CURVE ( 'NONE', #74900, #49355, #85579, .T. ) ;
#124522 = CARTESIAN_POINT ( 'NONE',  ( -16.93589915522259304, 65.99137474131637759, -149.0825473825641154 ) ) ;
#124524 = ORIENTED_EDGE ( 'NONE', *, *, #168457, .T. ) ;
#124525 = FACE_OUTER_BOUND ( 'NONE', #201816, .T. ) ;
#124526 = VERTEX_POINT ( 'NONE', #189668 ) ;
#124527 = AXIS2_PLACEMENT_3D ( 'NONE', #129463, #87745, #12106 ) ;
#124528 = TOROIDAL_SURFACE ( 'NONE', #66270, 12.77499999999999858, 0.1000000000000000056 ) ;
#124529 = DIRECTION ( 'NONE',  ( -1.073024830501117725E-15, 0.000000000000000000, -1.000000000000000000 ) ) ;
#124530 = LINE ( 'NONE', #3265, #1433 ) ;
#124531 = EDGE_LOOP ( 'NONE', ( #196459, #237288, #158281, #163369 ) ) ;
#124532 = CARTESIAN_POINT ( 'NONE',  ( -23.25000000000000000, 11.65000000001115588, -121.8500000000000227 ) ) ;
#124533 = AXIS2_PLACEMENT_3D ( 'NONE', #131504, #186364, #91098 ) ;
#124535 = ORIENTED_EDGE ( 'NONE', *, *, #141194, .T. ) ;
#124534 =( LENGTH_UNIT ( ) NAMED_UNIT ( * ) SI_UNIT ( .MILLI., .METRE. ) );
#124536 = B_SPLINE_CURVE_WITH_KNOTS ( 'NONE', 3,
 ( #48378, #66675, #227018, #211320, #129215, #208761, #91377, #126642, #70554, #30132 ),
 .UNSPECIFIED., .F., .F.,
 ( 4, 2, 2, 2, 4 ),
 ( 0.000000000000000000, 0.0001660831991682472993, 0.0002491247987523721144, 0.0002906455985444166869, 0.0003321663983364612593 ),
 .UNSPECIFIED. ) ;
#124537 = CARTESIAN_POINT ( 'NONE',  ( 21.06086055315980232, 67.22529248505637156, -191.3207853293704090 ) ) ;
#124538 = ORIENTED_EDGE ( 'NONE', *, *, #97858, .F. ) ;
#124539 = EDGE_CURVE ( 'NONE', #88490, #116117, #10625, .T. ) ;
#124540 = CIRCLE ( 'NONE', #45421, 7.800000000000001599 ) ;
#124542 = EDGE_CURVE ( 'NONE', #74828, #64641, #185404, .T. ) ;
#124541 = AXIS2_PLACEMENT_3D ( 'NONE', #116083, #219011, #35295 ) ;
#124543 = CIRCLE ( 'NONE', #245160, 0.09999999999998898659 ) ;
#124544 = VERTEX_POINT ( 'NONE', #166284 ) ;
#124546 = CIRCLE ( 'NONE', #70417, 0.09999999999999939493 ) ;
#124545 = DIRECTION ( 'NONE',  ( 0.000000000000000000, -6.982962677686266711E-15, 1.000000000000000000 ) ) ;
#124547 = CARTESIAN_POINT ( 'NONE',  ( 22.47110162079220785, 26.01533245542389849, -254.2878056764235737 ) ) ;
#124548 = CARTESIAN_POINT ( 'NONE',  ( 21.05000000000000071, 7.128833340093095217, -233.7327013124392749 ) ) ;
#124549 = CARTESIAN_POINT ( 'NONE',  ( -20.94999999999999929, -1.835341550224411922, -11.55515129256297868 ) ) ;
#124550 = DIRECTION ( 'NONE',  ( 1.000000000000000000, 0.000000000000000000, 0.000000000000000000 ) ) ;
#124551 = ORIENTED_EDGE ( 'NONE', *, *, #238319, .F. ) ;
#124552 = DIRECTION ( 'NONE',  ( -0.000000000000000000, -1.000000000000000000, -0.000000000000000000 ) ) ;
#124554 = EDGE_CURVE ( 'NONE', #160790, #12413, #149277, .T. ) ;
#124553 = CARTESIAN_POINT ( 'NONE',  ( 22.60000000000000142, 64.25043287652329127, -203.6239658536231332 ) ) ;
#124555 = CARTESIAN_POINT ( 'NONE',  ( -18.50000000000000000, 38.29773864426885410, -236.0513742605307925 ) ) ;
#124556 = CARTESIAN_POINT ( 'NONE',  ( -23.15000000000000213, 76.00000000001253397, -181.8231074845243711 ) ) ;
#124557 = EDGE_LOOP ( 'NONE', ( #3302, #1193, #81231 ) ) ;
#124558 = ADVANCED_FACE ( 'NONE', ( #230074 ), #73011, .F. ) ;
#124559 = CARTESIAN_POINT ( 'NONE',  ( -21.11833042828134666, 75.99289949095258123, -109.4687521783795319 ) ) ;
#124560 = ORIENTED_EDGE ( 'NONE', *, *, #176371, .F. ) ;
#124562 = CIRCLE ( 'NONE', #95335, 0.1000000000000028644 ) ;
#124561 = DIRECTION ( 'NONE',  ( 1.000000000000000000, 0.000000000000000000, -0.000000000000000000 ) ) ;
#124563 = EDGE_LOOP ( 'NONE', ( #75583, #160625, #12382, #108918 ) ) ;
#124564 = CARTESIAN_POINT ( 'NONE',  ( 20.09999999999999787, 66.25000000001227818, -157.3731074845244393 ) ) ;
#124565 = CARTESIAN_POINT ( 'NONE',  ( -17.73285935862697826, 65.14201819622552136, -180.2645456747497121 ) ) ;
#124566 = ORIENTED_EDGE ( 'NONE', *, *, #254215, .T. ) ;
#124568 = ORIENTED_EDGE ( 'NONE', *, *, #73564, .T. ) ;
#124567 = CARTESIAN_POINT ( 'NONE',  ( -23.25000000000000000, 76.00000000001193712, -106.9231074845242944 ) ) ;
#124569 = CARTESIAN_POINT ( 'NONE',  ( 23.25000000000000000, 64.25000000001151079, -48.17310748452440805 ) ) ;
#124570 = EDGE_LOOP ( 'NONE', ( #102658, #194569, #163945, #209634 ) ) ;
#124571 = EDGE_CURVE ( 'NONE', #32586, #105344, #188377, .T. ) ;
#124572 = CARTESIAN_POINT ( 'NONE',  ( -22.44366136229477249, 0.009341569497225225491, -21.85028144252609295 ) ) ;
#124573 = AXIS2_PLACEMENT_3D ( 'NONE', #175712, #71478, #173174 ) ;
#124574 = CARTESIAN_POINT ( 'NONE',  ( 18.49999999999996803, 7.070967871798842452, -37.24656422186831151 ) ) ;
#124575 = EDGE_CURVE ( 'NONE', #65489, #223143, #252028, .T. ) ;
#124576 = AXIS2_PLACEMENT_3D ( 'NONE', #216527, #75752, #138257 ) ;
#124577 = VERTEX_POINT ( 'NONE', #247050 ) ;
#124578 = CYLINDRICAL_SURFACE ( 'NONE', #85250, 0.1000000000000028644 ) ;
#124579 = AXIS2_PLACEMENT_3D ( 'NONE', #132791, #32423, #49387 ) ;
#124580 = CARTESIAN_POINT ( 'NONE',  ( -20.64999999999999858, 19.73066058418984170, -238.2142830767208466 ) ) ;
#124581 = EDGE_CURVE ( 'NONE', #178529, #222295, #31498, .T. ) ;
#124582 = VERTEX_POINT ( 'NONE', #86679 ) ;
#124583 = ORIENTED_EDGE ( 'NONE', *, *, #45778, .T. ) ;
#124584 = VECTOR ( 'NONE', #134866, 1000.000000000000114 ) ;
#124585 = CARTESIAN_POINT ( 'NONE',  ( 20.94999999999999929, 1.835341550235569663, -179.0551512925629538 ) ) ;
#124586 = ADVANCED_FACE ( 'NONE', ( #228804 ), #30613, .F. ) ;
#124588 = ORIENTED_EDGE ( 'NONE', *, *, #219712, .T. ) ;
#124587 = CARTESIAN_POINT ( 'NONE',  ( -2.995603634470884209E-16, -11.74999999998884448, -58.25000000000000000 ) ) ;
#124589 = CARTESIAN_POINT ( 'NONE',  ( -18.50000000000000000, 7.120270961708746960, -171.1595630418393625 ) ) ;
#124590 = VECTOR ( 'NONE', #19204, 1000.000000000000000 ) ;
#124591 = CARTESIAN_POINT ( 'NONE',  ( -22.47120815636973745, 75.97109617810785664, -81.17303947327782510 ) ) ;
#124592 = CARTESIAN_POINT ( 'NONE',  ( -16.90202395485776776, 9.965944544561994078, -121.4030137212604501 ) ) ;
#124593 = EDGE_CURVE ( 'NONE', #150376, #6293, #14737, .T. ) ;
#124594 = AXIS2_PLACEMENT_3D ( 'NONE', #21003, #122661, #61381 ) ;
#124596 = CARTESIAN_POINT ( 'NONE',  ( -21.05000000000000071, 0.5876173420563349792, -209.1618981382189588 ) ) ;
#124595 = CARTESIAN_POINT ( 'NONE',  ( -16.93262454970420094, 65.99797953208150147, -90.45018371076169217 ) ) ;
#124597 = CARTESIAN_POINT ( 'NONE',  ( -20.94999999999999929, 65.70729864261056719, -164.5657455973725121 ) ) ;
#124598 = DIRECTION ( 'NONE',  ( 0.000000000000000000, -0.9770955615653543758, -0.2128009952262553683 ) ) ;
#124599 = DIRECTION ( 'NONE',  ( 0.000000000000000000, 0.8814952561688429444, -0.4721928772777349570 ) ) ;
#124600 = LINE ( 'NONE', #183281, #246689 ) ;
#124601 = CIRCLE ( 'NONE', #95554, 0.09999999999999990841 ) ;
#124602 = ORIENTED_EDGE ( 'NONE', *, *, #241021, .T. ) ;
#124603 = ORIENTED_EDGE ( 'NONE', *, *, #57969, .F. ) ;
#124604 = CARTESIAN_POINT ( 'NONE',  ( 21.87500000000000355, 9.749999999999998224, -12.35000000000000320 ) ) ;
#124605 = ORIENTED_EDGE ( 'NONE', *, *, #31519, .F. ) ;
#124606 = CARTESIAN_POINT ( 'NONE',  ( 22.47071067811865319, 1.115600667400684642E-11, -33.50000000000000000 ) ) ;
#124607 = EDGE_LOOP ( 'NONE', ( #18446, #195607, #109203, #37751 ) ) ;
#124608 = CARTESIAN_POINT ( 'NONE',  ( 20.94983749550516450, 65.70233904877032671, -131.0487410911968880 ) ) ;
#124609 = AXIS2_PLACEMENT_3D ( 'NONE', #4809, #126052, #123507 ) ;
#124610 = EDGE_LOOP ( 'NONE', ( #130513, #36363, #31792, #50691 ) ) ;
#124611 = CARTESIAN_POINT ( 'NONE',  ( -16.97683809663752186, 9.849999999999983658, -13.40236401819648648 ) ) ;
#124612 = ORIENTED_EDGE ( 'NONE', *, *, #18927, .T. ) ;
#124613 = ORIENTED_EDGE ( 'NONE', *, *, #168405, .T. ) ;
#124614 = DIRECTION ( 'NONE',  ( 0.000000000000000000, -1.000000000000000000, 0.000000000000000000 ) ) ;
#124615 = CARTESIAN_POINT ( 'NONE',  ( -21.08621493067320429, 75.94380516053594476, -109.3724017756962468 ) ) ;
#124617 = ORIENTED_EDGE ( 'NONE', *, *, #238975, .T. ) ;
#124616 = DIRECTION ( 'NONE',  ( 0.000000000000000000, 0.8814952561688430555, -0.4721928772777346239 ) ) ;
#124618 = CARTESIAN_POINT ( 'NONE',  ( 19.94784844284930969, 11.71308993304057999, -158.7021987172990976 ) ) ;
#124620 = ORIENTED_EDGE ( 'NONE', *, *, #206645, .F. ) ;
#124619 = CARTESIAN_POINT ( 'NONE',  ( 21.30000000000002558, 0.000000000000000000, -4.049999999999998934 ) ) ;
#124621 = CARTESIAN_POINT ( 'NONE',  ( 21.05000000000000071, -11.48912529306489994, -197.9999999999999432 ) ) ;
#124622 = VERTEX_POINT ( 'NONE', #130976 ) ;
#124623 = LINE ( 'NONE', #127191, #116619 ) ;
#124625 = ORIENTED_EDGE ( 'NONE', *, *, #213042, .F. ) ;
#124624 = CARTESIAN_POINT ( 'NONE',  ( -18.59999999999999787, 77.16412189325286874, -61.60825939895269698 ) ) ;
#124626 = DIRECTION ( 'NONE',  ( 0.000000000000000000, 0.9654727137038715545, 0.2605042016806676242 ) ) ;
#124627 = LINE ( 'NONE', #64643, #66646 ) ;
#124628 = CARTESIAN_POINT ( 'NONE',  ( -16.97048326478264002, 12.51854146005355872, -211.7227473041271253 ) ) ;
#124629 = ORIENTED_EDGE ( 'NONE', *, *, #116792, .T. ) ;
#124630 = AXIS2_PLACEMENT_3D ( 'NONE', #226395, #162610, #127323 ) ;
#124633 = CARTESIAN_POINT ( 'NONE',  ( 20.21494484322224849, 9.303170737879936425, -108.8402651917702713 ) ) ;
#124632 = AXIS2_PLACEMENT_3D ( 'NONE', #252903, #50830, #71723 ) ;
#124631 = CYLINDRICAL_SURFACE ( 'NONE', #7418, 0.1000000000000054040 ) ;
#124634 = DIRECTION ( 'NONE',  ( -0.7071067811865474617, 0.7071067811865474617, 4.937700262164531476E-15 ) ) ;
#124635 = VECTOR ( 'NONE', #82998, 1000.000000000000000 ) ;
#124636 = CIRCLE ( 'NONE', #82896, 0.1000000000000010186 ) ;
#124637 = DIRECTION ( 'NONE',  ( 0.000000000000000000, -0.000000000000000000, 1.000000000000000000 ) ) ;
#124638 = DIRECTION ( 'NONE',  ( 0.000000000000000000, 0.000000000000000000, -1.000000000000000000 ) ) ;
#124639 = DIRECTION ( 'NONE',  ( -1.000000000000000000, -0.000000000000000000, -0.000000000000000000 ) ) ;
#124640 = ORIENTED_EDGE ( 'NONE', *, *, #51891, .T. ) ;
#124641 = ORIENTED_EDGE ( 'NONE', *, *, #61932, .F. ) ;
#124642 = ORIENTED_EDGE ( 'NONE', *, *, #190262, .T. ) ;
#124643 = DIRECTION ( 'NONE',  ( -1.000000000000000000, -0.000000000000000000, -0.000000000000000000 ) ) ;
#124644 = ORIENTED_EDGE ( 'NONE', *, *, #245317, .F. ) ;
#124645 = LINE ( 'NONE', #2105, #10160 ) ;
#124646 = ORIENTED_EDGE ( 'NONE', *, *, #176347, .T. ) ;
#124647 = CARTESIAN_POINT ( 'NONE',  ( -21.46681500593313885, 6.857511159395392575, -100.5000000000000426 ) ) ;
#124648 = ADVANCED_FACE ( 'NONE', ( #31905 ), #46283, .T. ) ;
#124649 = FACE_OUTER_BOUND ( 'NONE', #139062, .T. ) ;
#124650 = EDGE_CURVE ( 'NONE', #242007, #222495, #211808, .T. ) ;
#124651 = AXIS2_PLACEMENT_3D ( 'NONE', #209560, #127455, #189998 ) ;
#124653 = EDGE_CURVE ( 'NONE', #84368, #4548, #64769, .T. ) ;
#124652 = AXIS2_PLACEMENT_3D ( 'NONE', #76879, #14380, #156468 ) ;
#124654 = EDGE_LOOP ( 'NONE', ( #63653, #84227, #242218, #2849, #206785, #193079 ) ) ;
#124655 = CIRCLE ( 'NONE', #3852, 11.74999999999999645 ) ;
#124656 = CYLINDRICAL_SURFACE ( 'NONE', #236144, 0.1000000000000000472 ) ;
#124657 = SURFACE_STYLE_FILL_AREA ( #243295 ) ;
#124658 = ORIENTED_EDGE ( 'NONE', *, *, #255489, .T. ) ;
#124659 = AXIS2_PLACEMENT_3D ( 'NONE', #74655, #122751, #180148 ) ;
#124660 = ORIENTED_EDGE ( 'NONE', *, *, #163318, .F. ) ;
#124661 = ORIENTED_EDGE ( 'NONE', *, *, #8594, .T. ) ;
#124662 = DIRECTION ( 'NONE',  ( 1.000000000000000000, 0.000000000000000000, 0.000000000000000000 ) ) ;
#124663 = PRESENTATION_STYLE_ASSIGNMENT (( #167654 ) ) ;
#124664 = LINE ( 'NONE', #67245, #180152 ) ;
#124665 = CARTESIAN_POINT ( 'NONE',  ( 18.52928932188133970, 65.72071067813085676, -145.3731074845244109 ) ) ;
#124666 = CARTESIAN_POINT ( 'NONE',  ( -20.54999999999999716, 45.00644278977874535, -237.9768835835062077 ) ) ;
#124667 = DIRECTION ( 'NONE',  ( 0.000000000000000000, -6.982962677686266711E-15, 1.000000000000000000 ) ) ;
#124668 = ADVANCED_FACE ( 'NONE', ( #78371 ), #176221, .T. ) ;
#124670 = DIRECTION ( 'NONE',  ( 0.000000000000000000, -0.000000000000000000, -1.000000000000000000 ) ) ;
#124669 = DIRECTION ( 'NONE',  ( 0.000000000000000000, 0.8814952561688429444, -0.4721928772777345684 ) ) ;
#124671 = CARTESIAN_POINT ( 'NONE',  ( -20.85000000000000142, 11.75000000001115197, -160.7161343370219129 ) ) ;
#124673 = ORIENTED_EDGE ( 'NONE', *, *, #8485, .T. ) ;
#124672 = CARTESIAN_POINT ( 'NONE',  ( -20.89192007715127986, 10.32898536001801304, -139.5826683222764757 ) ) ;
#124674 = PLANE ( 'NONE',  #213263 ) ;
#124675 = CARTESIAN_POINT ( 'NONE',  ( -18.60000000000000142, -9.321008403350113269, -141.2359382490778899 ) ) ;
#124676 = ORIENTED_EDGE ( 'NONE', *, *, #124223, .T. ) ;
#124677 = CARTESIAN_POINT ( 'NONE',  ( 21.14999999999999858, 11.40444339177024169, -198.6185779617709670 ) ) ;
#124678 = DIRECTION ( 'NONE',  ( 1.000000000000000000, 1.186688945009009831E-16, 0.000000000000000000 ) ) ;
#124679 = CARTESIAN_POINT ( 'NONE',  ( 19.97071067695833690, 64.27928932305314902, -44.84685405172082540 ) ) ;
#124680 = ORIENTED_EDGE ( 'NONE', *, *, #109815, .T. ) ;
#124681 = CARTESIAN_POINT ( 'NONE',  ( -16.90987985657661241, 30.22701669195686591, -234.8092699405564190 ) ) ;
#124682 = VECTOR ( 'NONE', #19585, 1000.000000000000000 ) ;
#124683 = CARTESIAN_POINT ( 'NONE',  ( 18.50000000000000000, 85.50000000001202238, -114.7731074845242460 ) ) ;
#124684 = CARTESIAN_POINT ( 'NONE',  ( -18.40000000000000213, 5.650000000011139001, -57.75000000000000711 ) ) ;
#124685 = ORIENTED_EDGE ( 'NONE', *, *, #65525, .F. ) ;
#124686 = ORIENTED_EDGE ( 'NONE', *, *, #59276, .T. ) ;
#124687 = FACE_OUTER_BOUND ( 'NONE', #225686, .T. ) ;
#124689 = ORIENTED_EDGE ( 'NONE', *, *, #149901, .F. ) ;
#124688 = ADVANCED_FACE ( 'NONE', ( #178809 ), #68902, .T. ) ;
#124690 = CARTESIAN_POINT ( 'NONE',  ( 21.53699400380797613, 6.787711793200763566, -66.99999999998171063 ) ) ;
#124691 = EDGE_CURVE ( 'NONE', #70872, #154309, #23106, .T. ) ;
#124693 = CARTESIAN_POINT ( 'NONE',  ( 21.05000000000000071, -9.399999999988844834, -157.6060308773475640 ) ) ;
#124692 = AXIS2_PLACEMENT_3D ( 'NONE', #10781, #249398, #91600 ) ;
#124694 = DIRECTION ( 'NONE',  ( -1.000000000000000000, 7.304098846218134667E-16, -4.217023435051678980E-16 ) ) ;
#124695 = DIRECTION ( 'NONE',  ( 0.000000000000000000, 1.000000000000000000, -0.000000000000000000 ) ) ;
#124696 = VERTEX_POINT ( 'NONE', #1393 ) ;
#124697 = DIRECTION ( 'NONE',  ( -1.000000000000000000, 0.000000000000000000, 0.000000000000000000 ) ) ;
#124698 = CARTESIAN_POINT ( 'NONE',  ( -23.15000000000000213, 76.00000000001213607, -136.5231074845243313 ) ) ;
#124699 = EDGE_CURVE ( 'NONE', #25096, #22494, #171426, .T. ) ;
#124700 = DIRECTION ( 'NONE',  ( -1.020425574104004196E-15, 6.982962677686266711E-15, -1.000000000000000000 ) ) ;
#124701 = AXIS2_PLACEMENT_3D ( 'NONE', #5671, #219598, #41006 ) ;
#124702 = AXIS2_PLACEMENT_3D ( 'NONE', #74744, #30457, #231230 ) ;
#124703 = VERTEX_POINT ( 'NONE', #80931 ) ;
#124704 = AXIS2_PLACEMENT_3D ( 'NONE', #152707, #10603, #52264 ) ;
#124706 = ORIENTED_EDGE ( 'NONE', *, *, #20206, .T. ) ;
#124705 = CARTESIAN_POINT ( 'NONE',  ( -20.94999999999999929, 10.68863688179708049, -222.5873974249508933 ) ) ;
#124707 = DIRECTION ( 'NONE',  ( 0.000000000000000000, -6.789366196018718420E-15, 1.000000000000000000 ) ) ;
#124708 = FACE_OUTER_BOUND ( 'NONE', #111727, .T. ) ;
#124709 = DIRECTION ( 'NONE',  ( -1.000000000000000000, -0.000000000000000000, -0.000000000000000000 ) ) ;
#124710 = CARTESIAN_POINT ( 'NONE',  ( 20.94999999999999929, 18.56623428888383387, -239.8594038951179073 ) ) ;
#124711 = CARTESIAN_POINT ( 'NONE',  ( 23.14999999999999858, 1.115600667400684642E-11, -200.9999999999999432 ) ) ;
#124712 = CARTESIAN_POINT ( 'NONE',  ( -23.15000000000000213, 23.68770167995059595, -252.8127582590406348 ) ) ;
#124713 = AXIS2_PLACEMENT_3D ( 'NONE', #26958, #226383, #64763 ) ;
#124714 = ORIENTED_EDGE ( 'NONE', *, *, #150107, .F. ) ;
#124715 = ADVANCED_FACE ( 'NONE', ( #72299 ), #112700, .T. ) ;
#124716 = CARTESIAN_POINT ( 'NONE',  ( 23.25000000000000000, -11.48912529306489994, -164.4000000000000057 ) ) ;
#124717 = FACE_OUTER_BOUND ( 'NONE', #4101, .T. ) ;
#124718 = CYLINDRICAL_SURFACE ( 'NONE', #46646, 1.749999999999999778 ) ;
#124719 = LINE ( 'NONE', #84241, #108962 ) ;
#124720 = DIRECTION ( 'NONE',  ( 0.000000000000000000, 0.1350103645451807555, 0.9908441862701609093 ) ) ;
#124721 = CIRCLE ( 'NONE', #132918, 0.09999999999999609201 ) ;
#124722 = CIRCLE ( 'NONE', #12312, 0.09999999999999939493 ) ;
#124724 = ORIENTED_EDGE ( 'NONE', *, *, #222046, .F. ) ;
#124723 = CIRCLE ( 'NONE', #74691, 0.1000000000000026007 ) ;
#124725 = ORIENTED_EDGE ( 'NONE', *, *, #54510, .F. ) ;
#124726 = LINE ( 'NONE', #252332, #8488 ) ;
#124727 = CIRCLE ( 'NONE', #70589, 0.1000000000000032391 ) ;
#124728 = CARTESIAN_POINT ( 'NONE',  ( 23.14999999999999503, 6.650000000011155876, -179.6499999999999773 ) ) ;
#124729 = EDGE_CURVE ( 'NONE', #162338, #213938, #93810, .T. ) ;
#124730 = CARTESIAN_POINT ( 'NONE',  ( 22.49231231312462853, 11.64998490367728223, 0.06105288760137694143 ) ) ;
#124731 = CARTESIAN_POINT ( 'NONE',  ( -16.86132326855787511, 23.02093967300761079, -230.9580288822238003 ) ) ;
#124732 = CIRCLE ( 'NONE', #12317, 0.2000000000000057288 ) ;
#124733 = CARTESIAN_POINT ( 'NONE',  ( -23.15000000000000213, 55.48145342050125350, -241.1189016111836736 ) ) ;
#124734 = ADVANCED_FACE ( 'NONE', ( #255688 ), #127132, .T. ) ;
#124735 = EDGE_CURVE ( 'NONE', #187157, #143336, #210528, .T. ) ;
#124736 = SPHERICAL_SURFACE ( 'NONE', #1063, 0.1000000000000000056 ) ;
#124737 = CARTESIAN_POINT ( 'NONE',  ( -18.39999999999999858, -7.785976468740645196, -209.8926132507865816 ) ) ;
#124738 = PRODUCT_DEFINITION_SHAPE ( 'NONE', 'NONE',  #258119 ) ;
#124739 = CYLINDRICAL_SURFACE ( 'NONE', #112193, 1.749999999999999778 ) ;
#124740 = VECTOR ( 'NONE', #117553, 1000.000000000000000 ) ;
#124741 = EDGE_CURVE ( 'NONE', #68342, #201210, #189679, .T. ) ;
#124742 = EDGE_CURVE ( 'NONE', #163227, #155361, #73192, .T. ) ;
#124743 = VERTEX_POINT ( 'NONE', #240033 ) ;
#124744 = DIRECTION ( 'NONE',  ( -2.081668171172216981E-13, -0.9742838591452925856, -0.2253241261138180518 ) ) ;
#124745 = VERTEX_POINT ( 'NONE', #256967 ) ;
#124746 = DIRECTION ( 'NONE',  ( 0.000000000000000000, -1.000000000000000000, -6.837150591533219968E-15 ) ) ;
#124747 = CARTESIAN_POINT ( 'NONE',  ( -18.59999999999999787, 70.05000000001267324, -193.2174051794895320 ) ) ;
#124749 = EDGE_CURVE ( 'NONE', #74091, #45497, #190977, .T. ) ;
#124748 = DIRECTION ( 'NONE',  ( 0.000000000000000000, 1.000000000000000000, 0.000000000000000000 ) ) ;
#124750 = DIRECTION ( 'NONE',  ( -4.801466763864313332E-15, -0.2605042016806672911, -0.9654727137038716656 ) ) ;
#124751 = DIRECTION ( 'NONE',  ( 1.000000000000000000, -0.000000000000000000, -0.000000000000000000 ) ) ;
#124752 = CARTESIAN_POINT ( 'NONE',  ( -18.43473496883415663, -9.494952410999301762, -7.045871572228188384 ) ) ;
#124753 = AXIS2_PLACEMENT_3D ( 'NONE', #182901, #158229, #122927 ) ;
#124754 = FACE_OUTER_BOUND ( 'NONE', #66230, .T. ) ;
#124755 = EDGE_CURVE ( 'NONE', #244889, #150070, #143873, .T. ) ;
#124756 = CARTESIAN_POINT ( 'NONE',  ( -20.64999999999999858, 23.45160524131172508, -253.2535058871250726 ) ) ;
#124757 = VECTOR ( 'NONE', #212010, 1000.000000000000114 ) ;
#124758 = DIRECTION ( 'NONE',  ( 0.7071067811865476838, -0.6909108974501236844, -0.1504730267678055788 ) ) ;
#124759 = CARTESIAN_POINT ( 'NONE',  ( -20.54999999999999716, -8.999999999988846255, -43.39396912265245021 ) ) ;
#124760 = EDGE_CURVE ( 'NONE', #93991, #16075, #52709, .T. ) ;
#124761 = EDGE_CURVE ( 'NONE', #33564, #14366, #56381, .T. ) ;
#124762 = DIRECTION ( 'NONE',  ( 0.000000000000000000, 0.000000000000000000, 1.000000000000000000 ) ) ;
#124763 = DIRECTION ( 'NONE',  ( 0.000000000000000000, 0.2128009952263604232, -0.9770955615653316162 ) ) ;
#124764 = CIRCLE ( 'NONE', #191436, 0.09999999999998906985 ) ;
#124765 = ORIENTED_EDGE ( 'NONE', *, *, #214154, .F. ) ;
#124766 = DIRECTION ( 'NONE',  ( 1.000000000000000000, 0.000000000000000000, 0.000000000000000000 ) ) ;
#124768 = ADVANCED_FACE ( 'NONE', ( #123943 ), #63959, .F. ) ;
#124767 = CARTESIAN_POINT ( 'NONE',  ( -21.05000000000000071, 76.00000000001179501, -81.22310748452430573 ) ) ;
#124769 = ORIENTED_EDGE ( 'NONE', *, *, #157840, .F. ) ;
#124770 = CARTESIAN_POINT ( 'NONE',  ( 18.39999999999997371, 64.52683809664901560, -45.27310748452439526 ) ) ;
#124771 = CARTESIAN_POINT ( 'NONE',  ( -23.15000000000000213, 67.23127455305835554, -235.8551265064784559 ) ) ;
#124772 = EDGE_CURVE ( 'NONE', #235613, #85481, #60479, .T. ) ;
#124773 = AXIS2_PLACEMENT_3D ( 'NONE', #18888, #98383, #93291 ) ;
#124774 = EDGE_CURVE ( 'NONE', #136435, #221590, #202153, .T. ) ;
#124775 = CARTESIAN_POINT ( 'NONE',  ( -20.85000000000000142, 10.33248238083635151, -206.5948465439131496 ) ) ;
#124776 = VECTOR ( 'NONE', #208308, 1000.000000000000000 ) ;
#124777 = ORIENTED_EDGE ( 'NONE', *, *, #18115, .F. ) ;
#124778 = CARTESIAN_POINT ( 'NONE',  ( 20.99749315643149217, 64.25000000001146816, -43.03791325328343476 ) ) ;
#124779 = FACE_OUTER_BOUND ( 'NONE', #141227, .T. ) ;
#124780 = EDGE_CURVE ( 'NONE', #232431, #247867, #182638, .T. ) ;
#124781 = ORIENTED_EDGE ( 'NONE', *, *, #251674, .T. ) ;
#124782 = CIRCLE ( 'NONE', #74918, 0.09999999999999761857 ) ;
#124783 = DIRECTION ( 'NONE',  ( -0.000000000000000000, -1.000000000000000000, 6.308085367188393199E-16 ) ) ;
#124784 = ORIENTED_EDGE ( 'NONE', *, *, #171838, .F. ) ;
#124785 = EDGE_CURVE ( 'NONE', #248274, #76140, #222984, .T. ) ;
#124786 = LINE ( 'NONE', #66083, #133551 ) ;
#124788 =( BOUNDED_CURVE ( )  B_SPLINE_CURVE ( 3, ( #152550, #153851, #252889, #166005 ),
 .UNSPECIFIED., .F., .F. ) 
 B_SPLINE_CURVE_WITH_KNOTS ( ( 4, 4 ),
 ( 3.752122642744585956, 4.712388980384673687 ),
 .UNSPECIFIED. ) 
 CURVE ( )  GEOMETRIC_REPRESENTATION_ITEM ( )  RATIONAL_B_SPLINE_CURVE ( ( 1.000000000000000000, 0.9246222802177221922, 0.9246222802177221922, 1.000000000000000000 ) ) 
 REPRESENTATION_ITEM ( '' )  );
#124787 = DIRECTION ( 'NONE',  ( 1.000000000000000000, 0.000000000000000000, 0.000000000000000000 ) ) ;
#124789 = CYLINDRICAL_SURFACE ( 'NONE', #161593, 0.5000000000000004441 ) ;
#124790 = DIRECTION ( 'NONE',  ( 0.000000000000000000, 0.000000000000000000, 1.000000000000000000 ) ) ;
#124791 = FACE_OUTER_BOUND ( 'NONE', #79914, .T. ) ;
#124792 = CARTESIAN_POINT ( 'NONE',  ( -16.92280123533687686, 66.05000000001230376, -157.1724751704392986 ) ) ;
#124793 = CARTESIAN_POINT ( 'NONE',  ( -23.25000000000000000, 71.75000000001151079, -48.37310748452435405 ) ) ;
#124794 = DIRECTION ( 'NONE',  ( -1.000000000000000000, 0.000000000000000000, 0.000000000000000000 ) ) ;
#124795 = LINE ( 'NONE', #23145, #133008 ) ;
#124797 = ORIENTED_EDGE ( 'NONE', *, *, #110199, .T. ) ;
#124796 = DIRECTION ( 'NONE',  ( -0.000000000000000000, 6.982962677686266711E-15, -1.000000000000000000 ) ) ;
#124798 = EDGE_LOOP ( 'NONE', ( #220511, #170236, #252, #247754 ) ) ;
#124801 = CARTESIAN_POINT ( 'NONE',  ( 23.15000000000000213, -11.74999999998883560, -112.6500000000000341 ) ) ;
#124800 = CARTESIAN_POINT ( 'NONE',  ( 21.05000000000000071, 1.115600667400684642E-11, -100.5000000000000284 ) ) ;
#124799 = CIRCLE ( 'NONE', #166514, 0.2000000000000003997 ) ;
#124803 = ORIENTED_EDGE ( 'NONE', *, *, #34677, .T. ) ;
#124802 = CARTESIAN_POINT ( 'NONE',  ( 20.95392731769792150, 8.883061479199918509, -109.0222279795713405 ) ) ;
#124804 = VERTEX_POINT ( 'NONE', #125218 ) ;
#124805 = PLANE ( 'NONE',  #45791 ) ;
#124806 = CARTESIAN_POINT ( 'NONE',  ( -20.64999999999999858, 71.75000000001199396, -115.3731074845243256 ) ) ;
#124807 =( BOUNDED_CURVE ( )  B_SPLINE_CURVE ( 3, ( #126519, #211187, #169541, #48259 ),
 .UNSPECIFIED., .F., .T. ) 
 B_SPLINE_CURVE_WITH_KNOTS ( ( 4, 4 ),
 ( 1.570796326794908770, 3.141592653589791784 ),
 .UNSPECIFIED. ) 
 CURVE ( )  GEOMETRIC_REPRESENTATION_ITEM ( )  RATIONAL_B_SPLINE_CURVE ( ( 1.000000000000000000, 0.8047378541243681571, 0.8047378541243681571, 1.000000000000000000 ) ) 
 REPRESENTATION_ITEM ( '' )  );
#124808 = DIRECTION ( 'NONE',  ( 0.000000000000000000, -0.2128009952263713866, 0.9770955615653290627 ) ) ;
#124809 = CARTESIAN_POINT ( 'NONE',  ( -20.94788355080264353, 10.30207779525982659, -172.9895520716782755 ) ) ;
#124810 = DIRECTION ( 'NONE',  ( 0.000000000000000000, -0.9908441862701605762, -0.1350103645451835310 ) ) ;
#124811 = CARTESIAN_POINT ( 'NONE',  ( -18.40000000000000213, 11.47316190337364183, -87.95000000000004547 ) ) ;
#124812 = DIRECTION ( 'NONE',  ( 0.000000000000000000, 0.000000000000000000, -1.000000000000000000 ) ) ;
#124813 = AXIS2_PLACEMENT_3D ( 'NONE', #12517, #15072, #153332 ) ;
#124815 = VERTEX_POINT ( 'NONE', #7848 ) ;
#124814 = ADVANCED_FACE ( 'NONE', ( #45675 ), #143486, .T. ) ;
#124816 = ORIENTED_EDGE ( 'NONE', *, *, #138957, .T. ) ;
#124817 = AXIS2_PLACEMENT_3D ( 'NONE', #249706, #182371, #3711 ) ;
#124818 = DIRECTION ( 'NONE',  ( 1.000000000000000000, 0.000000000000000000, 0.000000000000000000 ) ) ;
#124819 = AXIS2_PLACEMENT_3D ( 'NONE', #64460, #63151, #47435 ) ;
#124820 = CIRCLE ( 'NONE', #70679, 0.2000000000000005107 ) ;
#124821 = ADVANCED_FACE ( 'NONE', ( #87350 ), #65230, .T. ) ;
#124822 = ORIENTED_EDGE ( 'NONE', *, *, #228412, .F. ) ;
#124823 = DIRECTION ( 'NONE',  ( -1.000000000000000000, -0.000000000000000000, -0.000000000000000000 ) ) ;
#124824 = EDGE_LOOP ( 'NONE', ( #104730, #169562, #163304, #74323 ) ) ;
#124825 = DIRECTION ( 'NONE',  ( 0.000000000000000000, 0.000000000000000000, -1.000000000000000000 ) ) ;
#124826 =( BOUNDED_SURFACE ( )  B_SPLINE_SURFACE ( 3, 2, ( 
 ( #16954, #18228, #116056 ),
 ( #176039, #14399, #35252 ),
 ( #212586, #195600, #114757 ),
 ( #58612, #178609, #193018 ),
 ( #113464, #75651, #258068 ),
 ( #255496, #135581, #37811 ) ),
 .UNSPECIFIED., .F., .F., .F. ) 
 B_SPLINE_SURFACE_WITH_KNOTS ( ( 4, 2, 4 ),
 ( 3, 3 ),
 ( 3.141592653589793116, 3.926990816987241395, 4.712388980384689674 ),
 ( 0.000000000000000000, 1.000000000000000000 ),
 .UNSPECIFIED. ) 
 GEOMETRIC_REPRESENTATION_ITEM ( )  RATIONAL_B_SPLINE_SURFACE ( (
 ( 1.000000000000000000, 0.9238795325112820755, 1.000000000000000000),
 ( 1.000000000000000000, 0.9240297172245068857, 1.000000000000000000),
 ( 1.000000000000000000, 0.9038128468037387453, 1.000000000000000000),
 ( 1.000000000000000000, 0.8282379607651308984, 1.000000000000000000),
 ( 1.000000000000000000, 0.7727932973489990420, 1.000000000000000000),
 ( 1.000000000000000000, 0.7071067811865352493, 1.000000000000000000) ) ) 
 REPRESENTATION_ITEM ( '' )  SURFACE ( )  );
#124827 = CIRCLE ( 'NONE', #212331, 0.9000000000000014655 ) ;
#124829 = EDGE_CURVE ( 'NONE', #83182, #140569, #198044, .T. ) ;
#124828 = CARTESIAN_POINT ( 'NONE',  ( -23.15000000000000213, 16.02417409648692725, -219.3605785455116006 ) ) ;
#124830 = DIRECTION ( 'NONE',  ( 7.304098846218134667E-16, -1.000000000000000000, 0.000000000000000000 ) ) ;
#124831 = VERTEX_POINT ( 'NONE', #24861 ) ;
#124832 = CARTESIAN_POINT ( 'NONE',  ( -20.94999999999999929, 76.00000000001244871, -170.0231074845243597 ) ) ;
#124833 = ORIENTED_EDGE ( 'NONE', *, *, #200606, .T. ) ;
#124834 = CARTESIAN_POINT ( 'NONE',  ( -16.86133551771148831, 66.05000000001155058, -48.72176404997775023 ) ) ;
#124835 = AXIS2_PLACEMENT_3D ( 'NONE', #212259, #33657, #133978 ) ;
#124836 = CARTESIAN_POINT ( 'NONE',  ( -21.93340585899782980, 29.97485316283794177, -252.5455442746994947 ) ) ;
#124837 = DIRECTION ( 'NONE',  ( 0.000000000000000000, 0.000000000000000000, -1.000000000000000000 ) ) ;
#124838 = CARTESIAN_POINT ( 'NONE',  ( 18.59999999999999076, 10.49142135624846439, -58.25000000000000000 ) ) ;
#124839 = EDGE_CURVE ( 'NONE', #116420, #4251, #163081, .T. ) ;
#124840 = ORIENTED_EDGE ( 'NONE', *, *, #27834, .F. ) ;
#124841 = CARTESIAN_POINT ( 'NONE',  ( -21.03571358705830718, 64.25000000001189449, -96.19800066246598647 ) ) ;
#124842 = ORIENTED_EDGE ( 'NONE', *, *, #98314, .F. ) ;
#124845 = VERTEX_POINT ( 'NONE', #200896 ) ;
#124844 = DIRECTION ( 'NONE',  ( 0.000000000000000000, 0.000000000000000000, -1.000000000000000000 ) ) ;
#124843 = DIRECTION ( 'NONE',  ( -3.265361837132813093E-16, -1.000000000000000000, -6.982962677686266711E-15 ) ) ;
#124846 = CARTESIAN_POINT ( 'NONE',  ( -18.40000000000000213, 5.649999999999983480, -12.65000000000000213 ) ) ;
#124847 = ORIENTED_EDGE ( 'NONE', *, *, #83515, .F. ) ;
#124848 = DIRECTION ( 'NONE',  ( -0.000000000000000000, 1.000000000000000000, -0.000000000000000000 ) ) ;
#124849 = ORIENTED_EDGE ( 'NONE', *, *, #84945, .T. ) ;
#124850 = CARTESIAN_POINT ( 'NONE',  ( 21.46681500598269565, 76.00000000001219291, -143.3806186439480825 ) ) ;
#124851 = DIRECTION ( 'NONE',  ( 1.186688945009010077E-16, 1.000000000000000000, 6.982962677686266711E-15 ) ) ;
#124852 = DIRECTION ( 'NONE',  ( -1.000000000000000000, 0.000000000000000000, -0.000000000000000000 ) ) ;
#124853 = CARTESIAN_POINT ( 'NONE',  ( -20.54999999999999716, 26.18196512540240661, -241.1028522842020152 ) ) ;
#124854 = FACE_OUTER_BOUND ( 'NONE', #233818, .T. ) ;
#124855 = ORIENTED_EDGE ( 'NONE', *, *, #52182, .T. ) ;
#124856 = DIRECTION ( 'NONE',  ( 1.000000000000000000, 0.000000000000000000, 0.000000000000000000 ) ) ;
#124857 = CARTESIAN_POINT ( 'NONE',  ( -18.39999999999999503, -9.682403433465244902, -140.6568433774128266 ) ) ;
#124858 = AXIS2_PLACEMENT_3D ( 'NONE', #97479, #195358, #158801 ) ;
#124859 = ORIENTED_EDGE ( 'NONE', *, *, #252808, .T. ) ;
#124860 = EDGE_CURVE ( 'NONE', #203210, #133719, #142205, .T. ) ;
#124861 = DIRECTION ( 'NONE',  ( 1.000000000000000000, 0.000000000000000000, -0.000000000000000000 ) ) ;
#124862 = ORIENTED_EDGE ( 'NONE', *, *, #96205, .F. ) ;
#124863 = DIRECTION ( 'NONE',  ( 1.000000000000000000, 0.000000000000000000, 0.000000000000000000 ) ) ;
#124864 = CARTESIAN_POINT ( 'NONE',  ( -20.54999999999999716, 6.268811756569107274, -220.3853799378769622 ) ) ;
#124865 = AXIS2_PLACEMENT_3D ( 'NONE', #113431, #153895, #98965 ) ;
#124867 = ORIENTED_EDGE ( 'NONE', *, *, #177007, .T. ) ;
#124866 = CARTESIAN_POINT ( 'NONE',  ( 20.94999999999999929, 48.98768910550767686, -253.5949463715719787 ) ) ;
#124868 = DIRECTION ( 'NONE',  ( 1.000000000000000000, 0.000000000000000000, 0.000000000000000000 ) ) ;
#124869 = AXIS2_PLACEMENT_3D ( 'NONE', #40164, #200493, #180933 ) ;
#124870 = ADVANCED_FACE ( 'NONE', ( #5233 ), #206428, .T. ) ;
#124871 = CARTESIAN_POINT ( 'NONE',  ( -14.45422546970484312, 62.93791375105570296, -215.5805554555300318 ) ) ;
#124872 = PLANE ( 'NONE',  #239365 ) ;
#124873 = ADVANCED_FACE ( 'NONE', ( #224308 ), #204732, .F. ) ;
#124874 = ORIENTED_EDGE ( 'NONE', *, *, #37636, .F. ) ;
#124875 = FACE_OUTER_BOUND ( 'NONE', #250899, .T. ) ;
#124876 = CARTESIAN_POINT ( 'NONE',  ( -20.94999999999999929, 76.00000000001126921, -203.5231074845248997 ) ) ;
#124877 = ORIENTED_EDGE ( 'NONE', *, *, #236007, .F. ) ;
#124878 = FACE_OUTER_BOUND ( 'NONE', #176989, .T. ) ;
#124879 = CIRCLE ( 'NONE', #103995, 0.09999999999999939493 ) ;
#124880 = VECTOR ( 'NONE', #77942, 1000.000000000000000 ) ;
#124881 = EDGE_LOOP ( 'NONE', ( #223815, #213155, #64269, #253846 ) ) ;
#124882 = EDGE_CURVE ( 'NONE', #131461, #187418, #106628, .T. ) ;
#124883 = CYLINDRICAL_SURFACE ( 'NONE', #233473, 0.1000000000000038219 ) ;
#124885 = ORIENTED_EDGE ( 'NONE', *, *, #114380, .F. ) ;
#124884 = CARTESIAN_POINT ( 'NONE',  ( -18.59999999999999787, 6.982009704856444898, -37.19615211825629331 ) ) ;
#124886 = AXIS2_PLACEMENT_3D ( 'NONE', #250720, #128222, #207776 ) ;
#124887 = EDGE_CURVE ( 'NONE', #4792, #95398, #221717, .T. ) ;
#124888 = AXIS2_PLACEMENT_3D ( 'NONE', #237890, #131409, #59211 ) ;
#124889 = EDGE_CURVE ( 'NONE', #202387, #212703, #106438, .T. ) ;
#124890 = VECTOR ( 'NONE', #57398, 1000.000000000000000 ) ;
#124891 = B_SPLINE_CURVE_WITH_KNOTS ( 'NONE', 3,
 ( #236058, #238634, #20898, #182531, #178693, #3870, #239928, #221608, #78257, #22172 ),
 .UNSPECIFIED., .F., .F.,
 ( 4, 3, 3, 4 ),
 ( 0.000000000000000000, 1.004626015991471073E-05, 1.831183478184062558E-05, 2.062343583996205056E-05 ),
 .UNSPECIFIED. ) ;
#124894 = ORIENTED_EDGE ( 'NONE', *, *, #206377, .F. ) ;
#124893 = ORIENTED_EDGE ( 'NONE', *, *, #236451, .F. ) ;
#124892 = CARTESIAN_POINT ( 'NONE',  ( -2.995603634470884209E-16, 6.649999999999999467, -21.25000000000000000 ) ) ;
#124895 = CARTESIAN_POINT ( 'NONE',  ( 23.15000000000000213, 84.66355140188177586, -193.9990063664569959 ) ) ;
#124896 = LINE ( 'NONE', #126152, #106486 ) ;
#124897 = CARTESIAN_POINT ( 'NONE',  ( -21.65000000000000213, 7.708578643773852157, -179.8499999999999943 ) ) ;
#124898 = EDGE_CURVE ( 'NONE', #2024, #150106, #206037, .T. ) ;
#124900 = CARTESIAN_POINT ( 'NONE',  ( -12.26136940704872202, 66.64859682586988754, -52.54357704768590054 ) ) ;
#124899 = DIRECTION ( 'NONE',  ( 1.000000000000000000, 0.000000000000000000, 0.000000000000000000 ) ) ;
#124901 = DIRECTION ( 'NONE',  ( 1.000000000000000000, 0.000000000000000000, 0.000000000000000000 ) ) ;
#124902 = CARTESIAN_POINT ( 'NONE',  ( -22.57848426163146627, 25.93747689298670878, -254.3589117886994586 ) ) ;
#124903 = CIRCLE ( 'NONE', #129011, 0.4999999999999944489 ) ;
#124904 = DIRECTION ( 'NONE',  ( 0.000000000000000000, 0.000000000000000000, -1.000000000000000000 ) ) ;
#124905 = DIRECTION ( 'NONE',  ( 1.000000000000000000, 0.000000000000000000, 0.000000000000000000 ) ) ;
#124906 = AXIS2_PLACEMENT_3D ( 'NONE', #251770, #87860, #193095 ) ;
#124907 = AXIS2_PLACEMENT_3D ( 'NONE', #168645, #129468, #208998 ) ;
#124908 = VERTEX_POINT ( 'NONE', #246446 ) ;
#124909 = AXIS2_PLACEMENT_3D ( 'NONE', #218567, #75257, #233044 ) ;
#124911 = VERTEX_POINT ( 'NONE', #202184 ) ;
#124910 = AXIS2_PLACEMENT_3D ( 'NONE', #144327, #107795, #222585 ) ;
#124912 = DIRECTION ( 'NONE',  ( -2.915501640297152804E-16, -1.000000000000000000, -6.997203936713167125E-15 ) ) ;
#124914 = ORIENTED_EDGE ( 'NONE', *, *, #5285, .F. ) ;
#124913 = CARTESIAN_POINT ( 'NONE',  ( -21.14999999999994174, 87.50449464844290048, -34.18759587077607165 ) ) ;
#124915 = ORIENTED_EDGE ( 'NONE', *, *, #100764, .F. ) ;
#124916 = EDGE_CURVE ( 'NONE', #45147, #21871, #109485, .T. ) ;
#124917 = CARTESIAN_POINT ( 'NONE',  ( -22.47071067811865319, 7.720074744498060859, 0.09909245470260481803 ) ) ;
#124918 = ORIENTED_EDGE ( 'NONE', *, *, #101034, .T. ) ;
#124919 = DIRECTION ( 'NONE',  ( 0.000000000000000000, 0.000000000000000000, 1.000000000000000000 ) ) ;
#124920 = ORIENTED_EDGE ( 'NONE', *, *, #89228, .T. ) ;
#124921 = FACE_OUTER_BOUND ( 'NONE', #152106, .T. ) ;
#124922 = DIRECTION ( 'NONE',  ( -0.000000000000000000, -0.000000000000000000, 1.000000000000000000 ) ) ;
#124924 = ORIENTED_EDGE ( 'NONE', *, *, #68496, .T. ) ;
#124923 = EDGE_LOOP ( 'NONE', ( #144723, #62239, #229446, #86562 ) ) ;
#124925 = ORIENTED_EDGE ( 'NONE', *, *, #2809, .T. ) ;
#124926 = FACE_OUTER_BOUND ( 'NONE', #10091, .T. ) ;
#124927 = ORIENTED_EDGE ( 'NONE', *, *, #180986, .T. ) ;
#124928 = ORIENTED_EDGE ( 'NONE', *, *, #39455, .T. ) ;
#124929 = DIRECTION ( 'NONE',  ( -1.000000000000000000, -8.674042436075348305E-17, -1.619280515896124405E-16 ) ) ;
#124930 = CARTESIAN_POINT ( 'NONE',  ( 18.52351027002947959, -9.642162904684028035, -73.71504695050977318 ) ) ;
#124932 = VERTEX_POINT ( 'NONE', #131628 ) ;
#124931 = CARTESIAN_POINT ( 'NONE',  ( 18.39999999999999503, 70.35000000001153353, -48.67310748452436542 ) ) ;
#124933 = LINE ( 'NONE', #204446, #236408 ) ;
#124934 = DIRECTION ( 'NONE',  ( 0.000000000000000000, 0.2617529984165071766, 0.9651348961777145297 ) ) ;
#124936 = ORIENTED_EDGE ( 'NONE', *, *, #243758, .F. ) ;
#124935 = PLANE ( 'NONE',  #122421 ) ;
#124937 = CARTESIAN_POINT ( 'NONE',  ( -17.73285935862606877, 10.85798180379781819, -177.7414381902257787 ) ) ;
#124938 = ORIENTED_EDGE ( 'NONE', *, *, #12161, .F. ) ;
#124939 = CARTESIAN_POINT ( 'NONE',  ( -20.64999999999999858, 76.00000000001237765, -170.0231074845243597 ) ) ;
#124940 = AXIS2_PLACEMENT_3D ( 'NONE', #57780, #236432, #137321 ) ;
#124941 = ORIENTED_EDGE ( 'NONE', *, *, #50060, .T. ) ;
#124942 = DIRECTION ( 'NONE',  ( 1.000000000000000000, 0.000000000000000000, 0.000000000000000000 ) ) ;
#124943 = DIRECTION ( 'NONE',  ( 0.000000000000000000, 0.2617529984165032908, 0.9651348961777156399 ) ) ;
#124944 = VECTOR ( 'NONE', #189015, 1000.000000000000000 ) ;
#124945 = VERTEX_POINT ( 'NONE', #52075 ) ;
#124947 = LINE ( 'NONE', #244877, #45629 ) ;
#124946 = CARTESIAN_POINT ( 'NONE',  ( 21.13461538461538680, 10.61458296203669427, -45.85000000000000142 ) ) ;
#124948 = CIRCLE ( 'NONE', #45830, 0.1000000000000028644 ) ;
#124949 = EDGE_CURVE ( 'NONE', #147021, #186245, #181503, .T. ) ;
#124950 = DIRECTION ( 'NONE',  ( 1.000000000000000000, 0.000000000000000000, 0.000000000000000000 ) ) ;
#124951 = CARTESIAN_POINT ( 'NONE',  ( -21.64999999999999858, 68.75000000001260503, -191.2731074845244166 ) ) ;
#124952 = ORIENTED_EDGE ( 'NONE', *, *, #213233, .F. ) ;
#124953 = ORIENTED_EDGE ( 'NONE', *, *, #67323, .F. ) ;
#124954 = DIRECTION ( 'NONE',  ( 0.000000000000000000, 0.2617529984165152257, 0.9651348961777124202 ) ) ;
#124955 = FACE_OUTER_BOUND ( 'NONE', #230078, .T. ) ;
#124956 = ORIENTED_EDGE ( 'NONE', *, *, #104343, .T. ) ;
#124957 = CARTESIAN_POINT ( 'NONE',  ( 21.14999999999999503, 76.10000000001174669, -81.17267829206912211 ) ) ;
#124958 = ORIENTED_EDGE ( 'NONE', *, *, #151567, .F. ) ;
#124959 = DIRECTION ( 'NONE',  ( 0.000000000000000000, 0.000000000000000000, 1.000000000000000000 ) ) ;
#124960 = EDGE_CURVE ( 'NONE', #52160, #171102, #173167, .T. ) ;
#124961 = DIRECTION ( 'NONE',  ( 0.000000000000000000, 0.000000000000000000, 1.000000000000000000 ) ) ;
#124962 = CIRCLE ( 'NONE', #108207, 0.1999999999999987899 ) ;
#124963 = DIRECTION ( 'NONE',  ( -4.801466763864314121E-15, 0.2605042016806606298, 0.9654727137038736640 ) ) ;
#124964 = DIRECTION ( 'NONE',  ( 3.469446951953635015E-14, -0.000000000000000000, 1.000000000000000000 ) ) ;
#124965 = CIRCLE ( 'NONE', #191451, 0.1000000000000028644 ) ;
#124966 = EDGE_CURVE ( 'NONE', #46891, #168999, #98235, .T. ) ;
#124967 = ADVANCED_FACE ( 'NONE', ( #49532 ), #177426, .T. ) ;
#124968 = EDGE_LOOP ( 'NONE', ( #121113, #242352, #220974, #179703 ) ) ;
#124969 = DIRECTION ( 'NONE',  ( -0.000000000000000000, 0.9126074666063771490, 0.4088369013363281623 ) ) ;
#124970 = AXIS2_PLACEMENT_3D ( 'NONE', #22657, #1767, #222082 ) ;
#124971 = ORIENTED_EDGE ( 'NONE', *, *, #194413, .T. ) ;
#124972 = ORIENTED_EDGE ( 'NONE', *, *, #228667, .F. ) ;
#124973 = EDGE_LOOP ( 'NONE', ( #72003, #175271, #165259, #132296 ) ) ;
#124974 = DIRECTION ( 'NONE',  ( 0.000000000000000000, -0.1335171055202867274, 0.9910465087640866200 ) ) ;
#124975 = CARTESIAN_POINT ( 'NONE',  ( -23.25000000000000000, 87.65000000001144542, -39.02310748452423894 ) ) ;
#124976 = DIRECTION ( 'NONE',  ( -1.000000000000000000, -0.000000000000000000, -0.000000000000000000 ) ) ;
#124977 = DIRECTION ( 'NONE',  ( -1.000000000000000000, -0.000000000000000000, -0.000000000000000000 ) ) ;
#124978 = DIRECTION ( 'NONE',  ( 1.000000000000000000, -0.000000000000000000, 0.000000000000000000 ) ) ;
#124979 = ADVANCED_FACE ( 'NONE', ( #110779 ), #73373, .F. ) ;
#124981 = CYLINDRICAL_SURFACE ( 'NONE', #136575, 0.09999999999998898659 ) ;
#124980 = DIRECTION ( 'NONE',  ( 1.000000000000000000, -0.000000000000000000, 0.000000000000000000 ) ) ;
#124983 = ORIENTED_EDGE ( 'NONE', *, *, #176169, .F. ) ;
#124982 = DIRECTION ( 'NONE',  ( 1.000000000000000000, 0.000000000000000000, 0.000000000000000000 ) ) ;
#124984 = DIRECTION ( 'NONE',  ( 1.000000000000000000, 0.000000000000000000, 0.000000000000000000 ) ) ;
#124985 = VERTEX_POINT ( 'NONE', #172083 ) ;
#124986 = ADVANCED_FACE ( 'NONE', ( #226875 ), #89923, .T. ) ;
#124987 = LINE ( 'NONE', #127546, #196740 ) ;
#124988 = EDGE_LOOP ( 'NONE', ( #237045, #196193, #240011, #93673, #70894 ) ) ;
#124989 = ORIENTED_EDGE ( 'NONE', *, *, #25505, .T. ) ;
#124990 = DIRECTION ( 'NONE',  ( 0.000000000000000000, 0.000000000000000000, -1.000000000000000000 ) ) ;
#124991 = CARTESIAN_POINT ( 'NONE',  ( -20.64999999999999858, 1.115600667400684642E-11, -167.5000000000000284 ) ) ;
#124992 = CARTESIAN_POINT ( 'NONE',  ( -16.89935556175728593, 66.05000000001153637, -49.16278384740906660 ) ) ;
#124993 = DIRECTION ( 'NONE',  ( -0.000000000000000000, 1.000000000000000000, 2.891205793294679805E-16 ) ) ;
#124994 = PRODUCT_RELATED_PRODUCT_CATEGORY ( 'part', '', ( #126320 ) ) ;
#124995 = VECTOR ( 'NONE', #252554, 1000.000000000000000 ) ;
#124996 = AXIS2_PLACEMENT_3D ( 'NONE', #35680, #209138, #30534 ) ;
#124997 = DIRECTION ( 'NONE',  ( -0.000000000000000000, 6.982962677686266711E-15, -1.000000000000000000 ) ) ;
#124998 = EDGE_LOOP ( 'NONE', ( #223606, #170532, #35725, #28750 ) ) ;
#124999 = ORIENTED_EDGE ( 'NONE', *, *, #41414, .F. ) ;
#125000 = EDGE_CURVE ( 'NONE', #200735, #146785, #48240, .T. ) ;
#125001 = DIRECTION ( 'NONE',  ( 0.000000000000000000, 0.1350103645451904977, 0.9908441862701596881 ) ) ;
#125003 = ORIENTED_EDGE ( 'NONE', *, *, #200030, .T. ) ;
#125002 = EDGE_CURVE ( 'NONE', #200872, #121232, #29996, .T. ) ;
#125004 = DIRECTION ( 'NONE',  ( 0.000000000000000000, 0.9126074666063772600, 0.4088369013363274407 ) ) ;
#125005 = CYLINDRICAL_SURFACE ( 'NONE', #240089, 0.09999999999999939493 ) ;
#125006 = ADVANCED_FACE ( 'NONE', ( #72978 ), #232037, .F. ) ;
#125007 = DIRECTION ( 'NONE',  ( 0.000000000000000000, -0.1350103645451945777, 0.9908441862701590219 ) ) ;
#125008 = FACE_OUTER_BOUND ( 'NONE', #257275, .T. ) ;
#125009 = CARTESIAN_POINT ( 'NONE',  ( -17.05016517656072139, 66.05000000001207638, -123.8504094885256706 ) ) ;
#125010 = DIRECTION ( 'NONE',  ( -1.000000000000000000, 0.000000000000000000, -0.000000000000000000 ) ) ;
#125011 = EDGE_LOOP ( 'NONE', ( #138427, #19253, #237565 ) ) ;
#125012 = CARTESIAN_POINT ( 'NONE',  ( 20.04142135623730070, 64.35000000001222986, -148.6731074845244507 ) ) ;
#125013 = DIRECTION ( 'NONE',  ( -0.000000000000000000, -0.1290532225515364506, -0.9916376685811525427 ) ) ;
#125014 = CARTESIAN_POINT ( 'NONE',  ( 20.94999999999999929, -9.000000000000000000, -24.10603087734755690 ) ) ;
#125015 = CARTESIAN_POINT ( 'NONE',  ( 18.49999999999999289, 65.75000000001250555, -178.8731074845244109 ) ) ;
#125016 = AXIS2_PLACEMENT_3D ( 'NONE', #76020, #17344, #214257 ) ;
#125017 = AXIS2_PLACEMENT_3D ( 'NONE', #183021, #102147, #200007 ) ;
#125018 = CYLINDRICAL_SURFACE ( 'NONE', #70694, 0.09999999999999939493 ) ;
#125019 = AXIS2_PLACEMENT_3D ( 'NONE', #96053, #219858, #41262 ) ;
#125020 = CARTESIAN_POINT ( 'NONE',  ( -20.85000000000000142, 68.97833521811159585, -65.88954208262707368 ) ) ;
#125021 = ORIENTED_EDGE ( 'NONE', *, *, #241375, .T. ) ;
#125022 = CIRCLE ( 'NONE', #104141, 11.70000000000000284 ) ;
#125023 = CARTESIAN_POINT ( 'NONE',  ( 23.14999999999999858, 1.115600667400684642E-11, -69.00000000000000000 ) ) ;
#125024 = VERTEX_POINT ( 'NONE', #187771 ) ;
#125025 = CARTESIAN_POINT ( 'NONE',  ( 23.24999999999999645, 1.115600667400684642E-11, -67.00000000000004263 ) ) ;
#125026 = CARTESIAN_POINT ( 'NONE',  ( 20.85000000000000142, 68.92903212821303782, -99.27654326265604823 ) ) ;
#125027 = DIRECTION ( 'NONE',  ( -1.000000000000000000, 0.000000000000000000, -0.000000000000000000 ) ) ;
#125028 = AXIS2_PLACEMENT_3D ( 'NONE', #157439, #236934, #58279 ) ;
#125029 = ORIENTED_EDGE ( 'NONE', *, *, #176001, .T. ) ;
#125030 = EDGE_CURVE ( 'NONE', #128716, #252010, #64950, .T. ) ;
#125032 = AXIS2_PLACEMENT_3D ( 'NONE', #113069, #217272, #197728 ) ;
#125031 = DIRECTION ( 'NONE',  ( 1.000000000000000000, 0.000000000000000000, 0.000000000000000000 ) ) ;
#125033 = CARTESIAN_POINT ( 'NONE',  ( -18.79999999999999716, 1.350000000000000089, 16.50000000000000000 ) ) ;
#125034 = CARTESIAN_POINT ( 'NONE',  ( -18.39999999999999858, -9.599999999988849453, -207.6001893912220169 ) ) ;
#125035 = CARTESIAN_POINT ( 'NONE',  ( 20.94999999999999929, 85.50000000001197975, -112.9170766071766820 ) ) ;
#125036 = B_SPLINE_CURVE_WITH_KNOTS ( 'NONE', 3,
 ( #189499, #30434, #10862, #173832, #171265, #232493, #92951, #150380, #51233, #72130, #130794, #210349, #212910, #31738, #111240, #34300, #252025, #190811, #12165 ),
 .UNSPECIFIED., .F., .F.,
 ( 4, 3, 3, 3, 3, 3, 4 ),
 ( 1.387778780781445521E-17, 2.646747978909188838E-05, 5.271166642128437155E-05, 9.008788829884586393E-05, 0.0001426648776560943404, 0.0001897378458659839079, 0.0001917382627806266040 ),
 .UNSPECIFIED. ) ;
#125037 = DIRECTION ( 'NONE',  ( 2.952720810173289112E-16, 0.4088369013363388205, -0.9126074666063722640 ) ) ;
#125038 = CARTESIAN_POINT ( 'NONE',  ( -23.25000000000000000, 66.23941198528750363, -222.8935984851895853 ) ) ;
#125039 = EDGE_LOOP ( 'NONE', ( #67843, #72864, #56217, #231999, #214652 ) ) ;
#125040 = DIRECTION ( 'NONE',  ( 1.000000000000000000, -0.000000000000000000, -0.000000000000000000 ) ) ;
#125042 = ORIENTED_EDGE ( 'NONE', *, *, #118864, .T. ) ;
#125041 = DIRECTION ( 'NONE',  ( 0.000000000000000000, 0.2617529984165030132, 0.9651348961777158619 ) ) ;
#125043 = CARTESIAN_POINT ( 'NONE',  ( 22.45380639572245940, 1.426796696685579650E-07, -122.2495671088909006 ) ) ;
#125044 = EDGE_CURVE ( 'NONE', #252329, #198528, #134476, .T. ) ;
#125045 = DIRECTION ( 'NONE',  ( -1.000000000000000000, -0.000000000000000000, -0.000000000000000000 ) ) ;
#125046 = ORIENTED_EDGE ( 'NONE', *, *, #199981, .F. ) ;
#125047 = DIRECTION ( 'NONE',  ( -1.000000000000000000, 0.000000000000000000, 0.000000000000000000 ) ) ;
#125048 = ADVANCED_FACE ( 'NONE', ( #243420 ), #204284, .T. ) ;
#125049 = APPLICATION_PROTOCOL_DEFINITION ( 'draft international standard', 'automotive_design', 1998, #180708 ) ;
#125050 = CARTESIAN_POINT ( 'NONE',  ( 21.05000000000000071, -0.09999999998884338825, -127.4593430482987912 ) ) ;
#125051 = EDGE_LOOP ( 'NONE', ( #234597, #128239, #115697, #54339 ) ) ;
#125053 = EDGE_CURVE ( 'NONE', #250411, #120222, #218530, .T. ) ;
#125052 = DIRECTION ( 'NONE',  ( -1.652117596168391700E-15, -1.000000000000000000, 0.000000000000000000 ) ) ;
#125054 = CIRCLE ( 'NONE', #204315, 0.09999999999999982514 ) ;
#125055 = ADVANCED_FACE ( 'NONE', ( #206867 ), #166488, .F. ) ;
#125056 = EDGE_CURVE ( 'NONE', #200161, #132241, #103889, .T. ) ;
#125057 = DIRECTION ( 'NONE',  ( 0.000000000000000000, 0.000000000000000000, 1.000000000000000000 ) ) ;
#125058 = EDGE_LOOP ( 'NONE', ( #257231, #64217, #148639, #43914 ) ) ;
#125059 = TOROIDAL_SURFACE ( 'NONE', #100072, 11.65000000000000036, 0.1000000000000000056 ) ;
#125060 = ORIENTED_EDGE ( 'NONE', *, *, #29642, .F. ) ;
#125061 = CYLINDRICAL_SURFACE ( 'NONE', #222281, 0.1000000000000028644 ) ;
#125062 = CARTESIAN_POINT ( 'NONE',  ( -23.25000000000000000, 77.73670573947964613, -125.0056848969006182 ) ) ;
#125063 = DIRECTION ( 'NONE',  ( 0.000000000000000000, 6.938893903907229955E-15, -1.000000000000000000 ) ) ;
#125064 = FACE_OUTER_BOUND ( 'NONE', #108921, .T. ) ;
#125065 = DIRECTION ( 'NONE',  ( 1.000000000000000000, 0.000000000000000000, 0.000000000000000000 ) ) ;
#125066 = DIRECTION ( 'NONE',  ( 0.000000000000000000, 0.9553114395362733990, 0.2956011730205631016 ) ) ;
#125067 = CARTESIAN_POINT ( 'NONE',  ( -16.93970660449832621, 10.01284139163557185, -12.55228173579446960 ) ) ;
#125069 = CARTESIAN_POINT ( 'NONE',  ( -21.05000000000000071, 1.115600667400684642E-11, -67.00000000000000000 ) ) ;
#125068 = CARTESIAN_POINT ( 'NONE',  ( 21.46681500593309622, 6.857511159384197974, -9.855405879750058190E-16 ) ) ;
#125070 = CARTESIAN_POINT ( 'NONE',  ( 18.49999999999999289, 51.95251559509352290, -231.4682683249995137 ) ) ;
#125071 = DIRECTION ( 'NONE',  ( 0.000000000000000000, 0.2128009952263678062, -0.9770955615653298398 ) ) ;
#125072 = CARTESIAN_POINT ( 'NONE',  ( 23.24999999999999645, 76.00000000001195133, -103.0231074845243171 ) ) ;
#125073 = DIRECTION ( 'NONE',  ( 1.000000000000000000, 1.186688945009010077E-16, 0.000000000000000000 ) ) ;
#125074 = CIRCLE ( 'NONE', #50046, 4.100000000000006750 ) ;
#125075 = VERTEX_POINT ( 'NONE', #64781 ) ;
#125076 = ADVANCED_FACE ( 'NONE', ( #201730 ), #84287, .T. ) ;
#125077 = EDGE_LOOP ( 'NONE', ( #107089, #173982, #72505 ) ) ;
#125078 = DIRECTION ( 'NONE',  ( 1.000000000000000000, 2.952720810173289112E-16, -0.000000000000000000 ) ) ;
#125080 = EDGE_CURVE ( 'NONE', #132561, #250352, #144292, .T. ) ;
#125079 = CIRCLE ( 'NONE', #254227, 0.5000000000000014433 ) ;
#125081 = CARTESIAN_POINT ( 'NONE',  ( -20.85000000000000142, 7.021664781911246322, -204.8335654018972605 ) ) ;
#125083 = CARTESIAN_POINT ( 'NONE',  ( -12.60829076262180948, 12.96596579538268834, -216.4109158611324233 ) ) ;
#125082 = FACE_OUTER_BOUND ( 'NONE', #162477, .T. ) ;
#125084 = VECTOR ( 'NONE', #61829, 1000.000000000000000 ) ;
#125085 = DIRECTION ( 'NONE',  ( 1.000000000000000000, 0.000000000000000000, 0.000000000000000000 ) ) ;
#125087 = ADVANCED_FACE ( 'NONE', ( #8668, #247261 ), #106450, .F. ) ;
#125086 = CARTESIAN_POINT ( 'NONE',  ( 21.05000000000000071, 11.65000000001116298, -79.15000000000004832 ) ) ;
#125088 = DIRECTION ( 'NONE',  ( -0.000000000000000000, 0.1298341882519953583, 0.9915357197604862671 ) ) ;
#125089 = VECTOR ( 'NONE', #194643, 1000.000000000000000 ) ;
#125090 = ORIENTED_EDGE ( 'NONE', *, *, #86238, .F. ) ;
#125091 = AXIS2_PLACEMENT_3D ( 'NONE', #248905, #70289, #186365 ) ;
#125092 = ORIENTED_EDGE ( 'NONE', *, *, #70619, .T. ) ;
#125093 = ADVANCED_FACE ( 'NONE', ( #6085 ), #85766, .T. ) ;
#125094 = CARTESIAN_POINT ( 'NONE',  ( -12.25000000000000178, 9.349999999999983658, -16.75000000000000000 ) ) ;
#125095 = ORIENTED_EDGE ( 'NONE', *, *, #233599, .F. ) ;
#125096 = DIRECTION ( 'NONE',  ( -1.000000000000000000, 2.952720810173289112E-16, 2.061873921506763405E-30 ) ) ;
#125097 = ADVANCED_FACE ( 'NONE', ( #145594 ), #43324, .F. ) ;
#125098 = AXIS2_PLACEMENT_3D ( 'NONE', #25270, #40995, #60505 ) ;
#125099 = VECTOR ( 'NONE', #119997, 999.9999999999998863 ) ;
#125101 = AXIS2_PLACEMENT_3D ( 'NONE', #6637, #238839, #28828 ) ;
#125100 = CARTESIAN_POINT ( 'NONE',  ( 23.15000000000000213, 23.68770167995059239, -252.8127582590406348 ) ) ;
#125102 = AXIS2_PLACEMENT_3D ( 'NONE', #85147, #46051, #66904 ) ;
#125103 = CIRCLE ( 'NONE', #216667, 0.2000000000000057288 ) ;
#125104 = ORIENTED_EDGE ( 'NONE', *, *, #214066, .F. ) ;
#125105 = CARTESIAN_POINT ( 'NONE',  ( -20.94999999999999929, 87.48912529308852015, -172.9231074845242802 ) ) ;
#125106 = VERTEX_POINT ( 'NONE', #172925 ) ;
#125107 = EDGE_CURVE ( 'NONE', #104349, #126467, #248176, .T. ) ;
#125108 = CARTESIAN_POINT ( 'NONE',  ( 23.24999999999999289, 11.75000000001116263, -67.10000000000005116 ) ) ;
#125109 = EDGE_CURVE ( 'NONE', #184791, #250208, #14912, .T. ) ;
#125110 = CARTESIAN_POINT ( 'NONE',  ( 21.05000000000000071, 77.73625713161000306, -191.9544551555068495 ) ) ;
#125111 = DIRECTION ( 'NONE',  ( 0.000000000000000000, 0.000000000000000000, -1.000000000000000000 ) ) ;
#125112 = CARTESIAN_POINT ( 'NONE',  ( 18.41789779300687258, -9.499999999988844479, -141.0320696663606839 ) ) ;
#125113 = DIRECTION ( 'NONE',  ( -3.890533409366484021E-14, 0.08413937888703756918, -0.9964539953858901900 ) ) ;
#125114 = AXIS2_PLACEMENT_3D ( 'NONE', #174006, #57837, #74891 ) ;
#125115 = CARTESIAN_POINT ( 'NONE',  ( -21.33487959338958362, 6.725558151922345296, -134.0000000000000000 ) ) ;
#125116 = FACE_OUTER_BOUND ( 'NONE', #184608, .T. ) ;
#125117 = DIRECTION ( 'NONE',  ( 0.000000000000000000, 0.4930308989875575865, 0.8700118002898125091 ) ) ;
#125119 = EDGE_LOOP ( 'NONE', ( #38031, #247457, #162374, #49300 ) ) ;
#125118 = FACE_OUTER_BOUND ( 'NONE', #118158, .T. ) ;
#125121 = CARTESIAN_POINT ( 'NONE',  ( 21.14999999999999858, 76.00000000001242029, -176.5637644362255969 ) ) ;
#125120 = CARTESIAN_POINT ( 'NONE',  ( -16.81744102076748959, 66.05000000001201954, -115.6731074845243796 ) ) ;
#125122 = EDGE_LOOP ( 'NONE', ( #60467, #46371, #15891, #118173 ) ) ;
#125124 = ORIENTED_EDGE ( 'NONE', *, *, #67282, .T. ) ;
#125123 = CARTESIAN_POINT ( 'NONE',  ( 21.05000000000000071, 38.43293829866423295, -234.5626268121764895 ) ) ;
#125125 = VERTEX_POINT ( 'NONE', #170359 ) ;
#125126 = CARTESIAN_POINT ( 'NONE',  ( 22.88900146558018989, 44.64493140999041998, -236.4361273983403180 ) ) ;
#125127 = DIRECTION ( 'NONE',  ( 0.000000000000000000, 0.2128009952263603954, -0.9770955615653315052 ) ) ;
#125128 = DIRECTION ( 'NONE',  ( 1.836970198721029934E-16, -1.000000000000000000, -0.000000000000000000 ) ) ;
#125129 = SPHERICAL_SURFACE ( 'NONE', #168319, 0.1000000000000000056 ) ;
#125130 = CARTESIAN_POINT ( 'NONE',  ( -21.05000000000000071, 74.16465844978765176, -124.8679561919613263 ) ) ;
#125131 = DIRECTION ( 'NONE',  ( 0.000000000000000000, 0.000000000000000000, 1.000000000000000000 ) ) ;
#125132 = CIRCLE ( 'NONE', #196039, 4.049999999999998934 ) ;
#125133 = FACE_OUTER_BOUND ( 'NONE', #130666, .T. ) ;
#125134 = VECTOR ( 'NONE', #247378, 1000.000000000000000 ) ;
#125135 = CARTESIAN_POINT ( 'NONE',  ( -20.85000000000000142, 87.65000000001191438, -103.0231074845242176 ) ) ;
#125136 = EDGE_LOOP ( 'NONE', ( #84090, #165860, #13522, #181886 ) ) ;
#125137 = ORIENTED_EDGE ( 'NONE', *, *, #193478, .T. ) ;
#125138 = CARTESIAN_POINT ( 'NONE',  ( 18.59999999999999787, 38.28679861725831302, -261.0868692510649680 ) ) ;
#125139 = AXIS2_PLACEMENT_3D ( 'NONE', #11487, #110567, #150990 ) ;
#125140 = EDGE_CURVE ( 'NONE', #67744, #132345, #23296, .T. ) ;
#125141 = ORIENTED_EDGE ( 'NONE', *, *, #127329, .F. ) ;
#125142 = CYLINDRICAL_SURFACE ( 'NONE', #242419, 0.1000000000000000472 ) ;
#125143 = ORIENTED_EDGE ( 'NONE', *, *, #72193, .T. ) ;
#125144 = LINE ( 'NONE', #24779, #246697 ) ;
#125145 = AXIS2_PLACEMENT_3D ( 'NONE', #12747, #154823, #231780 ) ;
#125146 = DIRECTION ( 'NONE',  ( 0.000000000000000000, 7.056502275159894776E-15, -1.000000000000000000 ) ) ;
#125147 = CARTESIAN_POINT ( 'NONE',  ( -21.13498764882296044, 30.73029760849721015, -252.2052994570879036 ) ) ;
#125148 = CARTESIAN_POINT ( 'NONE',  ( 21.06280952165543141, 10.62713230061201841, -179.7040538867792918 ) ) ;
#125149 = EDGE_LOOP ( 'NONE', ( #151222, #117236, #78069, #121409, #28005 ) ) ;
#125150 = DIRECTION ( 'NONE',  ( 1.000000000000000000, 2.952720810173289112E-16, -0.000000000000000000 ) ) ;
#125151 = CARTESIAN_POINT ( 'NONE',  ( 23.24999999999999289, 80.15000000001165859, -69.52310748452430289 ) ) ;
#125152 = DIRECTION ( 'NONE',  ( -1.000000000000000000, -0.000000000000000000, -0.000000000000000000 ) ) ;
#125154 = EDGE_CURVE ( 'NONE', #217170, #207209, #152053, .T. ) ;
#125153 = SPHERICAL_SURFACE ( 'NONE', #26737, 0.1000000000000000056 ) ;
#125155 = EDGE_LOOP ( 'NONE', ( #188414, #160621, #132520, #235475 ) ) ;
#125158 = DIRECTION ( 'NONE',  ( 0.000000000000000000, 0.000000000000000000, -1.000000000000000000 ) ) ;
#125157 = CARTESIAN_POINT ( 'NONE',  ( -22.39999999999999858, 7.790779598384560245, -167.4999999999999716 ) ) ;
#125156 = AXIS2_PLACEMENT_3D ( 'NONE', #70488, #28803, #9187 ) ;
#125159 = ORIENTED_EDGE ( 'NONE', *, *, #18355, .F. ) ;
#125161 = ORIENTED_EDGE ( 'NONE', *, *, #143036, .F. ) ;
#125160 = DIRECTION ( 'NONE',  ( 0.000000000000000000, 0.000000000000000000, 1.000000000000000000 ) ) ;
#125162 = VECTOR ( 'NONE', #78029, 1000.000000000000000 ) ;
#125163 = ORIENTED_EDGE ( 'NONE', *, *, #67009, .T. ) ;
#125164 = CARTESIAN_POINT ( 'NONE',  ( 21.05000000000000071, -8.730841121484166578, -157.9019252810156786 ) ) ;
#125165 = VECTOR ( 'NONE', #58173, 1000.000000000000114 ) ;
#125166 = CARTESIAN_POINT ( 'NONE',  ( 18.59999999999999432, 13.71992543034163958, -238.5823796952984992 ) ) ;
#125167 = DIRECTION ( 'NONE',  ( 1.000000000000000000, -0.000000000000000000, -0.000000000000000000 ) ) ;
#125168 = ORIENTED_EDGE ( 'NONE', *, *, #127715, .T. ) ;
#125169 = FACE_OUTER_BOUND ( 'NONE', #207598, .T. ) ;
#125170 = FACE_OUTER_BOUND ( 'NONE', #165969, .T. ) ;
#125172 = DIRECTION ( 'NONE',  ( 0.000000000000000000, 0.000000000000000000, -1.000000000000000000 ) ) ;
#125171 = DIRECTION ( 'NONE',  ( 1.000000000000000000, 0.000000000000000000, 0.000000000000000000 ) ) ;
#125174 = ORIENTED_EDGE ( 'NONE', *, *, #51315, .F. ) ;
#125173 = CARTESIAN_POINT ( 'NONE',  ( 20.85000000000000142, 11.75000000001115907, -93.71613433702195550 ) ) ;
#125175 = AXIS2_PLACEMENT_3D ( 'NONE', #134421, #18351, #116188 ) ;
#125176 = ORIENTED_EDGE ( 'NONE', *, *, #57903, .F. ) ;
#125177 = DIRECTION ( 'NONE',  ( 0.000000000000000000, 0.000000000000000000, 1.000000000000000000 ) ) ;
#125178 = CARTESIAN_POINT ( 'NONE',  ( -23.15000000000000213, 11.65000000001115588, -179.6499999999999773 ) ) ;
#125179 = DIRECTION ( 'NONE',  ( 0.000000000000000000, 0.000000000000000000, -1.000000000000000000 ) ) ;
#125180 = EDGE_LOOP ( 'NONE', ( #190580, #196727, #203591, #137048, #192215, #107383, #129949 ) ) ;
#125181 = CARTESIAN_POINT ( 'NONE',  ( -16.87372397896795562, 9.880599536652889370, -187.8507245100357181 ) ) ;
#125182 = VERTEX_POINT ( 'NONE', #114182 ) ;
#125183 = CARTESIAN_POINT ( 'NONE',  ( 18.59999999999999076, 69.45000000001181206, -81.77310748452434552 ) ) ;
#125184 = DIRECTION ( 'NONE',  ( 1.000000000000000000, 0.000000000000000000, 0.000000000000000000 ) ) ;
#125185 = CARTESIAN_POINT ( 'NONE',  ( 20.94999999999999574, 1.835341550224411922, -11.65515129256298010 ) ) ;
#125186 = VERTEX_POINT ( 'NONE', #73804 ) ;
#125187 = CARTESIAN_POINT ( 'NONE',  ( -18.59999999999999787, 74.65925378207803931, -79.79596998994550461 ) ) ;
#125188 = AXIS2_PLACEMENT_3D ( 'NONE', #207540, #151422, #189254 ) ;
#125189 = VECTOR ( 'NONE', #229836, 1000.000000000000000 ) ;
#125190 = EDGE_CURVE ( 'NONE', #169291, #171894, #249848, .T. ) ;
#125191 = CIRCLE ( 'NONE', #208418, 11.70000000000001528 ) ;
#125192 = DIRECTION ( 'NONE',  ( 2.694716079187273439E-16, 1.000000000000000000, 7.006261805886910842E-15 ) ) ;
#125193 = EDGE_LOOP ( 'NONE', ( #110370, #122626, #36867, #78118 ) ) ;
#125194 = CIRCLE ( 'NONE', #12789, 0.1000000000000028644 ) ;
#125195 = ORIENTED_EDGE ( 'NONE', *, *, #104062, .T. ) ;
#125196 = ORIENTED_EDGE ( 'NONE', *, *, #237142, .T. ) ;
#125197 = EDGE_CURVE ( 'NONE', #31330, #10681, #75092, .T. ) ;
#125198 = DIRECTION ( 'NONE',  ( -0.000000000000000000, 1.000000000000000000, 6.982962677686266711E-15 ) ) ;
#125199 = ORIENTED_EDGE ( 'NONE', *, *, #88220, .T. ) ;
#125201 = ORIENTED_EDGE ( 'NONE', *, *, #134463, .T. ) ;
#125200 = DIRECTION ( 'NONE',  ( -1.000000000000000000, -7.304098846218134667E-16, 4.217023435051678980E-16 ) ) ;
#125202 = SHAPE_REPRESENTATION ( 'Snap Open Cable Crossbars 14', ( #2425 ), #156768 ) ;
#125203 = ADVANCED_FACE ( 'NONE', ( #69947 ), #188579, .T. ) ;
#125204 = ORIENTED_EDGE ( 'NONE', *, *, #257772, .F. ) ;
#125205 = CIRCLE ( 'NONE', #25259, 0.09999999999998898659 ) ;
#125207 = VERTEX_POINT ( 'NONE', #174205 ) ;
#125206 = ORIENTED_EDGE ( 'NONE', *, *, #86463, .T. ) ;
#125208 = CARTESIAN_POINT ( 'NONE',  ( 20.85000000000000142, -1.164121893241208960, -41.41484808557160591 ) ) ;
#125210 = EDGE_CURVE ( 'NONE', #226256, #7157, #152474, .T. ) ;
#125209 = EDGE_LOOP ( 'NONE', ( #250001, #64851, #68679, #185496 ) ) ;
#125211 = DIRECTION ( 'NONE',  ( -0.000000000000000000, -6.982962677686266711E-15, 1.000000000000000000 ) ) ;
#125212 = CARTESIAN_POINT ( 'NONE',  ( 21.05000000000000426, 69.58617371119899531, -102.9373665474909672 ) ) ;
#125213 = DIRECTION ( 'NONE',  ( 1.000000000000000000, 2.986185139342072849E-16, -6.665775143889690802E-16 ) ) ;
#125214 = ORIENTED_EDGE ( 'NONE', *, *, #258026, .F. ) ;
#125216 = VERTEX_POINT ( 'NONE', #129884 ) ;
#125215 = CARTESIAN_POINT ( 'NONE',  ( -20.64999999999999858, 0.000000000000000000, 0.000000000000000000 ) ) ;
#125217 = CARTESIAN_POINT ( 'NONE',  ( 18.69999999999998153, -1.212568896937008089, -7.900000000000000355 ) ) ;
#125219 = ORIENTED_EDGE ( 'NONE', *, *, #62349, .T. ) ;
#125218 = CARTESIAN_POINT ( 'NONE',  ( 21.87500000000000355, 61.05385884576948996, -221.3836188041226762 ) ) ;
#125220 = EDGE_CURVE ( 'NONE', #178255, #52759, #153361, .T. ) ;
#125221 = CIRCLE ( 'NONE', #58556, 0.1000000000000028644 ) ;
#125222 = ORIENTED_EDGE ( 'NONE', *, *, #212464, .T. ) ;
#125223 = CARTESIAN_POINT ( 'NONE',  ( -21.14999999999999858, -11.65000000000000036, -2.900000000000001688 ) ) ;
#125224 = AXIS2_PLACEMENT_3D ( 'NONE', #72444, #98355, #18860 ) ;
#125225 = EDGE_LOOP ( 'NONE', ( #101467, #76765, #243513, #81789 ) ) ;
#125226 = VERTEX_POINT ( 'NONE', #208169 ) ;
#125228 = CIRCLE ( 'NONE', #237828, 0.09999999999999939493 ) ;
#125227 = DIRECTION ( 'NONE',  ( 0.7071067811865476838, -0.6909108974501236844, -0.1504730267678055788 ) ) ;
#125229 = DIRECTION ( 'NONE',  ( -0.000000000000000000, -1.000000000000000000, -6.982962677686266711E-15 ) ) ;
#125231 = ORIENTED_EDGE ( 'NONE', *, *, #160121, .T. ) ;
#125230 = ORIENTED_EDGE ( 'NONE', *, *, #54126, .T. ) ;
#125232 = ORIENTED_EDGE ( 'NONE', *, *, #127527, .T. ) ;
#125233 = CARTESIAN_POINT ( 'NONE',  ( -22.59999970745345976, 64.16457265427982293, -247.1984059110171188 ) ) ;
#125234 = ORIENTED_EDGE ( 'NONE', *, *, #78665, .T. ) ;
#125235 = ORIENTED_EDGE ( 'NONE', *, *, #32590, .F. ) ;
#125236 = CARTESIAN_POINT ( 'NONE',  ( -21.44999999999999929, 52.99650480578122824, -234.2878581050858884 ) ) ;
#125237 = AXIS2_PLACEMENT_3D ( 'NONE', #227288, #48650, #44810 ) ;
#125239 = ORIENTED_EDGE ( 'NONE', *, *, #94937, .F. ) ;
#125238 = DIRECTION ( 'NONE',  ( -0.000000000000000000, 0.000000000000000000, 1.000000000000000000 ) ) ;
#125240 = DIRECTION ( 'NONE',  ( 0.000000000000000000, 0.4721928772777346239, 0.8814952561688430555 ) ) ;
#125242 = CARTESIAN_POINT ( 'NONE',  ( -18.59999999999999787, 66.75000000001151079, -48.37310748452438247 ) ) ;
#125241 = CARTESIAN_POINT ( 'NONE',  ( -16.92925196614876171, 22.95929811576328916, -230.8996751924844659 ) ) ;
#125243 = CARTESIAN_POINT ( 'NONE',  ( 18.58703555225034876, 85.40633674080154947, -196.3981628432776461 ) ) ;
#125244 = EDGE_CURVE ( 'NONE', #233936, #201514, #81486, .T. ) ;
#125245 = VERTEX_POINT ( 'NONE', #30823 ) ;
#125246 = ORIENTED_EDGE ( 'NONE', *, *, #247990, .T. ) ;
#125247 = PLANE ( 'NONE',  #61036 ) ;
#125248 = FACE_OUTER_BOUND ( 'NONE', #41202, .T. ) ;
#125250 = EDGE_LOOP ( 'NONE', ( #112984, #74975, #41935, #69601, #2695, #232022, #30181, #214014, #82447, #257760, #123124, #69273 ) ) ;
#125249 = CIRCLE ( 'NONE', #175187, 0.09999999999999939493 ) ;
#125251 = AXIS2_PLACEMENT_3D ( 'NONE', #4519, #219715, #103605 ) ;
#125252 = EDGE_CURVE ( 'NONE', #238213, #202854, #223164, .T. ) ;
#125253 = AXIS2_PLACEMENT_3D ( 'NONE', #213964, #195709, #232266 ) ;
#125254 = FACE_OUTER_BOUND ( 'NONE', #135843, .T. ) ;
#125255 = ORIENTED_EDGE ( 'NONE', *, *, #51606, .F. ) ;
#125256 = ORIENTED_EDGE ( 'NONE', *, *, #102924, .T. ) ;
#125257 = VECTOR ( 'NONE', #197161, 1000.000000000000000 ) ;
#125258 = DIRECTION ( 'NONE',  ( -0.000000000000000000, 6.982962677686266711E-15, -1.000000000000000000 ) ) ;
#125259 = ORIENTED_EDGE ( 'NONE', *, *, #208252, .T. ) ;
#125260 = DIRECTION ( 'NONE',  ( 1.000000000000000000, 0.000000000000000000, 0.000000000000000000 ) ) ;
#125261 = CARTESIAN_POINT ( 'NONE',  ( -21.08479644141223019, 6.345038657743042876, -167.4414455574358556 ) ) ;
#125262 = EDGE_LOOP ( 'NONE', ( #178927, #25464, #245891, #228207 ) ) ;
#125263 = AXIS2_PLACEMENT_3D ( 'NONE', #166618, #240995, #3650 ) ;
#125264 = DIRECTION ( 'NONE',  ( 0.000000000000000000, 0.000000000000000000, 1.000000000000000000 ) ) ;
#125267 = ADVANCED_FACE ( 'NONE', ( #253680 ), #110330, .T. ) ;
#125266 = AXIS2_PLACEMENT_3D ( 'NONE', #6100, #7390, #28286 ) ;
#125265 = DIRECTION ( 'NONE',  ( 0.000000000000000000, 6.982962677686266711E-15, -1.000000000000000000 ) ) ;
#125269 = CARTESIAN_POINT ( 'NONE',  ( 20.12500000000000000, 40.07562767317620711, -237.3368484665046765 ) ) ;
#125268 = CARTESIAN_POINT ( 'NONE',  ( -21.05000000000000071, 79.26035508877831148, -236.0091442494974956 ) ) ;
#125270 = DIRECTION ( 'NONE',  ( 0.000000000000000000, 1.000000000000000000, 0.000000000000000000 ) ) ;
#125271 = DIRECTION ( 'NONE',  ( 1.000000000000000000, 0.000000000000000000, 0.000000000000000000 ) ) ;
#125272 = DIRECTION ( 'NONE',  ( 0.000000000000000000, 1.000000000000000000, 6.982962677686266711E-15 ) ) ;
#125273 = CARTESIAN_POINT ( 'NONE',  ( -21.05000000000000071, 87.65000000001172964, -72.42310748452422331 ) ) ;
#125274 = EDGE_CURVE ( 'NONE', #51801, #113685, #19528, .T. ) ;
#125275 = EDGE_LOOP ( 'NONE', ( #243089, #76999, #81743, #22348 ) ) ;
#125276 = CIRCLE ( 'NONE', #75216, 14.20833333333333748 ) ;
#125277 = CIRCLE ( 'NONE', #12860, 0.3999999999999975797 ) ;
#125278 = CIRCLE ( 'NONE', #233442, 4.049999999999997158 ) ;
#125279 = AXIS2_PLACEMENT_3D ( 'NONE', #210940, #250065, #191407 ) ;
#125281 = EDGE_LOOP ( 'NONE', ( #126742, #148351, #68536, #95576 ) ) ;
#125280 = VERTEX_POINT ( 'NONE', #176377 ) ;
#125282 = ORIENTED_EDGE ( 'NONE', *, *, #44807, .F. ) ;
#125283 = PLANE ( 'NONE',  #215952 ) ;
#125284 = EDGE_CURVE ( 'NONE', #189087, #117471, #39443, .T. ) ;
#125285 = DIRECTION ( 'NONE',  ( 1.000000000000000000, 0.000000000000000000, 0.000000000000000000 ) ) ;
#125286 = CARTESIAN_POINT ( 'NONE',  ( -14.56556274378147720, 9.446557523072533158, -15.08994195434589436 ) ) ;
#125287 = CARTESIAN_POINT ( 'NONE',  ( 21.04999999999999716, 67.10527618163473562, -161.5360231613763915 ) ) ;
#125288 = ORIENTED_EDGE ( 'NONE', *, *, #110025, .T. ) ;
#125289 = EDGE_CURVE ( 'NONE', #103521, #131441, #177669, .T. ) ;
#125290 = LINE ( 'NONE', #186554, #17490 ) ;
#125291 = EDGE_CURVE ( 'NONE', #94242, #7533, #118960, .T. ) ;
#125292 = AXIS2_PLACEMENT_3D ( 'NONE', #73953, #128768, #50474 ) ;
#125293 = DIRECTION ( 'NONE',  ( 1.000000000000000000, 0.000000000000000000, 0.000000000000000000 ) ) ;
#125294 = CARTESIAN_POINT ( 'NONE',  ( -16.86132326855785735, 66.05000000001189164, -90.32447169985607616 ) ) ;
#125295 = CARTESIAN_POINT ( 'NONE',  ( 21.00000000000000000, 66.25000000001158185, -57.17310748452438673 ) ) ;
#125296 = ORIENTED_EDGE ( 'NONE', *, *, #84117, .T. ) ;
#125297 = CARTESIAN_POINT ( 'NONE',  ( 18.44364597020194907, -9.490487317162260794, -7.057977889683861861 ) ) ;
#125298 = EDGE_CURVE ( 'NONE', #248700, #198075, #110744, .T. ) ;
#125299 = DIRECTION ( 'NONE',  ( 1.000000000000000000, -3.265361837132813093E-16, -2.280189983783949500E-30 ) ) ;
#125300 = EDGE_LOOP ( 'NONE', ( #66100, #62658, #127589, #233462 ) ) ;
#125301 = ORIENTED_EDGE ( 'NONE', *, *, #37997, .T. ) ;
#125302 = CARTESIAN_POINT ( 'NONE',  ( -20.85000000000000142, 11.65000000001115232, -194.2161343370218560 ) ) ;
#125303 = CARTESIAN_POINT ( 'NONE',  ( -22.47071067811865319, 0.3704148268516976872, -229.9999874772930752 ) ) ;
#125304 = CARTESIAN_POINT ( 'NONE',  ( -21.55000000000000071, 11.50825441376376901, -220.2417535673963300 ) ) ;
#125305 = EDGE_CURVE ( 'NONE', #244818, #113723, #168735, .T. ) ;
#125306 = FACE_OUTER_BOUND ( 'NONE', #71966, .T. ) ;
#125307 = CARTESIAN_POINT ( 'NONE',  ( 20.94999999999999929, -8.999999999988842703, -57.10603087734755690 ) ) ;
#125308 = ADVANCED_FACE ( 'NONE', ( #1551 ), #41999, .T. ) ;
#125309 = DIRECTION ( 'NONE',  ( 1.000000000000000000, 0.000000000000000000, 1.073024830501117725E-15 ) ) ;
#125310 = ORIENTED_EDGE ( 'NONE', *, *, #213063, .T. ) ;
#125311 = CARTESIAN_POINT ( 'NONE',  ( 23.24999999999999289, 6.650000000011155876, -188.6499999999999488 ) ) ;
#125312 = DIRECTION ( 'NONE',  ( 0.000000000000000000, 0.000000000000000000, -1.000000000000000000 ) ) ;
#125313 = AXIS2_PLACEMENT_3D ( 'NONE', #19672, #22246, #80896 ) ;
#125314 = DIRECTION ( 'NONE',  ( 1.000000000000000000, -0.000000000000000000, -0.000000000000000000 ) ) ;
#125316 = DIRECTION ( 'NONE',  ( -0.000000000000000000, 6.982962677686266711E-15, -1.000000000000000000 ) ) ;
#125315 = DIRECTION ( 'NONE',  ( 0.000000000000000000, 0.000000000000000000, -1.000000000000000000 ) ) ;
#125317 = CARTESIAN_POINT ( 'NONE',  ( 20.46382478191414833, 65.40137955871524866, -195.8452930151790099 ) ) ;
#125318 = DIRECTION ( 'NONE',  ( 3.616040088954490704E-32, 7.105427357601001859E-15, -1.000000000000000000 ) ) ;
#125319 = DIRECTION ( 'NONE',  ( 0.000000000000000000, 0.000000000000000000, -1.000000000000000000 ) ) ;
#125322 = EDGE_LOOP ( 'NONE', ( #150724, #53565, #244939, #122771, #38625, #125656, #211494, #245498, #192608, #71507 ) ) ;
#125321 = AXIS2_PLACEMENT_3D ( 'NONE', #4573, #223618, #68426 ) ;
#125320 = CARTESIAN_POINT ( 'NONE',  ( 18.59999999999999432, -1.736257131586239844, -145.5686523290175387 ) ) ;
#125323 = CIRCLE ( 'NONE', #167047, 0.09999999999999868716 ) ;
#125324 = EDGE_CURVE ( 'NONE', #99053, #109724, #35941, .T. ) ;
#125325 = EDGE_CURVE ( 'NONE', #136892, #243144, #41235, .T. ) ;
#125326 = CARTESIAN_POINT ( 'NONE',  ( 22.47071067811865319, 7.720074744509199505, -100.4009075452974287 ) ) ;
#125327 = VECTOR ( 'NONE', #194545, 1000.000000000000000 ) ;
#125328 = EDGE_CURVE ( 'NONE', #216004, #251640, #160671, .T. ) ;
#125329 = CARTESIAN_POINT ( 'NONE',  ( 21.22070241538126467, 65.44227650827568254, -242.0736050779767936 ) ) ;
#125330 = DIRECTION ( 'NONE',  ( -3.265361837132813093E-16, -1.000000000000000000, -6.982962677686266711E-15 ) ) ;
#125331 = CIRCLE ( 'NONE', #46373, 0.09999999999999484301 ) ;
#125332 = ORIENTED_EDGE ( 'NONE', *, *, #142115, .F. ) ;
#125333 = AXIS2_PLACEMENT_3D ( 'NONE', #70145, #34869, #14003 ) ;
#125334 = CARTESIAN_POINT ( 'NONE',  ( -18.59999999999999787, 74.83729825007408465, -128.5231074845243029 ) ) ;
#125335 = CARTESIAN_POINT ( 'NONE',  ( -20.94999999999999929, 16.44800918141279311, -240.8068063186265135 ) ) ;
#125337 = DIRECTION ( 'NONE',  ( 0.000000000000000000, 0.000000000000000000, -1.000000000000000000 ) ) ;
#125336 = AXIS2_PLACEMENT_3D ( 'NONE', #48140, #190233, #106820 ) ;
#125338 = ORIENTED_EDGE ( 'NONE', *, *, #223657, .F. ) ;
#125339 = DIRECTION ( 'NONE',  ( 0.000000000000000000, -0.8660254037844377084, -0.5000000000000016653 ) ) ;
#125341 = ORIENTED_EDGE ( 'NONE', *, *, #19240, .T. ) ;
#125340 = CARTESIAN_POINT ( 'NONE',  ( -16.79270642812294767, 9.946244216949358119, -188.3389332785629335 ) ) ;
#125343 = CARTESIAN_POINT ( 'NONE',  ( -16.85312964099708566, 66.08639531794410971, -82.42029177809392593 ) ) ;
#125342 = CARTESIAN_POINT ( 'NONE',  ( 21.05000000000000071, 4.850467289730772791, -79.03426740900172831 ) ) ;
#125344 = DIRECTION ( 'NONE',  ( 1.000000000000000000, 0.000000000000000000, 0.000000000000000000 ) ) ;
#125345 = ORIENTED_EDGE ( 'NONE', *, *, #134389, .F. ) ;
#125346 = LINE ( 'NONE', #119254, #176224 ) ;
#125347 = EDGE_CURVE ( 'NONE', #222996, #188810, #17293, .T. ) ;
#125348 = DIRECTION ( 'NONE',  ( 1.000000000000000000, 0.000000000000000000, 0.000000000000000000 ) ) ;
#125349 = FACE_OUTER_BOUND ( 'NONE', #136728, .T. ) ;
#125350 = CARTESIAN_POINT ( 'NONE',  ( -21.05000000000000071, 70.10000000001177511, -79.74220724918070857 ) ) ;
#125351 = DIRECTION ( 'NONE',  ( -1.000000000000000000, -0.000000000000000000, -0.000000000000000000 ) ) ;
#125352 = CIRCLE ( 'NONE', #96106, 0.1000000000000028644 ) ;
#125353 = ORIENTED_EDGE ( 'NONE', *, *, #93888, .T. ) ;
#125355 = ADVANCED_FACE ( 'NONE', ( #137222 ), #62822, .T. ) ;
#125354 = CARTESIAN_POINT ( 'NONE',  ( -21.05000000000000071, 1.115600667400684642E-11, -134.0000000000000000 ) ) ;
#125356 = DIRECTION ( 'NONE',  ( 2.940209281316622988E-16, 0.4088369013363260529, -0.9126074666063779262 ) ) ;
#125357 = ADVANCED_FACE ( 'NONE', ( #98059 ), #257120, .T. ) ;
#125358 = EDGE_CURVE ( 'NONE', #63948, #48255, #238901, .T. ) ;
#125359 = CARTESIAN_POINT ( 'NONE',  ( -22.47886152344871036, 0.03750093887284931121, -122.3500113569520806 ) ) ;
#125360 = ORIENTED_EDGE ( 'NONE', *, *, #69114, .T. ) ;
#125361 = VERTEX_POINT ( 'NONE', #120269 ) ;
#125362 = EDGE_CURVE ( 'NONE', #173652, #154226, #69258, .T. ) ;
#125363 = CARTESIAN_POINT ( 'NONE',  ( 21.09551895715238246, 65.37856267284368528, -124.2859828186246745 ) ) ;
#125364 = CARTESIAN_POINT ( 'NONE',  ( 18.39999999999999503, 5.650000000011139001, -113.1500000000000341 ) ) ;
#125365 = DIRECTION ( 'NONE',  ( -1.000000000000000000, -0.000000000000000000, -0.000000000000000000 ) ) ;
#125366 = AXIS2_PLACEMENT_3D ( 'NONE', #38521, #60625, #1933 ) ;
#125367 = CARTESIAN_POINT ( 'NONE',  ( 21.05000000000000071, 10.42338541492404680, -141.4920519238701218 ) ) ;
#125368 = VECTOR ( 'NONE', #170904, 1000.000000000000000 ) ;
#125369 = VECTOR ( 'NONE', #101954, 1000.000000000000000 ) ;
#125372 = SURFACE_STYLE_FILL_AREA ( #207486 ) ;
#125371 = CIRCLE ( 'NONE', #12963, 0.1000000000000000472 ) ;
#125370 = DIRECTION ( 'NONE',  ( 0.000000000000000000, 0.8660254037844482555, 0.4999999999999837907 ) ) ;
#125373 = CARTESIAN_POINT ( 'NONE',  ( -23.15000000000000213, 7.128833340093095217, -233.7327013124392749 ) ) ;
#125374 = DIRECTION ( 'NONE',  ( 1.000000000000000000, 0.000000000000000000, 0.000000000000000000 ) ) ;
#125375 = CARTESIAN_POINT ( 'NONE',  ( -22.49544290803740054, 64.25012976215485594, -136.5884194437824419 ) ) ;
#125376 = DIRECTION ( 'NONE',  ( -0.7071067811865388020, 0.7071067811865561215, 0.000000000000000000 ) ) ;
#125377 = EDGE_CURVE ( 'NONE', #108958, #153327, #65137, .T. ) ;
#125379 = ORIENTED_EDGE ( 'NONE', *, *, #15101, .T. ) ;
#125378 = DIRECTION ( 'NONE',  ( 1.186688945009010077E-16, -1.000000000000000000, -0.000000000000000000 ) ) ;
#125380 = AXIS2_PLACEMENT_3D ( 'NONE', #220905, #203926, #42293 ) ;
#125381 = CARTESIAN_POINT ( 'NONE',  ( -21.00448002041582640, 64.25000000001207923, -129.6747666222131556 ) ) ;
#125382 = EDGE_CURVE ( 'NONE', #214701, #188486, #242730, .T. ) ;
#125383 = CYLINDRICAL_SURFACE ( 'NONE', #207436, 0.09999999999999939493 ) ;
#125385 = CARTESIAN_POINT ( 'NONE',  ( 23.24999999999999289, 6.550000000011156231, -155.3500000000000227 ) ) ;
#125384 = FACE_OUTER_BOUND ( 'NONE', #124881, .T. ) ;
#125386 = B_SPLINE_CURVE_WITH_KNOTS ( 'NONE', 3,
 ( #25907, #164134, #128859, #144542, #184968, #208406, #126266, #169299, #45455, #248805 ),
 .UNSPECIFIED., .F., .F.,
 ( 4, 3, 3, 4 ),
 ( 0.000000000000000000, 0.0002000000000008539272, 0.001000000000082976398, 0.001967863649483329348 ),
 .UNSPECIFIED. ) ;
#125387 = ORIENTED_EDGE ( 'NONE', *, *, #247532, .T. ) ;
#125388 = CARTESIAN_POINT ( 'NONE',  ( -16.89081410710458542, 66.04868147016489388, -115.6687015646880070 ) ) ;
#125390 = ADVANCED_FACE ( 'NONE', ( #142351 ), #202514, .T. ) ;
#125389 = CARTESIAN_POINT ( 'NONE',  ( 20.85000000000000142, 77.26327546522965406, -162.1212428177779543 ) ) ;
#125391 = DIRECTION ( 'NONE',  ( 0.000000000000000000, 0.2617529984165034573, 0.9651348961777156399 ) ) ;
#125392 = CARTESIAN_POINT ( 'NONE',  ( -18.59999999999999787, 43.07541598710462694, -233.9110336739111631 ) ) ;
#125393 = FACE_OUTER_BOUND ( 'NONE', #36764, .T. ) ;
#125394 = ORIENTED_EDGE ( 'NONE', *, *, #33233, .T. ) ;
#125396 = ORIENTED_EDGE ( 'NONE', *, *, #228993, .T. ) ;
#125395 = CIRCLE ( 'NONE', #237807, 0.09999999999999939493 ) ;
#125397 = CARTESIAN_POINT ( 'NONE',  ( -23.15000000000000213, 11.75000000000000711, -12.15000000000000036 ) ) ;
#125398 = ORIENTED_EDGE ( 'NONE', *, *, #196277, .F. ) ;
#125399 = CARTESIAN_POINT ( 'NONE',  ( -20.85000000000000142, 87.34033503009941057, -206.5987052159188124 ) ) ;
#125400 = EDGE_CURVE ( 'NONE', #201984, #253337, #19356, .T. ) ;
#125401 = EDGE_CURVE ( 'NONE', #21668, #936, #225721, .T. ) ;
#125402 = VERTEX_POINT ( 'NONE', #124098 ) ;
#125403 = DIRECTION ( 'NONE',  ( 1.000000000000000000, -0.000000000000000000, -0.000000000000000000 ) ) ;
#125404 = FACE_OUTER_BOUND ( 'NONE', #179500, .T. ) ;
#125405 = EDGE_CURVE ( 'NONE', #209133, #135761, #187920, .T. ) ;
#125406 = CARTESIAN_POINT ( 'NONE',  ( 20.94999999999999929, -1.835341550213257733, -179.0551512925629538 ) ) ;
#125407 = EDGE_LOOP ( 'NONE', ( #149342, #96606, #51965, #213059 ) ) ;
#125408 = AXIS2_PLACEMENT_3D ( 'NONE', #27909, #125686, #205209 ) ;
#125409 = ADVANCED_FACE ( 'NONE', ( #186638 ), #103210, .T. ) ;
#125410 = DIRECTION ( 'NONE',  ( 0.000000000000000000, -0.5341055959866553016, 0.8454177738465993297 ) ) ;
#125411 = LINE ( 'NONE', #44589, #254859 ) ;
#125412 = EDGE_CURVE ( 'NONE', #56204, #59508, #140138, .T. ) ;
#125413 = LINE ( 'NONE', #242768, #124349 ) ;
#125414 = VECTOR ( 'NONE', #120561, 1000.000000000000000 ) ;
#125415 = CARTESIAN_POINT ( 'NONE',  ( 20.94999999999999929, 76.00000000001195133, -103.0231074845243171 ) ) ;
#125416 = CARTESIAN_POINT ( 'NONE',  ( -16.84421487269769102, 44.15327948857689933, -235.2909584192975672 ) ) ;
#125417 = DIRECTION ( 'NONE',  ( 1.000000000000000000, 0.000000000000000000, 0.000000000000000000 ) ) ;
#125419 = DIRECTION ( 'NONE',  ( 0.000000000000000000, 1.000000000000000000, 0.000000000000000000 ) ) ;
#125418 = CIRCLE ( 'NONE', #150364, 11.65000000000000036 ) ;
#125420 = VERTEX_POINT ( 'NONE', #5384 ) ;
#125422 = FACE_OUTER_BOUND ( 'NONE', #92702, .T. ) ;
#125421 = CARTESIAN_POINT ( 'NONE',  ( -18.50000000000000000, 85.40000000001138858, -29.14106563635158764 ) ) ;
#125423 = ORIENTED_EDGE ( 'NONE', *, *, #100693, .T. ) ;
#125425 = EDGE_LOOP ( 'NONE', ( #3722, #78082, #28047, #160688 ) ) ;
#125424 = CARTESIAN_POINT ( 'NONE',  ( 18.59999999999999076, 6.450000000011156587, -43.51702717044002355 ) ) ;
#125426 = ORIENTED_EDGE ( 'NONE', *, *, #111549, .T. ) ;
#125427 = CARTESIAN_POINT ( 'NONE',  ( -16.27683809663750480, 11.10425270649115603, -208.0484446391143649 ) ) ;
#125428 = AXIS2_PLACEMENT_3D ( 'NONE', #188190, #130771, #128215 ) ;
#125429 = DIRECTION ( 'NONE',  ( -0.000000000000000000, -0.9875055080513799322, 0.1575844902526464253 ) ) ;
#125430 = LINE ( 'NONE', #83680, #47306 ) ;
#125431 = CARTESIAN_POINT ( 'NONE',  ( -18.50000000000000000, 9.150000000011157653, -45.85000000000000142 ) ) ;
#125432 = VECTOR ( 'NONE', #11830, 1000.000000000000000 ) ;
#125433 = ORIENTED_EDGE ( 'NONE', *, *, #228741, .F. ) ;
#125434 = EDGE_CURVE ( 'NONE', #221067, #242867, #248303, .T. ) ;
#125435 = DIRECTION ( 'NONE',  ( 0.000000000000000000, 6.982962677686266711E-15, -1.000000000000000000 ) ) ;
#125436 = CARTESIAN_POINT ( 'NONE',  ( 18.54999999999999716, 60.93935776605888321, -221.0417277355861359 ) ) ;
#125437 = ORIENTED_EDGE ( 'NONE', *, *, #215289, .F. ) ;
#125438 = DIRECTION ( 'NONE',  ( 0.000000000000000000, 0.000000000000000000, 1.000000000000000000 ) ) ;
#125439 = EDGE_CURVE ( 'NONE', #255695, #177651, #94174, .T. ) ;
#125440 = DIRECTION ( 'NONE',  ( 0.000000000000000000, 0.000000000000000000, 1.000000000000000000 ) ) ;
#125441 = CIRCLE ( 'NONE', #200255, 0.8750000000000007772 ) ;
#125442 = ORIENTED_EDGE ( 'NONE', *, *, #149758, .F. ) ;
#125443 = CARTESIAN_POINT ( 'NONE',  ( -16.80070461187906261, 9.950000000011135270, -146.6469638291605975 ) ) ;
#125444 = ORIENTED_EDGE ( 'NONE', *, *, #232392, .T. ) ;
#125445 = DIRECTION ( 'NONE',  ( 0.000000000000000000, 0.2617529984164506107, 0.9651348961777299618 ) ) ;
#125446 = VERTEX_POINT ( 'NONE', #182790 ) ;
#125447 = CARTESIAN_POINT ( 'NONE',  ( -21.05000000000000071, 0.000000000000000000, -33.50000000000000000 ) ) ;
#125448 = AXIS2_PLACEMENT_3D ( 'NONE', #143306, #199458, #119938 ) ;
#125449 = ADVANCED_FACE ( 'NONE', ( #43266 ), #206187, .T. ) ;
#125450 = CARTESIAN_POINT ( 'NONE',  ( 21.05315837410544688, 64.25000000001173817, -76.36475148275641800 ) ) ;
#125451 = CARTESIAN_POINT ( 'NONE',  ( 18.59999999999999432, 1.162701749949165642, -142.1000000000000227 ) ) ;
#125452 = CIRCLE ( 'NONE', #141999, 0.09999999999999489853 ) ;
#125453 = CARTESIAN_POINT ( 'NONE',  ( -23.25000000000000000, 11.75000000001115552, -67.00000000000000000 ) ) ;
#125454 = CARTESIAN_POINT ( 'NONE',  ( -21.14999999999999858, 76.10000000001218723, -143.0637644362255401 ) ) ;
#125456 = EDGE_CURVE ( 'NONE', #120409, #152713, #65389, .T. ) ;
#125455 = CARTESIAN_POINT ( 'NONE',  ( -19.93974701750897083, 4.631764625248131928, 22.00000000173902137 ) ) ;
#125457 = CIRCLE ( 'NONE', #108703, 0.1999999999999896860 ) ;
#125459 = LINE ( 'NONE', #147581, #189588 ) ;
#125458 = CIRCLE ( 'NONE', #129724, 0.1000000000000028644 ) ;
#125460 = CIRCLE ( 'NONE', #217007, 0.1000000000000028644 ) ;
#125461 = ORIENTED_EDGE ( 'NONE', *, *, #257021, .T. ) ;
#125463 = DIRECTION ( 'NONE',  ( 0.000000000000000000, 0.2128009952263693050, -0.9770955615653296178 ) ) ;
#125462 = DIRECTION ( 'NONE',  ( -1.000000000000000000, 0.000000000000000000, 0.000000000000000000 ) ) ;
#125464 = AXIS2_PLACEMENT_3D ( 'NONE', #195331, #97452, #173226 ) ;
#125465 = CARTESIAN_POINT ( 'NONE',  ( 20.94999999999999929, -9.499999999988844479, -57.10603087734755690 ) ) ;
#125466 = DIRECTION ( 'NONE',  ( 0.000000000000000000, -1.000000000000000000, 0.000000000000000000 ) ) ;
#125467 = DIRECTION ( 'NONE',  ( 0.000000000000000000, 0.9126074666063771490, 0.4088369013363281623 ) ) ;
#125469 = EDGE_LOOP ( 'NONE', ( #109523, #96859, #171222, #233396 ) ) ;
#125468 = CARTESIAN_POINT ( 'NONE',  ( -18.59999999999999787, -9.480686695267820596, -207.9411151687577899 ) ) ;
#125471 = ORIENTED_EDGE ( 'NONE', *, *, #2597, .T. ) ;
#125470 = DIRECTION ( 'NONE',  ( 0.000000000000000000, 0.8814952561688444987, -0.4721928772777320149 ) ) ;
#125472 = CARTESIAN_POINT ( 'NONE',  ( 23.24999999999999289, 20.97908333644147660, -233.6079013178409411 ) ) ;
#125473 = DIRECTION ( 'NONE',  ( 1.000000000000000000, -0.000000000000000000, -0.000000000000000000 ) ) ;
#125474 = DIRECTION ( 'NONE',  ( -0.000000000000000000, 0.9579639084728149845, 0.2868887416116019384 ) ) ;
#125476 = EDGE_LOOP ( 'NONE', ( #12792, #84300, #23897, #66906 ) ) ;
#125475 = CARTESIAN_POINT ( 'NONE',  ( 20.94999999999999929, 8.776282895303632259, -79.15000000000004832 ) ) ;
#125477 = CARTESIAN_POINT ( 'NONE',  ( -20.85000000000000142, 68.97833521811203639, -132.6895420826271277 ) ) ;
#125478 = ORIENTED_EDGE ( 'NONE', *, *, #77318, .T. ) ;
#125479 = ORIENTED_EDGE ( 'NONE', *, *, #19245, .T. ) ;
#125480 = DIRECTION ( 'NONE',  ( -1.000000000000000000, -0.000000000000000000, -0.000000000000000000 ) ) ;
#125481 = CARTESIAN_POINT ( 'NONE',  ( 19.81427058490562132, 34.45565372986682462, -235.1336912300558311 ) ) ;
#125482 = ORIENTED_EDGE ( 'NONE', *, *, #205372, .T. ) ;
#125483 = DIRECTION ( 'NONE',  ( 1.073024830501117725E-15, -6.982962677686266711E-15, 1.000000000000000000 ) ) ;
#125484 = VECTOR ( 'NONE', #177172, 1000.000000000000000 ) ;
#125485 = ADVANCED_FACE ( 'NONE', ( #245321 ), #6877, .T. ) ;
#125486 = CARTESIAN_POINT ( 'NONE',  ( -21.14999999999999858, 1.115600667400684642E-11, -100.5000000000000284 ) ) ;
#125487 = VERTEX_POINT ( 'NONE', #88780 ) ;
#125488 = CARTESIAN_POINT ( 'NONE',  ( -16.87331047859649757, 66.05000000001153637, -48.67310748452439384 ) ) ;
#125490 = ORIENTED_EDGE ( 'NONE', *, *, #171103, .F. ) ;
#125489 = TOROIDAL_SURFACE ( 'NONE', #200504, 11.89999999999999858, 0.1000000000000000056 ) ;
#125491 = ORIENTED_EDGE ( 'NONE', *, *, #39522, .F. ) ;
#125492 = CARTESIAN_POINT ( 'NONE',  ( -21.11825140030087766, 61.00870122228366910, -234.1749742158648360 ) ) ;
#125493 = ORIENTED_EDGE ( 'NONE', *, *, #154511, .F. ) ;
#125494 = EDGE_CURVE ( 'NONE', #204482, #22587, #98415, .T. ) ;
#125495 = EDGE_LOOP ( 'NONE', ( #228333, #95118, #204645, #156889 ) ) ;
#125496 = EDGE_LOOP ( 'NONE', ( #230687, #40793, #243920, #113126 ) ) ;
#125498 = EDGE_CURVE ( 'NONE', #31603, #201851, #122815, .T. ) ;
#125497 = CARTESIAN_POINT ( 'NONE',  ( -21.14999999893415250, 11.75000000001115197, -73.84449534352643241 ) ) ;
#125499 = ORIENTED_EDGE ( 'NONE', *, *, #117319, .F. ) ;
#125500 = CARTESIAN_POINT ( 'NONE',  ( -23.25000000000000000, 76.00000000001190870, -103.0231074845243029 ) ) ;
#125501 = EDGE_LOOP ( 'NONE', ( #42236, #89355, #113965, #60104, #135430, #152635, #162347, #44516 ) ) ;
#125503 = VERTEX_POINT ( 'NONE', #227025 ) ;
#125502 = ORIENTED_EDGE ( 'NONE', *, *, #198737, .F. ) ;
#125504 = DIRECTION ( 'NONE',  ( -0.000000000000000000, -0.000000000000000000, -1.000000000000000000 ) ) ;
#125505 = CARTESIAN_POINT ( 'NONE',  ( -20.85000000106584750, 56.18110340670160952, -227.9302710413118973 ) ) ;
#125506 = CIRCLE ( 'NONE', #8984, 0.09999999999998898659 ) ;
#125508 = EDGE_CURVE ( 'NONE', #224268, #223315, #48384, .T. ) ;
#125507 = VERTEX_POINT ( 'NONE', #247877 ) ;
#125509 = AXIS2_PLACEMENT_3D ( 'NONE', #138994, #218548, #39968 ) ;
#125510 = AXIS2_PLACEMENT_3D ( 'NONE', #119305, #58012, #99704 ) ;
#125511 = EDGE_CURVE ( 'NONE', #40297, #729, #127505, .T. ) ;
#125512 = EDGE_CURVE ( 'NONE', #258015, #182460, #199636, .T. ) ;
#125513 = ORIENTED_EDGE ( 'NONE', *, *, #30, .F. ) ;
#125514 = CARTESIAN_POINT ( 'NONE',  ( -18.59999999999999787, 62.46832465249013921, -225.2232495205141731 ) ) ;
#125515 = CARTESIAN_POINT ( 'NONE',  ( -18.59999999999999787, -1.835859311443637010, -45.00443916879852679 ) ) ;
#125516 =( BOUNDED_SURFACE ( )  B_SPLINE_SURFACE ( 3, 2, ( 
 ( #201028, #170620, #71488 ),
 ( #106715, #147137, #89727 ),
 ( #29808, #186287, #28534 ),
 ( #7643, #121514, #101892 ),
 ( #87155, #181478, #161920 ),
 ( #247535, #130140, #169323 ),
 ( #2803, #68918, #62798 ),
 ( #31092, #82325, #241446 ),
 ( #149742, #126289, #108028 ),
 ( #187583, #142321, #221839 ),
 ( #190137, #229266, #50593 ),
 ( #70207, #209691, #166748 ) ),
 .UNSPECIFIED., .F., .F., .F. ) 
 B_SPLINE_SURFACE_WITH_KNOTS ( ( 4, 2, 2, 2, 2, 4 ),
 ( 3, 3 ),
 ( 3.174653483277205090, 3.943930578431714018, 4.713207673586222946, 5.482484768740731873, 5.867123316317986337, 6.251761863895240801 ),
 ( 0.000000000000000000, 1.000000000000000000 ),
 .UNSPECIFIED. ) 
 GEOMETRIC_REPRESENTATION_ITEM ( )  RATIONAL_B_SPLINE_SURFACE ( (
 ( 1.000000000000000000, 0.8659465255642114778, 1.000000000000000000),
 ( 1.000000000000000000, 0.8648614068487411322, 1.000000000000000000),
 ( 1.000000000000000000, 0.8489031841324523597, 1.000000000000000000),
 ( 1.000000000000000000, 0.7927507630160768315, 1.000000000000000000),
 ( 1.000000000000000000, 0.7523013859006951742, 1.000000000000000000),
 ( 1.000000000000000000, 0.6616226951198839190, 1.000000000000000000),
 ( 1.000000000000000000, 0.6112214368721479163, 1.000000000000000000),
 ( 1.000000000000000000, 0.5507684314500016498, 1.000000000000000000),
 ( 1.000000000000000000, 0.5333267243152196579, 1.000000000000000000),
 ( 1.000000000000000000, 0.5084565446481067452, 1.000000000000000000),
 ( 1.000000000000000000, 0.5010722703450574134, 1.000000000000000000),
 ( 1.000000000000000000, 0.5001234037138888588, 1.000000000000000000) ) ) 
 REPRESENTATION_ITEM ( '' )  SURFACE ( )  );
#125518 = EDGE_LOOP ( 'NONE', ( #132910, #114149, #36902, #107126 ) ) ;
#125517 = CARTESIAN_POINT ( 'NONE',  ( -20.00857864376270001, 9.150000000011157653, -88.15000000000004832 ) ) ;
#125519 = DIRECTION ( 'NONE',  ( 1.000000000000000000, 0.000000000000000000, -0.000000000000000000 ) ) ;
#125520 = ORIENTED_EDGE ( 'NONE', *, *, #35791, .T. ) ;
#125521 = ADVANCED_FACE ( 'NONE', ( #69260 ), #194161, .F. ) ;
#125522 = CARTESIAN_POINT ( 'NONE',  ( 18.59999999999999076, 6.450000000011156587, -177.5170271704400022 ) ) ;
#125523 = CARTESIAN_POINT ( 'NONE',  ( 18.49999999999999289, 65.79142135392881130, -111.8206006188944315 ) ) ;
#125524 = ORIENTED_EDGE ( 'NONE', *, *, #76817, .F. ) ;
#125525 = CARTESIAN_POINT ( 'NONE',  ( -20.94999999999999929, 7.633102355717365839, -241.5185714324494484 ) ) ;
#125526 = DIRECTION ( 'NONE',  ( 0.000000000000000000, 0.000000000000000000, -1.000000000000000000 ) ) ;
#125527 = ADVANCED_FACE ( 'NONE', ( #251732 ), #93936, .F. ) ;
#125528 = CIRCLE ( 'NONE', #246146, 7.720710678118678061 ) ;
#125529 = ORIENTED_EDGE ( 'NONE', *, *, #85308, .F. ) ;
#125530 = DIRECTION ( 'NONE',  ( 1.000000000000000000, 0.000000000000000000, 0.000000000000000000 ) ) ;
#125531 = VERTEX_POINT ( 'NONE', #34010 ) ;
#125533 = ORIENTED_EDGE ( 'NONE', *, *, #140393, .T. ) ;
#125532 = EDGE_LOOP ( 'NONE', ( #209012, #222695, #28265, #221896 ) ) ;
#125534 = VERTEX_POINT ( 'NONE', #73130 ) ;
#125535 = CARTESIAN_POINT ( 'NONE',  ( -20.94999999999999929, 77.83534155023700407, -191.9679561919613491 ) ) ;
#125536 = ORIENTED_EDGE ( 'NONE', *, *, #205891, .T. ) ;
#125537 = DIRECTION ( 'NONE',  ( -0.000000000000000000, 1.000000000000000000, 0.000000000000000000 ) ) ;
#125538 = VERTEX_POINT ( 'NONE', #52226 ) ;
#125539 = CARTESIAN_POINT ( 'NONE',  ( 21.13461538461538325, 22.21093039075207898, -231.7318303787629930 ) ) ;
#125540 = CARTESIAN_POINT ( 'NONE',  ( 20.95512820512820795, 43.44946199836419254, -234.8678826325710531 ) ) ;
#125541 = ADVANCED_FACE ( 'NONE', ( #150088 ), #73550, .T. ) ;
#125542 = ORIENTED_EDGE ( 'NONE', *, *, #99914, .T. ) ;
#125543 = VECTOR ( 'NONE', #170130, 1000.000000000000000 ) ;
#125544 = AXIS2_PLACEMENT_3D ( 'NONE', #122207, #162623, #43943 ) ;
#125545 = ORIENTED_EDGE ( 'NONE', *, *, #82829, .T. ) ;
#125546 = AXIS2_PLACEMENT_3D ( 'NONE', #98673, #235652, #196530 ) ;
#125547 = VERTEX_POINT ( 'NONE', #173535 ) ;
#125548 = ADVANCED_FACE ( 'NONE', ( #54801 ), #134331, .T. ) ;
#125549 = DIRECTION ( 'NONE',  ( 0.000000000000000000, 6.577889128801591149E-15, -1.000000000000000000 ) ) ;
#125550 = ORIENTED_EDGE ( 'NONE', *, *, #106231, .F. ) ;
#125551 = FACE_OUTER_BOUND ( 'NONE', #127677, .T. ) ;
#125553 = ORIENTED_EDGE ( 'NONE', *, *, #210911, .F. ) ;
#125552 = LINE ( 'NONE', #245513, #104283 ) ;
#125554 = CARTESIAN_POINT ( 'NONE',  ( -21.64999999999999858, 66.65000000001182912, -82.17310748452437963 ) ) ;
#125555 = DIRECTION ( 'NONE',  ( 1.000000000000000000, 1.110223024625155531E-13, 0.000000000000000000 ) ) ;
#125556 = DIRECTION ( 'NONE',  ( 1.000000000000000000, 0.000000000000000000, 0.000000000000000000 ) ) ;
#125557 = AXIS2_PLACEMENT_3D ( 'NONE', #71511, #191469, #251402 ) ;
#125558 = DIRECTION ( 'NONE',  ( 0.000000000000000000, -6.982962677686266711E-15, 1.000000000000000000 ) ) ;
#125559 = LINE ( 'NONE', #186834, #186060 ) ;
#125561 = DIRECTION ( 'NONE',  ( 1.000000000000000000, 1.110223024625155531E-13, 0.000000000000000000 ) ) ;
#125560 = CARTESIAN_POINT ( 'NONE',  ( -21.05000000000000071, 0.03363273534480391153, -60.74118280531856584 ) ) ;
#125562 = DIRECTION ( 'NONE',  ( 3.616040088954497272E-32, -1.224646799147352961E-16, 1.000000000000000000 ) ) ;
#125563 = CARTESIAN_POINT ( 'NONE',  ( 21.00000000000000000, 1.212568896937007645, -7.800000000000000711 ) ) ;
#125564 = DIRECTION ( 'NONE',  ( 0.000000000000000000, -1.000000000000000000, 0.000000000000000000 ) ) ;
#125565 = DIRECTION ( 'NONE',  ( 1.000000000000000000, -3.265361837132813093E-16, -2.280189983783949500E-30 ) ) ;
#125566 = ORIENTED_EDGE ( 'NONE', *, *, #219747, .F. ) ;
#125567 = ADVANCED_FACE ( 'NONE', ( #114789 ), #211327, .T. ) ;
#125569 = VERTEX_POINT ( 'NONE', #32729 ) ;
#125568 = DIRECTION ( 'NONE',  ( 0.000000000000000000, 0.2617529984165180013, 0.9651348961777117541 ) ) ;
#125570 = ORIENTED_EDGE ( 'NONE', *, *, #124385, .T. ) ;
#125571 = DIRECTION ( 'NONE',  ( 0.000000000000000000, -0.9999631594459053030, -0.008583690987162452199 ) ) ;
#125572 = AXIS2_PLACEMENT_3D ( 'NONE', #90220, #232347, #133224 ) ;
#125573 = ADVANCED_FACE ( 'NONE', ( #112240 ), #194356, .T. ) ;
#125574 = CARTESIAN_POINT ( 'NONE',  ( 20.58091095332318332, 9.018470153363605135, -142.4186501821585864 ) ) ;
#125575 = DIRECTION ( 'NONE',  ( 1.000000000000000000, -0.000000000000000000, -0.000000000000000000 ) ) ;
#125576 = ORIENTED_EDGE ( 'NONE', *, *, #99702, .T. ) ;
#125577 = EDGE_CURVE ( 'NONE', #27728, #193883, #189200, .T. ) ;
#125578 = EDGE_CURVE ( 'NONE', #148744, #39283, #174813, .T. ) ;
#125579 = DIRECTION ( 'NONE',  ( 0.000000000000000000, -7.109473446599835262E-15, 1.000000000000000000 ) ) ;
#125580 = VECTOR ( 'NONE', #29605, 1000.000000000000000 ) ;
#125581 = CARTESIAN_POINT ( 'NONE',  ( 20.94999999999999929, 67.23127455305835554, -235.8551265064784559 ) ) ;
#125582 = ORIENTED_EDGE ( 'NONE', *, *, #77243, .T. ) ;
#125583 = DIRECTION ( 'NONE',  ( 1.000000000000000000, -2.952720810173289112E-16, -2.061873921506763405E-30 ) ) ;
#125584 = AXIS2_PLACEMENT_3D ( 'NONE', #197156, #163190, #138448 ) ;
#125585 = DIRECTION ( 'NONE',  ( 1.000000000000000000, 0.000000000000000000, 0.000000000000000000 ) ) ;
#125586 = EDGE_CURVE ( 'NONE', #77358, #171611, #90071, .T. ) ;
#125587 = CIRCLE ( 'NONE', #121366, 0.1000000000000124678 ) ;
#125588 = CARTESIAN_POINT ( 'NONE',  ( -23.25000000000000355, 70.35000000001264198, -194.2731074845243882 ) ) ;
#125590 = ORIENTED_EDGE ( 'NONE', *, *, #151848, .T. ) ;
#125589 = DIRECTION ( 'NONE',  ( -1.000000000000000000, 0.000000000000000000, 0.000000000000000000 ) ) ;
#125591 = CARTESIAN_POINT ( 'NONE',  ( -20.65000000000000568, 7.250000000011138646, -176.7499999999999716 ) ) ;
#125592 = CARTESIAN_POINT ( 'NONE',  ( -20.85000000000000142, -1.835859311432481045, -179.0044391687985410 ) ) ;
#125593 = DIRECTION ( 'NONE',  ( 3.616040088954497272E-32, -1.224646799147352961E-16, 1.000000000000000000 ) ) ;
#125594 = CARTESIAN_POINT ( 'NONE',  ( -21.05000000000000071, 1.115653327213047955E-11, -29.20000000000004547 ) ) ;
#125595 = ORIENTED_EDGE ( 'NONE', *, *, #1133, .F. ) ;
#125596 = DIRECTION ( 'NONE',  ( 0.000000000000000000, 0.4999999999999088507, -0.8660254037844913322 ) ) ;
#125597 = CYLINDRICAL_SURFACE ( 'NONE', #206883, 7.899999999999990585 ) ;
#125599 = CYLINDRICAL_SURFACE ( 'NONE', #120843, 0.09999999999998898659 ) ;
#125598 = DIRECTION ( 'NONE',  ( 0.000000000000000000, 0.000000000000000000, -1.000000000000000000 ) ) ;
#125600 = PLANE ( 'NONE',  #224527 ) ;
#125601 = CARTESIAN_POINT ( 'NONE',  ( 18.39999999999998082, 64.52683809664912928, -60.27310748452440947 ) ) ;
#125603 = DIRECTION ( 'NONE',  ( -1.000000000000000000, -0.000000000000000000, -0.000000000000000000 ) ) ;
#125602 = CIRCLE ( 'NONE', #187981, 0.09999999999999538425 ) ;
#125604 = DIRECTION ( 'NONE',  ( 0.000000000000000000, -2.609498562153145121E-14, 1.000000000000000000 ) ) ;
#125605 = DIRECTION ( 'NONE',  ( -0.000000000000000000, -6.982962677686266711E-15, 1.000000000000000000 ) ) ;
#125606 = DIRECTION ( 'NONE',  ( 4.239556034732056743E-17, -0.1298341882520022694, -0.9915357197604852679 ) ) ;
#125607 = AXIS2_PLACEMENT_3D ( 'NONE', #98808, #156292, #217490 ) ;
#125608 = ORIENTED_EDGE ( 'NONE', *, *, #175466, .T. ) ;
#125609 = ORIENTED_EDGE ( 'NONE', *, *, #218307, .F. ) ;
#125611 =( BOUNDED_CURVE ( )  B_SPLINE_CURVE ( 3, ( #58932, #62818, #23729, #158116 ),
 .UNSPECIFIED., .F., .F. ) 
 B_SPLINE_CURVE_WITH_KNOTS ( ( 4, 4 ),
 ( 3.432212674861196522, 3.693332928900581624 ),
 .UNSPECIFIED. ) 
 CURVE ( )  GEOMETRIC_REPRESENTATION_ITEM ( )  RATIONAL_B_SPLINE_CURVE ( ( 1.000000000000000000, 0.9943260843901261525, 0.9943260843901261525, 1.000000000000000000 ) ) 
 REPRESENTATION_ITEM ( '' )  );
#125610 = CIRCLE ( 'NONE', #142178, 12.87500000000000178 ) ;
#125612 = ORIENTED_EDGE ( 'NONE', *, *, #251888, .F. ) ;
#125613 = CARTESIAN_POINT ( 'NONE',  ( 18.39999999999999858, 87.01908966642815813, -199.5693496768551825 ) ) ;
#125614 = DIRECTION ( 'NONE',  ( 0.000000000000000000, 0.000000000000000000, -1.000000000000000000 ) ) ;
#125615 = EDGE_CURVE ( 'NONE', #105539, #52458, #219012, .T. ) ;
#125616 = ORIENTED_EDGE ( 'NONE', *, *, #12072, .T. ) ;
#125617 = EDGE_CURVE ( 'NONE', #102370, #81005, #112328, .T. ) ;
#125618 = AXIS2_PLACEMENT_3D ( 'NONE', #201143, #119054, #95619 ) ;
#125619 = B_SPLINE_CURVE_WITH_KNOTS ( 'NONE', 3,
 ( #210419, #91742, #168765, #33095, #133434, #227389, #68330, #249543, #167450, #12224 ),
 .UNSPECIFIED., .F., .F.,
 ( 4, 3, 3, 4 ),
 ( 7.632826238683052976E-06, 4.756916949875583575E-05, 9.484459048150214273E-05, 0.0001435500935099850669 ),
 .UNSPECIFIED. ) ;
#125620 = VERTEX_POINT ( 'NONE', #56073 ) ;
#125621 = EDGE_CURVE ( 'NONE', #77073, #20758, #185948, .T. ) ;
#125623 = VERTEX_POINT ( 'NONE', #239882 ) ;
#125622 = AXIS2_PLACEMENT_3D ( 'NONE', #164814, #46135, #141382 ) ;
#125624 = DIRECTION ( 'NONE',  ( 1.000000000000000000, 0.000000000000000000, 0.000000000000000000 ) ) ;
#125625 = CIRCLE ( 'NONE', #109045, 0.1000000000000052097 ) ;
#125626 = VERTEX_POINT ( 'NONE', #116086 ) ;
#125627 = AXIS2_PLACEMENT_3D ( 'NONE', #58327, #98724, #257783 ) ;
#125628 = CARTESIAN_POINT ( 'NONE',  ( 18.59999999999999787, 48.05114133249968944, -246.4758750954581785 ) ) ;
#125629 = CARTESIAN_POINT ( 'NONE',  ( 18.59999999999999787, 87.75000000001179501, -81.67310748452422331 ) ) ;
#125631 = DIRECTION ( 'NONE',  ( 0.000000000000000000, 0.8371762388950346745, 0.5469332180710581026 ) ) ;
#125630 = AXIS2_PLACEMENT_3D ( 'NONE', #110863, #178573, #101534 ) ;
#125632 = CARTESIAN_POINT ( 'NONE',  ( -21.29999999999995808, 1.148907358139439339E-11, -201.0000000000015064 ) ) ;
#125633 = DIRECTION ( 'NONE',  ( 0.000000000000000000, -7.086529944415886769E-15, 1.000000000000000000 ) ) ;
#125634 = CARTESIAN_POINT ( 'NONE',  ( -20.65000000000000568, 28.93140779147704933, -237.1870821964559184 ) ) ;
#125635 = DIRECTION ( 'NONE',  ( 1.000000000000000000, -0.000000000000000000, -0.000000000000000000 ) ) ;
#125637 = ORIENTED_EDGE ( 'NONE', *, *, #54810, .T. ) ;
#125636 = FACE_OUTER_BOUND ( 'NONE', #36345, .T. ) ;
#125639 = FACE_OUTER_BOUND ( 'NONE', #256361, .T. ) ;
#125638 = CARTESIAN_POINT ( 'NONE',  ( 21.05000000000000071, -11.64999999998883595, -170.3999999999999773 ) ) ;
#125640 = LINE ( 'NONE', #63090, #19940 ) ;
#125641 = EDGE_LOOP ( 'NONE', ( #28944, #183136, #192862, #44172 ) ) ;
#125642 = LINE ( 'NONE', #218630, #214741 ) ;
#125643 = CYLINDRICAL_SURFACE ( 'NONE', #35594, 0.1000000000000124678 ) ;
#125644 = VERTEX_POINT ( 'NONE', #138181 ) ;
#125645 = CARTESIAN_POINT ( 'NONE',  ( -21.10257677756356998, 6.398381742543890915, -33.47504925043203627 ) ) ;
#125646 = ADVANCED_FACE ( 'NONE', ( #176077 ), #177612, .T. ) ;
#125647 = CARTESIAN_POINT ( 'NONE',  ( 20.04142135623730070, 11.65000000001115943, -155.7499999999999716 ) ) ;
#125648 = TOROIDAL_SURFACE ( 'NONE', #200679, 11.70000000000000639, 0.1000000000000000056 ) ;
#125649 = VERTEX_POINT ( 'NONE', #139471 ) ;
#125650 = CARTESIAN_POINT ( 'NONE',  ( 21.09096482362047809, 6.363544365415554793, -66.96055172122596844 ) ) ;
#125651 = DIRECTION ( 'NONE',  ( 1.000000000000000000, 0.000000000000000000, -0.000000000000000000 ) ) ;
#125652 = CARTESIAN_POINT ( 'NONE',  ( 21.14999999999999503, 64.35000000001194564, -103.0231074845244024 ) ) ;
#125653 = EDGE_CURVE ( 'NONE', #154965, #141135, #223345, .T. ) ;
#125654 = DIRECTION ( 'NONE',  ( 0.000000000000000000, -7.056502275159890043E-15, 1.000000000000000000 ) ) ;
#125655 = ORIENTED_EDGE ( 'NONE', *, *, #245933, .T. ) ;
#125656 = ORIENTED_EDGE ( 'NONE', *, *, #82528, .T. ) ;
#125657 = EDGE_CURVE ( 'NONE', #116815, #92883, #110933, .T. ) ;
#125658 = CARTESIAN_POINT ( 'NONE',  ( 23.24999999999999645, 1.115600667400684642E-11, -167.5000000000000284 ) ) ;
#125659 = DIRECTION ( 'NONE',  ( -2.952720810173288619E-16, 1.000000000000000000, 0.000000000000000000 ) ) ;
#125660 = DIRECTION ( 'NONE',  ( 1.000000000000000000, 0.000000000000000000, 0.000000000000000000 ) ) ;
#125661 = EDGE_CURVE ( 'NONE', #120433, #223762, #256618, .T. ) ;
#125662 = CARTESIAN_POINT ( 'NONE',  ( 21.11101077988997332, 6.423684734737197921, -167.4847147310856599 ) ) ;
#125663 = CARTESIAN_POINT ( 'NONE',  ( -20.94999999999999929, -1.162701749926853712, -108.6000000000000227 ) ) ;
#125664 = ORIENTED_EDGE ( 'NONE', *, *, #161146, .T. ) ;
#125665 = CARTESIAN_POINT ( 'NONE',  ( -5.999999999999938716, 64.75000000001119815, -26.02310748452479316 ) ) ;
#125666 = ADVANCED_FACE ( 'NONE', ( #156521 ), #31852, .T. ) ;
#125667 = CIRCLE ( 'NONE', #113205, 4.299999999999956302 ) ;
#125669 = ORIENTED_EDGE ( 'NONE', *, *, #52829, .T. ) ;
#125668 = DIRECTION ( 'NONE',  ( 1.000000000000000000, 0.000000000000000000, 0.000000000000000000 ) ) ;
#125670 = FACE_OUTER_BOUND ( 'NONE', #239329, .T. ) ;
#125672 = EDGE_CURVE ( 'NONE', #249995, #236891, #178648, .T. ) ;
#125671 = EDGE_CURVE ( 'NONE', #92384, #247087, #56912, .T. ) ;
#125673 = DIRECTION ( 'NONE',  ( -0.7070776581708965169, -0.7071359030027827286, -0.000000000000000000 ) ) ;
#125674 = CARTESIAN_POINT ( 'NONE',  ( -21.11101077989000174, 75.98471473109741225, -75.94679221925045454 ) ) ;
#125675 = CARTESIAN_POINT ( 'NONE',  ( -20.65000000000000568, 70.35000000001224407, -149.1731074845243938 ) ) ;
#125676 = CARTESIAN_POINT ( 'NONE',  ( -21.64999999999999858, 7.250000000011148416, -146.2500000000000284 ) ) ;
#125678 = VERTEX_POINT ( 'NONE', #238586 ) ;
#125677 = CARTESIAN_POINT ( 'NONE',  ( -17.11825945287482753, 9.950000000011138823, -146.7500000000000284 ) ) ;
#125679 = DIRECTION ( 'NONE',  ( 1.000000000000000000, 0.000000000000000000, 0.000000000000000000 ) ) ;
#125680 = CARTESIAN_POINT ( 'NONE',  ( -18.59999999999999787, 65.66751761918722252, -164.4282609406112670 ) ) ;
#125681 = CARTESIAN_POINT ( 'NONE',  ( 18.79999999999999716, -8.150000000000007461, 32.89999999999999858 ) ) ;
#125682 = DIRECTION ( 'NONE',  ( 0.000000000000000000, 0.2965989261549568656, 0.9550021345545394169 ) ) ;
#125683 = VERTEX_POINT ( 'NONE', #160367 ) ;
#125684 = LINE ( 'NONE', #207827, #242752 ) ;
#125685 = CARTESIAN_POINT ( 'NONE',  ( -18.59999999999999787, 5.341242990002807112, -157.6933497935119419 ) ) ;
#125686 = DIRECTION ( 'NONE',  ( -1.000000000000000000, -0.000000000000000000, 0.000000000000000000 ) ) ;
#125688 = AXIS2_PLACEMENT_3D ( 'NONE', #134289, #75644, #135576 ) ;
#125687 = DIRECTION ( 'NONE',  ( -1.652117596168391700E-15, 1.000000000000000000, 6.982962677686266711E-15 ) ) ;
#125689 = ORIENTED_EDGE ( 'NONE', *, *, #52095, .T. ) ;
#125691 = AXIS2_PLACEMENT_3D ( 'NONE', #252916, #136819, #168625 ) ;
#125690 = CARTESIAN_POINT ( 'NONE',  ( -16.87683809663752399, 9.865889849343686180, -87.23257319293058742 ) ) ;
#125692 = ADVANCED_FACE ( 'NONE', ( #140773 ), #121252, .F. ) ;
#125693 = EDGE_CURVE ( 'NONE', #150591, #191015, #200747, .T. ) ;
#125694 = ORIENTED_EDGE ( 'NONE', *, *, #209710, .T. ) ;
#125695 = AXIS2_PLACEMENT_3D ( 'NONE', #219371, #61594, #155599 ) ;
#125696 = DIRECTION ( 'NONE',  ( 1.000000000000000000, -0.000000000000000000, -0.000000000000000000 ) ) ;
#125697 = FACE_OUTER_BOUND ( 'NONE', #107359, .T. ) ;
#125698 = EDGE_CURVE ( 'NONE', #91270, #257751, #186127, .T. ) ;
#125699 = CARTESIAN_POINT ( 'NONE',  ( 21.14999999999999858, 44.24607648097409651, -236.5241869975821487 ) ) ;
#125700 = EDGE_LOOP ( 'NONE', ( #211438, #228678, #25552, #34360 ) ) ;
#125701 = DIRECTION ( 'NONE',  ( 0.000000000000000000, -1.000000000000000000, -0.000000000000000000 ) ) ;
#125702 = EDGE_CURVE ( 'NONE', #243534, #213669, #98595, .T. ) ;
#125703 = AXIS2_PLACEMENT_3D ( 'NONE', #247396, #248697, #243553 ) ;
#125704 = CARTESIAN_POINT ( 'NONE',  ( 21.12400247839513767, 13.08273057273256335, -210.6878773030995831 ) ) ;
#125705 = EDGE_CURVE ( 'NONE', #30650, #135846, #15276, .T. ) ;
#125706 = DIRECTION ( 'NONE',  ( 0.000000000000000000, 3.552713678800442159E-15, -1.000000000000000000 ) ) ;
#125707 = FACE_OUTER_BOUND ( 'NONE', #161572, .T. ) ;
#125708 = VERTEX_POINT ( 'NONE', #241172 ) ;
#125710 = ORIENTED_EDGE ( 'NONE', *, *, #163832, .F. ) ;
#125709 = CARTESIAN_POINT ( 'NONE',  ( -20.54999999999999716, -8.730841121484173684, -177.0980747189843214 ) ) ;
#125711 = ORIENTED_EDGE ( 'NONE', *, *, #51727, .F. ) ;
#125712 = CARTESIAN_POINT ( 'NONE',  ( -20.85000000000000142, 7.021664781900089913, -37.23356540189728747 ) ) ;
#125713 = ORIENTED_EDGE ( 'NONE', *, *, #196893, .F. ) ;
#125714 = CARTESIAN_POINT ( 'NONE',  ( 21.05000000000000071, 60.94483358488582070, -234.0465764481390636 ) ) ;
#125715 = FACE_OUTER_BOUND ( 'NONE', #109721, .T. ) ;
#125716 = DIRECTION ( 'NONE',  ( -0.000000000000000000, 0.2605042016806385363, 0.9654727137038795481 ) ) ;
#125717 = ORIENTED_EDGE ( 'NONE', *, *, #71944, .F. ) ;
#125718 = EDGE_CURVE ( 'NONE', #224475, #70441, #84599, .T. ) ;
#125719 = LINE ( 'NONE', #180568, #223812 ) ;
#125720 = CARTESIAN_POINT ( 'NONE',  ( 20.74625933824090751, 8.882913521095439080, -42.05517102412104435 ) ) ;
#125721 = ORIENTED_EDGE ( 'NONE', *, *, #28206, .F. ) ;
#125722 = DIRECTION ( 'NONE',  ( 0.000000000000000000, 0.000000000000000000, -1.000000000000000000 ) ) ;
#125724 = ORIENTED_EDGE ( 'NONE', *, *, #3560, .T. ) ;
#125723 = CARTESIAN_POINT ( 'NONE',  ( -20.64999999999999858, 26.26625913865096251, -241.7830784256010759 ) ) ;
#125725 = VECTOR ( 'NONE', #135992, 1000.000000000000000 ) ;
#125726 = CIRCLE ( 'NONE', #175630, 0.09999999999999817368 ) ;
#125727 = CARTESIAN_POINT ( 'NONE',  ( -23.25000000000000000, -4.914013037343267776, -233.1828366659746905 ) ) ;
#125728 = AXIS2_PLACEMENT_3D ( 'NONE', #49999, #70881, #150404 ) ;
#125729 = EDGE_CURVE ( 'NONE', #224623, #65906, #244385, .T. ) ;
#125730 = ORIENTED_EDGE ( 'NONE', *, *, #9887, .T. ) ;
#125731 = DIRECTION ( 'NONE',  ( 1.000000000000000000, 0.000000000000000000, 0.000000000000000000 ) ) ;
#125732 = CARTESIAN_POINT ( 'NONE',  ( -13.43673303185029333, 66.55335100938319215, -121.4339441886011883 ) ) ;
#125733 = DIRECTION ( 'NONE',  ( 0.000000000000000000, 0.000000000000000000, -1.000000000000000000 ) ) ;
#125734 = ORIENTED_EDGE ( 'NONE', *, *, #62454, .F. ) ;
#125735 = CARTESIAN_POINT ( 'NONE',  ( 18.39999999999997371, 64.52683809665003878, -179.2731074845244450 ) ) ;
#125736 = ADVANCED_FACE ( 'NONE', ( #29518 ), #102901, .T. ) ;
#125737 = DIRECTION ( 'NONE',  ( -0.000000000000000000, -0.3848449534832868446, -0.9229812358755982160 ) ) ;
#125738 = VECTOR ( 'NONE', #165145, 1000.000000000000000 ) ;
#125739 = EDGE_LOOP ( 'NONE', ( #20105, #148777, #44446, #133960 ) ) ;
#125740 = ORIENTED_EDGE ( 'NONE', *, *, #167585, .T. ) ;
#125741 = CARTESIAN_POINT ( 'NONE',  ( 20.94999999999999929, 69.35000000001151932, -48.27310748452436684 ) ) ;
#125742 = ORIENTED_EDGE ( 'NONE', *, *, #47982, .F. ) ;
#125743 = LINE ( 'NONE', #183177, #234969 ) ;
#125744 = DIRECTION ( 'NONE',  ( -1.000000000000000000, -0.000000000000000000, -0.000000000000000000 ) ) ;
#125745 = AXIS2_PLACEMENT_3D ( 'NONE', #113354, #151206, #35140 ) ;
#125747 = ORIENTED_EDGE ( 'NONE', *, *, #175227, .F. ) ;
#125746 = CARTESIAN_POINT ( 'NONE',  ( 21.05000000000000071, 11.65000000001116298, -160.4851942293460638 ) ) ;
#125748 = FACE_OUTER_BOUND ( 'NONE', #137645, .T. ) ;
#125749 = FACE_OUTER_BOUND ( 'NONE', #66801, .T. ) ;
#125750 = DIRECTION ( 'NONE',  ( 0.000000000000000000, 0.2128009952263607285, -0.9770955615653316162 ) ) ;
#125751 = CARTESIAN_POINT ( 'NONE',  ( -20.64999999999999858, 0.000000000000000000, 0.000000000000000000 ) ) ;
#125752 = DIRECTION ( 'NONE',  ( 0.000000000000000000, -1.000000000000000000, 0.000000000000000000 ) ) ;
#125753 = SPHERICAL_SURFACE ( 'NONE', #225170, 0.1000000000000000056 ) ;
#125754 = AXIS2_PLACEMENT_3D ( 'NONE', #183698, #165417, #164137 ) ;
#125755 = CARTESIAN_POINT ( 'NONE',  ( -18.59999999999999787, 0.000000000000000000, -33.50000000000000000 ) ) ;
#125756 = DIRECTION ( 'NONE',  ( 1.000000000000000000, 0.000000000000000000, 0.000000000000000000 ) ) ;
#125758 = VERTEX_POINT ( 'NONE', #24706 ) ;
#125757 = LINE ( 'NONE', #61949, #140257 ) ;
#125759 = FACE_OUTER_BOUND ( 'NONE', #30912, .T. ) ;
#125760 = CIRCLE ( 'NONE', #217694, 11.80000000000001670 ) ;
#125761 = ORIENTED_EDGE ( 'NONE', *, *, #162795, .F. ) ;
#125762 = CIRCLE ( 'NONE', #121524, 4.149999999999987033 ) ;
#125763 = CIRCLE ( 'NONE', #13353, 0.9750000000000036415 ) ;
#125764 = CARTESIAN_POINT ( 'NONE',  ( 18.49999999999999645, 18.14639373905162145, -237.6648341169113792 ) ) ;
#125765 = AXIS2_PLACEMENT_3D ( 'NONE', #126305, #106733, #186302 ) ;
#125766 = DIRECTION ( 'NONE',  ( 1.000000000000000000, 0.000000000000000000, 0.000000000000000000 ) ) ;
#125767 = CIRCLE ( 'NONE', #133962, 11.80000000000000249 ) ;
#125768 = DIRECTION ( 'NONE',  ( -1.000000000000000000, -0.000000000000000000, -0.000000000000000000 ) ) ;
#125769 = CARTESIAN_POINT ( 'NONE',  ( 20.19326291201646129, 65.84393901210869160, -195.7612456769175253 ) ) ;
#125770 = CYLINDRICAL_SURFACE ( 'NONE', #72246, 0.09999999999999939493 ) ;
#125771 = CIRCLE ( 'NONE', #59109, 0.5000000000000004441 ) ;
#125772 = ORIENTED_EDGE ( 'NONE', *, *, #18641, .T. ) ;
#125773 = DIRECTION ( 'NONE',  ( 0.000000000000000000, 6.982962677686266711E-15, -1.000000000000000000 ) ) ;
#125774 = AXIS2_PLACEMENT_3D ( 'NONE', #60507, #220873, #117920 ) ;
#125775 = EDGE_CURVE ( 'NONE', #161820, #152553, #122505, .T. ) ;
#125776 = DIRECTION ( 'NONE',  ( 1.000000000000000000, -2.849773892568378313E-16, 7.728835255496647986E-17 ) ) ;
#125777 = VECTOR ( 'NONE', #149522, 1000.000000000000000 ) ;
#125778 = ORIENTED_EDGE ( 'NONE', *, *, #66430, .F. ) ;
#125779 = VECTOR ( 'NONE', #21882, 1000.000000000000000 ) ;
#125780 = CARTESIAN_POINT ( 'NONE',  ( 21.04999999999999716, 75.94851711813100792, -209.8232873024375635 ) ) ;
#125781 = AXIS2_PLACEMENT_3D ( 'NONE', #2169, #183404, #102533 ) ;
#125782 = DIRECTION ( 'NONE',  ( 1.000000000000000000, 0.000000000000000000, 0.000000000000000000 ) ) ;
#125783 = EDGE_LOOP ( 'NONE', ( #200666, #210960, #74554, #202825 ) ) ;
#125784 = CARTESIAN_POINT ( 'NONE',  ( -18.50000000000000000, 44.18876898710608003, -236.1516686502934590 ) ) ;
#125785 = ORIENTED_EDGE ( 'NONE', *, *, #196254, .F. ) ;
#125787 = CIRCLE ( 'NONE', #871, 0.09999999999998898659 ) ;
#125786 = DIRECTION ( 'NONE',  ( 1.000000000000000000, 0.000000000000000000, 0.000000000000000000 ) ) ;
#125788 = ORIENTED_EDGE ( 'NONE', *, *, #236314, .T. ) ;
#125789 = EDGE_CURVE ( 'NONE', #131079, #110771, #184962, .T. ) ;
#125791 = EDGE_CURVE ( 'NONE', #108350, #155798, #219425, .T. ) ;
#125790 = CARTESIAN_POINT ( 'NONE',  ( 18.59999999999999076, 0.000000000000000000, -33.50000000000000000 ) ) ;
#125792 = DIRECTION ( 'NONE',  ( 0.000000000000000000, 0.3999834006488773852, 0.9165223833629813077 ) ) ;
#125793 = ORIENTED_EDGE ( 'NONE', *, *, #104963, .T. ) ;
#125794 = EDGE_LOOP ( 'NONE', ( #95291, #186850, #68966 ) ) ;
#125795 = DIRECTION ( 'NONE',  ( -1.000000000000000000, 0.000000000000000000, 0.000000000000000000 ) ) ;
#125796 = ORIENTED_EDGE ( 'NONE', *, *, #190774, .T. ) ;
#125797 = AXIS2_PLACEMENT_3D ( 'NONE', #248263, #189585, #50054 ) ;
#125798 = CARTESIAN_POINT ( 'NONE',  ( 20.95512828230159030, 67.12384868768731394, -191.3206772190213485 ) ) ;
#125800 = ORIENTED_EDGE ( 'NONE', *, *, #161407, .T. ) ;
#125799 = CIRCLE ( 'NONE', #4980, 0.1000000000000028644 ) ;
#125801 = AXIS2_PLACEMENT_3D ( 'NONE', #127018, #47455, #229966 ) ;
#125802 = CIRCLE ( 'NONE', #71670, 0.1000000000000032391 ) ;
#125803 = ADVANCED_FACE ( 'NONE', ( #202034 ), #107013, .T. ) ;
#125804 = EDGE_CURVE ( 'NONE', #170796, #8311, #188552, .T. ) ;
#125805 = ORIENTED_EDGE ( 'NONE', *, *, #173026, .T. ) ;
#125806 = PLANE ( 'NONE',  #211905 ) ;
#125807 = CARTESIAN_POINT ( 'NONE',  ( -21.05000000000000071, 77.83534155023646406, -124.8679561919613121 ) ) ;
#125808 = CARTESIAN_POINT ( 'NONE',  ( 20.12500000000000000, 9.749999999999998224, -8.111771282114276005 ) ) ;
#125809 = EDGE_CURVE ( 'NONE', #159302, #216065, #252752, .T. ) ;
#125810 = DIRECTION ( 'NONE',  ( 0.000000000000000000, 0.000000000000000000, -1.000000000000000000 ) ) ;
#125811 = CARTESIAN_POINT ( 'NONE',  ( -13.54795643572458985, 66.54933111084503139, -188.4675609943170400 ) ) ;
#125812 = DIRECTION ( 'NONE',  ( 0.000000000000000000, 0.000000000000000000, -1.000000000000000000 ) ) ;
#125813 = ORIENTED_EDGE ( 'NONE', *, *, #218045, .T. ) ;
#125814 = DIRECTION ( 'NONE',  ( 0.000000000000000000, 0.7397360091702792628, -0.6728971962616790981 ) ) ;
#125815 = CARTESIAN_POINT ( 'NONE',  ( -23.25000000000000000, 76.00000000001244871, -170.0231074845243597 ) ) ;
#125816 = EDGE_CURVE ( 'NONE', #97714, #172097, #82042, .T. ) ;
#125817 = CARTESIAN_POINT ( 'NONE',  ( 20.85000000000000142, 67.84340367245323478, -228.0791829662263410 ) ) ;
#125818 = ORIENTED_EDGE ( 'NONE', *, *, #143676, .F. ) ;
#125820 = CARTESIAN_POINT ( 'NONE',  ( -21.13422380239058995, 76.00000000001200817, -109.5164339993299620 ) ) ;
#125819 = AXIS2_PLACEMENT_3D ( 'NONE', #196798, #192970, #116009 ) ;
#125821 = ORIENTED_EDGE ( 'NONE', *, *, #77794, .F. ) ;
#125822 = CARTESIAN_POINT ( 'NONE',  ( 12.25000000000000711, 9.350000000011142731, -117.0215193718251641 ) ) ;
#125823 = ORIENTED_EDGE ( 'NONE', *, *, #187662, .T. ) ;
#125824 = EDGE_CURVE ( 'NONE', #255533, #44715, #182484, .T. ) ;
#125825 = DIRECTION ( 'NONE',  ( 0.000000000000000000, -0.9999631594459056361, -0.008583690987124413183 ) ) ;
#125826 = CARTESIAN_POINT ( 'NONE',  ( 23.14999999999999858, 65.63681063784667913, -232.2959573867136100 ) ) ;
#125827 = ORIENTED_EDGE ( 'NONE', *, *, #181020, .T. ) ;
#125828 = ORIENTED_EDGE ( 'NONE', *, *, #56155, .T. ) ;
#125830 = EDGE_LOOP ( 'NONE', ( #38454, #43951, #2570, #22792 ) ) ;
#125829 = DIRECTION ( 'NONE',  ( -1.000000000000000000, -7.304098846218134667E-16, -5.311601492717084346E-30 ) ) ;
#125831 = DIRECTION ( 'NONE',  ( 0.000000000000000000, 6.938893903907222067E-15, -1.000000000000000000 ) ) ;
#125832 = ORIENTED_EDGE ( 'NONE', *, *, #241044, .F. ) ;
#125833 = DIRECTION ( 'NONE',  ( 0.000000000000000000, 0.000000000000000000, 1.000000000000000000 ) ) ;
#125834 = DIRECTION ( 'NONE',  ( 1.000000000000000000, -0.000000000000000000, 0.000000000000000000 ) ) ;
#125835 = EDGE_CURVE ( 'NONE', #135375, #240562, #48569, .T. ) ;
#125836 = ORIENTED_EDGE ( 'NONE', *, *, #54667, .F. ) ;
#125837 = DIRECTION ( 'NONE',  ( 1.000000000000000000, -0.000000000000000000, -0.000000000000000000 ) ) ;
#125838 = CYLINDRICAL_SURFACE ( 'NONE', #165753, 0.09999999999999939493 ) ;
#125839 = VERTEX_POINT ( 'NONE', #104192 ) ;
#125840 = AXIS2_PLACEMENT_3D ( 'NONE', #62509, #200732, #22111 ) ;
#125841 = CARTESIAN_POINT ( 'NONE',  ( -21.14999999999999858, -3.187427350888460076, -228.3200064793908837 ) ) ;
#125842 = APPLICATION_CONTEXT ( 'automotive_design' ) ;
#125843 = FACE_OUTER_BOUND ( 'NONE', #88851, .T. ) ;
#125845 = EDGE_LOOP ( 'NONE', ( #146695, #141353, #175545, #140837, #189577 ) ) ;
#125844 = CARTESIAN_POINT ( 'NONE',  ( 23.14999999999999503, 11.65000000000000746, -26.48519422934605672 ) ) ;
#125846 = CARTESIAN_POINT ( 'NONE',  ( -18.50000000000000000, 64.35000000001187459, -90.87310748452438247 ) ) ;
#125847 = CARTESIAN_POINT ( 'NONE',  ( 18.39999999999999503, 11.75000000001113953, -54.35000000000000142 ) ) ;
#125848 = CARTESIAN_POINT ( 'NONE',  ( 20.94999999999999929, 70.08587962373171365, -198.1273832143211848 ) ) ;
#125850 = DIRECTION ( 'NONE',  ( 0.000000000000000000, -6.982962677686266711E-15, 1.000000000000000000 ) ) ;
#125849 = CARTESIAN_POINT ( 'NONE',  ( 20.94999999999999929, 85.50000000001251976, -179.9170766071767389 ) ) ;
#125851 = CARTESIAN_POINT ( 'NONE',  ( -20.86777300164944648, 65.66799936921584901, -164.4299399888601556 ) ) ;
#125852 = DIRECTION ( 'NONE',  ( -1.000000000000000000, -0.000000000000000000, 0.000000000000000000 ) ) ;
#125853 = CIRCLE ( 'NONE', #105153, 7.900000000000003908 ) ;
#125854 = CARTESIAN_POINT ( 'NONE',  ( -21.05000000000000071, -11.29603075032412995, -36.54789915966387071 ) ) ;
#125855 = FACE_OUTER_BOUND ( 'NONE', #240228, .T. ) ;
#125856 = CIRCLE ( 'NONE', #67612, 0.09999999999998898659 ) ;
#125857 = ORIENTED_EDGE ( 'NONE', *, *, #172080, .T. ) ;
#125858 = ADVANCED_FACE ( 'NONE', ( #249820 ), #69443, .T. ) ;
#125859 = EDGE_CURVE ( 'NONE', #133755, #91918, #203318, .T. ) ;
#125860 = ORIENTED_EDGE ( 'NONE', *, *, #105742, .T. ) ;
#125861 = CARTESIAN_POINT ( 'NONE',  ( -20.94999999999999929, 64.40000000001209912, -129.5949042542488314 ) ) ;
#125862 = ORIENTED_EDGE ( 'NONE', *, *, #79979, .F. ) ;
#125863 = EDGE_CURVE ( 'NONE', #162071, #4043, #156932, .T. ) ;
#125864 = EDGE_CURVE ( 'NONE', #57850, #168985, #248489, .T. ) ;
#125865 = CARTESIAN_POINT ( 'NONE',  ( -20.87155475150660777, 64.25000000001220712, -143.4275209553668162 ) ) ;
#125866 = VERTEX_POINT ( 'NONE', #15066 ) ;
#125867 = CIRCLE ( 'NONE', #159231, 0.09999999999999938105 ) ;
#125868 = EDGE_CURVE ( 'NONE', #126399, #107215, #94349, .T. ) ;
#125869 = VECTOR ( 'NONE', #114593, 1000.000000000000000 ) ;
#125870 = CARTESIAN_POINT ( 'NONE',  ( -21.05000000000000071, 69.72991413632323088, -170.0579754875375329 ) ) ;
#125871 = DIRECTION ( 'NONE',  ( 0.000000000000000000, -0.9628525332200033038, 0.2700277750006890298 ) ) ;
#125872 = EDGE_CURVE ( 'NONE', #138960, #199913, #256164, .T. ) ;
#125873 = EDGE_LOOP ( 'NONE', ( #94794, #21139, #248048, #44299 ) ) ;
#125874 = CARTESIAN_POINT ( 'NONE',  ( -20.85000000000000142, 0.000000000000000000, -33.50000000000000000 ) ) ;
#125875 = ORIENTED_EDGE ( 'NONE', *, *, #192442, .F. ) ;
#125876 = ADVANCED_FACE ( 'NONE', ( #171595 ), #194353, .F. ) ;
#125877 = ORIENTED_EDGE ( 'NONE', *, *, #114828, .F. ) ;
#125878 = CARTESIAN_POINT ( 'NONE',  ( -18.79999999999999716, 7.800000000000000711, -1.212568896937008089 ) ) ;
#125879 = DIRECTION ( 'NONE',  ( 1.000000000000000000, 0.000000000000000000, 0.000000000000000000 ) ) ;
#125880 = VERTEX_POINT ( 'NONE', #234092 ) ;
#125881 = ADVANCED_FACE ( 'NONE', ( #176715 ), #81850, .T. ) ;
#125882 = CARTESIAN_POINT ( 'NONE',  ( 19.81427058490544013, 11.66856398039208109, -158.7500000000000284 ) ) ;
#125884 = ORIENTED_EDGE ( 'NONE', *, *, #224938, .F. ) ;
#125883 = DIRECTION ( 'NONE',  ( 0.000000000000000000, -7.116814260417693756E-15, 1.000000000000000000 ) ) ;
#125885 = PLANE ( 'NONE',  #66764 ) ;
#125887 = EDGE_LOOP ( 'NONE', ( #228522, #51154, #193137, #215190 ) ) ;
#125886 = DIRECTION ( 'NONE',  ( 1.000000000000000000, -2.849773892568378313E-16, 7.728835255496647986E-17 ) ) ;
#125888 = CARTESIAN_POINT ( 'NONE',  ( 23.14999999999999858, 1.115600667400684642E-11, -100.5000000000000426 ) ) ;
#125890 = EDGE_CURVE ( 'NONE', #133755, #251907, #227629, .T. ) ;
#125889 = CARTESIAN_POINT ( 'NONE',  ( -18.50000000000000000, 10.29288807859935950, -72.45800201601217339 ) ) ;
#125891 = VECTOR ( 'NONE', #243790, 1000.000000000000000 ) ;
#125892 = CIRCLE ( 'NONE', #92584, 0.5999999999999978684 ) ;
#125893 = LINE ( 'NONE', #46352, #69357 ) ;
#125894 = CIRCLE ( 'NONE', #134277, 0.09999999999999939493 ) ;
#125896 = CARTESIAN_POINT ( 'NONE',  ( -21.14999999999999858, 69.45934304831143891, -203.5231074845243882 ) ) ;
#125895 = DIRECTION ( 'NONE',  ( 0.000000000000000000, 1.000000000000000000, 0.000000000000000000 ) ) ;
#125897 = DIRECTION ( 'NONE',  ( -1.000000000000000000, 0.000000000000000000, 0.000000000000000000 ) ) ;
#125898 = ADVANCED_FACE ( 'NONE', ( #17604 ), #214527, .T. ) ;
#125899 = DIRECTION ( 'NONE',  ( 0.000000000000000000, 0.2617529984165152257, 0.9651348961777124202 ) ) ;
#125900 = DIRECTION ( 'NONE',  ( 0.000000000000000000, 6.505213034913742890E-15, 1.000000000000000000 ) ) ;
#125901 = CARTESIAN_POINT ( 'NONE',  ( -20.15000000000000568, 66.70857864377498458, -157.6731074845244223 ) ) ;
#125902 = ORIENTED_EDGE ( 'NONE', *, *, #38774, .F. ) ;
#125903 = VERTEX_POINT ( 'NONE', #152025 ) ;
#125904 = ORIENTED_EDGE ( 'NONE', *, *, #184144, .T. ) ;
#125905 = ADVANCED_FACE ( 'NONE', ( #194999 ), #94579, .F. ) ;
#125906 = DIRECTION ( 'NONE',  ( 1.000000000000000000, 0.000000000000000000, 0.000000000000000000 ) ) ;
#125907 = ORIENTED_EDGE ( 'NONE', *, *, #101163, .F. ) ;
#125908 = CARTESIAN_POINT ( 'NONE',  ( 18.39999999999999503, 64.25000000001230660, -157.3731074845244393 ) ) ;
#125909 = ORIENTED_EDGE ( 'NONE', *, *, #243643, .T. ) ;
#125910 = FACE_OUTER_BOUND ( 'NONE', #31871, .T. ) ;
#125911 = SURFACE_STYLE_FILL_AREA ( #183340 ) ;
#125912 = EDGE_CURVE ( 'NONE', #256387, #219738, #2774, .T. ) ;
#125913 = EDGE_CURVE ( 'NONE', #45320, #59375, #32034, .T. ) ;
#125914 = ORIENTED_EDGE ( 'NONE', *, *, #108693, .F. ) ;
#125915 = CARTESIAN_POINT ( 'NONE',  ( 15.69410316191959609, 9.356746017089404788, -151.2033597213642224 ) ) ;
#125916 = CIRCLE ( 'NONE', #109348, 0.09999999999999939493 ) ;
#125917 = VERTEX_POINT ( 'NONE', #58007 ) ;
#125918 = VERTEX_POINT ( 'NONE', #54170 ) ;
#125919 = ORIENTED_EDGE ( 'NONE', *, *, #15321, .T. ) ;
#125920 = CARTESIAN_POINT ( 'NONE',  ( 11.60000000000006004, 67.75000000001118394, -16.98168612828748891 ) ) ;
#125921 = DIRECTION ( 'NONE',  ( -0.1538461538461484146, -0.9880948137434723000, 0.000000000000000000 ) ) ;
#125922 = CARTESIAN_POINT ( 'NONE',  ( -20.94999999999999929, 4.260086453440760756, -245.2296700999207246 ) ) ;
#125923 = CARTESIAN_POINT ( 'NONE',  ( 18.59999999999999076, 65.75000000001251976, -178.7731074845244450 ) ) ;
#125924 = CARTESIAN_POINT ( 'NONE',  ( -18.59999999999999787, 68.97833521811203639, -132.6895420826271277 ) ) ;
#125925 = AXIS2_PLACEMENT_3D ( 'NONE', #29370, #150566, #230092 ) ;
#125927 = FACE_OUTER_BOUND ( 'NONE', #50477, .T. ) ;
#125926 = DIRECTION ( 'NONE',  ( 0.000000000000000000, 6.982962677686266711E-15, -1.000000000000000000 ) ) ;
#125928 = CARTESIAN_POINT ( 'NONE',  ( -23.25000000000000000, 46.23295349378772556, -240.7147059833253309 ) ) ;
#125930 = ORIENTED_EDGE ( 'NONE', *, *, #58259, .F. ) ;
#125929 = CARTESIAN_POINT ( 'NONE',  ( 23.14999999999998437, -11.74999999998884448, -67.00000000000004263 ) ) ;
#125932 = DIRECTION ( 'NONE',  ( -1.000000000000000000, 0.000000000000000000, 0.000000000000000000 ) ) ;
#125931 = CARTESIAN_POINT ( 'NONE',  ( 20.96937028524355640, 10.62446937163783289, -74.49142610116966523 ) ) ;
#125933 = DIRECTION ( 'NONE',  ( 1.000000000000000000, -0.000000000000000000, 0.000000000000000000 ) ) ;
#125934 = EDGE_LOOP ( 'NONE', ( #140620, #179171, #31083, #83735 ) ) ;
#125935 = DIRECTION ( 'NONE',  ( -1.000000000000000000, 0.000000000000000000, 0.000000000000000000 ) ) ;
#125936 = AXIS2_PLACEMENT_3D ( 'NONE', #857, #137811, #180818 ) ;
#125937 = CARTESIAN_POINT ( 'NONE',  ( -21.44999999999999929, 7.150000000011155876, -54.65000000000000568 ) ) ;
#125938 = CARTESIAN_POINT ( 'NONE',  ( 19.86930884467584946, 64.31308993304044463, -44.78388484558566773 ) ) ;
#125939 = EDGE_LOOP ( 'NONE', ( #161126, #176853, #111336, #197837 ) ) ;
#125940 = AXIS2_PLACEMENT_3D ( 'NONE', #119728, #143106, #83107 ) ;
#125942 = CARTESIAN_POINT ( 'NONE',  ( -23.25000000000000355, 5.650000000011139001, -42.75000000000000000 ) ) ;
#125941 = AXIS2_PLACEMENT_3D ( 'NONE', #96476, #220312, #121243 ) ;
#125943 = VECTOR ( 'NONE', #247743, 1000.000000000000000 ) ;
#125944 = DIRECTION ( 'NONE',  ( 0.000000000000000000, 2.891205793294679805E-16, -1.000000000000000000 ) ) ;
#125945 = DIRECTION ( 'NONE',  ( 0.000000000000000000, 0.2128009952263601734, -0.9770955615653316162 ) ) ;
#125946 = VECTOR ( 'NONE', #62189, 1000.000000000000114 ) ;
#125947 = ORIENTED_EDGE ( 'NONE', *, *, #49561, .T. ) ;
#125948 = ORIENTED_EDGE ( 'NONE', *, *, #244919, .F. ) ;
#125949 = CIRCLE ( 'NONE', #76068, 0.09999999999999939493 ) ;
#125950 = DIRECTION ( 'NONE',  ( -1.000000000000000000, -0.000000000000000000, -0.000000000000000000 ) ) ;
#125951 = EDGE_LOOP ( 'NONE', ( #30876, #98642, #63092, #6409 ) ) ;
#125952 = DIRECTION ( 'NONE',  ( -1.000000000000000000, 0.000000000000000000, 0.000000000000000000 ) ) ;
#125953 = CARTESIAN_POINT ( 'NONE',  ( -18.39999999999999503, -9.682403433465244902, -174.1568433774128266 ) ) ;
#125954 = DIRECTION ( 'NONE',  ( 0.000000000000000000, -7.147358527629766941E-15, 1.000000000000000000 ) ) ;
#125955 = FACE_OUTER_BOUND ( 'NONE', #97748, .T. ) ;
#125956 = ORIENTED_EDGE ( 'NONE', *, *, #136034, .T. ) ;
#125957 = AXIS2_PLACEMENT_3D ( 'NONE', #113105, #11454, #153567 ) ;
#125959 = VECTOR ( 'NONE', #155510, 1000.000000000000000 ) ;
#125958 = LINE ( 'NONE', #11160, #528 ) ;
#125960 = EDGE_CURVE ( 'NONE', #67554, #140862, #12512, .T. ) ;
#125961 = DIRECTION ( 'NONE',  ( 1.000000000000000000, 0.000000000000000000, 0.000000000000000000 ) ) ;
#125963 = DIRECTION ( 'NONE',  ( -1.000000000000000000, -0.000000000000000000, -0.000000000000000000 ) ) ;
#125962 = AXIS2_PLACEMENT_3D ( 'NONE', #148212, #249882, #167807 ) ;
#125964 = CIRCLE ( 'NONE', #159323, 0.09999999999998898659 ) ;
#125965 = CARTESIAN_POINT ( 'NONE',  ( 23.24999999999999645, 76.00000000001142553, -36.02310748452432421 ) ) ;
#125966 = EDGE_CURVE ( 'NONE', #66263, #68492, #34642, .T. ) ;
#125967 = VECTOR ( 'NONE', #228904, 1000.000000000000000 ) ;
#125968 = ORIENTED_EDGE ( 'NONE', *, *, #138253, .T. ) ;
#125969 = DIRECTION ( 'NONE',  ( -0.000000000000000000, 0.000000000000000000, -1.000000000000000000 ) ) ;
#125970 = VECTOR ( 'NONE', #111067, 1000.000000000000000 ) ;
#125971 = CIRCLE ( 'NONE', #100805, 12.87499999999999822 ) ;
#125972 = EDGE_CURVE ( 'NONE', #132861, #236967, #231545, .T. ) ;
#125974 = VERTEX_POINT ( 'NONE', #16359 ) ;
#125973 = DIRECTION ( 'NONE',  ( -0.000000000000000000, 1.000000000000000000, 6.352154140967427193E-15 ) ) ;
#125975 = EDGE_CURVE ( 'NONE', #8746, #141218, #95854, .T. ) ;
#125976 = CARTESIAN_POINT ( 'NONE',  ( 18.49999999999999645, 79.19526988099229925, -196.1889237952725296 ) ) ;
#125977 = CARTESIAN_POINT ( 'NONE',  ( -21.07954640115351808, 34.01103892604695034, -243.8019938780049642 ) ) ;
#125978 = AXIS2_PLACEMENT_3D ( 'NONE', #255074, #179468, #235557 ) ;
#125979 = CARTESIAN_POINT ( 'NONE',  ( -18.59999999999999787, -1.162701749926853712, -175.5999999999999659 ) ) ;
#125980 = CYLINDRICAL_SURFACE ( 'NONE', #96301, 0.09999999999999781286 ) ;
#125981 = DIRECTION ( 'NONE',  ( 0.000000000000000000, -0.9651348961777155289, 0.2617529984165036794 ) ) ;
#125982 = DIRECTION ( 'NONE',  ( -1.000000000000000000, 0.000000000000000000, 0.000000000000000000 ) ) ;
#125983 = ORIENTED_EDGE ( 'NONE', *, *, #124465, .F. ) ;
#125984 = LINE ( 'NONE', #47720, #230102 ) ;
#125985 = CARTESIAN_POINT ( 'NONE',  ( -21.05000000000000071, -1.162701749926853712, -141.9000000000000341 ) ) ;
#125986 = CARTESIAN_POINT ( 'NONE',  ( -18.40000000000000213, 11.47316190337364183, -188.4499999999999886 ) ) ;
#125987 = FACE_OUTER_BOUND ( 'NONE', #225901, .T. ) ;
#125988 = VECTOR ( 'NONE', #214520, 1000.000000000000000 ) ;
#125989 = CYLINDRICAL_SURFACE ( 'NONE', #257295, 0.1000000000000028644 ) ;
#125990 = CIRCLE ( 'NONE', #67745, 11.65000000000000036 ) ;
#125991 = CIRCLE ( 'NONE', #163424, 0.1000000000000043493 ) ;
#125992 = EDGE_CURVE ( 'NONE', #133057, #58091, #37206, .T. ) ;
#125993 = ORIENTED_EDGE ( 'NONE', *, *, #163016, .F. ) ;
#125994 = ORIENTED_EDGE ( 'NONE', *, *, #254250, .T. ) ;
#125995 = CARTESIAN_POINT ( 'NONE',  ( 23.14999999999999858, 76.00000000001170974, -69.52310748452431710 ) ) ;
#125996 = FACE_OUTER_BOUND ( 'NONE', #123293, .T. ) ;
#125997 = CYLINDRICAL_SURFACE ( 'NONE', #249849, 0.5000000000000007772 ) ;
#125998 = DIRECTION ( 'NONE',  ( 0.000000000000000000, -0.2128009952263485993, 0.9770955615653341697 ) ) ;
#125999 = DIRECTION ( 'NONE',  ( 1.000000000000000000, 0.000000000000000000, 0.000000000000000000 ) ) ;
#126000 = FACE_OUTER_BOUND ( 'NONE', #153502, .T. ) ;
#126001 = ADVANCED_FACE ( 'NONE', ( #112874 ), #162288, .T. ) ;
#126002 = DIRECTION ( 'NONE',  ( -0.000000000000000000, 0.1350103645451876666, -0.9908441862701600211 ) ) ;
#126003 = EDGE_CURVE ( 'NONE', #110160, #19541, #202697, .T. ) ;
#126004 = AXIS2_PLACEMENT_3D ( 'NONE', #204149, #247130, #245865 ) ;
#126005 = VERTEX_POINT ( 'NONE', #80120 ) ;
#126006 = DIRECTION ( 'NONE',  ( 0.000000000000000000, 0.9126074666063660468, 0.4088369013363524762 ) ) ;
#126007 = AXIS2_PLACEMENT_3D ( 'NONE', #164517, #184058, #47096 ) ;
#126008 = EDGE_LOOP ( 'NONE', ( #229582, #114901, #83458, #62848 ) ) ;
#126009 = FACE_OUTER_BOUND ( 'NONE', #121369, .T. ) ;
#126010 = CYLINDRICAL_SURFACE ( 'NONE', #166182, 0.09999999999999781286 ) ;
#126011 = CYLINDRICAL_SURFACE ( 'NONE', #53584, 0.09999999999998898659 ) ;
#126012 = ADVANCED_FACE ( 'NONE', ( #20203 ), #63153, .F. ) ;
#126013 = CARTESIAN_POINT ( 'NONE',  ( 18.55857864376267941, 10.36715728753653565, -192.2499999999999432 ) ) ;
#126014 = FACE_OUTER_BOUND ( 'NONE', #207418, .T. ) ;
#126015 = CARTESIAN_POINT ( 'NONE',  ( -18.49346865148320518, -9.443073798524933338, -7.185196255314905578 ) ) ;
#126016 = DIRECTION ( 'NONE',  ( 0.000000000000000000, 3.469446951953515108E-14, 1.000000000000000000 ) ) ;
#126017 = ADVANCED_FACE ( 'NONE', ( #24066 ), #100956, .T. ) ;
#126018 = CARTESIAN_POINT ( 'NONE',  ( 22.00356870068398862, -8.772485052120828773E-13, -93.24575763823901298 ) ) ;
#126019 = CARTESIAN_POINT ( 'NONE',  ( -23.15000000000000213, 63.58084468663284383, -237.4904741118237723 ) ) ;
#126020 = LINE ( 'NONE', #205552, #52253 ) ;
#126021 = CARTESIAN_POINT ( 'NONE',  ( -18.39999999999999858, -9.599999999988844124, -174.5320693966996259 ) ) ;
#126022 = ADVANCED_FACE ( 'NONE', ( #239242 ), #4467, .T. ) ;
#126023 = FACE_OUTER_BOUND ( 'NONE', #90853, .T. ) ;
#126024 = AXIS2_PLACEMENT_3D ( 'NONE', #227361, #248220, #13464 ) ;
#126025 = ORIENTED_EDGE ( 'NONE', *, *, #174167, .F. ) ;
#126026 = DIRECTION ( 'NONE',  ( 2.952720810173289605E-16, 1.000000000000000000, 7.086529944415894657E-15 ) ) ;
#126027 = DIRECTION ( 'NONE',  ( 0.000000000000000000, -1.000000000000000000, 0.000000000000000000 ) ) ;
#126028 = EDGE_CURVE ( 'NONE', #95552, #193662, #53025, .T. ) ;
#126029 = VERTEX_POINT ( 'NONE', #179294 ) ;
#126030 = CARTESIAN_POINT ( 'NONE',  ( -16.94333152882356686, 51.64072791834932019, -231.8924685538414394 ) ) ;
#126031 = CARTESIAN_POINT ( 'NONE',  ( -1.739115166359751801E-14, 11.64999999999998970, -12.25000000000000000 ) ) ;
#126032 = DIRECTION ( 'NONE',  ( 6.484947573744954877E-15, 0.9274965247785529332, -0.3738317757009255171 ) ) ;
#126033 = ADVANCED_FACE ( 'NONE', ( #198821 ), #197534, .F. ) ;
#126034 = ORIENTED_EDGE ( 'NONE', *, *, #193809, .F. ) ;
#126035 = CARTESIAN_POINT ( 'NONE',  ( 20.94999999999999929, 64.25000000001146816, -42.80697314750248950 ) ) ;
#126036 = DIRECTION ( 'NONE',  ( 5.603264701231745086E-32, -1.897661533703520636E-16, 1.000000000000000000 ) ) ;
#126037 = AXIS2_PLACEMENT_3D ( 'NONE', #34618, #56686, #252342 ) ;
#126038 = VERTEX_POINT ( 'NONE', #42325 ) ;
#126039 = CARTESIAN_POINT ( 'NONE',  ( 18.49999999999999645, -1.102499207903926637, -187.8171010361417643 ) ) ;
#126040 = ORIENTED_EDGE ( 'NONE', *, *, #16673, .T. ) ;
#126041 = DIRECTION ( 'NONE',  ( 0.000000000000000000, -0.9651348961777157509, 0.2617529984165031243 ) ) ;
#126042 = CARTESIAN_POINT ( 'NONE',  ( 22.40000000000010516, 1.020945751984553285E-11, -21.85042919245488946 ) ) ;
#126043 = CYLINDRICAL_SURFACE ( 'NONE', #24205, 2.000000000000001776 ) ;
#126045 = UNCERTAINTY_MEASURE_WITH_UNIT (LENGTH_MEASURE( 1.000000000000000082E-05 ), #164287, 'distance_accuracy_value', 'NONE');
#126044 = CARTESIAN_POINT ( 'NONE',  ( 21.05000000000000071, 1.148907358139439339E-11, -201.0000000000015064 ) ) ;
#126046 = CARTESIAN_POINT ( 'NONE',  ( -21.53752568617682783, 69.21319212550889688, -203.6220819458087306 ) ) ;
#126047 = FACE_OUTER_BOUND ( 'NONE', #134990, .T. ) ;
#126048 = CARTESIAN_POINT ( 'NONE',  ( -21.05000000000000071, 11.60000000001115517, -194.0717967697244717 ) ) ;
#126049 = AXIS2_PLACEMENT_3D ( 'NONE', #114000, #73634, #115292 ) ;
#126050 = CARTESIAN_POINT ( 'NONE',  ( -23.25000000000000000, 76.10085836911117951, -181.7726746080137445 ) ) ;
#126052 = DIRECTION ( 'NONE',  ( 1.000000000000000000, -3.151514657663852580E-16, 8.547182517843351137E-17 ) ) ;
#126051 = AXIS2_PLACEMENT_3D ( 'NONE', #86980, #206962, #92143 ) ;
#126054 = ORIENTED_EDGE ( 'NONE', *, *, #122137, .T. ) ;
#126053 = CARTESIAN_POINT ( 'NONE',  ( 18.59999996954842771, 86.99283344320274125, -199.3727709741243075 ) ) ;
#126055 = ORIENTED_EDGE ( 'NONE', *, *, #186790, .T. ) ;
#126057 = DIRECTION ( 'NONE',  ( 0.000000000000000000, 0.4088369013363280513, -0.9126074666063769270 ) ) ;
#126056 = CARTESIAN_POINT ( 'NONE',  ( -23.15000000000000213, 54.27339256631721298, -236.8935360681107625 ) ) ;
#126059 = VERTEX_POINT ( 'NONE', #102254 ) ;
#126058 = DIRECTION ( 'NONE',  ( 0.000000000000000000, 0.000000000000000000, -1.000000000000000000 ) ) ;
#126060 = ORIENTED_EDGE ( 'NONE', *, *, #63368, .T. ) ;
#126061 = DIRECTION ( 'NONE',  ( 0.000000000000000000, -1.000000000000000000, 0.000000000000000000 ) ) ;
#126062 = DIRECTION ( 'NONE',  ( 0.000000000000000000, -0.000000000000000000, 1.000000000000000000 ) ) ;
#126063 = LINE ( 'NONE', #141782, #142350 ) ;
#126064 = CIRCLE ( 'NONE', #34358, 0.4999999999999997780 ) ;
#126065 = DIRECTION ( 'NONE',  ( -1.000000000000000000, 0.000000000000000000, 0.000000000000000000 ) ) ;
#126066 = DIRECTION ( 'NONE',  ( -1.000000000000000000, 0.000000000000000000, 0.000000000000000000 ) ) ;
#126067 = DIRECTION ( 'NONE',  ( 1.000000000000000000, 0.000000000000000000, -0.000000000000000000 ) ) ;
#126068 = AXIS2_PLACEMENT_3D ( 'NONE', #170288, #108969, #150681 ) ;
#126069 = CIRCLE ( 'NONE', #226010, 0.1000000000000026007 ) ;
#126070 = AXIS2_PLACEMENT_3D ( 'NONE', #92672, #13154, #172264 ) ;
#126072 = AXIS2_PLACEMENT_3D ( 'NONE', #195510, #16860, #235879 ) ;
#126071 = DIRECTION ( 'NONE',  ( 0.000000000000000000, -0.8814952561689786137, 0.4721928772774816596 ) ) ;
#126073 = VERTEX_POINT ( 'NONE', #141416 ) ;
#126074 = ORIENTED_EDGE ( 'NONE', *, *, #179087, .F. ) ;
#126075 = EDGE_CURVE ( 'NONE', #207794, #101319, #3173, .T. ) ;
#126076 = DIRECTION ( 'NONE',  ( -1.000000000000000000, 0.000000000000000000, 0.000000000000000000 ) ) ;
#126077 = VERTEX_POINT ( 'NONE', #140116 ) ;
#126078 = CARTESIAN_POINT ( 'NONE',  ( 21.05000000000000071, 0.03201369319893643955, -27.24115727646229601 ) ) ;
#126079 = EDGE_LOOP ( 'NONE', ( #26717, #43132, #139708, #132538 ) ) ;
#126080 = CARTESIAN_POINT ( 'NONE',  ( -16.89268316805466341, 66.04827818676967865, -90.37885996306994230 ) ) ;
#126081 = CARTESIAN_POINT ( 'NONE',  ( -21.05000000000000071, 6.412126976762837494, -199.7058512474018244 ) ) ;
#126082 = EDGE_CURVE ( 'NONE', #78455, #47226, #177997, .T. ) ;
#126083 = DIRECTION ( 'NONE',  ( 0.000000000000000000, 0.000000000000000000, -1.000000000000000000 ) ) ;
#126084 = CARTESIAN_POINT ( 'NONE',  ( -16.94878442675512176, 22.96408127013238598, -230.8802323934030767 ) ) ;
#126085 = ORIENTED_EDGE ( 'NONE', *, *, #114172, .T. ) ;
#126086 = CARTESIAN_POINT ( 'NONE',  ( 19.75857864376268935, 11.65000000001115943, -125.2500000000000284 ) ) ;
#126087 = ORIENTED_EDGE ( 'NONE', *, *, #186030, .T. ) ;
#126088 = ADVANCED_FACE ( 'NONE', ( #257454 ), #239814, .F. ) ;
#126089 = CARTESIAN_POINT ( 'NONE',  ( 23.14999999999999503, 61.57587952878035509, -212.2000740415318774 ) ) ;
#126090 = EDGE_CURVE ( 'NONE', #248650, #202021, #219613, .T. ) ;
#126091 = FACE_OUTER_BOUND ( 'NONE', #144764, .T. ) ;
#126092 = FACE_OUTER_BOUND ( 'NONE', #50032, .T. ) ;
#126093 = CYLINDRICAL_SURFACE ( 'NONE', #90755, 0.09999999999999939493 ) ;
#126094 = VERTEX_POINT ( 'NONE', #48732 ) ;
#126095 = CIRCLE ( 'NONE', #167648, 0.09999999999998712696 ) ;
#126096 = DIRECTION ( 'NONE',  ( -0.000000000000000000, -0.7049548389605067023, 0.7092521942342977503 ) ) ;
#126097 = ORIENTED_EDGE ( 'NONE', *, *, #107694, .T. ) ;
#126100 = VERTEX_POINT ( 'NONE', #69607 ) ;
#126099 = CARTESIAN_POINT ( 'NONE',  ( 15.48841904831874849, 8.561580951692381092, -46.14999999999999858 ) ) ;
#126098 = PLANE ( 'NONE',  #153439 ) ;
#126101 = CARTESIAN_POINT ( 'NONE',  ( 21.05000000000000071, 18.75506398265894958, -230.0044230565036116 ) ) ;
#126102 = VERTEX_POINT ( 'NONE', #205230 ) ;
#126103 = CARTESIAN_POINT ( 'NONE',  ( 19.75857864376268935, 62.46583972339646351, -208.9186153945276487 ) ) ;
#126104 = ORIENTED_EDGE ( 'NONE', *, *, #176592, .T. ) ;
#126105 = ADVANCED_FACE ( 'NONE', ( #26635 ), #227375, .T. ) ;
#126106 = VECTOR ( 'NONE', #22626, 1000.000000000000114 ) ;
#126107 = DIRECTION ( 'NONE',  ( 1.000000000000000000, 0.000000000000000000, 0.000000000000000000 ) ) ;
#126108 = CARTESIAN_POINT ( 'NONE',  ( 21.00000000000000000, 66.25000000001223555, -148.7731074845244450 ) ) ;
#126109 = CARTESIAN_POINT ( 'NONE',  ( -6.099999999999939249, 64.25000000001119815, -25.92310748452479174 ) ) ;
#126110 = DIRECTION ( 'NONE',  ( 0.000000000000000000, 6.982962677686267499E-15, -1.000000000000000000 ) ) ;
#126111 = AXIS2_PLACEMENT_3D ( 'NONE', #209199, #227471, #245771 ) ;
#126112 = ORIENTED_EDGE ( 'NONE', *, *, #83722, .F. ) ;
#126113 = AXIS2_PLACEMENT_3D ( 'NONE', #196723, #216280, #158913 ) ;
#126114 = AXIS2_PLACEMENT_3D ( 'NONE', #123648, #160227, #181063 ) ;
#126115 = DIRECTION ( 'NONE',  ( 1.000000000000000000, -0.000000000000000000, -0.000000000000000000 ) ) ;
#126116 = DIRECTION ( 'NONE',  ( 0.000000000000000000, 0.000000000000000000, -1.000000000000000000 ) ) ;
#126117 = CARTESIAN_POINT ( 'NONE',  ( -18.43459694179555441, -9.494210124986889099, -140.6170052026611188 ) ) ;
#126118 = ORIENTED_EDGE ( 'NONE', *, *, #251635, .F. ) ;
#126119 = DIRECTION ( 'NONE',  ( 0.000000000000000000, 0.000000000000000000, -1.000000000000000000 ) ) ;
#126120 = ORIENTED_EDGE ( 'NONE', *, *, #199533, .T. ) ;
#126121 = CYLINDRICAL_SURFACE ( 'NONE', #6345, 0.09999999999999939493 ) ;
#126122 = CIRCLE ( 'NONE', #167866, 12.87499999999998401 ) ;
#126123 = ADVANCED_FACE ( 'NONE', ( #226063 ), #61415, .T. ) ;
#126124 = DIRECTION ( 'NONE',  ( 1.000000000000000000, 0.000000000000000000, 0.000000000000000000 ) ) ;
#126125 = DIRECTION ( 'NONE',  ( 0.000000000000000000, 0.8814952561688430555, -0.4721928772777346239 ) ) ;
#126126 = EDGE_CURVE ( 'NONE', #232305, #107596, #207175, .T. ) ;
#126128 = ORIENTED_EDGE ( 'NONE', *, *, #120818, .F. ) ;
#126127 = CARTESIAN_POINT ( 'NONE',  ( -16.88705144915408596, 44.39190486951041237, -235.1840571886030489 ) ) ;
#126129 = DIRECTION ( 'NONE',  ( 0.000000000000000000, 0.000000000000000000, -1.000000000000000000 ) ) ;
#126130 = VECTOR ( 'NONE', #52804, 1000.000000000000000 ) ;
#126131 = CARTESIAN_POINT ( 'NONE',  ( -22.94999999999999929, 1.212568896937007645, -8.000000000000000000 ) ) ;
#126132 = AXIS2_PLACEMENT_3D ( 'NONE', #221532, #5049, #126302 ) ;
#126133 = DIRECTION ( 'NONE',  ( 0.000000000000000000, -1.000000000000000000, 0.000000000000000000 ) ) ;
#126135 = ADVANCED_FACE ( 'NONE', ( #106124 ), #164848, .F. ) ;
#126134 = ORIENTED_EDGE ( 'NONE', *, *, #140101, .T. ) ;
#126136 = CIRCLE ( 'NONE', #242678, 0.09999999999999949207 ) ;
#126137 = FACE_OUTER_BOUND ( 'NONE', #67832, .T. ) ;
#126138 = ORIENTED_EDGE ( 'NONE', *, *, #191991, .F. ) ;
#126139 = CARTESIAN_POINT ( 'NONE',  ( 20.95512820512820440, 8.876151316299271343, -79.15000000000004832 ) ) ;
#126140 = CIRCLE ( 'NONE', #13731, 12.87499999999999822 ) ;
#126141 = ORIENTED_EDGE ( 'NONE', *, *, #103943, .F. ) ;
#126142 = VECTOR ( 'NONE', #135939, 1000.000000000000000 ) ;
#126143 = CIRCLE ( 'NONE', #105854, 0.09999999999999939493 ) ;
#126144 = CARTESIAN_POINT ( 'NONE',  ( -16.87683809663752399, 44.86297841676450560, -235.0825981793917947 ) ) ;
#126145 = AXIS2_PLACEMENT_3D ( 'NONE', #152963, #156805, #117647 ) ;
#126147 = ORIENTED_EDGE ( 'NONE', *, *, #101516, .F. ) ;
#126146 = FACE_OUTER_BOUND ( 'NONE', #142805, .T. ) ;
#126150 = ORIENTED_EDGE ( 'NONE', *, *, #243428, .F. ) ;
#126149 = VERTEX_POINT ( 'NONE', #85266 ) ;
#126148 = CARTESIAN_POINT ( 'NONE',  ( -18.59999999999999787, 5.950000000011100632, -110.8057023050348988 ) ) ;
#126151 = DIRECTION ( 'NONE',  ( -1.000000000000000000, 0.000000000000000000, 1.073024830501117725E-15 ) ) ;
#126152 = CARTESIAN_POINT ( 'NONE',  ( 20.04142135623730070, 11.75000000001115907, -122.2500000000000284 ) ) ;
#126153 = DIRECTION ( 'NONE',  ( 0.000000000000000000, 0.000000000000000000, -1.000000000000000000 ) ) ;
#126155 = CARTESIAN_POINT ( 'NONE',  ( -12.30589683808040569, 66.64325398293328817, -52.31974776316020126 ) ) ;
#126154 = DIRECTION ( 'NONE',  ( 0.000000000000000000, -1.000000000000000000, -0.000000000000000000 ) ) ;
#126156 = DIRECTION ( 'NONE',  ( -1.000000000000000000, 0.000000000000000000, 0.000000000000000000 ) ) ;
#126157 = FACE_OUTER_BOUND ( 'NONE', #250559, .T. ) ;
#126158 = AXIS2_PLACEMENT_3D ( 'NONE', #225509, #9057, #89867 ) ;
#126159 = CARTESIAN_POINT ( 'NONE',  ( -23.25000000000000000, -2.576749817950531707, -189.6385361693310756 ) ) ;
#126160 = AXIS2_PLACEMENT_3D ( 'NONE', #36286, #255254, #156244 ) ;
#126161 = CARTESIAN_POINT ( 'NONE',  ( -22.49806830649814060, 11.64988965485023620, -33.42253568367449645 ) ) ;
#126162 = AXIS2_PLACEMENT_3D ( 'NONE', #199252, #4851, #84364 ) ;
#126163 = CARTESIAN_POINT ( 'NONE',  ( -20.94999999999999929, 74.16465844978715438, -57.96795619196134908 ) ) ;
#126164 = ORIENTED_EDGE ( 'NONE', *, *, #153141, .T. ) ;
#126165 = EDGE_LOOP ( 'NONE', ( #126913, #254539, #65731, #234920 ) ) ;
#126166 = EDGE_CURVE ( 'NONE', #243362, #238459, #57103, .T. ) ;
#126167 = CARTESIAN_POINT ( 'NONE',  ( -20.99780126800921565, 64.39461131213516865, -76.43575491281889356 ) ) ;
#126168 = EDGE_CURVE ( 'NONE', #68733, #229760, #140500, .T. ) ;
#126170 = ORIENTED_EDGE ( 'NONE', *, *, #52621, .T. ) ;
#126169 = DIRECTION ( 'NONE',  ( 0.000000000000000000, -6.982962677686266711E-15, 1.000000000000000000 ) ) ;
#126171 = VERTEX_POINT ( 'NONE', #7041 ) ;
#126172 = CARTESIAN_POINT ( 'NONE',  ( -16.81744102076749314, 12.41403342719998726, -211.2428889513006993 ) ) ;
#126173 = ORIENTED_EDGE ( 'NONE', *, *, #124887, .F. ) ;
#126174 = CARTESIAN_POINT ( 'NONE',  ( -21.14999999999999858, 69.45934304831089889, -136.5231074845243313 ) ) ;
#126175 = ADVANCED_FACE ( 'NONE', ( #188253 ), #50025, .F. ) ;
#126176 = EDGE_CURVE ( 'NONE', #139213, #125226, #206975, .T. ) ;
#126177 = ORIENTED_EDGE ( 'NONE', *, *, #39750, .F. ) ;
#126178 = EDGE_CURVE ( 'NONE', #153112, #173033, #258030, .T. ) ;
#126179 = CARTESIAN_POINT ( 'NONE',  ( 18.59999999999999076, 6.450000000011156587, -43.51702717044002355 ) ) ;
#126180 = CARTESIAN_POINT ( 'NONE',  ( 5.899999999999995914, -11.34999999999999964, 10.10000000000000142 ) ) ;
#126181 = CIRCLE ( 'NONE', #42424, 0.09999999999999954758 ) ;
#126182 = EDGE_CURVE ( 'NONE', #140362, #13818, #177948, .T. ) ;
#126184 = ORIENTED_EDGE ( 'NONE', *, *, #24283, .T. ) ;
#126183 = ORIENTED_EDGE ( 'NONE', *, *, #200033, .T. ) ;
#126185 = EDGE_LOOP ( 'NONE', ( #136277, #81976, #251551, #237979 ) ) ;
#126188 = ADVANCED_FACE ( 'NONE', ( #90423, #170024, #184391 ), #111293, .F. ) ;
#126187 = EDGE_CURVE ( 'NONE', #42831, #189870, #123781, .T. ) ;
#126186 = PLANE ( 'NONE',  #128066 ) ;
#126189 = VERTEX_POINT ( 'NONE', #36924 ) ;
#126190 = ORIENTED_EDGE ( 'NONE', *, *, #223347, .T. ) ;
#126191 = DIRECTION ( 'NONE',  ( 1.000000000000000000, 0.000000000000000000, 0.000000000000000000 ) ) ;
#126192 = DIRECTION ( 'NONE',  ( 1.000000000000000000, 0.000000000000000000, 0.000000000000000000 ) ) ;
#126194 = VERTEX_POINT ( 'NONE', #91724 ) ;
#126193 = DIRECTION ( 'NONE',  ( 1.000000000000000000, 3.265361837132813093E-16, -0.000000000000000000 ) ) ;
#126195 = EDGE_CURVE ( 'NONE', #10431, #215970, #240304, .T. ) ;
#126196 = DIRECTION ( 'NONE',  ( 0.000000000000000000, 0.4930308989874718772, 0.8700118002898612479 ) ) ;
#126197 = DIRECTION ( 'NONE',  ( 1.000000000000000000, 0.000000000000000000, 0.000000000000000000 ) ) ;
#126199 = ORIENTED_EDGE ( 'NONE', *, *, #83648, .F. ) ;
#126198 = LINE ( 'NONE', #248730, #68247 ) ;
#126200 = CARTESIAN_POINT ( 'NONE',  ( 18.49999999999999645, 1.115600667400684642E-11, -134.0000000000000000 ) ) ;
#126201 = EDGE_LOOP ( 'NONE', ( #133986, #69788, #245492, #220728 ) ) ;
#126202 = CARTESIAN_POINT ( 'NONE',  ( 23.14999999999999503, 6.650000000011155876, -188.8499999999999659 ) ) ;
#126203 = ORIENTED_EDGE ( 'NONE', *, *, #215305, .F. ) ;
#126204 = CARTESIAN_POINT ( 'NONE',  ( -16.97683809663752186, 9.950000000011138823, -154.0976359818037054 ) ) ;
#126206 = ADVANCED_FACE ( 'NONE', ( #171316 ), #2950, .F. ) ;
#126205 = CARTESIAN_POINT ( 'NONE',  ( -23.15000000000000213, 71.65000000001253966, -182.1731074845243938 ) ) ;
#126207 = ORIENTED_EDGE ( 'NONE', *, *, #133909, .F. ) ;
#126209 = DIRECTION ( 'NONE',  ( 1.000000000000000000, -0.000000000000000000, 0.000000000000000000 ) ) ;
#126208 = FACE_OUTER_BOUND ( 'NONE', #201460, .T. ) ;
#126210 = ADVANCED_FACE ( 'NONE', ( #72178 ), #51278, .F. ) ;
#126211 = EDGE_CURVE ( 'NONE', #107243, #162266, #214826, .T. ) ;
#126212 = AXIS2_PLACEMENT_3D ( 'NONE', #142379, #164532, #45852 ) ;
#126213 = CARTESIAN_POINT ( 'NONE',  ( -18.40000000000000213, 64.66825945288641719, -56.87310748452440379 ) ) ;
#126214 = CARTESIAN_POINT ( 'NONE',  ( -12.84409460144754433, 12.47889858296947807, -214.0750992090278260 ) ) ;
#126215 = ORIENTED_EDGE ( 'NONE', *, *, #16887, .T. ) ;
#126216 = ORIENTED_EDGE ( 'NONE', *, *, #142390, .F. ) ;
#126217 = EDGE_CURVE ( 'NONE', #109454, #182460, #256995, .T. ) ;
#126218 = CARTESIAN_POINT ( 'NONE',  ( 21.05000000000000071, 1.835341550235569663, -45.05515129256298223 ) ) ;
#126219 = CARTESIAN_POINT ( 'NONE',  ( 20.94999999999999929, -8.999999999988842703, -191.1060308773475072 ) ) ;
#126220 = ORIENTED_EDGE ( 'NONE', *, *, #142926, .F. ) ;
#126221 = DIRECTION ( 'NONE',  ( 0.000000000000000000, -6.982962677686266711E-15, 1.000000000000000000 ) ) ;
#126222 = ORIENTED_EDGE ( 'NONE', *, *, #132347, .T. ) ;
#126223 = DIRECTION ( 'NONE',  ( 1.000000000000000000, 0.000000000000000000, 0.000000000000000000 ) ) ;
#126224 = ORIENTED_EDGE ( 'NONE', *, *, #171401, .T. ) ;
#126225 = LINE ( 'NONE', #165369, #50293 ) ;
#126226 = EDGE_CURVE ( 'NONE', #82525, #39426, #195978, .T. ) ;
#126227 = CYLINDRICAL_SURFACE ( 'NONE', #107970, 0.1000000000000124678 ) ;
#126228 = ADVANCED_FACE ( 'NONE', ( #231256 ), #232130, .T. ) ;
#126229 = ORIENTED_EDGE ( 'NONE', *, *, #151169, .F. ) ;
#126230 = CARTESIAN_POINT ( 'NONE',  ( 18.58725287972330165, -9.566626910680657403, -207.8225048057653055 ) ) ;
#126231 = VECTOR ( 'NONE', #39845, 1000.000000000000227 ) ;
#126232 = ORIENTED_EDGE ( 'NONE', *, *, #170683, .F. ) ;
#126233 = EDGE_LOOP ( 'NONE', ( #112406, #71031, #93465, #129752 ) ) ;
#126234 = ORIENTED_EDGE ( 'NONE', *, *, #26142, .T. ) ;
#126235 = AXIS2_PLACEMENT_3D ( 'NONE', #58449, #221373, #256614 ) ;
#126236 = CYLINDRICAL_SURFACE ( 'NONE', #17001, 0.1000000000000028644 ) ;
#126237 = DIRECTION ( 'NONE',  ( 0.000000000000000000, 0.000000000000000000, 1.000000000000000000 ) ) ;
#126239 = CARTESIAN_POINT ( 'NONE',  ( 21.13461538461538325, 8.885417037985616773, -45.85000000000000142 ) ) ;
#126238 =( BOUNDED_CURVE ( )  B_SPLINE_CURVE ( 3, ( #138191, #220334, #179928, #75694 ),
 .UNSPECIFIED., .F., .T. ) 
 B_SPLINE_CURVE_WITH_KNOTS ( ( 4, 4 ),
 ( 1.570796326794895448, 3.141592653589791784 ),
 .UNSPECIFIED. ) 
 CURVE ( )  GEOMETRIC_REPRESENTATION_ITEM ( )  RATIONAL_B_SPLINE_CURVE ( ( 1.000000000000000000, 0.8047378541243650485, 0.8047378541243650485, 1.000000000000000000 ) ) 
 REPRESENTATION_ITEM ( '' )  );
#126240 = DIRECTION ( 'NONE',  ( 1.000000000000000000, 3.265361837132813093E-16, -0.000000000000000000 ) ) ;
#126241 = CARTESIAN_POINT ( 'NONE',  ( -20.94999999999999929, 74.26374286841520700, -191.9544551555068779 ) ) ;
#126242 = EDGE_CURVE ( 'NONE', #159539, #87242, #150434, .T. ) ;
#126243 = DIRECTION ( 'NONE',  ( 1.000000000000000000, 0.000000000000000000, 0.000000000000000000 ) ) ;
#126245 = ORIENTED_EDGE ( 'NONE', *, *, #218552, .F. ) ;
#126244 = CARTESIAN_POINT ( 'NONE',  ( 20.90000000000000213, 7.986648289447971116, 1.311673547813416718 ) ) ;
#126246 = CARTESIAN_POINT ( 'NONE',  ( -21.05000000000000071, 6.413662734880721139, -167.5855928633627343 ) ) ;
#126247 = EDGE_LOOP ( 'NONE', ( #241676, #44337, #88651, #189771 ) ) ;
#126248 = DIRECTION ( 'NONE',  ( 0.000000000000000000, 0.1495327102803792052, 0.9887567792719320625 ) ) ;
#126249 = ORIENTED_EDGE ( 'NONE', *, *, #11019, .F. ) ;
#126250 = ORIENTED_EDGE ( 'NONE', *, *, #48446, .F. ) ;
#126251 = DIRECTION ( 'NONE',  ( -1.000000000000000000, 0.000000000000000000, -0.000000000000000000 ) ) ;
#126253 = TOROIDAL_SURFACE ( 'NONE', #1343, 11.70000000000000462, 0.1000000000000000056 ) ;
#126252 = FACE_OUTER_BOUND ( 'NONE', #168614, .T. ) ;
#126254 = AXIS2_PLACEMENT_3D ( 'NONE', #189661, #11022, #249645 ) ;
#126255 = DIRECTION ( 'NONE',  ( -0.7071067811865388020, 0.7071067811865561215, 0.000000000000000000 ) ) ;
#126256 = CIRCLE ( 'NONE', #13834, 0.1999999999999987899 ) ;
#126257 = CARTESIAN_POINT ( 'NONE',  ( 21.05000000000000071, -9.499999999988844479, -57.10603087734755690 ) ) ;
#126258 = ORIENTED_EDGE ( 'NONE', *, *, #115274, .T. ) ;
#126259 = VERTEX_POINT ( 'NONE', #55129 ) ;
#126260 = CIRCLE ( 'NONE', #188617, 0.4000000000000114575 ) ;
#126261 = CARTESIAN_POINT ( 'NONE',  ( 18.59999999999999076, 11.75000000001115907, -108.6000000000000227 ) ) ;
#126262 = EDGE_LOOP ( 'NONE', ( #116477, #2295, #236878, #88321 ) ) ;
#126263 = DIRECTION ( 'NONE',  ( -1.000000000000000000, -0.000000000000000000, -0.000000000000000000 ) ) ;
#126264 = DIRECTION ( 'NONE',  ( -0.000000000000000000, 0.4088369013363281623, -0.9126074666063771490 ) ) ;
#126265 = CARTESIAN_POINT ( 'NONE',  ( -20.94999999999999929, -11.41227409413852989, -170.4999999999999716 ) ) ;
#126266 = CARTESIAN_POINT ( 'NONE',  ( 21.78635804494511419, -1.400458356024840922, -194.1044180137097044 ) ) ;
#126267 = DIRECTION ( 'NONE',  ( 1.000000000000000000, -2.952720810173289112E-16, -2.061873921506763405E-30 ) ) ;
#126268 = DIRECTION ( 'NONE',  ( 1.000000000000000000, 0.000000000000000000, 0.000000000000000000 ) ) ;
#126269 = VERTEX_POINT ( 'NONE', #134680 ) ;
#126270 = DIRECTION ( 'NONE',  ( -0.000000000000000000, -0.000000000000000000, 1.000000000000000000 ) ) ;
#126271 = CIRCLE ( 'NONE', #17929, 0.09999999999999939493 ) ;
#126273 = DIRECTION ( 'NONE',  ( -2.557131231893036492E-16, -0.7049548389605068133, 0.7092521942342976393 ) ) ;
#126272 = TOROIDAL_SURFACE ( 'NONE', #5451, 0.2000000000000000111, 0.1000000000000000056 ) ;
#126274 = DIRECTION ( 'NONE',  ( 0.000000000000000000, -0.4088369013363281068, 0.9126074666063770380 ) ) ;
#126275 = CIRCLE ( 'NONE', #30626, 0.1000000000000001860 ) ;
#126276 = DIRECTION ( 'NONE',  ( -1.000000000000000000, 0.000000000000000000, 0.000000000000000000 ) ) ;
#126277 = EDGE_CURVE ( 'NONE', #236302, #89014, #73477, .T. ) ;
#126278 = CARTESIAN_POINT ( 'NONE',  ( -20.54999999999999716, 54.70975502726918194, -239.2730902609777104 ) ) ;
#126279 = CARTESIAN_POINT ( 'NONE',  ( -16.97683809663752186, 41.03261631955726330, -236.6889770711509584 ) ) ;
#126280 = EDGE_CURVE ( 'NONE', #187086, #155258, #115384, .T. ) ;
#126281 = ORIENTED_EDGE ( 'NONE', *, *, #135079, .T. ) ;
#126282 = EDGE_CURVE ( 'NONE', #103754, #187553, #65498, .T. ) ;
#126283 = DIRECTION ( 'NONE',  ( 0.000000000000000000, -1.000000000000000000, -6.982962677686265922E-15 ) ) ;
#126284 = EDGE_CURVE ( 'NONE', #34916, #169346, #194705, .T. ) ;
#126285 = VERTEX_POINT ( 'NONE', #76011 ) ;
#126286 = PLANE ( 'NONE',  #112791 ) ;
#126287 = DIRECTION ( 'NONE',  ( -1.000000000000000000, -0.000000000000000000, 0.000000000000000000 ) ) ;
#126288 = CARTESIAN_POINT ( 'NONE',  ( 21.09546886439546398, 61.86536912340749694, -221.7206923045749249 ) ) ;
#126289 = CARTESIAN_POINT ( 'NONE',  ( 20.50589344625199217, 65.51681206853677963, -162.4501125058534399 ) ) ;
#126290 = ORIENTED_EDGE ( 'NONE', *, *, #150810, .T. ) ;
#126291 = CARTESIAN_POINT ( 'NONE',  ( 21.05000000000000071, 76.00000000001142553, -36.02310748452432421 ) ) ;
#126292 = AXIS2_PLACEMENT_3D ( 'NONE', #189231, #57059, #148826 ) ;
#126293 = DIRECTION ( 'NONE',  ( 1.000000000000000000, -0.000000000000000000, -0.000000000000000000 ) ) ;
#126294 = CARTESIAN_POINT ( 'NONE',  ( -21.05000000000000071, 1.851028230152016674, -179.1539132694224463 ) ) ;
#126295 = CARTESIAN_POINT ( 'NONE',  ( -18.59999999999999787, 77.86671491006917734, -91.27043223824227880 ) ) ;
#126296 = DIRECTION ( 'NONE',  ( 1.000000000000000000, 0.000000000000000000, 0.000000000000000000 ) ) ;
#126297 = FACE_OUTER_BOUND ( 'NONE', #30765, .T. ) ;
#126298 = ADVANCED_FACE ( 'NONE', ( #155590 ), #218065, .T. ) ;
#126299 = EDGE_LOOP ( 'NONE', ( #251482, #106616, #155224, #244037, #188556, #239411, #230452, #179388, #126362, #98175, #12575, #195773, #21031, #54268, #138339, #257770, #102626, #250529, #229155, #70908, #18495, #178489, #152099, #18781, #105262, #114269, #24082 ) ) ;
#126300 = EDGE_LOOP ( 'NONE', ( #196491, #15088, #83174, #34509 ) ) ;
#126301 = CARTESIAN_POINT ( 'NONE',  ( -18.50000000000000000, 77.68707439010378835, -149.3376804510659213 ) ) ;
#126303 = EDGE_LOOP ( 'NONE', ( #62542, #23790, #206374, #173634 ) ) ;
#126302 = DIRECTION ( 'NONE',  ( 0.000000000000000000, 0.000000000000000000, 1.000000000000000000 ) ) ;
#126304 = AXIS2_PLACEMENT_3D ( 'NONE', #24185, #125825, #103674 ) ;
#126305 = CARTESIAN_POINT ( 'NONE',  ( 11.60000000000006004, 64.35000000001120668, -23.72310748452479601 ) ) ;
#126306 = AXIS2_PLACEMENT_3D ( 'NONE', #189085, #213780, #92535 ) ;
#126307 = DIRECTION ( 'NONE',  ( -1.000000000000000000, -0.000000000000000000, -0.000000000000000000 ) ) ;
#126308 =( BOUNDED_CURVE ( )  B_SPLINE_CURVE ( 3, ( #122036, #46330, #201558, #222380 ),
 .UNSPECIFIED., .F., .F. ) 
 B_SPLINE_CURVE_WITH_KNOTS ( ( 4, 4 ),
 ( 3.432212674861196966, 3.693332928900582068 ),
 .UNSPECIFIED. ) 
 CURVE ( )  GEOMETRIC_REPRESENTATION_ITEM ( )  RATIONAL_B_SPLINE_CURVE ( ( 1.000000000000000000, 0.9943260843901261525, 0.9943260843901261525, 1.000000000000000000 ) ) 
 REPRESENTATION_ITEM ( '' )  );
#126309 = EDGE_LOOP ( 'NONE', ( #163816, #125993, #20764, #100220 ) ) ;
#126310 = CARTESIAN_POINT ( 'NONE',  ( 5.551115123125782702E-14, 67.65000000001118963, -3.123107484524795474 ) ) ;
#126311 = AXIS2_PLACEMENT_3D ( 'NONE', #44229, #99023, #238560 ) ;
#126312 = CONTEXT_DEPENDENT_SHAPE_REPRESENTATION ( #45905, #37089 ) ;
#126314 = CIRCLE ( 'NONE', #59843, 0.1999999999999987899 ) ;
#126313 = DIRECTION ( 'NONE',  ( 0.000000000000000000, -1.000000000000000000, -6.982962677686265922E-15 ) ) ;
#126315 = ORIENTED_EDGE ( 'NONE', *, *, #162162, .T. ) ;
#126316 = AXIS2_PLACEMENT_3D ( 'NONE', #134816, #151871, #54020 ) ;
#126317 = DIRECTION ( 'NONE',  ( 0.000000000000000000, -0.9908441862701791170, 0.1350103645450472789 ) ) ;
#126318 = AXIS2_PLACEMENT_3D ( 'NONE', #142042, #24701, #79491 ) ;
#126319 = CIRCLE ( 'NONE', #13899, 0.1000000000000013933 ) ;
#126320 = PRODUCT ( 'Injection Molded Chain Links 3', 'Injection Molded Chain Links 3', '', ( #114771 ) ) ;
#126321 = EDGE_CURVE ( 'NONE', #232107, #173153, #86320, .T. ) ;
#126322 = VECTOR ( 'NONE', #9077, 1000.000000000000000 ) ;
#126323 = ORIENTED_EDGE ( 'NONE', *, *, #133226, .T. ) ;
#126324 = ORIENTED_EDGE ( 'NONE', *, *, #31943, .T. ) ;
#126325 = DIRECTION ( 'NONE',  ( 0.000000000000000000, 0.000000000000000000, 1.000000000000000000 ) ) ;
#126326 = CARTESIAN_POINT ( 'NONE',  ( -21.05000000000000071, 87.48912529308798014, -100.1231074845242262 ) ) ;
#126328 = CIRCLE ( 'NONE', #63795, 0.09999999999998898659 ) ;
#126327 = DIRECTION ( 'NONE',  ( 0.000000000000000000, 0.000000000000000000, 1.000000000000000000 ) ) ;
#126329 = EDGE_CURVE ( 'NONE', #1255, #28426, #224049, .T. ) ;
#126331 = CIRCLE ( 'NONE', #184586, 11.70000000000000462 ) ;
#126330 = CYLINDRICAL_SURFACE ( 'NONE', #103113, 4.049999999999998046 ) ;
#126332 = CARTESIAN_POINT ( 'NONE',  ( 21.05000000000000071, 6.649999999999999467, -9.843822089683124332 ) ) ;
#126333 = PLANE ( 'NONE',  #57858 ) ;
#126334 = CARTESIAN_POINT ( 'NONE',  ( -16.93262454970420094, 10.00202046793035571, -12.57292377376268888 ) ) ;
#126335 = ADVANCED_FACE ( 'NONE', ( #98106 ), #23775, .F. ) ;
#126337 = CYLINDRICAL_SURFACE ( 'NONE', #178746, 0.09999999999999939493 ) ;
#126336 = DIRECTION ( 'NONE',  ( 3.469446951953347238E-14, -0.6413305999522614931, -0.7672646620071019719 ) ) ;
#126338 = CIRCLE ( 'NONE', #247124, 0.09999999999999939493 ) ;
#126339 = CARTESIAN_POINT ( 'NONE',  ( -23.39999999999994529, 76.00000000001119815, -3.023107484524792277 ) ) ;
#126340 = PLANE ( 'NONE',  #46264 ) ;
#126341 = DIRECTION ( 'NONE',  ( 0.000000000000000000, -1.000000000000000000, -6.982962677686266711E-15 ) ) ;
#126342 = ORIENTED_EDGE ( 'NONE', *, *, #183129, .T. ) ;
#126343 = ORIENTED_EDGE ( 'NONE', *, *, #28764, .F. ) ;
#126344 = LINE ( 'NONE', #147193, #110830 ) ;
#126345 = LINE ( 'NONE', #25978, #74365 ) ;
#126347 = CARTESIAN_POINT ( 'NONE',  ( -18.59999999999999787, 18.27574494880468592, -237.6039235467692947 ) ) ;
#126346 = CARTESIAN_POINT ( 'NONE',  ( -18.59999999999999787, 77.14957036958777792, -128.7071950000224092 ) ) ;
#126349 =( BOUNDED_SURFACE ( )  B_SPLINE_SURFACE ( 3, 2, ( 
 ( #173066, #170508, #249993 ),
 ( #130016, #53065, #229151 ),
 ( #51759, #29688, #190020 ),
 ( #71373, #111766, #212158 ),
 ( #253823, #169201, #149629 ),
 ( #15245, #233018, #109175 ) ),
 .UNSPECIFIED., .F., .F., .F. ) 
 B_SPLINE_SURFACE_WITH_KNOTS ( ( 4, 2, 4 ),
 ( 3, 3 ),
 ( 0.0001342700090130142393, 0.0002909192928057479071, 0.0004475685765984815478 ),
 ( 0.000000000000000000, 1.000000000000000000 ),
 .UNSPECIFIED. ) 
 GEOMETRIC_REPRESENTATION_ITEM ( )  RATIONAL_B_SPLINE_SURFACE ( (
 ( 1.000000000000000000, 0.7250110520819876836, 1.000000000000000000),
 ( 1.000000000000000000, 0.7257599279130237946, 1.000000000000000000),
 ( 1.000000000000000000, 0.7137594617289112486, 1.000000000000000000),
 ( 1.000000000000000000, 0.6959270178805850859, 1.000000000000000000),
 ( 1.000000000000000000, 0.6919879549343305181, 1.000000000000000000),
 ( 1.000000000000000000, 0.7071067811865487940, 1.000000000000000000) ) ) 
 REPRESENTATION_ITEM ( '' )  SURFACE ( )  );
#126348 = CIRCLE ( 'NONE', #193004, 0.09999999999999939493 ) ;
#126350 = CIRCLE ( 'NONE', #88733, 7.800000000000001599 ) ;
#126351 = EDGE_CURVE ( 'NONE', #70690, #133508, #11344, .T. ) ;
#126352 = TOROIDAL_SURFACE ( 'NONE', #163951, 11.70000000000000639, 0.1000000000000000056 ) ;
#126353 = DIRECTION ( 'NONE',  ( -1.000000000000000000, 0.000000000000000000, 0.000000000000000000 ) ) ;
#126354 = DIRECTION ( 'NONE',  ( 0.000000000000000000, -6.982962677686266711E-15, 1.000000000000000000 ) ) ;
#126355 = CARTESIAN_POINT ( 'NONE',  ( 18.59999999999999076, 11.75000000001115907, -58.35000000000000142 ) ) ;
#126356 = EDGE_CURVE ( 'NONE', #93005, #237169, #98783, .T. ) ;
#126357 = EDGE_CURVE ( 'NONE', #66750, #185693, #161993, .T. ) ;
#126358 = ORIENTED_EDGE ( 'NONE', *, *, #254163, .F. ) ;
#126359 = EDGE_LOOP ( 'NONE', ( #226542, #53455, #233100, #9290 ) ) ;
#126360 = DIRECTION ( 'NONE',  ( 1.000000000000000000, 0.000000000000000000, 0.000000000000000000 ) ) ;
#126361 = ADVANCED_FACE ( 'NONE', ( #142396 ), #26577, .T. ) ;
#126362 = ORIENTED_EDGE ( 'NONE', *, *, #215445, .F. ) ;
#126363 = DIRECTION ( 'NONE',  ( -1.000000000000000000, 0.000000000000000000, 0.000000000000000000 ) ) ;
#126364 = CIRCLE ( 'NONE', #47234, 0.1000000000000096922 ) ;
#126365 = AXIS2_PLACEMENT_3D ( 'NONE', #125755, #90483, #246988 ) ;
#126366 = CIRCLE ( 'NONE', #246972, 11.89999999999999858 ) ;
#126367 = CIRCLE ( 'NONE', #226292, 0.1000000000000028644 ) ;
#126368 = CARTESIAN_POINT ( 'NONE',  ( 16.27683809663750125, 41.27791846035906076, -237.2365415511148115 ) ) ;
#126369 = ORIENTED_EDGE ( 'NONE', *, *, #150197, .T. ) ;
#126370 = CARTESIAN_POINT ( 'NONE',  ( -20.85000000000000142, 77.83585931145526615, -58.01866831572577610 ) ) ;
#126371 = EDGE_CURVE ( 'NONE', #87486, #24894, #84064, .T. ) ;
#126372 = ORIENTED_EDGE ( 'NONE', *, *, #59120, .T. ) ;
#126373 = FACE_OUTER_BOUND ( 'NONE', #74884, .T. ) ;
#126374 = CARTESIAN_POINT ( 'NONE',  ( -23.25000000000000000, 46.02130280899747561, -256.6489974955837852 ) ) ;
#126375 = CARTESIAN_POINT ( 'NONE',  ( -23.25000000000000355, 11.75000000001113953, -154.8500000000000227 ) ) ;
#126376 = PLANE ( 'NONE',  #125091 ) ;
#126377 = CARTESIAN_POINT ( 'NONE',  ( -21.14999999999999858, 11.75000000001115552, -174.2838656629781156 ) ) ;
#126378 = CARTESIAN_POINT ( 'NONE',  ( -21.05000000000000071, 77.26178616857765746, -195.4366085209788935 ) ) ;
#126379 = CARTESIAN_POINT ( 'NONE',  ( -20.94999999999999929, 1.115600667400684642E-11, -88.70000000000004547 ) ) ;
#126380 = LINE ( 'NONE', #28623, #137259 ) ;
#126382 = VERTEX_POINT ( 'NONE', #223209 ) ;
#126381 = DIRECTION ( 'NONE',  ( -1.000000000000000000, 0.000000000000000000, -0.000000000000000000 ) ) ;
#126384 = CARTESIAN_POINT ( 'NONE',  ( -21.14999999999999858, 6.540656951712397138, -33.50000000000000000 ) ) ;
#126383 = DIRECTION ( 'NONE',  ( 0.000000000000000000, -0.000000000000000000, -1.000000000000000000 ) ) ;
#126385 = ORIENTED_EDGE ( 'NONE', *, *, #196466, .T. ) ;
#126387 = EDGE_LOOP ( 'NONE', ( #124220, #129035 ) ) ;
#126386 = CARTESIAN_POINT ( 'NONE',  ( 18.49999999999999289, 10.29270135741298731, -139.4573618871519614 ) ) ;
#126388 = ORIENTED_EDGE ( 'NONE', *, *, #191429, .T. ) ;
#126389 = CARTESIAN_POINT ( 'NONE',  ( 23.14999999999999858, 76.00000000001205080, -123.6481074845242887 ) ) ;
#126390 = TOROIDAL_SURFACE ( 'NONE', #143117, 0.2000000000000000111, 0.1000000000000000056 ) ;
#126391 = DIRECTION ( 'NONE',  ( 1.000000000000000000, 0.000000000000000000, 0.000000000000000000 ) ) ;
#126392 = DIRECTION ( 'NONE',  ( 1.000000000000000000, 0.000000000000000000, 0.000000000000000000 ) ) ;
#126393 = DIRECTION ( 'NONE',  ( 0.000000000000000000, 0.000000000000000000, -1.000000000000000000 ) ) ;
#126394 = LINE ( 'NONE', #225473, #166104 ) ;
#126395 = CARTESIAN_POINT ( 'NONE',  ( -17.22767730083581839, 12.52910306356951686, -209.8951030483589193 ) ) ;
#126396 = DIRECTION ( 'NONE',  ( 0.000000000000000000, 0.000000000000000000, -1.000000000000000000 ) ) ;
#126397 = CARTESIAN_POINT ( 'NONE',  ( 21.14999999999999858, 64.35000000001275566, -215.2731074845244450 ) ) ;
#126398 = ORIENTED_EDGE ( 'NONE', *, *, #256833, .F. ) ;
#126399 = VERTEX_POINT ( 'NONE', #244059 ) ;
#126400 = CARTESIAN_POINT ( 'NONE',  ( -20.94999999999999929, 77.25000000001263345, -195.5231074845243313 ) ) ;
#126401 = CIRCLE ( 'NONE', #47268, 0.2000000000000084766 ) ;
#126402 = AXIS2_PLACEMENT_3D ( 'NONE', #178677, #254301, #75702 ) ;
#126403 = ORIENTED_EDGE ( 'NONE', *, *, #120014, .F. ) ;
#126404 = DIRECTION ( 'NONE',  ( 0.000000000000000000, 0.8814952561688476074, -0.4721928772777262417 ) ) ;
#126405 = ORIENTED_EDGE ( 'NONE', *, *, #253664, .F. ) ;
#126406 = CARTESIAN_POINT ( 'NONE',  ( -21.44999999999999929, 44.83341466285084209, -237.8352457803185871 ) ) ;
#126407 = VECTOR ( 'NONE', #137147, 1000.000000000000000 ) ;
#126408 = DIRECTION ( 'NONE',  ( 1.000000000000000000, 0.000000000000000000, 0.000000000000000000 ) ) ;
#126409 = CARTESIAN_POINT ( 'NONE',  ( 18.54999999999999716, 9.950000000011153034, -121.3500000000000938 ) ) ;
#126410 = EDGE_CURVE ( 'NONE', #187924, #189298, #46694, .T. ) ;
#126411 = CARTESIAN_POINT ( 'NONE',  ( -21.10320863425827298, 30.80775347085393889, -252.1449967823172642 ) ) ;
#126412 = CARTESIAN_POINT ( 'NONE',  ( 21.13461538461538680, 10.61458296203669427, -179.7500000000000000 ) ) ;
#126413 = ORIENTED_EDGE ( 'NONE', *, *, #164686, .F. ) ;
#126414 = CARTESIAN_POINT ( 'NONE',  ( -20.85000000000000142, 69.06610602788607878, -166.2374616501508342 ) ) ;
#126415 = EDGE_CURVE ( 'NONE', #60636, #113073, #247912, .T. ) ;
#126416 = EDGE_CURVE ( 'NONE', #136655, #200182, #132155, .T. ) ;
#126418 = CIRCLE ( 'NONE', #76522, 0.1000000000000028644 ) ;
#126417 = CARTESIAN_POINT ( 'NONE',  ( -20.64999999999999858, 54.18117728009210055, -239.0715820348696923 ) ) ;
#126419 = CARTESIAN_POINT ( 'NONE',  ( -21.09813707148783735, 0.03135149954058948085, -27.11493789426332413 ) ) ;
#126420 = FACE_OUTER_BOUND ( 'NONE', #20418, .T. ) ;
#126421 = ORIENTED_EDGE ( 'NONE', *, *, #69411, .F. ) ;
#126423 = FACE_OUTER_BOUND ( 'NONE', #78817, .T. ) ;
#126422 = DIRECTION ( 'NONE',  ( 1.000000000000000000, 0.000000000000000000, 0.000000000000000000 ) ) ;
#126425 = ORIENTED_EDGE ( 'NONE', *, *, #69519, .F. ) ;
#126424 = AXIS2_PLACEMENT_3D ( 'NONE', #18348, #178749, #135714 ) ;
#126428 = VERTEX_POINT ( 'NONE', #126694 ) ;
#126427 = DIRECTION ( 'NONE',  ( -1.000000000000000000, 0.000000000000000000, 0.000000000000000000 ) ) ;
#126426 = DIRECTION ( 'NONE',  ( 1.000000000000000000, 0.000000000000000000, 0.000000000000000000 ) ) ;
#126429 = VERTEX_POINT ( 'NONE', #45868 ) ;
#126430 = CARTESIAN_POINT ( 'NONE',  ( 18.59999999999999787, 74.13328508995425636, -57.77043223824233564 ) ) ;
#126431 = TOROIDAL_SURFACE ( 'NONE', #14014, 12.97499999999999609, 0.1000000000000000056 ) ;
#126432 = CARTESIAN_POINT ( 'NONE',  ( -21.44999999999999929, 68.65000000001222702, -148.7731074845244166 ) ) ;
#126433 = CARTESIAN_POINT ( 'NONE',  ( 18.59999999999999787, 87.75000000001197975, -115.1731074845242233 ) ) ;
#126434 = ORIENTED_EDGE ( 'NONE', *, *, #84140, .T. ) ;
#126435 = CARTESIAN_POINT ( 'NONE',  ( -20.54999999999999716, 29.14863708059993286, -237.4168895852561434 ) ) ;
#126436 = EDGE_CURVE ( 'NONE', #816, #86497, #153046, .T. ) ;
#126437 = CARTESIAN_POINT ( 'NONE',  ( 19.97071067811864609, 54.45410018515091366, -228.7360413143871654 ) ) ;
#126438 = EDGE_CURVE ( 'NONE', #155470, #102511, #109680, .T. ) ;
#126440 = PLANE ( 'NONE',  #67496 ) ;
#126439 = DIRECTION ( 'NONE',  ( 0.000000000000000000, 0.9908441862701605762, -0.1350103645451835310 ) ) ;
#126442 = ORIENTED_EDGE ( 'NONE', *, *, #100533, .T. ) ;
#126441 = CARTESIAN_POINT ( 'NONE',  ( 21.05000000000000071, 11.75000000001115907, -93.48519422934610645 ) ) ;
#126443 = AXIS2_PLACEMENT_3D ( 'NONE', #149662, #49251, #170544 ) ;
#126444 = VECTOR ( 'NONE', #168563, 1000.000000000000000 ) ;
#126445 = CIRCLE ( 'NONE', #163866, 0.5999999999999934275 ) ;
#126446 = ORIENTED_EDGE ( 'NONE', *, *, #223844, .F. ) ;
#126447 = LINE ( 'NONE', #22236, #60407 ) ;
#126448 = CARTESIAN_POINT ( 'NONE',  ( 18.69999999999999929, 6.644425182197215562, 9.641788261573355001 ) ) ;
#126449 = EDGE_LOOP ( 'NONE', ( #227189, #249340, #225928, #210869 ) ) ;
#126450 = B_SPLINE_CURVE_WITH_KNOTS ( 'NONE', 3,
 ( #189277, #37918, #232268, #174893 ),
 .UNSPECIFIED., .F., .F.,
 ( 4, 4 ),
 ( 0.000000000000000000, 7.713889350930393175E-05 ),
 .UNSPECIFIED. ) ;
#126451 = EDGE_CURVE ( 'NONE', #146076, #96541, #157296, .T. ) ;
#126452 = AXIS2_PLACEMENT_3D ( 'NONE', #40970, #219563, #61790 ) ;
#126454 = EDGE_CURVE ( 'NONE', #28788, #105519, #207528, .T. ) ;
#126453 = DIRECTION ( 'NONE',  ( 0.000000000000000000, -1.000000000000000000, 0.000000000000000000 ) ) ;
#126455 = DIRECTION ( 'NONE',  ( 1.000000000000000000, 1.159508501126949537E-16, 2.525285885220370376E-17 ) ) ;
#126456 = EDGE_CURVE ( 'NONE', #151773, #110239, #147540, .T. ) ;
#126457 = ORIENTED_EDGE ( 'NONE', *, *, #191890, .T. ) ;
#126458 = DIRECTION ( 'NONE',  ( 0.000000000000000000, -0.9998779222360097974, 0.01562500000000363945 ) ) ;
#126459 = VECTOR ( 'NONE', #127942, 1000.000000000000000 ) ;
#126460 = VECTOR ( 'NONE', #1350, 1000.000000000000000 ) ;
#126461 = AXIS2_PLACEMENT_3D ( 'NONE', #76647, #156220, #58344 ) ;
#126462 = AXIS2_PLACEMENT_3D ( 'NONE', #146504, #108686, #111261 ) ;
#126464 = EDGE_CURVE ( 'NONE', #116410, #7857, #61604, .T. ) ;
#126463 = EDGE_LOOP ( 'NONE', ( #219790, #235646, #1656, #176830 ) ) ;
#126465 = DIRECTION ( 'NONE',  ( -1.000000000000000000, -1.836970198721029934E-16, 0.000000000000000000 ) ) ;
#126466 = CARTESIAN_POINT ( 'NONE',  ( -18.38204789744325396, 64.52049896284670183, -78.77310748452438816 ) ) ;
#126467 = VERTEX_POINT ( 'NONE', #228367 ) ;
#126468 = ORIENTED_EDGE ( 'NONE', *, *, #77684, .T. ) ;
#126469 = CARTESIAN_POINT ( 'NONE',  ( 23.14999999999999858, 4.813084112149527805, -21.55848224347618114 ) ) ;
#126470 = ORIENTED_EDGE ( 'NONE', *, *, #96311, .F. ) ;
#126472 = ORIENTED_EDGE ( 'NONE', *, *, #43480, .T. ) ;
#126471 = CARTESIAN_POINT ( 'NONE',  ( 12.26145404764308822, 66.64858632091117840, -186.5427639169754173 ) ) ;
#126473 = ORIENTED_EDGE ( 'NONE', *, *, #238295, .F. ) ;
#126476 = ADVANCED_FACE ( 'NONE', ( #47127 ), #49720, .F. ) ;
#126475 = EDGE_LOOP ( 'NONE', ( #154184, #27463, #120857, #108200 ) ) ;
#126474 = VERTEX_POINT ( 'NONE', #242775 ) ;
#126477 = CIRCLE ( 'NONE', #197216, 0.9000000000000014655 ) ;
#126478 = CIRCLE ( 'NONE', #55519, 0.09999999999999530098 ) ;
#126479 = CARTESIAN_POINT ( 'NONE',  ( -20.54999999999999716, 1.115600667400684642E-11, -100.5000000000000426 ) ) ;
#126480 = ORIENTED_EDGE ( 'NONE', *, *, #37329, .F. ) ;
#126481 = CARTESIAN_POINT ( 'NONE',  ( -18.39999999999999858, 11.75000000001113953, -176.7499999999999716 ) ) ;
#126482 = CARTESIAN_POINT ( 'NONE',  ( -18.59999999999999787, 76.00000000001195133, -103.0231074845243171 ) ) ;
#126483 = VECTOR ( 'NONE', #145928, 1000.000000000000000 ) ;
#126484 = DIRECTION ( 'NONE',  ( 0.000000000000000000, -0.9887567792719351711, 0.1495327102803594987 ) ) ;
#126485 = CARTESIAN_POINT ( 'NONE',  ( -18.58744394320964943, 87.01875307878489707, -199.4421687346215037 ) ) ;
#126486 = EDGE_LOOP ( 'NONE', ( #176701, #122695, #14342, #16195 ) ) ;
#126488 = EDGE_LOOP ( 'NONE', ( #257176, #64737, #56141, #240781 ) ) ;
#126487 = VECTOR ( 'NONE', #35324, 1000.000000000000000 ) ;
#126489 = ADVANCED_FACE ( 'NONE', ( #246626 ), #227063, .F. ) ;
#126490 = DIRECTION ( 'NONE',  ( 0.000000000000000000, -0.5341055959866553016, 0.8454177738465993297 ) ) ;
#126491 = CIRCLE ( 'NONE', #197395, 0.1000000000000043771 ) ;
#126493 = EDGE_LOOP ( 'NONE', ( #124928, #241609, #255402, #43321, #49533, #62487, #197535, #52996, #86276, #142807, #4528, #229653, #210829, #203397, #2300, #50766, #167165, #224663 ) ) ;
#126492 = LINE ( 'NONE', #106917, #74270 ) ;
#126494 = DIRECTION ( 'NONE',  ( 1.000000000000000000, 0.000000000000000000, 0.000000000000000000 ) ) ;
#126496 = ORIENTED_EDGE ( 'NONE', *, *, #53523, .F. ) ;
#126495 = DIRECTION ( 'NONE',  ( 1.000000000000000000, 0.000000000000000000, 0.000000000000000000 ) ) ;
#126497 = ORIENTED_EDGE ( 'NONE', *, *, #241429, .T. ) ;
#126498 = CARTESIAN_POINT ( 'NONE',  ( 18.59999999999999432, -1.637172712959223952, -78.58215336547205254 ) ) ;
#126499 = CIRCLE ( 'NONE', #84949, 0.1000000000000028644 ) ;
#126500 = EDGE_CURVE ( 'NONE', #98906, #153515, #174857, .T. ) ;
#126501 = EDGE_CURVE ( 'NONE', #176509, #148744, #15765, .T. ) ;
#126502 = AXIS2_PLACEMENT_3D ( 'NONE', #125515, #146345, #168547 ) ;
#126504 = EDGE_LOOP ( 'NONE', ( #140109, #256965, #148415, #249051, #175044 ) ) ;
#126503 = TOROIDAL_SURFACE ( 'NONE', #159833, 7.800000000000000711, 0.1000000000000000056 ) ;
#126505 = ORIENTED_EDGE ( 'NONE', *, *, #86892, .F. ) ;
#126506 = CIRCLE ( 'NONE', #247101, 0.5000000000000004441 ) ;
#126507 = FACE_OUTER_BOUND ( 'NONE', #5456, .T. ) ;
#126508 = FACE_OUTER_BOUND ( 'NONE', #72616, .T. ) ;
#126509 = CIRCLE ( 'NONE', #151673, 0.1000000000000124678 ) ;
#126510 = EDGE_CURVE ( 'NONE', #218493, #38619, #69805, .T. ) ;
#126512 = VERTEX_POINT ( 'NONE', #54837 ) ;
#126511 = EDGE_LOOP ( 'NONE', ( #80678, #107450, #104847 ) ) ;
#126513 = ORIENTED_EDGE ( 'NONE', *, *, #87740, .F. ) ;
#126515 = EDGE_CURVE ( 'NONE', #86438, #240059, #3123, .T. ) ;
#126514 = CARTESIAN_POINT ( 'NONE',  ( -16.97683809663752186, 9.950000000011138823, -53.59763598180368405 ) ) ;
#126516 = ORIENTED_EDGE ( 'NONE', *, *, #151790, .F. ) ;
#126517 = ORIENTED_EDGE ( 'NONE', *, *, #121659, .T. ) ;
#126518 = CARTESIAN_POINT ( 'NONE',  ( 20.46382478191414833, 65.40137955871422548, -61.84529301517892463 ) ) ;
#126520 = EDGE_LOOP ( 'NONE', ( #15428, #220207, #80128, #131481, #159625 ) ) ;
#126519 = CARTESIAN_POINT ( 'NONE',  ( -21.14999999999999858, 18.65704504850842582, -226.5784250989226507 ) ) ;
#126521 = DIRECTION ( 'NONE',  ( 2.557131231893037478E-16, 0.8660254037844420383, -0.4999999999999943379 ) ) ;
#126523 = CARTESIAN_POINT ( 'NONE',  ( -21.65000000000000213, 68.29142135624935861, -124.1731074845243512 ) ) ;
#126522 = DIRECTION ( 'NONE',  ( 0.000000000000000000, -1.000000000000000000, 0.000000000000000000 ) ) ;
#126524 = CARTESIAN_POINT ( 'NONE',  ( 18.50000000000000355, 85.42145614550778987, -196.2811254005050330 ) ) ;
#126525 = CARTESIAN_POINT ( 'NONE',  ( -13.77178122865954535, 62.03415779510192607, -218.8921516991029534 ) ) ;
#126526 = EDGE_LOOP ( 'NONE', ( #222188, #159033, #221997, #68884 ) ) ;
#126527 = ORIENTED_EDGE ( 'NONE', *, *, #194625, .T. ) ;
#126528 = CIRCLE ( 'NONE', #97251, 0.2000000000000057288 ) ;
#126529 = LINE ( 'NONE', #147375, #148548 ) ;
#126531 = ADVANCED_FACE ( 'NONE', ( #234778 ), #53212, .F. ) ;
#126530 = DIRECTION ( 'NONE',  ( 0.000000000000000000, 0.7397890806274345366, 0.6728388485992877754 ) ) ;
#126532 = ORIENTED_EDGE ( 'NONE', *, *, #13491, .T. ) ;
#126533 = ADVANCED_FACE ( 'NONE', ( #232233 ), #191831, .T. ) ;
#126534 = AXIS2_PLACEMENT_3D ( 'NONE', #161140, #116869, #136397 ) ;
#126535 = CIRCLE ( 'NONE', #93200, 0.09999999999999609201 ) ;
#126536 = CARTESIAN_POINT ( 'NONE',  ( 23.14999999999999858, 67.23127455305835554, -235.8551265064784559 ) ) ;
#126537 = EDGE_LOOP ( 'NONE', ( #65198, #124706, #6901 ) ) ;
#126538 = ORIENTED_EDGE ( 'NONE', *, *, #27177, .F. ) ;
#126539 = EDGE_CURVE ( 'NONE', #182622, #196101, #150129, .T. ) ;
#126540 = CARTESIAN_POINT ( 'NONE',  ( -21.05000000000000071, 5.900000000011102586, -77.21909976465646253 ) ) ;
#126541 = DIRECTION ( 'NONE',  ( 0.000000000000000000, 0.2534589355812664757, 0.9673461469267405910 ) ) ;
#126542 = EDGE_LOOP ( 'NONE', ( #206363, #58950, #237940, #141255 ) ) ;
#126543 = CARTESIAN_POINT ( 'NONE',  ( -20.94999999999999929, 11.60000000001115339, -107.4282032302755852 ) ) ;
#126544 = CARTESIAN_POINT ( 'NONE',  ( 21.12802099929860944, 8.780552590233368093, -112.7481899849316420 ) ) ;
#126545 = ORIENTED_EDGE ( 'NONE', *, *, #143595, .F. ) ;
#126546 = DIRECTION ( 'NONE',  ( 1.000000000000000000, 0.000000000000000000, 0.000000000000000000 ) ) ;
#126547 = CARTESIAN_POINT ( 'NONE',  ( -20.64999999999999858, 73.60000000001200249, -116.2477294072864140 ) ) ;
#126549 = CARTESIAN_POINT ( 'NONE',  ( 23.14999999999999503, 11.65000000001116298, -21.75000000000000355 ) ) ;
#126548 = DIRECTION ( 'NONE',  ( 1.000000000000000000, 0.000000000000000000, 0.000000000000000000 ) ) ;
#126550 = DIRECTION ( 'NONE',  ( 1.000000000000000000, 0.000000000000000000, 0.000000000000000000 ) ) ;
#126551 = DIRECTION ( 'NONE',  ( 0.000000000000000000, -7.034366652768095332E-15, 1.000000000000000000 ) ) ;
#126553 = EDGE_CURVE ( 'NONE', #6055, #234784, #190613, .T. ) ;
#126552 = DIRECTION ( 'NONE',  ( 0.000000000000000000, -1.000000000000000000, -6.982962677686265922E-15 ) ) ;
#126554 = DIRECTION ( 'NONE',  ( -1.836970198721029934E-16, -1.000000000000000000, -6.982962677686266711E-15 ) ) ;
#126555 = EDGE_CURVE ( 'NONE', #194263, #122855, #71869, .T. ) ;
#126557 = ORIENTED_EDGE ( 'NONE', *, *, #200652, .T. ) ;
#126556 = AXIS2_PLACEMENT_3D ( 'NONE', #21262, #138571, #83729 ) ;
#126558 = PRESENTATION_LAYER_ASSIGNMENT (  '', '', ( #113894 ) ) ;
#126559 = AXIS2_PLACEMENT_3D ( 'NONE', #230093, #149300, #89289 ) ;
#126561 = ORIENTED_EDGE ( 'NONE', *, *, #181995, .F. ) ;
#126560 = VERTEX_POINT ( 'NONE', #32765 ) ;
#126562 = ORIENTED_EDGE ( 'NONE', *, *, #227403, .T. ) ;
#126563 = DIRECTION ( 'NONE',  ( 1.000000000000000000, -0.000000000000000000, -0.000000000000000000 ) ) ;
#126564 = CARTESIAN_POINT ( 'NONE',  ( 20.94999999999999929, 14.86477715130881272, -235.7932433709592601 ) ) ;
#126565 = ADVANCED_FACE ( 'NONE', ( #53575 ), #212660, .T. ) ;
#126566 = B_SPLINE_CURVE_WITH_KNOTS ( 'NONE', 3,
 ( #240921, #67411, #42714, #7429, #243478, #102657, #184787, #86944, #64834, #166545, #84350, #165229, #204341, #4838, #123540, #220072, #85649, #63551, #81802 ),
 .UNSPECIFIED., .F., .F.,
 ( 4, 3, 3, 3, 3, 3, 4 ),
 ( 0.000000000000000000, 1.655171619026472822E-05, 2.773500582848447909E-05, 5.941817267378178010E-05, 0.0001114174635873323616, 0.0001914169455916120898, 0.0002627181070750313511 ),
 .UNSPECIFIED. ) ;
#126568 = CARTESIAN_POINT ( 'NONE',  ( -17.11825945287482753, 9.950000000011140600, -146.6500000000000341 ) ) ;
#126567 = CARTESIAN_POINT ( 'NONE',  ( -20.64999999999999858, 7.150000000011155876, -45.75000000000000000 ) ) ;
#126569 = EDGE_CURVE ( 'NONE', #106788, #69230, #136384, .T. ) ;
#126570 = CARTESIAN_POINT ( 'NONE',  ( -18.59999999999999787, -1.261786168553869603, -142.0864989635454947 ) ) ;
#126571 = VERTEX_POINT ( 'NONE', #1281 ) ;
#126572 = CARTESIAN_POINT ( 'NONE',  ( 20.94999999999999574, 14.00000000001115730, -38.92709253038254502 ) ) ;
#126573 = CARTESIAN_POINT ( 'NONE',  ( -21.05000000000000071, -7.589415207398530052E-16, 6.540656951701240729 ) ) ;
#126574 = CARTESIAN_POINT ( 'NONE',  ( -16.81744102076749314, 9.949999999999986855, -12.65000000000000213 ) ) ;
#126575 = CARTESIAN_POINT ( 'NONE',  ( 23.14999999999999858, 66.41360075038569732, -234.0299115732657071 ) ) ;
#126576 = ORIENTED_EDGE ( 'NONE', *, *, #249502, .F. ) ;
#126577 = DIRECTION ( 'NONE',  ( 0.000000000000000000, 2.891205793294679805E-16, -1.000000000000000000 ) ) ;
#126578 = CIRCLE ( 'NONE', #5741, 0.1000000000000028644 ) ;
#126579 = DIRECTION ( 'NONE',  ( 1.000000000000000000, 0.000000000000000000, 0.000000000000000000 ) ) ;
#126580 = EDGE_LOOP ( 'NONE', ( #69063, #62887, #98523, #237663, #146033, #149493, #224585, #152901, #98038, #171764, #150974, #197093 ) ) ;
#126581 = ORIENTED_EDGE ( 'NONE', *, *, #77361, .F. ) ;
#126582 = CARTESIAN_POINT ( 'NONE',  ( -20.94999999999999929, -1.849153571964891274, -179.1059666197970728 ) ) ;
#126583 = CARTESIAN_POINT ( 'NONE',  ( -22.42357213249529124, 0.4119679992451404926, -230.0222526030509016 ) ) ;
#126584 = CARTESIAN_POINT ( 'NONE',  ( 18.49999999999999289, 15.53922597307775000, -223.0482397989536025 ) ) ;
#126585 = DIRECTION ( 'NONE',  ( -1.000000000000000000, 0.000000000000000000, -0.000000000000000000 ) ) ;
#126586 = CARTESIAN_POINT ( 'NONE',  ( 18.59999999999999432, 74.26374286841446803, -91.45445515550682103 ) ) ;
#126587 = CARTESIAN_POINT ( 'NONE',  ( 18.39999999999999503, 5.650000000011139001, -54.35000000000000142 ) ) ;
#126588 = ORIENTED_EDGE ( 'NONE', *, *, #51930, .T. ) ;
#126589 = DIRECTION ( 'NONE',  ( 0.000000000000000000, -7.056502275159890832E-15, 1.000000000000000000 ) ) ;
#126590 = DIRECTION ( 'NONE',  ( 1.000000000000000000, 0.000000000000000000, 0.000000000000000000 ) ) ;
#126592 = FACE_OUTER_BOUND ( 'NONE', #169959, .T. ) ;
#126591 = CARTESIAN_POINT ( 'NONE',  ( -16.93860193097148326, 9.993107767340399405, -87.90013836730690855 ) ) ;
#126593 = CARTESIAN_POINT ( 'NONE',  ( 21.00000000000000000, 9.750000000011153745, -188.7499999999999716 ) ) ;
#126594 = CARTESIAN_POINT ( 'NONE',  ( -20.64999999999999858, 68.76258920191057200, -222.5680764032308048 ) ) ;
#126595 = EDGE_CURVE ( 'NONE', #127923, #4697, #79845, .T. ) ;
#126596 = SPHERICAL_SURFACE ( 'NONE', #153745, 0.1000000000000000056 ) ;
#126597 = CARTESIAN_POINT ( 'NONE',  ( 18.41416235934317314, -9.499999999988842703, -207.6001893912219884 ) ) ;
#126598 = VECTOR ( 'NONE', #64220, 1000.000000000000000 ) ;
#126600 = ORIENTED_EDGE ( 'NONE', *, *, #64251, .T. ) ;
#126599 = CYLINDRICAL_SURFACE ( 'NONE', #11290, 0.1000000000000004496 ) ;
#126601 = ADVANCED_FACE ( 'NONE', ( #96524 ), #181244, .F. ) ;
#126602 = VECTOR ( 'NONE', #135542, 1000.000000000000000 ) ;
#126603 = CARTESIAN_POINT ( 'NONE',  ( 21.30740335185486245, 6.556657922039159203, -100.4010654742241826 ) ) ;
#126605 = CARTESIAN_POINT ( 'NONE',  ( -18.59999999999999787, 1.115600667400684642E-11, -167.5000000000000284 ) ) ;
#126604 = CIRCLE ( 'NONE', #72640, 0.09999999999998898659 ) ;
#126606 = EDGE_CURVE ( 'NONE', #228033, #236044, #194725, .T. ) ;
#126607 = CARTESIAN_POINT ( 'NONE',  ( 15.15590539855246099, 9.410682294279107296, -149.4311434419482794 ) ) ;
#126608 = ORIENTED_EDGE ( 'NONE', *, *, #89537, .T. ) ;
#126609 = VECTOR ( 'NONE', #12793, 1000.000000000000000 ) ;
#126610 = CARTESIAN_POINT ( 'NONE',  ( -21.05000000000000071, 62.00000000001175238, -74.95020001490686923 ) ) ;
#126611 = AXIS2_PLACEMENT_3D ( 'NONE', #10003, #170415, #33462 ) ;
#126612 = CARTESIAN_POINT ( 'NONE',  ( 20.94999999999999929, 71.14953271029195037, -57.48884007552268116 ) ) ;
#126613 = LINE ( 'NONE', #189159, #111055 ) ;
#126614 = CIRCLE ( 'NONE', #134777, 0.09999999999999939493 ) ;
#126615 = EDGE_LOOP ( 'NONE', ( #39346, #111714, #136122, #144220 ) ) ;
#126616 = CARTESIAN_POINT ( 'NONE',  ( -17.11825945287482753, 65.95000000001159890, -56.87310748452439668 ) ) ;
#126618 = ORIENTED_EDGE ( 'NONE', *, *, #59620, .F. ) ;
#126617 = DIRECTION ( 'NONE',  ( -0.000000000000000000, 0.1350103645451876666, -0.9908441862701600211 ) ) ;
#126620 = CARTESIAN_POINT ( 'NONE',  ( 20.95000000000005969, 65.36599112033563586, -30.02023607076051803 ) ) ;
#126619 = LINE ( 'NONE', #165770, #117220 ) ;
#126621 = ORIENTED_EDGE ( 'NONE', *, *, #226340, .F. ) ;
#126622 = AXIS2_PLACEMENT_3D ( 'NONE', #175341, #151925, #112774 ) ;
#126623 = DIRECTION ( 'NONE',  ( 1.000000000000000000, 0.000000000000000000, 0.000000000000000000 ) ) ;
#126625 = FACE_OUTER_BOUND ( 'NONE', #200899, .T. ) ;
#126624 = CIRCLE ( 'NONE', #1528, 1.749999999999999778 ) ;
#126627 = VECTOR ( 'NONE', #97811, 1000.000000000000000 ) ;
#126626 = DIRECTION ( 'NONE',  ( 0.000000000000000000, 1.000000000000000000, -0.000000000000000000 ) ) ;
#126628 = LINE ( 'NONE', #78805, #237869 ) ;
#126629 = ORIENTED_EDGE ( 'NONE', *, *, #52203, .F. ) ;
#126630 = DIRECTION ( 'NONE',  ( 0.000000000000000000, 0.01562499999998609446, -0.9998779222360101304 ) ) ;
#126631 = DIRECTION ( 'NONE',  ( 0.000000000000000000, 0.000000000000000000, -1.000000000000000000 ) ) ;
#126632 = AXIS2_PLACEMENT_3D ( 'NONE', #72237, #250844, #190919 ) ;
#126633 = DIRECTION ( 'NONE',  ( -7.304098846218135653E-16, 0.9651348961777157509, -0.2617529984165031243 ) ) ;
#126634 = AXIS2_PLACEMENT_3D ( 'NONE', #118770, #61348, #78329 ) ;
#126635 = CARTESIAN_POINT ( 'NONE',  ( -22.50000000000000000, 0.1000000000111554016, -122.3504291924552234 ) ) ;
#126636 = EDGE_LOOP ( 'NONE', ( #189068, #86645, #197057, #88386 ) ) ;
#126637 = VERTEX_POINT ( 'NONE', #139514 ) ;
#126638 = VECTOR ( 'NONE', #123889, 1000.000000000000000 ) ;
#126639 = DIRECTION ( 'NONE',  ( 0.000000000000000000, 1.000000000000000000, 0.000000000000000000 ) ) ;
#126640 = AXIS2_PLACEMENT_3D ( 'NONE', #71891, #211390, #191857 ) ;
#126641 = CIRCLE ( 'NONE', #193298, 0.09999999999999939493 ) ;
#126642 = CARTESIAN_POINT ( 'NONE',  ( 18.42636655943171320, 85.49694431578251397, -96.41402691336872977 ) ) ;
#126643 = CARTESIAN_POINT ( 'NONE',  ( -20.94999999999999929, 76.25610579210417939, -103.0580039261966050 ) ) ;
#126644 = CARTESIAN_POINT ( 'NONE',  ( 20.95512820512820085, 10.62384868372303615, -141.6649135690876449 ) ) ;
#126645 = CARTESIAN_POINT ( 'NONE',  ( -21.55000000000000426, 7.708578643773852157, -155.1500000000000057 ) ) ;
#126646 = EDGE_CURVE ( 'NONE', #154058, #77073, #238630, .T. ) ;
#126648 = DIRECTION ( 'NONE',  ( 0.000000000000000000, -1.000000000000000000, 0.000000000000000000 ) ) ;
#126647 = DIRECTION ( 'NONE',  ( 0.000000000000000000, -1.000000000000000000, -1.897661533703519897E-16 ) ) ;
#126649 = DIRECTION ( 'NONE',  ( 1.000000000000000000, 0.000000000000000000, 0.000000000000000000 ) ) ;
#126650 = DIRECTION ( 'NONE',  ( -1.000000000000000000, 0.000000000000000000, 0.000000000000000000 ) ) ;
#126651 = CARTESIAN_POINT ( 'NONE',  ( 18.49999999999999289, 19.00443933019177223, -232.7770257915295531 ) ) ;
#126652 = DIRECTION ( 'NONE',  ( 1.000000000000000000, -3.265361837132813093E-16, -2.280189983783949500E-30 ) ) ;
#126654 = EDGE_LOOP ( 'NONE', ( #11474, #119423, #199199, #160838 ) ) ;
#126653 = CARTESIAN_POINT ( 'NONE',  ( 13.77030915526557386, 62.94440715787351337, -215.5359628679902357 ) ) ;
#126655 = CARTESIAN_POINT ( 'NONE',  ( -20.85000000000000142, 0.000000000000000000, -33.50000000000000000 ) ) ;
#126656 = DIRECTION ( 'NONE',  ( 0.000000000000000000, -1.000000000000000000, -0.000000000000000000 ) ) ;
#126658 = FACE_OUTER_BOUND ( 'NONE', #36457, .T. ) ;
#126657 = CARTESIAN_POINT ( 'NONE',  ( 21.15000000000005542, 83.80000000001119531, -34.86056257560453986 ) ) ;
#126659 = EDGE_CURVE ( 'NONE', #19568, #200, #28310, .T. ) ;
#126660 = ORIENTED_EDGE ( 'NONE', *, *, #188299, .F. ) ;
#126661 = CARTESIAN_POINT ( 'NONE',  ( -20.94999999999999929, 1.115600667400684642E-11, -100.5000000000000426 ) ) ;
#126662 = DIRECTION ( 'NONE',  ( 1.000000000000000000, 0.000000000000000000, 0.000000000000000000 ) ) ;
#126663 = LINE ( 'NONE', #9283, #184601 ) ;
#126664 = DIRECTION ( 'NONE',  ( 0.000000000000000000, -1.000000000000000000, 0.000000000000000000 ) ) ;
#126665 = EDGE_CURVE ( 'NONE', #65850, #100316, #15665, .T. ) ;
#126666 = ORIENTED_EDGE ( 'NONE', *, *, #54762, .T. ) ;
#126667 = ORIENTED_EDGE ( 'NONE', *, *, #244263, .F. ) ;
#126668 = VECTOR ( 'NONE', #18506, 1000.000000000000000 ) ;
#126669 = AXIS2_PLACEMENT_3D ( 'NONE', #158509, #97172, #196314 ) ;
#126670 = CARTESIAN_POINT ( 'NONE',  ( -21.14999999999999858, 31.94635157770351341, -238.7871412784868994 ) ) ;
#126671 = EDGE_CURVE ( 'NONE', #12740, #9341, #153208, .T. ) ;
#126672 = ORIENTED_EDGE ( 'NONE', *, *, #202215, .F. ) ;
#126673 = CARTESIAN_POINT ( 'NONE',  ( 20.85000000000000142, 67.23127455305835554, -235.8551265064784559 ) ) ;
#126674 = AXIS2_PLACEMENT_3D ( 'NONE', #177085, #77940, #58360 ) ;
#126675 = EDGE_LOOP ( 'NONE', ( #139876, #198897, #94702, #144301, #44806, #195466, #134876, #6858, #34014, #3314, #112814, #204420 ) ) ;
#126676 =( BOUNDED_CURVE ( )  B_SPLINE_CURVE ( 3, ( #108123, #187677, #9017, #228075 ),
 .UNSPECIFIED., .F., .T. ) 
 B_SPLINE_CURVE_WITH_KNOTS ( ( 4, 4 ),
 ( 3.141592653589791784, 4.712388980384688786 ),
 .UNSPECIFIED. ) 
 CURVE ( )  GEOMETRIC_REPRESENTATION_ITEM ( )  RATIONAL_B_SPLINE_CURVE ( ( 1.000000000000000000, 0.8047378541243649375, 0.8047378541243649375, 1.000000000000000000 ) ) 
 REPRESENTATION_ITEM ( '' )  );
#126677 = DIRECTION ( 'NONE',  ( 0.000000000000000000, 0.000000000000000000, 1.000000000000000000 ) ) ;
#126678 = DIRECTION ( 'NONE',  ( -0.000000000000000000, 0.9770955615653313941, 0.2128009952263603954 ) ) ;
#126679 = AXIS2_PLACEMENT_3D ( 'NONE', #84687, #6467, #83413 ) ;
#126680 = VECTOR ( 'NONE', #243287, 1000.000000000000000 ) ;
#126681 = DIRECTION ( 'NONE',  ( -0.000000000000000000, -0.000000000000000000, -1.000000000000000000 ) ) ;
#126682 = ORIENTED_EDGE ( 'NONE', *, *, #218958, .F. ) ;
#126683 = ADVANCED_FACE ( 'NONE', ( #101646 ), #97801, .F. ) ;
#126684 = AXIS2_PLACEMENT_3D ( 'NONE', #90417, #72168, #95559 ) ;
#126685 = DIRECTION ( 'NONE',  ( 1.000000000000000000, 0.000000000000000000, 0.000000000000000000 ) ) ;
#126686 = DIRECTION ( 'NONE',  ( -1.000000000000000000, 0.000000000000000000, -0.000000000000000000 ) ) ;
#126688 = AXIS2_PLACEMENT_3D ( 'NONE', #99064, #203335, #239901 ) ;
#126687 = FACE_OUTER_BOUND ( 'NONE', #251776, .T. ) ;
#126689 = PLANE ( 'NONE',  #245696 ) ;
#126691 = CIRCLE ( 'NONE', #68249, 0.1000000000000010186 ) ;
#126690 = CARTESIAN_POINT ( 'NONE',  ( 18.69999999999999929, 7.973296578895943121, 1.410778198689824903 ) ) ;
#126692 = CARTESIAN_POINT ( 'NONE',  ( 18.54999999999999716, 8.750000000011182166, -87.85000000000003695 ) ) ;
#126693 = VECTOR ( 'NONE', #79054, 1000.000000000000000 ) ;
#126694 = CARTESIAN_POINT ( 'NONE',  ( 20.95512820512820440, 61.84489010471549619, -221.8053782964821039 ) ) ;
#126695 = ORIENTED_EDGE ( 'NONE', *, *, #123483, .F. ) ;
#126697 = DIRECTION ( 'NONE',  ( 0.000000000000000000, -0.9126074666063769270, -0.4088369013363282733 ) ) ;
#126696 = LINE ( 'NONE', #48430, #128382 ) ;
#126698 = VERTEX_POINT ( 'NONE', #156560 ) ;
#126699 = VERTEX_POINT ( 'NONE', #241212 ) ;
#126700 = VECTOR ( 'NONE', #7474, 1000.000000000000000 ) ;
#126701 = ORIENTED_EDGE ( 'NONE', *, *, #162393, .T. ) ;
#126702 = DIRECTION ( 'NONE',  ( -1.000000000000000000, -0.000000000000000000, -0.000000000000000000 ) ) ;
#126703 = CARTESIAN_POINT ( 'NONE',  ( 18.50596464788227280, 10.30632246271648889, -72.50418367788958562 ) ) ;
#126704 = DIRECTION ( 'NONE',  ( 0.000000000000000000, 1.000000000000000000, -0.000000000000000000 ) ) ;
#126705 = ORIENTED_EDGE ( 'NONE', *, *, #17861, .T. ) ;
#126706 = DIRECTION ( 'NONE',  ( 0.000000000000000000, 0.000000000000000000, -1.000000000000000000 ) ) ;
#126708 = FACE_OUTER_BOUND ( 'NONE', #168516, .T. ) ;
#126707 = CIRCLE ( 'NONE', #135047, 0.1000000000000001860 ) ;
#126709 = VERTEX_POINT ( 'NONE', #239925 ) ;
#126710 = B_SPLINE_CURVE_WITH_KNOTS ( 'NONE', 3,
 ( #127562, #88403, #227944, #128855, #123717, #203242, #166719, #246228, #148416, #67583 ),
 .UNSPECIFIED., .F., .F.,
 ( 4, 3, 3, 4 ),
 ( 0.000000000000000000, 0.0002000000000002785953, 0.001000000000045107385, 0.001967863649472122601 ),
 .UNSPECIFIED. ) ;
#126711 = CARTESIAN_POINT ( 'NONE',  ( 22.39999999999999503, -0.09999999999999939493, 11.64957080754479968 ) ) ;
#126712 = TOROIDAL_SURFACE ( 'NONE', #109943, 0.2000000000000000111, 0.1000000000000000056 ) ;
#126713 = LINE ( 'NONE', #206254, #180821 ) ;
#126714 = VERTEX_POINT ( 'NONE', #177403 ) ;
#126715 = CARTESIAN_POINT ( 'NONE',  ( 21.05000000000000071, 28.60154115857409352, -258.4512230915049713 ) ) ;
#126716 = AXIS2_PLACEMENT_3D ( 'NONE', #203490, #65255, #24877 ) ;
#126717 = AXIS2_PLACEMENT_3D ( 'NONE', #195774, #17133, #233601 ) ;
#126718 = EDGE_CURVE ( 'NONE', #180781, #114870, #39171, .T. ) ;
#126719 = ORIENTED_EDGE ( 'NONE', *, *, #96633, .T. ) ;
#126720 = AXIS2_PLACEMENT_3D ( 'NONE', #36912, #216783, #154305 ) ;
#126721 = CARTESIAN_POINT ( 'NONE',  ( -22.39999999999999858, 11.45959274888149970, -198.4018787499352641 ) ) ;
#126722 = ORIENTED_EDGE ( 'NONE', *, *, #233429, .F. ) ;
#126723 = FACE_OUTER_BOUND ( 'NONE', #216340, .T. ) ;
#126724 = CARTESIAN_POINT ( 'NONE',  ( 20.85000000000000142, 64.25000000001175238, -76.30697314750248950 ) ) ;
#126725 = CARTESIAN_POINT ( 'NONE',  ( 22.88900146558018989, 29.61793127808049775, -235.9054720201688156 ) ) ;
#126726 = ADVANCED_FACE ( 'NONE', ( #20895 ), #100371, .F. ) ;
#126727 = CARTESIAN_POINT ( 'NONE',  ( -21.14999999999999858, 12.91220014178004050, -205.0716606970938187 ) ) ;
#126728 = ADVANCED_FACE ( 'NONE', ( #57403 ), #179951, .F. ) ;
#126729 = EDGE_CURVE ( 'NONE', #92094, #160394, #220361, .T. ) ;
#126730 = CYLINDRICAL_SURFACE ( 'NONE', #161344, 12.87499999999999822 ) ;
#126731 = DIRECTION ( 'NONE',  ( -0.000000000000000000, -1.000000000000000000, -0.000000000000000000 ) ) ;
#126732 = AXIS2_PLACEMENT_3D ( 'NONE', #130687, #111132, #231103 ) ;
#126733 = ORIENTED_EDGE ( 'NONE', *, *, #254182, .F. ) ;
#126735 = DIRECTION ( 'NONE',  ( 0.000000000000000000, -0.9651348961777161950, 0.2617529984165014589 ) ) ;
#126734 = DIRECTION ( 'NONE',  ( -1.000000000000000000, 0.000000000000000000, 1.073024830501117725E-15 ) ) ;
#126736 = VERTEX_POINT ( 'NONE', #142085 ) ;
#126737 = CARTESIAN_POINT ( 'NONE',  ( -20.64999999999999858, 2.000000000011154189, -87.27537807723794572 ) ) ;
#126738 = DIRECTION ( 'NONE',  ( 0.000000000000000000, 0.000000000000000000, 1.000000000000000000 ) ) ;
#126739 = DIRECTION ( 'NONE',  ( 1.000000000000000000, 0.000000000000000000, 0.000000000000000000 ) ) ;
#126740 = VECTOR ( 'NONE', #104155, 1000.000000000000000 ) ;
#126743 = EDGE_CURVE ( 'NONE', #109777, #71883, #232313, .T. ) ;
#126742 = ORIENTED_EDGE ( 'NONE', *, *, #111204, .T. ) ;
#126741 = SPHERICAL_SURFACE ( 'NONE', #21206, 0.1000000000000000056 ) ;
#126745 = ORIENTED_EDGE ( 'NONE', *, *, #117042, .T. ) ;
#126744 = DIRECTION ( 'NONE',  ( 4.336808689942017736E-16, 0.000000000000000000, 1.000000000000000000 ) ) ;
#126746 = EDGE_CURVE ( 'NONE', #114547, #140343, #119896, .T. ) ;
#126747 = DIRECTION ( 'NONE',  ( 0.000000000000000000, 0.2617529984164856383, 0.9651348961777204138 ) ) ;
#126748 = EDGE_CURVE ( 'NONE', #19120, #23864, #7413, .T. ) ;
#126749 = CARTESIAN_POINT ( 'NONE',  ( 22.84999999999999787, 0.000000000000000000, 0.000000000000000000 ) ) ;
#126751 = ORIENTED_EDGE ( 'NONE', *, *, #5209, .F. ) ;
#126750 = CARTESIAN_POINT ( 'NONE',  ( -16.88593481969334675, 9.950560090095464716, -154.8518722569445174 ) ) ;
#126752 = DIRECTION ( 'NONE',  ( 0.000000000000000000, -1.000000000000000000, -6.982962677686265922E-15 ) ) ;
#126753 = VECTOR ( 'NONE', #36300, 1000.000000000000000 ) ;
#126754 = ORIENTED_EDGE ( 'NONE', *, *, #175210, .F. ) ;
#126755 = CYLINDRICAL_SURFACE ( 'NONE', #172638, 0.1000000000000028644 ) ;
#126756 = ORIENTED_EDGE ( 'NONE', *, *, #249182, .T. ) ;
#126757 = EDGE_CURVE ( 'NONE', #5184, #127256, #36508, .T. ) ;
#126759 = ADVANCED_FACE ( 'NONE', ( #246332 ), #243763, .F. ) ;
#126758 = DIRECTION ( 'NONE',  ( -0.000000000000000000, 0.1298341882520022694, 0.9915357197604853789 ) ) ;
#126760 = CARTESIAN_POINT ( 'NONE',  ( -2.995603634470891112E-16, 87.75000000001178080, -78.27310748452423184 ) ) ;
#126761 = EDGE_CURVE ( 'NONE', #5002, #29239, #98982, .T. ) ;
#126762 = ORIENTED_EDGE ( 'NONE', *, *, #198016, .T. ) ;
#126763 = DIRECTION ( 'NONE',  ( -0.000000000000000000, 1.000000000000000000, 1.734723475976807292E-15 ) ) ;
#126764 = DIRECTION ( 'NONE',  ( 0.000000000000000000, 0.000000000000000000, -1.000000000000000000 ) ) ;
#126765 = VERTEX_POINT ( 'NONE', #166831 ) ;
#126766 = AXIS2_PLACEMENT_3D ( 'NONE', #6184, #182280, #220117 ) ;
#126767 = FACE_OUTER_BOUND ( 'NONE', #212186, .T. ) ;
#126768 = AXIS2_PLACEMENT_3D ( 'NONE', #49073, #227705, #205568 ) ;
#126769 = AXIS2_PLACEMENT_3D ( 'NONE', #209652, #89687, #127550 ) ;
#126770 = AXIS2_PLACEMENT_3D ( 'NONE', #93509, #209616, #188760 ) ;
#126771 = VERTEX_POINT ( 'NONE', #144647 ) ;
#126772 = EDGE_LOOP ( 'NONE', ( #37334, #128374, #13463 ) ) ;
#126773 = CARTESIAN_POINT ( 'NONE',  ( -18.48408745364673322, -9.664322258651884212, -73.68307853332848367 ) ) ;
#126774 = EDGE_CURVE ( 'NONE', #83250, #105032, #19930, .T. ) ;
#126775 = VERTEX_POINT ( 'NONE', #88511 ) ;
#126776 = EDGE_CURVE ( 'NONE', #96601, #151810, #40790, .T. ) ;
#126777 = CARTESIAN_POINT ( 'NONE',  ( -16.80468759584939775, 23.00963892154194923, -230.9608765328473226 ) ) ;
#126778 = VERTEX_POINT ( 'NONE', #145932 ) ;
#126780 = VERTEX_POINT ( 'NONE', #226759 ) ;
#126779 = DIRECTION ( 'NONE',  ( -1.000000000000000000, 0.000000000000000000, 0.000000000000000000 ) ) ;
#126781 = CARTESIAN_POINT ( 'NONE',  ( -21.14999999999999858, 11.75000000001115197, -73.78386566297820082 ) ) ;
#126782 = ORIENTED_EDGE ( 'NONE', *, *, #207151, .F. ) ;
#126783 = CARTESIAN_POINT ( 'NONE',  ( -23.15000000000000213, 64.25000000001222134, -148.2731074845243882 ) ) ;
#126784 = EDGE_LOOP ( 'NONE', ( #213672, #208532, #212937, #257583 ) ) ;
#126788 = ADVANCED_FACE ( 'NONE', ( #242465 ), #6428, .F. ) ;
#126787 = ORIENTED_EDGE ( 'NONE', *, *, #223318, .F. ) ;
#126786 = ORIENTED_EDGE ( 'NONE', *, *, #171213, .T. ) ;
#126785 = CARTESIAN_POINT ( 'NONE',  ( 20.94999999999999574, 74.14897176987101091, -91.36919421510182815 ) ) ;
#126790 = DIRECTION ( 'NONE',  ( -1.836970198721029934E-16, 1.000000000000000000, 0.000000000000000000 ) ) ;
#126789 = CIRCLE ( 'NONE', #147451, 0.5000000000000013323 ) ;
#126791 = DIRECTION ( 'NONE',  ( 1.000000000000000000, 0.000000000000000000, 0.000000000000000000 ) ) ;
#126792 = EDGE_LOOP ( 'NONE', ( #79901, #149665, #38123, #245199 ) ) ;
#126793 = AXIS2_PLACEMENT_3D ( 'NONE', #213768, #52106, #36441 ) ;
#126794 = AXIS2_PLACEMENT_3D ( 'NONE', #51034, #107183, #129326 ) ;
#126795 = AXIS2_PLACEMENT_3D ( 'NONE', #113013, #97252, #176855 ) ;
#126796 = AXIS2_PLACEMENT_3D ( 'NONE', #42011, #242742, #82365 ) ;
#126797 = ORIENTED_EDGE ( 'NONE', *, *, #245202, .F. ) ;
#126798 = CARTESIAN_POINT ( 'NONE',  ( -20.94999999999999929, 11.65000000001115588, -174.5148057706539930 ) ) ;
#126799 = DIRECTION ( 'NONE',  ( -1.000000000000000000, 0.000000000000000000, 0.000000000000000000 ) ) ;
#126801 = EDGE_LOOP ( 'NONE', ( #48210, #171409, #95979, #44384 ) ) ;
#126800 = DIRECTION ( 'NONE',  ( 0.000000000000000000, 0.000000000000000000, 1.000000000000000000 ) ) ;
#126802 = CARTESIAN_POINT ( 'NONE',  ( 18.54999999999999716, 8.750000000011182166, -54.35000000000000142 ) ) ;
#126803 = ORIENTED_EDGE ( 'NONE', *, *, #104922, .F. ) ;
#126804 = DIRECTION ( 'NONE',  ( 1.000000000000000000, 0.000000000000000000, 0.000000000000000000 ) ) ;
#126805 = CYLINDRICAL_SURFACE ( 'NONE', #60703, 0.09999999999999939493 ) ;
#126806 = AXIS2_PLACEMENT_3D ( 'NONE', #18796, #257350, #78759 ) ;
#126808 = VERTEX_POINT ( 'NONE', #143372 ) ;
#126807 = EDGE_CURVE ( 'NONE', #227300, #187280, #74106, .T. ) ;
#126809 = AXIS2_PLACEMENT_3D ( 'NONE', #32219, #79520, #159104 ) ;
#126810 = CARTESIAN_POINT ( 'NONE',  ( -20.85000000000000142, -1.835859311432481045, -212.5044391687984842 ) ) ;
#126811 = CARTESIAN_POINT ( 'NONE',  ( 21.05000000000000071, 69.35000000001186038, -90.87310748452435405 ) ) ;
#126812 = EDGE_CURVE ( 'NONE', #170483, #149519, #183791, .T. ) ;
#126813 = ORIENTED_EDGE ( 'NONE', *, *, #28086, .T. ) ;
#126814 = CARTESIAN_POINT ( 'NONE',  ( 19.97071067695875968, 54.38679851776535656, -228.7661916334623413 ) ) ;
#126815 = AXIS2_PLACEMENT_3D ( 'NONE', #114454, #216108, #134009 ) ;
#126816 = EDGE_CURVE ( 'NONE', #39363, #86653, #170450, .T. ) ;
#126819 = ORIENTED_EDGE ( 'NONE', *, *, #92395, .F. ) ;
#126818 = ORIENTED_EDGE ( 'NONE', *, *, #102875, .T. ) ;
#126817 = VECTOR ( 'NONE', #199263, 1000.000000000000000 ) ;
#126820 = ORIENTED_EDGE ( 'NONE', *, *, #196568, .F. ) ;
#126822 = EDGE_CURVE ( 'NONE', #182833, #95624, #126380, .T. ) ;
#126821 = FACE_OUTER_BOUND ( 'NONE', #247133, .T. ) ;
#126823 = ORIENTED_EDGE ( 'NONE', *, *, #35719, .F. ) ;
#126824 = CARTESIAN_POINT ( 'NONE',  ( -20.64999999999999858, 1.115600667400684642E-11, -167.5000000000000284 ) ) ;
#126825 = ORIENTED_EDGE ( 'NONE', *, *, #20362, .T. ) ;
#126826 = CARTESIAN_POINT ( 'NONE',  ( -16.85718274719394572, 66.02385768538961486, -48.58645381670633867 ) ) ;
#126827 = AXIS2_PLACEMENT_3D ( 'NONE', #214639, #231667, #53000 ) ;
#126828 = EDGE_CURVE ( 'NONE', #83634, #86372, #69001, .T. ) ;
#126829 = AXIS2_PLACEMENT_3D ( 'NONE', #246355, #12902, #87255 ) ;
#126830 = EDGE_LOOP ( 'NONE', ( #20262, #175569, #160652, #141288 ) ) ;
#126831 = ORIENTED_EDGE ( 'NONE', *, *, #3417, .F. ) ;
#126832 = EDGE_LOOP ( 'NONE', ( #220073, #4983, #210430, #159984 ) ) ;
#126833 = ADVANCED_FACE ( 'NONE', ( #27327 ), #67691, .F. ) ;
#126834 = EDGE_CURVE ( 'NONE', #84341, #186134, #170644, .T. ) ;
#126835 = LINE ( 'NONE', #147686, #30662 ) ;
#126836 = ORIENTED_EDGE ( 'NONE', *, *, #224996, .T. ) ;
#126837 = EDGE_CURVE ( 'NONE', #37214, #113112, #222903, .T. ) ;
#126838 = CARTESIAN_POINT ( 'NONE',  ( -22.39999999999999858, 55.96127771274636586, -232.9022175645438892 ) ) ;
#126840 = ORIENTED_EDGE ( 'NONE', *, *, #138199, .T. ) ;
#126839 = CARTESIAN_POINT ( 'NONE',  ( -21.51976009735018991, 69.08954155835317579, -170.0231074845243882 ) ) ;
#126841 = CARTESIAN_POINT ( 'NONE',  ( -20.64999999999999858, 7.250000000011155521, -45.85000000000000142 ) ) ;
#126842 = DIRECTION ( 'NONE',  ( 1.000000000000000000, -0.000000000000000000, -0.000000000000000000 ) ) ;
#126843 = CARTESIAN_POINT ( 'NONE',  ( -16.97092634996727867, 12.45953117125834453, -211.2126573136994523 ) ) ;
#126844 = FACE_OUTER_BOUND ( 'NONE', #231138, .T. ) ;
#126845 = DIRECTION ( 'NONE',  ( -1.000000000000000000, -0.000000000000000000, -0.000000000000000000 ) ) ;
#126846 = AXIS2_PLACEMENT_3D ( 'NONE', #241216, #142089, #121295 ) ;
#126848 = DIRECTION ( 'NONE',  ( 0.000000000000000000, -6.938893903907222067E-15, 1.000000000000000000 ) ) ;
#126847 = CARTESIAN_POINT ( 'NONE',  ( -20.64999999999999858, 7.150000000011155876, -155.1500000000000057 ) ) ;
#126849 = CARTESIAN_POINT ( 'NONE',  ( -20.94999999999999929, -1.362429037182149694, -108.3888812479212476 ) ) ;
#126850 = CARTESIAN_POINT ( 'NONE',  ( 22.49999999999999645, 75.89914163091373212, -181.7726746080137445 ) ) ;
#126851 = AXIS2_PLACEMENT_3D ( 'NONE', #92734, #172337, #251817 ) ;
#126852 = DIRECTION ( 'NONE',  ( 0.000000000000000000, -0.9915357197604792727, 0.1298341882520475943 ) ) ;
#126853 = CIRCLE ( 'NONE', #243550, 0.2000000000000057288 ) ;
#126854 = ADVANCED_FACE ( 'NONE', ( #122548 ), #23467, .F. ) ;
#126855 = ORIENTED_EDGE ( 'NONE', *, *, #169238, .T. ) ;
#126856 = TOROIDAL_SURFACE ( 'NONE', #110279, 0.2000000000000000111, 0.1000000000000000056 ) ;
#126857 = EDGE_CURVE ( 'NONE', #21030, #168386, #44292, .T. ) ;
#126858 = ORIENTED_EDGE ( 'NONE', *, *, #86451, .F. ) ;
#126859 = CIRCLE ( 'NONE', #230938, 0.1000000000000001860 ) ;
#126861 = EDGE_LOOP ( 'NONE', ( #183266, #94970, #85123, #96829 ) ) ;
#126860 = CARTESIAN_POINT ( 'NONE',  ( -23.15000000000000213, 64.35000000001195986, -110.0379132551783243 ) ) ;
#126862 = ORIENTED_EDGE ( 'NONE', *, *, #3321, .T. ) ;
#126863 = CARTESIAN_POINT ( 'NONE',  ( -22.59999999999999787, 64.35042919246734527, -136.6231074845243825 ) ) ;
#126864 = EDGE_CURVE ( 'NONE', #20774, #215603, #110670, .T. ) ;
#126865 = DIRECTION ( 'NONE',  ( 0.000000000000000000, 0.000000000000000000, -1.000000000000000000 ) ) ;
#126867 = DIRECTION ( 'NONE',  ( 0.000000000000000000, 0.000000000000000000, -1.000000000000000000 ) ) ;
#126866 = CARTESIAN_POINT ( 'NONE',  ( -23.25000000000000000, 87.48912529308798014, -106.1231074845242262 ) ) ;
#126868 = EDGE_CURVE ( 'NONE', #45717, #141855, #149818, .T. ) ;
#126869 = ORIENTED_EDGE ( 'NONE', *, *, #236653, .T. ) ;
#126870 = AXIS2_PLACEMENT_3D ( 'NONE', #180745, #98585, #3360 ) ;
#126871 = AXIS2_PLACEMENT_3D ( 'NONE', #117699, #65426, #184089 ) ;
#126872 = CARTESIAN_POINT ( 'NONE',  ( -15.55912972643740488, 8.490870273573721150, -121.4500000000000313 ) ) ;
#126873 = CIRCLE ( 'NONE', #135036, 0.9750000000000036415 ) ;
#126874 = CARTESIAN_POINT ( 'NONE',  ( -23.15000000000000213, 11.65000000001115588, -33.50000000000000000 ) ) ;
#126875 = ORIENTED_EDGE ( 'NONE', *, *, #10864, .T. ) ;
#126876 = CIRCLE ( 'NONE', #14482, 0.09999999999999939493 ) ;
#126877 = DIRECTION ( 'NONE',  ( 1.000000000000000000, 0.000000000000000000, -0.000000000000000000 ) ) ;
#126878 = CYLINDRICAL_SURFACE ( 'NONE', #171608, 0.09999999999999939493 ) ;
#126879 = CARTESIAN_POINT ( 'NONE',  ( 21.14999999999999858, 11.65000000001116298, -179.6499999999999773 ) ) ;
#126880 = CARTESIAN_POINT ( 'NONE',  ( 20.04142135623730070, 21.13195309841794867, -243.6318585593224100 ) ) ;
#126881 = EDGE_CURVE ( 'NONE', #57378, #225164, #220484, .T. ) ;
#126882 = DIRECTION ( 'NONE',  ( -1.000000000000000000, 0.000000000000000000, 0.000000000000000000 ) ) ;
#126884 = EDGE_LOOP ( 'NONE', ( #99266, #191677, #143759, #31937, #251743, #234693, #45528, #108170, #43619, #123845 ) ) ;
#126883 = CARTESIAN_POINT ( 'NONE',  ( 23.24999999999999645, 1.115600667400684642E-11, -33.50000000000000000 ) ) ;
#126885 = VECTOR ( 'NONE', #137230, 1000.000000000000000 ) ;
#126886 = CARTESIAN_POINT ( 'NONE',  ( 13.40000000000000036, -11.75000000000000000, 17.70000000000000284 ) ) ;
#126887 = CARTESIAN_POINT ( 'NONE',  ( -20.94999999999999929, 77.26178616857710324, -128.4366085209788366 ) ) ;
#126888 = DIRECTION ( 'NONE',  ( 0.000000000000000000, 1.000000000000000000, 6.352154140967427193E-15 ) ) ;
#126889 = CARTESIAN_POINT ( 'NONE',  ( 23.04999999999999716, 67.17743825834520521, -60.27310748452438816 ) ) ;
#126890 = ORIENTED_EDGE ( 'NONE', *, *, #227664, .T. ) ;
#126891 = CARTESIAN_POINT ( 'NONE',  ( 21.07928932188134397, 6.328516656393303741, 0.09889514565439641580 ) ) ;
#126892 = PLANE ( 'NONE',  #248572 ) ;
#126893 = AXIS2_PLACEMENT_3D ( 'NONE', #48896, #33234, #90583 ) ;
#126895 = CARTESIAN_POINT ( 'NONE',  ( -18.34374000495059676, 64.52683809664949877, -112.2731074845243739 ) ) ;
#126894 = DIRECTION ( 'NONE',  ( -0.000000000000000000, 0.8814952561688430555, -0.4721928772777346239 ) ) ;
#126896 = FACE_OUTER_BOUND ( 'NONE', #170646, .T. ) ;
#126897 = DIRECTION ( 'NONE',  ( 1.000000000000000000, -7.304098846218134667E-16, -5.100424963727256530E-30 ) ) ;
#126898 = CYLINDRICAL_SURFACE ( 'NONE', #128824, 0.1000000000000004496 ) ;
#126899 = CARTESIAN_POINT ( 'NONE',  ( 20.94999999999999929, 6.650000000011155876, -112.6500000000000341 ) ) ;
#126900 = DIRECTION ( 'NONE',  ( -0.7071067811865475727, -0.7071067811865475727, 0.000000000000000000 ) ) ;
#126901 = DIRECTION ( 'NONE',  ( 0.000000000000000000, 0.000000000000000000, 1.000000000000000000 ) ) ;
#126902 = VECTOR ( 'NONE', #115946, 1000.000000000000114 ) ;
#126904 = ORIENTED_EDGE ( 'NONE', *, *, #179694, .T. ) ;
#126903 = CIRCLE ( 'NONE', #114430, 0.1000000000000028644 ) ;
#126905 = CARTESIAN_POINT ( 'NONE',  ( 21.05000000000000071, -11.48912529306489994, -164.4000000000000057 ) ) ;
#126906 = CIRCLE ( 'NONE', #110322, 0.1000000000000024342 ) ;
#126907 = ORIENTED_EDGE ( 'NONE', *, *, #171923, .T. ) ;
#126908 = ORIENTED_EDGE ( 'NONE', *, *, #243718, .T. ) ;
#126909 = EDGE_CURVE ( 'NONE', #150821, #147343, #257826, .T. ) ;
#126910 = DIRECTION ( 'NONE',  ( 0.000000000000000000, -0.000000000000000000, 1.000000000000000000 ) ) ;
#126911 = DIRECTION ( 'NONE',  ( 0.000000000000000000, 0.000000000000000000, -1.000000000000000000 ) ) ;
#126912 = VERTEX_POINT ( 'NONE', #171971 ) ;
#126913 = ORIENTED_EDGE ( 'NONE', *, *, #118936, .F. ) ;
#126914 =( NAMED_UNIT ( * ) SI_UNIT ( $, .STERADIAN. ) SOLID_ANGLE_UNIT ( ) );
#126915 = ADVANCED_FACE ( 'NONE', ( #170697 ), #190217, .T. ) ;
#126916 = VERTEX_POINT ( 'NONE', #192783 ) ;
#126917 = LINE ( 'NONE', #206447, #237482 ) ;
#126918 = VECTOR ( 'NONE', #49573, 1000.000000000000341 ) ;
#126919 = EDGE_LOOP ( 'NONE', ( #237444, #8788, #258029 ) ) ;
#126920 = DIRECTION ( 'NONE',  ( -1.000000000000000000, -2.952720810173289112E-16, 0.000000000000000000 ) ) ;
#126921 = DIRECTION ( 'NONE',  ( -1.000000000000000000, 1.772924042024179204E-16, -4.808324575169892332E-17 ) ) ;
#126922 = DIRECTION ( 'NONE',  ( 0.000000000000000000, 0.9908441862701791170, -0.1350103645450472789 ) ) ;
#126923 = CYLINDRICAL_SURFACE ( 'NONE', #73500, 0.09999999999999939493 ) ;
#126924 = AXIS2_PLACEMENT_3D ( 'NONE', #5385, #182791, #42000 ) ;
#126925 = FACE_OUTER_BOUND ( 'NONE', #60762, .T. ) ;
#126926 = CARTESIAN_POINT ( 'NONE',  ( -15.55912972643740488, 67.50912972644967169, -149.0731074845244279 ) ) ;
#126928 = VERTEX_POINT ( 'NONE', #128959 ) ;
#126927 = CARTESIAN_POINT ( 'NONE',  ( 23.24999999999999645, 5.000000000011153745, -45.90526601891310321 ) ) ;
#126930 = DIRECTION ( 'NONE',  ( 1.000000000000000000, 0.000000000000000000, 0.000000000000000000 ) ) ;
#126929 = CARTESIAN_POINT ( 'NONE',  ( 20.96428641294230033, 11.75000000000034461, -26.67489317794139936 ) ) ;
#126931 = CARTESIAN_POINT ( 'NONE',  ( -21.53699400384554963, 76.00000000001170974, -76.31081927776580187 ) ) ;
#126932 = ORIENTED_EDGE ( 'NONE', *, *, #4434, .F. ) ;
#126933 = DIRECTION ( 'NONE',  ( 0.000000000000000000, -0.2617529984165034018, -0.9651348961777157509 ) ) ;
#126934 = CARTESIAN_POINT ( 'NONE',  ( -15.39946565075090668, 9.389534562357859215, -116.1748093043900099 ) ) ;
#126935 = DIRECTION ( 'NONE',  ( -1.000000000000000000, 0.000000000000000000, 0.000000000000000000 ) ) ;
#126936 = ORIENTED_EDGE ( 'NONE', *, *, #143257, .T. ) ;
#126937 = CARTESIAN_POINT ( 'NONE',  ( 21.14999999999999858, 64.18196446391819165, -247.0985338183330668 ) ) ;
#126938 = CARTESIAN_POINT ( 'NONE',  ( -16.84981964351502270, 66.08268176591278120, -82.39270909854334946 ) ) ;
#126939 = ORIENTED_EDGE ( 'NONE', *, *, #38502, .T. ) ;
#126940 = CIRCLE ( 'NONE', #197842, 0.09999999999999939493 ) ;
#126942 = DIRECTION ( 'NONE',  ( -1.000000000000000000, 3.265361837132813093E-16, 2.280189983783949500E-30 ) ) ;
#126941 = AXIS2_PLACEMENT_3D ( 'NONE', #16943, #255486, #156477 ) ;
#126943 = LINE ( 'NONE', #143925, #37123 ) ;
#126944 = CARTESIAN_POINT ( 'NONE',  ( -16.87331047859651179, 66.05000000001230376, -157.3731074845244393 ) ) ;
#126945 = DIRECTION ( 'NONE',  ( -1.000000000000000000, 0.000000000000000000, 0.000000000000000000 ) ) ;
#126946 = EDGE_LOOP ( 'NONE', ( #189557, #199619, #150435, #116342 ) ) ;
#126947 = ORIENTED_EDGE ( 'NONE', *, *, #180082, .T. ) ;
#126948 = ADVANCED_FACE ( 'NONE', ( #209776 ), #3984, .F. ) ;
#126949 = DIRECTION ( 'NONE',  ( 0.000000000000000000, 6.982962677686266711E-15, -1.000000000000000000 ) ) ;
#126950 = CARTESIAN_POINT ( 'NONE',  ( 21.05000000000000071, 10.48443348964172728, -7.456805801491905861 ) ) ;
#126951 = DIRECTION ( 'NONE',  ( 0.000000000000000000, 0.5283051335750404975, -0.8490545835446967615 ) ) ;
#126952 = CARTESIAN_POINT ( 'NONE',  ( -23.49999999999994316, 87.51781941433023349, -37.75951082105083145 ) ) ;
#126953 = CIRCLE ( 'NONE', #177051, 0.09999999999998951394 ) ;
#126954 = CARTESIAN_POINT ( 'NONE',  ( 21.08621493067296626, 6.349294291182826733, -167.4438051605238513 ) ) ;
#126955 = CIRCLE ( 'NONE', #51918, 0.1000000000000028644 ) ;
#126956 = DIRECTION ( 'NONE',  ( 0.000000000000000000, 0.000000000000000000, -1.000000000000000000 ) ) ;
#126957 = ORIENTED_EDGE ( 'NONE', *, *, #17888, .F. ) ;
#126958 = CARTESIAN_POINT ( 'NONE',  ( -20.94999999999999929, 65.70711192142366031, -97.56510546851220056 ) ) ;
#126959 = AXIS2_PLACEMENT_3D ( 'NONE', #72502, #152047, #229003 ) ;
#126961 = VERTEX_POINT ( 'NONE', #230630 ) ;
#126960 = DIRECTION ( 'NONE',  ( 0.000000000000000000, -6.982962677686266711E-15, 1.000000000000000000 ) ) ;
#126962 = CARTESIAN_POINT ( 'NONE',  ( -16.87683809663752399, 9.850000000011140955, -46.15000000000000568 ) ) ;
#126963 = CARTESIAN_POINT ( 'NONE',  ( 20.04999999999999716, 8.750000000000014211, -12.65000000000000391 ) ) ;
#126964 = DIRECTION ( 'NONE',  ( -1.000000000000000000, -0.000000000000000000, -0.000000000000000000 ) ) ;
#126965 = DIRECTION ( 'NONE',  ( -1.000000000000000000, 0.000000000000000000, 0.000000000000000000 ) ) ;
#126966 = ADVANCED_FACE ( 'NONE', ( #111971 ), #212358, .T. ) ;
#126968 = ORIENTED_EDGE ( 'NONE', *, *, #232167, .F. ) ;
#126967 = DIRECTION ( 'NONE',  ( 1.836970198721030427E-16, 0.4088369013363281623, -0.9126074666063771490 ) ) ;
#126969 = DIRECTION ( 'NONE',  ( -0.000000000000000000, 0.8900778951570254005, 0.4558084472153182132 ) ) ;
#126970 = CYLINDRICAL_SURFACE ( 'NONE', #220388, 0.1000000000000054040 ) ;
#126971 = CARTESIAN_POINT ( 'NONE',  ( -20.94999999999999929, 14.05000000001115623, -128.4863049292391395 ) ) ;
#126972 = CARTESIAN_POINT ( 'NONE',  ( 18.49999999999998934, 69.45000000001199680, -115.3731074845243398 ) ) ;
#126973 = ADVANCED_FACE ( 'NONE', ( #51956 ), #128902, .F. ) ;
#126974 = ORIENTED_EDGE ( 'NONE', *, *, #91386, .F. ) ;
#126975 = CARTESIAN_POINT ( 'NONE',  ( 18.58703555225022797, -7.674694569411833811, -209.9634296052368256 ) ) ;
#126976 = CARTESIAN_POINT ( 'NONE',  ( -16.80621392010915471, 66.05779742250425102, -115.7126994499414820 ) ) ;
#126977 = CARTESIAN_POINT ( 'NONE',  ( 20.94999999999999574, 74.83729825007408465, -128.4231074845243086 ) ) ;
#126978 = CARTESIAN_POINT ( 'NONE',  ( -18.49999999999997868, 78.12133356376092763, -231.3112718935514920 ) ) ;
#126979 = EDGE_CURVE ( 'NONE', #11153, #116241, #31035, .T. ) ;
#126980 = ORIENTED_EDGE ( 'NONE', *, *, #243538, .F. ) ;
#126981 = FACE_OUTER_BOUND ( 'NONE', #132141, .T. ) ;
#126982 = ORIENTED_EDGE ( 'NONE', *, *, #62665, .T. ) ;
#126983 = DIRECTION ( 'NONE',  ( 0.000000000000000000, 0.000000000000000000, -1.000000000000000000 ) ) ;
#126985 = CYLINDRICAL_SURFACE ( 'NONE', #179144, 4.000000000000003553 ) ;
#126984 = CIRCLE ( 'NONE', #14579, 7.791421356237310469 ) ;
#126986 = PLANE ( 'NONE',  #53999 ) ;
#126987 = CARTESIAN_POINT ( 'NONE',  ( 18.59999999999999076, 76.00000000001142553, -36.02310748452432421 ) ) ;
#126988 = ORIENTED_EDGE ( 'NONE', *, *, #45630, .T. ) ;
#126989 = EDGE_CURVE ( 'NONE', #106788, #134956, #131513, .T. ) ;
#126990 = CIRCLE ( 'NONE', #218536, 0.2000000000000057288 ) ;
#126991 = AXIS2_PLACEMENT_3D ( 'NONE', #21831, #257811, #220024 ) ;
#126992 = DIRECTION ( 'NONE',  ( -0.000000000000000000, -6.982962677686266711E-15, 1.000000000000000000 ) ) ;
#126993 = EDGE_CURVE ( 'NONE', #64278, #153515, #211058, .T. ) ;
#126994 = CARTESIAN_POINT ( 'NONE',  ( -12.25000000000000178, 66.15000000001258229, -186.7731074845244166 ) ) ;
#126995 = CARTESIAN_POINT ( 'NONE',  ( 15.51872946208854920, 9.376580978043941528, -17.62694624701194002 ) ) ;
#126996 = CARTESIAN_POINT ( 'NONE',  ( -20.94999999999999929, 5.850000000011108092, -110.6324972242780120 ) ) ;
#126997 = CARTESIAN_POINT ( 'NONE',  ( 23.25000000000000355, -22.45632476062292326, -6.793898447731608670 ) ) ;
#126998 = ORIENTED_EDGE ( 'NONE', *, *, #70594, .F. ) ;
#127000 = ORIENTED_EDGE ( 'NONE', *, *, #168521, .T. ) ;
#126999 = FACE_OUTER_BOUND ( 'NONE', #148910, .T. ) ;
#127001 = CIRCLE ( 'NONE', #2071, 0.2000000000000005107 ) ;
#127002 = ORIENTED_EDGE ( 'NONE', *, *, #214552, .F. ) ;
#127003 = FACE_OUTER_BOUND ( 'NONE', #222227, .T. ) ;
#127004 = ORIENTED_EDGE ( 'NONE', *, *, #56616, .F. ) ;
#127005 = CARTESIAN_POINT ( 'NONE',  ( 21.11701782572533048, 65.27839088400459389, -124.2780700550131598 ) ) ;
#127006 = AXIS2_PLACEMENT_3D ( 'NONE', #206848, #24381, #242113 ) ;
#127007 = CARTESIAN_POINT ( 'NONE',  ( 21.00023020733503643, 1.115542391533913547E-11, -27.10913075473163403 ) ) ;
#127008 = DIRECTION ( 'NONE',  ( 0.000000000000000000, -0.2605042016806740079, 0.9654727137038698892 ) ) ;
#127009 = ORIENTED_EDGE ( 'NONE', *, *, #156369, .F. ) ;
#127011 = CIRCLE ( 'NONE', #193653, 0.9000000000000014655 ) ;
#127010 = LINE ( 'NONE', #110007, #24122 ) ;
#127012 = PLANE ( 'NONE',  #180383 ) ;
#127013 = CARTESIAN_POINT ( 'NONE',  ( 21.14999999999999858, 56.01362831242965967, -232.7091905853083347 ) ) ;
#127014 = AXIS2_PLACEMENT_3D ( 'NONE', #51657, #187361, #145634 ) ;
#127015 = ORIENTED_EDGE ( 'NONE', *, *, #12510, .T. ) ;
#127016 = EDGE_CURVE ( 'NONE', #44671, #46048, #93671, .T. ) ;
#127017 = CARTESIAN_POINT ( 'NONE',  ( 21.05000000000000071, 76.00000000001185185, -90.04810748452430857 ) ) ;
#127019 = ORIENTED_EDGE ( 'NONE', *, *, #31088, .F. ) ;
#127018 = CARTESIAN_POINT ( 'NONE',  ( 18.59999999999999076, 1.835341550224411922, -11.55515129256298046 ) ) ;
#127020 = CARTESIAN_POINT ( 'NONE',  ( -21.05000000000000071, 14.05000000000000071, -5.513695070760990191 ) ) ;
#127021 = CYLINDRICAL_SURFACE ( 'NONE', #43880, 0.1000000000000028644 ) ;
#127022 = ORIENTED_EDGE ( 'NONE', *, *, #153972, .T. ) ;
#127023 = DIRECTION ( 'NONE',  ( -0.000000000000000000, -0.2128009952263603677, 0.9770955615653313941 ) ) ;
#127025 = EDGE_CURVE ( 'NONE', #160332, #122268, #24689, .T. ) ;
#127024 = LINE ( 'NONE', #90452, #229489 ) ;
#127026 = CARTESIAN_POINT ( 'NONE',  ( 20.04142135623730070, 31.36165455396662693, -233.4973802202241302 ) ) ;
#127027 = EDGE_LOOP ( 'NONE', ( #234697, #134170, #82201, #197355, #176539, #198861, #198219, #234301, #154623, #4182, #8, #11774, #90862, #124936, #164534, #13673 ) ) ;
#127028 = CYLINDRICAL_SURFACE ( 'NONE', #63253, 0.5000000000000008882 ) ;
#127029 = CARTESIAN_POINT ( 'NONE',  ( 21.05000000000000071, 85.50000000001159606, -59.62913836187181715 ) ) ;
#127030 = EDGE_CURVE ( 'NONE', #245368, #39159, #152396, .T. ) ;
#127031 = CIRCLE ( 'NONE', #181220, 0.1000000000000028644 ) ;
#127032 = ORIENTED_EDGE ( 'NONE', *, *, #201790, .T. ) ;
#127033 = AXIS2_PLACEMENT_3D ( 'NONE', #97537, #139237, #178426 ) ;
#127034 = ADVANCED_FACE ( 'NONE', ( #231920 ), #10306, .F. ) ;
#127035 = AXIS2_PLACEMENT_3D ( 'NONE', #199244, #165235, #163962 ) ;
#127036 = EDGE_CURVE ( 'NONE', #46873, #109463, #130217, .T. ) ;
#127037 = VERTEX_POINT ( 'NONE', #177088 ) ;
#127038 = CARTESIAN_POINT ( 'NONE',  ( -16.87036670365549895, 43.98904843454555902, -235.2166589526560472 ) ) ;
#127039 = TOROIDAL_SURFACE ( 'NONE', #235193, 11.65000000000000036, 0.1000000000000000056 ) ;
#127040 = ORIENTED_EDGE ( 'NONE', *, *, #179152, .F. ) ;
#127041 = DIRECTION ( 'NONE',  ( 1.000000000000000000, -0.000000000000000000, -0.000000000000000000 ) ) ;
#127042 = CARTESIAN_POINT ( 'NONE',  ( -22.20000000000000284, 3.362550747017869046, 28.82623795144604983 ) ) ;
#127046 = EDGE_CURVE ( 'NONE', #34172, #202111, #245429, .T. ) ;
#127045 = ORIENTED_EDGE ( 'NONE', *, *, #2110, .T. ) ;
#127044 = CARTESIAN_POINT ( 'NONE',  ( 13.76927104934458157, 24.82647667088539833, -232.4856315176584474 ) ) ;
#127043 =( BOUNDED_CURVE ( )  B_SPLINE_CURVE ( 3, ( #125986, #108986, #146823, #89425 ),
 .UNSPECIFIED., .F., .F. ) 
 B_SPLINE_CURVE_WITH_KNOTS ( ( 4, 4 ),
 ( 0.000000000000000000, 1.570796326794896558 ),
 .UNSPECIFIED. ) 
 CURVE ( )  GEOMETRIC_REPRESENTATION_ITEM ( )  RATIONAL_B_SPLINE_CURVE ( ( 1.000000000000000000, 0.8047378541243649375, 0.8047378541243649375, 1.000000000000000000 ) ) 
 REPRESENTATION_ITEM ( '' )  );
#127047 = DIRECTION ( 'NONE',  ( 1.000000000000000000, 0.000000000000000000, 0.000000000000000000 ) ) ;
#127048 = CARTESIAN_POINT ( 'NONE',  ( 18.79999999999999716, 0.000000000000000000, 33.00000000000000000 ) ) ;
#127049 = DIRECTION ( 'NONE',  ( 0.000000000000000000, 0.000000000000000000, -1.000000000000000000 ) ) ;
#127050 = CARTESIAN_POINT ( 'NONE',  ( -22.50000000000000000, 68.20922040163824818, -69.62310748452438247 ) ) ;
#127051 = CARTESIAN_POINT ( 'NONE',  ( -21.05000000000000071, 1.162701749949165642, -175.4999999999999716 ) ) ;
#127052 = VECTOR ( 'NONE', #207718, 1000.000000000000114 ) ;
#127053 = ADVANCED_FACE ( 'NONE', ( #37566 ), #36287, .T. ) ;
#127054 = CARTESIAN_POINT ( 'NONE',  ( -21.05000000000000071, 44.52640028187936849, -247.3006740988509193 ) ) ;
#127055 = ADVANCED_FACE ( 'NONE', ( #197895 ), #106488, .F. ) ;
#127056 = CARTESIAN_POINT ( 'NONE',  ( -18.42609945526379178, -9.499999710479226422, -107.4993624902486431 ) ) ;
#127058 = VERTEX_POINT ( 'NONE', #256535 ) ;
#127057 = CARTESIAN_POINT ( 'NONE',  ( -22.42253884134832020, 75.99806764887672728, -114.6727131818727372 ) ) ;
#127059 = CYLINDRICAL_SURFACE ( 'NONE', #249731, 0.4999999999999944489 ) ;
#127060 = AXIS2_PLACEMENT_3D ( 'NONE', #62635, #163032, #65186 ) ;
#127061 = ORIENTED_EDGE ( 'NONE', *, *, #45799, .F. ) ;
#127062 = VECTOR ( 'NONE', #96241, 1000.000000000000000 ) ;
#127064 = ADVANCED_FACE ( 'NONE', ( #218730 ), #157976, .T. ) ;
#127063 = CARTESIAN_POINT ( 'NONE',  ( -20.64999999999999858, 2.000000000011154189, -46.22462192276210402 ) ) ;
#127065 = FACE_OUTER_BOUND ( 'NONE', #185190, .T. ) ;
#127066 = AXIS2_PLACEMENT_3D ( 'NONE', #31890, #192236, #9716 ) ;
#127067 = DIRECTION ( 'NONE',  ( 0.000000000000000000, 0.2128009952263618387, -0.9770955615653311721 ) ) ;
#127068 = LINE ( 'NONE', #224864, #22193 ) ;
#127069 = EDGE_CURVE ( 'NONE', #176891, #257458, #77944, .T. ) ;
#127070 = ORIENTED_EDGE ( 'NONE', *, *, #19474, .T. ) ;
#127071 = DIRECTION ( 'NONE',  ( 0.000000000000000000, 0.4088369013363311599, -0.9126074666063757057 ) ) ;
#127072 = CARTESIAN_POINT ( 'NONE',  ( -21.12230431290519306, 6.457566653304161797, -100.4947901483110400 ) ) ;
#127073 = ORIENTED_EDGE ( 'NONE', *, *, #246257, .F. ) ;
#127074 = AXIS2_PLACEMENT_3D ( 'NONE', #199684, #216649, #200941 ) ;
#127075 = CARTESIAN_POINT ( 'NONE',  ( -20.54999999999999716, 74.00000000001223555, -149.7477294072864709 ) ) ;
#127076 = AXIS2_PLACEMENT_3D ( 'NONE', #143998, #220967, #24093 ) ;
#127077 = CARTESIAN_POINT ( 'NONE',  ( 22.39999999999999503, -0.1008583690875579364, -21.75043287651061164 ) ) ;
#127078 = VERTEX_POINT ( 'NONE', #217446 ) ;
#127079 = CARTESIAN_POINT ( 'NONE',  ( -21.05000000000000071, 6.257814610492678398, -66.90220970869081896 ) ) ;
#127080 = EDGE_CURVE ( 'NONE', #178041, #5568, #180916, .T. ) ;
#127081 = ORIENTED_EDGE ( 'NONE', *, *, #10714, .T. ) ;
#127082 = EDGE_CURVE ( 'NONE', #121041, #75451, #237040, .T. ) ;
#127083 = DIRECTION ( 'NONE',  ( 0.000000000000000000, 6.982962677686266711E-15, -1.000000000000000000 ) ) ;
#127084 = ORIENTED_EDGE ( 'NONE', *, *, #121761, .T. ) ;
#127085 = LINE ( 'NONE', #107513, #27501 ) ;
#127086 = DIRECTION ( 'NONE',  ( 0.7071067811865474617, -0.7071067811865474617, -4.937700262164531476E-15 ) ) ;
#127087 = ORIENTED_EDGE ( 'NONE', *, *, #117071, .T. ) ;
#127089 = EDGE_CURVE ( 'NONE', #143749, #213386, #108055, .T. ) ;
#127088 = VERTEX_POINT ( 'NONE', #119666 ) ;
#127090 = CARTESIAN_POINT ( 'NONE',  ( 18.48536876927988359, 85.46352724987957572, -129.4744892194416366 ) ) ;
#127092 = VERTEX_POINT ( 'NONE', #38847 ) ;
#127091 = CARTESIAN_POINT ( 'NONE',  ( 18.59999999999999787, 77.26327546522891510, -61.62124281777789037 ) ) ;
#127093 = CARTESIAN_POINT ( 'NONE',  ( 21.05000000000000071, -1.360870587192041681, -8.072997927090961312 ) ) ;
#127094 = CIRCLE ( 'NONE', #114622, 11.64999999999999325 ) ;
#127095 = VERTEX_POINT ( 'NONE', #118381 ) ;
#127096 = AXIS2_PLACEMENT_3D ( 'NONE', #239883, #87195, #165484 ) ;
#127097 = ORIENTED_EDGE ( 'NONE', *, *, #52518, .F. ) ;
#127098 = CARTESIAN_POINT ( 'NONE',  ( 21.05000000000000071, 65.61575147395463148, -242.1939180743342774 ) ) ;
#127099 = FACE_OUTER_BOUND ( 'NONE', #70297, .T. ) ;
#127100 = DIRECTION ( 'NONE',  ( -1.000000000000000000, -2.952720810173289112E-16, 0.000000000000000000 ) ) ;
#127101 = DIRECTION ( 'NONE',  ( -0.000000000000000000, -6.982962677686266711E-15, 1.000000000000000000 ) ) ;
#127102 = CARTESIAN_POINT ( 'NONE',  ( -20.94999999999999929, 1.835341550235567887, -78.55515129256303908 ) ) ;
#127104 = ORIENTED_EDGE ( 'NONE', *, *, #79933, .T. ) ;
#127103 = ADVANCED_FACE ( 'NONE', ( #79218 ), #199196, .T. ) ;
#127105 = LINE ( 'NONE', #241908, #154217 ) ;
#127106 = CARTESIAN_POINT ( 'NONE',  ( -20.54999999999999716, 68.63171270270233038, -223.0506438513196770 ) ) ;
#127107 = CARTESIAN_POINT ( 'NONE',  ( -23.15000000000000213, 6.759468328187065111, -212.0650163994647812 ) ) ;
#127108 = DIRECTION ( 'NONE',  ( 0.000000000000000000, 0.2617529984165031243, 0.9651348961777156399 ) ) ;
#127109 = EDGE_CURVE ( 'NONE', #111618, #76393, #69985, .T. ) ;
#127110 = ORIENTED_EDGE ( 'NONE', *, *, #160580, .T. ) ;
#127111 = FACE_OUTER_BOUND ( 'NONE', #252425, .T. ) ;
#127112 = ORIENTED_EDGE ( 'NONE', *, *, #47040, .T. ) ;
#127113 = CARTESIAN_POINT ( 'NONE',  ( 27.30103769104855971, 12.20000000000000284, 33.00000000000000000 ) ) ;
#127114 = ORIENTED_EDGE ( 'NONE', *, *, #79345, .T. ) ;
#127115 = AXIS2_PLACEMENT_3D ( 'NONE', #50147, #55262, #119132 ) ;
#127116 = AXIS2_PLACEMENT_3D ( 'NONE', #125034, #148451, #109289 ) ;
#127117 = FACE_OUTER_BOUND ( 'NONE', #181819, .T. ) ;
#127118 = DIRECTION ( 'NONE',  ( 1.000000000000000000, -0.000000000000000000, 0.000000000000000000 ) ) ;
#127119 = VERTEX_POINT ( 'NONE', #238307 ) ;
#127120 = VERTEX_POINT ( 'NONE', #200478 ) ;
#127123 = VERTEX_POINT ( 'NONE', #106475 ) ;
#127122 = ADVANCED_FACE ( 'NONE', ( #21844, #55789 ), #135350, .T. ) ;
#127121 = DIRECTION ( 'NONE',  ( 0.000000000000000000, -6.308085367188393199E-16, -1.000000000000000000 ) ) ;
#127124 = CARTESIAN_POINT ( 'NONE',  ( 22.39999999999999503, 76.00000000001273293, -211.2731074845243882 ) ) ;
#127125 = VERTEX_POINT ( 'NONE', #26999 ) ;
#127126 = DIRECTION ( 'NONE',  ( 0.000000000000000000, 0.8814952561688438326, -0.4721928772777331806 ) ) ;
#127127 = EDGE_CURVE ( 'NONE', #55862, #63429, #186049, .T. ) ;
#127128 = DIRECTION ( 'NONE',  ( 0.000000000000000000, 3.469446951953995998E-14, 1.000000000000000000 ) ) ;
#127129 = ORIENTED_EDGE ( 'NONE', *, *, #212927, .F. ) ;
#127130 = CARTESIAN_POINT ( 'NONE',  ( 25.10847955711010115, 9.068702471349586958, -347.0000000000001137 ) ) ;
#127131 = EDGE_CURVE ( 'NONE', #148851, #14237, #45504, .T. ) ;
#127133 = CARTESIAN_POINT ( 'NONE',  ( -21.05000000000000071, 1.250000000011155299, -175.4999999999999716 ) ) ;
#127132 = TOROIDAL_SURFACE ( 'NONE', #235447, 3.900000000000000355, 0.1000000000000000056 ) ;
#127134 = CIRCLE ( 'NONE', #152103, 0.09999999999999939493 ) ;
#127135 = VERTEX_POINT ( 'NONE', #105173 ) ;
#127136 = CIRCLE ( 'NONE', #193779, 0.09999999999999939493 ) ;
#127137 = AXIS2_PLACEMENT_3D ( 'NONE', #77082, #19699, #18397 ) ;
#127138 = ADVANCED_FACE ( 'NONE', ( #141768 ), #7394, .F. ) ;
#127141 = ADVANCED_FACE ( 'NONE', ( #63515 ), #66356, .T. ) ;
#127140 = ADVANCED_FACE ( 'NONE', ( #144318 ), #208010, .T. ) ;
#127139 = CARTESIAN_POINT ( 'NONE',  ( -21.44999999999999929, 68.75000000001199396, -115.2731074845243455 ) ) ;
#127142 =( BOUNDED_SURFACE ( )  B_SPLINE_SURFACE ( 3, 2, ( 
 ( #193330, #94206, #253279 ),
 ( #55064, #156788, #155513 ),
 ( #12143, #134602, #152947 ),
 ( #35558, #235021, #56352 ),
 ( #15995, #171238, #95496 ),
 ( #135887, #36848, #57640 ) ),
 .UNSPECIFIED., .F., .F., .T. ) 
 B_SPLINE_SURFACE_WITH_KNOTS ( ( 4, 2, 4 ),
 ( 3, 3 ),
 ( 4.712388980384689674, 5.497787143782137953, 6.283185307179586232 ),
 ( 0.000000000000000000, 1.000000000000000000 ),
 .UNSPECIFIED. ) 
 GEOMETRIC_REPRESENTATION_ITEM ( )  RATIONAL_B_SPLINE_SURFACE ( (
 ( 1.000000000000000000, 0.7071067811864555352, 1.000000000000000000),
 ( 1.000000000000000000, 0.7727932973496255409, 1.000000000000000000),
 ( 1.000000000000000000, 0.8282379607643716168, 1.000000000000000000),
 ( 1.000000000000000000, 0.9038128468045815156, 1.000000000000000000),
 ( 1.000000000000000000, 0.9240297172238780554, 1.000000000000000000),
 ( 1.000000000000000000, 0.9238795325112914014, 1.000000000000000000) ) ) 
 REPRESENTATION_ITEM ( '' )  SURFACE ( )  );
#127143 = COLOUR_RGB ( '', 0.66274510, 0.83137255, 0.94901961) ;
#127144 = DIRECTION ( 'NONE',  ( 1.000000000000000000, 7.304098846218133681E-16, 5.100424963727255128E-30 ) ) ;
#127145 = DIRECTION ( 'NONE',  ( 1.000000000000000000, 0.000000000000000000, 0.000000000000000000 ) ) ;
#127147 = ORIENTED_EDGE ( 'NONE', *, *, #198049, .F. ) ;
#127146 = DIRECTION ( 'NONE',  ( 0.000000000000000000, 0.000000000000000000, -1.000000000000000000 ) ) ;
#127148 = CARTESIAN_POINT ( 'NONE',  ( -20.94999999999999929, 87.48912529308842068, -166.9231074845242802 ) ) ;
#127149 = DIRECTION ( 'NONE',  ( 1.000000000000000000, 0.000000000000000000, 0.000000000000000000 ) ) ;
#127150 = DIRECTION ( 'NONE',  ( 0.000000000000000000, -0.1350103645451904977, 0.9908441862701596881 ) ) ;
#127152 = DIRECTION ( 'NONE',  ( -1.000000000000000000, 0.000000000000000000, 0.000000000000000000 ) ) ;
#127151 = PLANE ( 'NONE',  #19363 ) ;
#127153 = CARTESIAN_POINT ( 'NONE',  ( 20.95595012432476167, 39.25550045643235109, -236.7682787779284581 ) ) ;
#127154 = DIRECTION ( 'NONE',  ( 0.000000000000000000, 1.000000000000000000, 6.982962677686266711E-15 ) ) ;
#127155 = CARTESIAN_POINT ( 'NONE',  ( -20.85000000000000142, 64.25000000001196554, -109.8069731475024895 ) ) ;
#127156 = CARTESIAN_POINT ( 'NONE',  ( -21.05000000000000071, 74.83729825007388570, -95.02310748452431710 ) ) ;
#127157 = ADVANCED_FACE ( 'NONE', ( #102623 ), #122227, .T. ) ;
#127158 = EDGE_CURVE ( 'NONE', #75404, #76759, #124795, .T. ) ;
#127159 = CIRCLE ( 'NONE', #214627, 0.09999999999999939493 ) ;
#127160 = ORIENTED_EDGE ( 'NONE', *, *, #131208, .F. ) ;
#127161 = CIRCLE ( 'NONE', #106285, 7.791421356237338891 ) ;
#127162 = CIRCLE ( 'NONE', #6349, 0.09999999999998898659 ) ;
#127163 = EDGE_LOOP ( 'NONE', ( #86895, #150731, #201771, #209529, #192202 ) ) ;
#127164 = EDGE_CURVE ( 'NONE', #95340, #128522, #166333, .T. ) ;
#127165 = FACE_OUTER_BOUND ( 'NONE', #129937, .T. ) ;
#127166 = ORIENTED_EDGE ( 'NONE', *, *, #111316, .T. ) ;
#127167 = EDGE_CURVE ( 'NONE', #238290, #195092, #233156, .T. ) ;
#127168 = CYLINDRICAL_SURFACE ( 'NONE', #206831, 2.000000000000001776 ) ;
#127169 = AXIS2_PLACEMENT_3D ( 'NONE', #330, #236381, #257175 ) ;
#127170 = TOROIDAL_SURFACE ( 'NONE', #89555, 0.9750000000000019762, 0.1000000000000000056 ) ;
#127171 = AXIS2_PLACEMENT_3D ( 'NONE', #35760, #116558, #95694 ) ;
#127172 = EDGE_CURVE ( 'NONE', #178769, #251279, #187348, .T. ) ;
#127173 = VERTEX_POINT ( 'NONE', #25691 ) ;
#127174 = DIRECTION ( 'NONE',  ( 1.296989514748957725E-15, -0.9979305700607959961, -0.06430067914209769420 ) ) ;
#127175 = ORIENTED_EDGE ( 'NONE', *, *, #143834, .T. ) ;
#127176 = CARTESIAN_POINT ( 'NONE',  ( -21.07928932188134041, 6.162520550847337297, -199.5566553493351307 ) ) ;
#127177 = ORIENTED_EDGE ( 'NONE', *, *, #64383, .T. ) ;
#127178 = ORIENTED_EDGE ( 'NONE', *, *, #227454, .T. ) ;
#127180 = DIRECTION ( 'NONE',  ( 1.000000000000000000, -0.000000000000000000, 0.000000000000000000 ) ) ;
#127179 = CIRCLE ( 'NONE', #235499, 0.09999999999999971412 ) ;
#127181 = DIRECTION ( 'NONE',  ( 0.000000000000000000, 8.673617379884087537E-15, -1.000000000000000000 ) ) ;
#127183 = ORIENTED_EDGE ( 'NONE', *, *, #193492, .F. ) ;
#127182 = DIRECTION ( 'NONE',  ( 1.000000000000000000, -0.000000000000000000, 0.000000000000000000 ) ) ;
#127184 = AXIS2_PLACEMENT_3D ( 'NONE', #245481, #182943, #186795 ) ;
#127185 = EDGE_CURVE ( 'NONE', #53595, #111851, #74930, .T. ) ;
#127186 = CARTESIAN_POINT ( 'NONE',  ( 18.59999999999999076, 1.835341550235567887, -78.65515129256301918 ) ) ;
#127188 = ORIENTED_EDGE ( 'NONE', *, *, #41246, .F. ) ;
#127187 = FACE_OUTER_BOUND ( 'NONE', #49615, .T. ) ;
#127189 = FACE_OUTER_BOUND ( 'NONE', #6744, .T. ) ;
#127190 = AXIS2_PLACEMENT_3D ( 'NONE', #234419, #139147, #218694 ) ;
#127191 = CARTESIAN_POINT ( 'NONE',  ( -21.05000000000000071, 87.75000000001247713, -173.0231074845243029 ) ) ;
#127192 = AXIS2_PLACEMENT_3D ( 'NONE', #54239, #175512, #215870 ) ;
#127194 = ORIENTED_EDGE ( 'NONE', *, *, #256763, .F. ) ;
#127193 = DIRECTION ( 'NONE',  ( 0.000000000000000000, 0.000000000000000000, 1.000000000000000000 ) ) ;
#127195 = CARTESIAN_POINT ( 'NONE',  ( 18.59999999999999076, 65.79142135624879018, -44.77310748452439526 ) ) ;
#127196 = CARTESIAN_POINT ( 'NONE',  ( 18.39999999999999858, -9.519327731092436906, -6.972976376559336664 ) ) ;
#127197 = CARTESIAN_POINT ( 'NONE',  ( 18.59999999999999787, 74.13328508995456900, -91.27043223824230722 ) ) ;
#127198 = EDGE_CURVE ( 'NONE', #185202, #189058, #91484, .T. ) ;
#127199 = DIRECTION ( 'NONE',  ( 0.000000000000000000, 0.8814952561688437216, -0.4721928772777335692 ) ) ;
#127200 = CARTESIAN_POINT ( 'NONE',  ( 18.49999999999999289, 10.49142135624846617, -91.75000000000005684 ) ) ;
#127201 = DIRECTION ( 'NONE',  ( 0.000000000000000000, 1.224646799142185182E-16, 1.000000000000000000 ) ) ;
#127202 = CARTESIAN_POINT ( 'NONE',  ( -20.54999999999999716, 2.500000000011154633, -87.27537807723794572 ) ) ;
#127203 = LINE ( 'NONE', #205434, #225934 ) ;
#127204 = ORIENTED_EDGE ( 'NONE', *, *, #21382, .F. ) ;
#127205 = EDGE_LOOP ( 'NONE', ( #90374, #171076, #136785, #162042 ) ) ;
#127206 = ORIENTED_EDGE ( 'NONE', *, *, #157776, .F. ) ;
#127207 = DIRECTION ( 'NONE',  ( 0.000000000000000000, -0.01562499999996560217, -0.9998779222360102414 ) ) ;
#127208 = ORIENTED_EDGE ( 'NONE', *, *, #14435, .F. ) ;
#127209 = CARTESIAN_POINT ( 'NONE',  ( 18.49999999999999289, 64.25000000001251976, -178.6731074845244507 ) ) ;
#127210 = VERTEX_POINT ( 'NONE', #243444 ) ;
#127211 = EDGE_CURVE ( 'NONE', #65925, #139968, #179004, .T. ) ;
#127212 = DIRECTION ( 'NONE',  ( 0.000000000000000000, 0.4999999999999478195, -0.8660254037844686836 ) ) ;
#127213 = DIRECTION ( 'NONE',  ( -1.000000000000000000, 0.000000000000000000, 0.000000000000000000 ) ) ;
#127214 = VECTOR ( 'NONE', #23515, 1000.000000000000000 ) ;
#127215 = CIRCLE ( 'NONE', #14822, 0.1000000000000028644 ) ;
#127216 = ORIENTED_EDGE ( 'NONE', *, *, #58426, .T. ) ;
#127217 = CARTESIAN_POINT ( 'NONE',  ( 12.60873083341397383, 9.389571634557567492, -151.8176407123691547 ) ) ;
#127218 = FILL_AREA_STYLE_COLOUR ( '', #210712 ) ;
#127219 = ORIENTED_EDGE ( 'NONE', *, *, #90289, .T. ) ;
#127220 = ORIENTED_EDGE ( 'NONE', *, *, #84259, .T. ) ;
#127221 = ORIENTED_EDGE ( 'NONE', *, *, #82479, .T. ) ;
#127222 = AXIS2_PLACEMENT_3D ( 'NONE', #39255, #58761, #41821 ) ;
#127223 = LINE ( 'NONE', #48958, #71343 ) ;
#127224 = CARTESIAN_POINT ( 'NONE',  ( -18.69999999999999929, -10.64999999999999325, 31.39999999999999858 ) ) ;
#127225 = CIRCLE ( 'NONE', #64674, 11.80000000000000426 ) ;
#127226 = DIRECTION ( 'NONE',  ( 0.000000000000000000, 0.000000000000000000, 1.000000000000000000 ) ) ;
#127227 = CARTESIAN_POINT ( 'NONE',  ( -18.34804628011471195, 20.70020979027686892, -227.9869476361872955 ) ) ;
#127228 = LINE ( 'NONE', #227600, #231694 ) ;
#127229 = DIRECTION ( 'NONE',  ( 0.000000000000000000, 0.9915357197604862671, -0.1298341882519953583 ) ) ;
#127231 = CARTESIAN_POINT ( 'NONE',  ( -21.44999999999999929, 7.350000000011155166, -179.7499999999999716 ) ) ;
#127230 = DIRECTION ( 'NONE',  ( -1.000000000000000000, 0.000000000000000000, 0.000000000000000000 ) ) ;
#127232 = LINE ( 'NONE', #245902, #108286 ) ;
#127234 = ORIENTED_EDGE ( 'NONE', *, *, #74811, .F. ) ;
#127233 = FACE_OUTER_BOUND ( 'NONE', #225609, .T. ) ;
#127236 = CARTESIAN_POINT ( 'NONE',  ( 23.15000000000000213, 1.627786319807483340, -244.0021210468063089 ) ) ;
#127235 = CARTESIAN_POINT ( 'NONE',  ( 20.51284917709620359, 10.31088662285602275, -74.67247318559205382 ) ) ;
#127237 = DIRECTION ( 'NONE',  ( 0.000000000000000000, 0.000000000000000000, 1.000000000000000000 ) ) ;
#127238 = CIRCLE ( 'NONE', #173067, 7.720710678118679837 ) ;
#127239 = ORIENTED_EDGE ( 'NONE', *, *, #127354, .T. ) ;
#127240 = DIRECTION ( 'NONE',  ( 0.000000000000000000, -0.2617529984165031243, -0.9651348961777157509 ) ) ;
#127241 = CIRCLE ( 'NONE', #60581, 0.09999999999999939493 ) ;
#127242 = DIRECTION ( 'NONE',  ( -7.304098846218443309E-16, -0.4088369013363783999, 0.9126074666063545004 ) ) ;
#127243 = FACE_OUTER_BOUND ( 'NONE', #2033, .T. ) ;
#127244 = ORIENTED_EDGE ( 'NONE', *, *, #68268, .F. ) ;
#127245 = AXIS2_PLACEMENT_3D ( 'NONE', #203264, #142000, #42915 ) ;
#127246 = CARTESIAN_POINT ( 'NONE',  ( 18.59999999999997655, 76.00000000001136868, -28.12310748452432208 ) ) ;
#127247 = ORIENTED_EDGE ( 'NONE', *, *, #24938, .F. ) ;
#127248 = VERTEX_POINT ( 'NONE', #244715 ) ;
#127249 = CARTESIAN_POINT ( 'NONE',  ( -17.01473183483380325, 51.52760218553058280, -231.9873527057832234 ) ) ;
#127250 = VERTEX_POINT ( 'NONE', #64805 ) ;
#127251 = CARTESIAN_POINT ( 'NONE',  ( 22.00356870142806187, 7.254242362486740703, -67.00000000000004263 ) ) ;
#127252 = CARTESIAN_POINT ( 'NONE',  ( -20.54999999999999716, 1.115600667400684642E-11, -135.9000000000000625 ) ) ;
#127253 = CIRCLE ( 'NONE', #256351, 0.09999999999999817368 ) ;
#127254 = CARTESIAN_POINT ( 'NONE',  ( 18.46905048506369695, 85.47374425739408821, -62.84712119226885818 ) ) ;
#127255 = PLANE ( 'NONE',  #109357 ) ;
#127256 = VERTEX_POINT ( 'NONE', #66093 ) ;
#127257 = CARTESIAN_POINT ( 'NONE',  ( -15.73854595235692244, 9.351413679112546617, -117.4803435675490135 ) ) ;
#127259 = EDGE_CURVE ( 'NONE', #19688, #158624, #58313, .T. ) ;
#127258 = DIRECTION ( 'NONE',  ( 1.000000000000000000, 0.000000000000000000, 0.000000000000000000 ) ) ;
#127260 = DIRECTION ( 'NONE',  ( 1.000000000000000000, 0.000000000000000000, 0.000000000000000000 ) ) ;
#127261 = FACE_OUTER_BOUND ( 'NONE', #199642, .T. ) ;
#127262 = VECTOR ( 'NONE', #43557, 1000.000000000000000 ) ;
#127263 = AXIS2_PLACEMENT_3D ( 'NONE', #37740, #217605, #218899 ) ;
#127264 = ORIENTED_EDGE ( 'NONE', *, *, #12603, .T. ) ;
#127265 = TOROIDAL_SURFACE ( 'NONE', #14857, 12.77500000000000036, 0.1000000000000000056 ) ;
#127266 = DIRECTION ( 'NONE',  ( 0.000000000000000000, 0.9126074666063772600, 0.4088369013363276627 ) ) ;
#127268 = ORIENTED_EDGE ( 'NONE', *, *, #48694, .T. ) ;
#127267 = DIRECTION ( 'NONE',  ( 0.000000000000000000, 0.000000000000000000, 1.000000000000000000 ) ) ;
#127269 = CARTESIAN_POINT ( 'NONE',  ( -16.93433913041102912, 10.00597842153509376, -121.4353654273952117 ) ) ;
#127270 = FACE_OUTER_BOUND ( 'NONE', #245511, .T. ) ;
#127271 = DIRECTION ( 'NONE',  ( 0.000000000000000000, 0.000000000000000000, 1.000000000000000000 ) ) ;
#127272 = EDGE_CURVE ( 'NONE', #126474, #74995, #66539, .T. ) ;
#127273 = FACE_OUTER_BOUND ( 'NONE', #96584, .T. ) ;
#127274 = LINE ( 'NONE', #49012, #237965 ) ;
#127275 = CARTESIAN_POINT ( 'NONE',  ( 20.89999999999999858, -11.75000000000000000, -15.00000000000000000 ) ) ;
#127276 = FACE_OUTER_BOUND ( 'NONE', #52835, .T. ) ;
#127277 = EDGE_CURVE ( 'NONE', #228417, #150739, #195742, .T. ) ;
#127278 = VERTEX_POINT ( 'NONE', #150770 ) ;
#127279 = DIRECTION ( 'NONE',  ( 0.000000000000000000, 0.1350103645451945777, -0.9908441862701591329 ) ) ;
#127280 = DIRECTION ( 'NONE',  ( 1.000000000000000000, 2.952720810173289112E-16, -0.000000000000000000 ) ) ;
#127281 = CARTESIAN_POINT ( 'NONE',  ( -16.86379686415369150, 51.68465521706279731, -231.8893622364056171 ) ) ;
#127282 = CIRCLE ( 'NONE', #164883, 0.1000000000000076522 ) ;
#127283 = CARTESIAN_POINT ( 'NONE',  ( -23.25000000000000000, 85.00000000001232081, -160.1291383618718385 ) ) ;
#127284 = EDGE_CURVE ( 'NONE', #154073, #6368, #37508, .T. ) ;
#127285 = CARTESIAN_POINT ( 'NONE',  ( -22.39999999999999858, 1.115600667400684642E-11, -159.7092204016265384 ) ) ;
#127286 = EDGE_LOOP ( 'NONE', ( #222447, #93754, #22553, #157672 ) ) ;
#127287 = ORIENTED_EDGE ( 'NONE', *, *, #159450, .T. ) ;
#127288 = DIRECTION ( 'NONE',  ( 0.000000000000000000, -0.9910465087640860649, 0.1335171055202901413 ) ) ;
#127289 = EDGE_CURVE ( 'NONE', #217036, #177234, #167796, .T. ) ;
#127291 = CARTESIAN_POINT ( 'NONE',  ( 21.14999999999999858, 13.96869538424788715, -210.3925794786331949 ) ) ;
#127290 = AXIS2_PLACEMENT_3D ( 'NONE', #42642, #83018, #218693 ) ;
#127292 = CARTESIAN_POINT ( 'NONE',  ( 21.05000000000005400, 66.15000000001120384, -4.623107484524796362 ) ) ;
#127293 = EDGE_CURVE ( 'NONE', #61914, #85377, #54046, .T. ) ;
#127294 = DIRECTION ( 'NONE',  ( -0.000000000000000000, -6.982962677686266711E-15, 1.000000000000000000 ) ) ;
#127295 = EDGE_CURVE ( 'NONE', #56611, #249805, #199831, .T. ) ;
#127296 = DIRECTION ( 'NONE',  ( 1.000000000000000000, 0.000000000000000000, 0.000000000000000000 ) ) ;
#127297 = ADVANCED_FACE ( 'NONE', ( #153382 ), #112340, .T. ) ;
#127298 = CARTESIAN_POINT ( 'NONE',  ( 23.15000000000000213, -8.663551401857999323, -124.4758988819327215 ) ) ;
#127299 = AXIS2_PLACEMENT_3D ( 'NONE', #103383, #202510, #23906 ) ;
#127300 = CIRCLE ( 'NONE', #102320, 0.09999999999999939493 ) ;
#127301 = EDGE_CURVE ( 'NONE', #112216, #142489, #95728, .T. ) ;
#127302 = ORIENTED_EDGE ( 'NONE', *, *, #42333, .F. ) ;
#127303 = DIRECTION ( 'NONE',  ( 0.2834754621636439431, -0.2834754621636535465, -0.9161240771326838450 ) ) ;
#127304 = VERTEX_POINT ( 'NONE', #73832 ) ;
#127305 = CARTESIAN_POINT ( 'NONE',  ( -18.50000000000000000, 66.65000000001253966, -182.1731074845244223 ) ) ;
#127307 = ADVANCED_FACE ( 'NONE', ( #252416 ), #58122, .T. ) ;
#127306 = CARTESIAN_POINT ( 'NONE',  ( -23.25000000000000000, 4.350000000011156054, -45.65000000000000568 ) ) ;
#127308 = CARTESIAN_POINT ( 'NONE',  ( 20.85000000000000142, 78.57213941646344324, -232.7862224702232652 ) ) ;
#127309 = CARTESIAN_POINT ( 'NONE',  ( -16.79184697841823493, 9.948761661669548673, -46.15414227060252728 ) ) ;
#127310 = DIRECTION ( 'NONE',  ( 0.000000000000000000, 1.000000000000000000, 0.000000000000000000 ) ) ;
#127311 = CARTESIAN_POINT ( 'NONE',  ( -18.41799967126733506, -9.500000000000007105, -7.032069813255726665 ) ) ;
#127312 = CARTESIAN_POINT ( 'NONE',  ( -16.93388492042257809, 66.01145817749589639, -82.12256236133821119 ) ) ;
#127313 = ORIENTED_EDGE ( 'NONE', *, *, #197709, .T. ) ;
#127314 = ADVANCED_FACE ( 'NONE', ( #109062 ), #49089, .T. ) ;
#127315 = DIRECTION ( 'NONE',  ( -1.000000000000000000, -0.000000000000000000, -0.000000000000000000 ) ) ;
#127316 = CARTESIAN_POINT ( 'NONE',  ( 18.54999999999999716, 8.750000000011182166, -46.15000000000000568 ) ) ;
#127317 = CARTESIAN_POINT ( 'NONE',  ( -20.85000000000000142, 46.46967969402478360, -243.0849751855955674 ) ) ;
#127318 = SPHERICAL_SURFACE ( 'NONE', #201913, 0.1000000000000000056 ) ;
#127319 = VECTOR ( 'NONE', #146868, 1000.000000000000000 ) ;
#127320 = AXIS2_PLACEMENT_3D ( 'NONE', #139209, #179665, #972 ) ;
#127321 = FACE_OUTER_BOUND ( 'NONE', #245251, .T. ) ;
#127323 = DIRECTION ( 'NONE',  ( 0.000000000000000000, 0.000000000000000000, -1.000000000000000000 ) ) ;
#127322 = VECTOR ( 'NONE', #14075, 1000.000000000000000 ) ;
#127324 = CIRCLE ( 'NONE', #14915, 0.5000000000000004441 ) ;
#127325 = ORIENTED_EDGE ( 'NONE', *, *, #239482, .T. ) ;
#127327 = CYLINDRICAL_SURFACE ( 'NONE', #247786, 0.09999999999999939493 ) ;
#127326 =( GEOMETRIC_REPRESENTATION_CONTEXT ( 3 ) GLOBAL_UNCERTAINTY_ASSIGNED_CONTEXT ( ( #162634 ) ) GLOBAL_UNIT_ASSIGNED_CONTEXT ( ( #72395, #235288, #55337 ) ) REPRESENTATION_CONTEXT ( 'NONE', 'WORKASPACE' ) );
#127329 = EDGE_CURVE ( 'NONE', #230022, #201378, #114578, .T. ) ;
#127328 = DIRECTION ( 'NONE',  ( 1.000000000000000000, 0.000000000000000000, -0.000000000000000000 ) ) ;
#127330 = ORIENTED_EDGE ( 'NONE', *, *, #79439, .F. ) ;
#127331 = CARTESIAN_POINT ( 'NONE',  ( -22.59999999999999787, 0.1000000000111554016, -88.85042919245522341 ) ) ;
#127332 = DIRECTION ( 'NONE',  ( -0.000000000000000000, 0.4721928772777345684, 0.8814952561688429444 ) ) ;
#127333 = DIRECTION ( 'NONE',  ( 1.000000000000000000, -2.952720810173289112E-16, -2.061873921506763405E-30 ) ) ;
#127334 = ORIENTED_EDGE ( 'NONE', *, *, #94426, .T. ) ;
#127335 = CARTESIAN_POINT ( 'NONE',  ( 18.33683296300457499, -9.511149971121650282, -174.4057074127099725 ) ) ;
#127336 = CARTESIAN_POINT ( 'NONE',  ( 5.900000000000059863, 64.65000000001120384, -26.02310748452479316 ) ) ;
#127337 = VERTEX_POINT ( 'NONE', #69971 ) ;
#127338 = PRESENTATION_LAYER_ASSIGNMENT (  '', '', ( #10648 ) ) ;
#127339 = ADVANCED_FACE ( 'NONE', ( #29572, #191209 ), #188603, .T. ) ;
#127340 = VECTOR ( 'NONE', #216203, 1000.000000000000227 ) ;
#127341 = CARTESIAN_POINT ( 'NONE',  ( -21.05000000000000426, 76.02103547655211457, -109.3275633064719869 ) ) ;
#127342 = ORIENTED_EDGE ( 'NONE', *, *, #150912, .T. ) ;
#127343 = AXIS2_PLACEMENT_3D ( 'NONE', #132139, #254625, #193415 ) ;
#127344 = DIRECTION ( 'NONE',  ( 0.000000000000000000, 0.8814952561688429444, -0.4721928772777348460 ) ) ;
#127346 = EDGE_CURVE ( 'NONE', #133238, #164153, #174927, .T. ) ;
#127345 = DIRECTION ( 'NONE',  ( 1.734723475976817192E-14, -0.4721928772777346239, -0.8814952561688430555 ) ) ;
#127347 = DIRECTION ( 'NONE',  ( 0.000000000000000000, 1.000000000000000000, -0.000000000000000000 ) ) ;
#127349 = AXIS2_PLACEMENT_3D ( 'NONE', #172302, #35350, #114844 ) ;
#127348 = DIRECTION ( 'NONE',  ( 0.000000000000000000, 0.1332476588733589318, -0.9910827722268050755 ) ) ;
#127350 = DIRECTION ( 'NONE',  ( 1.000000000000000000, 0.000000000000000000, 0.000000000000000000 ) ) ;
#127351 = AXIS2_PLACEMENT_3D ( 'NONE', #13303, #169852, #88962 ) ;
#127352 = DIRECTION ( 'NONE',  ( 1.734723475976817507E-14, 0.000000000000000000, -1.000000000000000000 ) ) ;
#127353 = CARTESIAN_POINT ( 'NONE',  ( 21.05000000000000071, 1.115600667400684642E-11, -134.0000000000000284 ) ) ;
#127354 = EDGE_CURVE ( 'NONE', #219674, #218042, #237234, .T. ) ;
#127355 = DIRECTION ( 'NONE',  ( 0.000000000000000000, -0.1350103645451557199, -0.9908441862701644620 ) ) ;
#127356 = DIRECTION ( 'NONE',  ( 0.000000000000000000, 0.000000000000000000, 1.000000000000000000 ) ) ;
#127357 = EDGE_CURVE ( 'NONE', #64016, #87492, #253955, .T. ) ;
#127359 = ORIENTED_EDGE ( 'NONE', *, *, #217770, .F. ) ;
#127358 = CARTESIAN_POINT ( 'NONE',  ( 18.50000000000000000, 86.87893363400692692, -199.4025658100844680 ) ) ;
#127360 = VERTEX_POINT ( 'NONE', #231602 ) ;
#127362 = DIRECTION ( 'NONE',  ( 0.000000000000000000, 0.000000000000000000, -1.000000000000000000 ) ) ;
#127361 = CARTESIAN_POINT ( 'NONE',  ( -23.25000000000000000, 1.115600667400684642E-11, -134.0000000000000284 ) ) ;
#127364 = EDGE_LOOP ( 'NONE', ( #161858, #92772, #222527, #53359 ) ) ;
#127363 = DIRECTION ( 'NONE',  ( -1.000000000000000000, 2.952720810173289112E-16, 2.061873921506763405E-30 ) ) ;
#127365 = EDGE_CURVE ( 'NONE', #219135, #75871, #99808, .T. ) ;
#127366 = ORIENTED_EDGE ( 'NONE', *, *, #155616, .T. ) ;
#127367 = DIRECTION ( 'NONE',  ( 0.7071067811865475727, -0.7071067811865475727, 0.000000000000000000 ) ) ;
#127368 = ADVANCED_FACE ( 'NONE', ( #2914 ), #221945, .T. ) ;
#127369 = CARTESIAN_POINT ( 'NONE',  ( 21.05000000000000071, 77.73625713160946304, -124.9544551555067926 ) ) ;
#127370 = VECTOR ( 'NONE', #33697, 1000.000000000000000 ) ;
#127372 = EDGE_CURVE ( 'NONE', #95759, #246109, #124799, .T. ) ;
#127371 = CARTESIAN_POINT ( 'NONE',  ( -23.25000000000000000, 74.08971962618008433, -90.39173962932538586 ) ) ;
#127373 = CARTESIAN_POINT ( 'NONE',  ( -20.87600722750343252, 10.33112638556969465, -173.0901228926974795 ) ) ;
#127374 = AXIS2_PLACEMENT_3D ( 'NONE', #168415, #208783, #185357 ) ;
#127375 = DIRECTION ( 'NONE',  ( 0.000000000000000000, 0.2128009952263604232, -0.9770955615653316162 ) ) ;
#127376 = VECTOR ( 'NONE', #220600, 1000.000000000000000 ) ;
#127377 = DIRECTION ( 'NONE',  ( 1.000000000000000000, 0.000000000000000000, 0.000000000000000000 ) ) ;
#127378 = DIRECTION ( 'NONE',  ( 0.000000000000000000, 0.000000000000000000, 1.000000000000000000 ) ) ;
#127379 = ORIENTED_EDGE ( 'NONE', *, *, #76066, .F. ) ;
#127380 = VERTEX_POINT ( 'NONE', #43352 ) ;
#127381 = FACE_OUTER_BOUND ( 'NONE', #183433, .T. ) ;
#127382 = VERTEX_POINT ( 'NONE', #143717 ) ;
#127383 = DIRECTION ( 'NONE',  ( -0.000000000000000000, 1.000000000000000000, 6.352154140967427193E-15 ) ) ;
#127384 = ORIENTED_EDGE ( 'NONE', *, *, #48480, .F. ) ;
#127385 = DIRECTION ( 'NONE',  ( 1.000000000000000000, 0.000000000000000000, 0.000000000000000000 ) ) ;
#127386 = ADVANCED_FACE ( 'NONE', ( #196303 ), #122891, .T. ) ;
#127387 = CARTESIAN_POINT ( 'NONE',  ( 22.39999999999999503, 75.90000000001219860, -144.3138870828976792 ) ) ;
#127388 = DIRECTION ( 'NONE',  ( -0.000000000000000000, 1.000000000000000000, 1.734723475976807292E-15 ) ) ;
#127389 = EDGE_CURVE ( 'NONE', #208842, #220457, #129077, .T. ) ;
#127390 = CARTESIAN_POINT ( 'NONE',  ( -20.94999999999999929, 1.851028230152016674, -112.1539132694225316 ) ) ;
#127391 = VERTEX_POINT ( 'NONE', #83707 ) ;
#127392 = APPLICATION_CONTEXT ( 'automotive_design' ) ;
#127393 = EDGE_CURVE ( 'NONE', #69711, #226308, #83258, .T. ) ;
#127394 = CARTESIAN_POINT ( 'NONE',  ( -23.15000000000000213, 76.00000000001186606, -90.14810748452431710 ) ) ;
#127395 = EDGE_LOOP ( 'NONE', ( #207446, #180300, #26678, #177700 ) ) ;
#127396 = CIRCLE ( 'NONE', #52560, 0.09999999999999939493 ) ;
#127397 = DIRECTION ( 'NONE',  ( 0.000000000000000000, 1.084202172485510997E-13, -1.000000000000000000 ) ) ;
#127398 = DIRECTION ( 'NONE',  ( 1.000000000000000000, 0.000000000000000000, -0.000000000000000000 ) ) ;
#127399 = CIRCLE ( 'NONE', #81563, 11.70000000000000284 ) ;
#127400 = DIRECTION ( 'NONE',  ( -1.000000000000000000, 0.000000000000000000, 0.000000000000000000 ) ) ;
#127401 = CARTESIAN_POINT ( 'NONE',  ( 13.99999999999999822, 66.15000000001258229, -186.7731074845244450 ) ) ;
#127402 = AXIS2_PLACEMENT_3D ( 'NONE', #196767, #215059, #153860 ) ;
#127403 = AXIS2_PLACEMENT_3D ( 'NONE', #176501, #233889, #236452 ) ;
#127404 = VERTEX_POINT ( 'NONE', #76345 ) ;
#127405 = PLANE ( 'NONE',  #156843 ) ;
#127406 = ORIENTED_EDGE ( 'NONE', *, *, #197316, .F. ) ;
#127409 = ORIENTED_EDGE ( 'NONE', *, *, #50388, .T. ) ;
#127408 = CARTESIAN_POINT ( 'NONE',  ( -21.55000000000000426, 7.708578643773852157, -88.15000000000004832 ) ) ;
#127407 = FACE_OUTER_BOUND ( 'NONE', #179335, .T. ) ;
#127410 = DIRECTION ( 'NONE',  ( 7.304098846218134667E-16, -1.000000000000000000, 0.000000000000000000 ) ) ;
#127411 = ORIENTED_EDGE ( 'NONE', *, *, #203542, .F. ) ;
#127412 = VECTOR ( 'NONE', #32213, 1000.000000000000000 ) ;
#127413 = CARTESIAN_POINT ( 'NONE',  ( 20.94999999999997442, -1.263275465206102233, -141.9018646667464338 ) ) ;
#127414 = VERTEX_POINT ( 'NONE', #253705 ) ;
#127415 = DIRECTION ( 'NONE',  ( 1.000000000000000000, 0.000000000000000000, 0.000000000000000000 ) ) ;
#127416 = AXIS2_PLACEMENT_3D ( 'NONE', #161847, #140989, #220521 ) ;
#127417 = DIRECTION ( 'NONE',  ( -1.000000000000000000, 0.000000000000000000, 0.000000000000000000 ) ) ;
#127418 = SPHERICAL_SURFACE ( 'NONE', #172662, 0.1000000000000000056 ) ;
#127419 = CIRCLE ( 'NONE', #69193, 0.09999999999999999167 ) ;
#127420 = ORIENTED_EDGE ( 'NONE', *, *, #17544, .F. ) ;
#127421 = DIRECTION ( 'NONE',  ( 0.000000000000000000, -6.982962677686267499E-15, 1.000000000000000000 ) ) ;
#127422 = LINE ( 'NONE', #110416, #41009 ) ;
#127423 = DIRECTION ( 'NONE',  ( 0.000000000000000000, 0.8814952561688429444, -0.4721928772777345684 ) ) ;
#127424 = EDGE_LOOP ( 'NONE', ( #241722, #172586, #243988, #30243 ) ) ;
#127425 = DIRECTION ( 'NONE',  ( 0.7071067811865388020, -0.7071067811865561215, 0.000000000000000000 ) ) ;
#127426 = EDGE_LOOP ( 'NONE', ( #131501, #141848, #217045, #231269 ) ) ;
#127427 = LINE ( 'NONE', #246101, #43767 ) ;
#127428 = DIRECTION ( 'NONE',  ( -3.265361837132813093E-16, -1.000000000000000000, -6.982962677686266711E-15 ) ) ;
#127429 = DIRECTION ( 'NONE',  ( 1.000000000000000000, 0.000000000000000000, 0.000000000000000000 ) ) ;
#127431 = EDGE_LOOP ( 'NONE', ( #64253, #116329, #132483, #195763 ) ) ;
#127430 = CARTESIAN_POINT ( 'NONE',  ( -21.05000000000000071, -4.969162394454528453, -233.3995358778103935 ) ) ;
#127432 = CARTESIAN_POINT ( 'NONE',  ( 22.39999999999999858, 0.000000000000000000, 0.000000000000000000 ) ) ;
#127433 = CARTESIAN_POINT ( 'NONE',  ( -18.50000000000000000, 0.6656436123793491033, -212.6810495496487476 ) ) ;
#127434 = EDGE_CURVE ( 'NONE', #62589, #212495, #191470, .T. ) ;
#127435 = CARTESIAN_POINT ( 'NONE',  ( -21.05000000000000071, 76.00000000001168132, -65.42310748452432279 ) ) ;
#127436 = ORIENTED_EDGE ( 'NONE', *, *, #247201, .T. ) ;
#127437 = CYLINDRICAL_SURFACE ( 'NONE', #197519, 0.1000000000000028644 ) ;
#127439 = ADVANCED_FACE ( 'NONE', ( #195051 ), #116595, .T. ) ;
#127438 = CARTESIAN_POINT ( 'NONE',  ( 18.60000000000000142, 85.32100840337361092, -162.7871692354463846 ) ) ;
#127440 = ORIENTED_EDGE ( 'NONE', *, *, #36647, .F. ) ;
#127441 = DIRECTION ( 'NONE',  ( 0.000000000000000000, 0.000000000000000000, 1.000000000000000000 ) ) ;
#127442 = VECTOR ( 'NONE', #230170, 1000.000000000000000 ) ;
#127443 = VECTOR ( 'NONE', #156102, 1000.000000000000227 ) ;
#127444 = CIRCLE ( 'NONE', #73503, 0.5000000000000004441 ) ;
#127445 = TOROIDAL_SURFACE ( 'NONE', #56669, 0.2000000000000000111, 0.1000000000000000056 ) ;
#127446 = ORIENTED_EDGE ( 'NONE', *, *, #68912, .T. ) ;
#127447 = EDGE_CURVE ( 'NONE', #83522, #60627, #158163, .T. ) ;
#127448 = FACE_OUTER_BOUND ( 'NONE', #225241, .T. ) ;
#127451 = EDGE_CURVE ( 'NONE', #237722, #169627, #234146, .T. ) ;
#127450 = ORIENTED_EDGE ( 'NONE', *, *, #99381, .F. ) ;
#127449 = CYLINDRICAL_SURFACE ( 'NONE', #167882, 0.1000000000000028644 ) ;
#127454 = ORIENTED_EDGE ( 'NONE', *, *, #68866, .T. ) ;
#127453 = ORIENTED_EDGE ( 'NONE', *, *, #145765, .F. ) ;
#127452 = CYLINDRICAL_SURFACE ( 'NONE', #5349, 4.000000000000003553 ) ;
#127455 = DIRECTION ( 'NONE',  ( 0.000000000000000000, -0.4721928772777346239, -0.8814952561688430555 ) ) ;
#127456 = CARTESIAN_POINT ( 'NONE',  ( -18.79999999999999716, 11.61130914238355771, -1.800000000000000044 ) ) ;
#127457 = CARTESIAN_POINT ( 'NONE',  ( -21.05000000000000071, 17.01923898301589944, -224.3994341343041867 ) ) ;
#127458 = CARTESIAN_POINT ( 'NONE',  ( -18.50000000000000000, 77.83585931145526615, -58.01866831572577610 ) ) ;
#127459 = CARTESIAN_POINT ( 'NONE',  ( -13.39999999999994529, 67.75000000001118394, -25.06452884076210452 ) ) ;
#127460 = DIRECTION ( 'NONE',  ( 0.000000000000000000, 0.01562500000001262185, 0.9998779222360095753 ) ) ;
#127461 = CIRCLE ( 'NONE', #15055, 0.1000000000000016015 ) ;
#127462 = DIRECTION ( 'NONE',  ( 1.186688945009009831E-16, 1.000000000000000000, 6.982962677686266711E-15 ) ) ;
#127463 = DIRECTION ( 'NONE',  ( 0.000000000000000000, 0.000000000000000000, 1.000000000000000000 ) ) ;
#127464 = EDGE_CURVE ( 'NONE', #127854, #216920, #258023, .T. ) ;
#127465 = EDGE_CURVE ( 'NONE', #75338, #36049, #216558, .T. ) ;
#127466 = EDGE_LOOP ( 'NONE', ( #173703, #228763, #71612, #144192, #540, #78390, #40176, #118537 ) ) ;
#127467 = ORIENTED_EDGE ( 'NONE', *, *, #86899, .F. ) ;
#127468 = DIRECTION ( 'NONE',  ( 0.000000000000000000, -6.982962677686266711E-15, 1.000000000000000000 ) ) ;
#127469 = CIRCLE ( 'NONE', #6656, 0.09999999999999646672 ) ;
#127471 = ORIENTED_EDGE ( 'NONE', *, *, #151493, .T. ) ;
#127470 = DIRECTION ( 'NONE',  ( 1.000000000000000000, 0.000000000000000000, 0.000000000000000000 ) ) ;
#127472 = VERTEX_POINT ( 'NONE', #16415 ) ;
#127473 = CARTESIAN_POINT ( 'NONE',  ( -16.77779411503079388, 12.41300279975761889, -211.2564769120770336 ) ) ;
#127474 = ORIENTED_EDGE ( 'NONE', *, *, #123963, .T. ) ;
#127475 = DIRECTION ( 'NONE',  ( 0.000000000000000000, 0.000000000000000000, 1.000000000000000000 ) ) ;
#127476 = ADVANCED_FACE ( 'NONE', ( #61623 ), #162029, .T. ) ;
#127477 = ORIENTED_EDGE ( 'NONE', *, *, #5662, .T. ) ;
#127478 = DIRECTION ( 'NONE',  ( -0.000000000000000000, -0.000000000000000000, -1.000000000000000000 ) ) ;
#127479 = DIRECTION ( 'NONE',  ( -1.000000000000000000, -1.040834085586090568E-13, 0.000000000000000000 ) ) ;
#127480 = ADVANCED_FACE ( 'NONE', ( #37261 ), #33242, .T. ) ;
#127483 = EDGE_LOOP ( 'NONE', ( #47472, #15511, #245161, #180634 ) ) ;
#127482 = EDGE_LOOP ( 'NONE', ( #53315, #136127, #200913, #235979 ) ) ;
#127481 = CIRCLE ( 'NONE', #202501, 0.8750000000000007772 ) ;
#127484 = EDGE_LOOP ( 'NONE', ( #21595, #30562, #139521, #207638 ) ) ;
#127485 = CARTESIAN_POINT ( 'NONE',  ( 21.05000000000000071, 23.49882452903949570, -253.1653563615082305 ) ) ;
#127486 = VERTEX_POINT ( 'NONE', #181589 ) ;
#127487 = VERTEX_POINT ( 'NONE', #64194 ) ;
#127488 = FACE_OUTER_BOUND ( 'NONE', #226483, .T. ) ;
#127489 = CARTESIAN_POINT ( 'NONE',  ( 18.59999999999999076, 74.16465844978715438, -57.86795619196135476 ) ) ;
#127490 = DIRECTION ( 'NONE',  ( 0.000000000000000000, 0.000000000000000000, -1.000000000000000000 ) ) ;
#127492 = VERTEX_POINT ( 'NONE', #116773 ) ;
#127491 = FACE_OUTER_BOUND ( 'NONE', #249400, .T. ) ;
#127493 = DIRECTION ( 'NONE',  ( 0.000000000000000000, 0.2128009952263604232, -0.9770955615653316162 ) ) ;
#127494 = ADVANCED_FACE ( 'NONE', ( #201128 ), #214581, .T. ) ;
#127495 = DIRECTION ( 'NONE',  ( 0.000000000000000000, 0.000000000000000000, -1.000000000000000000 ) ) ;
#127497 = VERTEX_POINT ( 'NONE', #10639 ) ;
#127496 = DIRECTION ( 'NONE',  ( 1.000000000000000000, -0.000000000000000000, -0.000000000000000000 ) ) ;
#127498 = FACE_OUTER_BOUND ( 'NONE', #90953, .T. ) ;
#127499 = EDGE_LOOP ( 'NONE', ( #170265, #55437, #48477, #223290 ) ) ;
#127500 = CARTESIAN_POINT ( 'NONE',  ( 20.94999999999999574, 87.65000000001234071, -166.9231074845242802 ) ) ;
#127501 = EDGE_CURVE ( 'NONE', #2887, #1640, #88860, .T. ) ;
#127502 = ORIENTED_EDGE ( 'NONE', *, *, #120034, .T. ) ;
#127503 = CARTESIAN_POINT ( 'NONE',  ( -21.12844524849339223, 18.76330736928263221, -226.6353469151677587 ) ) ;
#127504 = DIRECTION ( 'NONE',  ( -1.000000000000000000, 1.207181226542539700E-16, -2.694675058168174199E-16 ) ) ;
#127505 = CIRCLE ( 'NONE', #152662, 11.65000000000000036 ) ;
#127507 = ADVANCED_FACE ( 'NONE', ( #189280 ), #186721, .T. ) ;
#127506 = ORIENTED_EDGE ( 'NONE', *, *, #167990, .F. ) ;
#127509 = FACE_OUTER_BOUND ( 'NONE', #171844, .T. ) ;
#127508 = CARTESIAN_POINT ( 'NONE',  ( -23.39999999999994529, 83.88667523412387084, -37.37221576174746929 ) ) ;
#127510 = DIRECTION ( 'NONE',  ( 0.000000000000000000, 0.000000000000000000, -1.000000000000000000 ) ) ;
#127511 = AXIS2_PLACEMENT_3D ( 'NONE', #36396, #78051, #153805 ) ;
#127512 = DIRECTION ( 'NONE',  ( 1.000000000000000000, 0.000000000000000000, 0.000000000000000000 ) ) ;
#127513 = CARTESIAN_POINT ( 'NONE',  ( -12.47155713865591586, 12.53760658702567810, -214.5091953838863503 ) ) ;
#127514 = ORIENTED_EDGE ( 'NONE', *, *, #224498, .T. ) ;
#127515 = EDGE_LOOP ( 'NONE', ( #60071, #13420, #38255, #149168 ) ) ;
#127516 = STYLED_ITEM ( 'NONE', ( #195892 ), #178764 ) ;
#127517 = FACE_OUTER_BOUND ( 'NONE', #31111, .T. ) ;
#127518 = DIRECTION ( 'NONE',  ( 0.000000000000000000, 1.000000000000000000, 0.000000000000000000 ) ) ;
#127519 = ORIENTED_EDGE ( 'NONE', *, *, #200142, .F. ) ;
#127520 = CARTESIAN_POINT ( 'NONE',  ( -14.00000000000000178, 66.15000000001258229, -186.7731074845244166 ) ) ;
#127521 = ORIENTED_EDGE ( 'NONE', *, *, #81714, .T. ) ;
#127522 = EDGE_CURVE ( 'NONE', #4003, #11973, #169746, .T. ) ;
#127523 = DIRECTION ( 'NONE',  ( -1.073024830501117725E-15, 0.000000000000000000, 1.000000000000000000 ) ) ;
#127524 = EDGE_LOOP ( 'NONE', ( #131869, #101834, #183663, #150233 ) ) ;
#127525 = CARTESIAN_POINT ( 'NONE',  ( -21.05000000000000071, 64.40000000001147384, -42.95131071479990936 ) ) ;
#127527 = EDGE_CURVE ( 'NONE', #249371, #66847, #169749, .T. ) ;
#127526 = CARTESIAN_POINT ( 'NONE',  ( -20.64999999999999858, 11.60058429089262333, -246.3380203656811887 ) ) ;
#127528 = ORIENTED_EDGE ( 'NONE', *, *, #174616, .T. ) ;
#127529 = TOROIDAL_SURFACE ( 'NONE', #15103, 12.77499999999999858, 0.1000000000000000056 ) ;
#127530 = EDGE_LOOP ( 'NONE', ( #142815, #230005, #72493, #132246 ) ) ;
#127531 = ORIENTED_EDGE ( 'NONE', *, *, #215185, .T. ) ;
#127532 = CIRCLE ( 'NONE', #98260, 0.09999999999998898659 ) ;
#127533 = ORIENTED_EDGE ( 'NONE', *, *, #39884, .F. ) ;
#127534 = CARTESIAN_POINT ( 'NONE',  ( 22.59066674512275696, 64.25000000001213607, -136.5536116081545401 ) ) ;
#127535 = FACE_OUTER_BOUND ( 'NONE', #185659, .T. ) ;
#127536 = FACE_OUTER_BOUND ( 'NONE', #18968, .T. ) ;
#127537 = DIRECTION ( 'NONE',  ( -0.000000000000000000, 1.000000000000000000, -0.000000000000000000 ) ) ;
#127538 = CARTESIAN_POINT ( 'NONE',  ( -16.87036670365548474, 30.33914847462231279, -234.8334748671511818 ) ) ;
#127540 = CARTESIAN_POINT ( 'NONE',  ( 21.04999999999908411, 8.776282895290673736, -12.15790900265250052 ) ) ;
#127539 = CARTESIAN_POINT ( 'NONE',  ( 20.85000000000000142, 77.85161776048025217, -24.41991776492064758 ) ) ;
#127542 = ORIENTED_EDGE ( 'NONE', *, *, #77294, .T. ) ;
#127541 = CARTESIAN_POINT ( 'NONE',  ( 21.00000000000000000, 9.749999999999998224, -12.35000000000000320 ) ) ;
#127543 = DIRECTION ( 'NONE',  ( -1.073024830501117725E-15, 0.9126074666063770380, 0.4088369013363281068 ) ) ;
#127544 = VERTEX_POINT ( 'NONE', #249254 ) ;
#127545 = CIRCLE ( 'NONE', #60890, 11.65000000000000036 ) ;
#127546 = CARTESIAN_POINT ( 'NONE',  ( 20.95512820512820440, 8.876151316299271343, -188.7499999999999716 ) ) ;
#127547 = ORIENTED_EDGE ( 'NONE', *, *, #169591, .T. ) ;
#127548 = ORIENTED_EDGE ( 'NONE', *, *, #140322, .F. ) ;
#127549 = DIRECTION ( 'NONE',  ( 0.000000000000000000, 0.2128009952263601456, -0.9770955615653315052 ) ) ;
#127550 = DIRECTION ( 'NONE',  ( 0.000000000000000000, 0.000000000000000000, 1.000000000000000000 ) ) ;
#127551 = CARTESIAN_POINT ( 'NONE',  ( -16.94052228080552069, 66.01372026691267081, -48.63273198185498103 ) ) ;
#127552 = CARTESIAN_POINT ( 'NONE',  ( 20.94999999999999929, 67.22371710471912820, -60.96447848938343839 ) ) ;
#127553 = B_SPLINE_CURVE_WITH_KNOTS ( 'NONE', 3,
 ( #74360, #110881, #211268, #247824 ),
 .UNSPECIFIED., .F., .F.,
 ( 4, 4 ),
 ( 0.000000000000000000, 0.001767853679387111458 ),
 .UNSPECIFIED. ) ;
#127554 = VECTOR ( 'NONE', #56863, 1000.000000000000000 ) ;
#127555 = FACE_OUTER_BOUND ( 'NONE', #165867, .T. ) ;
#127557 = ORIENTED_EDGE ( 'NONE', *, *, #226356, .F. ) ;
#127556 = AXIS2_PLACEMENT_3D ( 'NONE', #196166, #235283, #20112 ) ;
#127558 = ORIENTED_EDGE ( 'NONE', *, *, #136394, .F. ) ;
#127559 = CIRCLE ( 'NONE', #15131, 0.2000000000000057288 ) ;
#127560 = DIRECTION ( 'NONE',  ( 1.000000000000000000, -0.000000000000000000, -0.000000000000000000 ) ) ;
#127561 = ORIENTED_EDGE ( 'NONE', *, *, #151917, .F. ) ;
#127562 = CARTESIAN_POINT ( 'NONE',  ( -22.47071067811865319, 0.09909245471376171288, -126.2799252555019649 ) ) ;
#127563 = FACE_OUTER_BOUND ( 'NONE', #94159, .T. ) ;
#127564 = ORIENTED_EDGE ( 'NONE', *, *, #2166, .T. ) ;
#127565 = CARTESIAN_POINT ( 'NONE',  ( -18.69999999999999929, -9.849999999999994316, 30.09999999999999787 ) ) ;
#127566 = CIRCLE ( 'NONE', #256484, 4.150000000000001243 ) ;
#127567 = CARTESIAN_POINT ( 'NONE',  ( -16.97092634996618798, 65.99911103366422083, -123.8929647182264944 ) ) ;
#127568 = CARTESIAN_POINT ( 'NONE',  ( 18.50000000000000000, 8.841736820195473356, -245.4273993276876240 ) ) ;
#127569 = ORIENTED_EDGE ( 'NONE', *, *, #43350, .T. ) ;
#127570 = FACE_OUTER_BOUND ( 'NONE', #245638, .T. ) ;
#127571 = CYLINDRICAL_SURFACE ( 'NONE', #170738, 0.09999999999999939493 ) ;
#127572 = CARTESIAN_POINT ( 'NONE',  ( 23.14999999999999858, 5.500000000011153745, -188.5947339810868755 ) ) ;
#127573 = CARTESIAN_POINT ( 'NONE',  ( 21.14999999999999858, 69.45934304831071415, -102.9231074845243512 ) ) ;
#127575 = EDGE_CURVE ( 'NONE', #72307, #227912, #245404, .T. ) ;
#127574 = CYLINDRICAL_SURFACE ( 'NONE', #179040, 0.1000000000000098310 ) ;
#127576 = CIRCLE ( 'NONE', #44199, 0.1000000000000028644 ) ;
#127577 = DIRECTION ( 'NONE',  ( -3.756152431956878006E-15, -0.9910827722268042983, 0.1332476588733650935 ) ) ;
#127578 = ORIENTED_EDGE ( 'NONE', *, *, #108554, .F. ) ;
#127579 = DIRECTION ( 'NONE',  ( 0.000000000000000000, 1.000000000000000000, 0.000000000000000000 ) ) ;
#127580 = EDGE_CURVE ( 'NONE', #252649, #24761, #115525, .T. ) ;
#127581 = ORIENTED_EDGE ( 'NONE', *, *, #43022, .T. ) ;
#127582 = CARTESIAN_POINT ( 'NONE',  ( -20.94999999999999929, 87.41227409416161720, -105.9231074845242091 ) ) ;
#127584 = CIRCLE ( 'NONE', #15156, 0.2000000000000057288 ) ;
#127583 = DIRECTION ( 'NONE',  ( 0.000000000000000000, 0.000000000000000000, -1.000000000000000000 ) ) ;
#127585 = CARTESIAN_POINT ( 'NONE',  ( -20.54999999999999716, 74.07476635515278929, -190.7928639513982318 ) ) ;
#127586 = CARTESIAN_POINT ( 'NONE',  ( 23.14999999999999858, 5.000000000011153745, -146.4052660189131245 ) ) ;
#127587 = ADVANCED_FACE ( 'NONE', ( #87581 ), #126730, .T. ) ;
#127589 = ORIENTED_EDGE ( 'NONE', *, *, #213553, .T. ) ;
#127588 = AXIS2_PLACEMENT_3D ( 'NONE', #166795, #202040, #65090 ) ;
#127590 = DIRECTION ( 'NONE',  ( 0.000000000000000000, 0.2128009952263602844, -0.9770955615653315052 ) ) ;
#127591 = CARTESIAN_POINT ( 'NONE',  ( 23.14999999999999503, 64.35000000001156195, -57.37310748452439668 ) ) ;
#127592 = AXIS2_PLACEMENT_3D ( 'NONE', #126219, #31017, #87079 ) ;
#127593 = CIRCLE ( 'NONE', #60934, 0.09999999999999939493 ) ;
#127594 = LINE ( 'NONE', #46753, #239551 ) ;
#127595 = SPHERICAL_SURFACE ( 'NONE', #142165, 0.1000000000000000056 ) ;
#127596 = DIRECTION ( 'NONE',  ( 0.000000000000000000, 0.2617529984164915779, 0.9651348961777187485 ) ) ;
#127597 = DIRECTION ( 'NONE',  ( 0.000000000000000000, 0.000000000000000000, 1.000000000000000000 ) ) ;
#127598 = AXIS2_PLACEMENT_3D ( 'NONE', #101769, #138341, #120128 ) ;
#127599 = ORIENTED_EDGE ( 'NONE', *, *, #94339, .F. ) ;
#127600 = ORIENTED_EDGE ( 'NONE', *, *, #60887, .F. ) ;
#127601 = CARTESIAN_POINT ( 'NONE',  ( -20.85000000000000142, 7.070967871798842452, -37.24656422186831151 ) ) ;
#127602 = DIRECTION ( 'NONE',  ( -1.000000000000000000, -0.000000000000000000, 0.000000000000000000 ) ) ;
#127603 = LINE ( 'NONE', #123757, #104886 ) ;
#127605 = EDGE_CURVE ( 'NONE', #225270, #110468, #236348, .T. ) ;
#127604 = LINE ( 'NONE', #50609, #239241 ) ;
#127606 = CARTESIAN_POINT ( 'NONE',  ( 18.49999999999999645, 77.36242903720467723, -28.13422623660311217 ) ) ;
#127607 = ADVANCED_FACE ( 'NONE', ( #148876 ), #153000, .T. ) ;
#127608 = AXIS2_PLACEMENT_3D ( 'NONE', #188444, #223702, #86757 ) ;
#127609 = ORIENTED_EDGE ( 'NONE', *, *, #11767, .T. ) ;
#127610 = PLANE ( 'NONE',  #243013 ) ;
#127611 = ITEM_DEFINED_TRANSFORMATION ( 'NONE', 'NONE', #244390,  #2425 ) ;
#127612 = AXIS2_PLACEMENT_3D ( 'NONE', #235341, #56680, #136222 ) ;
#127613 = DIRECTION ( 'NONE',  ( -0.000000000000000000, -0.4856429311786292224, -0.8741572761215394838 ) ) ;
#127614 = VERTEX_POINT ( 'NONE', #206269 ) ;
#127615 = LINE ( 'NONE', #29827, #216939 ) ;
#127616 = EDGE_CURVE ( 'NONE', #51112, #125620, #150164, .T. ) ;
#127617 = ORIENTED_EDGE ( 'NONE', *, *, #75278, .F. ) ;
#127618 = VERTEX_POINT ( 'NONE', #25092 ) ;
#127619 = CIRCLE ( 'NONE', #165021, 0.09999999999999817368 ) ;
#127620 = ORIENTED_EDGE ( 'NONE', *, *, #161860, .T. ) ;
#127621 = CARTESIAN_POINT ( 'NONE',  ( 20.95595624212412744, 10.62389120310530544, -74.62963291412694389 ) ) ;
#127622 = PLANE ( 'NONE',  #9001 ) ;
#127623 = CARTESIAN_POINT ( 'NONE',  ( 18.49999999999999289, 10.20857864377385127, -88.35000000000003695 ) ) ;
#127624 = DIRECTION ( 'NONE',  ( 0.000000000000000000, 0.1298341882519953583, 0.9915357197604862671 ) ) ;
#127625 = CARTESIAN_POINT ( 'NONE',  ( 21.05000000000000071, 67.17357026049543833, -195.1090527715807070 ) ) ;
#127626 = CARTESIAN_POINT ( 'NONE',  ( -23.15000000000000213, 71.65000000001199965, -115.3731074845243256 ) ) ;
#127627 = CARTESIAN_POINT ( 'NONE',  ( 18.59999999999999076, 10.92199707682457088, -220.3694341645321515 ) ) ;
#127628 = ADVANCED_FACE ( 'NONE', ( #207568 ), #27674, .F. ) ;
#127630 = DIRECTION ( 'NONE',  ( -0.000000000000000000, -0.8814952561688430555, 0.4721928772777344574 ) ) ;
#127629 = CARTESIAN_POINT ( 'NONE',  ( 21.14999999999999858, 52.64219947837469959, -255.2660483925003803 ) ) ;
#127631 = DIRECTION ( 'NONE',  ( -1.000000000000000000, -0.000000000000000000, -0.000000000000000000 ) ) ;
#127632 = DIRECTION ( 'NONE',  ( -0.7070776581708965169, -0.7071359030027827286, -0.000000000000000000 ) ) ;
#127633 = DIRECTION ( 'NONE',  ( 0.000000000000000000, 0.4721928772776973204, 0.8814952561688629284 ) ) ;
#127634 = DIRECTION ( 'NONE',  ( 1.000000000000000000, -0.000000000000000000, -0.000000000000000000 ) ) ;
#127635 = CIRCLE ( 'NONE', #44253, 4.049999999999998934 ) ;
#127636 = ORIENTED_EDGE ( 'NONE', *, *, #221831, .F. ) ;
#127637 = CIRCLE ( 'NONE', #227574, 0.09999999999999939493 ) ;
#127638 = ORIENTED_EDGE ( 'NONE', *, *, #229332, .F. ) ;
#127639 = VECTOR ( 'NONE', #124496, 999.9999999999998863 ) ;
#127640 = CYLINDRICAL_SURFACE ( 'NONE', #140025, 4.000000000000003553 ) ;
#127641 = CIRCLE ( 'NONE', #219199, 0.09999999999999939493 ) ;
#127642 = LINE ( 'NONE', #87203, #95350 ) ;
#127644 = CARTESIAN_POINT ( 'NONE',  ( -12.42749937872395627, 12.88570875296796459, -216.1309391439169758 ) ) ;
#127643 = DIRECTION ( 'NONE',  ( 1.476360405086644309E-16, -1.000000000000000000, 0.000000000000000000 ) ) ;
#127645 = DIRECTION ( 'NONE',  ( 0.000000000000000000, -0.9126074666063770380, -0.4088369013363281068 ) ) ;
#127646 = CARTESIAN_POINT ( 'NONE',  ( -21.44999999999999929, 68.85000000001222986, -148.8731074845244109 ) ) ;
#127647 = DIRECTION ( 'NONE',  ( 1.000000000000000000, 0.000000000000000000, 0.000000000000000000 ) ) ;
#127648 = VERTEX_POINT ( 'NONE', #108453 ) ;
#127649 = VERTEX_POINT ( 'NONE', #5468 ) ;
#127650 = ADVANCED_FACE ( 'NONE', ( #164583 ), #40569, .F. ) ;
#127651 = DIRECTION ( 'NONE',  ( 0.000000000000000000, 0.9126074666063791474, 0.4088369013363231663 ) ) ;
#127652 = CIRCLE ( 'NONE', #111076, 0.1000000000000066530 ) ;
#127653 = EDGE_LOOP ( 'NONE', ( #151346, #214750, #17129, #177435 ) ) ;
#127654 = DIRECTION ( 'NONE',  ( -1.000000000000000000, 0.000000000000000000, 0.000000000000000000 ) ) ;
#127655 = AXIS2_PLACEMENT_3D ( 'NONE', #155171, #39059, #78147 ) ;
#127656 = AXIS2_PLACEMENT_3D ( 'NONE', #238681, #140872, #22220 ) ;
#127657 = B_SPLINE_CURVE_WITH_KNOTS ( 'NONE', 3,
 ( #220359, #102944, #144645, #83371, #245044, #125115, #45561 ),
 .UNSPECIFIED., .F., .F.,
 ( 4, 3, 4 ),
 ( 0.000000000000000000, 0.0009834301579439998740, 0.001767853679402675614 ),
 .UNSPECIFIED. ) ;
#127658 = LINE ( 'NONE', #28611, #138086 ) ;
#127659 = EDGE_CURVE ( 'NONE', #4296, #256132, #247950, .T. ) ;
#127660 = AXIS2_PLACEMENT_3D ( 'NONE', #115161, #151747, #13502 ) ;
#127661 = EDGE_CURVE ( 'NONE', #241817, #63155, #244100, .T. ) ;
#127662 = ORIENTED_EDGE ( 'NONE', *, *, #232940, .T. ) ;
#127663 = DIRECTION ( 'NONE',  ( -0.000000000000000000, -0.2617529984165031243, -0.9651348961777157509 ) ) ;
#127664 = VERTEX_POINT ( 'NONE', #65466 ) ;
#127665 = EDGE_CURVE ( 'NONE', #199002, #14594, #194692, .T. ) ;
#127667 = EDGE_CURVE ( 'NONE', #9341, #219647, #251807, .T. ) ;
#127666 = DIRECTION ( 'NONE',  ( 0.000000000000000000, -0.2617529984164506107, -0.9651348961777299618 ) ) ;
#127668 = LINE ( 'NONE', #151079, #141112 ) ;
#127669 = CARTESIAN_POINT ( 'NONE',  ( -17.11825945287482753, 10.05000000001113847, -146.6500000000000341 ) ) ;
#127670 = DIRECTION ( 'NONE',  ( 1.000000000000000000, -0.000000000000000000, -0.000000000000000000 ) ) ;
#127671 = DIRECTION ( 'NONE',  ( 1.186688945009009831E-16, 0.9651348961777157509, -0.2617529984165031243 ) ) ;
#127672 = CARTESIAN_POINT ( 'NONE',  ( -22.00356870068980442, 1.356251047821719177E-11, -59.74575763824462626 ) ) ;
#127673 = EDGE_CURVE ( 'NONE', #139380, #145808, #11509, .T. ) ;
#127674 = CARTESIAN_POINT ( 'NONE',  ( -16.92507428761701505, 9.950000000011138823, -79.71339745962158929 ) ) ;
#127675 = CARTESIAN_POINT ( 'NONE',  ( -20.54999999999999716, 85.00000000001179501, -79.41707660717668205 ) ) ;
#127677 = EDGE_LOOP ( 'NONE', ( #5396, #225744, #22701, #197325, #54211, #236500, #1086, #158881, #254437, #230329, #98025, #161254, #179254, #193085, #50311, #35135 ) ) ;
#127676 = CARTESIAN_POINT ( 'NONE',  ( 18.54271179734046626, -0.8403326744508465840, -242.3672828657570051 ) ) ;
#127679 = CARTESIAN_POINT ( 'NONE',  ( -23.25000000000000000, 4.350000000011156054, -188.6499999999999488 ) ) ;
#127678 = CARTESIAN_POINT ( 'NONE',  ( -16.77828822459933633, 66.05377062495554696, -115.6857357354433162 ) ) ;
#127680 = ORIENTED_EDGE ( 'NONE', *, *, #224203, .T. ) ;
#127682 = ORIENTED_EDGE ( 'NONE', *, *, #196716, .F. ) ;
#127681 = CARTESIAN_POINT ( 'NONE',  ( -21.05000000000000071, 1.162701749949165642, -108.6000000000000227 ) ) ;
#127683 = ADVANCED_FACE ( 'NONE', ( #211405 ), #168254, .T. ) ;
#127684 = VECTOR ( 'NONE', #241035, 1000.000000000000000 ) ;
#127685 = VERTEX_POINT ( 'NONE', #112317 ) ;
#127686 = DIRECTION ( 'NONE',  ( 0.000000000000000000, 6.982962677686266711E-15, -1.000000000000000000 ) ) ;
#127688 = ADVANCED_FACE ( 'NONE', ( #114868 ), #116170, .T. ) ;
#127687 = EDGE_CURVE ( 'NONE', #73461, #199162, #210134, .T. ) ;
#127689 = CARTESIAN_POINT ( 'NONE',  ( 21.14999999999999858, 64.35000000001204512, -124.3731074845243825 ) ) ;
#127690 = CARTESIAN_POINT ( 'NONE',  ( -21.56666275994539816, 0.9959460939976478855, -230.4474815061071240 ) ) ;
#127691 = CARTESIAN_POINT ( 'NONE',  ( 22.50000000000000000, 25.98655542988603173, -254.2226763854395983 ) ) ;
#127693 = DIRECTION ( 'NONE',  ( 1.000000000000000000, 0.000000000000000000, -0.000000000000000000 ) ) ;
#127692 = AXIS2_PLACEMENT_3D ( 'NONE', #257385, #218295, #201324 ) ;
#127694 = DIRECTION ( 'NONE',  ( -1.000000000000000000, -7.125593699324843413E-30, 1.020425574104004196E-15 ) ) ;
#127695 = CARTESIAN_POINT ( 'NONE',  ( 18.59999999999999787, -1.835341550213255957, -112.0551512925630107 ) ) ;
#127696 = EDGE_CURVE ( 'NONE', #88936, #111063, #236041, .T. ) ;
#127697 = CARTESIAN_POINT ( 'NONE',  ( -20.94999999999999929, -1.360870587180885716, -175.5729979270909382 ) ) ;
#127698 = VERTEX_POINT ( 'NONE', #34088 ) ;
#127699 = ORIENTED_EDGE ( 'NONE', *, *, #163470, .F. ) ;
#127700 = CARTESIAN_POINT ( 'NONE',  ( 20.94999999999999929, 7.661991824395936845, -241.5144583139544636 ) ) ;
#127701 = ADVANCED_FACE ( 'NONE', ( #51007 ), #113585, .F. ) ;
#127702 = EDGE_CURVE ( 'NONE', #785, #149628, #36467, .T. ) ;
#127703 = AXIS2_PLACEMENT_3D ( 'NONE', #214917, #252750, #53287 ) ;
#127704 = ORIENTED_EDGE ( 'NONE', *, *, #40552, .T. ) ;
#127705 = DIRECTION ( 'NONE',  ( 1.000000000000000000, 0.000000000000000000, 0.000000000000000000 ) ) ;
#127706 = ORIENTED_EDGE ( 'NONE', *, *, #94036, .F. ) ;
#127707 = LINE ( 'NONE', #28652, #242596 ) ;
#127708 = AXIS2_PLACEMENT_3D ( 'NONE', #246561, #44533, #87482 ) ;
#127709 = EDGE_CURVE ( 'NONE', #216121, #221539, #74503, .T. ) ;
#127710 = CARTESIAN_POINT ( 'NONE',  ( 20.94999999999999929, 4.813084112160680661, -179.4415177565237798 ) ) ;
#127711 = DIRECTION ( 'NONE',  ( -0.000000000000000000, -0.000000000000000000, 1.000000000000000000 ) ) ;
#127712 = DIRECTION ( 'NONE',  ( 1.000000000000000000, 0.000000000000000000, 0.000000000000000000 ) ) ;
#127713 = DIRECTION ( 'NONE',  ( 0.000000000000000000, 3.469446951953605354E-14, -1.000000000000000000 ) ) ;
#127714 = ORIENTED_EDGE ( 'NONE', *, *, #111307, .T. ) ;
#127715 = EDGE_CURVE ( 'NONE', #67166, #119072, #217793, .T. ) ;
#127716 = DIRECTION ( 'NONE',  ( 1.000000000000000000, 0.000000000000000000, 0.000000000000000000 ) ) ;
#127717 = DIRECTION ( 'NONE',  ( -1.000000000000000000, -2.952720810173289112E-16, 0.000000000000000000 ) ) ;
#127718 = CARTESIAN_POINT ( 'NONE',  ( 18.49999999999998224, 85.32100840337292880, -62.28716923544642015 ) ) ;
#127719 = DIRECTION ( 'NONE',  ( 1.000000000000000000, 0.000000000000000000, 0.000000000000000000 ) ) ;
#127720 = ORIENTED_EDGE ( 'NONE', *, *, #221891, .T. ) ;
#127722 = DIRECTION ( 'NONE',  ( 1.000000000000000000, 0.000000000000000000, 0.000000000000000000 ) ) ;
#127721 = DIRECTION ( 'NONE',  ( 0.000000000000000000, -1.000000000000000000, 0.000000000000000000 ) ) ;
#127723 = CIRCLE ( 'NONE', #236038, 4.099999999999998757 ) ;
#127724 = ORIENTED_EDGE ( 'NONE', *, *, #254983, .F. ) ;
#127727 = ORIENTED_EDGE ( 'NONE', *, *, #51988, .F. ) ;
#127726 = CARTESIAN_POINT ( 'NONE',  ( -16.77683809663752257, 51.60783545504968117, -231.9559722212415522 ) ) ;
#127725 = PRESENTATION_STYLE_ASSIGNMENT (( #45615 ) ) ;
#127728 = ORIENTED_EDGE ( 'NONE', *, *, #185169, .F. ) ;
#127729 = CARTESIAN_POINT ( 'NONE',  ( 21.14999999999999858, 11.75000000001116263, -21.75000000000000355 ) ) ;
#127730 = CIRCLE ( 'NONE', #136055, 0.1000000000000054040 ) ;
#127731 = CARTESIAN_POINT ( 'NONE',  ( -20.54999999999999716, 7.150000000011155876, -179.8499999999999943 ) ) ;
#127732 = CIRCLE ( 'NONE', #174117, 0.09999999999999939493 ) ;
#127733 = DIRECTION ( 'NONE',  ( 0.000000000000000000, 0.000000000000000000, -1.000000000000000000 ) ) ;
#127734 = VERTEX_POINT ( 'NONE', #178733 ) ;
#127735 = DIRECTION ( 'NONE',  ( 0.000000000000000000, -1.000000000000000000, -8.717686153663073805E-15 ) ) ;
#127736 = CIRCLE ( 'NONE', #156962, 0.1000000000000055844 ) ;
#127737 = CYLINDRICAL_SURFACE ( 'NONE', #65536, 0.1000000000000028644 ) ;
#127738 = AXIS2_PLACEMENT_3D ( 'NONE', #82756, #236720, #58075 ) ;
#127740 = DIRECTION ( 'NONE',  ( 0.000000000000000000, -0.2128009952263636428, 0.9770955615653308390 ) ) ;
#127739 = DIRECTION ( 'NONE',  ( -0.7071067811865389130, -0.1504730267678074107, 0.6909108974501321221 ) ) ;
#127741 = AXIS2_PLACEMENT_3D ( 'NONE', #112740, #210556, #71064 ) ;
#127743 = ORIENTED_EDGE ( 'NONE', *, *, #146712, .T. ) ;
#127742 = CARTESIAN_POINT ( 'NONE',  ( 20.85000000106584750, 11.75000000001115907, -93.65550465647376654 ) ) ;
#127744 = ORIENTED_EDGE ( 'NONE', *, *, #137287, .T. ) ;
#127745 = CARTESIAN_POINT ( 'NONE',  ( -16.88219499860498374, 9.950206425438743452, -79.64930969010735851 ) ) ;
#127746 = CARTESIAN_POINT ( 'NONE',  ( 15.74999999999999645, 9.349999999999983658, -16.75000000000000000 ) ) ;
#127747 = VECTOR ( 'NONE', #21352, 1000.000000000000000 ) ;
#127748 = LINE ( 'NONE', #6495, #22248 ) ;
#127749 = ORIENTED_EDGE ( 'NONE', *, *, #48944, .T. ) ;
#127751 = CIRCLE ( 'NONE', #244433, 0.1000000000000003803 ) ;
#127750 = FACE_OUTER_BOUND ( 'NONE', #229453, .T. ) ;
#127752 = AXIS2_PLACEMENT_3D ( 'NONE', #188256, #89146, #168751 ) ;
#127753 = CARTESIAN_POINT ( 'NONE',  ( -18.40000000000000213, 20.94763808724815846, -234.7254930126486556 ) ) ;
#127754 = DIRECTION ( 'NONE',  ( -1.000000000000000000, 1.836970198721029934E-16, 1.282749433769087582E-30 ) ) ;
#127755 = ORIENTED_EDGE ( 'NONE', *, *, #219239, .T. ) ;
#127756 = CARTESIAN_POINT ( 'NONE',  ( 20.90000000000000213, 0.000000000000000000, 0.000000000000000000 ) ) ;
#127757 = EDGE_CURVE ( 'NONE', #200243, #60057, #128022, .T. ) ;
#127758 = VECTOR ( 'NONE', #197687, 1000.000000000000000 ) ;
#127759 = EDGE_LOOP ( 'NONE', ( #193756, #92756, #164860, #175280 ) ) ;
#127760 = DIRECTION ( 'NONE',  ( 0.000000000000000000, 1.000000000000000000, 0.000000000000000000 ) ) ;
#127761 = EDGE_CURVE ( 'NONE', #88245, #224443, #256953, .T. ) ;
#127762 = VERTEX_POINT ( 'NONE', #179993 ) ;
#127763 = ORIENTED_EDGE ( 'NONE', *, *, #255989, .T. ) ;
#127764 = EDGE_CURVE ( 'NONE', #209959, #210119, #237389, .T. ) ;
#127765 = CYLINDRICAL_SURFACE ( 'NONE', #149899, 0.09999999999999990841 ) ;
#127766 = VERTEX_POINT ( 'NONE', #121331 ) ;
#127769 = EDGE_CURVE ( 'NONE', #113334, #138262, #57446, .T. ) ;
#127768 = ORIENTED_EDGE ( 'NONE', *, *, #8973, .T. ) ;
#127767 = CARTESIAN_POINT ( 'NONE',  ( 22.59999999999999432, 25.89494711235934687, -254.2627752153468350 ) ) ;
#127770 = ORIENTED_EDGE ( 'NONE', *, *, #223980, .F. ) ;
#127771 = AXIS2_PLACEMENT_3D ( 'NONE', #173977, #73571, #153122 ) ;
#127772 = AXIS2_PLACEMENT_3D ( 'NONE', #30603, #149265, #107536 ) ;
#127774 = ORIENTED_EDGE ( 'NONE', *, *, #7795, .F. ) ;
#127773 = ORIENTED_EDGE ( 'NONE', *, *, #157477, .F. ) ;
#127775 = CIRCLE ( 'NONE', #98488, 0.09999999999999817368 ) ;
#127776 = CARTESIAN_POINT ( 'NONE',  ( -18.59999994787167310, -9.523637689750348301, -107.3824495347726753 ) ) ;
#127777 = ORIENTED_EDGE ( 'NONE', *, *, #151310, .F. ) ;
#127778 = DIRECTION ( 'NONE',  ( 0.000000000000000000, -0.2128009952263604232, 0.9770955615653316162 ) ) ;
#127779 = DIRECTION ( 'NONE',  ( -1.000000000000000000, -0.000000000000000000, 0.000000000000000000 ) ) ;
#127780 = CARTESIAN_POINT ( 'NONE',  ( 23.14999999999999503, 62.92003201576280702, -207.2439188921395612 ) ) ;
#127781 = VECTOR ( 'NONE', #224318, 1000.000000000000000 ) ;
#127782 = ADVANCED_FACE ( 'NONE', ( #61319 ), #133186, .T. ) ;
#127783 = CARTESIAN_POINT ( 'NONE',  ( -18.69999999999999929, -10.80884033489985363, 6.100000000000002309 ) ) ;
#127784 = ADVANCED_FACE ( 'NONE', ( #182567 ), #120038, .T. ) ;
#127785 = VERTEX_POINT ( 'NONE', #18336 ) ;
#127786 = VERTEX_POINT ( 'NONE', #181286 ) ;
#127787 = CARTESIAN_POINT ( 'NONE',  ( -23.15000000000000213, 82.09643798151613225, -215.4278993322501208 ) ) ;
#127788 =( BOUNDED_CURVE ( )  B_SPLINE_CURVE ( 3, ( #227967, #108025, #49323, #208427 ),
 .UNSPECIFIED., .F., .F. ) 
 B_SPLINE_CURVE_WITH_KNOTS ( ( 4, 4 ),
 ( 0.000000000000000000, 1.570796326794896558 ),
 .UNSPECIFIED. ) 
 CURVE ( )  GEOMETRIC_REPRESENTATION_ITEM ( )  RATIONAL_B_SPLINE_CURVE ( ( 1.000000000000000000, 0.8047378541243649375, 0.8047378541243649375, 1.000000000000000000 ) ) 
 REPRESENTATION_ITEM ( '' )  );
#127790 = ORIENTED_EDGE ( 'NONE', *, *, #232254, .F. ) ;
#127789 = DIRECTION ( 'NONE',  ( -1.000000000000000000, 0.000000000000000000, 0.000000000000000000 ) ) ;
#127791 = CARTESIAN_POINT ( 'NONE',  ( -12.25000000000000178, 13.18880795147152440, -215.2702608532411830 ) ) ;
#127793 = ORIENTED_EDGE ( 'NONE', *, *, #46404, .T. ) ;
#127792 = CARTESIAN_POINT ( 'NONE',  ( -20.64999999999999858, 76.00000000001213607, -136.5231074845242745 ) ) ;
#127794 = AXIS2_PLACEMENT_3D ( 'NONE', #66908, #146426, #108605 ) ;
#127795 = VERTEX_POINT ( 'NONE', #239963 ) ;
#127796 = DIRECTION ( 'NONE',  ( 2.342056488767301376E-15, -0.1350103645451904977, -0.9908441862701596881 ) ) ;
#127797 = AXIS2_PLACEMENT_3D ( 'NONE', #145886, #125065, #84593 ) ;
#127798 = EDGE_CURVE ( 'NONE', #223140, #77481, #65463, .T. ) ;
#127799 = VERTEX_POINT ( 'NONE', #41779 ) ;
#127800 = FACE_OUTER_BOUND ( 'NONE', #164757, .T. ) ;
#127801 = CARTESIAN_POINT ( 'NONE',  ( 18.59999999999999432, 0.7653315920341953182, -212.6731560895497353 ) ) ;
#127802 = ADVANCED_FACE ( 'NONE', ( #101688 ), #221650, .F. ) ;
#127804 = ORIENTED_EDGE ( 'NONE', *, *, #129387, .T. ) ;
#127803 = EDGE_LOOP ( 'NONE', ( #122340, #70989, #199679, #107602 ) ) ;
#127805 = VERTEX_POINT ( 'NONE', #37925 ) ;
#127806 = CARTESIAN_POINT ( 'NONE',  ( 21.05000000000000071, 6.540656951712400691, -33.60000000000000142 ) ) ;
#127807 = ORIENTED_EDGE ( 'NONE', *, *, #226988, .F. ) ;
#127808 = ORIENTED_EDGE ( 'NONE', *, *, #89703, .F. ) ;
#127809 = DIRECTION ( 'NONE',  ( 0.000000000000000000, 0.5868805631290353597, 0.8096735173027127530 ) ) ;
#127811 = ORIENTED_EDGE ( 'NONE', *, *, #172973, .F. ) ;
#127810 = CARTESIAN_POINT ( 'NONE',  ( -21.05000000000000071, 11.65000000001115232, -107.2838656629781724 ) ) ;
#127812 = DIRECTION ( 'NONE',  ( 1.000000000000000000, 0.000000000000000000, -0.000000000000000000 ) ) ;
#127814 = DIRECTION ( 'NONE',  ( 0.000000000000000000, -0.8660254037844383745, 0.5000000000000003331 ) ) ;
#127813 = CARTESIAN_POINT ( 'NONE',  ( 20.94999999999997442, 77.26327546522911405, -95.12124281777788326 ) ) ;
#127815 = EDGE_CURVE ( 'NONE', #109487, #166243, #161727, .T. ) ;
#127816 = DIRECTION ( 'NONE',  ( 0.000000000000000000, 0.000000000000000000, 1.000000000000000000 ) ) ;
#127817 = CARTESIAN_POINT ( 'NONE',  ( -13.43673303185029511, 62.06361769656464134, -218.8193597571736575 ) ) ;
#127818 = ORIENTED_EDGE ( 'NONE', *, *, #173443, .F. ) ;
#127819 = EDGE_CURVE ( 'NONE', #190151, #70987, #117326, .T. ) ;
#127820 = ORIENTED_EDGE ( 'NONE', *, *, #19690, .F. ) ;
#127821 = FACE_BOUND ( 'NONE', #152085, .T. ) ;
#127823 = ADVANCED_FACE ( 'NONE', ( #6466 ), #194877, .T. ) ;
#127822 = ORIENTED_EDGE ( 'NONE', *, *, #66796, .F. ) ;
#127824 = AXIS2_PLACEMENT_3D ( 'NONE', #152938, #134596, #215439 ) ;
#127825 = TOROIDAL_SURFACE ( 'NONE', #81990, 11.70000000000000639, 0.1000000000000000056 ) ;
#127826 = AXIS2_PLACEMENT_3D ( 'NONE', #225003, #242019, #221162 ) ;
#127827 = ADVANCED_FACE ( 'NONE', ( #44331 ), #123871, .T. ) ;
#127828 = CARTESIAN_POINT ( 'NONE',  ( 20.94999999999999929, -6.438379425586758131, -212.1495692908769684 ) ) ;
#127829 = EDGE_LOOP ( 'NONE', ( #75819, #217827, #140312 ) ) ;
#127830 = ORIENTED_EDGE ( 'NONE', *, *, #216867, .T. ) ;
#127831 = CARTESIAN_POINT ( 'NONE',  ( -20.97625342178413277, 64.39999999919218965, -196.5949042547225645 ) ) ;
#127832 = CARTESIAN_POINT ( 'NONE',  ( -18.40000000000000213, 64.51332499825441857, -127.2731074845243882 ) ) ;
#127833 = ORIENTED_EDGE ( 'NONE', *, *, #165990, .T. ) ;
#127834 = FACE_OUTER_BOUND ( 'NONE', #65598, .T. ) ;
#127835 = CARTESIAN_POINT ( 'NONE',  ( 21.04999999999908411, 8.776282895301829257, -112.6579090026525307 ) ) ;
#127836 = VERTEX_POINT ( 'NONE', #45608 ) ;
#127837 = EDGE_CURVE ( 'NONE', #171058, #118840, #88558, .T. ) ;
#127838 = DIRECTION ( 'NONE',  ( 0.000000000000000000, -0.1332476588733448597, 0.9910827722268067408 ) ) ;
#127839 = CARTESIAN_POINT ( 'NONE',  ( -22.39999999999999858, 29.50811709945089945, -252.6450601445781103 ) ) ;
#127841 = CARTESIAN_POINT ( 'NONE',  ( -21.04999999999999361, 6.307425219576558995, -67.01681986838568150 ) ) ;
#127840 = DIRECTION ( 'NONE',  ( 0.000000000000000000, 0.8814952561688444987, -0.4721928772777320149 ) ) ;
#127842 = DIRECTION ( 'NONE',  ( -2.489438768765008884E-17, 0.1686199900910312910, -0.9856811345164826488 ) ) ;
#127843 = CARTESIAN_POINT ( 'NONE',  ( -21.05000000000000071, 9.685169582982728897, -235.1020606565447224 ) ) ;
#127844 = DIRECTION ( 'NONE',  ( 1.000000000000000000, 0.000000000000000000, 0.000000000000000000 ) ) ;
#127846 = EDGE_CURVE ( 'NONE', #152028, #154736, #87276, .T. ) ;
#127845 = FACE_OUTER_BOUND ( 'NONE', #125518, .T. ) ;
#127847 = CIRCLE ( 'NONE', #48713, 2.000000000000001776 ) ;
#127848 = AXIS2_PLACEMENT_3D ( 'NONE', #214792, #176988, #76564 ) ;
#127849 = AXIS2_PLACEMENT_3D ( 'NONE', #109423, #169457, #106857 ) ;
#127850 = ORIENTED_EDGE ( 'NONE', *, *, #53549, .T. ) ;
#127852 = ORIENTED_EDGE ( 'NONE', *, *, #66796, .T. ) ;
#127851 = ORIENTED_EDGE ( 'NONE', *, *, #205510, .T. ) ;
#127853 = AXIS2_PLACEMENT_3D ( 'NONE', #219718, #237996, #218421 ) ;
#127854 = VERTEX_POINT ( 'NONE', #49458 ) ;
#127856 = ADVANCED_FACE ( 'NONE', ( #166873 ), #129002, .F. ) ;
#127855 = CARTESIAN_POINT ( 'NONE',  ( 23.14999999999999147, 4.150000000011154988, -134.0000000000000000 ) ) ;
#127857 = LINE ( 'NONE', #33936, #28662 ) ;
#127858 =( BOUNDED_SURFACE ( )  B_SPLINE_SURFACE ( 3, 2, ( 
 ( #164274, #243793, #46857 ),
 ( #248943, #148555, #228095 ),
 ( #65146, #204650, #245077 ),
 ( #147257, #70328, #183818 ) ),
 .UNSPECIFIED., .F., .F., .F. ) 
 B_SPLINE_SURFACE_WITH_KNOTS ( ( 4, 4 ),
 ( 3, 3 ),
 ( 4.712388980384689674, 5.765869716888459173 ),
 ( 0.000000000000000000, 1.000000000000000000 ),
 .UNSPECIFIED. ) 
 GEOMETRIC_REPRESENTATION_ITEM ( )  RATIONAL_B_SPLINE_SURFACE ( (
 ( 1.000000000000000000, 0.7071067811864494290, 1.000000000000000000),
 ( 1.000000000000000000, 0.7953136715914208565, 1.000000000000000000),
 ( 1.000000000000000000, 0.8646876308614606099, 1.000000000000000000),
 ( 1.000000000000000000, 0.8984936768950610997, 1.000000000000000000) ) ) 
 REPRESENTATION_ITEM ( '' )  SURFACE ( )  );
#127860 = CARTESIAN_POINT ( 'NONE',  ( -22.59066674512253670, 11.75000000001115552, -33.46949587636949275 ) ) ;
#127859 = DIRECTION ( 'NONE',  ( 1.000000000000000000, 0.000000000000000000, 0.000000000000000000 ) ) ;
#127861 = ORIENTED_EDGE ( 'NONE', *, *, #40824, .T. ) ;
#127862 = CARTESIAN_POINT ( 'NONE',  ( -23.15000000000000213, 1.115600667400684642E-11, -33.50000000000000000 ) ) ;
#127863 = DIRECTION ( 'NONE',  ( 0.000000000000000000, 0.000000000000000000, -1.000000000000000000 ) ) ;
#127864 = CARTESIAN_POINT ( 'NONE',  ( -21.05000000000000071, 1.561467271655390121, -230.7743560730225454 ) ) ;
#127865 = ORIENTED_EDGE ( 'NONE', *, *, #250932, .F. ) ;
#127866 = AXIS2_PLACEMENT_3D ( 'NONE', #224668, #27803, #65600 ) ;
#127867 = FACE_OUTER_BOUND ( 'NONE', #218456, .T. ) ;
#127868 = DIRECTION ( 'NONE',  ( 0.000000000000000000, -5.270046002967521614E-15, 1.000000000000000000 ) ) ;
#127869 = EDGE_LOOP ( 'NONE', ( #206912, #33674, #69816, #59768 ) ) ;
#127870 = VERTEX_POINT ( 'NONE', #46867 ) ;
#127871 = CARTESIAN_POINT ( 'NONE',  ( -16.89146115310546037, 9.951443245667611848, -54.35482241895421396 ) ) ;
#127872 = CARTESIAN_POINT ( 'NONE',  ( -23.15000000000000213, 51.28888318656201761, -230.2315015618842153 ) ) ;
#127873 = CARTESIAN_POINT ( 'NONE',  ( -23.25000000000000000, 2.600000000011156054, -187.7753780772378889 ) ) ;
#127874 = DIRECTION ( 'NONE',  ( -1.000000000000000000, -0.000000000000000000, -0.000000000000000000 ) ) ;
#127875 = FACE_OUTER_BOUND ( 'NONE', #72138, .T. ) ;
#127876 = TOROIDAL_SURFACE ( 'NONE', #86139, 12.97499999999999609, 0.1000000000000000056 ) ;
#127877 = DIRECTION ( 'NONE',  ( 0.000000000000000000, -0.000000000000000000, -1.000000000000000000 ) ) ;
#127878 = ORIENTED_EDGE ( 'NONE', *, *, #123252, .F. ) ;
#127879 = DIRECTION ( 'NONE',  ( 0.000000000000000000, 0.000000000000000000, 1.000000000000000000 ) ) ;
#127880 = LINE ( 'NONE', #48331, #220762 ) ;
#127882 = CYLINDRICAL_SURFACE ( 'NONE', #195652, 0.09999999999999939493 ) ;
#127881 = CARTESIAN_POINT ( 'NONE',  ( -16.93262454970419384, 10.00202046794151478, -87.92707622623736086 ) ) ;
#127883 = CARTESIAN_POINT ( 'NONE',  ( -21.05000000000000071, -1.835341550213255957, -112.1551512925630050 ) ) ;
#127885 = VECTOR ( 'NONE', #82694, 1000.000000000000000 ) ;
#127884 = B_SPLINE_CURVE_WITH_KNOTS ( 'NONE', 3,
 ( #163485, #141350, #123084, #100891, #142613, #42260, #183060, #201321, #22717, #3100, #83898, #82623, #243008, #64389, #223440, #44821, #70833, #249456, #166087, #49946, #86481, #89068 ),
 .UNSPECIFIED., .F., .F.,
 ( 4, 3, 3, 3, 3, 3, 3, 4 ),
 ( 0.000000000000000000, 7.307836821083771763E-06, 4.161455748548197731E-05, 7.576591810646988155E-05, 0.0001098090429817560448, 0.0001438003617351108854, 0.0001777914035423656264, 0.0002117966137403014628 ),
 .UNSPECIFIED. ) ;
#127886 = DIRECTION ( 'NONE',  ( 1.000000000000000000, 0.000000000000000000, 0.000000000000000000 ) ) ;
#127887 = DIRECTION ( 'NONE',  ( 0.000000000000000000, 0.9126074666063774821, 0.4088369013363268301 ) ) ;
#127888 = CARTESIAN_POINT ( 'NONE',  ( 18.45139536634708932, -9.486081720270037820, -207.6405116178106312 ) ) ;
#127889 = VECTOR ( 'NONE', #38865, 1000.000000000000000 ) ;
#127891 = ORIENTED_EDGE ( 'NONE', *, *, #243669, .T. ) ;
#127890 = DIRECTION ( 'NONE',  ( 1.000000000000000000, 1.476360405086655403E-16, 0.000000000000000000 ) ) ;
#127892 =( BOUNDED_SURFACE ( )  B_SPLINE_SURFACE ( 3, 2, ( 
 ( #206858, #66056, #145587 ),
 ( #43932, #123472, #245993 ),
 ( #146859, #223833, #186010 ),
 ( #67349, #105139, #203001 ) ),
 .UNSPECIFIED., .F., .F., .F. ) 
 B_SPLINE_SURFACE_WITH_KNOTS ( ( 4, 4 ),
 ( 3, 3 ),
 ( 0.0002700421466196765378, 0.0004789321604330627779 ),
 ( 0.000000000000000000, 1.000000000000000000 ),
 .UNSPECIFIED. ) 
 GEOMETRIC_REPRESENTATION_ITEM ( )  RATIONAL_B_SPLINE_SURFACE ( (
 ( 1.000000000000000000, 0.7071067811865475727, 1.000000000000000000),
 ( 1.000000000000000000, 0.7163411249511861811, 1.000000000000000000),
 ( 1.000000000000000000, 0.7221957104841836284, 1.000000000000000000),
 ( 1.000000000000000000, 0.7250110520819876836, 1.000000000000000000) ) ) 
 REPRESENTATION_ITEM ( '' )  SURFACE ( )  );
#127893 = DIRECTION ( 'NONE',  ( -1.000000000000000000, 0.000000000000000000, 0.000000000000000000 ) ) ;
#127894 = CIRCLE ( 'NONE', #86159, 0.1000000000000106498 ) ;
#127895 = CIRCLE ( 'NONE', #19566, 0.1000000000000070832 ) ;
#127896 = EDGE_CURVE ( 'NONE', #186298, #150427, #244519, .T. ) ;
#127897 = EDGE_CURVE ( 'NONE', #186134, #28381, #84686, .T. ) ;
#127898 = EDGE_CURVE ( 'NONE', #218531, #19219, #19695, .T. ) ;
#127899 = CARTESIAN_POINT ( 'NONE',  ( 21.30000000000002558, 0.000000000000000000, 0.000000000000000000 ) ) ;
#127900 = CARTESIAN_POINT ( 'NONE',  ( -18.59999999999999787, 45.93315328338058379, -256.6017782078560003 ) ) ;
#127901 = AXIS2_PLACEMENT_3D ( 'NONE', #71822, #131775, #210050 ) ;
#127902 = ORIENTED_EDGE ( 'NONE', *, *, #123495, .F. ) ;
#127903 = DIRECTION ( 'NONE',  ( 0.000000000000000000, 0.000000000000000000, -1.000000000000000000 ) ) ;
#127904 = TOROIDAL_SURFACE ( 'NONE', #36341, 11.65000000000000036, 0.1000000000000000056 ) ;
#127905 = DIRECTION ( 'NONE',  ( 1.000000000000000000, 0.000000000000000000, 0.000000000000000000 ) ) ;
#127906 = CARTESIAN_POINT ( 'NONE',  ( -23.15000000000000213, 87.65000000001214175, -136.5231074845242176 ) ) ;
#127907 = AXIS2_PLACEMENT_3D ( 'NONE', #240124, #44496, #141025 ) ;
#127908 = ORIENTED_EDGE ( 'NONE', *, *, #122873, .F. ) ;
#127909 = LINE ( 'NONE', #66651, #258054 ) ;
#127912 = ORIENTED_EDGE ( 'NONE', *, *, #69114, .F. ) ;
#127911 = CARTESIAN_POINT ( 'NONE',  ( -16.88783316861808714, 9.950000000011137047, -188.2477359580206837 ) ) ;
#127910 = VECTOR ( 'NONE', #244104, 1000.000000000000000 ) ;
#127913 = DIRECTION ( 'NONE',  ( 0.000000000000000000, 0.000000000000000000, -1.000000000000000000 ) ) ;
#127914 = EDGE_CURVE ( 'NONE', #216222, #216494, #7183, .T. ) ;
#127915 = AXIS2_PLACEMENT_3D ( 'NONE', #202131, #3931, #183846 ) ;
#127917 = ORIENTED_EDGE ( 'NONE', *, *, #6457, .F. ) ;
#127916 = AXIS2_PLACEMENT_3D ( 'NONE', #143840, #185553, #25215 ) ;
#127918 = CARTESIAN_POINT ( 'NONE',  ( -16.87683809663752754, 66.13411015068207632, -190.2556806774549898 ) ) ;
#127919 = DIRECTION ( 'NONE',  ( 1.000000000000000000, 0.000000000000000000, 0.000000000000000000 ) ) ;
#127920 = DIRECTION ( 'NONE',  ( -1.000000000000000000, 0.000000000000000000, 0.000000000000000000 ) ) ;
#127921 = FACE_OUTER_BOUND ( 'NONE', #231812, .T. ) ;
#127922 = CARTESIAN_POINT ( 'NONE',  ( 22.48660254037844197, 64.35000000001164722, -69.57310748452439952 ) ) ;
#127923 = VERTEX_POINT ( 'NONE', #251495 ) ;
#127924 = DIRECTION ( 'NONE',  ( 1.000000000000000000, -1.186688945009009831E-16, -8.286604613020806758E-31 ) ) ;
#127925 = LINE ( 'NONE', #105755, #200698 ) ;
#127926 = AXIS2_PLACEMENT_3D ( 'NONE', #44455, #60132, #203517 ) ;
#127927 = CARTESIAN_POINT ( 'NONE',  ( -20.94999999999999929, 7.128833340094563376, -233.7327013124401276 ) ) ;
#127928 = EDGE_CURVE ( 'NONE', #54863, #18309, #167241, .T. ) ;
#127929 = ORIENTED_EDGE ( 'NONE', *, *, #232990, .T. ) ;
#127930 = EDGE_CURVE ( 'NONE', #114917, #15410, #198735, .T. ) ;
#127931 = EDGE_LOOP ( 'NONE', ( #94976, #87348, #113491, #205309, #19178, #25253, #27601, #31558, #214023, #62795, #256940, #184536 ) ) ;
#127932 = DIRECTION ( 'NONE',  ( 0.000000000000000000, 1.000000000000000000, 6.608470384673536824E-15 ) ) ;
#127933 = DIRECTION ( 'NONE',  ( -0.000000000000000000, 1.000000000000000000, -1.224646799147352961E-16 ) ) ;
#127934 = CARTESIAN_POINT ( 'NONE',  ( 21.05000000000000071, 70.15000000001163016, -59.39061026024639744 ) ) ;
#127935 = CARTESIAN_POINT ( 'NONE',  ( -18.50000000000000000, 8.006782298343173565, -209.8034900594678618 ) ) ;
#127936 = CARTESIAN_POINT ( 'NONE',  ( -20.64999999999999858, 2.000000000011154189, -188.2753780772378889 ) ) ;
#127937 = EDGE_CURVE ( 'NONE', #249899, #214183, #53310, .T. ) ;
#127939 = LINE ( 'NONE', #133074, #228423 ) ;
#127938 = FACE_OUTER_BOUND ( 'NONE', #66081, .T. ) ;
#127940 = CARTESIAN_POINT ( 'NONE',  ( 21.14999999999999858, 13.09610049681062982, -210.7873096111272844 ) ) ;
#127941 = FACE_OUTER_BOUND ( 'NONE', #65058, .T. ) ;
#127942 = DIRECTION ( 'NONE',  ( -1.000000000000000000, 0.000000000000000000, -0.000000000000000000 ) ) ;
#127943 = CARTESIAN_POINT ( 'NONE',  ( 13.99999999999999822, 9.850000000011137402, -150.7500000000000284 ) ) ;
#127945 = ORIENTED_EDGE ( 'NONE', *, *, #239400, .T. ) ;
#127944 = FACE_OUTER_BOUND ( 'NONE', #258081, .T. ) ;
#127946 = CARTESIAN_POINT ( 'NONE',  ( -20.90000000000000213, 1.800000000000000044, -11.61130914238355771 ) ) ;
#127947 = LINE ( 'NONE', #187926, #228276 ) ;
#127949 = FACE_OUTER_BOUND ( 'NONE', #21923, .T. ) ;
#127948 = CARTESIAN_POINT ( 'NONE',  ( 18.59999999999999076, 74.25000000001156764, -57.85359592662268824 ) ) ;
#127950 = CIRCLE ( 'NONE', #98667, 0.09999999999999741040 ) ;
#127951 = ORIENTED_EDGE ( 'NONE', *, *, #167239, .F. ) ;
#127952 = DIRECTION ( 'NONE',  ( 1.000000000000000000, -1.335000415235278971E-16, 2.979993593738921214E-16 ) ) ;
#127953 = CARTESIAN_POINT ( 'NONE',  ( -23.15000000000000213, 1.115600667400684642E-11, -67.00000000000000000 ) ) ;
#127954 = DIRECTION ( 'NONE',  ( 0.000000000000000000, 0.000000000000000000, 1.000000000000000000 ) ) ;
#127955 = DIRECTION ( 'NONE',  ( -0.000000000000000000, 1.000000000000000000, 6.982962677686266711E-15 ) ) ;
#127956 = EDGE_LOOP ( 'NONE', ( #97077, #129383, #9961, #86317 ) ) ;
#127957 = AXIS2_PLACEMENT_3D ( 'NONE', #165944, #45965, #153787 ) ;
#127958 = ORIENTED_EDGE ( 'NONE', *, *, #12329, .T. ) ;
#127959 = CIRCLE ( 'NONE', #57179, 0.09999999999999510669 ) ;
#127960 = ADVANCED_FACE ( 'NONE', ( #114567 ), #174600, .F. ) ;
#127961 = VECTOR ( 'NONE', #32665, 999.9999999999998863 ) ;
#127962 = AXIS2_PLACEMENT_3D ( 'NONE', #38711, #175659, #21714 ) ;
#127963 = CARTESIAN_POINT ( 'NONE',  ( -16.80939487329394666, 9.950000000011138823, -54.35000000000088249 ) ) ;
#127964 = ORIENTED_EDGE ( 'NONE', *, *, #49983, .F. ) ;
#127965 = CARTESIAN_POINT ( 'NONE',  ( 21.05000000000000426, 65.43724016256084042, -95.56629352660579002 ) ) ;
#127966 = ORIENTED_EDGE ( 'NONE', *, *, #63923, .F. ) ;
#127967 = AXIS2_PLACEMENT_3D ( 'NONE', #10101, #53067, #192590 ) ;
#127968 = DIRECTION ( 'NONE',  ( 0.000000000000000000, 1.000000000000000000, 0.000000000000000000 ) ) ;
#127969 = DIRECTION ( 'NONE',  ( 0.000000000000000000, -0.9651348961777157509, 0.2617529984165031243 ) ) ;
#127970 = ADVANCED_FACE ( 'NONE', ( #132860 ), #230672, .F. ) ;
#127971 = CARTESIAN_POINT ( 'NONE',  ( -20.94999999999999929, 62.98048128140160173, -207.0210305352945852 ) ) ;
#127972 = ORIENTED_EDGE ( 'NONE', *, *, #32961, .F. ) ;
#127973 = EDGE_CURVE ( 'NONE', #173033, #206061, #15484, .T. ) ;
#127975 = EDGE_CURVE ( 'NONE', #52785, #15098, #89851, .T. ) ;
#127974 = DIRECTION ( 'NONE',  ( 0.000000000000000000, 1.000000000000000000, 6.982962677686266711E-15 ) ) ;
#127976 = CIRCLE ( 'NONE', #219526, 0.1000000000000102612 ) ;
#127977 = CARTESIAN_POINT ( 'NONE',  ( -21.05000000000000071, 0.03363273534480442500, -161.2411828053184877 ) ) ;
#127978 = TOROIDAL_SURFACE ( 'NONE', #48849, 0.2000000000000000111, 0.1000000000000000056 ) ;
#127979 = CARTESIAN_POINT ( 'NONE',  ( -18.50000000000000000, 64.35000000001171827, -69.52310748452438816 ) ) ;
#127980 = CARTESIAN_POINT ( 'NONE',  ( -18.59999999999999787, 85.40000000001241176, -163.1410656363516125 ) ) ;
#127981 = DIRECTION ( 'NONE',  ( 0.000000000000000000, -0.9999631594459053030, -0.008583690987162452199 ) ) ;
#127982 = DIRECTION ( 'NONE',  ( -0.000000000000000000, -1.000000000000000000, -6.982962677686266711E-15 ) ) ;
#127983 = EDGE_LOOP ( 'NONE', ( #67564, #53657, #223057, #105090 ) ) ;
#127985 = FACE_OUTER_BOUND ( 'NONE', #25910, .T. ) ;
#127984 = DIRECTION ( 'NONE',  ( 0.000000000000000000, 0.000000000000000000, -1.000000000000000000 ) ) ;
#127986 = ORIENTED_EDGE ( 'NONE', *, *, #242687, .F. ) ;
#127988 = ORIENTED_EDGE ( 'NONE', *, *, #213214, .T. ) ;
#127987 = DIRECTION ( 'NONE',  ( 0.000000000000000000, 0.2128009952263601179, -0.9770955615653315052 ) ) ;
#127989 = TOROIDAL_SURFACE ( 'NONE', #186254, 3.899999999999999467, 0.1000000000000000056 ) ;
#127990 = EDGE_CURVE ( 'NONE', #123224, #158124, #113280, .T. ) ;
#127991 = ORIENTED_EDGE ( 'NONE', *, *, #255705, .F. ) ;
#127992 = LINE ( 'NONE', #165847, #202978 ) ;
#127993 = ADVANCED_FACE ( 'NONE', ( #231966 ), #207321, .F. ) ;
#127994 = CARTESIAN_POINT ( 'NONE',  ( 18.54148534481893407, 10.32532329027886675, -72.56993430183595706 ) ) ;
#127995 = CARTESIAN_POINT ( 'NONE',  ( -21.10000000000000142, 0.000000000000000000, 0.000000000000000000 ) ) ;
#127996 = FACE_OUTER_BOUND ( 'NONE', #137491, .T. ) ;
#127997 = ORIENTED_EDGE ( 'NONE', *, *, #255726, .T. ) ;
#127998 = DIRECTION ( 'NONE',  ( -0.000000000000000000, 1.000000000000000000, 8.717686153663073805E-15 ) ) ;
#128000 = EDGE_CURVE ( 'NONE', #106299, #174560, #36648, .T. ) ;
#127999 = LINE ( 'NONE', #87560, #2244 ) ;
#128001 = ORIENTED_EDGE ( 'NONE', *, *, #210980, .T. ) ;
#128002 = CARTESIAN_POINT ( 'NONE',  ( 18.43579564894481138, -9.519327535281362884, -174.4729766438603349 ) ) ;
#128003 = EDGE_CURVE ( 'NONE', #241028, #196984, #16668, .T. ) ;
#128004 = DIRECTION ( 'NONE',  ( 1.000000000000000000, 0.000000000000000000, 0.000000000000000000 ) ) ;
#128005 = AXIS2_PLACEMENT_3D ( 'NONE', #22091, #2491, #82009 ) ;
#128006 = VERTEX_POINT ( 'NONE', #70339 ) ;
#128007 = AXIS2_PLACEMENT_3D ( 'NONE', #88406, #23360, #39392 ) ;
#128009 = EDGE_CURVE ( 'NONE', #121706, #218126, #252774, .T. ) ;
#128008 = CIRCLE ( 'NONE', #252890, 0.1000000000000024342 ) ;
#128010 = VECTOR ( 'NONE', #200696, 1000.000000000000000 ) ;
#128011 = EDGE_CURVE ( 'NONE', #182615, #153127, #54581, .T. ) ;
#128012 = VERTEX_POINT ( 'NONE', #115850 ) ;
#128013 = CARTESIAN_POINT ( 'NONE',  ( -16.27683809663750480, 9.349999999999978328, -20.94999999999999929 ) ) ;
#128014 = EDGE_LOOP ( 'NONE', ( #63852, #89814, #122523, #92081 ) ) ;
#128015 = CARTESIAN_POINT ( 'NONE',  ( 21.14999999999999503, -0.09999999998884338825, -21.85042919245520210 ) ) ;
#128016 = ADVANCED_FACE ( 'NONE', ( #31222 ), #195412, .F. ) ;
#128017 = CARTESIAN_POINT ( 'NONE',  ( -23.25000000000000000, 0.000000000000000000, 0.000000000000000000 ) ) ;
#128018 = DIRECTION ( 'NONE',  ( -1.000000000000000000, 0.000000000000000000, -0.000000000000000000 ) ) ;
#128019 = CARTESIAN_POINT ( 'NONE',  ( -23.25000000000000355, 11.75000000001113953, -76.25000000000004263 ) ) ;
#128020 = EDGE_CURVE ( 'NONE', #125487, #218291, #52001, .T. ) ;
#128021 = ADVANCED_FACE ( 'NONE', ( #100101 ), #218778, .F. ) ;
#128022 = CIRCLE ( 'NONE', #157257, 0.09999999999999939493 ) ;
#128023 = EDGE_CURVE ( 'NONE', #62457, #62255, #37612, .T. ) ;
#128024 = AXIS2_PLACEMENT_3D ( 'NONE', #42326, #121876, #61891 ) ;
#128025 = DIRECTION ( 'NONE',  ( 1.000000000000000000, 0.000000000000000000, -0.000000000000000000 ) ) ;
#128026 = FACE_OUTER_BOUND ( 'NONE', #34487, .T. ) ;
#128027 = EDGE_LOOP ( 'NONE', ( #106027, #235810, #90171 ) ) ;
#128028 = CARTESIAN_POINT ( 'NONE',  ( -22.48660254037843487, 11.65000000001115588, -100.4500000000000597 ) ) ;
#128029 = VERTEX_POINT ( 'NONE', #160131 ) ;
#128031 = CARTESIAN_POINT ( 'NONE',  ( 11.60000000000000142, -11.65000000000000036, 15.00000000000000355 ) ) ;
#128030 = CARTESIAN_POINT ( 'NONE',  ( -20.94999999999999929, 7.021664781911246322, -104.3335654018973315 ) ) ;
#128032 = ORIENTED_EDGE ( 'NONE', *, *, #214573, .T. ) ;
#128033 = AXIS2_PLACEMENT_3D ( 'NONE', #232605, #250837, #53935 ) ;
#128034 = CARTESIAN_POINT ( 'NONE',  ( -20.94999999999999929, -1.851028230129704522, -145.6539132694225032 ) ) ;
#128035 = DIRECTION ( 'NONE',  ( -1.000000000000000000, 0.000000000000000000, -0.000000000000000000 ) ) ;
#128036 = VERTEX_POINT ( 'NONE', #119709 ) ;
#128038 = ORIENTED_EDGE ( 'NONE', *, *, #82601, .T. ) ;
#128037 = CARTESIAN_POINT ( 'NONE',  ( -23.25000000000000000, 76.00000000001143974, -38.12310748452432563 ) ) ;
#128039 = EDGE_CURVE ( 'NONE', #201306, #159653, #186463, .T. ) ;
#128040 = CYLINDRICAL_SURFACE ( 'NONE', #25667, 0.09999999999999939493 ) ;
#128042 = CARTESIAN_POINT ( 'NONE',  ( 18.49999999999999289, 15.46667084161607164, -223.0640415323869945 ) ) ;
#128041 = LINE ( 'NONE', #88883, #72398 ) ;
#128044 = ORIENTED_EDGE ( 'NONE', *, *, #251225, .F. ) ;
#128043 = DIRECTION ( 'NONE',  ( 1.000000000000000000, -0.000000000000000000, 0.000000000000000000 ) ) ;
#128045 = EDGE_LOOP ( 'NONE', ( #30203, #227261, #92529, #118852 ) ) ;
#128046 = CARTESIAN_POINT ( 'NONE',  ( -23.15000000000000213, -3.281532336344783918, -226.3283167004137226 ) ) ;
#128047 = DIRECTION ( 'NONE',  ( 0.000000000000000000, 0.1350103645451904977, -0.9908441862701596881 ) ) ;
#128048 = VERTEX_POINT ( 'NONE', #161408 ) ;
#128049 = FACE_OUTER_BOUND ( 'NONE', #225641, .T. ) ;
#128050 = ORIENTED_EDGE ( 'NONE', *, *, #164073, .T. ) ;
#128051 = CARTESIAN_POINT ( 'NONE',  ( 18.69999999999999929, -10.84999999999999076, 32.89999999999999858 ) ) ;
#128052 = CARTESIAN_POINT ( 'NONE',  ( 20.94999999999999929, 4.850467289730772791, -112.5342674090017141 ) ) ;
#128053 = EDGE_LOOP ( 'NONE', ( #26124, #57017, #133893 ) ) ;
#128054 = DIRECTION ( 'NONE',  ( 1.000000000000000000, -1.541976423090492636E-14, 0.000000000000000000 ) ) ;
#128055 = CARTESIAN_POINT ( 'NONE',  ( 18.49713797159842343, -9.446482327567830239, -74.07145812161023457 ) ) ;
#128056 = AXIS2_PLACEMENT_3D ( 'NONE', #245367, #28926, #125419 ) ;
#128057 = ADVANCED_FACE ( 'NONE', ( #40190 ), #220084, .T. ) ;
#128058 = EDGE_LOOP ( 'NONE', ( #96573, #185097, #115464, #225147 ) ) ;
#128059 = CIRCLE ( 'NONE', #244738, 0.2000000000000057288 ) ;
#128060 = AXIS2_PLACEMENT_3D ( 'NONE', #20408, #76501, #135187 ) ;
#128062 = ADVANCED_FACE ( 'NONE', ( #179682 ), #74068, .T. ) ;
#128061 = CARTESIAN_POINT ( 'NONE',  ( -16.88593481969334320, 66.04943990992720160, -48.67123522757989917 ) ) ;
#128063 = ORIENTED_EDGE ( 'NONE', *, *, #233745, .F. ) ;
#128064 = ORIENTED_EDGE ( 'NONE', *, *, #89389, .F. ) ;
#128065 = ORIENTED_EDGE ( 'NONE', *, *, #120588, .T. ) ;
#128066 = AXIS2_PLACEMENT_3D ( 'NONE', #247420, #68805, #205726 ) ;
#128067 = ORIENTED_EDGE ( 'NONE', *, *, #94623, .T. ) ;
#128068 = CARTESIAN_POINT ( 'NONE',  ( 18.47149038651510367, -0.9011289498978589663, -242.3107469318997857 ) ) ;
#128069 = ORIENTED_EDGE ( 'NONE', *, *, #45744, .F. ) ;
#128071 = ORIENTED_EDGE ( 'NONE', *, *, #236877, .T. ) ;
#128070 = CARTESIAN_POINT ( 'NONE',  ( 21.05000000000000071, 28.27358281186466371, -238.9334100630653381 ) ) ;
#128072 = CARTESIAN_POINT ( 'NONE',  ( -21.05000000000000071, 11.63687328911505325, -73.82175921332471091 ) ) ;
#128073 = ORIENTED_EDGE ( 'NONE', *, *, #23133, .F. ) ;
#128074 = FACE_OUTER_BOUND ( 'NONE', #85547, .T. ) ;
#128075 = ORIENTED_EDGE ( 'NONE', *, *, #211385, .F. ) ;
#128078 = ORIENTED_EDGE ( 'NONE', *, *, #139030, .F. ) ;
#128077 = ORIENTED_EDGE ( 'NONE', *, *, #57563, .T. ) ;
#128076 = DIRECTION ( 'NONE',  ( -0.7071067811865127117, -0.7071067811865821007, 0.000000000000000000 ) ) ;
#128079 = DIRECTION ( 'NONE',  ( 0.000000000000000000, 0.2617529984165045120, 0.9651348961777153068 ) ) ;
#128080 = EDGE_CURVE ( 'NONE', #19771, #13368, #62288, .T. ) ;
#128081 = DIRECTION ( 'NONE',  ( -0.000000000000000000, -0.4721928772777346239, -0.8814952561688430555 ) ) ;
#128083 = EDGE_LOOP ( 'NONE', ( #36990, #172730, #8444, #192186 ) ) ;
#128082 = AXIS2_PLACEMENT_3D ( 'NONE', #110622, #71523, #127624 ) ;
#128084 = CIRCLE ( 'NONE', #232149, 0.09999999999999939493 ) ;
#128085 = AXIS2_PLACEMENT_3D ( 'NONE', #206057, #44429, #183926 ) ;
#128086 = ORIENTED_EDGE ( 'NONE', *, *, #213079, .F. ) ;
#128087 = CIRCLE ( 'NONE', #98820, 4.299999999999953637 ) ;
#128088 = CARTESIAN_POINT ( 'NONE',  ( -21.05000000000000071, 69.74218538953117275, -203.6208977758336118 ) ) ;
#128089 = LINE ( 'NONE', #248021, #14095 ) ;
#128091 = VERTEX_POINT ( 'NONE', #989 ) ;
#128090 = DIRECTION ( 'NONE',  ( 1.000000000000000000, 0.000000000000000000, 0.000000000000000000 ) ) ;
#128092 = DIRECTION ( 'NONE',  ( -0.000000000000000000, 1.000000000000000000, 6.982962677686266711E-15 ) ) ;
#128093 = VERTEX_POINT ( 'NONE', #19312 ) ;
#128094 = CIRCLE ( 'NONE', #203093, 0.09999999999999990841 ) ;
#128095 = DIRECTION ( 'NONE',  ( -1.000000000000000000, 0.000000000000000000, 0.000000000000000000 ) ) ;
#128096 = CARTESIAN_POINT ( 'NONE',  ( 18.59999999999999076, 43.10494791715829166, -239.6505508802563327 ) ) ;
#128097 = ORIENTED_EDGE ( 'NONE', *, *, #41371, .F. ) ;
#128098 = DIRECTION ( 'NONE',  ( -1.000000000000000000, -0.000000000000000000, 0.000000000000000000 ) ) ;
#128099 = DIRECTION ( 'NONE',  ( 1.000000000000000000, 0.000000000000000000, 0.000000000000000000 ) ) ;
#128100 = ORIENTED_EDGE ( 'NONE', *, *, #45311, .T. ) ;
#128102 = ORIENTED_EDGE ( 'NONE', *, *, #157543, .T. ) ;
#128101 = DIRECTION ( 'NONE',  ( 1.000000000000000000, 0.000000000000000000, 0.000000000000000000 ) ) ;
#128103 = DIRECTION ( 'NONE',  ( 1.000000000000000000, 0.000000000000000000, 0.000000000000000000 ) ) ;
#128104 = VECTOR ( 'NONE', #88672, 1000.000000000000000 ) ;
#128105 = AXIS2_PLACEMENT_3D ( 'NONE', #98067, #177676, #199797 ) ;
#128106 = AXIS2_PLACEMENT_3D ( 'NONE', #108956, #222473, #43870 ) ;
#128108 = VERTEX_POINT ( 'NONE', #18023 ) ;
#128107 = ORIENTED_EDGE ( 'NONE', *, *, #91706, .F. ) ;
#128109 = VERTEX_POINT ( 'NONE', #118427 ) ;
#128110 = CARTESIAN_POINT ( 'NONE',  ( -23.39999999999994529, 76.00000000001119815, -36.02310748452479316 ) ) ;
#128111 = EDGE_LOOP ( 'NONE', ( #246802, #49042, #64562, #83525 ) ) ;
#128112 = CARTESIAN_POINT ( 'NONE',  ( -21.05000000000000071, 1.115600667400684642E-11, -33.50000000000000000 ) ) ;
#128114 = ORIENTED_EDGE ( 'NONE', *, *, #216524, .F. ) ;
#128113 = B_SPLINE_CURVE_WITH_KNOTS ( 'NONE', 3,
 ( #185799, #48853, #26753, #188369, #89257, #9722, #226169, #145380, #166273, #46273 ),
 .UNSPECIFIED., .F., .F.,
 ( 4, 3, 3, 4 ),
 ( 0.000000000000000000, 3.394313611810396763E-05, 6.779740500698037422E-05, 0.0001049857339142504432 ),
 .UNSPECIFIED. ) ;
#128115 = LINE ( 'NONE', #207663, #23141 ) ;
#128116 = DIRECTION ( 'NONE',  ( 1.000000000000000000, 0.000000000000000000, -1.020425574104004196E-15 ) ) ;
#128117 = EDGE_CURVE ( 'NONE', #164178, #11451, #165625, .T. ) ;
#128118 = ORIENTED_EDGE ( 'NONE', *, *, #22746, .T. ) ;
#128119 = VECTOR ( 'NONE', #88378, 1000.000000000000000 ) ;
#128120 = EDGE_CURVE ( 'NONE', #70810, #29169, #215655, .T. ) ;
#128121 = AXIS2_PLACEMENT_3D ( 'NONE', #106972, #69169, #127844 ) ;
#128122 = VERTEX_POINT ( 'NONE', #41468 ) ;
#128123 = VECTOR ( 'NONE', #34314, 1000.000000000000000 ) ;
#128124 = ORIENTED_EDGE ( 'NONE', *, *, #1434, .F. ) ;
#128125 = AXIS2_PLACEMENT_3D ( 'NONE', #100816, #216943, #215657 ) ;
#128126 = EDGE_CURVE ( 'NONE', #145620, #154671, #53183, .T. ) ;
#128127 = DIRECTION ( 'NONE',  ( 0.000000000000000000, -1.000000000000000000, 0.000000000000000000 ) ) ;
#128128 = VERTEX_POINT ( 'NONE', #137956 ) ;
#128129 = CARTESIAN_POINT ( 'NONE',  ( 20.85000000000000142, -1.835859311432481045, -179.0044391687985410 ) ) ;
#128132 = ADVANCED_FACE ( 'NONE', ( #221336 ), #140663, .F. ) ;
#128131 = VERTEX_POINT ( 'NONE', #42721 ) ;
#128130 = DIRECTION ( 'NONE',  ( 0.000000000000000000, -0.9126074666063769270, -0.4088369013363282733 ) ) ;
#128133 = CARTESIAN_POINT ( 'NONE',  ( 23.24999999999999289, 6.650000000011155876, -121.6500000000000341 ) ) ;
#128134 = DIRECTION ( 'NONE',  ( 1.000000000000000000, 0.000000000000000000, 0.000000000000000000 ) ) ;
#128135 = TOROIDAL_SURFACE ( 'NONE', #182303, 0.4000000000000010214, 0.1000000000000000056 ) ;
#128136 = EDGE_CURVE ( 'NONE', #6394, #54060, #141814, .T. ) ;
#128137 = CARTESIAN_POINT ( 'NONE',  ( -21.05000000000000071, 77.83534155023598089, -57.96795619196132776 ) ) ;
#128138 = CARTESIAN_POINT ( 'NONE',  ( -23.15000000000000213, 76.00000000001170974, -69.52310748452431710 ) ) ;
#128139 = CARTESIAN_POINT ( 'NONE',  ( 23.24999999999999645, 1.115600667400684642E-11, -33.50000000000000000 ) ) ;
#128141 = DIRECTION ( 'NONE',  ( 0.000000000000000000, 0.000000000000000000, 1.000000000000000000 ) ) ;
#128140 = CARTESIAN_POINT ( 'NONE',  ( 18.59999999999996945, 68.97833521811203639, -132.6895420826271277 ) ) ;
#128143 = VECTOR ( 'NONE', #127560, 1000.000000000000000 ) ;
#128142 = DIRECTION ( 'NONE',  ( -1.000000000000000000, 0.000000000000000000, 0.000000000000000000 ) ) ;
#128144 = VECTOR ( 'NONE', #243002, 1000.000000000000114 ) ;
#128145 = FACE_OUTER_BOUND ( 'NONE', #2066, .T. ) ;
#128146 = EDGE_CURVE ( 'NONE', #67578, #189375, #119847, .T. ) ;
#128148 = CARTESIAN_POINT ( 'NONE',  ( -23.15000000000000213, 0.000000000000000000, -37.40000000000000568 ) ) ;
#128147 = AXIS2_PLACEMENT_3D ( 'NONE', #161045, #163612, #27984 ) ;
#128149 = B_SPLINE_CURVE_WITH_KNOTS ( 'NONE', 3,
 ( #90593, #167604, #247100, #48908, #29393, #89312, #69785, #209269, #110165, #150593, #191022, #12385, #236528, #155756, #157026, #20075, #235250, #174045, #77440 ),
 .UNSPECIFIED., .F., .F.,
 ( 4, 3, 3, 3, 3, 3, 4 ),
 ( 1.387778780781445676E-17, 2.646747978909242031E-05, 5.271166642130207115E-05, 9.008788829887291478E-05, 0.0001426648776561344830, 0.0001897378458660081940, 0.0001917382627806528145 ),
 .UNSPECIFIED. ) ;
#128151 = ORIENTED_EDGE ( 'NONE', *, *, #120311, .T. ) ;
#128150 = VECTOR ( 'NONE', #135161, 1000.000000000000114 ) ;
#128152 = VERTEX_POINT ( 'NONE', #180960 ) ;
#128154 = VERTEX_POINT ( 'NONE', #122267 ) ;
#128153 = DIRECTION ( 'NONE',  ( 1.000000000000000000, 1.394253735153569469E-16, 2.602809386958778209E-16 ) ) ;
#128155 = ORIENTED_EDGE ( 'NONE', *, *, #132597, .F. ) ;
#128157 = EDGE_CURVE ( 'NONE', #130548, #212715, #16766, .T. ) ;
#128156 = CARTESIAN_POINT ( 'NONE',  ( 22.39999999999999503, 26.06832281015329755, -254.4051978787608732 ) ) ;
#128158 = CARTESIAN_POINT ( 'NONE',  ( 20.41140022480508520, 10.41043084241320216, -141.6150013036338464 ) ) ;
#128159 = VERTEX_POINT ( 'NONE', #58407 ) ;
#128160 = DIRECTION ( 'NONE',  ( -0.000000000000000000, -0.01283462868040327436, 0.9999176327611370985 ) ) ;
#128161 = CARTESIAN_POINT ( 'NONE',  ( 21.72449340488910607, 65.71604372252048165, -60.27310748452440237 ) ) ;
#128162 = ORIENTED_EDGE ( 'NONE', *, *, #109150, .T. ) ;
#128163 = CIRCLE ( 'NONE', #98897, 0.09999999999999459321 ) ;
#128164 = CARTESIAN_POINT ( 'NONE',  ( 23.04999999999999716, 8.822561741677553471, -57.75000000000000000 ) ) ;
#128165 = CYLINDRICAL_SURFACE ( 'NONE', #254564, 0.5000000000000004441 ) ;
#128166 = DIRECTION ( 'NONE',  ( -1.000000000000000000, -0.000000000000000000, 0.000000000000000000 ) ) ;
#128167 = CARTESIAN_POINT ( 'NONE',  ( 23.15000000000000213, 87.65000000001144542, -39.12310748452424747 ) ) ;
#128168 = CARTESIAN_POINT ( 'NONE',  ( -18.43569575749026868, 78.24390740893983320, -231.6169762517609456 ) ) ;
#128170 = ORIENTED_EDGE ( 'NONE', *, *, #239377, .F. ) ;
#128169 = CARTESIAN_POINT ( 'NONE',  ( -16.97048326478264357, 66.05000000001231797, -156.8820006043973194 ) ) ;
#128171 = CARTESIAN_POINT ( 'NONE',  ( 20.94999999999999929, 6.256349259666489360, -229.7266095100222572 ) ) ;
#128172 = CARTESIAN_POINT ( 'NONE',  ( -16.27683809663751191, 66.65000000001208491, -123.9731074845243626 ) ) ;
#128173 = CARTESIAN_POINT ( 'NONE',  ( 21.05000000000000071, 87.65000000001192859, -100.1231074845242262 ) ) ;
#128174 = CARTESIAN_POINT ( 'NONE',  ( 18.50000000000000355, 85.42145614550825883, -95.78112540050472035 ) ) ;
#128175 = ORIENTED_EDGE ( 'NONE', *, *, #250735, .T. ) ;
#128176 = CARTESIAN_POINT ( 'NONE',  ( 12.25000000000000000, 66.65000000001185754, -86.15883987690831702 ) ) ;
#128177 = DIRECTION ( 'NONE',  ( 1.000000000000000000, 5.603460673774837551E-17, 1.046060675573451153E-16 ) ) ;
#128179 = DIRECTION ( 'NONE',  ( 0.000000000000000000, 0.000000000000000000, 1.000000000000000000 ) ) ;
#128178 = DIRECTION ( 'NONE',  ( 0.000000000000000000, -0.9126074666063622720, -0.4088369013363611360 ) ) ;
#128180 = DIRECTION ( 'NONE',  ( 1.000000000000000000, 0.000000000000000000, 0.000000000000000000 ) ) ;
#128181 = CARTESIAN_POINT ( 'NONE',  ( -16.85697194749128514, 9.908543714134763647, -54.06499573238597378 ) ) ;
#128182 = DIRECTION ( 'NONE',  ( -0.000000000000000000, -0.000000000000000000, 1.000000000000000000 ) ) ;
#128183 = DIRECTION ( 'NONE',  ( 4.336808689942017736E-16, -0.000000000000000000, 1.000000000000000000 ) ) ;
#128184 = CIRCLE ( 'NONE', #140640, 0.1000000000000002692 ) ;
#128185 = AXIS2_PLACEMENT_3D ( 'NONE', #160950, #185635, #224740 ) ;
#128186 = FACE_OUTER_BOUND ( 'NONE', #244978, .T. ) ;
#128187 = CARTESIAN_POINT ( 'NONE',  ( -16.81744102076748959, 9.950000000011138823, -87.85000000000005116 ) ) ;
#128188 = AXIS2_PLACEMENT_3D ( 'NONE', #219941, #238211, #76577 ) ;
#128189 = ORIENTED_EDGE ( 'NONE', *, *, #245508, .F. ) ;
#128190 = EDGE_CURVE ( 'NONE', #179110, #124908, #253078, .T. ) ;
#128191 = VERTEX_POINT ( 'NONE', #46555 ) ;
#128192 = EDGE_LOOP ( 'NONE', ( #32515, #135116, #64157, #3244 ) ) ;
#128193 = CARTESIAN_POINT ( 'NONE',  ( 20.77766267348356166, 65.55095760939289562, -95.43039856864687920 ) ) ;
#128194 = CARTESIAN_POINT ( 'NONE',  ( -23.39999999999994529, 74.63923853664559260, -43.99645795275012006 ) ) ;
#128195 = ORIENTED_EDGE ( 'NONE', *, *, #72698, .F. ) ;
#128196 = ADVANCED_FACE ( 'NONE', ( #143088 ), #27045, .F. ) ;
#128197 = VERTEX_POINT ( 'NONE', #165238 ) ;
#128198 = EDGE_CURVE ( 'NONE', #242024, #255081, #136551, .T. ) ;
#128199 = AXIS2_PLACEMENT_3D ( 'NONE', #33787, #11634, #155000 ) ;
#128200 = ADVANCED_FACE ( 'NONE', ( #144358 ), #206935, .T. ) ;
#128201 = AXIS2_PLACEMENT_3D ( 'NONE', #253360, #155592, #192132 ) ;
#128202 = ORIENTED_EDGE ( 'NONE', *, *, #65681, .T. ) ;
#128203 = CARTESIAN_POINT ( 'NONE',  ( 21.04999999999999716, 76.00000000001199396, -109.5637644362255685 ) ) ;
#128204 = ORIENTED_EDGE ( 'NONE', *, *, #111803, .F. ) ;
#128205 =( BOUNDED_CURVE ( )  B_SPLINE_CURVE ( 3, ( #18778, #177880, #59156, #239123 ),
 .UNSPECIFIED., .F., .T. ) 
 B_SPLINE_CURVE_WITH_KNOTS ( ( 4, 4 ),
 ( 3.141592653589793116, 4.712388980384689674 ),
 .UNSPECIFIED. ) 
 CURVE ( )  GEOMETRIC_REPRESENTATION_ITEM ( )  RATIONAL_B_SPLINE_CURVE ( ( 1.000000000000000000, 0.8047378541243649375, 0.8047378541243649375, 1.000000000000000000 ) ) 
 REPRESENTATION_ITEM ( '' )  );
#128206 = DIRECTION ( 'NONE',  ( 0.000000000000000000, 0.000000000000000000, 1.000000000000000000 ) ) ;
#128207 = VECTOR ( 'NONE', #112115, 1000.000000000000000 ) ;
#128208 = FACE_OUTER_BOUND ( 'NONE', #17249, .T. ) ;
#128209 = CARTESIAN_POINT ( 'NONE',  ( -21.14999999999994174, 76.00000000001119815, -36.02310748452479316 ) ) ;
#128210 = CARTESIAN_POINT ( 'NONE',  ( -21.13498764882296044, 1.403758898530641952, -230.6640565874768640 ) ) ;
#128211 = CARTESIAN_POINT ( 'NONE',  ( -16.84419801905645642, 30.18914835313876210, -234.7978420382347906 ) ) ;
#128212 = LINE ( 'NONE', #109912, #145098 ) ;
#128214 = ORIENTED_EDGE ( 'NONE', *, *, #194691, .F. ) ;
#128213 = CARTESIAN_POINT ( 'NONE',  ( -23.15000000000000213, 76.00000000001188027, -99.12310748452429721 ) ) ;
#128216 = FACE_OUTER_BOUND ( 'NONE', #253777, .T. ) ;
#128215 = DIRECTION ( 'NONE',  ( -1.000000000000000000, 0.000000000000000000, 0.000000000000000000 ) ) ;
#128217 = ADVANCED_FACE ( 'NONE', ( #162681 ), #47833, .T. ) ;
#128218 = CARTESIAN_POINT ( 'NONE',  ( 20.94999999999999929, -4.756823075239758225, -233.1486023682345490 ) ) ;
#128219 = ORIENTED_EDGE ( 'NONE', *, *, #120588, .F. ) ;
#128220 = LINE ( 'NONE', #111218, #23812 ) ;
#128221 = CARTESIAN_POINT ( 'NONE',  ( -15.52965525596988172, 9.375538102059159939, -116.3698758809908753 ) ) ;
#128223 = ADVANCED_FACE ( 'NONE', ( #85658 ), #183525, .T. ) ;
#128222 = DIRECTION ( 'NONE',  ( -2.602085213965226419E-14, 6.982962677686266711E-15, -1.000000000000000000 ) ) ;
#128224 = VERTEX_POINT ( 'NONE', #124838 ) ;
#128225 = CARTESIAN_POINT ( 'NONE',  ( -21.14999999999999858, 6.540656951712397138, -33.50000000000000000 ) ) ;
#128226 = AXIS2_PLACEMENT_3D ( 'NONE', #138098, #40344, #136825 ) ;
#128227 = CARTESIAN_POINT ( 'NONE',  ( -16.80891096016330621, 66.05000000001182059, -82.15544467725624145 ) ) ;
#128228 = ORIENTED_EDGE ( 'NONE', *, *, #243027, .F. ) ;
#128229 = AXIS2_PLACEMENT_3D ( 'NONE', #10710, #248023, #69414 ) ;
#128230 = CARTESIAN_POINT ( 'NONE',  ( 20.94999999999999929, 0.000000000000000000, -33.50000000000000000 ) ) ;
#128231 = CARTESIAN_POINT ( 'NONE',  ( 22.94999999999999929, 11.99999999999999822, 12.00000000000000000 ) ) ;
#128232 = EDGE_CURVE ( 'NONE', #35759, #142216, #103233, .T. ) ;
#128233 = DIRECTION ( 'NONE',  ( -0.000000000000000000, 1.000000000000000000, 2.891205793294679805E-16 ) ) ;
#128234 = DIRECTION ( 'NONE',  ( 0.000000000000000000, 6.853228547068871147E-15, -1.000000000000000000 ) ) ;
#128235 = EDGE_CURVE ( 'NONE', #38202, #98142, #67418, .T. ) ;
#128236 = EDGE_LOOP ( 'NONE', ( #53768, #219704, #26396, #137765, #184509, #21342, #173701, #197872, #221000, #247602, #188470, #67148, #129874, #257937, #212784, #108260, #220533, #217526, #194325, #109977, #211711, #125479, #198200 ) ) ;
#128237 = ADVANCED_FACE ( 'NONE', ( #66139 ), #169938, .T. ) ;
#128238 = CIRCLE ( 'NONE', #161577, 11.79999999999999361 ) ;
#128239 = ORIENTED_EDGE ( 'NONE', *, *, #58461, .F. ) ;
#128240 = CYLINDRICAL_SURFACE ( 'NONE', #48591, 0.09999999999998898659 ) ;
#128241 = DIRECTION ( 'NONE',  ( -1.000000000000000000, 0.000000000000000000, -0.000000000000000000 ) ) ;
#128242 = DIRECTION ( 'NONE',  ( 0.000000000000000000, -0.8660254037844377084, -0.5000000000000016653 ) ) ;
#128243 = FACE_OUTER_BOUND ( 'NONE', #46565, .T. ) ;
#128244 = VECTOR ( 'NONE', #41136, 1000.000000000000000 ) ;
#128246 = FACE_OUTER_BOUND ( 'NONE', #145982, .T. ) ;
#128245 = CIRCLE ( 'NONE', #44849, 4.099999999999992539 ) ;
#128247 = CARTESIAN_POINT ( 'NONE',  ( -21.05000000000000071, 6.300000000000014033, -0.09999999999999939493 ) ) ;
#128248 = DIRECTION ( 'NONE',  ( 0.000000000000000000, 0.8814952561688428334, -0.4721928772777348460 ) ) ;
#128249 = AXIS2_PLACEMENT_3D ( 'NONE', #76336, #17654, #196297 ) ;
#128250 = ORIENTED_EDGE ( 'NONE', *, *, #19713, .F. ) ;
#128251 = FACE_OUTER_BOUND ( 'NONE', #106939, .T. ) ;
#128253 = EDGE_LOOP ( 'NONE', ( #43734, #192440, #138050, #78040 ) ) ;
#128252 = CARTESIAN_POINT ( 'NONE',  ( -37.88850191057539973, -9.749999999999943157, -15.00000000000002309 ) ) ;
#128254 = DIRECTION ( 'NONE',  ( -0.000000000000000000, -1.000000000000000000, -0.000000000000000000 ) ) ;
#128255 = CIRCLE ( 'NONE', #74116, 7.899999999999990585 ) ;
#128256 = DIRECTION ( 'NONE',  ( 0.000000000000000000, -0.9651348961777161950, 0.2617529984165014589 ) ) ;
#128257 = DIRECTION ( 'NONE',  ( 0.000000000000000000, -0.4721928772777343464, -0.8814952561688431665 ) ) ;
#128258 = CARTESIAN_POINT ( 'NONE',  ( -16.80070461187861142, 66.05000000001206217, -123.8761436553653397 ) ) ;
#128259 = ORIENTED_EDGE ( 'NONE', *, *, #159188, .F. ) ;
#128260 = CARTESIAN_POINT ( 'NONE',  ( -21.05000000000000071, 68.48451787451661232, -224.2224406095231757 ) ) ;
#128261 = CARTESIAN_POINT ( 'NONE',  ( -21.14999999999999858, 64.25000000001190870, -96.29697684846520644 ) ) ;
#128262 = CARTESIAN_POINT ( 'NONE',  ( 22.49999999999999645, 11.64987090377453960, -66.91748010912705524 ) ) ;
#128263 = DIRECTION ( 'NONE',  ( 0.000000000000000000, -0.8103668758649577031, 0.5859227990963212784 ) ) ;
#128264 =( BOUNDED_CURVE ( )  B_SPLINE_CURVE ( 3, ( #96504, #193077, #57383, #14456 ),
 .UNSPECIFIED., .F., .F. ) 
 B_SPLINE_CURVE_WITH_KNOTS ( ( 4, 4 ),
 ( 3.141592653589793116, 4.712388980384689674 ),
 .UNSPECIFIED. ) 
 CURVE ( )  GEOMETRIC_REPRESENTATION_ITEM ( )  RATIONAL_B_SPLINE_CURVE ( ( 1.000000000000000000, 0.8047378541243649375, 0.8047378541243649375, 1.000000000000000000 ) ) 
 REPRESENTATION_ITEM ( '' )  );
#128265 = ORIENTED_EDGE ( 'NONE', *, *, #196241, .F. ) ;
#128266 = CARTESIAN_POINT ( 'NONE',  ( -15.15564720441980384, 66.58929125296516816, -151.9538990786803083 ) ) ;
#128267 = DIRECTION ( 'NONE',  ( -0.000000000000000000, 0.2128009952263604232, -0.9770955615653316162 ) ) ;
#128268 = ORIENTED_EDGE ( 'NONE', *, *, #226798, .T. ) ;
#128269 = CARTESIAN_POINT ( 'NONE',  ( -21.07928932188134041, 1.596973512272247042, -230.6572452218044020 ) ) ;
#128270 = ADVANCED_FACE ( 'NONE', ( #3591 ), #126093, .F. ) ;
#128271 = CARTESIAN_POINT ( 'NONE',  ( -16.91049119928363353, 66.05000000001190585, -90.40482787771522055 ) ) ;
#128272 = AXIS2_PLACEMENT_3D ( 'NONE', #53882, #172593, #12207 ) ;
#128273 = ORIENTED_EDGE ( 'NONE', *, *, #31803, .T. ) ;
#128274 = DIRECTION ( 'NONE',  ( 1.000000000000000000, -0.000000000000000000, -0.000000000000000000 ) ) ;
#128275 = VECTOR ( 'NONE', #186809, 1000.000000000000000 ) ;
#128276 = ORIENTED_EDGE ( 'NONE', *, *, #187537, .T. ) ;
#128277 = CIRCLE ( 'NONE', #124000, 12.87499999999999822 ) ;
#128278 = DIRECTION ( 'NONE',  ( -0.000000000000000000, -0.000000000000000000, -1.000000000000000000 ) ) ;
#128280 = DIRECTION ( 'NONE',  ( -1.000000000000000000, 0.000000000000000000, 0.000000000000000000 ) ) ;
#128279 = AXIS2_PLACEMENT_3D ( 'NONE', #248302, #129639, #10976 ) ;
#128281 = CIRCLE ( 'NONE', #153244, 11.65000000000000036 ) ;
#128282 = EDGE_CURVE ( 'NONE', #117519, #144953, #236512, .T. ) ;
#128283 = DIRECTION ( 'NONE',  ( 1.000000000000000000, 0.000000000000000000, 0.000000000000000000 ) ) ;
#128284 = EDGE_LOOP ( 'NONE', ( #242299, #242594, #54452, #72049 ) ) ;
#128285 = AXIS2_PLACEMENT_3D ( 'NONE', #200219, #41171, #62000 ) ;
#128286 = ADVANCED_FACE ( 'NONE', ( #203074 ), #84358, .T. ) ;
#128287 = SPHERICAL_SURFACE ( 'NONE', #129464, 0.1000000000000000056 ) ;
#128288 = CARTESIAN_POINT ( 'NONE',  ( 21.06280952165566589, 12.98075861599861724, -210.6630625559073735 ) ) ;
#128289 = EDGE_CURVE ( 'NONE', #116380, #260, #111439, .T. ) ;
#128290 = CARTESIAN_POINT ( 'NONE',  ( 15.73863059295127798, 9.351403174141653452, -16.97953043683848762 ) ) ;
#128291 = DIRECTION ( 'NONE',  ( 0.000000000000000000, 0.3738317757009345654, 0.9274965247785492695 ) ) ;
#128292 = AXIS2_PLACEMENT_3D ( 'NONE', #40959, #200008, #21392 ) ;
#128293 = DIRECTION ( 'NONE',  ( 0.000000000000000000, -0.9126074666063769270, -0.4088369013363280513 ) ) ;
#128294 = AXIS2_PLACEMENT_3D ( 'NONE', #112524, #13426, #113793 ) ;
#128295 = ORIENTED_EDGE ( 'NONE', *, *, #11767, .F. ) ;
#128297 = VERTEX_POINT ( 'NONE', #202633 ) ;
#128296 = CARTESIAN_POINT ( 'NONE',  ( 20.89878130938411616, 10.32747123227773045, -106.0774032850249711 ) ) ;
#128298 = ADVANCED_FACE ( 'NONE', ( #121832 ), #78812, .T. ) ;
#128299 = ORIENTED_EDGE ( 'NONE', *, *, #78700, .F. ) ;
#128300 = PLANE ( 'NONE',  #157030 ) ;
#128301 = ADVANCED_FACE ( 'NONE', ( #241756 ), #201349, .F. ) ;
#128302 = ORIENTED_EDGE ( 'NONE', *, *, #109757, .T. ) ;
#128303 = CARTESIAN_POINT ( 'NONE',  ( 21.05000000000000071, 60.96493190257000805, -234.1404541814610241 ) ) ;
#128304 = FACE_OUTER_BOUND ( 'NONE', #180188, .T. ) ;
#128305 = DIRECTION ( 'NONE',  ( 1.000000000000000000, 2.952720810173289112E-16, -0.000000000000000000 ) ) ;
#128306 = ORIENTED_EDGE ( 'NONE', *, *, #217433, .T. ) ;
#128307 = DIRECTION ( 'NONE',  ( 0.000000000000000000, 0.000000000000000000, 1.000000000000000000 ) ) ;
#128308 = DIRECTION ( 'NONE',  ( 1.000000000000000000, 3.265361837132813093E-16, -0.000000000000000000 ) ) ;
#128309 = DIRECTION ( 'NONE',  ( -1.000000000000000000, 0.000000000000000000, -0.000000000000000000 ) ) ;
#128310 = EDGE_LOOP ( 'NONE', ( #145187, #203607, #226099, #249395, #142513 ) ) ;
#128311 = DIRECTION ( 'NONE',  ( -0.000000000000000000, -1.000000000000000000, -6.982962677686266711E-15 ) ) ;
#128312 = AXIS2_PLACEMENT_3D ( 'NONE', #52802, #191072, #55343 ) ;
#128314 = EDGE_LOOP ( 'NONE', ( #25472, #192792, #251343, #43191 ) ) ;
#128313 = CARTESIAN_POINT ( 'NONE',  ( 23.15000000000000213, 69.19063053712525857, -247.5666987377248631 ) ) ;
#128315 = CYLINDRICAL_SURFACE ( 'NONE', #44278, 0.1000000000000028644 ) ;
#128316 = AXIS2_PLACEMENT_3D ( 'NONE', #179192, #77461, #138708 ) ;
#128317 = TOROIDAL_SURFACE ( 'NONE', #157567, 0.6000000000000017542, 0.1000000000000000056 ) ;
#128318 = EDGE_CURVE ( 'NONE', #241890, #57917, #65642, .T. ) ;
#128319 = EDGE_CURVE ( 'NONE', #138090, #75643, #98943, .T. ) ;
#128320 = ORIENTED_EDGE ( 'NONE', *, *, #17075, .T. ) ;
#128321 = AXIS2_PLACEMENT_3D ( 'NONE', #49873, #129416, #231110 ) ;
#128322 = CARTESIAN_POINT ( 'NONE',  ( 21.05000000000000071, 69.20602499728043711, -247.8456586332460176 ) ) ;
#128323 = CARTESIAN_POINT ( 'NONE',  ( 18.59999999999999432, -1.736257131597395809, -11.56865232901749785 ) ) ;
#128324 = CARTESIAN_POINT ( 'NONE',  ( 21.05000000000000071, 39.23476235320398331, -236.9756760510740037 ) ) ;
#128325 = VERTEX_POINT ( 'NONE', #160960 ) ;
#128326 = FACE_OUTER_BOUND ( 'NONE', #238335, .T. ) ;
#128327 = EDGE_CURVE ( 'NONE', #212172, #179904, #61737, .T. ) ;
#128328 = DIRECTION ( 'NONE',  ( -0.7071067811865456854, 0.7071067811865493491, 0.000000000000000000 ) ) ;
#128329 = AXIS2_PLACEMENT_3D ( 'NONE', #124303, #43475, #179162 ) ;
#128330 = ORIENTED_EDGE ( 'NONE', *, *, #94742, .F. ) ;
#128331 = AXIS2_PLACEMENT_3D ( 'NONE', #123400, #84207, #4709 ) ;
#128332 = AXIS2_PLACEMENT_3D ( 'NONE', #256088, #254815, #175368 ) ;
#128333 = ADVANCED_FACE ( 'NONE', ( #158410 ), #15984, .T. ) ;
#128334 = CIRCLE ( 'NONE', #165758, 0.1999999999999987899 ) ;
#128335 = EDGE_CURVE ( 'NONE', #26629, #103428, #211592, .T. ) ;
#128336 = ORIENTED_EDGE ( 'NONE', *, *, #13632, .T. ) ;
#128337 = CARTESIAN_POINT ( 'NONE',  ( 22.47071067811865319, 68.27992525551464098, -203.6221999392270448 ) ) ;
#128338 = EDGE_CURVE ( 'NONE', #218193, #19640, #65823, .T. ) ;
#128339 = EDGE_LOOP ( 'NONE', ( #233009, #257531, #214822, #7223 ) ) ;
#128340 = DIRECTION ( 'NONE',  ( 1.000000000000000000, -0.000000000000000000, -0.000000000000000000 ) ) ;
#128341 = CARTESIAN_POINT ( 'NONE',  ( -23.15000000000000213, 2.600000000011156054, -155.7499999999999716 ) ) ;
#128343 = EDGE_LOOP ( 'NONE', ( #101963, #37369, #65957, #188781 ) ) ;
#128342 = CARTESIAN_POINT ( 'NONE',  ( 14.11444803880196197, 24.81692076904265321, -232.4788742220511608 ) ) ;
#128344 = CARTESIAN_POINT ( 'NONE',  ( 20.94999999999999929, 11.75000000001115552, -127.2161343370219413 ) ) ;
#128345 = CARTESIAN_POINT ( 'NONE',  ( 21.05000000000000071, 65.27628289530404970, -57.37310748452439668 ) ) ;
#128346 = CARTESIAN_POINT ( 'NONE',  ( -21.44999999999999929, 68.65000000001150227, -48.27310748452437394 ) ) ;
#128347 = DIRECTION ( 'NONE',  ( 0.000000000000000000, 0.000000000000000000, 1.000000000000000000 ) ) ;
#128348 = DIRECTION ( 'NONE',  ( 1.000000000000000000, 3.265361837132813093E-16, -0.000000000000000000 ) ) ;
#128349 = EDGE_CURVE ( 'NONE', #100304, #25027, #142643, .T. ) ;
#128350 = AXIS2_PLACEMENT_3D ( 'NONE', #109356, #67683, #24744 ) ;
#128351 = CARTESIAN_POINT ( 'NONE',  ( -11.59999999999994458, 66.35000000001119247, -23.62310748452479103 ) ) ;
#128352 = CARTESIAN_POINT ( 'NONE',  ( -18.49999999999996803, -9.321008403350131033, -107.7359382490779183 ) ) ;
#128354 = VERTEX_POINT ( 'NONE', #98351 ) ;
#128353 = DIRECTION ( 'NONE',  ( -1.000000000000000000, 0.000000000000000000, -0.000000000000000000 ) ) ;
#128355 = VECTOR ( 'NONE', #135668, 1000.000000000000000 ) ;
#128356 = DIRECTION ( 'NONE',  ( 0.000000000000000000, 0.8814952561688438326, -0.4721928772777332362 ) ) ;
#128357 = FACE_OUTER_BOUND ( 'NONE', #241769, .T. ) ;
#128358 = CARTESIAN_POINT ( 'NONE',  ( 18.49999999999999645, 77.83534155023627932, -91.46795619196132066 ) ) ;
#128359 = FACE_OUTER_BOUND ( 'NONE', #36760, .T. ) ;
#128360 = ORIENTED_EDGE ( 'NONE', *, *, #61619, .F. ) ;
#128361 = CARTESIAN_POINT ( 'NONE',  ( 20.05000000000002913, 68.75000000001251976, -182.6731074845244223 ) ) ;
#128362 = CARTESIAN_POINT ( 'NONE',  ( -23.15000000000000213, 74.00000000001151079, -49.24772940728643533 ) ) ;
#128363 = B_SPLINE_CURVE_WITH_KNOTS ( 'NONE', 3,
 ( #242657, #202263, #180141, #26203, #143562, #124016, #103136, #105690, #163147, #183976, #165720, #182713, #81003 ),
 .UNSPECIFIED., .F., .F.,
 ( 4, 3, 3, 3, 4 ),
 ( -3.224855718275878119E-06, 0.000000000000000000, 6.199515528665969596E-06, 4.034952380127002048E-05, 7.452715123699844260E-05 ),
 .UNSPECIFIED. ) ;
#128364 = VECTOR ( 'NONE', #67968, 1000.000000000000000 ) ;
#128365 = AXIS2_PLACEMENT_3D ( 'NONE', #92939, #228629, #91665 ) ;
#128366 = VECTOR ( 'NONE', #257603, 1000.000000000000000 ) ;
#128367 = ORIENTED_EDGE ( 'NONE', *, *, #29198, .F. ) ;
#128368 = VECTOR ( 'NONE', #136204, 1000.000000000000000 ) ;
#128369 = CARTESIAN_POINT ( 'NONE',  ( 18.59999999999999787, 77.83534155023598089, -57.96795619196132776 ) ) ;
#128370 = CARTESIAN_POINT ( 'NONE',  ( -18.59999999999999787, 46.01276039807270024, -256.6622985126337539 ) ) ;
#128371 = ORIENTED_EDGE ( 'NONE', *, *, #165090, .T. ) ;
#128372 = EDGE_CURVE ( 'NONE', #223851, #116446, #77523, .T. ) ;
#128373 = CARTESIAN_POINT ( 'NONE',  ( -21.07928932188134041, 6.328516656409859387, -66.90110485434540522 ) ) ;
#128374 = ORIENTED_EDGE ( 'NONE', *, *, #130286, .T. ) ;
#128375 = DIRECTION ( 'NONE',  ( 1.000000000000000000, 1.875376730785737719E-16, 0.000000000000000000 ) ) ;
#128376 = ORIENTED_EDGE ( 'NONE', *, *, #61072, .T. ) ;
#128377 = CARTESIAN_POINT ( 'NONE',  ( 20.95512820512820440, 8.876151316299271343, -54.75000000000000000 ) ) ;
#128378 = DIRECTION ( 'NONE',  ( 0.000000000000000000, 7.147358527629766941E-15, -1.000000000000000000 ) ) ;
#128379 = AXIS2_PLACEMENT_3D ( 'NONE', #74728, #252031, #175120 ) ;
#128380 = ORIENTED_EDGE ( 'NONE', *, *, #156813, .F. ) ;
#128381 = ORIENTED_EDGE ( 'NONE', *, *, #153750, .F. ) ;
#128383 = CARTESIAN_POINT ( 'NONE',  ( 23.50000000000005684, 83.97335046823651794, -34.66234602115918051 ) ) ;
#128382 = VECTOR ( 'NONE', #107122, 1000.000000000000000 ) ;
#128384 = ORIENTED_EDGE ( 'NONE', *, *, #209514, .T. ) ;
#128385 = EDGE_CURVE ( 'NONE', #65265, #57106, #138767, .T. ) ;
#128386 = CARTESIAN_POINT ( 'NONE',  ( 22.39999999999999858, 76.00000000001213607, -136.5231074845242745 ) ) ;
#128387 = EDGE_LOOP ( 'NONE', ( #167633, #20952, #88216, #85425 ) ) ;
#128388 = AXIS2_PLACEMENT_3D ( 'NONE', #230445, #171789, #54365 ) ;
#128389 = ORIENTED_EDGE ( 'NONE', *, *, #89724, .F. ) ;
#128390 = CARTESIAN_POINT ( 'NONE',  ( -21.05000000000000071, 76.00000000001162448, -65.22310748452436258 ) ) ;
#128391 = CARTESIAN_POINT ( 'NONE',  ( -18.50000000000000000, 77.73625713160946304, -124.9544551555067926 ) ) ;
#128392 = CARTESIAN_POINT ( 'NONE',  ( -18.49999999999998934, 38.23183114100727664, -261.0790748268677817 ) ) ;
#128393 = CARTESIAN_POINT ( 'NONE',  ( -23.25000000000000000, 11.75000000001115552, -67.00000000000004263 ) ) ;
#128394 = CARTESIAN_POINT ( 'NONE',  ( 21.06280952165552733, 65.37286769941061948, -57.31905359774562214 ) ) ;
#128395 = DIRECTION ( 'NONE',  ( 1.000000000000000000, -1.186688945009010077E-16, -8.286604613020808509E-31 ) ) ;
#128396 = ORIENTED_EDGE ( 'NONE', *, *, #90753, .F. ) ;
#128397 = CARTESIAN_POINT ( 'NONE',  ( 23.24999999999999289, 6.650000000011155876, -79.15000000000004832 ) ) ;
#128398 = FACE_OUTER_BOUND ( 'NONE', #230165, .T. ) ;
#128399 = DIRECTION ( 'NONE',  ( 1.000000000000000000, 0.000000000000000000, 0.000000000000000000 ) ) ;
#128400 = AXIS2_PLACEMENT_3D ( 'NONE', #116962, #196484, #17843 ) ;
#128401 = ORIENTED_EDGE ( 'NONE', *, *, #111742, .T. ) ;
#128402 = CARTESIAN_POINT ( 'NONE',  ( 22.50927854361889402, -0.1008580735143571466, -55.25043287397313208 ) ) ;
#128403 = VERTEX_POINT ( 'NONE', #218321 ) ;
#128404 = FACE_OUTER_BOUND ( 'NONE', #196348, .T. ) ;
#128405 = AXIS2_PLACEMENT_3D ( 'NONE', #87347, #65227, #109482 ) ;
#128406 = ORIENTED_EDGE ( 'NONE', *, *, #125872, .T. ) ;
#128407 = CIRCLE ( 'NONE', #207535, 0.09999999999999996392 ) ;
#128408 = DIRECTION ( 'NONE',  ( 1.000000000000000000, -0.000000000000000000, 0.000000000000000000 ) ) ;
#128409 = DIRECTION ( 'NONE',  ( -2.812466655313719426E-14, -0.3896596508880124654, -0.9209589331071350582 ) ) ;
#128410 = VERTEX_POINT ( 'NONE', #220898 ) ;
#128411 = ORIENTED_EDGE ( 'NONE', *, *, #78544, .F. ) ;
#128413 = ORIENTED_EDGE ( 'NONE', *, *, #59279, .F. ) ;
#128412 = CARTESIAN_POINT ( 'NONE',  ( -18.50000000000000000, 64.25000000001203659, -114.7731074845243882 ) ) ;
#128414 = CARTESIAN_POINT ( 'NONE',  ( 21.14999999999999858, 69.35000000001186038, -90.77310748452435973 ) ) ;
#128415 = VERTEX_POINT ( 'NONE', #236613 ) ;
#128416 = AXIS2_PLACEMENT_3D ( 'NONE', #134647, #173857, #72155 ) ;
#128417 = CARTESIAN_POINT ( 'NONE',  ( -22.42253884134832020, 0.001932351146464880492, -21.85039430265157634 ) ) ;
#128418 = ORIENTED_EDGE ( 'NONE', *, *, #149346, .F. ) ;
#128419 = DIRECTION ( 'NONE',  ( -1.000000000000000000, 2.952720810173289112E-16, 2.061873921506763405E-30 ) ) ;
#128420 = ADVANCED_FACE ( 'NONE', ( #57968 ), #86642, .T. ) ;
#128421 = AXIS2_PLACEMENT_3D ( 'NONE', #76070, #231322, #136019 ) ;
#128422 = AXIS2_PLACEMENT_3D ( 'NONE', #21099, #180159, #61484 ) ;
#128423 = VERTEX_POINT ( 'NONE', #38429 ) ;
#128425 = DIRECTION ( 'NONE',  ( -0.000000000000000000, 0.9908441862701591329, 0.1350103645451946055 ) ) ;
#128424 = AXIS2_PLACEMENT_3D ( 'NONE', #186634, #107073, #143633 ) ;
#128426 = EDGE_CURVE ( 'NONE', #131339, #109375, #219958, .T. ) ;
#128427 = FACE_OUTER_BOUND ( 'NONE', #153922, .T. ) ;
#128428 = EDGE_CURVE ( 'NONE', #187418, #88973, #42287, .T. ) ;
#128429 = CARTESIAN_POINT ( 'NONE',  ( -21.07928932188134041, 6.328516656404449492, -66.90110485434564680 ) ) ;
#128431 = ORIENTED_EDGE ( 'NONE', *, *, #116022, .T. ) ;
#128430 = CARTESIAN_POINT ( 'NONE',  ( -20.54999999999999716, 76.00000000001142553, -36.02310748452432421 ) ) ;
#128433 = VECTOR ( 'NONE', #244010, 1000.000000000000114 ) ;
#128432 = FACE_OUTER_BOUND ( 'NONE', #10150, .T. ) ;
#128434 = CARTESIAN_POINT ( 'NONE',  ( -22.48660254037843131, 12.63302488529805601, -223.3515224085914781 ) ) ;
#128435 = CARTESIAN_POINT ( 'NONE',  ( -16.94107738177414291, 10.01423928514777373, -121.4500000000000313 ) ) ;
#128437 = CARTESIAN_POINT ( 'NONE',  ( -17.80356949364355401, 59.42639550586179098, -223.0798372515704102 ) ) ;
#128436 = FACE_OUTER_BOUND ( 'NONE', #103264, .T. ) ;
#128438 = CARTESIAN_POINT ( 'NONE',  ( -20.89878130938411616, 65.67252876774583115, -164.4457041994994881 ) ) ;
#128439 = CARTESIAN_POINT ( 'NONE',  ( 20.94999999999999929, 76.00000000001242029, -165.9231074845243654 ) ) ;
#128441 = ADVANCED_FACE ( 'NONE', ( #140073 ), #219620, .F. ) ;
#128440 = AXIS2_PLACEMENT_3D ( 'NONE', #52259, #191827, #73164 ) ;
#128442 = DIRECTION ( 'NONE',  ( 1.000000000000000000, 0.000000000000000000, 0.000000000000000000 ) ) ;
#128443 = DIRECTION ( 'NONE',  ( -1.000000000000000000, -0.000000000000000000, -0.000000000000000000 ) ) ;
#128444 = EDGE_LOOP ( 'NONE', ( #230762, #67289, #45920, #88359, #183718, #135337 ) ) ;
#128445 = CIRCLE ( 'NONE', #249261, 0.1999999999999987899 ) ;
#128446 = AXIS2_PLACEMENT_3D ( 'NONE', #30290, #211485, #154123 ) ;
#128447 = CIRCLE ( 'NONE', #16058, 0.09999999999998898659 ) ;
#128448 = AXIS2_PLACEMENT_3D ( 'NONE', #231652, #131246, #132539 ) ;
#128449 = ORIENTED_EDGE ( 'NONE', *, *, #99233, .F. ) ;
#128450 = EDGE_LOOP ( 'NONE', ( #220531, #164008, #214572, #144979 ) ) ;
#128451 = VECTOR ( 'NONE', #81567, 1000.000000000000000 ) ;
#128452 = EDGE_CURVE ( 'NONE', #180952, #201418, #240479, .T. ) ;
#128453 = CARTESIAN_POINT ( 'NONE',  ( -20.85000000106584750, 64.25000000001220712, -143.3676028280510764 ) ) ;
#128454 = CARTESIAN_POINT ( 'NONE',  ( 20.95496329884391784, 65.43256679391929254, -162.4487975522395971 ) ) ;
#128455 = ORIENTED_EDGE ( 'NONE', *, *, #214480, .F. ) ;
#128456 = CARTESIAN_POINT ( 'NONE',  ( -18.59999999999999787, 14.81796439977981272, -236.5325475414793743 ) ) ;
#128457 = DIRECTION ( 'NONE',  ( 0.000000000000000000, 0.1618390714546044939, -0.9868171638914228216 ) ) ;
#128458 = PRODUCT_DEFINITION_SHAPE ( 'NONE', 'NONE',  #62861 ) ;
#128459 = DIRECTION ( 'NONE',  ( 0.000000000000000000, 6.982962677686266711E-15, -1.000000000000000000 ) ) ;
#128460 = ORIENTED_EDGE ( 'NONE', *, *, #29325, .T. ) ;
#128461 = ORIENTED_EDGE ( 'NONE', *, *, #42882, .F. ) ;
#128462 = CARTESIAN_POINT ( 'NONE',  ( -16.86578989773641979, 9.984809801269951990, -46.03533511337776929 ) ) ;
#128463 = SPHERICAL_SURFACE ( 'NONE', #163407, 0.1000000000000000056 ) ;
#128464 = ORIENTED_EDGE ( 'NONE', *, *, #12196, .T. ) ;
#128465 = DIRECTION ( 'NONE',  ( 1.441126678808781001E-14, -0.9876197685951241256, -0.1568667991644932258 ) ) ;
#128467 = ORIENTED_EDGE ( 'NONE', *, *, #42522, .F. ) ;
#128466 = CARTESIAN_POINT ( 'NONE',  ( 23.14999999999999858, 76.00000000001126921, -203.5231074845248997 ) ) ;
#128468 = CARTESIAN_POINT ( 'NONE',  ( 21.05000000000000071, 0.000000000000000000, 0.000000000000000000 ) ) ;
#128469 = CARTESIAN_POINT ( 'NONE',  ( -20.64999999999999858, 74.00000000001180922, -82.74772940728641402 ) ) ;
#128472 = ADVANCED_FACE ( 'NONE', ( #85218 ), #20058, .T. ) ;
#128471 = EDGE_LOOP ( 'NONE', ( #125296, #184552, #95379, #16141 ) ) ;
#128470 = CARTESIAN_POINT ( 'NONE',  ( 21.05000000000000071, 17.83900070254454562, -239.4698447713637677 ) ) ;
#128473 = AXIS2_PLACEMENT_3D ( 'NONE', #142604, #52183, #222129 ) ;
#128474 = SURFACE_STYLE_FILL_AREA ( #168931 ) ;
#128475 = CARTESIAN_POINT ( 'NONE',  ( 20.99551997958397465, 64.25000000001217870, -143.3714483468355638 ) ) ;
#128476 = CARTESIAN_POINT ( 'NONE',  ( -20.85000000000000142, 64.65966496992309942, -200.4475097531309586 ) ) ;
#128477 = CIRCLE ( 'NONE', #149348, 0.09999999999999939493 ) ;
#128478 = CARTESIAN_POINT ( 'NONE',  ( -16.84421487269769102, 12.41818349826529477, -211.2619443885827764 ) ) ;
#128480 = CARTESIAN_POINT ( 'NONE',  ( 20.11144452914179226, 9.933610851133071407, -108.3902934539540439 ) ) ;
#128479 = LINE ( 'NONE', #91907, #124164 ) ;
#128481 = DIRECTION ( 'NONE',  ( 0.000000000000000000, 0.000000000000000000, -1.000000000000000000 ) ) ;
#128482 = CIRCLE ( 'NONE', #170231, 0.1999999999999987899 ) ;
#128483 = LINE ( 'NONE', #172789, #205986 ) ;
#128484 = CARTESIAN_POINT ( 'NONE',  ( -21.05000000000000071, 36.52237217006333481, -249.3317055962219229 ) ) ;
#128485 = PLANE ( 'NONE',  #42812 ) ;
#128486 = ORIENTED_EDGE ( 'NONE', *, *, #83916, .F. ) ;
#128488 = ORIENTED_EDGE ( 'NONE', *, *, #255058, .F. ) ;
#128487 = CIRCLE ( 'NONE', #82655, 7.900000000000010125 ) ;
#128489 = EDGE_CURVE ( 'NONE', #156660, #68788, #68269, .T. ) ;
#128490 = DIRECTION ( 'NONE',  ( 1.000000000000000000, -0.000000000000000000, -0.000000000000000000 ) ) ;
#128491 = ORIENTED_EDGE ( 'NONE', *, *, #116483, .F. ) ;
#128492 = DIRECTION ( 'NONE',  ( 0.000000000000000000, 0.1332476588733589318, 0.9910827722268049644 ) ) ;
#128493 = ORIENTED_EDGE ( 'NONE', *, *, #243650, .F. ) ;
#128494 = CARTESIAN_POINT ( 'NONE',  ( -21.05000000000000071, 18.62343931468261360, -223.9512205031617498 ) ) ;
#128495 = DIRECTION ( 'NONE',  ( 1.000000000000000000, 0.000000000000000000, -0.000000000000000000 ) ) ;
#128496 = CIRCLE ( 'NONE', #41035, 0.09999999999999939493 ) ;
#128497 = EDGE_CURVE ( 'NONE', #231923, #227300, #136733, .T. ) ;
#128498 = VECTOR ( 'NONE', #159656, 1000.000000000000000 ) ;
#128499 = CIRCLE ( 'NONE', #45108, 0.1000000000000055844 ) ;
#128500 = ORIENTED_EDGE ( 'NONE', *, *, #216948, .F. ) ;
#128501 = TOROIDAL_SURFACE ( 'NONE', #11827, 0.2000000000000000111, 0.1000000000000000056 ) ;
#128502 = DIRECTION ( 'NONE',  ( 0.000000000000000000, 0.000000000000000000, -1.000000000000000000 ) ) ;
#128503 = SURFACE_STYLE_FILL_AREA ( #11125 ) ;
#128504 = ADVANCED_FACE ( 'NONE', ( #69565 ), #48687, .T. ) ;
#128505 = EDGE_LOOP ( 'NONE', ( #150789, #175188, #234335, #34056 ) ) ;
#128506 = VERTEX_POINT ( 'NONE', #206490 ) ;
#128507 = ORIENTED_EDGE ( 'NONE', *, *, #64973, .F. ) ;
#128508 = DIRECTION ( 'NONE',  ( -1.000000000000000000, 2.775557561562908012E-13, 0.000000000000000000 ) ) ;
#128509 =( NAMED_UNIT ( * ) SI_UNIT ( $, .STERADIAN. ) SOLID_ANGLE_UNIT ( ) );
#128510 = FACE_OUTER_BOUND ( 'NONE', #2813, .T. ) ;
#128511 = CARTESIAN_POINT ( 'NONE',  ( 12.42718393586866732, 27.00251997126095560, -233.7480822475820048 ) ) ;
#128512 = CARTESIAN_POINT ( 'NONE',  ( 20.94999999999999574, 2.902497314256400784, -208.4530536923346915 ) ) ;
#128513 = ADVANCED_FACE ( 'NONE', ( #128246 ), #165822, .F. ) ;
#128515 = CARTESIAN_POINT ( 'NONE',  ( -18.35668295345803713, 11.47316190337363118, -57.75000000000000711 ) ) ;
#128514 = FACE_OUTER_BOUND ( 'NONE', #192067, .T. ) ;
#128516 = CARTESIAN_POINT ( 'NONE',  ( -15.52965525596987995, 9.375538102059159939, -82.86987588099090374 ) ) ;
#128518 = ORIENTED_EDGE ( 'NONE', *, *, #172480, .T. ) ;
#128517 = CARTESIAN_POINT ( 'NONE',  ( -20.64999999999999858, 71.65000000001259650, -191.1731074845243654 ) ) ;
#128520 = CARTESIAN_POINT ( 'NONE',  ( -18.59999999999999787, 11.60000000001115872, -107.4282032302755852 ) ) ;
#128519 = CARTESIAN_POINT ( 'NONE',  ( 20.97250901189795513, 10.62456803371303593, -74.66454571696704079 ) ) ;
#128521 = DIRECTION ( 'NONE',  ( 1.000000000000000000, 0.000000000000000000, 0.000000000000000000 ) ) ;
#128522 = VERTEX_POINT ( 'NONE', #183090 ) ;
#128523 = CIRCLE ( 'NONE', #49409, 12.87499999999999822 ) ;
#128524 = PLANE ( 'NONE',  #135316 ) ;
#128526 = EDGE_CURVE ( 'NONE', #62147, #176943, #174208, .T. ) ;
#128525 = LINE ( 'NONE', #192350, #253863 ) ;
#128528 = ADVANCED_FACE ( 'NONE', ( #5690 ), #108674, .F. ) ;
#128527 = ORIENTED_EDGE ( 'NONE', *, *, #44323, .T. ) ;
#128529 = DIRECTION ( 'NONE',  ( -0.000000000000000000, -6.982962677686266711E-15, 1.000000000000000000 ) ) ;
#128530 = CARTESIAN_POINT ( 'NONE',  ( -21.05000000000000071, 74.16465844978715438, -57.96795619196135618 ) ) ;
#128531 = CARTESIAN_POINT ( 'NONE',  ( -21.14999999999999858, 87.75000000001165290, -69.52310748452424605 ) ) ;
#128532 = ORIENTED_EDGE ( 'NONE', *, *, #241486, .F. ) ;
#128533 = ORIENTED_EDGE ( 'NONE', *, *, #177512, .T. ) ;
#128534 = EDGE_CURVE ( 'NONE', #149638, #41516, #9566, .T. ) ;
#128535 = CARTESIAN_POINT ( 'NONE',  ( -16.87036670365549540, 66.01058118071064484, -157.5026676018264880 ) ) ;
#128536 = CARTESIAN_POINT ( 'NONE',  ( 18.49505816908824940, 85.43787255322283158, -62.74545028285337622 ) ) ;
#128538 = EDGE_CURVE ( 'NONE', #250267, #126765, #236689, .T. ) ;
#128537 = CARTESIAN_POINT ( 'NONE',  ( -20.91682497891423154, 10.32263460347359185, -206.5605957968671476 ) ) ;
#128539 = VERTEX_POINT ( 'NONE', #243040 ) ;
#128540 = EDGE_CURVE ( 'NONE', #139130, #234836, #257489, .T. ) ;
#128541 = CARTESIAN_POINT ( 'NONE',  ( -14.45422546970483957, 9.450602096099682825, -118.9438959630967219 ) ) ;
#128542 = LINE ( 'NONE', #3444, #108279 ) ;
#128543 = CYLINDRICAL_SURFACE ( 'NONE', #116156, 0.09999999999999939493 ) ;
#128544 = AXIS2_PLACEMENT_3D ( 'NONE', #41699, #217727, #59935 ) ;
#128545 = LINE ( 'NONE', #148112, #224026 ) ;
#128546 = AXIS2_PLACEMENT_3D ( 'NONE', #67175, #146678, #226204 ) ;
#128547 = CIRCLE ( 'NONE', #120217, 0.1000000000000013933 ) ;
#128548 = ORIENTED_EDGE ( 'NONE', *, *, #159471, .T. ) ;
#128549 = CARTESIAN_POINT ( 'NONE',  ( 20.94999027547553894, 10.29326151434211489, -38.95928225104149334 ) ) ;
#128551 = VERTEX_POINT ( 'NONE', #44850 ) ;
#128550 = LINE ( 'NONE', #208107, #221058 ) ;
#128552 = AXIS2_PLACEMENT_3D ( 'NONE', #97038, #77491, #20131 ) ;
#128554 = ADVANCED_FACE ( 'NONE', ( #223469 ), #66976, .T. ) ;
#128553 = FACE_OUTER_BOUND ( 'NONE', #225309, .T. ) ;
#128555 = LINE ( 'NONE', #105095, #155856 ) ;
#128556 = CYLINDRICAL_SURFACE ( 'NONE', #80262, 0.1000000000000028644 ) ;
#128557 = EDGE_CURVE ( 'NONE', #187086, #223496, #27306, .T. ) ;
#128558 = CARTESIAN_POINT ( 'NONE',  ( 18.49999999999999645, 74.26374286841418382, -57.95445515550683524 ) ) ;
#128559 = CARTESIAN_POINT ( 'NONE',  ( 20.27550659511088682, 9.216043722508848290, -12.65000000000000391 ) ) ;
#128560 = DIRECTION ( 'NONE',  ( 1.000000000000000000, 0.000000000000000000, -0.000000000000000000 ) ) ;
#128561 = DIRECTION ( 'NONE',  ( 0.000000000000000000, 0.9126074666063660468, 0.4088369013363524762 ) ) ;
#128562 = EDGE_LOOP ( 'NONE', ( #181962, #163957, #2428, #38480 ) ) ;
#128563 = CARTESIAN_POINT ( 'NONE',  ( -23.15000000000000213, 23.34004772283015328, -229.2004250369967338 ) ) ;
#128564 = FACE_OUTER_BOUND ( 'NONE', #221322, .T. ) ;
#128565 = FACE_OUTER_BOUND ( 'NONE', #186947, .T. ) ;
#128566 = AXIS2_PLACEMENT_3D ( 'NONE', #171410, #254708, #252175 ) ;
#128567 = VECTOR ( 'NONE', #27509, 1000.000000000000000 ) ;
#128568 = CARTESIAN_POINT ( 'NONE',  ( -20.64999999999999858, 85.00000000001207923, -126.6291383618717816 ) ) ;
#128569 = EDGE_CURVE ( 'NONE', #71101, #241787, #186660, .T. ) ;
#128570 = CIRCLE ( 'NONE', #99492, 0.2000000000000057288 ) ;
#128571 = DIRECTION ( 'NONE',  ( 1.000000000000000000, 0.000000000000000000, 0.000000000000000000 ) ) ;
#128572 = DIRECTION ( 'NONE',  ( 0.000000000000000000, 0.000000000000000000, 1.000000000000000000 ) ) ;
#128573 = AXIS2_PLACEMENT_3D ( 'NONE', #150603, #128465, #209277 ) ;
#128574 = EDGE_LOOP ( 'NONE', ( #201223, #97507, #156649, #225793 ) ) ;
#128575 = ORIENTED_EDGE ( 'NONE', *, *, #35503, .T. ) ;
#128576 = DIRECTION ( 'NONE',  ( -1.000000000000000000, -0.000000000000000000, -0.000000000000000000 ) ) ;
#128577 = DIRECTION ( 'NONE',  ( 1.000000000000000000, 0.000000000000000000, 0.000000000000000000 ) ) ;
#128578 = FACE_OUTER_BOUND ( 'NONE', #178462, .T. ) ;
#128579 =( BOUNDED_SURFACE ( )  B_SPLINE_SURFACE ( 3, 2, ( 
 ( #17288, #175115, #75967 ),
 ( #178955, #219315, #236315 ),
 ( #138474, #60239, #139763 ),
 ( #214197, #194659, #218016 ),
 ( #19857, #35583, #96774 ),
 ( #39438, #56378, #176373 ),
 ( #255833, #115091, #155537 ),
 ( #233767, #235047, #40726 ),
 ( #38138, #78515, #120265 ),
 ( #16016, #118956, #197185 ) ),
 .UNSPECIFIED., .F., .F., .F. ) 
 B_SPLINE_SURFACE_WITH_KNOTS ( ( 4, 2, 2, 2, 4 ),
 ( 3, 3 ),
 ( 0.002161241639767263849, 0.002579950749615834808, 0.002789305304540120288, 0.002893982582002263028, 0.002998659859464405768 ),
 ( 0.000000000000000000, 1.000000000000000000 ),
 .UNSPECIFIED. ) 
 GEOMETRIC_REPRESENTATION_ITEM ( )  RATIONAL_B_SPLINE_SURFACE ( (
 ( 1.000000000000000000, 0.7071067811865475727, 1.000000000000000000),
 ( 1.000000000000000000, 0.7632447400659811976, 1.000000000000000000),
 ( 1.000000000000000000, 0.8158073005116185383, 1.000000000000000000),
 ( 1.000000000000000000, 0.8906973462392635543, 1.000000000000000000),
 ( 1.000000000000000000, 0.9149408947804374970, 1.000000000000000000),
 ( 1.000000000000000000, 0.9493368785273612609, 1.000000000000000000),
 ( 1.000000000000000000, 0.9605194247158702625, 1.000000000000000000),
 ( 1.000000000000000000, 0.9803630264779076287, 1.000000000000000000),
 ( 1.000000000000000000, 0.9900844824272719835, 1.000000000000000000),
 ( 1.000000000000000000, 0.9894588281429380627, 1.000000000000000000) ) ) 
 REPRESENTATION_ITEM ( '' )  SURFACE ( )  );
#128580 = DIRECTION ( 'NONE',  ( -1.000000000000000000, -0.000000000000000000, -0.000000000000000000 ) ) ;
#128581 = LINE ( 'NONE', #165144, #5163 ) ;
#128582 = EDGE_CURVE ( 'NONE', #59315, #248135, #115911, .T. ) ;
#128583 = CARTESIAN_POINT ( 'NONE',  ( -20.64999999999999858, 49.36776662947724503, -253.7196102226803021 ) ) ;
#128584 = FACE_OUTER_BOUND ( 'NONE', #64913, .T. ) ;
#128585 = EDGE_CURVE ( 'NONE', #66263, #71912, #149242, .T. ) ;
#128586 = CIRCLE ( 'NONE', #124307, 0.1999999999999987899 ) ;
#128587 = AXIS2_PLACEMENT_3D ( 'NONE', #3659, #127470, #85733 ) ;
#128588 = CIRCLE ( 'NONE', #224258, 0.2000000000000057288 ) ;
#128589 = EDGE_LOOP ( 'NONE', ( #26491, #159968, #64087, #52010 ) ) ;
#128590 = CARTESIAN_POINT ( 'NONE',  ( 23.25000000000000000, 87.48912529308852015, -173.1231074845242688 ) ) ;
#128591 = EDGE_CURVE ( 'NONE', #174999, #21693, #74246, .T. ) ;
#128592 = ORIENTED_EDGE ( 'NONE', *, *, #135379, .T. ) ;
#128593 = CARTESIAN_POINT ( 'NONE',  ( -21.65000000000000213, 66.05000000001153637, -48.77310748452439526 ) ) ;
#128594 = CARTESIAN_POINT ( 'NONE',  ( 21.05000000000000426, -0.1000000000000014072, 6.477046381789850926 ) ) ;
#128595 = CIRCLE ( 'NONE', #78509, 6.329289321881370611 ) ;
#128596 = CARTESIAN_POINT ( 'NONE',  ( -20.54999999999999716, 1.115600667400684642E-11, -98.50000000000004263 ) ) ;
#128597 = FACE_OUTER_BOUND ( 'NONE', #129342, .T. ) ;
#128599 = EDGE_CURVE ( 'NONE', #163852, #246766, #235051, .T. ) ;
#128598 = CARTESIAN_POINT ( 'NONE',  ( -15.75000000000000355, 66.65000000001228386, -153.2731074845243882 ) ) ;
#128600 = CARTESIAN_POINT ( 'NONE',  ( 20.84999999999998721, 87.75000000001172396, -69.52310748452423184 ) ) ;
#128601 = CARTESIAN_POINT ( 'NONE',  ( 22.39999999999999858, 7.790779598384538929, -100.4000000000000341 ) ) ;
#128602 = ORIENTED_EDGE ( 'NONE', *, *, #244179, .T. ) ;
#128603 = CARTESIAN_POINT ( 'NONE',  ( -22.19999999999999929, -11.75000000000000000, 12.09999999999999609 ) ) ;
#128604 = DIRECTION ( 'NONE',  ( 0.000000000000000000, 0.9908441862701596881, -0.1350103645451904977 ) ) ;
#128605 = ADVANCED_FACE ( 'NONE', ( #154273 ), #134631, .F. ) ;
#128606 = DIRECTION ( 'NONE',  ( 0.000000000000000000, -0.1332476588733645106, -0.9910827722268042983 ) ) ;
#128607 = CYLINDRICAL_SURFACE ( 'NONE', #98016, 0.09999999999999939493 ) ;
#128608 = CIRCLE ( 'NONE', #149292, 0.09999999999998898659 ) ;
#128609 = VECTOR ( 'NONE', #136853, 1000.000000000000000 ) ;
#128610 = AXIS2_PLACEMENT_3D ( 'NONE', #255926, #44329, #236415 ) ;
#128611 = CARTESIAN_POINT ( 'NONE',  ( -22.59999985501179154, 11.74986979301414181, -167.4344013302005862 ) ) ;
#128612 = EDGE_CURVE ( 'NONE', #162622, #173033, #92955, .T. ) ;
#128615 = EDGE_CURVE ( 'NONE', #38916, #256420, #257309, .T. ) ;
#128614 = EDGE_CURVE ( 'NONE', #252148, #106883, #45169, .T. ) ;
#128613 = CIRCLE ( 'NONE', #170166, 0.09999999999999939493 ) ;
#128616 = EDGE_LOOP ( 'NONE', ( #38028, #170447, #115374, #2551 ) ) ;
#128617 = DIRECTION ( 'NONE',  ( -1.000000000000000000, -0.000000000000000000, -0.000000000000000000 ) ) ;
#128618 = FACE_OUTER_BOUND ( 'NONE', #77094, .T. ) ;
#128619 = EDGE_LOOP ( 'NONE', ( #129952, #107396, #72169, #198650, #172364, #11533, #56363 ) ) ;
#128620 = ADVANCED_FACE ( 'NONE', ( #31743 ), #232499, .F. ) ;
#128621 = ORIENTED_EDGE ( 'NONE', *, *, #56374, .T. ) ;
#128622 = DIRECTION ( 'NONE',  ( 0.000000000000000000, 0.000000000000000000, -1.000000000000000000 ) ) ;
#128623 = CARTESIAN_POINT ( 'NONE',  ( 23.14999999999999147, -4.149999999988843058, -167.4999999999999716 ) ) ;
#128624 = CIRCLE ( 'NONE', #232876, 0.09999999999999875655 ) ;
#128625 = DIRECTION ( 'NONE',  ( 2.978066053179069723E-16, 1.000000000000000000, 9.529811370173023114E-15 ) ) ;
#128626 = VERTEX_POINT ( 'NONE', #133384 ) ;
#128627 = CARTESIAN_POINT ( 'NONE',  ( -18.59999999999999787, -1.835341550213255957, -179.0551512925629538 ) ) ;
#128628 = CARTESIAN_POINT ( 'NONE',  ( 18.59999999999999076, 11.65000000001115943, -158.8500000000000227 ) ) ;
#128629 = AXIS2_PLACEMENT_3D ( 'NONE', #940, #123498, #23135 ) ;
#128630 = ORIENTED_EDGE ( 'NONE', *, *, #76753, .T. ) ;
#128631 = ADVANCED_FACE ( 'NONE', ( #91680 ), #16023, .T. ) ;
#128632 = EDGE_CURVE ( 'NONE', #9791, #45573, #215834, .T. ) ;
#128633 = TOROIDAL_SURFACE ( 'NONE', #7840, 12.97499999999999609, 0.1000000000000000056 ) ;
#128634 = VECTOR ( 'NONE', #9153, 1000.000000000000000 ) ;
#128635 = DIRECTION ( 'NONE',  ( 0.000000000000000000, 0.000000000000000000, 1.000000000000000000 ) ) ;
#128636 = EDGE_CURVE ( 'NONE', #97217, #12088, #14739, .T. ) ;
#128637 = EDGE_LOOP ( 'NONE', ( #174883, #197321, #187163, #64694 ) ) ;
#128638 = CARTESIAN_POINT ( 'NONE',  ( 21.12230431290520372, 75.99479014832319024, -142.9806741378172887 ) ) ;
#128639 = AXIS2_PLACEMENT_3D ( 'NONE', #162143, #104675, #43460 ) ;
#128640 = DIRECTION ( 'NONE',  ( 0.000000000000000000, -6.982962677686266711E-15, 1.000000000000000000 ) ) ;
#128642 = ORIENTED_EDGE ( 'NONE', *, *, #236387, .T. ) ;
#128641 = DIRECTION ( 'NONE',  ( 0.000000000000000000, 0.000000000000000000, -1.000000000000000000 ) ) ;
#128643 = EDGE_CURVE ( 'NONE', #156135, #223255, #178295, .T. ) ;
#128644 = DIRECTION ( 'NONE',  ( -1.000000000000000000, 0.000000000000000000, 0.000000000000000000 ) ) ;
#128646 = CARTESIAN_POINT ( 'NONE',  ( -21.05000000000000071, 14.88773611405353314, -236.3451124650200370 ) ) ;
#128645 = UNCERTAINTY_MEASURE_WITH_UNIT (LENGTH_MEASURE( 1.000000000000000082E-05 ), #93169, 'distance_accuracy_value', 'NONE');
#128647 = DIRECTION ( 'NONE',  ( -1.000000000000000000, 0.000000000000000000, 0.000000000000000000 ) ) ;
#128648 = PLANE ( 'NONE',  #76773 ) ;
#128649 = EDGE_CURVE ( 'NONE', #173153, #122837, #145108, .T. ) ;
#128650 = DIRECTION ( 'NONE',  ( 0.000000000000000000, -6.853228547068871147E-15, 1.000000000000000000 ) ) ;
#128651 = LINE ( 'NONE', #231601, #67918 ) ;
#128652 = DIRECTION ( 'NONE',  ( 0.000000000000000000, -0.4088369013363280513, 0.9126074666063769270 ) ) ;
#128654 = ORIENTED_EDGE ( 'NONE', *, *, #252259, .F. ) ;
#128653 = DIRECTION ( 'NONE',  ( -6.938893903907210707E-14, -0.9999176327611372095, -0.01283462868039623485 ) ) ;
#128655 = ORIENTED_EDGE ( 'NONE', *, *, #223145, .F. ) ;
#128657 = CARTESIAN_POINT ( 'NONE',  ( -21.05000000000000071, -1.162701749926853712, -75.10000000000003695 ) ) ;
#128656 = CARTESIAN_POINT ( 'NONE',  ( -23.25000000000000000, 75.39949836213489220, -250.2448839681187849 ) ) ;
#128659 = VERTEX_POINT ( 'NONE', #90384 ) ;
#128658 = DIRECTION ( 'NONE',  ( -0.000000000000000000, 0.000000000000000000, 1.000000000000000000 ) ) ;
#128660 = ORIENTED_EDGE ( 'NONE', *, *, #230553, .T. ) ;
#128661 = DIRECTION ( 'NONE',  ( 0.000000000000000000, 1.561251128379298294E-13, 1.000000000000000000 ) ) ;
#128662 = CIRCLE ( 'NONE', #253525, 0.09999999999999939493 ) ;
#128663 = CARTESIAN_POINT ( 'NONE',  ( -23.15000000000000213, 2.000000000011154189, -46.72462192276210402 ) ) ;
#128664 = CARTESIAN_POINT ( 'NONE',  ( -21.64999999999999858, 19.69766786220170829, -229.8585047820796490 ) ) ;
#128665 = DIRECTION ( 'NONE',  ( 0.000000000000000000, 6.853228547068871147E-15, -1.000000000000000000 ) ) ;
#128666 = EDGE_CURVE ( 'NONE', #31770, #205304, #190817, .T. ) ;
#128667 = DIRECTION ( 'NONE',  ( 0.000000000000000000, 0.000000000000000000, -1.000000000000000000 ) ) ;
#128668 = DIRECTION ( 'NONE',  ( 0.000000000000000000, -6.467318590049456648E-15, 1.000000000000000000 ) ) ;
#128669 = CIRCLE ( 'NONE', #8057, 0.09999999999999938105 ) ;
#128670 = AXIS2_PLACEMENT_3D ( 'NONE', #156316, #118451, #197962 ) ;
#128671 = FACE_OUTER_BOUND ( 'NONE', #191667, .T. ) ;
#128672 = EDGE_CURVE ( 'NONE', #242161, #139303, #178472, .T. ) ;
#128673 = VERTEX_POINT ( 'NONE', #130959 ) ;
#128674 = ORIENTED_EDGE ( 'NONE', *, *, #67987, .T. ) ;
#128675 = PLANE ( 'NONE',  #235448 ) ;
#128676 = AXIS2_PLACEMENT_3D ( 'NONE', #200442, #180884, #63479 ) ;
#128677 = EDGE_LOOP ( 'NONE', ( #221890, #182396, #167691, #144897 ) ) ;
#128678 = CARTESIAN_POINT ( 'NONE',  ( -23.15000000000000213, 1.115600667400684642E-11, -137.9000000000000341 ) ) ;
#128679 = ORIENTED_EDGE ( 'NONE', *, *, #181227, .F. ) ;
#128680 = DIRECTION ( 'NONE',  ( 1.000000000000000000, 0.000000000000000000, 0.000000000000000000 ) ) ;
#128681 = AXIS2_PLACEMENT_3D ( 'NONE', #72377, #54069, #111484 ) ;
#128682 =( BOUNDED_CURVE ( )  B_SPLINE_CURVE ( 3, ( #17291, #98058, #159371, #60242 ),
 .UNSPECIFIED., .F., .T. ) 
 B_SPLINE_CURVE_WITH_KNOTS ( ( 4, 4 ),
 ( 0.000000000000000000, 1.570796326794908992 ),
 .UNSPECIFIED. ) 
 CURVE ( )  GEOMETRIC_REPRESENTATION_ITEM ( )  RATIONAL_B_SPLINE_CURVE ( ( 1.000000000000000000, 0.8047378541243619399, 0.8047378541243619399, 1.000000000000000000 ) ) 
 REPRESENTATION_ITEM ( '' )  );
#128683 = DIRECTION ( 'NONE',  ( 1.000000000000000000, -2.952720810173289112E-16, -2.061873921506763405E-30 ) ) ;
#128684 = EDGE_CURVE ( 'NONE', #207244, #74308, #34462, .T. ) ;
#128685 = DIRECTION ( 'NONE',  ( 0.000000000000000000, 7.116814260417668513E-15, -1.000000000000000000 ) ) ;
#128686 = CARTESIAN_POINT ( 'NONE',  ( -20.54999999999999716, 20.02211948220868365, -235.8179285081017156 ) ) ;
#128687 = ORIENTED_EDGE ( 'NONE', *, *, #79587, .T. ) ;
#128688 = LINE ( 'NONE', #208228, #125580 ) ;
#128689 = ORIENTED_EDGE ( 'NONE', *, *, #205441, .F. ) ;
#128690 = CARTESIAN_POINT ( 'NONE',  ( -16.92989507731676824, 66.05000000001152216, -48.90560855391422734 ) ) ;
#128691 = CIRCLE ( 'NONE', #66133, 0.09999999999999999167 ) ;
#128692 = CARTESIAN_POINT ( 'NONE',  ( 18.42595409746882140, 8.812905803731212018, -245.4119551287989509 ) ) ;
#128693 = AXIS2_PLACEMENT_3D ( 'NONE', #39596, #1699, #100765 ) ;
#128694 = EDGE_LOOP ( 'NONE', ( #231335, #187248, #134620, #212918 ) ) ;
#128695 = DIRECTION ( 'NONE',  ( 1.000000000000000000, -0.000000000000000000, -0.000000000000000000 ) ) ;
#128696 = EDGE_LOOP ( 'NONE', ( #173668, #155786, #14064, #158283 ) ) ;
#128699 = ORIENTED_EDGE ( 'NONE', *, *, #233851, .T. ) ;
#128698 = FACE_OUTER_BOUND ( 'NONE', #219254, .T. ) ;
#128697 = DIRECTION ( 'NONE',  ( 0.7071067811865493491, -0.6824534298470356086, 0.1850873201762205378 ) ) ;
#128700 = EDGE_CURVE ( 'NONE', #18904, #149886, #145294, .T. ) ;
#128701 = CARTESIAN_POINT ( 'NONE',  ( -23.25000000000000000, 76.00000000001267608, -203.5231074845243597 ) ) ;
#128702 = TOROIDAL_SURFACE ( 'NONE', #178801, 0.4000000000000012990, 0.1000000000000000056 ) ;
#128703 = VERTEX_POINT ( 'NONE', #94388 ) ;
#128704 = FACE_OUTER_BOUND ( 'NONE', #23577, .T. ) ;
#128705 = ORIENTED_EDGE ( 'NONE', *, *, #169255, .T. ) ;
#128706 = LINE ( 'NONE', #208247, #86547 ) ;
#128707 = DIRECTION ( 'NONE',  ( 0.000000000000000000, -7.026728003956683390E-15, 1.000000000000000000 ) ) ;
#128708 = DIRECTION ( 'NONE',  ( -7.304098846218134667E-16, 0.4088369013363281068, -0.9126074666063770380 ) ) ;
#128709 = CARTESIAN_POINT ( 'NONE',  ( -21.05000000000000071, 1.261786168576181755, -175.5864989635454378 ) ) ;
#128710 = ORIENTED_EDGE ( 'NONE', *, *, #1149, .F. ) ;
#128711 = CARTESIAN_POINT ( 'NONE',  ( -21.05000000000000071, 87.75000000001143974, -38.92310748452424463 ) ) ;
#128712 = CARTESIAN_POINT ( 'NONE',  ( -16.80469485234340610, 14.14281391749209860, -219.2176264709205498 ) ) ;
#128713 = CARTESIAN_POINT ( 'NONE',  ( -12.29659703204452015, 66.64411154550971617, -153.7344645877464302 ) ) ;
#128714 = ORIENTED_EDGE ( 'NONE', *, *, #81222, .F. ) ;
#128715 = CARTESIAN_POINT ( 'NONE',  ( 20.94999999999999929, 85.00000000001179501, -79.41707660717668205 ) ) ;
#128716 = VERTEX_POINT ( 'NONE', #196077 ) ;
#128717 = CARTESIAN_POINT ( 'NONE',  ( -21.07928932188134041, 33.98134083355423485, -243.8161431329846778 ) ) ;
#128718 = ORIENTED_EDGE ( 'NONE', *, *, #130416, .T. ) ;
#128719 = LINE ( 'NONE', #25760, #189249 ) ;
#128720 = CARTESIAN_POINT ( 'NONE',  ( -23.15000000000000213, -9.000000000000001776, -23.60603087734756045 ) ) ;
#128722 = ORIENTED_EDGE ( 'NONE', *, *, #149145, .T. ) ;
#128721 = CARTESIAN_POINT ( 'NONE',  ( 23.24999999999999645, 1.115600667400684642E-11, -200.9999999999999432 ) ) ;
#128723 = DIRECTION ( 'NONE',  ( 0.000000000000000000, 0.000000000000000000, 1.000000000000000000 ) ) ;
#128724 = B_SPLINE_CURVE_WITH_KNOTS ( 'NONE', 3,
 ( #43676, #164904, #202736, #104885, #24130, #103615 ),
 .UNSPECIFIED., .F., .F.,
 ( 4, 2, 4 ),
 ( 0.000000000000000000, 0.0001497467027049214044, 0.0002994934054098428089 ),
 .UNSPECIFIED. ) ;
#128725 = DIRECTION ( 'NONE',  ( 0.000000000000000000, 0.000000000000000000, -1.000000000000000000 ) ) ;
#128726 = ADVANCED_FACE ( 'NONE', ( #73585 ), #112685, .T. ) ;
#128727 = DIRECTION ( 'NONE',  ( 1.000000000000000000, -0.000000000000000000, 0.000000000000000000 ) ) ;
#128728 = ORIENTED_EDGE ( 'NONE', *, *, #37036, .F. ) ;
#128729 = CIRCLE ( 'NONE', #91328, 0.09999999999999742428 ) ;
#128731 = VECTOR ( 'NONE', #87696, 1000.000000000000000 ) ;
#128730 = CARTESIAN_POINT ( 'NONE',  ( 22.00356870141233401, 68.74575763752109481, -203.5231074845244450 ) ) ;
#128732 = DIRECTION ( 'NONE',  ( 1.000000000000000000, 0.000000000000000000, -0.000000000000000000 ) ) ;
#128733 = VERTEX_POINT ( 'NONE', #175263 ) ;
#128734 = AXIS2_PLACEMENT_3D ( 'NONE', #76614, #216119, #94888 ) ;
#128736 = DIRECTION ( 'NONE',  ( 0.000000000000000000, -6.982962677686266711E-15, 1.000000000000000000 ) ) ;
#128735 = VECTOR ( 'NONE', #74942, 999.9999999999998863 ) ;
#128737 = ORIENTED_EDGE ( 'NONE', *, *, #168902, .T. ) ;
#128738 = PLANE ( 'NONE',  #187683 ) ;
#128739 = AXIS2_PLACEMENT_3D ( 'NONE', #254537, #193326, #217984 ) ;
#128740 = CARTESIAN_POINT ( 'NONE',  ( 18.39999999999999503, 70.35000000001187459, -90.37310748452433984 ) ) ;
#128741 = EDGE_CURVE ( 'NONE', #187198, #215216, #253442, .T. ) ;
#128742 = EDGE_CURVE ( 'NONE', #64319, #194507, #186837, .T. ) ;
#128745 = ORIENTED_EDGE ( 'NONE', *, *, #71824, .T. ) ;
#128744 = EDGE_LOOP ( 'NONE', ( #90230, #67963, #257972, #177582 ) ) ;
#128743 = LINE ( 'NONE', #12663, #209762 ) ;
#128747 = AXIS2_PLACEMENT_3D ( 'NONE', #18077, #19375, #79319 ) ;
#128746 = CYLINDRICAL_SURFACE ( 'NONE', #178855, 4.049999999999998046 ) ;
#128748 = VECTOR ( 'NONE', #174757, 1000.000000000000000 ) ;
#128749 = DIRECTION ( 'NONE',  ( 0.000000000000000000, -0.000000000000000000, -1.000000000000000000 ) ) ;
#128750 = DIRECTION ( 'NONE',  ( 0.000000000000000000, 0.6728971962616412394, 0.7397360091703134577 ) ) ;
#128751 = TOROIDAL_SURFACE ( 'NONE', #178861, 0.2000000000000000111, 0.1000000000000000056 ) ;
#128753 = CARTESIAN_POINT ( 'NONE',  ( -23.39999999999994529, 83.97335046823651794, -34.66234602115918051 ) ) ;
#128752 = CARTESIAN_POINT ( 'NONE',  ( -16.87683809663752399, 66.15000000001261071, -190.8731074845244393 ) ) ;
#128754 = LINE ( 'NONE', #68774, #3398 ) ;
#128755 = DIRECTION ( 'NONE',  ( -2.602085213965226419E-14, -0.000000000000000000, 1.000000000000000000 ) ) ;
#128756 = EDGE_CURVE ( 'NONE', #229898, #29396, #12320, .T. ) ;
#128757 = DIRECTION ( 'NONE',  ( 1.000000000000000000, 0.000000000000000000, 0.000000000000000000 ) ) ;
#128758 = CARTESIAN_POINT ( 'NONE',  ( -20.54999999999999716, -8.730841121484170131, -124.4019252810157070 ) ) ;
#128759 = ORIENTED_EDGE ( 'NONE', *, *, #108636, .T. ) ;
#128760 = ORIENTED_EDGE ( 'NONE', *, *, #138957, .F. ) ;
#128761 = EDGE_CURVE ( 'NONE', #51212, #30385, #13592, .T. ) ;
#128762 = CARTESIAN_POINT ( 'NONE',  ( -20.85000000106584750, 64.25000000001175238, -76.36760282805070688 ) ) ;
#128765 = EDGE_LOOP ( 'NONE', ( #25892, #163872, #204470, #9977, #209602, #115718, #101676, #237119, #110750, #204999, #100731 ) ) ;
#128764 = EDGE_CURVE ( 'NONE', #47876, #149809, #178672, .T. ) ;
#128763 = DIRECTION ( 'NONE',  ( 1.000000000000000000, 0.000000000000000000, 0.000000000000000000 ) ) ;
#128766 = VERTEX_POINT ( 'NONE', #253460 ) ;
#128767 = ORIENTED_EDGE ( 'NONE', *, *, #143200, .F. ) ;
#128768 = DIRECTION ( 'NONE',  ( -0.000000000000000000, 0.9875055080513808203, -0.1575844902526395142 ) ) ;
#128769 = ADVANCED_FACE ( 'NONE', ( #154417 ), #136065, .F. ) ;
#128770 = ORIENTED_EDGE ( 'NONE', *, *, #10910, .T. ) ;
#128771 = ADVANCED_FACE ( 'NONE', ( #134784 ), #31887, .T. ) ;
#128772 = CARTESIAN_POINT ( 'NONE',  ( -16.89146115310546392, 66.04855675435578632, -149.1682850655701884 ) ) ;
#128773 = DIRECTION ( 'NONE',  ( 0.000000000000000000, 0.000000000000000000, 1.000000000000000000 ) ) ;
#128774 = AXIS2_PLACEMENT_3D ( 'NONE', #73163, #152700, #190536 ) ;
#128776 = ORIENTED_EDGE ( 'NONE', *, *, #135923, .T. ) ;
#128775 = ORIENTED_EDGE ( 'NONE', *, *, #169667, .F. ) ;
#128777 = ORIENTED_EDGE ( 'NONE', *, *, #83583, .T. ) ;
#128778 = CARTESIAN_POINT ( 'NONE',  ( 21.05000000000000071, 10.72371710471867701, -45.65000000000000568 ) ) ;
#128779 = ORIENTED_EDGE ( 'NONE', *, *, #92358, .T. ) ;
#128780 = ORIENTED_EDGE ( 'NONE', *, *, #5710, .F. ) ;
#128781 = CARTESIAN_POINT ( 'NONE',  ( -16.89146115310546392, 14.16143799253418400, -219.2594773961805288 ) ) ;
#128782 = DIRECTION ( 'NONE',  ( -3.787827842127534447E-15, -0.7397360091702729346, -0.6728971962616859814 ) ) ;
#128783 = CARTESIAN_POINT ( 'NONE',  ( -23.15000000000000213, -9.499999999988848032, -143.8939691226524644 ) ) ;
#128785 = ORIENTED_EDGE ( 'NONE', *, *, #3775, .F. ) ;
#128784 = CARTESIAN_POINT ( 'NONE',  ( -18.39999999999999858, -9.599999999988849453, -174.1001893912220737 ) ) ;
#128786 = AXIS2_PLACEMENT_3D ( 'NONE', #22660, #162167, #6915 ) ;
#128787 = DIRECTION ( 'NONE',  ( 0.000000000000000000, -6.982962677686266711E-15, 1.000000000000000000 ) ) ;
#128788 = DIRECTION ( 'NONE',  ( 1.000000000000000000, 2.952720810173289112E-16, -0.000000000000000000 ) ) ;
#128790 = ORIENTED_EDGE ( 'NONE', *, *, #115906, .F. ) ;
#128789 = DIRECTION ( 'NONE',  ( 1.000000000000000000, 0.000000000000000000, 0.000000000000000000 ) ) ;
#128791 = DIRECTION ( 'NONE',  ( -1.000000000000000000, -0.000000000000000000, -0.000000000000000000 ) ) ;
#128792 = ORIENTED_EDGE ( 'NONE', *, *, #257486, .T. ) ;
#128793 = CARTESIAN_POINT ( 'NONE',  ( 23.24999999999999645, 73.90000000001141700, -36.02310748452433842 ) ) ;
#128795 = ADVANCED_FACE ( 'NONE', ( #231360 ), #35740, .F. ) ;
#128794 = ORIENTED_EDGE ( 'NONE', *, *, #90372, .F. ) ;
#128796 = CARTESIAN_POINT ( 'NONE',  ( -20.97625342178423224, 18.71344899774613424, -226.7788045575993863 ) ) ;
#128797 = CARTESIAN_POINT ( 'NONE',  ( -21.05000000000000071, 74.83729825007431202, -162.0231074845243597 ) ) ;
#128798 = ORIENTED_EDGE ( 'NONE', *, *, #156278, .F. ) ;
#128801 = PLANE ( 'NONE',  #8213 ) ;
#128800 = DIRECTION ( 'NONE',  ( 0.000000000000000000, -6.982962677686266711E-15, 1.000000000000000000 ) ) ;
#128799 = AXIS2_PLACEMENT_3D ( 'NONE', #93238, #150659, #210628 ) ;
#128802 = CARTESIAN_POINT ( 'NONE',  ( 18.49999999999998934, 48.66983769917126779, -228.4584249288054423 ) ) ;
#128803 = CARTESIAN_POINT ( 'NONE',  ( -18.40000000000000213, 70.35000000001181775, -82.17310748452435121 ) ) ;
#128804 = CARTESIAN_POINT ( 'NONE',  ( -20.54999999999999716, 26.26625913865096251, -241.7830784256010759 ) ) ;
#128805 = AXIS2_PLACEMENT_3D ( 'NONE', #215512, #101957, #197240 ) ;
#128806 = ORIENTED_EDGE ( 'NONE', *, *, #5441, .F. ) ;
#128807 = ORIENTED_EDGE ( 'NONE', *, *, #4987, .T. ) ;
#128808 = ADVANCED_FACE ( 'NONE', ( #232650 ), #194812, .F. ) ;
#128809 = LINE ( 'NONE', #188764, #172102 ) ;
#128810 = DIRECTION ( 'NONE',  ( 0.000000000000000000, 6.982962677686266711E-15, -1.000000000000000000 ) ) ;
#128811 = ORIENTED_EDGE ( 'NONE', *, *, #152703, .T. ) ;
#128812 = CARTESIAN_POINT ( 'NONE',  ( 20.95512820512820440, 10.62384868372303615, -79.15000000000004832 ) ) ;
#128813 = ORIENTED_EDGE ( 'NONE', *, *, #252432, .F. ) ;
#128814 = CYLINDRICAL_SURFACE ( 'NONE', #31619, 0.09999999999999939493 ) ;
#128815 = AXIS2_PLACEMENT_3D ( 'NONE', #15966, #237555, #36818 ) ;
#128816 = AXIS2_PLACEMENT_3D ( 'NONE', #114163, #11222, #212000 ) ;
#128817 = DIRECTION ( 'NONE',  ( 1.000000000000000000, 0.000000000000000000, 0.000000000000000000 ) ) ;
#128818 = EDGE_LOOP ( 'NONE', ( #151293, #155522, #231748, #84422, #78635, #74654, #58776, #252469, #139449, #63518, #106503, #158031, #157820 ) ) ;
#128819 = CARTESIAN_POINT ( 'NONE',  ( 20.94999999999999929, 65.27628289530470340, -148.7731074845244450 ) ) ;
#128820 = EDGE_CURVE ( 'NONE', #212844, #251754, #32747, .T. ) ;
#128822 = ORIENTED_EDGE ( 'NONE', *, *, #52061, .T. ) ;
#128821 = TOROIDAL_SURFACE ( 'NONE', #212027, 11.70000000000000107, 0.1000000000000000056 ) ;
#128823 = ORIENTED_EDGE ( 'NONE', *, *, #98920, .F. ) ;
#128824 = AXIS2_PLACEMENT_3D ( 'NONE', #132030, #91622, #112484 ) ;
#128825 = ORIENTED_EDGE ( 'NONE', *, *, #102325, .T. ) ;
#128826 = CIRCLE ( 'NONE', #91412, 11.65000000000000036 ) ;
#128827 = CARTESIAN_POINT ( 'NONE',  ( -22.57320508075687115, 55.98745301258801987, -232.8057040749260977 ) ) ;
#128828 = DIRECTION ( 'NONE',  ( -1.000000000000000000, 0.000000000000000000, 0.000000000000000000 ) ) ;
#128829 = CARTESIAN_POINT ( 'NONE',  ( 21.05000000000000071, -1.489567864901280680, -194.6304332222954372 ) ) ;
#128830 = LINE ( 'NONE', #104094, #81940 ) ;
#128831 = AXIS2_PLACEMENT_3D ( 'NONE', #194558, #14629, #135819 ) ;
#128832 = EDGE_CURVE ( 'NONE', #173897, #189309, #176597, .T. ) ;
#128834 = DIRECTION ( 'NONE',  ( 0.000000000000000000, 0.9126074666063780372, 0.4088369013363259419 ) ) ;
#128833 = CARTESIAN_POINT ( 'NONE',  ( -22.40000000000000568, 10.80758397488571099, -226.8651660546161111 ) ) ;
#128836 = ORIENTED_EDGE ( 'NONE', *, *, #213328, .F. ) ;
#128835 = DIRECTION ( 'NONE',  ( 1.000000000000000000, 0.000000000000000000, 0.000000000000000000 ) ) ;
#128837 = CARTESIAN_POINT ( 'NONE',  ( 20.04999999999999716, 67.25000000001149658, -48.67310748452438673 ) ) ;
#128838 = EDGE_LOOP ( 'NONE', ( #172246, #173144, #99231, #111581 ) ) ;
#128839 = DIRECTION ( 'NONE',  ( 0.000000000000000000, -6.938893903907222067E-15, 1.000000000000000000 ) ) ;
#128840 = ORIENTED_EDGE ( 'NONE', *, *, #90539, .T. ) ;
#128841 = ORIENTED_EDGE ( 'NONE', *, *, #211534, .T. ) ;
#128842 = LINE ( 'NONE', #229226, #29676 ) ;
#128843 = FACE_OUTER_BOUND ( 'NONE', #154847, .T. ) ;
#128845 = EDGE_CURVE ( 'NONE', #104106, #117472, #123602, .T. ) ;
#128844 = CARTESIAN_POINT ( 'NONE',  ( -23.25000000000000000, 77.85161776048025217, -24.41991776492064758 ) ) ;
#128846 = ADVANCED_FACE ( 'NONE', ( #241616 ), #220146, .F. ) ;
#128847 = CYLINDRICAL_SURFACE ( 'NONE', #145692, 0.09999999999999939493 ) ;
#128848 = CIRCLE ( 'NONE', #74713, 0.4000000000000010214 ) ;
#128849 = CARTESIAN_POINT ( 'NONE',  ( 23.14999999999999858, 1.115600667400684642E-11, -200.9999999999999432 ) ) ;
#128850 = ORIENTED_EDGE ( 'NONE', *, *, #101034, .F. ) ;
#128851 = ORIENTED_EDGE ( 'NONE', *, *, #257192, .F. ) ;
#128852 = ADVANCED_FACE ( 'NONE', ( #98208 ), #60398, .F. ) ;
#128853 = CARTESIAN_POINT ( 'NONE',  ( -20.64999999999999858, 48.89266972451527948, -253.5637804087949121 ) ) ;
#128854 = ORIENTED_EDGE ( 'NONE', *, *, #59147, .F. ) ;
#128855 = CARTESIAN_POINT ( 'NONE',  ( -22.32929514600008503, 0.09907567812507747651, -126.4213524346235147 ) ) ;
#128856 = LINE ( 'NONE', #105389, #65464 ) ;
#128857 = EDGE_LOOP ( 'NONE', ( #33752, #185803 ) ) ;
#128858 = DIRECTION ( 'NONE',  ( 0.000000000000000000, 1.000000000000000000, 0.000000000000000000 ) ) ;
#128859 = CARTESIAN_POINT ( 'NONE',  ( 21.17356465864818915, -1.270133162812157934, -194.7032591620159678 ) ) ;
#128860 = DIRECTION ( 'NONE',  ( -1.284434275755705296E-16, 0.7071067811865471286, -0.7071067811865479058 ) ) ;
#128861 = CARTESIAN_POINT ( 'NONE',  ( -20.15000000000000568, 66.70857864377522617, -182.2731074845244166 ) ) ;
#128862 = EDGE_LOOP ( 'NONE', ( #58031, #50068, #22499, #135475 ) ) ;
#128863 = CARTESIAN_POINT ( 'NONE',  ( 20.85000000000000142, -1.835859311443637010, -45.00443916879852679 ) ) ;
#128864 = B_SPLINE_CURVE_WITH_KNOTS ( 'NONE', 3,
 ( #44926, #60610, #240554, #234794, #209122, #68346, #210432, #47465, #8372, #227402, #167465, #246961, #245690, #87869, #129598, #26663, #125732, #147884, #48764, #30516, #91753, #27961, #107460, #206563, #31812, #190884 ),
 .UNSPECIFIED., .F., .F.,
 ( 4, 2, 2, 2, 2, 2, 2, 2, 2, 2, 2, 2, 4 ),
 ( 0.005476422646581359521, 0.006160811967703593017, 0.006845201288825827381, 0.007187395949386929384, 0.007529590609948032254, 0.007871785270509135124, 0.008213979931070237994, 0.008556174591631339130, 0.008898369252192442000, 0.009240563912753543135, 0.009582758573314646006, 0.01026714789443684828, 0.01095153721555904881 ),
 .UNSPECIFIED. ) ;
#128865 = CARTESIAN_POINT ( 'NONE',  ( -18.39999999999999858, 85.40000000001276703, -215.2731074845243029 ) ) ;
#128866 = DIRECTION ( 'NONE',  ( 1.000000000000000000, 0.000000000000000000, -0.000000000000000000 ) ) ;
#128867 = AXIS2_PLACEMENT_3D ( 'NONE', #135696, #116165, #99128 ) ;
#128868 = CARTESIAN_POINT ( 'NONE',  ( -21.05000000000000071, 1.835341550235567887, -78.55515129256302487 ) ) ;
#128869 = DIRECTION ( 'NONE',  ( 0.2834754621636358940, -0.2834754621636437211, 0.9161240771326893961 ) ) ;
#128870 = CIRCLE ( 'NONE', #145583, 0.1000000000000002554 ) ;
#128871 = CARTESIAN_POINT ( 'NONE',  ( 20.94999999999999929, 1.115600667400684642E-11, -69.00000000000000000 ) ) ;
#128872 = EDGE_CURVE ( 'NONE', #176500, #153561, #136936, .T. ) ;
#128873 = ORIENTED_EDGE ( 'NONE', *, *, #137025, .T. ) ;
#128874 = DIRECTION ( 'NONE',  ( 1.000000000000000000, 0.000000000000000000, 0.000000000000000000 ) ) ;
#128875 = VERTEX_POINT ( 'NONE', #119109 ) ;
#128876 = EDGE_CURVE ( 'NONE', #158029, #41121, #181655, .T. ) ;
#128877 = EDGE_CURVE ( 'NONE', #67768, #218279, #81232, .T. ) ;
#128878 = FACE_OUTER_BOUND ( 'NONE', #62590, .T. ) ;
#128879 = DIRECTION ( 'NONE',  ( -1.000000000000000000, 0.000000000000000000, 0.000000000000000000 ) ) ;
#128880 = CARTESIAN_POINT ( 'NONE',  ( -23.25000000000000000, 11.65000000001115588, -167.4999999999999716 ) ) ;
#128881 = ORIENTED_EDGE ( 'NONE', *, *, #77576, .T. ) ;
#128882 = LINE ( 'NONE', #186289, #171692 ) ;
#128883 = CONICAL_SURFACE ( 'NONE', #191248, 4.000000000000000000, 0.7853981633974487231 ) ;
#128884 = SPHERICAL_SURFACE ( 'NONE', #144047, 0.1000000000000000056 ) ;
#128885 = CARTESIAN_POINT ( 'NONE',  ( 21.05000000000000071, 1.115600667400684642E-11, -138.0000000000000284 ) ) ;
#128886 = PLANE ( 'NONE',  #46285 ) ;
#128887 = ADVANCED_FACE ( 'NONE', ( #102077 ), #245083, .T. ) ;
#128888 = CIRCLE ( 'NONE', #145424, 0.09999999999999986677 ) ;
#128889 = CARTESIAN_POINT ( 'NONE',  ( 22.49436431346199683, 75.93309647029019516, -181.6730584321778110 ) ) ;
#128890 = ORIENTED_EDGE ( 'NONE', *, *, #127284, .T. ) ;
#128891 = ORIENTED_EDGE ( 'NONE', *, *, #208436, .F. ) ;
#128892 = DIRECTION ( 'NONE',  ( -0.000000000000000000, -0.9126074666063770380, -0.4088369013363281068 ) ) ;
#128893 = CARTESIAN_POINT ( 'NONE',  ( 20.90000000000000213, -1.885425182446133885, -11.49641995933507843 ) ) ;
#128894 = CARTESIAN_POINT ( 'NONE',  ( -18.39999999999999858, -9.519327731081281385, -107.4729763765593589 ) ) ;
#128895 = CARTESIAN_POINT ( 'NONE',  ( 18.59999999999999076, 54.48300931968434213, -228.8005724072070564 ) ) ;
#128896 = ORIENTED_EDGE ( 'NONE', *, *, #137989, .T. ) ;
#128897 = CARTESIAN_POINT ( 'NONE',  ( 22.50014994444008209, 11.74971973190328534, -33.41691984328090825 ) ) ;
#128898 = EDGE_CURVE ( 'NONE', #253814, #145079, #207846, .T. ) ;
#128899 = CARTESIAN_POINT ( 'NONE',  ( -18.59999999999999787, -8.175168544775697654, 10.42878401658402510 ) ) ;
#128900 = ORIENTED_EDGE ( 'NONE', *, *, #104417, .T. ) ;
#128901 = FACE_OUTER_BOUND ( 'NONE', #118086, .T. ) ;
#128902 = TOROIDAL_SURFACE ( 'NONE', #62252, 0.4000000000000010214, 0.1000000000000000056 ) ;
#128903 = EDGE_CURVE ( 'NONE', #91045, #249684, #228530, .T. ) ;
#128904 = EDGE_LOOP ( 'NONE', ( #32542, #233013, #229764, #164956 ) ) ;
#128905 = VERTEX_POINT ( 'NONE', #197341 ) ;
#128906 = ADVANCED_FACE ( 'NONE', ( #42150 ), #22584, .F. ) ;
#128907 = ORIENTED_EDGE ( 'NONE', *, *, #207621, .F. ) ;
#128908 = CARTESIAN_POINT ( 'NONE',  ( -18.40000000000000213, 5.650000000011139001, -46.15000000000000568 ) ) ;
#128909 = DIRECTION ( 'NONE',  ( 0.000000000000000000, 0.2128009952263630322, -0.9770955615653309501 ) ) ;
#128910 = CARTESIAN_POINT ( 'NONE',  ( 21.05000000000000071, -8.999999999988842703, -124.1060308773475924 ) ) ;
#128911 = CARTESIAN_POINT ( 'NONE',  ( 23.40000000000005187, 79.88763423575340994, -7.282924647898262549 ) ) ;
#128912 = DIRECTION ( 'NONE',  ( 1.000000000000000000, 0.000000000000000000, 0.000000000000000000 ) ) ;
#128913 = EDGE_CURVE ( 'NONE', #148934, #194645, #211772, .T. ) ;
#128914 = SPHERICAL_SURFACE ( 'NONE', #120294, 0.1000000000000000056 ) ;
#128915 = CARTESIAN_POINT ( 'NONE',  ( -16.93255653858138388, 9.998451453977155623, -12.58164336798968108 ) ) ;
#128917 = DIRECTION ( 'NONE',  ( 0.000000000000000000, 0.8127272543710951647, -0.5826443254700255370 ) ) ;
#128916 = CARTESIAN_POINT ( 'NONE',  ( -20.64999999999999858, 68.85000000001205933, -124.1731074845243370 ) ) ;
#128918 = DIRECTION ( 'NONE',  ( 0.000000000000000000, 0.000000000000000000, 1.000000000000000000 ) ) ;
#128919 = EDGE_CURVE ( 'NONE', #202163, #104681, #28661, .T. ) ;
#128920 = CARTESIAN_POINT ( 'NONE',  ( -23.15000000000000213, 1.999999999999998224, -13.22462192276210224 ) ) ;
#128921 = CARTESIAN_POINT ( 'NONE',  ( -23.15000000000000213, 2.499999999999998668, -20.27537807723789953 ) ) ;
#128922 = AXIS2_PLACEMENT_3D ( 'NONE', #5733, #85262, #244358 ) ;
#128924 = CARTESIAN_POINT ( 'NONE',  ( -20.94999999999999929, -11.29603075032412640, -97.45210084033617193 ) ) ;
#128923 = AXIS2_PLACEMENT_3D ( 'NONE', #117279, #96404, #100244 ) ;
#128925 = ORIENTED_EDGE ( 'NONE', *, *, #183919, .F. ) ;
#128926 = ORIENTED_EDGE ( 'NONE', *, *, #158339, .F. ) ;
#128927 = CARTESIAN_POINT ( 'NONE',  ( -21.04386569057651357, 11.75000000001136513, -93.64283735177980361 ) ) ;
#128928 = FACE_OUTER_BOUND ( 'NONE', #149648, .T. ) ;
#128930 = CARTESIAN_POINT ( 'NONE',  ( 18.59999999999999076, 69.60000000001207354, -126.5926828544627654 ) ) ;
#128929 = FACE_OUTER_BOUND ( 'NONE', #76801, .T. ) ;
#128931 = ADVANCED_FACE ( 'NONE', ( #59084 ), #138627, .F. ) ;
#128932 = AXIS2_PLACEMENT_3D ( 'NONE', #183728, #24675, #61204 ) ;
#128933 = EDGE_CURVE ( 'NONE', #204719, #49363, #45347, .T. ) ;
#128934 = CARTESIAN_POINT ( 'NONE',  ( 22.39999999999999503, 64.35000000001213039, -136.5231074845243597 ) ) ;
#128935 = DIRECTION ( 'NONE',  ( 0.000000000000000000, 0.000000000000000000, 1.000000000000000000 ) ) ;
#128936 = CARTESIAN_POINT ( 'NONE',  ( -21.51976009735018991, 6.752178271738374704, -199.5294475661460467 ) ) ;
#128937 = ORIENTED_EDGE ( 'NONE', *, *, #219703, .F. ) ;
#128938 = ORIENTED_EDGE ( 'NONE', *, *, #110300, .T. ) ;
#128939 = AXIS2_PLACEMENT_3D ( 'NONE', #97704, #39071, #118605 ) ;
#128941 = AXIS2_PLACEMENT_3D ( 'NONE', #161730, #45612, #130264 ) ;
#128940 = DIRECTION ( 'NONE',  ( 0.000000000000000000, 0.000000000000000000, -1.000000000000000000 ) ) ;
#128942 = ORIENTED_EDGE ( 'NONE', *, *, #43470, .F. ) ;
#128943 = DIRECTION ( 'NONE',  ( 0.000000000000000000, -1.000000000000000000, 0.000000000000000000 ) ) ;
#128944 = ADVANCED_FACE ( 'NONE', ( #10715 ), #245483, .T. ) ;
#128945 = EDGE_CURVE ( 'NONE', #42435, #50990, #61926, .T. ) ;
#128946 = CARTESIAN_POINT ( 'NONE',  ( 20.94999999999999929, -1.362429037182151470, -208.8888812479211765 ) ) ;
#128947 = VERTEX_POINT ( 'NONE', #185497 ) ;
#128948 = DIRECTION ( 'NONE',  ( 0.000000000000000000, 0.2128009952263678062, -0.9770955615653298398 ) ) ;
#128949 = EDGE_CURVE ( 'NONE', #77793, #141325, #49831, .T. ) ;
#128950 = VERTEX_POINT ( 'NONE', #85071 ) ;
#128951 = CARTESIAN_POINT ( 'NONE',  ( 20.94999999999999929, 69.55000000001207638, -126.5060803140843291 ) ) ;
#128952 = DIRECTION ( 'NONE',  ( 0.000000000000000000, 0.1686199900910312910, -0.9856811345164826488 ) ) ;
#128953 = CARTESIAN_POINT ( 'NONE',  ( 23.14999999999999503, 64.25000000001179501, -81.67310748452439384 ) ) ;
#128954 = CARTESIAN_POINT ( 'NONE',  ( -20.64999999999999858, 26.38661631484796644, -241.7796963509253203 ) ) ;
#128955 = FACE_OUTER_BOUND ( 'NONE', #62374, .T. ) ;
#128956 = EDGE_CURVE ( 'NONE', #245427, #244742, #170305, .T. ) ;
#128957 = CARTESIAN_POINT ( 'NONE',  ( 20.12500000000000000, 11.25287472715600146, -206.8511660127314826 ) ) ;
#128958 = CARTESIAN_POINT ( 'NONE',  ( -17.11825945287482753, 9.950000000011138823, -79.75000000000004263 ) ) ;
#128959 = CARTESIAN_POINT ( 'NONE',  ( -22.39999999999999858, 76.00000000001200817, -110.8138870828977218 ) ) ;
#128962 = VERTEX_POINT ( 'NONE', #124252 ) ;
#128961 = EDGE_CURVE ( 'NONE', #69705, #207624, #191132, .T. ) ;
#128960 = CARTESIAN_POINT ( 'NONE',  ( 20.97565083910961548, 65.52538259873327320, -128.9451643079358405 ) ) ;
#128964 = FACE_OUTER_BOUND ( 'NONE', #18798, .T. ) ;
#128963 = DIRECTION ( 'NONE',  ( 1.000000000000000000, -0.000000000000000000, -0.000000000000000000 ) ) ;
#128965 = EDGE_LOOP ( 'NONE', ( #211408, #86514, #238164, #54363 ) ) ;
#128967 = VERTEX_POINT ( 'NONE', #64266 ) ;
#128966 = CYLINDRICAL_SURFACE ( 'NONE', #131809, 0.09999999999999939493 ) ;
#128968 = VECTOR ( 'NONE', #101305, 1000.000000000000000 ) ;
#128969 = VERTEX_POINT ( 'NONE', #223319 ) ;
#128970 = DIRECTION ( 'NONE',  ( 0.000000000000000000, 0.000000000000000000, 1.000000000000000000 ) ) ;
#128971 = CARTESIAN_POINT ( 'NONE',  ( 22.39999999999999503, 65.49880482333749399, -241.8610443077474486 ) ) ;
#128972 = CARTESIAN_POINT ( 'NONE',  ( 22.48508240969612615, 75.95372358549481362, -81.17311821609789035 ) ) ;
#128973 = DIRECTION ( 'NONE',  ( -1.000000000000000000, 0.000000000000000000, -0.000000000000000000 ) ) ;
#128974 = CONICAL_SURFACE ( 'NONE', #74831, 7.750000000000023981, 0.7853981633974531640 ) ;
#128975 = CARTESIAN_POINT ( 'NONE',  ( -18.50000000000000000, 56.01362831242967388, -232.7091905853083347 ) ) ;
#128976 = ADVANCED_FACE ( 'NONE', ( #206351 ), #66835, .F. ) ;
#128977 = DIRECTION ( 'NONE',  ( -1.000000000000000000, 0.000000000000000000, 0.000000000000000000 ) ) ;
#128978 = LINE ( 'NONE', #110686, #100359 ) ;
#128979 = CARTESIAN_POINT ( 'NONE',  ( -18.59999999999999787, 77.14957036958807635, -162.2071950000224092 ) ) ;
#128980 = DIRECTION ( 'NONE',  ( 1.000000000000000000, 0.000000000000000000, 0.000000000000000000 ) ) ;
#128981 = EDGE_CURVE ( 'NONE', #45344, #3631, #132665, .T. ) ;
#128982 = ORIENTED_EDGE ( 'NONE', *, *, #162737, .T. ) ;
#128983 = ORIENTED_EDGE ( 'NONE', *, *, #204957, .T. ) ;
#128984 = DIRECTION ( 'NONE',  ( 0.000000000000000000, -7.272083257015735086E-15, 1.000000000000000000 ) ) ;
#128985 = AXIS2_PLACEMENT_3D ( 'NONE', #245335, #184064, #5398 ) ;
#128986 = ORIENTED_EDGE ( 'NONE', *, *, #1267, .F. ) ;
#128987 = CARTESIAN_POINT ( 'NONE',  ( -21.44999999999999929, 7.150000000000000355, -21.15000000000000213 ) ) ;
#128989 = ORIENTED_EDGE ( 'NONE', *, *, #145227, .T. ) ;
#128988 = AXIS2_PLACEMENT_3D ( 'NONE', #163265, #241505, #221910 ) ;
#128990 = FACE_OUTER_BOUND ( 'NONE', #145777, .T. ) ;
#128991 = VECTOR ( 'NONE', #108946, 1000.000000000000000 ) ;
#128992 = LINE ( 'NONE', #127710, #171782 ) ;
#128993 = DIRECTION ( 'NONE',  ( -0.000000000000000000, 1.000000000000000000, -0.000000000000000000 ) ) ;
#128994 = EDGE_CURVE ( 'NONE', #14935, #66123, #166006, .T. ) ;
#128995 = DIRECTION ( 'NONE',  ( 0.000000000000000000, 0.000000000000000000, 1.000000000000000000 ) ) ;
#128996 = CARTESIAN_POINT ( 'NONE',  ( -21.14999999999999858, -11.64999999998884483, -67.00000000000004263 ) ) ;
#128997 = EDGE_LOOP ( 'NONE', ( #207719, #223026, #26195, #129054 ) ) ;
#128998 = AXIS2_PLACEMENT_3D ( 'NONE', #113445, #215113, #117303 ) ;
#128999 = CIRCLE ( 'NONE', #112433, 0.1000000000000028644 ) ;
#129000 = DIRECTION ( 'NONE',  ( 1.000000000000000000, -0.000000000000000000, -0.000000000000000000 ) ) ;
#129001 = CARTESIAN_POINT ( 'NONE',  ( 20.99999999999999645, 63.27875933230978234, -213.1799721866121047 ) ) ;
#129002 = PLANE ( 'NONE',  #98741 ) ;
#129003 = CARTESIAN_POINT ( 'NONE',  ( 13.99999999999999822, 13.18880795147152618, -215.2702608532411830 ) ) ;
#129004 = ORIENTED_EDGE ( 'NONE', *, *, #61494, .T. ) ;
#129006 = CARTESIAN_POINT ( 'NONE',  ( -20.54999999999999716, 44.87429835298446790, -237.9265065269792103 ) ) ;
#129005 = LINE ( 'NONE', #225498, #199871 ) ;
#129007 = ORIENTED_EDGE ( 'NONE', *, *, #114172, .F. ) ;
#129010 = VERTEX_POINT ( 'NONE', #105929 ) ;
#129009 = DIRECTION ( 'NONE',  ( 0.000000000000000000, 0.2617529984165152257, 0.9651348961777124202 ) ) ;
#129008 = FACE_OUTER_BOUND ( 'NONE', #247980, .T. ) ;
#129011 = AXIS2_PLACEMENT_3D ( 'NONE', #77814, #158685, #200350 ) ;
#129012 = CARTESIAN_POINT ( 'NONE',  ( -23.15000000000000213, 85.00000000001188027, -93.62913836187181005 ) ) ;
#129013 = VECTOR ( 'NONE', #2212, 1000.000000000000114 ) ;
#129014 = AXIS2_PLACEMENT_3D ( 'NONE', #139715, #22379, #101866 ) ;
#129015 = AXIS2_PLACEMENT_3D ( 'NONE', #38672, #255089, #157368 ) ;
#129016 = AXIS2_PLACEMENT_3D ( 'NONE', #3553, #166521, #162651 ) ;
#129017 = DIRECTION ( 'NONE',  ( 1.000000000000000000, 0.000000000000000000, -0.000000000000000000 ) ) ;
#129018 = CARTESIAN_POINT ( 'NONE',  ( -18.59999999999999787, 7.250000000011155521, -188.8499999999999659 ) ) ;
#129019 = VERTEX_POINT ( 'NONE', #48547 ) ;
#129020 = CARTESIAN_POINT ( 'NONE',  ( -22.39999999999999858, 1.115600667400684642E-11, -167.3999999999999773 ) ) ;
#129021 = AXIS2_PLACEMENT_3D ( 'NONE', #233986, #239134, #74953 ) ;
#129022 = DIRECTION ( 'NONE',  ( -0.000000000000000000, -0.8814952561688430555, 0.4721928772777346239 ) ) ;
#129024 = DIRECTION ( 'NONE',  ( 1.000000000000000000, -0.000000000000000000, -0.000000000000000000 ) ) ;
#129023 = CARTESIAN_POINT ( 'NONE',  ( -22.48660254037843487, 11.65000000000000036, 0.04999999999998249595 ) ) ;
#129026 = ORIENTED_EDGE ( 'NONE', *, *, #86983, .F. ) ;
#129025 = DIRECTION ( 'NONE',  ( 0.7071067811865475727, 0.7071067811865475727, 4.937700262164531476E-15 ) ) ;
#129027 = ORIENTED_EDGE ( 'NONE', *, *, #70521, .T. ) ;
#129028 = CYLINDRICAL_SURFACE ( 'NONE', #70056, 0.1000000000000028644 ) ;
#129029 = FACE_OUTER_BOUND ( 'NONE', #257357, .T. ) ;
#129030 = DIRECTION ( 'NONE',  ( 0.000000000000000000, 0.000000000000000000, -1.000000000000000000 ) ) ;
#129031 = EDGE_LOOP ( 'NONE', ( #38080, #103986 ) ) ;
#129032 = CARTESIAN_POINT ( 'NONE',  ( -16.80100914604133777, 9.943149094114717812, -188.3170441272875451 ) ) ;
#129033 = DIRECTION ( 'NONE',  ( 0.000000000000000000, -0.000000000000000000, 1.000000000000000000 ) ) ;
#129034 = DIRECTION ( 'NONE',  ( 0.000000000000000000, -0.9770955615653312831, -0.2128009952263614224 ) ) ;
#129035 = ORIENTED_EDGE ( 'NONE', *, *, #257772, .T. ) ;
#129036 = FACE_OUTER_BOUND ( 'NONE', #8084, .T. ) ;
#129037 = CIRCLE ( 'NONE', #62394, 1.899999999999999023 ) ;
#129038 = EDGE_CURVE ( 'NONE', #46619, #221229, #86359, .T. ) ;
#129039 = VECTOR ( 'NONE', #122646, 1000.000000000000000 ) ;
#129040 = ORIENTED_EDGE ( 'NONE', *, *, #257192, .T. ) ;
#129041 = CARTESIAN_POINT ( 'NONE',  ( 18.49999999999999645, -1.164121893241208960, -41.41484808557160591 ) ) ;
#129042 = CARTESIAN_POINT ( 'NONE',  ( -22.94999999999999929, -1.885425182446134107, -11.59641995933507808 ) ) ;
#129043 = CIRCLE ( 'NONE', #58282, 0.09999999999999939493 ) ;
#129044 = EDGE_LOOP ( 'NONE', ( #9898, #91215, #134661, #97466 ) ) ;
#129045 = VERTEX_POINT ( 'NONE', #30285 ) ;
#129046 = CARTESIAN_POINT ( 'NONE',  ( 20.94999999999999929, 77.83534155023646406, -124.9679561919612922 ) ) ;
#129047 = EDGE_LOOP ( 'NONE', ( #239208, #101388, #217744 ) ) ;
#129049 = EDGE_LOOP ( 'NONE', ( #41878, #48708, #196556, #208934 ) ) ;
#129048 = CARTESIAN_POINT ( 'NONE',  ( -22.59999970745345976, -0.009356377315826230542, -155.7494867923307424 ) ) ;
#129050 = ORIENTED_EDGE ( 'NONE', *, *, #86107, .T. ) ;
#129052 = ADVANCED_FACE ( 'NONE', ( #29034 ), #232634, .T. ) ;
#129051 = AXIS2_PLACEMENT_3D ( 'NONE', #168734, #224782, #104814 ) ;
#129055 = VERTEX_POINT ( 'NONE', #164658 ) ;
#129054 = ORIENTED_EDGE ( 'NONE', *, *, #109448, .F. ) ;
#129053 = DIRECTION ( 'NONE',  ( -1.000000000000000000, -0.000000000000000000, -0.000000000000000000 ) ) ;
#129056 = VECTOR ( 'NONE', #169516, 1000.000000000000000 ) ;
#129057 = CARTESIAN_POINT ( 'NONE',  ( -18.46919391072059113, -9.670724388266654259, -107.1738035317995070 ) ) ;
#129058 = ORIENTED_EDGE ( 'NONE', *, *, #98227, .T. ) ;
#129059 = DIRECTION ( 'NONE',  ( 1.000000000000000000, 0.000000000000000000, 0.000000000000000000 ) ) ;
#129060 = DIRECTION ( 'NONE',  ( 0.000000000000000000, -0.9126074666063770380, -0.4088369013363281068 ) ) ;
#129061 = CARTESIAN_POINT ( 'NONE',  ( -18.59999999999999787, 77.16270174995064224, -195.4231074845243370 ) ) ;
#129062 = CARTESIAN_POINT ( 'NONE',  ( 20.94999999999999929, 36.65892442174935439, -249.5511627012433848 ) ) ;
#129063 = ORIENTED_EDGE ( 'NONE', *, *, #155929, .F. ) ;
#129064 = EDGE_LOOP ( 'NONE', ( #32165, #68068 ) ) ;
#129065 = ADVANCED_FACE ( 'NONE', ( #205029 ), #88944, .F. ) ;
#129066 = CARTESIAN_POINT ( 'NONE',  ( -23.25000000000000000, -6.388372595096676321, -212.0629706944429813 ) ) ;
#129069 = ORIENTED_EDGE ( 'NONE', *, *, #108229, .F. ) ;
#129068 = EDGE_CURVE ( 'NONE', #200753, #92332, #240989, .T. ) ;
#129067 = CARTESIAN_POINT ( 'NONE',  ( 18.49999999999964473, 63.70204416476671128, -209.2375263527553102 ) ) ;
#129070 = DIRECTION ( 'NONE',  ( 0.000000000000000000, 0.000000000000000000, -1.000000000000000000 ) ) ;
#129072 = VERTEX_POINT ( 'NONE', #148956 ) ;
#129071 = CARTESIAN_POINT ( 'NONE',  ( -21.44999999999999929, 53.04688186230822566, -234.1557136682916394 ) ) ;
#129073 = EDGE_LOOP ( 'NONE', ( #122071, #194229, #174701, #71746 ) ) ;
#129074 = DIRECTION ( 'NONE',  ( 0.000000000000000000, 0.000000000000000000, 1.000000000000000000 ) ) ;
#129075 = ADVANCED_FACE ( 'NONE', ( #208906 ), #147652, .T. ) ;
#129076 = ORIENTED_EDGE ( 'NONE', *, *, #229977, .F. ) ;
#129077 = CIRCLE ( 'NONE', #204068, 0.09999999999999939493 ) ;
#129078 = EDGE_CURVE ( 'NONE', #50212, #7516, #203757, .T. ) ;
#129079 = AXIS2_PLACEMENT_3D ( 'NONE', #249574, #111339, #231299 ) ;
#129080 = CARTESIAN_POINT ( 'NONE',  ( -16.80621392010912984, 9.942202577518864715, -180.1895919654171507 ) ) ;
#129081 = LINE ( 'NONE', #233336, #198685 ) ;
#129083 = VERTEX_POINT ( 'NONE', #217546 ) ;
#129082 = ORIENTED_EDGE ( 'NONE', *, *, #225598, .F. ) ;
#129084 = ORIENTED_EDGE ( 'NONE', *, *, #247463, .T. ) ;
#129085 = CARTESIAN_POINT ( 'NONE',  ( -16.86133551771148475, 9.950000000011137047, -54.30134343454665924 ) ) ;
#129087 = ORIENTED_EDGE ( 'NONE', *, *, #167454, .F. ) ;
#129086 = EDGE_CURVE ( 'NONE', #171727, #178174, #24726, .T. ) ;
#129088 = ORIENTED_EDGE ( 'NONE', *, *, #26939, .T. ) ;
#129089 = LINE ( 'NONE', #189059, #30292 ) ;
#129090 = ORIENTED_EDGE ( 'NONE', *, *, #173494, .T. ) ;
#129091 = FACE_OUTER_BOUND ( 'NONE', #161220, .T. ) ;
#129093 = CYLINDRICAL_SURFACE ( 'NONE', #140117, 0.1000000000000028644 ) ;
#129092 = DIRECTION ( 'NONE',  ( 0.000000000000000000, -6.982962677686266711E-15, 1.000000000000000000 ) ) ;
#129094 = CARTESIAN_POINT ( 'NONE',  ( 20.99142135623731065, 62.99095723518624368, -207.1734234082434796 ) ) ;
#129095 = CARTESIAN_POINT ( 'NONE',  ( 23.24999999999999289, 11.65000000000000746, 11.75000000000000000 ) ) ;
#129096 = EDGE_LOOP ( 'NONE', ( #244531, #224609, #122647 ) ) ;
#129098 = ADVANCED_FACE ( 'NONE', ( #238415 ), #257923, .F. ) ;
#129097 = ORIENTED_EDGE ( 'NONE', *, *, #193658, .F. ) ;
#129100 = CIRCLE ( 'NONE', #170846, 3.899999999999999467 ) ;
#129099 = FACE_OUTER_BOUND ( 'NONE', #196442, .T. ) ;
#129101 = DIRECTION ( 'NONE',  ( -0.000000000000000000, 0.9126074666063770380, 0.4088369013363281068 ) ) ;
#129102 = AXIS2_PLACEMENT_3D ( 'NONE', #20090, #203843, #159598 ) ;
#129103 = AXIS2_PLACEMENT_3D ( 'NONE', #42502, #37400, #140310 ) ;
#129104 = CIRCLE ( 'NONE', #74956, 0.1000000000000018374 ) ;
#129105 = VERTEX_POINT ( 'NONE', #16821 ) ;
#129106 = CIRCLE ( 'NONE', #16692, 0.1000000000000028644 ) ;
#129107 = LINE ( 'NONE', #9155, #63566 ) ;
#129108 = ORIENTED_EDGE ( 'NONE', *, *, #186153, .F. ) ;
#129109 = ORIENTED_EDGE ( 'NONE', *, *, #114851, .F. ) ;
#129110 = CARTESIAN_POINT ( 'NONE',  ( -12.25000000000000178, 66.15000000001228386, -153.2731074845244166 ) ) ;
#129111 = DIRECTION ( 'NONE',  ( 1.713247197920696616E-14, 0.9876197685951252359, -0.1568667991644863424 ) ) ;
#129112 = ORIENTED_EDGE ( 'NONE', *, *, #111955, .F. ) ;
#129113 = CARTESIAN_POINT ( 'NONE',  ( -20.94999999999999929, 4.193200906077805712, -212.0298262072164164 ) ) ;
#129114 = VERTEX_POINT ( 'NONE', #40245 ) ;
#129115 = DIRECTION ( 'NONE',  ( -1.000000000000000000, 0.000000000000000000, -0.000000000000000000 ) ) ;
#129116 = DIRECTION ( 'NONE',  ( 0.000000000000000000, 0.8700118002898393765, -0.4930308989875104575 ) ) ;
#129118 = SPHERICAL_SURFACE ( 'NONE', #216301, 0.1000000000000000056 ) ;
#129117 = CARTESIAN_POINT ( 'NONE',  ( 20.94999999999999574, 74.26374286841446803, -91.45445515550682103 ) ) ;
#129119 = CARTESIAN_POINT ( 'NONE',  ( 19.90621891164687440, 11.75000000001116263, -91.82844527787746358 ) ) ;
#129121 = CARTESIAN_POINT ( 'NONE',  ( -20.54999999999999716, -8.999999999988846255, -177.3939691226524076 ) ) ;
#129120 = AXIS2_PLACEMENT_3D ( 'NONE', #7303, #206796, #86822 ) ;
#129122 = DIRECTION ( 'NONE',  ( 0.000000000000000000, 0.4721928772777351790, 0.8814952561688427224 ) ) ;
#129123 = VECTOR ( 'NONE', #33790, 1000.000000000000114 ) ;
#129124 = CARTESIAN_POINT ( 'NONE',  ( 23.14999999999999858, 64.40000000001145963, -42.95131071479990226 ) ) ;
#129125 = ORIENTED_EDGE ( 'NONE', *, *, #182768, .T. ) ;
#129127 = EDGE_CURVE ( 'NONE', #67356, #52417, #57988, .T. ) ;
#129126 = B_SPLINE_CURVE_WITH_KNOTS ( 'NONE', 3,
 ( #208635, #189056, #10426, #89938, #70429, #149948, #44420 ),
 .UNSPECIFIED., .F., .F.,
 ( 4, 3, 4 ),
 ( 0.000000000000000000, 4.520325912680733322E-05, 5.794988040901469109E-05 ),
 .UNSPECIFIED. ) ;
#129129 = ORIENTED_EDGE ( 'NONE', *, *, #81127, .T. ) ;
#129128 = VERTEX_POINT ( 'NONE', #32883 ) ;
#129130 = VERTEX_POINT ( 'NONE', #231064 ) ;
#129131 = EDGE_CURVE ( 'NONE', #53024, #96904, #141217, .T. ) ;
#129132 = CARTESIAN_POINT ( 'NONE',  ( -23.15000000000000213, 78.37638820354418101, -229.1444560783390898 ) ) ;
#129133 = CARTESIAN_POINT ( 'NONE',  ( 21.15000000000004476, 84.00000000001119815, -34.86056257560453986 ) ) ;
#129134 = EDGE_CURVE ( 'NONE', #86852, #197986, #175902, .T. ) ;
#129135 = EDGE_CURVE ( 'NONE', #208557, #37324, #153743, .T. ) ;
#129137 = CARTESIAN_POINT ( 'NONE',  ( -22.59999999999999787, 11.74956712350054744, -33.39914163090129762 ) ) ;
#129136 = CARTESIAN_POINT ( 'NONE',  ( 18.59999999999999432, 48.14768554360777841, -246.4498133360871179 ) ) ;
#129138 = CARTESIAN_POINT ( 'NONE',  ( 20.85000000000000142, 68.87972903831379767, -32.36354444268504693 ) ) ;
#129139 = EDGE_LOOP ( 'NONE', ( #104007, #97826, #15935, #77952, #153620 ) ) ;
#129140 = DIRECTION ( 'NONE',  ( -0.000000000000000000, 0.000000000000000000, 1.000000000000000000 ) ) ;
#129141 = ORIENTED_EDGE ( 'NONE', *, *, #31328, .F. ) ;
#129142 = CARTESIAN_POINT ( 'NONE',  ( -21.05000000000000426, -0.01771943330858751983, 6.441084688471355513 ) ) ;
#129143 = DIRECTION ( 'NONE',  ( 3.469446951953515108E-14, 0.000000000000000000, 1.000000000000000000 ) ) ;
#129144 = EDGE_CURVE ( 'NONE', #99386, #148681, #182925, .T. ) ;
#129145 = CARTESIAN_POINT ( 'NONE',  ( 18.39999999999998082, 64.52683809665015247, -194.2731074845244450 ) ) ;
#129146 = EDGE_LOOP ( 'NONE', ( #7076, #191325, #245217, #147332 ) ) ;
#129147 = CIRCLE ( 'NONE', #233218, 11.64999999999998970 ) ;
#129148 = EDGE_CURVE ( 'NONE', #112295, #206700, #66392, .T. ) ;
#129149 = EDGE_CURVE ( 'NONE', #166275, #21828, #249336, .T. ) ;
#129150 = FACE_OUTER_BOUND ( 'NONE', #46196, .T. ) ;
#129151 = CARTESIAN_POINT ( 'NONE',  ( -21.05000000000000071, 77.25000000001209344, -128.5231074845242745 ) ) ;
#129152 = ORIENTED_EDGE ( 'NONE', *, *, #46746, .F. ) ;
#129153 = ORIENTED_EDGE ( 'NONE', *, *, #1617, .F. ) ;
#129154 = CARTESIAN_POINT ( 'NONE',  ( -1.820710678118658388, -9.929289321870186313, -58.15000000000000568 ) ) ;
#129155 = CARTESIAN_POINT ( 'NONE',  ( -20.54999999999999716, 74.00000000001229239, -156.7984855617622770 ) ) ;
#129156 = ADVANCED_FACE ( 'NONE', ( #139289 ), #197993, .F. ) ;
#129157 = AXIS2_PLACEMENT_3D ( 'NONE', #246219, #187549, #10181 ) ;
#129158 = DIRECTION ( 'NONE',  ( -0.000000000000000000, 6.982962677686266711E-15, -1.000000000000000000 ) ) ;
#129159 = DIRECTION ( 'NONE',  ( 0.000000000000000000, 0.000000000000000000, -1.000000000000000000 ) ) ;
#129160 = CARTESIAN_POINT ( 'NONE',  ( 20.94999999999999929, 5.000000000011153745, -155.5947339810869323 ) ) ;
#129161 = DIRECTION ( 'NONE',  ( 0.000000000000000000, 0.9916376685811618685, -0.1290532225514649800 ) ) ;
#129162 = ORIENTED_EDGE ( 'NONE', *, *, #41246, .T. ) ;
#129163 = CYLINDRICAL_SURFACE ( 'NONE', #38290, 0.09999999999999939493 ) ;
#129164 = DIRECTION ( 'NONE',  ( 0.000000000000000000, -0.8814952561688428334, 0.4721928772777349570 ) ) ;
#129165 = ADVANCED_FACE ( 'NONE', ( #117190 ), #51078, .T. ) ;
#129167 = CARTESIAN_POINT ( 'NONE',  ( 21.30000000000002558, 76.00000000001216449, -140.5731074845242858 ) ) ;
#129166 = DIRECTION ( 'NONE',  ( 0.000000000000000000, 0.3896596508880098009, 0.9209589331071361684 ) ) ;
#129168 = CARTESIAN_POINT ( 'NONE',  ( -20.94999999999999929, 68.97833521811159585, -65.88954208262707368 ) ) ;
#129169 = CARTESIAN_POINT ( 'NONE',  ( -20.65000000000000568, 45.23934133962703186, -237.7629717664446787 ) ) ;
#129170 = CARTESIAN_POINT ( 'NONE',  ( -23.25000000000000000, 7.128833340094563376, -233.7327013124401276 ) ) ;
#129171 = CARTESIAN_POINT ( 'NONE',  ( 20.93975676684922504, 10.31104185824063002, -139.5204516983105805 ) ) ;
#129172 = EDGE_CURVE ( 'NONE', #217539, #232829, #151532, .T. ) ;
#129173 = ADVANCED_FACE ( 'NONE', ( #130650 ), #29629, .F. ) ;
#129174 = AXIS2_PLACEMENT_3D ( 'NONE', #190195, #28598, #191496 ) ;
#129175 = EDGE_LOOP ( 'NONE', ( #194277, #165572, #164793, #87762 ) ) ;
#129176 = CIRCLE ( 'NONE', #45773, 0.09999999999999860389 ) ;
#129177 = ADVANCED_FACE ( 'NONE', ( #101418 ), #232822, .T. ) ;
#129178 = CIRCLE ( 'NONE', #162502, 0.2000000000000057288 ) ;
#129179 = ADVANCED_FACE ( 'NONE', ( #80595 ), #3642, .T. ) ;
#129180 = EDGE_CURVE ( 'NONE', #57171, #7237, #121072, .T. ) ;
#129181 = AXIS2_PLACEMENT_3D ( 'NONE', #106700, #109270, #145831 ) ;
#129182 = VECTOR ( 'NONE', #29875, 1000.000000000000000 ) ;
#129183 = CARTESIAN_POINT ( 'NONE',  ( -22.50000000000000000, 64.35012909624775546, -103.1056273753973613 ) ) ;
#129184 = DIRECTION ( 'NONE',  ( -4.448008912761043807E-16, 1.000000000000000000, 0.000000000000000000 ) ) ;
#129185 = CARTESIAN_POINT ( 'NONE',  ( 20.85000000000000142, 76.00000000001213607, -136.5231074845243313 ) ) ;
#129186 = ORIENTED_EDGE ( 'NONE', *, *, #148378, .F. ) ;
#129187 = CIRCLE ( 'NONE', #187452, 0.09999999999999939493 ) ;
#129188 = DIRECTION ( 'NONE',  ( 0.000000000000000000, -6.467318590049456648E-15, 1.000000000000000000 ) ) ;
#129189 = TOROIDAL_SURFACE ( 'NONE', #16776, 6.258578643762700899, 0.1000000000000000056 ) ;
#129190 = AXIS2_PLACEMENT_3D ( 'NONE', #39069, #176019, #118603 ) ;
#129191 = DIRECTION ( 'NONE',  ( 1.000000000000000000, 0.000000000000000000, 0.000000000000000000 ) ) ;
#129192 = CIRCLE ( 'NONE', #83543, 0.09999999999998898659 ) ;
#129193 = AXIS2_PLACEMENT_3D ( 'NONE', #216387, #239825, #160303 ) ;
#129194 = ORIENTED_EDGE ( 'NONE', *, *, #122122, .F. ) ;
#129195 = CARTESIAN_POINT ( 'NONE',  ( -16.86422026484316916, 12.41958735970269956, -211.1723035762320535 ) ) ;
#129197 = ORIENTED_EDGE ( 'NONE', *, *, #137926, .F. ) ;
#129196 = CARTESIAN_POINT ( 'NONE',  ( 21.14999999999999858, 69.45934304831114048, -170.0231074845243882 ) ) ;
#129198 = CARTESIAN_POINT ( 'NONE',  ( 21.14999999999999858, -1.391858308744748696, -194.6091531227727955 ) ) ;
#129199 = DIRECTION ( 'NONE',  ( 1.000000000000000000, 0.000000000000000000, 0.000000000000000000 ) ) ;
#129200 = ORIENTED_EDGE ( 'NONE', *, *, #135602, .F. ) ;
#129201 = CARTESIAN_POINT ( 'NONE',  ( -16.97683809663752186, 66.05000000001261640, -190.1207434663279514 ) ) ;
#129202 = APPLICATION_PROTOCOL_DEFINITION ( 'draft international standard', 'automotive_design', 1998, #137289 ) ;
#129203 = CARTESIAN_POINT ( 'NONE',  ( -21.05000000000000071, 69.58624026620188374, -136.4374944237204375 ) ) ;
#129204 = AXIS2_PLACEMENT_3D ( 'NONE', #11035, #89271, #48868 ) ;
#129205 = DIRECTION ( 'NONE',  ( 1.000000000000000000, -0.000000000000000000, -0.000000000000000000 ) ) ;
#129206 = CARTESIAN_POINT ( 'NONE',  ( 22.49806830649814060, 64.35011034517256689, -69.60057180084992012 ) ) ;
#129207 = ORIENTED_EDGE ( 'NONE', *, *, #72390, .F. ) ;
#129208 = DIRECTION ( 'NONE',  ( 1.000000000000000000, -2.952720810173289112E-16, -2.061873921506763405E-30 ) ) ;
#129209 = CARTESIAN_POINT ( 'NONE',  ( 18.59999999999999432, -1.162701749926855266, -108.6000000000000227 ) ) ;
#129210 = DIRECTION ( 'NONE',  ( -1.000000000000000000, 0.000000000000000000, 0.000000000000000000 ) ) ;
#129211 = VERTEX_POINT ( 'NONE', #124895 ) ;
#129212 = VERTEX_POINT ( 'NONE', #161465 ) ;
#129213 = DIRECTION ( 'NONE',  ( -1.000000000000000000, -2.952720810173289112E-16, 0.000000000000000000 ) ) ;
#129214 = AXIS2_PLACEMENT_3D ( 'NONE', #92762, #95345, #251842 ) ;
#129215 = CARTESIAN_POINT ( 'NONE',  ( 18.46905048506370406, 85.47374425739423032, -96.34712119226884397 ) ) ;
#129216 = CARTESIAN_POINT ( 'NONE',  ( -23.30000000000000426, -11.79999999999999893, 33.00000000000000000 ) ) ;
#129217 = EDGE_CURVE ( 'NONE', #251180, #50839, #66199, .T. ) ;
#129218 = CARTESIAN_POINT ( 'NONE',  ( 21.08804582317323906, 8.878166167103058726, -146.3499998294057605 ) ) ;
#129219 = TOROIDAL_SURFACE ( 'NONE', #133490, 11.65000000000000036, 0.1000000000000000056 ) ;
#129221 = CARTESIAN_POINT ( 'NONE',  ( -18.59999999999999787, 0.5876173420563349792, -209.1618981382189588 ) ) ;
#129220 = DIRECTION ( 'NONE',  ( 0.000000000000000000, 0.000000000000000000, 1.000000000000000000 ) ) ;
#129222 = CARTESIAN_POINT ( 'NONE',  ( -21.13498764882296044, 75.99834360528109301, -176.5187256279983217 ) ) ;
#129223 = EDGE_CURVE ( 'NONE', #165825, #137060, #62111, .T. ) ;
#129224 = CARTESIAN_POINT ( 'NONE',  ( -20.94999999999999929, 36.65892442174935439, -249.5511627012433848 ) ) ;
#129225 = CARTESIAN_POINT ( 'NONE',  ( -18.48550754431968457, 46.96068962191068863, -255.3057266380914712 ) ) ;
#129226 = B_SPLINE_CURVE_WITH_KNOTS ( 'NONE', 3,
 ( #120082, #236142, #176192, #254390, #174945, #60061, #198295, #195761, #75789, #139582, #138299, #37967, #199611, #240005 ),
 .UNSPECIFIED., .F., .F.,
 ( 4, 2, 2, 2, 2, 2, 4 ),
 ( 1.398578778534940505E-17, 0.0003823333598417805049, 0.0005735000397626734137, 0.0006690833797231096223, 0.0007168750497033291903, 0.0007407708846934367517, 0.0007646667196835443131 ),
 .UNSPECIFIED. ) ;
#129228 = ORIENTED_EDGE ( 'NONE', *, *, #184007, .T. ) ;
#129227 = DIRECTION ( 'NONE',  ( -1.000000000000000000, -6.754466386607082172E-16, 1.507734853975053202E-15 ) ) ;
#129229 = CARTESIAN_POINT ( 'NONE',  ( 21.07933241753356768, 69.67135405163263329, -170.1164870749437057 ) ) ;
#129230 = CARTESIAN_POINT ( 'NONE',  ( -23.15000000000000213, 85.50000000001159606, -59.62913836187181005 ) ) ;
#129232 = DIRECTION ( 'NONE',  ( -1.000000000000000000, 0.000000000000000000, 0.000000000000000000 ) ) ;
#129231 = DIRECTION ( 'NONE',  ( -1.000000000000000000, 0.000000000000000000, 0.000000000000000000 ) ) ;
#129233 = EDGE_CURVE ( 'NONE', #143687, #40333, #23250, .T. ) ;
#129234 = EDGE_CURVE ( 'NONE', #108130, #68524, #206287, .T. ) ;
#129235 = ORIENTED_EDGE ( 'NONE', *, *, #252195, .F. ) ;
#129236 = DIRECTION ( 'NONE',  ( 0.000000000000000000, -0.8700118002898359348, 0.4930308989875165082 ) ) ;
#129237 = CARTESIAN_POINT ( 'NONE',  ( -18.40000000000000213, 11.75000000001113953, -79.65000000000004832 ) ) ;
#129238 = DIRECTION ( 'NONE',  ( -1.000000000000000000, 0.000000000000000000, 0.000000000000000000 ) ) ;
#129239 = CARTESIAN_POINT ( 'NONE',  ( -23.25000000000000000, 1.115600667400684642E-11, -33.50000000000000000 ) ) ;
#129240 = FACE_OUTER_BOUND ( 'NONE', #232380, .T. ) ;
#129241 = ORIENTED_EDGE ( 'NONE', *, *, #10910, .F. ) ;
#129243 = EDGE_LOOP ( 'NONE', ( #213209, #155406, #198265, #103560 ) ) ;
#129242 = AXIS2_PLACEMENT_3D ( 'NONE', #14776, #171305, #194699 ) ;
#129244 = AXIS2_PLACEMENT_3D ( 'NONE', #137715, #136417, #118175 ) ;
#129245 = DIRECTION ( 'NONE',  ( 0.000000000000000000, -1.000000000000000000, 8.881784197001250351E-16 ) ) ;
#129246 = ORIENTED_EDGE ( 'NONE', *, *, #6348, .T. ) ;
#129247 = CARTESIAN_POINT ( 'NONE',  ( -21.00857864376268935, 12.80863705670245878, -205.3010250813005655 ) ) ;
#129248 = VECTOR ( 'NONE', #192005, 1000.000000000000000 ) ;
#129249 = ORIENTED_EDGE ( 'NONE', *, *, #210181, .F. ) ;
#129250 = TOROIDAL_SURFACE ( 'NONE', #62617, 11.70000000000000639, 0.1000000000000000056 ) ;
#129251 = CARTESIAN_POINT ( 'NONE',  ( -20.54999999999999716, 46.19206980365409265, -240.6234452366647076 ) ) ;
#129252 = ADVANCED_FACE ( 'NONE', ( #66198 ), #62354, .F. ) ;
#129253 = FACE_OUTER_BOUND ( 'NONE', #8289, .T. ) ;
#129254 = DIRECTION ( 'NONE',  ( -1.000000000000000000, 0.000000000000000000, 0.000000000000000000 ) ) ;
#129255 = ORIENTED_EDGE ( 'NONE', *, *, #188004, .F. ) ;
#129256 = CARTESIAN_POINT ( 'NONE',  ( -23.25000000000000000, 43.21392023178790964, -245.1418509714632421 ) ) ;
#129257 = CARTESIAN_POINT ( 'NONE',  ( -18.53317502108577131, 68.08564185115265843, -224.1612363371343122 ) ) ;
#129258 = DIRECTION ( 'NONE',  ( -1.000000000000000000, -0.000000000000000000, -0.000000000000000000 ) ) ;
#129259 = DIRECTION ( 'NONE',  ( 0.000000000000000000, 0.000000000000000000, -1.000000000000000000 ) ) ;
#129260 = EDGE_CURVE ( 'NONE', #146901, #46606, #200570, .T. ) ;
#129262 = CIRCLE ( 'NONE', #199994, 0.1000000000000001860 ) ;
#129261 = DIRECTION ( 'NONE',  ( 0.000000000000000000, -1.000000000000000000, 0.000000000000000000 ) ) ;
#129263 = AXIS2_PLACEMENT_3D ( 'NONE', #106859, #222956, #62622 ) ;
#129264 = CARTESIAN_POINT ( 'NONE',  ( 21.14999999999999858, 11.19216743630477673, -211.0996217964688810 ) ) ;
#129266 = EDGE_LOOP ( 'NONE', ( #15291, #27952, #123474, #202220, #151591 ) ) ;
#129265 = EDGE_CURVE ( 'NONE', #244617, #145757, #237075, .T. ) ;
#129268 = DIRECTION ( 'NONE',  ( 1.000000000000000000, 0.000000000000000000, -0.000000000000000000 ) ) ;
#129267 = DIRECTION ( 'NONE',  ( -1.000000000000000000, 0.000000000000000000, -0.000000000000000000 ) ) ;
#129269 = ORIENTED_EDGE ( 'NONE', *, *, #58039, .T. ) ;
#129271 = ORIENTED_EDGE ( 'NONE', *, *, #100537, .F. ) ;
#129270 = DIRECTION ( 'NONE',  ( 1.000000000000000000, 0.000000000000000000, 0.000000000000000000 ) ) ;
#129272 = VERTEX_POINT ( 'NONE', #25786 ) ;
#129273 = DIRECTION ( 'NONE',  ( 0.000000000000000000, 0.2128009952263603677, -0.9770955615653313941 ) ) ;
#129274 = CARTESIAN_POINT ( 'NONE',  ( 23.14999999999998437, 11.75000000001115552, -33.50000000000000000 ) ) ;
#129275 = CARTESIAN_POINT ( 'NONE',  ( 18.59999999999997655, -4.531599869146433551E-30, -41.40000000000000568 ) ) ;
#129276 = ORIENTED_EDGE ( 'NONE', *, *, #49390, .F. ) ;
#129277 = CARTESIAN_POINT ( 'NONE',  ( 18.59999999999999432, -1.162701749926853712, -175.4999999999999716 ) ) ;
#129278 = CARTESIAN_POINT ( 'NONE',  ( -23.15000000000000213, 13.96869538424788360, -210.3925794786332233 ) ) ;
#129279 = EDGE_CURVE ( 'NONE', #102259, #192523, #228722, .T. ) ;
#129280 = ORIENTED_EDGE ( 'NONE', *, *, #249679, .T. ) ;
#129281 = EDGE_CURVE ( 'NONE', #169429, #216161, #55211, .T. ) ;
#129282 = DIRECTION ( 'NONE',  ( 0.000000000000000000, -1.000000000000000000, -0.000000000000000000 ) ) ;
#129283 = CIRCLE ( 'NONE', #254158, 0.5000000000000004441 ) ;
#129284 = CIRCLE ( 'NONE', #75137, 2.099999999999990763 ) ;
#129286 = CIRCLE ( 'NONE', #233363, 0.1000000000000028783 ) ;
#129285 = DIRECTION ( 'NONE',  ( 0.000000000000000000, 0.9908441862701782288, 0.1350103645450542456 ) ) ;
#129287 = EDGE_CURVE ( 'NONE', #253128, #110463, #87013, .T. ) ;
#129288 = ORIENTED_EDGE ( 'NONE', *, *, #47488, .F. ) ;
#129289 = CARTESIAN_POINT ( 'NONE',  ( -22.39999999999999503, 7.790779598384560245, -66.90000000000004832 ) ) ;
#129290 = ORIENTED_EDGE ( 'NONE', *, *, #255289, .T. ) ;
#129291 = CIRCLE ( 'NONE', #166740, 0.09999999999999543976 ) ;
#129292 = DIRECTION ( 'NONE',  ( 0.000000000000000000, 0.2617529984164915779, 0.9651348961777187485 ) ) ;
#129293 = ORIENTED_EDGE ( 'NONE', *, *, #19012, .F. ) ;
#129294 = CARTESIAN_POINT ( 'NONE',  ( -16.87331047859651179, 66.05000000001157900, -56.87310748452438958 ) ) ;
#129295 = DIRECTION ( 'NONE',  ( 1.000000000000000000, -3.427148797533456523E-14, 5.467925025959484217E-15 ) ) ;
#129296 = DIRECTION ( 'NONE',  ( 0.000000000000000000, 0.000000000000000000, -1.000000000000000000 ) ) ;
#129297 = ADVANCED_FACE ( 'NONE', ( #243543 ), #85715, .F. ) ;
#129298 = CARTESIAN_POINT ( 'NONE',  ( 20.94999999999999929, 85.40000000001148805, -45.91707660717669626 ) ) ;
#129299 = AXIS2_PLACEMENT_3D ( 'NONE', #242713, #4111, #64088 ) ;
#129300 = ADVANCED_FACE ( 'NONE', ( #205693 ), #251233, .T. ) ;
#129301 = CARTESIAN_POINT ( 'NONE',  ( -23.15000000000000213, 1.115600667400684642E-11, -100.5000000000000426 ) ) ;
#129302 = FACE_OUTER_BOUND ( 'NONE', #244139, .T. ) ;
#129303 = ORIENTED_EDGE ( 'NONE', *, *, #90879, .F. ) ;
#129304 = DIRECTION ( 'NONE',  ( 0.000000000000000000, 0.000000000000000000, -1.000000000000000000 ) ) ;
#129305 = ORIENTED_EDGE ( 'NONE', *, *, #151029, .F. ) ;
#129307 = DIRECTION ( 'NONE',  ( 0.000000000000000000, -0.9126074666063773710, -0.4088369013363272741 ) ) ;
#129306 = PLANE ( 'NONE',  #257031 ) ;
#129308 = ORIENTED_EDGE ( 'NONE', *, *, #123917, .T. ) ;
#129309 = CARTESIAN_POINT ( 'NONE',  ( 20.04142135623730070, 11.65000000001115943, -125.1500000000000341 ) ) ;
#129310 = DIRECTION ( 'NONE',  ( 0.000000000000000000, 0.000000000000000000, 1.000000000000000000 ) ) ;
#129311 = CARTESIAN_POINT ( 'NONE',  ( 20.95017935633852346, 59.10443188204394716, -225.7998842055091302 ) ) ;
#129313 = ORIENTED_EDGE ( 'NONE', *, *, #136652, .T. ) ;
#129312 =( BOUNDED_SURFACE ( )  B_SPLINE_SURFACE ( 3, 2, ( 
 ( #47391, #162244, #142639 ),
 ( #86500, #183082, #65684 ),
 ( #166114, #123109, #181789 ),
 ( #6992, #3124, #104778 ),
 ( #61846, #21453, #241752 ),
 ( #202627, #4418, #184342 ) ),
 .UNSPECIFIED., .F., .F., .F. ) 
 B_SPLINE_SURFACE_WITH_KNOTS ( ( 4, 2, 4 ),
 ( 3, 3 ),
 ( 0.0001381104793128061785, 0.0002947094729387726578, 0.0004513084665647390829 ),
 ( 0.000000000000000000, 1.000000000000000000 ),
 .UNSPECIFIED. ) 
 GEOMETRIC_REPRESENTATION_ITEM ( )  RATIONAL_B_SPLINE_SURFACE ( (
 ( 1.000000000000000000, 0.7071067811865985320, 1.000000000000000000),
 ( 1.000000000000000000, 0.6919563088098532599, 1.000000000000000000),
 ( 1.000000000000000000, 0.6959445945717439574, 1.000000000000000000),
 ( 1.000000000000000000, 0.7137882985313119821, 1.000000000000000000),
 ( 1.000000000000000000, 0.7257496306096471450, 1.000000000000000000),
 ( 1.000000000000000000, 0.7250110520819876836, 1.000000000000000000) ) ) 
 REPRESENTATION_ITEM ( '' )  SURFACE ( )  );
#129315 = ORIENTED_EDGE ( 'NONE', *, *, #25466, .F. ) ;
#129314 = CARTESIAN_POINT ( 'NONE',  ( 21.14999999999999858, 6.540656951712400691, -67.00000000000004263 ) ) ;
#129316 = DIRECTION ( 'NONE',  ( 1.000000000000000000, -0.000000000000000000, 0.000000000000000000 ) ) ;
#129318 = CARTESIAN_POINT ( 'NONE',  ( -16.92778301347241054, 65.99905508317772274, -190.9516255924938264 ) ) ;
#129317 = CARTESIAN_POINT ( 'NONE',  ( -18.40000000000000213, 51.05395640845380711, -230.6854822754303314 ) ) ;
#129320 = VERTEX_POINT ( 'NONE', #68768 ) ;
#129319 = CARTESIAN_POINT ( 'NONE',  ( 20.85000000000000142, 80.82423061532404063, -192.8091306798888525 ) ) ;
#129321 = ORIENTED_EDGE ( 'NONE', *, *, #109624, .T. ) ;
#129322 = CIRCLE ( 'NONE', #4408, 0.5000000000000004441 ) ;
#129323 = DIRECTION ( 'NONE',  ( -0.000000000000000000, -0.5795995782408138730, -0.8149014228132570592 ) ) ;
#129324 = FACE_OUTER_BOUND ( 'NONE', #164204, .T. ) ;
#129325 = ORIENTED_EDGE ( 'NONE', *, *, #242449, .T. ) ;
#129326 = DIRECTION ( 'NONE',  ( 0.000000000000000000, 0.8814952561688438326, -0.4721928772777331806 ) ) ;
#129327 = EDGE_LOOP ( 'NONE', ( #216497, #6549, #154741, #173793 ) ) ;
#129328 = CIRCLE ( 'NONE', #254210, 0.1000000000000024342 ) ;
#129329 = CARTESIAN_POINT ( 'NONE',  ( -23.15000000000000213, 4.150000000000001243, -12.35000000000000142 ) ) ;
#129330 = ORIENTED_EDGE ( 'NONE', *, *, #206571, .F. ) ;
#129331 = DIRECTION ( 'NONE',  ( -1.000000000000000000, -2.952720810173289112E-16, 0.000000000000000000 ) ) ;
#129332 = VERTEX_POINT ( 'NONE', #50453 ) ;
#129333 = AXIS2_PLACEMENT_3D ( 'NONE', #240864, #163893, #239580 ) ;
#129334 = FACE_OUTER_BOUND ( 'NONE', #230697, .T. ) ;
#129335 = AXIS2_PLACEMENT_3D ( 'NONE', #120962, #204303, #25689 ) ;
#129336 = VERTEX_POINT ( 'NONE', #148305 ) ;
#129337 = VERTEX_POINT ( 'NONE', #129997 ) ;
#129338 = DIRECTION ( 'NONE',  ( 0.000000000000000000, 0.2128009952263403282, -0.9770955615653358350 ) ) ;
#129339 = CIRCLE ( 'NONE', #158419, 0.09999999999999939493 ) ;
#129340 = ORIENTED_EDGE ( 'NONE', *, *, #220276, .T. ) ;
#129341 = DIRECTION ( 'NONE',  ( 1.000000000000000000, 0.000000000000000000, 0.000000000000000000 ) ) ;
#129343 = EDGE_CURVE ( 'NONE', #232908, #109044, #37185, .T. ) ;
#129342 = EDGE_LOOP ( 'NONE', ( #131361, #29846, #185757, #38977 ) ) ;
#129345 = EDGE_LOOP ( 'NONE', ( #92636, #106785, #138647 ) ) ;
#129344 = DIRECTION ( 'NONE',  ( 0.000000000000000000, 0.000000000000000000, 1.000000000000000000 ) ) ;
#129346 = AXIS2_PLACEMENT_3D ( 'NONE', #227312, #249466, #33023 ) ;
#129347 = VECTOR ( 'NONE', #26994, 1000.000000000000000 ) ;
#129348 = EDGE_LOOP ( 'NONE', ( #112061, #179435, #251394, #187226, #120042, #113693 ) ) ;
#129349 = EDGE_CURVE ( 'NONE', #47116, #135449, #32229, .T. ) ;
#129350 = DIRECTION ( 'NONE',  ( 0.000000000000000000, -0.7489048840758955050, 0.6626775042260523163 ) ) ;
#129351 = ADVANCED_FACE ( 'NONE', ( #249971 ), #220341, .F. ) ;
#129352 = ORIENTED_EDGE ( 'NONE', *, *, #225667, .F. ) ;
#129355 = VERTEX_POINT ( 'NONE', #106582 ) ;
#129354 = EDGE_LOOP ( 'NONE', ( #94814, #109311, #202508, #91375, #156940 ) ) ;
#129353 = DIRECTION ( 'NONE',  ( 0.000000000000000000, 0.000000000000000000, 1.000000000000000000 ) ) ;
#129356 = DIRECTION ( 'NONE',  ( 0.000000000000000000, 0.000000000000000000, 1.000000000000000000 ) ) ;
#129357 = DIRECTION ( 'NONE',  ( 1.073024830501117725E-15, -6.982962677686266711E-15, 1.000000000000000000 ) ) ;
#129358 = ORIENTED_EDGE ( 'NONE', *, *, #166615, .F. ) ;
#129359 = CIRCLE ( 'NONE', #145915, 0.1000000000000024342 ) ;
#129360 = AXIS2_PLACEMENT_3D ( 'NONE', #231210, #31742, #249483 ) ;
#129361 = AXIS2_PLACEMENT_3D ( 'NONE', #16623, #74047, #212257 ) ;
#129362 = AXIS2_PLACEMENT_3D ( 'NONE', #116973, #98646, #238185 ) ;
#129363 = AXIS2_PLACEMENT_3D ( 'NONE', #81983, #161582, #241116 ) ;
#129364 = ORIENTED_EDGE ( 'NONE', *, *, #28637, .F. ) ;
#129365 = EDGE_CURVE ( 'NONE', #23820, #105209, #170485, .T. ) ;
#129366 = DIRECTION ( 'NONE',  ( 0.000000000000000000, 1.000000000000000000, 6.982962677686266711E-15 ) ) ;
#129368 = ORIENTED_EDGE ( 'NONE', *, *, #107610, .F. ) ;
#129367 = DIRECTION ( 'NONE',  ( 0.000000000000000000, 0.000000000000000000, -1.000000000000000000 ) ) ;
#129369 = FACE_OUTER_BOUND ( 'NONE', #238176, .T. ) ;
#129370 = VERTEX_POINT ( 'NONE', #12666 ) ;
#129372 = DIRECTION ( 'NONE',  ( -0.5932847527679298016, 0.8049926720990051576, 0.000000000000000000 ) ) ;
#129371 =( BOUNDED_CURVE ( )  B_SPLINE_CURVE ( 3, ( #208675, #91283, #247776, #192948 ),
 .UNSPECIFIED., .F., .F. ) 
 B_SPLINE_CURVE_WITH_KNOTS ( ( 4, 4 ),
 ( 4.712388980384690562, 6.283185307179586232 ),
 .UNSPECIFIED. ) 
 CURVE ( )  GEOMETRIC_REPRESENTATION_ITEM ( )  RATIONAL_B_SPLINE_CURVE ( ( 1.000000000000000000, 0.8047378541243652705, 0.8047378541243652705, 1.000000000000000000 ) ) 
 REPRESENTATION_ITEM ( '' )  );
#129373 = CARTESIAN_POINT ( 'NONE',  ( 18.59999999999999076, 65.50857864377465489, -111.7731074845243597 ) ) ;
#129374 = ORIENTED_EDGE ( 'NONE', *, *, #87413, .T. ) ;
#129375 = B_SPLINE_CURVE_WITH_KNOTS ( 'NONE', 3,
 ( #243216, #3311, #41209, #22925, #141557, #181979, #120748, #102398, #200254, #222348 ),
 .UNSPECIFIED., .F., .F.,
 ( 4, 3, 3, 4 ),
 ( 0.000000000000000000, 4.874959354401577961E-05, 9.785140065119720494E-05, 0.0001360444631935916505 ),
 .UNSPECIFIED. ) ;
#129376 = DIRECTION ( 'NONE',  ( 0.000000000000000000, 0.9908441862701600211, -0.1350103645451876666 ) ) ;
#129377 = AXIS2_PLACEMENT_3D ( 'NONE', #226878, #247729, #67807 ) ;
#129378 = CARTESIAN_POINT ( 'NONE',  ( 18.50596464788227280, 18.37039103902861470, -236.9176190769589141 ) ) ;
#129379 = EDGE_LOOP ( 'NONE', ( #79028, #119287, #42650, #50650, #96900, #102005, #146653 ) ) ;
#129381 = EDGE_LOOP ( 'NONE', ( #154552, #21318, #32964, #153265 ) ) ;
#129380 = CARTESIAN_POINT ( 'NONE',  ( 19.75857864376269291, 54.44212562955072343, -228.7093116605464047 ) ) ;
#129382 = DIRECTION ( 'NONE',  ( 0.000000000000000000, -1.000000000000000000, 0.000000000000000000 ) ) ;
#129384 = ORIENTED_EDGE ( 'NONE', *, *, #127527, .F. ) ;
#129383 = ORIENTED_EDGE ( 'NONE', *, *, #171683, .F. ) ;
#129385 = ORIENTED_EDGE ( 'NONE', *, *, #171046, .F. ) ;
#129386 = DIRECTION ( 'NONE',  ( 1.000000000000000000, -3.265361837132813093E-16, -2.280189983783949500E-30 ) ) ;
#129388 = EDGE_LOOP ( 'NONE', ( #4321, #28566, #221316, #112396 ) ) ;
#129387 = EDGE_CURVE ( 'NONE', #103375, #83472, #245279, .T. ) ;
#129389 = ORIENTED_EDGE ( 'NONE', *, *, #166195, .T. ) ;
#129390 = EDGE_CURVE ( 'NONE', #233386, #139309, #33118, .T. ) ;
#129391 = DIRECTION ( 'NONE',  ( 0.000000000000000000, 0.000000000000000000, -1.000000000000000000 ) ) ;
#129392 = ORIENTED_EDGE ( 'NONE', *, *, #108069, .T. ) ;
#129393 = DIRECTION ( 'NONE',  ( -0.000000000000000000, -0.4721928772777351790, -0.8814952561688427224 ) ) ;
#129394 = CARTESIAN_POINT ( 'NONE',  ( -18.40000000000000213, 5.650000000011139001, -146.6500000000000341 ) ) ;
#129395 = AXIS2_PLACEMENT_3D ( 'NONE', #56195, #135743, #91495 ) ;
#129396 = ORIENTED_EDGE ( 'NONE', *, *, #1607, .F. ) ;
#129398 = ADVANCED_FACE ( 'NONE', ( #169180 ), #128746, .F. ) ;
#129397 = ORIENTED_EDGE ( 'NONE', *, *, #45938, .T. ) ;
#129399 = CARTESIAN_POINT ( 'NONE',  ( 23.15000000000000213, 84.59626168225520360, -145.9732350016745954 ) ) ;
#129400 = EDGE_LOOP ( 'NONE', ( #239932, #93593, #207156, #98107 ) ) ;
#129401 = VECTOR ( 'NONE', #200827, 1000.000000000000000 ) ;
#129402 =( BOUNDED_SURFACE ( )  B_SPLINE_SURFACE ( 3, 2, ( 
 ( #55135, #134688, #33090 ),
 ( #112588, #113861, #16077 ),
 ( #95577, #193419, #156873 ),
 ( #155598, #56438, #77290 ) ),
 .UNSPECIFIED., .F., .F., .T. ) 
 B_SPLINE_SURFACE_WITH_KNOTS ( ( 4, 4 ),
 ( 3, 3 ),
 ( -5.204170427930421283E-18, 0.001979672783031532438 ),
 ( 0.000000000000000000, 1.000000000000000000 ),
 .UNSPECIFIED. ) 
 GEOMETRIC_REPRESENTATION_ITEM ( )  RATIONAL_B_SPLINE_SURFACE ( (
 ( 1.000000000000000000, 0.7103081912008367693, 1.000000000000000000),
 ( 1.000000000000000000, 0.7104998333558518731, 1.000000000000000000),
 ( 1.000000000000000000, 0.7107238315755336489, 1.000000000000000000),
 ( 1.000000000000000000, 0.7110073749539377319, 1.000000000000000000) ) ) 
 REPRESENTATION_ITEM ( '' )  SURFACE ( )  );
#129403 = PLANE ( 'NONE',  #188671 ) ;
#129404 = EDGE_LOOP ( 'NONE', ( #189900, #97234, #192648, #22929 ) ) ;
#129405 = CARTESIAN_POINT ( 'NONE',  ( -20.94999999999999929, 1.835341550224413698, -11.55515129256298401 ) ) ;
#129407 = ORIENTED_EDGE ( 'NONE', *, *, #12959, .T. ) ;
#129406 = CARTESIAN_POINT ( 'NONE',  ( -23.25000000000000000, 76.00000000001244871, -170.0231074845243597 ) ) ;
#129408 = DIRECTION ( 'NONE',  ( 2.952720810173290591E-16, -0.4721928772777312933, -0.8814952561688448318 ) ) ;
#129409 = DIRECTION ( 'NONE',  ( -0.000000000000000000, 0.9274965247785350586, 0.3738317757009704811 ) ) ;
#129410 = CARTESIAN_POINT ( 'NONE',  ( -17.11825945287482753, 12.43531352672261825, -211.3405985074572300 ) ) ;
#129411 = DIRECTION ( 'NONE',  ( 0.000000000000000000, -6.938893903907222067E-15, 1.000000000000000000 ) ) ;
#129413 = ADVANCED_FACE ( 'NONE', ( #248688 ), #111743, .F. ) ;
#129412 = CARTESIAN_POINT ( 'NONE',  ( -23.25000000000000000, 3.470628026992396808, -231.7731008717366876 ) ) ;
#129414 = CIRCLE ( 'NONE', #8620, 0.1000000000000124678 ) ;
#129415 = CARTESIAN_POINT ( 'NONE',  ( -23.25000000000000000, 73.40000000001259650, -190.2984855617622770 ) ) ;
#129416 = DIRECTION ( 'NONE',  ( 1.000000000000000000, 0.000000000000000000, 0.000000000000000000 ) ) ;
#129417 = CARTESIAN_POINT ( 'NONE',  ( 22.50046968637550648, 75.95483015286804118, -181.7731526389976295 ) ) ;
#129418 = CYLINDRICAL_SURFACE ( 'NONE', #201336, 0.1000000000000004496 ) ;
#129419 = CIRCLE ( 'NONE', #104273, 12.97499999999999964 ) ;
#129420 = ORIENTED_EDGE ( 'NONE', *, *, #100696, .T. ) ;
#129421 = AXIS2_PLACEMENT_3D ( 'NONE', #183655, #25867, #4974 ) ;
#129422 = ADVANCED_FACE ( 'NONE', ( #10071, #149608 ), #132595, .T. ) ;
#129423 = VERTEX_POINT ( 'NONE', #131297 ) ;
#129426 = ORIENTED_EDGE ( 'NONE', *, *, #21072, .F. ) ;
#129425 = ADVANCED_FACE ( 'NONE', ( #191313 ), #53728, .T. ) ;
#129424 = CARTESIAN_POINT ( 'NONE',  ( 20.94999999999999929, 76.00000000001143974, -38.02310748452432421 ) ) ;
#129427 = EDGE_LOOP ( 'NONE', ( #157970, #42804, #257397, #97, #218001 ) ) ;
#129428 = DIRECTION ( 'NONE',  ( 1.073024830501117725E-15, 0.000000000000000000, 1.000000000000000000 ) ) ;
#129429 = FACE_OUTER_BOUND ( 'NONE', #195003, .T. ) ;
#129430 = EDGE_CURVE ( 'NONE', #210905, #179010, #152180, .T. ) ;
#129431 = EDGE_CURVE ( 'NONE', #248822, #110463, #199689, .T. ) ;
#129433 = CARTESIAN_POINT ( 'NONE',  ( 21.14999999999999858, 10.71339244341104013, -112.7500000000000284 ) ) ;
#129432 = CARTESIAN_POINT ( 'NONE',  ( 20.50589344625223731, 39.28418211382209790, -236.8880073202264782 ) ) ;
#129434 = EDGE_LOOP ( 'NONE', ( #207967, #154329, #176286 ) ) ;
#129435 = ORIENTED_EDGE ( 'NONE', *, *, #148501, .F. ) ;
#129436 =( NAMED_UNIT ( * ) PLANE_ANGLE_UNIT ( ) SI_UNIT ( $, .RADIAN. ) );
#129437 = CARTESIAN_POINT ( 'NONE',  ( -18.59999999999999787, 66.75000000001205080, -124.2731074845243597 ) ) ;
#129438 = CIRCLE ( 'NONE', #229409, 0.09999999999999939493 ) ;
#129439 = DIRECTION ( 'NONE',  ( 0.000000000000000000, -0.9126074666063773710, -0.4088369013363271631 ) ) ;
#129440 = ORIENTED_EDGE ( 'NONE', *, *, #131754, .T. ) ;
#129441 = VERTEX_POINT ( 'NONE', #166613 ) ;
#129442 = ADVANCED_FACE ( 'NONE', ( #107883 ), #28448, .F. ) ;
#129443 = CARTESIAN_POINT ( 'NONE',  ( 18.79999999999999716, 7.973296578895943121, -1.410778198689825347 ) ) ;
#129445 = EDGE_CURVE ( 'NONE', #108203, #122253, #133039, .T. ) ;
#129444 = EDGE_CURVE ( 'NONE', #224878, #50997, #153349, .T. ) ;
#129446 = CARTESIAN_POINT ( 'NONE',  ( 21.30000000000002558, 76.00000000001240608, -174.0731074845243711 ) ) ;
#129447 = FACE_OUTER_BOUND ( 'NONE', #53059, .T. ) ;
#129448 = DIRECTION ( 'NONE',  ( 0.000000000000000000, 0.000000000000000000, 1.000000000000000000 ) ) ;
#129450 = ORIENTED_EDGE ( 'NONE', *, *, #101182, .F. ) ;
#129449 = DIRECTION ( 'NONE',  ( 0.000000000000000000, 0.000000000000000000, -1.000000000000000000 ) ) ;
#129451 = ADVANCED_FACE ( 'NONE', ( #56862 ), #75207, .F. ) ;
#129452 = DIRECTION ( 'NONE',  ( -0.000000000000000000, 0.000000000000000000, 1.000000000000000000 ) ) ;
#129453 = CARTESIAN_POINT ( 'NONE',  ( 22.39999999999999858, 0.09999999999999939493, 7.790779598373383408 ) ) ;
#129454 = FACE_OUTER_BOUND ( 'NONE', #231495, .T. ) ;
#129455 = CARTESIAN_POINT ( 'NONE',  ( 18.48536876927948924, 85.46352724987913518, -95.97448921944113920 ) ) ;
#129456 = ORIENTED_EDGE ( 'NONE', *, *, #162695, .F. ) ;
#129457 = CARTESIAN_POINT ( 'NONE',  ( 12.93279065517212345, 66.58230930894873723, -84.88150678775981817 ) ) ;
#129458 = DIRECTION ( 'NONE',  ( 2.952720810173289112E-16, 1.000000000000000000, 6.982962677686266711E-15 ) ) ;
#129459 = CIRCLE ( 'NONE', #233709, 11.75000000000000000 ) ;
#129460 = EDGE_CURVE ( 'NONE', #205417, #155942, #108091, .T. ) ;
#129463 = CARTESIAN_POINT ( 'NONE',  ( 23.24999999999999289, 11.65000000001116298, -134.1000000000000227 ) ) ;
#129462 = AXIS2_PLACEMENT_3D ( 'NONE', #237244, #19487, #139400 ) ;
#129461 = DIRECTION ( 'NONE',  ( -1.000000000000000000, -0.000000000000000000, -0.000000000000000000 ) ) ;
#129465 = CARTESIAN_POINT ( 'NONE',  ( -23.25000000000000000, 76.00000000001142553, -36.02310748452432421 ) ) ;
#129464 = AXIS2_PLACEMENT_3D ( 'NONE', #86548, #147853, #241799 ) ;
#129466 = CARTESIAN_POINT ( 'NONE',  ( -16.96982749440705973, 9.950000000011137047, -53.87522159118827858 ) ) ;
#129467 = CIRCLE ( 'NONE', #62820, 2.000000000000002220 ) ;
#129468 = DIRECTION ( 'NONE',  ( 1.000000000000000000, 0.000000000000000000, 0.000000000000000000 ) ) ;
#129469 = CARTESIAN_POINT ( 'NONE',  ( -16.77828822459933633, 66.05377062495506379, -48.68573573544333755 ) ) ;
#129470 = FACE_OUTER_BOUND ( 'NONE', #69957, .T. ) ;
#129471 = DIRECTION ( 'NONE',  ( -0.000000000000000000, 1.000000000000000000, -0.000000000000000000 ) ) ;
#129472 = EDGE_CURVE ( 'NONE', #179534, #178504, #61725, .T. ) ;
#129473 = EDGE_CURVE ( 'NONE', #59214, #233299, #174196, .T. ) ;
#129474 = ORIENTED_EDGE ( 'NONE', *, *, #159279, .F. ) ;
#129475 = AXIS2_PLACEMENT_3D ( 'NONE', #57680, #178971, #38153 ) ;
#129476 = EDGE_LOOP ( 'NONE', ( #27301, #234154, #219076, #220955 ) ) ;
#129477 = ORIENTED_EDGE ( 'NONE', *, *, #155947, .F. ) ;
#129478 = EDGE_CURVE ( 'NONE', #226022, #245137, #103389, .T. ) ;
#129479 = CARTESIAN_POINT ( 'NONE',  ( 20.22894356738409272, 66.72150177717416852, -94.75458457828102610 ) ) ;
#129480 = DIRECTION ( 'NONE',  ( 0.000000000000000000, 0.1298341882520022694, 0.9915357197604852679 ) ) ;
#129481 = ORIENTED_EDGE ( 'NONE', *, *, #234994, .T. ) ;
#129482 = ADVANCED_FACE ( 'NONE', ( #77725 ), #114304, .F. ) ;
#129483 = AXIS2_PLACEMENT_3D ( 'NONE', #215155, #36557, #37832 ) ;
#129484 = EDGE_LOOP ( 'NONE', ( #183958, #135489, #256769, #204927 ) ) ;
#129485 =( LENGTH_UNIT ( ) NAMED_UNIT ( * ) SI_UNIT ( .MILLI., .METRE. ) );
#129486 = EDGE_CURVE ( 'NONE', #102511, #191930, #99116, .T. ) ;
#129487 = B_SPLINE_CURVE_WITH_KNOTS ( 'NONE', 3,
 ( #125326, #43222, #163178, #142304, #66634, #27546, #225670, #84865, #126603, #206143 ),
 .UNSPECIFIED., .F., .F.,
 ( 4, 3, 3, 4 ),
 ( 0.000000000000000000, 0.0002000000000002884074, 0.001000000000045112589, 0.001967863649472103085 ),
 .UNSPECIFIED. ) ;
#129488 = ORIENTED_EDGE ( 'NONE', *, *, #21294, .T. ) ;
#129489 = CARTESIAN_POINT ( 'NONE',  ( 21.76363531954645936, 7.012936547882880234, -66.90099812570059612 ) ) ;
#129490 = ORIENTED_EDGE ( 'NONE', *, *, #9151, .T. ) ;
#129491 = DIRECTION ( 'NONE',  ( 0.000000000000000000, 0.9651348961777158619, -0.2617529984165031243 ) ) ;
#129492 = DIRECTION ( 'NONE',  ( 1.000000000000000000, 0.000000000000000000, 0.000000000000000000 ) ) ;
#129493 = DIRECTION ( 'NONE',  ( 0.000000000000000000, 0.9856811345164800953, 0.1686199900910462790 ) ) ;
#129494 = DIRECTION ( 'NONE',  ( 1.000000000000000000, 0.000000000000000000, 0.000000000000000000 ) ) ;
#129495 = CARTESIAN_POINT ( 'NONE',  ( 21.05000000000000071, 4.813084112160680661, -78.94151775652387926 ) ) ;
#129497 = VERTEX_POINT ( 'NONE', #118160 ) ;
#129496 = CARTESIAN_POINT ( 'NONE',  ( 23.14999999999999858, 37.60331017630482364, -247.7881721889056905 ) ) ;
#129499 = DIRECTION ( 'NONE',  ( -0.000000000000000000, 0.9126074666063770380, 0.4088369013363281068 ) ) ;
#129498 = DIRECTION ( 'NONE',  ( 0.000000000000000000, -0.000000000000000000, -1.000000000000000000 ) ) ;
#129500 = EDGE_CURVE ( 'NONE', #41312, #187599, #249176, .T. ) ;
#129502 = CARTESIAN_POINT ( 'NONE',  ( -17.11825945287481687, 10.04999999999998472, -20.85000000000000142 ) ) ;
#129501 = VECTOR ( 'NONE', #49022, 1000.000000000000000 ) ;
#129503 = ORIENTED_EDGE ( 'NONE', *, *, #251062, .T. ) ;
#129504 = CARTESIAN_POINT ( 'NONE',  ( 20.95512820512820440, 65.37615131630035137, -148.7731074845244450 ) ) ;
#129505 = CYLINDRICAL_SURFACE ( 'NONE', #29259, 0.09999999999999939493 ) ;
#129506 = VERTEX_POINT ( 'NONE', #135133 ) ;
#129507 = AXIS2_PLACEMENT_3D ( 'NONE', #142948, #41338, #40061 ) ;
#129508 = DIRECTION ( 'NONE',  ( 0.000000000000000000, 0.000000000000000000, -1.000000000000000000 ) ) ;
#129509 = CIRCLE ( 'NONE', #200231, 4.149999999999987033 ) ;
#129510 = CARTESIAN_POINT ( 'NONE',  ( -16.84793658983463516, 66.05000000001182059, -82.25675416233410431 ) ) ;
#129511 = VERTEX_POINT ( 'NONE', #96011 ) ;
#129512 = DIRECTION ( 'NONE',  ( 0.000000000000000000, -0.9126074666063769270, -0.4088369013363280513 ) ) ;
#129513 = CARTESIAN_POINT ( 'NONE',  ( 21.05000000000000071, -11.74999999999999112, -2.900000000000003464 ) ) ;
#129515 = CARTESIAN_POINT ( 'NONE',  ( 20.94999999999999929, 87.48912529308798014, -106.1231074845242262 ) ) ;
#129514 = CIRCLE ( 'NONE', #191905, 0.5000000000000054401 ) ;
#129516 = CARTESIAN_POINT ( 'NONE',  ( -21.05000000000000071, 13.59055429284667404, -238.6121134008722038 ) ) ;
#129517 = ORIENTED_EDGE ( 'NONE', *, *, #170723, .F. ) ;
#129518 = ORIENTED_EDGE ( 'NONE', *, *, #72193, .F. ) ;
#129519 = DIRECTION ( 'NONE',  ( 0.000000000000000000, 0.9915357197604804940, -0.1298341882520397950 ) ) ;
#129520 = DIRECTION ( 'NONE',  ( 0.000000000000000000, 0.000000000000000000, 1.000000000000000000 ) ) ;
#129521 = EDGE_CURVE ( 'NONE', #196244, #180058, #62282, .T. ) ;
#129522 = DIRECTION ( 'NONE',  ( 0.000000000000000000, 0.4999999999999088507, -0.8660254037844913322 ) ) ;
#129523 = CARTESIAN_POINT ( 'NONE',  ( -22.47071067811865319, 75.90090754530939421, -110.7431822290223806 ) ) ;
#129525 = DIRECTION ( 'NONE',  ( 1.000000000000000000, 0.000000000000000000, 0.000000000000000000 ) ) ;
#129524 = FACE_OUTER_BOUND ( 'NONE', #254763, .T. ) ;
#129526 = CIRCLE ( 'NONE', #171269, 0.09999999999999939493 ) ;
#129527 = DIRECTION ( 'NONE',  ( 1.000000000000000000, 0.000000000000000000, 0.000000000000000000 ) ) ;
#129528 = EDGE_CURVE ( 'NONE', #31859, #14872, #156026, .T. ) ;
#129529 = CARTESIAN_POINT ( 'NONE',  ( -20.94999999999999929, 74.75000000001261924, -195.5231074845243597 ) ) ;
#129531 = LINE ( 'NONE', #86509, #217834 ) ;
#129530 = CIRCLE ( 'NONE', #221086, 0.1000000000000028644 ) ;
#129532 = ORIENTED_EDGE ( 'NONE', *, *, #133617, .T. ) ;
#129533 = CARTESIAN_POINT ( 'NONE',  ( -20.87600722750343252, 65.66887361445333227, -97.43298459182690863 ) ) ;
#129534 = AXIS2_PLACEMENT_3D ( 'NONE', #30206, #189276, #164576 ) ;
#129536 = VERTEX_POINT ( 'NONE', #19054 ) ;
#129535 = DIRECTION ( 'NONE',  ( -0.000000000000000000, -0.1350103645451807555, -0.9908441862701610203 ) ) ;
#129537 = CARTESIAN_POINT ( 'NONE',  ( 21.53752568617687402, 69.21319212550855582, -170.1220819458087874 ) ) ;
#129538 = CYLINDRICAL_SURFACE ( 'NONE', #28196, 0.09999999999998898659 ) ;
#129539 = FACE_OUTER_BOUND ( 'NONE', #111094, .T. ) ;
#129540 = AXIS2_PLACEMENT_3D ( 'NONE', #131755, #74393, #215148 ) ;
#129541 = CARTESIAN_POINT ( 'NONE',  ( -16.87683809663752399, 66.15000000001208491, -123.1207434663278804 ) ) ;
#129542 = EDGE_CURVE ( 'NONE', #14799, #214929, #76453, .T. ) ;
#129543 = EDGE_CURVE ( 'NONE', #25370, #38969, #136402, .T. ) ;
#129544 = CARTESIAN_POINT ( 'NONE',  ( 20.96077737575349786, 11.62390063401585394, -194.1407919571063019 ) ) ;
#129546 = VERTEX_POINT ( 'NONE', #37355 ) ;
#129545 = CARTESIAN_POINT ( 'NONE',  ( -20.64999999999999858, 74.00000000001229239, -157.2984855617622770 ) ) ;
#129547 = DIRECTION ( 'NONE',  ( 0.000000000000000000, 0.9868171638914230437, -0.1618390714546045217 ) ) ;
#129548 = CARTESIAN_POINT ( 'NONE',  ( -21.05000000000000071, -11.64999999998884483, -167.4999999999999432 ) ) ;
#129549 = VECTOR ( 'NONE', #90054, 1000.000000000000227 ) ;
#129550 = CARTESIAN_POINT ( 'NONE',  ( 20.94999999999999929, 76.00000000001212186, -134.5231074845243313 ) ) ;
#129551 = DIRECTION ( 'NONE',  ( 0.000000000000000000, 0.000000000000000000, -1.000000000000000000 ) ) ;
#129552 = VERTEX_POINT ( 'NONE', #116875 ) ;
#129553 = FACE_OUTER_BOUND ( 'NONE', #121640, .T. ) ;
#129554 = ORIENTED_EDGE ( 'NONE', *, *, #1477, .T. ) ;
#129555 = CARTESIAN_POINT ( 'NONE',  ( -17.11825945287482753, 66.05000000001189164, -90.37310748452436826 ) ) ;
#129556 = VERTEX_POINT ( 'NONE', #212138 ) ;
#129558 = DIRECTION ( 'NONE',  ( 0.000000000000000000, 0.8814952561688441657, -0.4721928772777325145 ) ) ;
#129557 = VECTOR ( 'NONE', #76268, 1000.000000000000000 ) ;
#129559 = CIRCLE ( 'NONE', #121209, 0.1000000000000002554 ) ;
#129560 = VECTOR ( 'NONE', #124697, 1000.000000000000000 ) ;
#129561 = ORIENTED_EDGE ( 'NONE', *, *, #144677, .T. ) ;
#129562 = AXIS2_PLACEMENT_3D ( 'NONE', #115369, #17541, #237886 ) ;
#129563 = AXIS2_PLACEMENT_3D ( 'NONE', #192750, #158770, #255219 ) ;
#129564 = CARTESIAN_POINT ( 'NONE',  ( -20.94999999999994600, 66.15000000001120384, -5.923107484524795296 ) ) ;
#129565 = CARTESIAN_POINT ( 'NONE',  ( -18.59999999999999787, 77.16412189325258453, -28.10825939895270764 ) ) ;
#129566 = EDGE_LOOP ( 'NONE', ( #247016, #182474, #257942, #189129 ) ) ;
#129567 = DIRECTION ( 'NONE',  ( 1.000000000000000000, 0.000000000000000000, 0.000000000000000000 ) ) ;
#129568 = VECTOR ( 'NONE', #184872, 1000.000000000000227 ) ;
#129569 = DIRECTION ( 'NONE',  ( 0.000000000000000000, 0.3738317757009942399, -0.9274965247785252886 ) ) ;
#129570 = CARTESIAN_POINT ( 'NONE',  ( -21.40925344232282512, 6.484952525504856347, -199.4863767698734307 ) ) ;
#129571 = FACE_OUTER_BOUND ( 'NONE', #58010, .T. ) ;
#129572 = DIRECTION ( 'NONE',  ( -1.000000000000000000, -0.000000000000000000, -0.000000000000000000 ) ) ;
#129573 = EDGE_CURVE ( 'NONE', #59304, #66247, #132455, .T. ) ;
#129574 = DIRECTION ( 'NONE',  ( -2.557131231893036985E-16, 0.8660254037844384856, -0.5000000000000002220 ) ) ;
#129575 = ORIENTED_EDGE ( 'NONE', *, *, #195168, .T. ) ;
#129577 = ORIENTED_EDGE ( 'NONE', *, *, #169208, .F. ) ;
#129576 = FACE_OUTER_BOUND ( 'NONE', #121299, .T. ) ;
#129578 = VERTEX_POINT ( 'NONE', #192566 ) ;
#129579 = DIRECTION ( 'NONE',  ( 1.000000000000000000, 0.000000000000000000, 0.000000000000000000 ) ) ;
#129580 = ORIENTED_EDGE ( 'NONE', *, *, #242015, .F. ) ;
#129581 = CARTESIAN_POINT ( 'NONE',  ( 21.00000000000000000, 9.750000000011153745, -121.7500000000000426 ) ) ;
#129582 = DIRECTION ( 'NONE',  ( -1.000000000000000000, -0.000000000000000000, -0.000000000000000000 ) ) ;
#129583 = CARTESIAN_POINT ( 'NONE',  ( 21.14999999999999858, 87.65000000001164437, -69.52310748452424605 ) ) ;
#129584 = ORIENTED_EDGE ( 'NONE', *, *, #169002, .T. ) ;
#129585 = DIRECTION ( 'NONE',  ( -1.000000000000000000, -0.000000000000000000, -0.000000000000000000 ) ) ;
#129586 = CARTESIAN_POINT ( 'NONE',  ( -21.07928932188134041, 6.328516656404449492, -167.4011048543455615 ) ) ;
#129587 = CARTESIAN_POINT ( 'NONE',  ( -18.59999999999999787, 66.65000000001198543, -115.3731074845243683 ) ) ;
#129588 = EDGE_CURVE ( 'NONE', #360, #159084, #3448, .T. ) ;
#129590 = ORIENTED_EDGE ( 'NONE', *, *, #164768, .T. ) ;
#129589 = CIRCLE ( 'NONE', #254446, 11.80000000000000426 ) ;
#129592 = ORIENTED_EDGE ( 'NONE', *, *, #95749, .F. ) ;
#129591 = LINE ( 'NONE', #110012, #42611 ) ;
#129594 = EDGE_CURVE ( 'NONE', #98329, #42259, #232995, .T. ) ;
#129593 = FACE_OUTER_BOUND ( 'NONE', #67524, .T. ) ;
#129595 = DIRECTION ( 'NONE',  ( 1.000000000000000000, 0.000000000000000000, 0.000000000000000000 ) ) ;
#129596 = VERTEX_POINT ( 'NONE', #94736 ) ;
#129597 = FACE_OUTER_BOUND ( 'NONE', #26736, .T. ) ;
#129599 = EDGE_CURVE ( 'NONE', #199626, #73216, #119476, .T. ) ;
#129598 = CARTESIAN_POINT ( 'NONE',  ( -13.77178122865954180, 66.54397173950414413, -121.5119094494586847 ) ) ;
#129600 = CIRCLE ( 'NONE', #225233, 0.09999999999998898659 ) ;
#129601 = CARTESIAN_POINT ( 'NONE',  ( 21.05000000000000071, -8.999999999988842703, -157.6060308773475640 ) ) ;
#129602 = EDGE_LOOP ( 'NONE', ( #43431, #45659, #143669 ) ) ;
#129603 = CARTESIAN_POINT ( 'NONE',  ( 18.59999999999999787, 64.21185867012613357, -224.4479740254296303 ) ) ;
#129604 = EDGE_CURVE ( 'NONE', #173093, #50671, #53918, .T. ) ;
#129605 = DIRECTION ( 'NONE',  ( -2.342056488767302165E-15, -0.8490545835447238510, -0.5283051335749973099 ) ) ;
#129606 = EDGE_CURVE ( 'NONE', #167418, #31326, #20612, .T. ) ;
#129607 = VERTEX_POINT ( 'NONE', #42465 ) ;
#129608 = ADVANCED_FACE ( 'NONE', ( #200268, #20365, #122012 ), #24214, .F. ) ;
#129609 = CIRCLE ( 'NONE', #4501, 0.1000000000000013933 ) ;
#129610 = AXIS2_PLACEMENT_3D ( 'NONE', #193889, #180738, #102437 ) ;
#129612 = EDGE_LOOP ( 'NONE', ( #47128, #138944, #238670, #156884, #225218, #52950, #120421, #61389, #226794, #199819, #139396, #109392 ) ) ;
#129611 = AXIS2_PLACEMENT_3D ( 'NONE', #38915, #136703, #54605 ) ;
#129613 = CARTESIAN_POINT ( 'NONE',  ( 21.13461538461538325, 65.38541703798705385, -191.2731074845244166 ) ) ;
#129614 = EDGE_LOOP ( 'NONE', ( #197042, #158423, #24872, #208607 ) ) ;
#129615 = CARTESIAN_POINT ( 'NONE',  ( -21.05000000000000071, 1.115600667400684642E-11, -71.29999999999999716 ) ) ;
#129617 = EDGE_CURVE ( 'NONE', #256073, #212672, #120756, .T. ) ;
#129616 = DIRECTION ( 'NONE',  ( -0.000000000000000000, 7.172728831056617961E-15, -1.000000000000000000 ) ) ;
#129619 = ORIENTED_EDGE ( 'NONE', *, *, #79738, .F. ) ;
#129618 = CARTESIAN_POINT ( 'NONE',  ( 13.88302573338719448, 24.81705829073095515, -232.4789712399791313 ) ) ;
#129620 = CARTESIAN_POINT ( 'NONE',  ( -18.59999999999999787, 1.261786168565025568, -8.086498963545480478 ) ) ;
#129621 = CYLINDRICAL_SURFACE ( 'NONE', #232399, 7.900000000000003908 ) ;
#129622 = LINE ( 'NONE', #151776, #218309 ) ;
#129623 = CARTESIAN_POINT ( 'NONE',  ( 21.13736287352038445, 8.046642376395153562, -42.75000000000000000 ) ) ;
#129624 = CARTESIAN_POINT ( 'NONE',  ( -18.50000000000000000, 77.63717271298195044, -57.94095411905229298 ) ) ;
#129625 = DIRECTION ( 'NONE',  ( -1.000000000000000000, 2.952720810173289112E-16, 2.061873921506763405E-30 ) ) ;
#129627 = EDGE_LOOP ( 'NONE', ( #161118, #24556, #207840, #41722 ) ) ;
#129626 = CARTESIAN_POINT ( 'NONE',  ( 20.85000000000000142, 64.35000000001170406, -69.52310748452438816 ) ) ;
#129628 = CARTESIAN_POINT ( 'NONE',  ( 21.11344571971278228, 22.93732951038863632, -230.1555751630206714 ) ) ;
#129629 = AXIS2_PLACEMENT_3D ( 'NONE', #205003, #8123, #225841 ) ;
#129630 = DIRECTION ( 'NONE',  ( 0.000000000000000000, -0.7397360091702802620, 0.6728971962616779878 ) ) ;
#129631 = FACE_OUTER_BOUND ( 'NONE', #68604, .T. ) ;
#129632 = CARTESIAN_POINT ( 'NONE',  ( -20.64999999999999858, 76.00000000001170974, -69.52310748452431710 ) ) ;
#129633 = CARTESIAN_POINT ( 'NONE',  ( 18.49999999999999645, -1.162701749926855266, -75.10000000000003695 ) ) ;
#129634 = ORIENTED_EDGE ( 'NONE', *, *, #210109, .F. ) ;
#129635 = DIRECTION ( 'NONE',  ( 1.000000000000000000, 2.952720810173289112E-16, -0.000000000000000000 ) ) ;
#129636 = CIRCLE ( 'NONE', #217099, 0.1000000000000055844 ) ;
#129637 = VECTOR ( 'NONE', #249852, 1000.000000000000000 ) ;
#129638 = DIRECTION ( 'NONE',  ( 1.000000000000000000, 0.000000000000000000, 0.000000000000000000 ) ) ;
#129639 = DIRECTION ( 'NONE',  ( -1.000000000000000000, 2.952720810173289112E-16, 2.061873921506763405E-30 ) ) ;
#129640 = CIRCLE ( 'NONE', #137995, 0.1000000000000013378 ) ;
#129641 = VERTEX_POINT ( 'NONE', #119456 ) ;
#129643 = EDGE_CURVE ( 'NONE', #129684, #45297, #87214, .T. ) ;
#129642 = DIRECTION ( 'NONE',  ( -3.265361837132814079E-16, 0.4721928772777359007, 0.8814952561688425003 ) ) ;
#129644 = CARTESIAN_POINT ( 'NONE',  ( 20.85000000000000142, 11.65000000000000391, -33.50000000000000000 ) ) ;
#129645 = ORIENTED_EDGE ( 'NONE', *, *, #20427, .F. ) ;
#129646 = CARTESIAN_POINT ( 'NONE',  ( -21.05000000000000071, 6.478078221105993961, -67.09999993530584561 ) ) ;
#129647 = ORIENTED_EDGE ( 'NONE', *, *, #224111, .F. ) ;
#129649 = ADVANCED_FACE ( 'NONE', ( #85409 ), #741, .T. ) ;
#129648 = CARTESIAN_POINT ( 'NONE',  ( -20.94999999999999929, 74.16465844978765176, -124.9679561919613207 ) ) ;
#129651 = EDGE_LOOP ( 'NONE', ( #160383, #255872, #21325, #199353 ) ) ;
#129650 = CARTESIAN_POINT ( 'NONE',  ( 5.551115123125782702E-14, 64.35000000001120668, -3.023107484524792277 ) ) ;
#129652 = AXIS2_PLACEMENT_3D ( 'NONE', #214839, #15382, #174495 ) ;
#129653 = CARTESIAN_POINT ( 'NONE',  ( 23.24999999999999645, 1.115600667400684642E-11, -200.9999999999999432 ) ) ;
#129654 = EDGE_LOOP ( 'NONE', ( #27173, #146027, #23428, #147863 ) ) ;
#129655 = EDGE_CURVE ( 'NONE', #79096, #65394, #166374, .T. ) ;
#129656 = LINE ( 'NONE', #147940, #201169 ) ;
#129657 = ADVANCED_FACE ( 'NONE', ( #144116 ), #120024, .T. ) ;
#129658 = ORIENTED_EDGE ( 'NONE', *, *, #60324, .F. ) ;
#129659 = ORIENTED_EDGE ( 'NONE', *, *, #67340, .T. ) ;
#129660 = CARTESIAN_POINT ( 'NONE',  ( 18.49351773456780634, 85.44302569515717494, -129.3377819584974020 ) ) ;
#129661 = ORIENTED_EDGE ( 'NONE', *, *, #20918, .T. ) ;
#129662 = CARTESIAN_POINT ( 'NONE',  ( 20.88420186297724257, 65.66974365629646115, -63.93601455626049557 ) ) ;
#129663 = ORIENTED_EDGE ( 'NONE', *, *, #3053, .F. ) ;
#129664 = ORIENTED_EDGE ( 'NONE', *, *, #178116, .T. ) ;
#129665 = EDGE_CURVE ( 'NONE', #154024, #92185, #7556, .T. ) ;
#129666 = DIRECTION ( 'NONE',  ( 0.000000000000000000, 0.8814952561688430555, -0.4721928772777346239 ) ) ;
#129667 = DIRECTION ( 'NONE',  ( 1.000000000000000000, 0.000000000000000000, 0.000000000000000000 ) ) ;
#129668 = CARTESIAN_POINT ( 'NONE',  ( -20.94999999999999929, 67.23127455305841238, -235.8551265064783991 ) ) ;
#129669 = VERTEX_POINT ( 'NONE', #161145 ) ;
#129670 = EDGE_CURVE ( 'NONE', #206540, #35640, #45040, .T. ) ;
#129671 = DIRECTION ( 'NONE',  ( -1.000000000000000000, 2.986185139342070877E-16, -6.665775143889692774E-16 ) ) ;
#129672 = CARTESIAN_POINT ( 'NONE',  ( -12.25000000000000178, 66.65000000001258229, -186.7731074845244166 ) ) ;
#129673 = DIRECTION ( 'NONE',  ( 1.000000000000000000, 0.000000000000000000, 0.000000000000000000 ) ) ;
#129674 = VECTOR ( 'NONE', #52544, 1000.000000000000227 ) ;
#129675 = ORIENTED_EDGE ( 'NONE', *, *, #44030, .T. ) ;
#129676 = DIRECTION ( 'NONE',  ( 0.000000000000000000, -7.487053152578127080E-15, 1.000000000000000000 ) ) ;
#129677 = CARTESIAN_POINT ( 'NONE',  ( -23.25000000000000000, -1.164121893230052995, -108.4148480855716485 ) ) ;
#129678 = DIRECTION ( 'NONE',  ( 1.000000000000000000, -1.646408749285562060E-14, -1.073024830501232702E-15 ) ) ;
#129679 = CARTESIAN_POINT ( 'NONE',  ( -20.94999999999999929, -1.135018845899022466, -74.71697688343232358 ) ) ;
#129680 = ORIENTED_EDGE ( 'NONE', *, *, #203542, .T. ) ;
#129681 = CARTESIAN_POINT ( 'NONE',  ( 18.55121869061587958, 10.32747123227773400, -106.0774032850249711 ) ) ;
#129682 = ORIENTED_EDGE ( 'NONE', *, *, #180891, .F. ) ;
#129683 = CARTESIAN_POINT ( 'NONE',  ( -16.87036670365548474, 63.08160062417908165, -212.9922606024214531 ) ) ;
#129684 = VERTEX_POINT ( 'NONE', #124589 ) ;
#129685 = AXIS2_PLACEMENT_3D ( 'NONE', #33013, #156787, #231187 ) ;
#129686 = DIRECTION ( 'NONE',  ( 1.186688945009010077E-16, -1.000000000000000000, -0.000000000000000000 ) ) ;
#129687 = DIRECTION ( 'NONE',  ( 0.000000000000000000, 0.1335171055202901413, 0.9910465087640860649 ) ) ;
#129688 = ADVANCED_FACE ( 'NONE', ( #198976 ), #74233, .F. ) ;
#129689 = ORIENTED_EDGE ( 'NONE', *, *, #143398, .F. ) ;
#129690 = AXIS2_PLACEMENT_3D ( 'NONE', #66339, #104157, #63758 ) ;
#129691 = VERTEX_POINT ( 'NONE', #240670 ) ;
#129693 = VERTEX_POINT ( 'NONE', #123301 ) ;
#129692 = CARTESIAN_POINT ( 'NONE',  ( -15.55912972643741199, 62.32143948325225580, -221.5201728061774986 ) ) ;
#129694 = ADVANCED_FACE ( 'NONE', ( #140264 ), #184537, .F. ) ;
#129695 = CARTESIAN_POINT ( 'NONE',  ( 20.94999999999999574, 74.73821383144729680, -161.9366085209788935 ) ) ;
#129696 = ORIENTED_EDGE ( 'NONE', *, *, #151970, .F. ) ;
#129697 = ADVANCED_FACE ( 'NONE', ( #221097 ), #39933, .F. ) ;
#129698 = CARTESIAN_POINT ( 'NONE',  ( 11.60000000000006004, 63.75000000001119815, -21.02310748452479316 ) ) ;
#129699 = CIRCLE ( 'NONE', #171435, 0.1000000000000033223 ) ;
#129700 = VERTEX_POINT ( 'NONE', #219818 ) ;
#129701 = DIRECTION ( 'NONE',  ( -1.000000000000000000, 0.000000000000000000, 0.000000000000000000 ) ) ;
#129702 = EDGE_CURVE ( 'NONE', #42819, #69180, #107501, .T. ) ;
#129703 = CIRCLE ( 'NONE', #225534, 0.1000000000000028644 ) ;
#129704 = CIRCLE ( 'NONE', #29798, 0.09999999999999731326 ) ;
#129705 = VERTEX_POINT ( 'NONE', #129713 ) ;
#129706 = CARTESIAN_POINT ( 'NONE',  ( 23.25000000000000000, 69.20602499728043711, -247.8456586332460176 ) ) ;
#129707 = VECTOR ( 'NONE', #10741, 1000.000000000000000 ) ;
#129708 = DIRECTION ( 'NONE',  ( 0.000000000000000000, -1.000000000000000000, 0.000000000000000000 ) ) ;
#129709 = AXIS2_PLACEMENT_3D ( 'NONE', #28980, #9354, #88880 ) ;
#129710 = CARTESIAN_POINT ( 'NONE',  ( -23.15000000000000213, 1.115600667400684642E-11, -134.0000000000000000 ) ) ;
#129712 = ORIENTED_EDGE ( 'NONE', *, *, #246333, .T. ) ;
#129711 = CARTESIAN_POINT ( 'NONE',  ( 20.94999999999999929, 76.00000000001193712, -105.9231074845242944 ) ) ;
#129713 = CARTESIAN_POINT ( 'NONE',  ( -18.59999999999999787, -1.164121893230052995, -208.8148480855715832 ) ) ;
#129714 = DIRECTION ( 'NONE',  ( -1.000000000000000000, -0.000000000000000000, -0.000000000000000000 ) ) ;
#129716 = ADVANCED_FACE ( 'NONE', ( #128432 ), #106273, .T. ) ;
#129715 = DIRECTION ( 'NONE',  ( 0.000000000000000000, 1.000000000000000000, 0.000000000000000000 ) ) ;
#129718 = DIRECTION ( 'NONE',  ( 0.000000000000000000, -0.4999999999999689138, -0.8660254037844565822 ) ) ;
#129717 = CARTESIAN_POINT ( 'NONE',  ( -18.39999999999999858, -9.682403433465239573, -140.6568433774128266 ) ) ;
#129719 = DIRECTION ( 'NONE',  ( -0.000000000000000000, 0.2128009952263603677, -0.9770955615653313941 ) ) ;
#129720 = DIRECTION ( 'NONE',  ( 0.000000000000000000, -1.000000000000000000, 0.000000000000000000 ) ) ;
#129721 = DIRECTION ( 'NONE',  ( 1.000000000000000000, 0.000000000000000000, 0.000000000000000000 ) ) ;
#129722 = VECTOR ( 'NONE', #239911, 1000.000000000000000 ) ;
#129723 = CARTESIAN_POINT ( 'NONE',  ( 18.59999999999998366, 36.65892442174935439, -249.5511627012433848 ) ) ;
#129724 = AXIS2_PLACEMENT_3D ( 'NONE', #77994, #237086, #153756 ) ;
#129725 = AXIS2_PLACEMENT_3D ( 'NONE', #134311, #15703, #193035 ) ;
#129726 =( BOUNDED_SURFACE ( )  B_SPLINE_SURFACE ( 3, 2, ( 
 ( #241901, #142785, #243186 ),
 ( #144074, #4566, #60687 ),
 ( #159825, #180661, #102363 ),
 ( #39890, #2000, #222314 ),
 ( #219767, #140219, #161105 ),
 ( #62004, #181944, #702 ) ),
 .UNSPECIFIED., .F., .F., .T. ) 
 B_SPLINE_SURFACE_WITH_KNOTS ( ( 4, 2, 4 ),
 ( 3, 3 ),
 ( 4.712388980384689674, 5.497787143782137953, 6.283185307179586232 ),
 ( 0.000000000000000000, 1.000000000000000000 ),
 .UNSPECIFIED. ) 
 GEOMETRIC_REPRESENTATION_ITEM ( )  RATIONAL_B_SPLINE_SURFACE ( (
 ( 1.000000000000000000, 0.7071067811865475727, 1.000000000000000000),
 ( 1.000000000000000000, 0.7727932973489580748, 1.000000000000000000),
 ( 1.000000000000000000, 0.8282379607652672338, 1.000000000000000000),
 ( 1.000000000000000000, 0.9038128468036616958, 1.000000000000000000),
 ( 1.000000000000000000, 0.9240297172245867108, 1.000000000000000000),
 ( 1.000000000000000000, 0.9238795325112961754, 1.000000000000000000) ) ) 
 REPRESENTATION_ITEM ( '' )  SURFACE ( )  );
#129727 = ORIENTED_EDGE ( 'NONE', *, *, #156590, .F. ) ;
#129728 = ORIENTED_EDGE ( 'NONE', *, *, #84987, .F. ) ;
#129729 = ADVANCED_FACE ( 'NONE', ( #130998 ), #140839, .F. ) ;
#129730 = ORIENTED_EDGE ( 'NONE', *, *, #244879, .T. ) ;
#129731 = CYLINDRICAL_SURFACE ( 'NONE', #2807, 0.09999999999999939493 ) ;
#129732 = EDGE_CURVE ( 'NONE', #47453, #160655, #49247, .T. ) ;
#129733 = FACE_OUTER_BOUND ( 'NONE', #3149, .T. ) ;
#129734 = VERTEX_POINT ( 'NONE', #188400 ) ;
#129735 = DIRECTION ( 'NONE',  ( 1.000000000000000000, 0.000000000000000000, 0.000000000000000000 ) ) ;
#129736 = CARTESIAN_POINT ( 'NONE',  ( -16.89081410710458542, 63.08561305663506857, -213.1230241508039853 ) ) ;
#129737 = FACE_OUTER_BOUND ( 'NONE', #21942, .T. ) ;
#129738 = ORIENTED_EDGE ( 'NONE', *, *, #2408, .F. ) ;
#129739 = ORIENTED_EDGE ( 'NONE', *, *, #192442, .T. ) ;
#129740 = ADVANCED_FACE ( 'NONE', ( #207987 ), #185831, .T. ) ;
#129741 = CARTESIAN_POINT ( 'NONE',  ( 21.05563370358598263, 60.06990615304147241, -221.2897009653380564 ) ) ;
#129742 = DIRECTION ( 'NONE',  ( 0.000000000000000000, -0.4088369013363280513, 0.9126074666063769270 ) ) ;
#129744 = EDGE_CURVE ( 'NONE', #117646, #60099, #230095, .T. ) ;
#129743 = ORIENTED_EDGE ( 'NONE', *, *, #172929, .T. ) ;
#129745 = DIRECTION ( 'NONE',  ( -1.000000000000000000, -0.000000000000000000, 0.000000000000000000 ) ) ;
#129747 = ORIENTED_EDGE ( 'NONE', *, *, #206140, .F. ) ;
#129746 = DIRECTION ( 'NONE',  ( 0.000000000000000000, 0.000000000000000000, -1.000000000000000000 ) ) ;
#129748 = FACE_BOUND ( 'NONE', #212383, .T. ) ;
#129749 = CARTESIAN_POINT ( 'NONE',  ( -17.01825945287482966, 65.95000000001232365, -157.3731074845244393 ) ) ;
#129750 = AXIS2_PLACEMENT_3D ( 'NONE', #167565, #30619, #110126 ) ;
#129752 = ORIENTED_EDGE ( 'NONE', *, *, #198332, .F. ) ;
#129751 = DIRECTION ( 'NONE',  ( -0.000000000000000000, 0.5474227397873200340, -0.8368562265788217491 ) ) ;
#129753 = CARTESIAN_POINT ( 'NONE',  ( -23.15000000000000213, 1.115625160336667635E-11, -102.5000000000000426 ) ) ;
#129754 = CARTESIAN_POINT ( 'NONE',  ( 21.04386569057582079, 64.25000000001217870, -143.3802701327438172 ) ) ;
#129755 = DIRECTION ( 'NONE',  ( -1.000000000000000000, -0.000000000000000000, -0.000000000000000000 ) ) ;
#129756 = CARTESIAN_POINT ( 'NONE',  ( -16.97683809663752186, 12.57413723904469904, -211.9780204941619104 ) ) ;
#129758 = CARTESIAN_POINT ( 'NONE',  ( 20.30531438145591139, 10.09690106110208596, -108.2960178072733868 ) ) ;
#129757 = CARTESIAN_POINT ( 'NONE',  ( -21.05000000000000071, 1.835341550235567887, -45.05515129256298223 ) ) ;
#129759 = CARTESIAN_POINT ( 'NONE',  ( -23.15000000000000213, -11.48912529306489994, -63.89999999999999858 ) ) ;
#129760 = LINE ( 'NONE', #107625, #168442 ) ;
#129761 = DIRECTION ( 'NONE',  ( -1.000000000000000000, 1.646408749285562691E-14, 1.149681084847720908E-28 ) ) ;
#129762 = DIRECTION ( 'NONE',  ( -0.000000000000000000, -6.982962677686266711E-15, 1.000000000000000000 ) ) ;
#129763 = EDGE_CURVE ( 'NONE', #246027, #68319, #153538, .T. ) ;
#129764 = ORIENTED_EDGE ( 'NONE', *, *, #140617, .T. ) ;
#129765 = AXIS2_PLACEMENT_3D ( 'NONE', #71120, #154525, #231472 ) ;
#129766 = EDGE_LOOP ( 'NONE', ( #152281, #185467, #108603, #164426 ) ) ;
#129767 = DIRECTION ( 'NONE',  ( 1.000000000000000000, 0.000000000000000000, 0.000000000000000000 ) ) ;
#129768 = EDGE_LOOP ( 'NONE', ( #17852, #133207 ) ) ;
#129769 = ADVANCED_FACE ( 'NONE', ( #87992 ), #166311, .F. ) ;
#129770 = LINE ( 'NONE', #170242, #23618 ) ;
#129771 = DIRECTION ( 'NONE',  ( 0.000000000000000000, 0.2617529984165180013, 0.9651348961777117541 ) ) ;
#129772 = EDGE_CURVE ( 'NONE', #83361, #205893, #116085, .T. ) ;
#129773 = ORIENTED_EDGE ( 'NONE', *, *, #85953, .F. ) ;
#129774 = CARTESIAN_POINT ( 'NONE',  ( 22.60000000000000142, 11.74956712350054744, -100.3991416309013260 ) ) ;
#129775 =( NAMED_UNIT ( * ) SI_UNIT ( $, .STERADIAN. ) SOLID_ANGLE_UNIT ( ) );
#129776 = EDGE_CURVE ( 'NONE', #156798, #198318, #247075, .T. ) ;
#129778 = VERTEX_POINT ( 'NONE', #29373 ) ;
#129777 = AXIS2_PLACEMENT_3D ( 'NONE', #14344, #33934, #114697 ) ;
#129779 = ORIENTED_EDGE ( 'NONE', *, *, #252873, .F. ) ;
#129780 = ORIENTED_EDGE ( 'NONE', *, *, #179673, .T. ) ;
#129781 = AXIS2_PLACEMENT_3D ( 'NONE', #16365, #174181, #48091 ) ;
#129782 = DIRECTION ( 'NONE',  ( 0.000000000000000000, 0.9126074666063772600, 0.4088369013363274407 ) ) ;
#129783 = DIRECTION ( 'NONE',  ( 0.000000000000000000, 0.000000000000000000, -1.000000000000000000 ) ) ;
#129784 = LINE ( 'NONE', #51503, #126130 ) ;
#129785 = CARTESIAN_POINT ( 'NONE',  ( 19.58285714285715073, 9.015001489659738354, -41.92065281608173422 ) ) ;
#129786 = CARTESIAN_POINT ( 'NONE',  ( 22.50000000000000000, 1.115600667400684642E-11, -67.00000000000004263 ) ) ;
#129788 = DIRECTION ( 'NONE',  ( 1.000000000000000000, 0.000000000000000000, 0.000000000000000000 ) ) ;
#129787 = DIRECTION ( 'NONE',  ( 0.000000000000000000, 0.2605042016806715099, 0.9654727137038706664 ) ) ;
#129789 = DIRECTION ( 'NONE',  ( 2.557131231893037478E-16, 0.8660254037844420383, -0.4999999999999943379 ) ) ;
#129791 = EDGE_LOOP ( 'NONE', ( #210903, #5116, #241821, #159203 ) ) ;
#129790 = DIRECTION ( 'NONE',  ( 1.000000000000000000, 1.186688945009010077E-16, 0.000000000000000000 ) ) ;
#129793 = CARTESIAN_POINT ( 'NONE',  ( -23.25000000000000000, 4.250000000011156409, -112.6500000000000483 ) ) ;
#129792 = CARTESIAN_POINT ( 'NONE',  ( -20.54999999999999716, 85.40000000001198543, -112.9170766071766820 ) ) ;
#129794 = EDGE_CURVE ( 'NONE', #17744, #86948, #24509, .T. ) ;
#129795 = CARTESIAN_POINT ( 'NONE',  ( 21.14999999999999503, -0.09999999998884338825, -155.8504291924551808 ) ) ;
#129796 = ADVANCED_FACE ( 'NONE', ( #149302 ), #7178, .F. ) ;
#129797 = ORIENTED_EDGE ( 'NONE', *, *, #155847, .F. ) ;
#129798 = DIRECTION ( 'NONE',  ( 1.000000000000000000, 0.000000000000000000, 0.000000000000000000 ) ) ;
#129799 = CARTESIAN_POINT ( 'NONE',  ( 21.00000000000000000, 66.25000000001206502, -124.1731074845243654 ) ) ;
#129800 = DIRECTION ( 'NONE',  ( -0.000000000000000000, -6.982962677686266711E-15, 1.000000000000000000 ) ) ;
#129801 = ORIENTED_EDGE ( 'NONE', *, *, #65457, .T. ) ;
#129802 = CIRCLE ( 'NONE', #46575, 0.09999999999998898659 ) ;
#129803 = CARTESIAN_POINT ( 'NONE',  ( -16.83794237512074332, 61.00236442716369822, -220.8997268849512920 ) ) ;
#129804 = DIRECTION ( 'NONE',  ( 0.000000000000000000, 1.000000000000000000, 6.982962677686266711E-15 ) ) ;
#129805 = CARTESIAN_POINT ( 'NONE',  ( 12.47034474403011828, 66.62446189796384033, -87.15323160353354126 ) ) ;
#129806 = ORIENTED_EDGE ( 'NONE', *, *, #198246, .F. ) ;
#129807 = ORIENTED_EDGE ( 'NONE', *, *, #143591, .F. ) ;
#129808 = CARTESIAN_POINT ( 'NONE',  ( -18.50000000000000000, 10.29270135741298375, -172.9573618871519614 ) ) ;
#129809 = CARTESIAN_POINT ( 'NONE',  ( -20.64999999999999858, 2.400000000011155432, -87.27537807723794572 ) ) ;
#129810 = DIRECTION ( 'NONE',  ( 1.000000000000000000, 0.000000000000000000, 0.000000000000000000 ) ) ;
#129811 = ORIENTED_EDGE ( 'NONE', *, *, #226731, .F. ) ;
#129812 = CARTESIAN_POINT ( 'NONE',  ( 23.40000000000005542, 87.51781941433023349, -34.28670414799875488 ) ) ;
#129813 = AXIS2_PLACEMENT_3D ( 'NONE', #206262, #163291, #182869 ) ;
#129814 = CIRCLE ( 'NONE', #88094, 11.75000000000001066 ) ;
#129815 = CIRCLE ( 'NONE', #254675, 0.09999999999999939493 ) ;
#129816 = DIRECTION ( 'NONE',  ( 1.000000000000000000, -0.000000000000000000, 0.000000000000000000 ) ) ;
#129817 = DIRECTION ( 'NONE',  ( 2.168404344971008868E-16, -0.000000000000000000, 1.000000000000000000 ) ) ;
#129818 = ADVANCED_FACE ( 'NONE', ( #111435 ), #91868, .F. ) ;
#129819 = VERTEX_POINT ( 'NONE', #125846 ) ;
#129820 = SPHERICAL_SURFACE ( 'NONE', #159433, 0.1000000000000000056 ) ;
#129822 = ORIENTED_EDGE ( 'NONE', *, *, #218386, .T. ) ;
#129821 = DIRECTION ( 'NONE',  ( 0.000000000000000000, 0.000000000000000000, 1.000000000000000000 ) ) ;
#129823 = FACE_OUTER_BOUND ( 'NONE', #14601, .T. ) ;
#129824 = CARTESIAN_POINT ( 'NONE',  ( -21.05000000000000071, 36.65892442174472876, -249.5511627012454596 ) ) ;
#129825 = DIRECTION ( 'NONE',  ( 0.000000000000000000, -0.9770955615653313941, -0.2128009952263606730 ) ) ;
#129826 = DIRECTION ( 'NONE',  ( 1.000000000000000000, -0.000000000000000000, -0.000000000000000000 ) ) ;
#129827 = CYLINDRICAL_SURFACE ( 'NONE', #83806, 0.1000000000000028644 ) ;
#129828 = CARTESIAN_POINT ( 'NONE',  ( 18.59999999999999787, 45.93315328338058379, -256.6017782078560003 ) ) ;
#129829 = FACE_OUTER_BOUND ( 'NONE', #199074, .T. ) ;
#129830 = VECTOR ( 'NONE', #170324, 1000.000000000000000 ) ;
#129831 = ORIENTED_EDGE ( 'NONE', *, *, #193584, .F. ) ;
#129832 = CARTESIAN_POINT ( 'NONE',  ( -14.00000000000000178, 9.849999999999978328, -16.75000000000000355 ) ) ;
#129833 = CARTESIAN_POINT ( 'NONE',  ( 23.15000000000000213, -8.999999999988842703, -191.1060308773475072 ) ) ;
#129834 = CARTESIAN_POINT ( 'NONE',  ( -21.14999999999999858, -11.64999999998884483, -100.5000000000000284 ) ) ;
#129835 = DIRECTION ( 'NONE',  ( -1.000000000000000000, 0.000000000000000000, 0.000000000000000000 ) ) ;
#129836 = EDGE_CURVE ( 'NONE', #77400, #177630, #3625, .T. ) ;
#129837 = CARTESIAN_POINT ( 'NONE',  ( 21.05000000000000071, 6.304516329275450914, -167.5211033080591392 ) ) ;
#129838 = DIRECTION ( 'NONE',  ( -1.000000000000000000, 0.000000000000000000, 0.000000000000000000 ) ) ;
#129839 = ORIENTED_EDGE ( 'NONE', *, *, #16108, .F. ) ;
#129840 = ORIENTED_EDGE ( 'NONE', *, *, #249137, .T. ) ;
#129841 = FACE_OUTER_BOUND ( 'NONE', #45992, .T. ) ;
#129842 = CARTESIAN_POINT ( 'NONE',  ( 21.05000000000000071, 0.000000000000000000, -37.50000000000000000 ) ) ;
#129843 = CARTESIAN_POINT ( 'NONE',  ( -20.94999999999999929, 76.00000000001170974, -69.52310748452431710 ) ) ;
#129844 = AXIS2_PLACEMENT_3D ( 'NONE', #79644, #139611, #40581 ) ;
#129845 = FACE_OUTER_BOUND ( 'NONE', #120399, .T. ) ;
#129846 = LINE ( 'NONE', #89437, #243188 ) ;
#129847 = CARTESIAN_POINT ( 'NONE',  ( -17.11825945287481332, 66.05000000001224691, -149.2731074845244450 ) ) ;
#129848 = TOROIDAL_SURFACE ( 'NONE', #9064, 7.800000000000000711, 0.1000000000000000056 ) ;
#129849 = FACE_OUTER_BOUND ( 'NONE', #135244, .T. ) ;
#129850 = CARTESIAN_POINT ( 'NONE',  ( -16.93658211146646408, 9.994108662352344297, -113.0957049300443487 ) ) ;
#129851 = CIRCLE ( 'NONE', #138219, 0.09999999999998898659 ) ;
#129852 = DIRECTION ( 'NONE',  ( -1.000000000000000000, 0.000000000000000000, 0.000000000000000000 ) ) ;
#129853 = CIRCLE ( 'NONE', #146412, 0.1000000000000026007 ) ;
#129854 = ORIENTED_EDGE ( 'NONE', *, *, #33485, .F. ) ;
#129855 = CARTESIAN_POINT ( 'NONE',  ( -21.14999999999999858, 64.18196446391819165, -247.0985338183330668 ) ) ;
#129856 = AXIS2_PLACEMENT_3D ( 'NONE', #106723, #186293, #207138 ) ;
#129857 = ORIENTED_EDGE ( 'NONE', *, *, #169743, .F. ) ;
#129858 = CARTESIAN_POINT ( 'NONE',  ( 20.94999999999999929, 20.42498087366621817, -235.1829032864613396 ) ) ;
#129859 = CARTESIAN_POINT ( 'NONE',  ( 21.72449340488909897, 10.28395627750227703, -154.8500000000000227 ) ) ;
#129860 = DIRECTION ( 'NONE',  ( 1.000000000000000000, 0.000000000000000000, 0.000000000000000000 ) ) ;
#129861 = CARTESIAN_POINT ( 'NONE',  ( -20.94999999999999929, 64.40000000001263913, -196.5949042542488883 ) ) ;
#129863 = CARTESIAN_POINT ( 'NONE',  ( 18.43466021071409955, 85.49419069046821562, -62.90604592439652265 ) ) ;
#129862 = TOROIDAL_SURFACE ( 'NONE', #200620, 4.900000000000003020, 0.1000000000000000056 ) ;
#129864 = DIRECTION ( 'NONE',  ( 0.000000000000000000, -0.9126074666063769270, -0.4088369013363280513 ) ) ;
#129865 = ORIENTED_EDGE ( 'NONE', *, *, #238838, .F. ) ;
#129866 = CARTESIAN_POINT ( 'NONE',  ( -23.25000000000000000, -8.596261682231832069, -158.0498724828497359 ) ) ;
#129867 = AXIS2_PLACEMENT_3D ( 'NONE', #66945, #209029, #166085 ) ;
#129868 = DIRECTION ( 'NONE',  ( 1.000000000000000000, 0.000000000000000000, 0.000000000000000000 ) ) ;
#129870 = EDGE_CURVE ( 'NONE', #41664, #241914, #141033, .T. ) ;
#129869 = DIRECTION ( 'NONE',  ( 0.000000000000000000, -0.1455152366551721865, -0.9893560106964475187 ) ) ;
#129871 = DIRECTION ( 'NONE',  ( 0.000000000000000000, -1.000000000000000000, -0.000000000000000000 ) ) ;
#129872 = AXIS2_PLACEMENT_3D ( 'NONE', #3588, #27044, #201787 ) ;
#129873 = DIRECTION ( 'NONE',  ( 0.000000000000000000, -1.000000000000000000, -6.860497997771531562E-15 ) ) ;
#129874 = ORIENTED_EDGE ( 'NONE', *, *, #182837, .T. ) ;
#129875 = CIRCLE ( 'NONE', #17459, 0.09999999999998898659 ) ;
#129876 = CARTESIAN_POINT ( 'NONE',  ( -16.78055652883087134, 9.946776916136505164, -79.66079183759246973 ) ) ;
#129878 = EDGE_CURVE ( 'NONE', #151746, #185310, #36989, .T. ) ;
#129877 = CARTESIAN_POINT ( 'NONE',  ( -16.94445028196807002, 9.992063609708893068, -188.3926698215815350 ) ) ;
#129879 = ORIENTED_EDGE ( 'NONE', *, *, #234843, .T. ) ;
#129880 = CIRCLE ( 'NONE', #104909, 0.09999999999999939493 ) ;
#129881 = ORIENTED_EDGE ( 'NONE', *, *, #256323, .F. ) ;
#129883 = EDGE_CURVE ( 'NONE', #250167, #232336, #199282, .T. ) ;
#129882 = DIRECTION ( 'NONE',  ( 0.000000000000000000, -0.1569827930593259702, 0.9876013379310970564 ) ) ;
#129884 = CARTESIAN_POINT ( 'NONE',  ( 21.05000000000000071, -9.500000000000000000, -23.60603087734755690 ) ) ;
#129885 = ORIENTED_EDGE ( 'NONE', *, *, #97952, .T. ) ;
#129886 = PLANE ( 'NONE',  #162985 ) ;
#129887 = DIRECTION ( 'NONE',  ( 1.000000000000000000, 0.000000000000000000, 0.000000000000000000 ) ) ;
#129888 = ADVANCED_FACE ( 'NONE', ( #16213 ), #250925, .F. ) ;
#129889 = AXIS2_PLACEMENT_3D ( 'NONE', #209125, #249560, #130874 ) ;
#129890 = ORIENTED_EDGE ( 'NONE', *, *, #233429, .T. ) ;
#129891 = VECTOR ( 'NONE', #250123, 1000.000000000000000 ) ;
#129892 = TOROIDAL_SURFACE ( 'NONE', #885, 2.699999999999999734, 0.1000000000000000056 ) ;
#129893 = CIRCLE ( 'NONE', #79993, 0.1000000000000124678 ) ;
#129894 = DIRECTION ( 'NONE',  ( -1.000000000000000000, 0.000000000000000000, 0.000000000000000000 ) ) ;
#129895 = EDGE_LOOP ( 'NONE', ( #51074, #87971, #48528, #216376 ) ) ;
#129896 = DIRECTION ( 'NONE',  ( -1.000000000000000000, 0.000000000000000000, 0.000000000000000000 ) ) ;
#129898 = ADVANCED_FACE ( 'NONE', ( #95708 ), #253500, .F. ) ;
#129897 = CARTESIAN_POINT ( 'NONE',  ( 20.99999999999997868, 1.115600667400684642E-11, -167.4999999999999716 ) ) ;
#129900 = VERTEX_POINT ( 'NONE', #74906 ) ;
#129899 = DIRECTION ( 'NONE',  ( 1.000000000000000000, -0.000000000000000000, -0.000000000000000000 ) ) ;
#129901 = CARTESIAN_POINT ( 'NONE',  ( -18.59999999999999787, 1.866714910068465239, -179.2526752462819672 ) ) ;
#129902 = CARTESIAN_POINT ( 'NONE',  ( -21.64999999999999858, 44.83341466285084209, -237.8352457803185871 ) ) ;
#129903 = CARTESIAN_POINT ( 'NONE',  ( -22.50000000000000000, 11.36146383068193622, -198.4232501820394816 ) ) ;
#129904 = CARTESIAN_POINT ( 'NONE',  ( 20.00000000000000355, 11.61130914238355771, 16.50000000000000000 ) ) ;
#129905 = CYLINDRICAL_SURFACE ( 'NONE', #12654, 0.09999999999998898659 ) ;
#129906 = CARTESIAN_POINT ( 'NONE',  ( 20.94999999999999574, 0.5663372425336981042, -209.0641885820623997 ) ) ;
#129907 = DIRECTION ( 'NONE',  ( 0.000000000000000000, -7.086529944415894657E-15, 1.000000000000000000 ) ) ;
#129909 = ORIENTED_EDGE ( 'NONE', *, *, #209895, .T. ) ;
#129908 = DIRECTION ( 'NONE',  ( 0.000000000000000000, 0.9229812358756199764, -0.3848449534832346086 ) ) ;
#129910 = VERTEX_POINT ( 'NONE', #151877 ) ;
#129912 = CARTESIAN_POINT ( 'NONE',  ( -14.87770893841226894, 9.430637101707898040, -85.26826061806100654 ) ) ;
#129911 = CARTESIAN_POINT ( 'NONE',  ( -23.25000000000000000, 87.08727414655710675, -199.6327537731849873 ) ) ;
#129914 = VERTEX_POINT ( 'NONE', #77419 ) ;
#129913 = DIRECTION ( 'NONE',  ( -0.000000000000000000, 0.000000000000000000, -1.000000000000000000 ) ) ;
#129915 = EDGE_LOOP ( 'NONE', ( #241489, #103670, #108805, #138579 ) ) ;
#129916 = DIRECTION ( 'NONE',  ( 1.000000000000000000, -0.000000000000000000, -0.000000000000000000 ) ) ;
#129917 = DIRECTION ( 'NONE',  ( 0.000000000000000000, -0.4834676483507011624, -0.8753622295931228203 ) ) ;
#129918 = CARTESIAN_POINT ( 'NONE',  ( 20.94999999999999574, 87.65000000001161595, -66.42310748452423752 ) ) ;
#129919 = CARTESIAN_POINT ( 'NONE',  ( -20.93302460841142931, 10.31565961587945246, -173.0364194119178478 ) ) ;
#129920 = CARTESIAN_POINT ( 'NONE',  ( -21.29999999999995808, 76.00000000001234923, -165.9731074845243768 ) ) ;
#129921 = CARTESIAN_POINT ( 'NONE',  ( -21.14999999999994174, 83.90000000001120384, -37.27310748452479316 ) ) ;
#129922 = SPHERICAL_SURFACE ( 'NONE', #14609, 0.1000000000000000056 ) ;
#129923 = VERTEX_POINT ( 'NONE', #232684 ) ;
#129924 = ORIENTED_EDGE ( 'NONE', *, *, #234532, .F. ) ;
#129925 = CARTESIAN_POINT ( 'NONE',  ( 20.90000000000000213, 11.50977166988710820, 1.786320531569725478 ) ) ;
#129926 = ORIENTED_EDGE ( 'NONE', *, *, #73307, .F. ) ;
#129927 = CARTESIAN_POINT ( 'NONE',  ( 15.74999999999999645, 26.54497872210689735, -232.9592037335782209 ) ) ;
#129928 = VERTEX_POINT ( 'NONE', #214384 ) ;
#129929 = DIRECTION ( 'NONE',  ( 2.840903330521633255E-16, 0.8700118002898357128, -0.4930308989875171188 ) ) ;
#129930 = ADVANCED_FACE ( 'NONE', ( #98247 ), #33225, .T. ) ;
#129931 = VECTOR ( 'NONE', #27574, 1000.000000000000000 ) ;
#129932 = LINE ( 'NONE', #191241, #184396 ) ;
#129933 = CARTESIAN_POINT ( 'NONE',  ( 21.05000000000000071, 1.115600667400684642E-11, -169.4000000000000625 ) ) ;
#129934 = ORIENTED_EDGE ( 'NONE', *, *, #82573, .T. ) ;
#129936 = EDGE_CURVE ( 'NONE', #140091, #75404, #145093, .T. ) ;
#129935 = LINE ( 'NONE', #150802, #478 ) ;
#129937 = EDGE_LOOP ( 'NONE', ( #201840, #204153, #56496, #89788 ) ) ;
#129938 = DIRECTION ( 'NONE',  ( 1.000000000000000000, 0.000000000000000000, 0.000000000000000000 ) ) ;
#129939 = FACE_OUTER_BOUND ( 'NONE', #246575, .T. ) ;
#129940 = EDGE_CURVE ( 'NONE', #207052, #180463, #72325, .T. ) ;
#129941 = ORIENTED_EDGE ( 'NONE', *, *, #112105, .F. ) ;
#129943 = CARTESIAN_POINT ( 'NONE',  ( -20.54999999999999716, 66.65000000001187175, -90.77310748452437394 ) ) ;
#129942 = CIRCLE ( 'NONE', #204786, 0.1999999999999987899 ) ;
#129944 = ORIENTED_EDGE ( 'NONE', *, *, #175225, .T. ) ;
#129947 = ORIENTED_EDGE ( 'NONE', *, *, #87536, .T. ) ;
#129946 = CARTESIAN_POINT ( 'NONE',  ( 18.55121869061587958, 46.45193731540634019, -243.0811559066744110 ) ) ;
#129945 = LINE ( 'NONE', #12613, #132548 ) ;
#129948 = CYLINDRICAL_SURFACE ( 'NONE', #23007, 0.09999999999999892308 ) ;
#129949 = ORIENTED_EDGE ( 'NONE', *, *, #250870, .T. ) ;
#129950 = VECTOR ( 'NONE', #216805, 1000.000000000000000 ) ;
#129951 = CARTESIAN_POINT ( 'NONE',  ( -23.15000000000000213, 71.85000000001186038, -90.67310748452433700 ) ) ;
#129952 = ORIENTED_EDGE ( 'NONE', *, *, #66930, .F. ) ;
#129954 = EDGE_CURVE ( 'NONE', #220391, #174834, #61912, .T. ) ;
#129953 = CARTESIAN_POINT ( 'NONE',  ( 0.9000000000000547562, 64.25000000001119815, -10.02310748452479139 ) ) ;
#129955 = ORIENTED_EDGE ( 'NONE', *, *, #9068, .F. ) ;
#129956 = CARTESIAN_POINT ( 'NONE',  ( 21.05000000000000071, -12.41227409413852811, -64.00000000000000000 ) ) ;
#129957 = PLANE ( 'NONE',  #180310 ) ;
#129958 = CARTESIAN_POINT ( 'NONE',  ( 21.30000000000002558, 1.115600667400684642E-11, -134.0000000000000000 ) ) ;
#129959 = EDGE_CURVE ( 'NONE', #139023, #205773, #132276, .T. ) ;
#129960 = DIRECTION ( 'NONE',  ( 1.000000000000000000, -0.000000000000000000, -0.000000000000000000 ) ) ;
#129961 = CIRCLE ( 'NONE', #163322, 0.1000000000000076522 ) ;
#129962 = VERTEX_POINT ( 'NONE', #254748 ) ;
#129963 = CARTESIAN_POINT ( 'NONE',  ( -16.94062896051973865, 44.07468280125904414, -235.2793588221107086 ) ) ;
#129964 = CARTESIAN_POINT ( 'NONE',  ( -12.47155713865592119, 66.62433047358651095, -154.1553174751385313 ) ) ;
#129965 = VERTEX_POINT ( 'NONE', #76148 ) ;
#129966 = DIRECTION ( 'NONE',  ( 2.952720810173289112E-16, -1.000000000000000000, -0.000000000000000000 ) ) ;
#129967 = ORIENTED_EDGE ( 'NONE', *, *, #122331, .F. ) ;
#129968 = DIRECTION ( 'NONE',  ( -0.000000000000000000, 0.9969158384938637818, -0.07847809223010315804 ) ) ;
#129969 = VERTEX_POINT ( 'NONE', #96963 ) ;
#129970 = ADVANCED_FACE ( 'NONE', ( #155731 ), #86825, .T. ) ;
#129971 = DIRECTION ( 'NONE',  ( 0.000000000000000000, 0.8814952561688444987, -0.4721928772777320149 ) ) ;
#129972 = CARTESIAN_POINT ( 'NONE',  ( -18.59999999999999787, 47.16152503674116048, -255.1462838189583238 ) ) ;
#129974 = VERTEX_POINT ( 'NONE', #37066 ) ;
#129973 = DIRECTION ( 'NONE',  ( 1.000000000000000000, 0.000000000000000000, 0.000000000000000000 ) ) ;
#129975 = EDGE_CURVE ( 'NONE', #165339, #38619, #13624, .T. ) ;
#129976 = DIRECTION ( 'NONE',  ( 0.9880948137434723000, 0.1538461538461484146, -0.000000000000000000 ) ) ;
#129977 = ORIENTED_EDGE ( 'NONE', *, *, #241537, .T. ) ;
#129978 = EDGE_CURVE ( 'NONE', #107983, #229722, #181175, .T. ) ;
#129979 = CARTESIAN_POINT ( 'NONE',  ( 23.14999999999999858, 70.40000000001207070, -124.1178414656112352 ) ) ;
#129980 = CIRCLE ( 'NONE', #80072, 11.70000000000000284 ) ;
#129981 = CARTESIAN_POINT ( 'NONE',  ( -23.25000000000000000, 7.788796164756791818, -245.4641525896719543 ) ) ;
#129982 = ORIENTED_EDGE ( 'NONE', *, *, #14131, .F. ) ;
#129983 = VECTOR ( 'NONE', #77252, 1000.000000000000000 ) ;
#129984 = DIRECTION ( 'NONE',  ( 0.000000000000000000, 6.982962677686266711E-15, -1.000000000000000000 ) ) ;
#129985 = CARTESIAN_POINT ( 'NONE',  ( 19.99999999999998934, 11.65000000000000391, -21.25000000000000000 ) ) ;
#129986 = EDGE_LOOP ( 'NONE', ( #106424, #155013, #68407, #51054 ) ) ;
#129987 = CARTESIAN_POINT ( 'NONE',  ( -20.64999999999999858, 71.75000000001229239, -157.7731074845243882 ) ) ;
#129988 = ORIENTED_EDGE ( 'NONE', *, *, #81973, .F. ) ;
#129989 = CARTESIAN_POINT ( 'NONE',  ( -23.25000000000000000, 84.59626168225447884, -45.47323500167453858 ) ) ;
#129990 = DIRECTION ( 'NONE',  ( 0.000000000000000000, 1.000000000000000000, 0.000000000000000000 ) ) ;
#129991 = ADVANCED_FACE ( 'NONE', ( #172742 ), #113990, .T. ) ;
#129992 = ADVANCED_FACE ( 'NONE', ( #153173 ), #111801, .T. ) ;
#129993 = CIRCLE ( 'NONE', #96669, 0.5000000000000014433 ) ;
#129996 = EDGE_LOOP ( 'NONE', ( #117489, #241442, #194344, #43946 ) ) ;
#129995 = EDGE_LOOP ( 'NONE', ( #178300, #64396, #74874 ) ) ;
#129994 = DIRECTION ( 'NONE',  ( 0.000000000000000000, -1.000000000000000000, 0.000000000000000000 ) ) ;
#129997 = CARTESIAN_POINT ( 'NONE',  ( -18.50000000000000000, 10.29270135741298375, -206.4573618871519045 ) ) ;
#129998 = CARTESIAN_POINT ( 'NONE',  ( -20.94999999999999929, 64.25000000001232081, -163.0083017138704236 ) ) ;
#130000 = EDGE_CURVE ( 'NONE', #209151, #146391, #216938, .T. ) ;
#129999 = CARTESIAN_POINT ( 'NONE',  ( -16.93658211146644987, 9.994108662341188776, -20.90429506995567621 ) ) ;
#130002 = CARTESIAN_POINT ( 'NONE',  ( -23.39999999999994529, 76.00000000001119815, -36.02310748452479316 ) ) ;
#130001 = LINE ( 'NONE', #128752, #206609 ) ;
#130003 = DIRECTION ( 'NONE',  ( 0.000000000000000000, -6.982962677686266711E-15, 1.000000000000000000 ) ) ;
#130004 = DIRECTION ( 'NONE',  ( 0.000000000000000000, 0.9876197685951252359, -0.1568667991644863424 ) ) ;
#130005 = DIRECTION ( 'NONE',  ( -0.000000000000000000, -0.000000000000000000, 1.000000000000000000 ) ) ;
#130006 = AXIS2_PLACEMENT_3D ( 'NONE', #72013, #231096, #193238 ) ;
#130007 = FACE_OUTER_BOUND ( 'NONE', #127426, .T. ) ;
#130008 = ORIENTED_EDGE ( 'NONE', *, *, #38589, .F. ) ;
#130009 = ORIENTED_EDGE ( 'NONE', *, *, #80610, .F. ) ;
#130010 = DIRECTION ( 'NONE',  ( 0.000000000000000000, 0.000000000000000000, -1.000000000000000000 ) ) ;
#130012 = ORIENTED_EDGE ( 'NONE', *, *, #19691, .F. ) ;
#130011 = CARTESIAN_POINT ( 'NONE',  ( -18.39999999999999858, 11.75000000001113953, -42.75000000000000000 ) ) ;
#130013 = ORIENTED_EDGE ( 'NONE', *, *, #40616, .T. ) ;
#130014 = CIRCLE ( 'NONE', #17594, 0.09999999999998807065 ) ;
#130015 = EDGE_LOOP ( 'NONE', ( #224119, #160797, #97359, #142668 ) ) ;
#130016 = CARTESIAN_POINT ( 'NONE',  ( 20.95512840106804120, 43.45157668952643348, -234.8669352659592846 ) ) ;
#130017 = TOROIDAL_SURFACE ( 'NONE', #217510, 0.2000000000000000111, 0.1000000000000000056 ) ;
#130018 = ADVANCED_FACE ( 'NONE', ( #40918 ), #180404, .T. ) ;
#130019 = VERTEX_POINT ( 'NONE', #22629 ) ;
#130020 = CIRCLE ( 'NONE', #75884, 0.5000000000000004441 ) ;
#130022 = AXIS2_PLACEMENT_3D ( 'NONE', #250433, #71820, #140762 ) ;
#130021 = DIRECTION ( 'NONE',  ( 1.000000000000000000, 7.304098846218133681E-16, -4.607487905232622991E-31 ) ) ;
#130024 = EDGE_CURVE ( 'NONE', #126194, #192257, #178458, .T. ) ;
#130023 = CYLINDRICAL_SURFACE ( 'NONE', #127967, 1.749999999999999778 ) ;
#130025 = VECTOR ( 'NONE', #214062, 1000.000000000000227 ) ;
#130027 = ORIENTED_EDGE ( 'NONE', *, *, #167776, .T. ) ;
#130026 = VERTEX_POINT ( 'NONE', #102110 ) ;
#130028 = ORIENTED_EDGE ( 'NONE', *, *, #55718, .T. ) ;
#130029 = VECTOR ( 'NONE', #84567, 1000.000000000000000 ) ;
#130030 = ORIENTED_EDGE ( 'NONE', *, *, #50789, .F. ) ;
#130031 = ORIENTED_EDGE ( 'NONE', *, *, #178890, .T. ) ;
#130032 = EDGE_CURVE ( 'NONE', #162761, #170728, #238601, .T. ) ;
#130033 = CARTESIAN_POINT ( 'NONE',  ( -22.39999999999999858, 11.36188319272496727, -198.4231588494578773 ) ) ;
#130034 = CARTESIAN_POINT ( 'NONE',  ( 21.05193202509564543, 43.38332961584228542, -234.7878372896277881 ) ) ;
#130035 = DIRECTION ( 'NONE',  ( -1.000000000000000000, 0.000000000000000000, 0.000000000000000000 ) ) ;
#130038 = ADVANCED_FACE ( 'NONE', ( #218207 ), #220801, .F. ) ;
#130037 = ORIENTED_EDGE ( 'NONE', *, *, #222853, .T. ) ;
#130036 = CARTESIAN_POINT ( 'NONE',  ( -23.15000000000000213, 0.000000000000000000, -33.50000000000000000 ) ) ;
#130039 = PLANE ( 'NONE',  #70024 ) ;
#130040 = DIRECTION ( 'NONE',  ( 1.186688945009009831E-16, -1.000000000000000000, 0.000000000000000000 ) ) ;
#130042 = ORIENTED_EDGE ( 'NONE', *, *, #151213, .T. ) ;
#130041 = CARTESIAN_POINT ( 'NONE',  ( -20.94999999999999929, 68.03098227380377239, -227.7073825336181869 ) ) ;
#130043 = LINE ( 'NONE', #145758, #109517 ) ;
#130044 = ORIENTED_EDGE ( 'NONE', *, *, #159107, .T. ) ;
#130045 = ADVANCED_FACE ( 'NONE', ( #163411 ), #209327, .F. ) ;
#130046 = CARTESIAN_POINT ( 'NONE',  ( -20.94999999999999929, -12.41227409414968541, -30.50000000000000000 ) ) ;
#130047 = CIRCLE ( 'NONE', #142520, 0.1000000000000054040 ) ;
#130048 = ORIENTED_EDGE ( 'NONE', *, *, #177007, .F. ) ;
#130049 = TOROIDAL_SURFACE ( 'NONE', #171798, 12.97499999999999787, 0.1000000000000000056 ) ;
#130050 = DIRECTION ( 'NONE',  ( 1.734723475976817507E-14, -6.982962677686266711E-15, 1.000000000000000000 ) ) ;
#130051 = CARTESIAN_POINT ( 'NONE',  ( 18.49999999999999645, 1.115600667400684642E-11, -200.9999999999999432 ) ) ;
#130053 = ORIENTED_EDGE ( 'NONE', *, *, #165815, .T. ) ;
#130052 = VECTOR ( 'NONE', #137612, 1000.000000000000000 ) ;
#130054 = AXIS2_PLACEMENT_3D ( 'NONE', #11751, #172128, #156409 ) ;
#130056 = CARTESIAN_POINT ( 'NONE',  ( 21.13736287352038445, 67.95335762362807941, -127.2731074845243597 ) ) ;
#130055 = LINE ( 'NONE', #250019, #173904 ) ;
#130057 = CIRCLE ( 'NONE', #142528, 0.1000000000000028644 ) ;
#130058 = DIRECTION ( 'NONE',  ( -1.000000000000000000, -3.265361837132813093E-16, 0.000000000000000000 ) ) ;
#130059 = EDGE_CURVE ( 'NONE', #19024, #241094, #239092, .T. ) ;
#130060 = CARTESIAN_POINT ( 'NONE',  ( -21.45000000000000284, 7.708578643773852157, -188.7499999999999716 ) ) ;
#130061 = DIRECTION ( 'NONE',  ( 0.000000000000000000, 0.9910827722268055195, -0.1332476588733540468 ) ) ;
#130062 = EDGE_CURVE ( 'NONE', #188779, #129556, #211756, .T. ) ;
#130064 = ORIENTED_EDGE ( 'NONE', *, *, #55824, .T. ) ;
#130063 = CIRCLE ( 'NONE', #184798, 0.09999999999999939493 ) ;
#130065 = ORIENTED_EDGE ( 'NONE', *, *, #198123, .T. ) ;
#130066 = CIRCLE ( 'NONE', #84225, 0.09999999999998898659 ) ;
#130067 = DIRECTION ( 'NONE',  ( 0.000000000000000000, -1.000000000000000000, -0.000000000000000000 ) ) ;
#130068 = CYLINDRICAL_SURFACE ( 'NONE', #181588, 12.87500000000000178 ) ;
#130069 = ORIENTED_EDGE ( 'NONE', *, *, #206612, .T. ) ;
#130070 = DIRECTION ( 'NONE',  ( 0.000000000000000000, -1.000000000000000000, 0.000000000000000000 ) ) ;
#130071 = ORIENTED_EDGE ( 'NONE', *, *, #232382, .T. ) ;
#130072 = ADVANCED_FACE ( 'NONE', ( #63006 ), #236676, .T. ) ;
#130073 = CARTESIAN_POINT ( 'NONE',  ( -22.59999970745345976, -0.009356377315832288197, -55.24948679233083482 ) ) ;
#130074 = AXIS2_PLACEMENT_3D ( 'NONE', #158629, #98579, #238123 ) ;
#130075 = LINE ( 'NONE', #135199, #179328 ) ;
#130076 = DIRECTION ( 'NONE',  ( 0.000000000000000000, 0.000000000000000000, -1.000000000000000000 ) ) ;
#130077 = VERTEX_POINT ( 'NONE', #202527 ) ;
#130078 = DIRECTION ( 'NONE',  ( -0.000000000000000000, 0.000000000000000000, -1.000000000000000000 ) ) ;
#130079 = EDGE_CURVE ( 'NONE', #198869, #62294, #119148, .T. ) ;
#130080 = AXIS2_PLACEMENT_3D ( 'NONE', #75058, #82688, #3169 ) ;
#130081 = VECTOR ( 'NONE', #48121, 1000.000000000000000 ) ;
#130082 = ORIENTED_EDGE ( 'NONE', *, *, #60001, .T. ) ;
#130084 = EDGE_LOOP ( 'NONE', ( #193436, #158925, #196622, #89666 ) ) ;
#130083 = AXIS2_PLACEMENT_3D ( 'NONE', #157426, #23037, #21737 ) ;
#130085 = EDGE_LOOP ( 'NONE', ( #88565, #220471, #75447, #230727 ) ) ;
#130086 = ADVANCED_FACE ( 'NONE', ( #203806 ), #177849, .F. ) ;
#130087 = CARTESIAN_POINT ( 'NONE',  ( -23.25000000000000000, -1.835859311443637010, -45.00443916879852679 ) ) ;
#130088 = CARTESIAN_POINT ( 'NONE',  ( -22.39999999999999858, 31.76383008438224564, -238.8689086587541510 ) ) ;
#130089 = LINE ( 'NONE', #71431, #213443 ) ;
#130090 = DIRECTION ( 'NONE',  ( 1.000000000000000000, 0.000000000000000000, 0.000000000000000000 ) ) ;
#130091 = DIRECTION ( 'NONE',  ( 0.000000000000000000, -1.000000000000000000, 0.000000000000000000 ) ) ;
#130092 =( BOUNDED_CURVE ( )  B_SPLINE_CURVE ( 3, ( #196192, #41002, #136180, #1823 ),
 .UNSPECIFIED., .F., .F. ) 
 B_SPLINE_CURVE_WITH_KNOTS ( ( 4, 4 ),
 ( 4.712388980384689674, 6.283185307179586232 ),
 .UNSPECIFIED. ) 
 CURVE ( )  GEOMETRIC_REPRESENTATION_ITEM ( )  RATIONAL_B_SPLINE_CURVE ( ( 1.000000000000000000, 0.8047378541243649375, 0.8047378541243649375, 1.000000000000000000 ) ) 
 REPRESENTATION_ITEM ( '' )  );
#130094 = CARTESIAN_POINT ( 'NONE',  ( -21.53699400384035201, 1.437176978725413726E-11, -160.7122882067533567 ) ) ;
#130093 = CARTESIAN_POINT ( 'NONE',  ( 22.42196299218230493, -3.139091170936018749, -228.2296853193599304 ) ) ;
#130095 = EDGE_CURVE ( 'NONE', #36387, #143318, #124278, .T. ) ;
#130097 = ORIENTED_EDGE ( 'NONE', *, *, #214189, .T. ) ;
#130096 = CARTESIAN_POINT ( 'NONE',  ( -21.05000000000000071, 61.14816101960737882, -234.1879056010411659 ) ) ;
#130098 = CARTESIAN_POINT ( 'NONE',  ( 17.23472005113827876, 10.30788195451192024, -44.95342313993132422 ) ) ;
#130099 = VERTEX_POINT ( 'NONE', #79980 ) ;
#130100 = DIRECTION ( 'NONE',  ( -0.000000000000000000, -0.000000000000000000, 1.000000000000000000 ) ) ;
#130101 = ADVANCED_FACE ( 'NONE', ( #248073 ), #182734, .T. ) ;
#130102 = ORIENTED_EDGE ( 'NONE', *, *, #102336, .F. ) ;
#130103 = ORIENTED_EDGE ( 'NONE', *, *, #64667, .F. ) ;
#130104 = CARTESIAN_POINT ( 'NONE',  ( 20.85000000000000142, 7.783179459866048866, -245.3643104511423303 ) ) ;
#130105 = DIRECTION ( 'NONE',  ( 0.000000000000000000, 6.982962677686266711E-15, -1.000000000000000000 ) ) ;
#130106 = CARTESIAN_POINT ( 'NONE',  ( -16.86422026484316916, 66.02955263915092132, -56.94089425885139377 ) ) ;
#130107 = FACE_OUTER_BOUND ( 'NONE', #199501, .T. ) ;
#130108 = AXIS2_PLACEMENT_3D ( 'NONE', #255447, #54728, #113424 ) ;
#130109 = CARTESIAN_POINT ( 'NONE',  ( 22.59080734064468388, 55.88289069467541026, -232.8092063914162111 ) ) ;
#130110 = ORIENTED_EDGE ( 'NONE', *, *, #245151, .F. ) ;
#130111 = ORIENTED_EDGE ( 'NONE', *, *, #132589, .F. ) ;
#130112 = AXIS2_PLACEMENT_3D ( 'NONE', #100638, #194677, #219329 ) ;
#130113 = DIRECTION ( 'NONE',  ( -1.000000000000000000, 0.000000000000000000, 0.000000000000000000 ) ) ;
#130115 = ADVANCED_FACE ( 'NONE', ( #65581 ), #20225, .T. ) ;
#130114 = ORIENTED_EDGE ( 'NONE', *, *, #223931, .F. ) ;
#130116 = DIRECTION ( 'NONE',  ( -0.000000000000000000, 0.7397890806274345366, 0.6728388485992878865 ) ) ;
#130117 = PLANE ( 'NONE',  #111078 ) ;
#130118 = ORIENTED_EDGE ( 'NONE', *, *, #107735, .T. ) ;
#130119 = CARTESIAN_POINT ( 'NONE',  ( -18.59999999999999787, 1.148907358139439339E-11, -201.0000000000015064 ) ) ;
#130120 = LINE ( 'NONE', #34919, #187913 ) ;
#130121 = CARTESIAN_POINT ( 'NONE',  ( -18.60000000000000142, -9.523954320741637503, -207.8820170568272943 ) ) ;
#130122 = CARTESIAN_POINT ( 'NONE',  ( -23.25000000000000000, -0.1008583690987122083, 11.74956712348939192 ) ) ;
#130123 = EDGE_LOOP ( 'NONE', ( #1054, #26346, #87282, #217203, #244225 ) ) ;
#130124 = FACE_OUTER_BOUND ( 'NONE', #179349, .T. ) ;
#130125 = FACE_OUTER_BOUND ( 'NONE', #200118, .T. ) ;
#130126 = FACE_OUTER_BOUND ( 'NONE', #73692, .T. ) ;
#130128 = EDGE_CURVE ( 'NONE', #156872, #78593, #74418, .T. ) ;
#130127 = DIRECTION ( 'NONE',  ( 1.000000000000000000, -0.000000000000000000, -0.000000000000000000 ) ) ;
#130129 = DIRECTION ( 'NONE',  ( 0.000000000000000000, 6.982962677686267499E-15, -1.000000000000000000 ) ) ;
#130130 = DIRECTION ( 'NONE',  ( -1.000000000000000000, 2.952720810173289112E-16, 2.061873921506763405E-30 ) ) ;
#130132 = ORIENTED_EDGE ( 'NONE', *, *, #242993, .F. ) ;
#130131 = AXIS2_PLACEMENT_3D ( 'NONE', #160350, #178630, #222847 ) ;
#130134 = ADVANCED_FACE ( 'NONE', ( #229791 ), #46327, .T. ) ;
#130133 = CARTESIAN_POINT ( 'NONE',  ( -21.55000000000000426, 68.25000000001185185, -90.67310748452436542 ) ) ;
#130135 = ORIENTED_EDGE ( 'NONE', *, *, #133374, .F. ) ;
#130136 = CARTESIAN_POINT ( 'NONE',  ( -21.05000000000000071, 43.39316802731212874, -245.2602608822587342 ) ) ;
#130137 = CARTESIAN_POINT ( 'NONE',  ( -20.09999999999999787, 5.454087299794355026, 16.60000000000000142 ) ) ;
#130138 = CARTESIAN_POINT ( 'NONE',  ( -23.15000000000000213, 19.73066058418984170, -238.2142830767208466 ) ) ;
#130139 = DIRECTION ( 'NONE',  ( 1.000000000000000000, 0.000000000000000000, 0.000000000000000000 ) ) ;
#130140 = CARTESIAN_POINT ( 'NONE',  ( 20.11144452914042802, 66.06638914889235537, -162.1328140305747070 ) ) ;
#130141 = ORIENTED_EDGE ( 'NONE', *, *, #187515, .T. ) ;
#130142 = CARTESIAN_POINT ( 'NONE',  ( 22.39999999999999503, 11.65000000000000746, -3.469446951953614189E-15 ) ) ;
#130143 = FACE_OUTER_BOUND ( 'NONE', #145035, .T. ) ;
#130144 = DIRECTION ( 'NONE',  ( -3.265361837132813586E-16, 1.000000000000000000, 0.000000000000000000 ) ) ;
#130145 = DIRECTION ( 'NONE',  ( 4.408576920032446739E-17, 0.1350103645451945777, -0.9908441862701590219 ) ) ;
#130146 = AXIS2_PLACEMENT_3D ( 'NONE', #129832, #46443, #249794 ) ;
#130147 = EDGE_CURVE ( 'NONE', #171566, #208058, #103575, .T. ) ;
#130149 = CYLINDRICAL_SURFACE ( 'NONE', #248995, 7.900000000000003908 ) ;
#130148 = AXIS2_PLACEMENT_3D ( 'NONE', #255579, #76989, #1291 ) ;
#130150 = EDGE_LOOP ( 'NONE', ( #133878, #110785, #133892, #236540 ) ) ;
#130151 = ORIENTED_EDGE ( 'NONE', *, *, #182937, .F. ) ;
#130152 = DIRECTION ( 'NONE',  ( -1.000000000000000000, -0.000000000000000000, 0.000000000000000000 ) ) ;
#130154 = CARTESIAN_POINT ( 'NONE',  ( -21.04552871983376505, 6.223900101736508539, 12.00000000000000178 ) ) ;
#130153 = CIRCLE ( 'NONE', #196787, 0.09999999999999993616 ) ;
#130155 = CARTESIAN_POINT ( 'NONE',  ( -18.52139480978222963, -9.481358845055737561, -107.5245565671190917 ) ) ;
#130156 = CARTESIAN_POINT ( 'NONE',  ( -21.53699400380208928, 69.21228820681662341, -170.0231074845244166 ) ) ;
#130157 = ORIENTED_EDGE ( 'NONE', *, *, #6773, .T. ) ;
#130158 = DIRECTION ( 'NONE',  ( 0.000000000000000000, 0.8814952561688738086, -0.4721928772776773364 ) ) ;
#130159 = DIRECTION ( 'NONE',  ( -1.000000000000000000, -0.000000000000000000, -0.000000000000000000 ) ) ;
#130160 = VECTOR ( 'NONE', #163723, 1000.000000000000000 ) ;
#130161 = ORIENTED_EDGE ( 'NONE', *, *, #15626, .T. ) ;
#130162 = AXIS2_PLACEMENT_3D ( 'NONE', #148595, #168193, #12950 ) ;
#130163 = DIRECTION ( 'NONE',  ( 1.000000000000000000, -0.000000000000000000, -0.000000000000000000 ) ) ;
#130164 = ORIENTED_EDGE ( 'NONE', *, *, #246286, .F. ) ;
#130165 = EDGE_LOOP ( 'NONE', ( #60278, #23356, #48260, #36175 ) ) ;
#130166 = AXIS2_PLACEMENT_3D ( 'NONE', #247642, #162994, #9032 ) ;
#130167 = ORIENTED_EDGE ( 'NONE', *, *, #188960, .T. ) ;
#130168 = DIRECTION ( 'NONE',  ( 0.000000000000000000, 0.000000000000000000, 1.000000000000000000 ) ) ;
#130169 = DIRECTION ( 'NONE',  ( -1.000000000000000000, 1.646408749285563322E-14, -1.073024830501002749E-15 ) ) ;
#130171 = CIRCLE ( 'NONE', #38607, 0.4000000000000114575 ) ;
#130170 = DIRECTION ( 'NONE',  ( 0.000000000000000000, 0.8814952561688439436, -0.4721928772777330141 ) ) ;
#130173 = CARTESIAN_POINT ( 'NONE',  ( 20.94999999999999929, -8.730841121484171907, -143.5980747189843783 ) ) ;
#130172 = AXIS2_PLACEMENT_3D ( 'NONE', #177116, #59675, #96251 ) ;
#130174 = EDGE_CURVE ( 'NONE', #5643, #18809, #257650, .T. ) ;
#130175 = CARTESIAN_POINT ( 'NONE',  ( -16.94062896051973865, 9.992719105100677623, -12.60251654211879924 ) ) ;
#130178 = CARTESIAN_POINT ( 'NONE',  ( -23.25000000000000000, 67.23127455305835554, -235.8551265064784559 ) ) ;
#130177 = VECTOR ( 'NONE', #51785, 1000.000000000000114 ) ;
#130176 = DIRECTION ( 'NONE',  ( 1.000000000000000000, 0.000000000000000000, 0.000000000000000000 ) ) ;
#130179 = CARTESIAN_POINT ( 'NONE',  ( 21.04999999999999716, -1.384190162761350429, -194.8207525781398886 ) ) ;
#130180 = DIRECTION ( 'NONE',  ( 0.000000000000000000, -6.982962677686266711E-15, 1.000000000000000000 ) ) ;
#130181 = CARTESIAN_POINT ( 'NONE',  ( 20.94999999999999574, 77.26178616857710324, -128.4366085209788366 ) ) ;
#130182 = CYLINDRICAL_SURFACE ( 'NONE', #153002, 0.09999999999998898659 ) ;
#130183 = ORIENTED_EDGE ( 'NONE', *, *, #111778, .T. ) ;
#130184 = ORIENTED_EDGE ( 'NONE', *, *, #226947, .T. ) ;
#130185 = FACE_OUTER_BOUND ( 'NONE', #62872, .T. ) ;
#130186 = DIRECTION ( 'NONE',  ( 2.952720810173289112E-16, -1.000000000000000000, 0.000000000000000000 ) ) ;
#130187 = DIRECTION ( 'NONE',  ( 0.000000000000000000, 0.6728971962617388280, -0.7397360091702248619 ) ) ;
#130188 = FACE_OUTER_BOUND ( 'NONE', #205479, .T. ) ;
#130190 = EDGE_CURVE ( 'NONE', #122312, #164528, #145282, .T. ) ;
#130189 = CARTESIAN_POINT ( 'NONE',  ( 23.14999999999999503, 38.54769593086029289, -246.0251816765679962 ) ) ;
#130191 = CYLINDRICAL_SURFACE ( 'NONE', #194032, 1.749999999999998002 ) ;
#130192 = EDGE_LOOP ( 'NONE', ( #234917, #150534, #186658, #45442 ) ) ;
#130193 = EDGE_LOOP ( 'NONE', ( #80213, #95784, #223459, #35452, #43203 ) ) ;
#130194 = EDGE_CURVE ( 'NONE', #69695, #76100, #211944, .T. ) ;
#130195 = LINE ( 'NONE', #51932, #101091 ) ;
#130196 = EDGE_LOOP ( 'NONE', ( #72635, #240537, #100774, #232284 ) ) ;
#130197 = DIRECTION ( 'NONE',  ( 0.000000000000000000, 0.1350103645451904977, -0.9908441862701596881 ) ) ;
#130198 = VECTOR ( 'NONE', #233842, 1000.000000000000000 ) ;
#130199 = EDGE_CURVE ( 'NONE', #179596, #64893, #137103, .T. ) ;
#130200 = EDGE_CURVE ( 'NONE', #139671, #101287, #253605, .T. ) ;
#130201 = ORIENTED_EDGE ( 'NONE', *, *, #19366, .T. ) ;
#130202 = CARTESIAN_POINT ( 'NONE',  ( -21.64999999999999858, 68.65000000001150227, -48.27310748452437394 ) ) ;
#130203 = AXIS2_PLACEMENT_3D ( 'NONE', #233946, #16210, #31920 ) ;
#130204 = ORIENTED_EDGE ( 'NONE', *, *, #79933, .F. ) ;
#130205 = EDGE_CURVE ( 'NONE', #10139, #59289, #169873, .T. ) ;
#130206 = DIRECTION ( 'NONE',  ( 1.000000000000000000, -3.151514657663852580E-16, 8.547182517843351137E-17 ) ) ;
#130207 = CARTESIAN_POINT ( 'NONE',  ( -20.64999999999999858, 7.250000000011155521, -88.15000000000004832 ) ) ;
#130209 = CIRCLE ( 'NONE', #205031, 0.1000000000000028644 ) ;
#130208 = SPHERICAL_SURFACE ( 'NONE', #78618, 0.1000000000000000056 ) ;
#130210 = CARTESIAN_POINT ( 'NONE',  ( 18.48536876927993688, -9.463527249856078072, -141.0486182650826379 ) ) ;
#130211 = DIRECTION ( 'NONE',  ( 0.000000000000000000, -0.2128009952264086346, 0.9770955615653210691 ) ) ;
#130212 = DIRECTION ( 'NONE',  ( -0.7071067811865388020, 0.7071067811865561215, 0.000000000000000000 ) ) ;
#130214 = EDGE_CURVE ( 'NONE', #96347, #208477, #166183, .T. ) ;
#130213 = CIRCLE ( 'NONE', #34406, 7.900000000000003908 ) ;
#130215 = DIRECTION ( 'NONE',  ( 0.000000000000000000, 1.000000000000000000, 0.000000000000000000 ) ) ;
#130217 = LINE ( 'NONE', #139188, #183069 ) ;
#130216 = CIRCLE ( 'NONE', #200972, 0.09999999999999939493 ) ;
#130218 = AXIS2_PLACEMENT_3D ( 'NONE', #15582, #255390, #37710 ) ;
#130220 = ORIENTED_EDGE ( 'NONE', *, *, #202512, .F. ) ;
#130219 = CARTESIAN_POINT ( 'NONE',  ( 21.00000000000000000, 66.25000000001260503, -191.1731074845244223 ) ) ;
#130222 = DIRECTION ( 'NONE',  ( 1.000000000000000000, 0.000000000000000000, 0.000000000000000000 ) ) ;
#130221 = LINE ( 'NONE', #71574, #116107 ) ;
#130223 = ORIENTED_EDGE ( 'NONE', *, *, #213973, .F. ) ;
#130225 = ORIENTED_EDGE ( 'NONE', *, *, #213877, .T. ) ;
#130224 = DIRECTION ( 'NONE',  ( 1.000000000000000000, 0.000000000000000000, 0.000000000000000000 ) ) ;
#130226 = ORIENTED_EDGE ( 'NONE', *, *, #200044, .T. ) ;
#130227 = DIRECTION ( 'NONE',  ( 1.000000000000000000, 0.000000000000000000, 0.000000000000000000 ) ) ;
#130228 = VECTOR ( 'NONE', #196546, 1000.000000000000000 ) ;
#130229 = DIRECTION ( 'NONE',  ( 0.000000000000000000, 0.000000000000000000, -1.000000000000000000 ) ) ;
#130230 = AXIS2_PLACEMENT_3D ( 'NONE', #169434, #226789, #149850 ) ;
#130231 = DIRECTION ( 'NONE',  ( 0.000000000000000000, -0.8660254037844383745, 0.5000000000000003331 ) ) ;
#130232 = DIRECTION ( 'NONE',  ( 1.000000000000000000, 2.952720810173289112E-16, -0.000000000000000000 ) ) ;
#130233 = FACE_OUTER_BOUND ( 'NONE', #23273, .T. ) ;
#130234 = CARTESIAN_POINT ( 'NONE',  ( 20.95512820512820440, 60.15812638745688901, -221.3479132702343009 ) ) ;
#130235 = TOROIDAL_SURFACE ( 'NONE', #88716, 0.2000000000000000111, 0.1000000000000000056 ) ;
#130236 = LINE ( 'NONE', #209796, #171170 ) ;
#130238 = ADVANCED_FACE ( 'NONE', ( #147695 ), #48582, .F. ) ;
#130237 = DIRECTION ( 'NONE',  ( -2.889348024582214003E-15, -0.9910827722268042983, -0.1332476588733650935 ) ) ;
#130239 = VECTOR ( 'NONE', #99015, 1000.000000000000000 ) ;
#130240 = CARTESIAN_POINT ( 'NONE',  ( 20.94999999999999929, 77.16270174994990327, -95.12310748452431142 ) ) ;
#130241 = VECTOR ( 'NONE', #11020, 1000.000000000000000 ) ;
#130242 = ORIENTED_EDGE ( 'NONE', *, *, #82966, .T. ) ;
#130243 = ORIENTED_EDGE ( 'NONE', *, *, #79876, .F. ) ;
#130244 = LINE ( 'NONE', #148547, #85399 ) ;
#130245 = VERTEX_POINT ( 'NONE', #88980 ) ;
#130246 = CARTESIAN_POINT ( 'NONE',  ( -23.15000000000000213, -9.499999999988846255, -90.60603087734760663 ) ) ;
#130247 = ORIENTED_EDGE ( 'NONE', *, *, #103341, .F. ) ;
#130249 = AXIS2_PLACEMENT_3D ( 'NONE', #155366, #154096, #94060 ) ;
#130248 = LINE ( 'NONE', #110701, #250956 ) ;
#130250 = AXIS2_PLACEMENT_3D ( 'NONE', #199593, #220422, #41799 ) ;
#130251 = EDGE_CURVE ( 'NONE', #11074, #222021, #141199, .T. ) ;
#130252 = AXIS2_PLACEMENT_3D ( 'NONE', #226433, #8699, #170393 ) ;
#130253 = CARTESIAN_POINT ( 'NONE',  ( -20.54999999999999716, 1.115600667400684642E-11, -100.5000000000000284 ) ) ;
#130254 = DIRECTION ( 'NONE',  ( 1.000000000000000000, 0.000000000000000000, 0.000000000000000000 ) ) ;
#130255 = CARTESIAN_POINT ( 'NONE',  ( 20.94999999999999574, 76.00000000001195133, -103.0231074845243171 ) ) ;
#130256 = CARTESIAN_POINT ( 'NONE',  ( 21.00000000000000000, 14.04870287383362992, -219.6884709798077893 ) ) ;
#130257 = EDGE_LOOP ( 'NONE', ( #117294, #50409, #203170, #211347 ) ) ;
#130258 = DIRECTION ( 'NONE',  ( 0.000000000000000000, 0.9525900758537746427, -0.3042567129660413983 ) ) ;
#130259 = DIRECTION ( 'NONE',  ( 0.000000000000000000, 0.000000000000000000, -1.000000000000000000 ) ) ;
#130260 = LINE ( 'NONE', #88557, #67165 ) ;
#130261 = CARTESIAN_POINT ( 'NONE',  ( -21.05000000000000071, 6.270085863700304962, -133.9651319969869405 ) ) ;
#130262 = ADVANCED_FACE ( 'NONE', ( #30328 ), #146119, .T. ) ;
#130263 = ORIENTED_EDGE ( 'NONE', *, *, #23451, .T. ) ;
#130265 = DIRECTION ( 'NONE',  ( -0.000000000000000000, 0.4088369013363281068, -0.9126074666063770380 ) ) ;
#130264 = DIRECTION ( 'NONE',  ( 1.000000000000000000, 0.000000000000000000, 0.000000000000000000 ) ) ;
#130266 = EDGE_LOOP ( 'NONE', ( #168321, #134015, #113287, #52024 ) ) ;
#130269 = ORIENTED_EDGE ( 'NONE', *, *, #47699, .T. ) ;
#130268 = DIRECTION ( 'NONE',  ( -1.836970198721029934E-16, 1.000000000000000000, 0.000000000000000000 ) ) ;
#130267 = DIRECTION ( 'NONE',  ( 0.000000000000000000, 0.000000000000000000, -1.000000000000000000 ) ) ;
#130270 = CIRCLE ( 'NONE', #176099, 0.09999999999999868716 ) ;
#130271 = EDGE_CURVE ( 'NONE', #120146, #51370, #153727, .T. ) ;
#130272 = CARTESIAN_POINT ( 'NONE',  ( 22.59999999999999432, 75.95218160930723172, -114.7731299035715296 ) ) ;
#130273 = AXIS2_PLACEMENT_3D ( 'NONE', #242251, #64898, #3638 ) ;
#130274 = CARTESIAN_POINT ( 'NONE',  ( -21.05000000000000071, 1.851028230152016674, -179.1539132694224463 ) ) ;
#130275 = FACE_OUTER_BOUND ( 'NONE', #156648, .T. ) ;
#130276 = ORIENTED_EDGE ( 'NONE', *, *, #58546, .F. ) ;
#130277 = CARTESIAN_POINT ( 'NONE',  ( -20.64999999999999858, 44.87429835298446790, -237.9265065269792103 ) ) ;
#130279 = ADVANCED_FACE ( 'NONE', ( #173731 ), #52426, .T. ) ;
#130278 = DIRECTION ( 'NONE',  ( 0.000000000000000000, 1.000000000000000000, 0.000000000000000000 ) ) ;
#130282 = CARTESIAN_POINT ( 'NONE',  ( 22.50000000000000000, 12.54152817314149715, -223.4164406214577241 ) ) ;
#130281 = DIRECTION ( 'NONE',  ( -0.000000000000000000, 0.9165223833629858596, -0.3999834006488672267 ) ) ;
#130280 = B_SPLINE_CURVE_WITH_KNOTS ( 'NONE', 3,
 ( #158351, #237848, #81306, #183029, #43511, #223405, #65624, #83865, #107319, #22682 ),
 .UNSPECIFIED., .F., .F.,
 ( 4, 3, 3, 4 ),
 ( 0.000000000000000000, 3.394313611811697806E-05, 6.779740500700335930E-05, 0.0001049857339142755560 ),
 .UNSPECIFIED. ) ;
#130284 = ORIENTED_EDGE ( 'NONE', *, *, #240143, .T. ) ;
#130283 = CARTESIAN_POINT ( 'NONE',  ( 22.39999999999999503, 75.90000000001199965, -110.8138870828976934 ) ) ;
#130285 = EDGE_CURVE ( 'NONE', #152520, #217417, #41272, .T. ) ;
#130286 = EDGE_CURVE ( 'NONE', #216709, #241817, #116269, .T. ) ;
#130287 = ORIENTED_EDGE ( 'NONE', *, *, #93439, .F. ) ;
#130288 = CARTESIAN_POINT ( 'NONE',  ( -21.05000000000000071, -1.835341550213255957, -78.55515129256302487 ) ) ;
#130289 = VECTOR ( 'NONE', #69814, 1000.000000000000000 ) ;
#130290 = DIRECTION ( 'NONE',  ( 0.000000000000000000, -6.982962677686266711E-15, 1.000000000000000000 ) ) ;
#130291 = DIRECTION ( 'NONE',  ( 1.000000000000000000, -2.952720810173289112E-16, -2.061873921506763405E-30 ) ) ;
#130292 = ORIENTED_EDGE ( 'NONE', *, *, #39287, .T. ) ;
#130293 = DIRECTION ( 'NONE',  ( -0.000000000000000000, 1.000000000000000000, -0.000000000000000000 ) ) ;
#130294 = ADVANCED_FACE ( 'NONE', ( #155440 ), #154158, .T. ) ;
#130295 = AXIS2_PLACEMENT_3D ( 'NONE', #63169, #185707, #27946 ) ;
#130296 = CARTESIAN_POINT ( 'NONE',  ( 21.05000000000000071, -11.48912529306489994, -164.4000000000000057 ) ) ;
#130297 = CARTESIAN_POINT ( 'NONE',  ( 18.60000000000001563, -9.364236010355611484, -141.1802544007246354 ) ) ;
#130298 = ORIENTED_EDGE ( 'NONE', *, *, #133235, .F. ) ;
#130299 = CARTESIAN_POINT ( 'NONE',  ( 20.50589344625456789, 59.09583819986320918, -225.8021589099539597 ) ) ;
#130300 = ORIENTED_EDGE ( 'NONE', *, *, #171033, .T. ) ;
#130301 = CARTESIAN_POINT ( 'NONE',  ( 18.59999999999999432, 74.27191306321776665, -149.6386724793565577 ) ) ;
#130302 = DIRECTION ( 'NONE',  ( -0.000000000000000000, -6.982962677686266711E-15, 1.000000000000000000 ) ) ;
#130305 = ORIENTED_EDGE ( 'NONE', *, *, #89034, .F. ) ;
#130304 = TOROIDAL_SURFACE ( 'NONE', #67775, 12.97499999999999787, 0.1000000000000000056 ) ;
#130303 = B_SPLINE_CURVE_WITH_KNOTS ( 'NONE', 3,
 ( #111926, #255208, #74100, #175754, #192739, #75376, #154915, #135302, #117047, #216127 ),
 .UNSPECIFIED., .F., .F.,
 ( 4, 3, 3, 4 ),
 ( 0.000000000000000000, 0.0002000000000008733344, 0.001000000000082982470, 0.001967863649483324578 ),
 .UNSPECIFIED. ) ;
#130306 = EDGE_LOOP ( 'NONE', ( #215060, #164230, #245871, #15677 ) ) ;
#130307 = DIRECTION ( 'NONE',  ( 1.000000000000000000, 0.000000000000000000, 0.000000000000000000 ) ) ;
#130308 = VERTEX_POINT ( 'NONE', #57560 ) ;
#130310 = EDGE_LOOP ( 'NONE', ( #216823, #226598, #17036, #74029 ) ) ;
#130309 = CARTESIAN_POINT ( 'NONE',  ( -22.01447462590972748, 7.263800201229918763, 0.09903700005953296193 ) ) ;
#130311 = EDGE_CURVE ( 'NONE', #246680, #188088, #162060, .T. ) ;
#130312 = EDGE_CURVE ( 'NONE', #160823, #65006, #78634, .T. ) ;
#130313 = ORIENTED_EDGE ( 'NONE', *, *, #235281, .T. ) ;
#130316 = VERTEX_POINT ( 'NONE', #131977 ) ;
#130315 = VERTEX_POINT ( 'NONE', #172436 ) ;
#130314 = CYLINDRICAL_SURFACE ( 'NONE', #72031, 0.09999999999999939493 ) ;
#130318 = ADVANCED_FACE ( 'NONE', ( #116287 ), #195835, .F. ) ;
#130317 = CYLINDRICAL_SURFACE ( 'NONE', #243778, 0.9000000000000014655 ) ;
#130319 = TOROIDAL_SURFACE ( 'NONE', #155313, 0.9750000000000019762, 0.1000000000000000056 ) ;
#130320 = VERTEX_POINT ( 'NONE', #77137 ) ;
#130321 = DIRECTION ( 'NONE',  ( -1.000000000000000000, 0.000000000000000000, 0.000000000000000000 ) ) ;
#130322 = DIRECTION ( 'NONE',  ( 0.000000000000000000, 0.000000000000000000, -1.000000000000000000 ) ) ;
#130323 = LINE ( 'NONE', #69098, #168083 ) ;
#130324 = VECTOR ( 'NONE', #109378, 1000.000000000000114 ) ;
#130325 = CARTESIAN_POINT ( 'NONE',  ( 23.14999999999999858, 6.650000000011155876, -112.8500000000000369 ) ) ;
#130326 = ORIENTED_EDGE ( 'NONE', *, *, #116935, .T. ) ;
#130327 = ORIENTED_EDGE ( 'NONE', *, *, #178468, .T. ) ;
#130328 = ORIENTED_EDGE ( 'NONE', *, *, #229537, .T. ) ;
#130329 = TOROIDAL_SURFACE ( 'NONE', #17904, 2.100000000000002309, 0.1000000000000000056 ) ;
#130330 = DIRECTION ( 'NONE',  ( 1.000000000000000000, 0.000000000000000000, 0.000000000000000000 ) ) ;
#130332 = EDGE_LOOP ( 'NONE', ( #49265, #212830, #27350, #219305 ) ) ;
#130331 = CARTESIAN_POINT ( 'NONE',  ( -23.15000000000000213, 11.65000000001115588, -193.9851942293460070 ) ) ;
#130333 = CARTESIAN_POINT ( 'NONE',  ( -20.94999999999999929, 77.26178616857662007, -61.43660852097883662 ) ) ;
#130335 = EDGE_LOOP ( 'NONE', ( #81971, #136047, #36617, #99070 ) ) ;
#130334 = CARTESIAN_POINT ( 'NONE',  ( 18.46858270002952906, 78.23413370411033441, -231.4806182615872103 ) ) ;
#130336 = ORIENTED_EDGE ( 'NONE', *, *, #228380, .F. ) ;
#130337 = CARTESIAN_POINT ( 'NONE',  ( -18.46907102845854709, -0.7072367829275776341, -242.2718438362406062 ) ) ;
#130338 = CIRCLE ( 'NONE', #17913, 0.2000000000000122791 ) ;
#130339 = VECTOR ( 'NONE', #137666, 1000.000000000000000 ) ;
#130340 = VERTEX_POINT ( 'NONE', #251924 ) ;
#130341 = AXIS2_PLACEMENT_3D ( 'NONE', #59278, #80130, #234098 ) ;
#130342 = CARTESIAN_POINT ( 'NONE',  ( 23.24999999999999289, 11.65000000001116298, -67.00000000000004263 ) ) ;
#130343 = EDGE_CURVE ( 'NONE', #23701, #244468, #220320, .T. ) ;
#130345 = ORIENTED_EDGE ( 'NONE', *, *, #228889, .F. ) ;
#130344 = ORIENTED_EDGE ( 'NONE', *, *, #246489, .T. ) ;
#130346 = ORIENTED_EDGE ( 'NONE', *, *, #194738, .F. ) ;
#130347 = DIRECTION ( 'NONE',  ( 0.000000000000000000, 0.000000000000000000, 1.000000000000000000 ) ) ;
#130348 = EDGE_LOOP ( 'NONE', ( #126147, #254253, #179099, #38133 ) ) ;
#130349 = ORIENTED_EDGE ( 'NONE', *, *, #13391, .T. ) ;
#130351 = CARTESIAN_POINT ( 'NONE',  ( -21.65000000000000213, 68.29142135624881860, -48.27310748452437394 ) ) ;
#130350 = CIRCLE ( 'NONE', #221921, 0.1000000000000019207 ) ;
#130354 = EDGE_CURVE ( 'NONE', #225394, #123416, #12043, .T. ) ;
#130353 = ORIENTED_EDGE ( 'NONE', *, *, #18431, .F. ) ;
#130352 = CARTESIAN_POINT ( 'NONE',  ( 23.24999999999999289, 6.649999999999999467, -21.35000000000000142 ) ) ;
#130355 = CARTESIAN_POINT ( 'NONE',  ( 18.59999999999999432, 77.83585931145600512, -158.5186683157258187 ) ) ;
#130357 = CARTESIAN_POINT ( 'NONE',  ( 21.05000000000000071, 31.89597452117650533, -238.9192857152811484 ) ) ;
#130356 = DIRECTION ( 'NONE',  ( 1.000000000000000000, 0.000000000000000000, 0.000000000000000000 ) ) ;
#130358 = CARTESIAN_POINT ( 'NONE',  ( -20.64999999999999858, 45.00644278977874535, -237.9768835835062077 ) ) ;
#130359 = DIRECTION ( 'NONE',  ( 1.000000000000000000, 0.000000000000000000, 0.000000000000000000 ) ) ;
#130360 = ORIENTED_EDGE ( 'NONE', *, *, #168915, .F. ) ;
#130361 = AXIS2_PLACEMENT_3D ( 'NONE', #167393, #85220, #126956 ) ;
#130362 = ADVANCED_FACE ( 'NONE', ( #111134 ), #191983, .F. ) ;
#130363 = TOROIDAL_SURFACE ( 'NONE', #234409, 0.2000000000000000111, 0.1000000000000000056 ) ;
#130364 = VECTOR ( 'NONE', #207200, 1000.000000000000000 ) ;
#130365 = VERTEX_POINT ( 'NONE', #212814 ) ;
#130366 = CIRCLE ( 'NONE', #130556, 0.09999999999999939493 ) ;
#130367 = FACE_OUTER_BOUND ( 'NONE', #193063, .T. ) ;
#130368 = CARTESIAN_POINT ( 'NONE',  ( 21.05000000000000071, 1.148907358139439339E-11, -201.0000000000015064 ) ) ;
#130369 = EDGE_CURVE ( 'NONE', #90944, #220406, #99256, .T. ) ;
#130370 = EDGE_LOOP ( 'NONE', ( #183598, #146359, #257356, #249498 ) ) ;
#130371 = EDGE_CURVE ( 'NONE', #253401, #131663, #45332, .T. ) ;
#130372 = CARTESIAN_POINT ( 'NONE',  ( -22.94999999999999929, 11.50977166988710820, 1.786320531569725478 ) ) ;
#130373 = CARTESIAN_POINT ( 'NONE',  ( 21.05000000000000071, -9.399999999988844834, -57.10603087734755690 ) ) ;
#130375 = ADVANCED_FACE ( 'NONE', ( #161844 ), #64612, .T. ) ;
#130374 = EDGE_CURVE ( 'NONE', #152529, #105943, #191110, .T. ) ;
#130376 = EDGE_LOOP ( 'NONE', ( #158789, #141477, #199120, #126413 ) ) ;
#130377 = EDGE_LOOP ( 'NONE', ( #135747, #79465, #135020, #45251 ) ) ;
#130378 = CARTESIAN_POINT ( 'NONE',  ( -21.03571358705832850, 64.25000000001264766, -196.6980006624660859 ) ) ;
#130379 = CARTESIAN_POINT ( 'NONE',  ( 18.59999999999999076, 6.450000000011156587, -54.65000000000000568 ) ) ;
#130380 = VERTEX_POINT ( 'NONE', #198372 ) ;
#130381 = CARTESIAN_POINT ( 'NONE',  ( -18.45068461519105441, -9.486506529077933791, -174.5687771689046883 ) ) ;
#130382 = ORIENTED_EDGE ( 'NONE', *, *, #39594, .F. ) ;
#130383 = CARTESIAN_POINT ( 'NONE',  ( 18.59999996954842771, -9.523204137847017137, -140.8830417119173433 ) ) ;
#130384 = CARTESIAN_POINT ( 'NONE',  ( 18.49999999999998934, 28.95347087985017609, -237.9930060266852081 ) ) ;
#130386 = CARTESIAN_POINT ( 'NONE',  ( -18.59999999999999787, 74.16465844978787914, -158.4679561919613775 ) ) ;
#130385 = DIRECTION ( 'NONE',  ( -1.000000000000000000, 0.000000000000000000, 0.000000000000000000 ) ) ;
#130387 = DIRECTION ( 'NONE',  ( 0.000000000000000000, 0.8814952561688476074, -0.4721928772777262417 ) ) ;
#130388 = LINE ( 'NONE', #33920, #191053 ) ;
#130389 = CARTESIAN_POINT ( 'NONE',  ( -20.54999999999999716, 7.250000000011155521, -79.25000000000004263 ) ) ;
#130390 = DIRECTION ( 'NONE',  ( -1.000000000000000000, -0.000000000000000000, 0.000000000000000000 ) ) ;
#130391 = CIRCLE ( 'NONE', #242991, 11.74999999999999822 ) ;
#130392 = AXIS2_PLACEMENT_3D ( 'NONE', #6920, #164722, #89020 ) ;
#130393 = EDGE_LOOP ( 'NONE', ( #37962, #160283, #106448, #42589 ) ) ;
#130394 = EDGE_CURVE ( 'NONE', #49064, #241890, #228707, .T. ) ;
#130395 = ADVANCED_FACE ( 'NONE', ( #240078 ), #24705, .T. ) ;
#130397 = VERTEX_POINT ( 'NONE', #118856 ) ;
#130396 = ORIENTED_EDGE ( 'NONE', *, *, #127158, .F. ) ;
#130398 = ORIENTED_EDGE ( 'NONE', *, *, #223156, .T. ) ;
#130399 = CIRCLE ( 'NONE', #255436, 0.09999999999998898659 ) ;
#130400 = EDGE_CURVE ( 'NONE', #61299, #184336, #107391, .T. ) ;
#130401 = CARTESIAN_POINT ( 'NONE',  ( 21.56666275994539461, 1.115600667400684642E-11, -93.54263159310670517 ) ) ;
#130402 = CIRCLE ( 'NONE', #188661, 0.09999999999999344136 ) ;
#130403 = DIRECTION ( 'NONE',  ( 0.000000000000000000, 0.000000000000000000, 1.000000000000000000 ) ) ;
#130405 = FACE_OUTER_BOUND ( 'NONE', #86017, .T. ) ;
#130404 = DIRECTION ( 'NONE',  ( 0.7071067811865487940, 0.000000000000000000, -0.7071067811865463515 ) ) ;
#130406 = DIRECTION ( 'NONE',  ( 0.000000000000000000, -0.2617529984165031243, -0.9651348961777157509 ) ) ;
#130407 = ORIENTED_EDGE ( 'NONE', *, *, #150075, .F. ) ;
#130408 = AXIS2_PLACEMENT_3D ( 'NONE', #104170, #220302, #20825 ) ;
#130409 = ADVANCED_FACE ( 'NONE', ( #140986 ), #200942, .T. ) ;
#130410 = ORIENTED_EDGE ( 'NONE', *, *, #47586, .F. ) ;
#130411 = CARTESIAN_POINT ( 'NONE',  ( 20.04142135623730070, 11.65000000001115943, -188.8499999999999659 ) ) ;
#130412 = AXIS2_PLACEMENT_3D ( 'NONE', #37314, #93408, #232955 ) ;
#130413 = CARTESIAN_POINT ( 'NONE',  ( 20.94999999999999574, 77.83534155023598089, -57.96795619196132776 ) ) ;
#130414 = CIRCLE ( 'NONE', #22109, 0.1999999999999987899 ) ;
#130415 = AXIS2_PLACEMENT_3D ( 'NONE', #182343, #44102, #119810 ) ;
#130416 = EDGE_CURVE ( 'NONE', #91084, #57292, #3828, .T. ) ;
#130417 = CARTESIAN_POINT ( 'NONE',  ( 16.87683809663750267, 66.05000000001261640, -190.8731074845244393 ) ) ;
#130418 = VERTEX_POINT ( 'NONE', #41896 ) ;
#130419 = CARTESIAN_POINT ( 'NONE',  ( 21.05000000000000071, 84.73084112150783653, -179.6211822035086527 ) ) ;
#130420 = VECTOR ( 'NONE', #67103, 1000.000000000000000 ) ;
#130421 = DIRECTION ( 'NONE',  ( -1.000000000000000000, 0.000000000000000000, 0.000000000000000000 ) ) ;
#130422 = ORIENTED_EDGE ( 'NONE', *, *, #175243, .T. ) ;
#130423 = ORIENTED_EDGE ( 'NONE', *, *, #74848, .F. ) ;
#130424 = FACE_OUTER_BOUND ( 'NONE', #104905, .T. ) ;
#130425 = DIRECTION ( 'NONE',  ( -0.000000000000000000, -0.000000000000000000, 1.000000000000000000 ) ) ;
#130426 = CARTESIAN_POINT ( 'NONE',  ( -20.64999999999999858, -8.663551401858001100, -157.9758988819327215 ) ) ;
#130427 = ADVANCED_FACE ( 'NONE', ( #18454 ), #158011, .T. ) ;
#130428 = CARTESIAN_POINT ( 'NONE',  ( -23.15000000000000213, 28.51339163295720169, -258.4040038037771865 ) ) ;
#130429 = DIRECTION ( 'NONE',  ( 1.713247197920696616E-14, -0.9876197685951263461, 0.1568667991644794590 ) ) ;
#130431 = CIRCLE ( 'NONE', #17991, 11.80000000000000426 ) ;
#130430 = DIRECTION ( 'NONE',  ( -0.000000000000000000, 0.2128009952263604232, -0.9770955615653316162 ) ) ;
#130432 = ORIENTED_EDGE ( 'NONE', *, *, #81712, .T. ) ;
#130433 = CARTESIAN_POINT ( 'NONE',  ( -23.15000000000000213, 71.65000000001207070, -124.1731074845243228 ) ) ;
#130434 = FACE_OUTER_BOUND ( 'NONE', #205706, .T. ) ;
#130435 = VECTOR ( 'NONE', #17677, 1000.000000000000000 ) ;
#130437 = DIRECTION ( 'NONE',  ( 1.000000000000000000, 2.952720810173289112E-16, -0.000000000000000000 ) ) ;
#130436 = CARTESIAN_POINT ( 'NONE',  ( 20.94999999999999574, 77.36087058720393372, -94.95010955743333625 ) ) ;
#130438 = DIRECTION ( 'NONE',  ( -0.000000000000000000, -1.000000000000000000, 0.000000000000000000 ) ) ;
#130440 = EDGE_CURVE ( 'NONE', #227344, #237934, #121441, .T. ) ;
#130439 = CARTESIAN_POINT ( 'NONE',  ( -18.46856557590792747, -9.474215907786497581, -7.101986240882300017 ) ) ;
#130441 = AXIS2_PLACEMENT_3D ( 'NONE', #203464, #126484, #143476 ) ;
#130442 = CARTESIAN_POINT ( 'NONE',  ( 18.50000000000000000, 47.16152503674118890, -255.1462838189583806 ) ) ;
#130443 = CARTESIAN_POINT ( 'NONE',  ( 20.93302460841142931, 10.31565961587945424, -139.5364194119178478 ) ) ;
#130445 = VERTEX_POINT ( 'NONE', #122715 ) ;
#130444 = CARTESIAN_POINT ( 'NONE',  ( 21.46681500598917580, 30.40070853532387929, -252.3547663145410240 ) ) ;
#130446 = CIRCLE ( 'NONE', #18005, 11.80000000000001137 ) ;
#130447 = AXIS2_PLACEMENT_3D ( 'NONE', #8016, #148807, #192742 ) ;
#130448 = AXIS2_PLACEMENT_3D ( 'NONE', #248972, #144706, #85998 ) ;
#130449 = TOROIDAL_SURFACE ( 'NONE', #97078, 0.2000000000000000111, 0.1000000000000000056 ) ;
#130451 = ADVANCED_FACE ( 'NONE', ( #202232 ), #242627, .F. ) ;
#130450 = DIRECTION ( 'NONE',  ( 1.000000000000000000, 0.000000000000000000, -0.000000000000000000 ) ) ;
#130452 = DIRECTION ( 'NONE',  ( 0.000000000000000000, 0.000000000000000000, 1.000000000000000000 ) ) ;
#130453 = DIRECTION ( 'NONE',  ( -1.000000000000000000, 0.000000000000000000, 0.000000000000000000 ) ) ;
#130454 = CARTESIAN_POINT ( 'NONE',  ( 19.75857864376268935, 11.65000000001115943, -91.85000000000003695 ) ) ;
#130455 = AXIS2_PLACEMENT_3D ( 'NONE', #209836, #76719, #214957 ) ;
#130456 = ORIENTED_EDGE ( 'NONE', *, *, #96928, .T. ) ;
#130457 = AXIS2_PLACEMENT_3D ( 'NONE', #51332, #111347, #205286 ) ;
#130458 = AXIS2_PLACEMENT_3D ( 'NONE', #253749, #75160, #56811 ) ;
#130460 = CARTESIAN_POINT ( 'NONE',  ( -20.64999999999999858, -8.999999999988844479, -157.6060308773475924 ) ) ;
#130459 = CIRCLE ( 'NONE', #34814, 0.5000000000000004441 ) ;
#130461 = CARTESIAN_POINT ( 'NONE',  ( 12.25000000000000000, 13.18880795147152618, -215.2702608532411830 ) ) ;
#130462 = DIRECTION ( 'NONE',  ( 0.000000000000000000, -1.000000000000000000, 0.000000000000000000 ) ) ;
#130463 = ORIENTED_EDGE ( 'NONE', *, *, #143398, .T. ) ;
#130464 = CARTESIAN_POINT ( 'NONE',  ( -16.89268316805466341, 12.41449167011727361, -211.2369018264743090 ) ) ;
#130466 = VERTEX_POINT ( 'NONE', #83528 ) ;
#130465 = DIRECTION ( 'NONE',  ( 1.000000000000000000, -2.952720810173289112E-16, -2.061873921506763405E-30 ) ) ;
#130467 = CARTESIAN_POINT ( 'NONE',  ( -23.15000000000000213, 8.653397185701672711, -220.7611668973962367 ) ) ;
#130468 = DIRECTION ( 'NONE',  ( 0.000000000000000000, -0.2128009952263603954, 0.9770955615653315052 ) ) ;
#130469 = ORIENTED_EDGE ( 'NONE', *, *, #84945, .F. ) ;
#130470 = CARTESIAN_POINT ( 'NONE',  ( -16.87401514999222840, 66.05000000001261640, -190.8031254770564829 ) ) ;
#130471 = DIRECTION ( 'NONE',  ( 1.000000000000000000, 0.000000000000000000, 0.000000000000000000 ) ) ;
#130472 = CARTESIAN_POINT ( 'NONE',  ( -20.94999999999999929, 4.158309866074138661, -211.9342015984041439 ) ) ;
#130473 = CARTESIAN_POINT ( 'NONE',  ( -18.79999999999999716, 7.973296578895943121, 1.410778198689825347 ) ) ;
#130474 = CYLINDRICAL_SURFACE ( 'NONE', #67368, 0.1000000000000028644 ) ;
#130475 = VERTEX_POINT ( 'NONE', #104382 ) ;
#130476 = CARTESIAN_POINT ( 'NONE',  ( 20.94999999999999574, 18.18127959618848521, -237.5711165786817389 ) ) ;
#130477 = DIRECTION ( 'NONE',  ( -0.7071067811865475727, -0.7071067811865475727, 0.000000000000000000 ) ) ;
#130478 = CIRCLE ( 'NONE', #196937, 0.09999999999999939493 ) ;
#130479 = LINE ( 'NONE', #172232, #145201 ) ;
#130480 = ORIENTED_EDGE ( 'NONE', *, *, #106340, .T. ) ;
#130481 = ORIENTED_EDGE ( 'NONE', *, *, #209262, .T. ) ;
#130482 = DIRECTION ( 'NONE',  ( 1.000000000000000000, 0.000000000000000000, 0.000000000000000000 ) ) ;
#130483 = DIRECTION ( 'NONE',  ( 1.000000000000000000, 0.000000000000000000, 0.000000000000000000 ) ) ;
#130484 = CARTESIAN_POINT ( 'NONE',  ( -23.25000000000000000, 87.75000000001192291, -106.1231074845242262 ) ) ;
#130485 = DIRECTION ( 'NONE',  ( 0.000000000000000000, 0.000000000000000000, -1.000000000000000000 ) ) ;
#130486 = EDGE_CURVE ( 'NONE', #147965, #139128, #249551, .T. ) ;
#130488 = CARTESIAN_POINT ( 'NONE',  ( 21.13736287352038445, 67.95335762362789467, -93.77310748452437394 ) ) ;
#130487 = LINE ( 'NONE', #212616, #20107 ) ;
#130489 = DIRECTION ( 'NONE',  ( 0.000000000000000000, -0.2128009952263601456, 0.9770955615653316162 ) ) ;
#130490 = CARTESIAN_POINT ( 'NONE',  ( -16.94107738177414291, 65.98576071487538286, -115.5731074845243711 ) ) ;
#130492 = DIRECTION ( 'NONE',  ( -0.000000000000000000, -0.9770955615653315052, -0.2128009952263603954 ) ) ;
#130491 = VECTOR ( 'NONE', #33780, 1000.000000000000114 ) ;
#130493 = ORIENTED_EDGE ( 'NONE', *, *, #12817, .T. ) ;
#130494 = AXIS2_PLACEMENT_3D ( 'NONE', #194377, #36599, #34035 ) ;
#130496 = VERTEX_POINT ( 'NONE', #243911 ) ;
#130495 = DIRECTION ( 'NONE',  ( 0.000000000000000000, 0.9908441862701596881, -0.1350103645451904977 ) ) ;
#130497 = CARTESIAN_POINT ( 'NONE',  ( 21.12757541349815682, 69.52661942876092382, -170.0282687003341664 ) ) ;
#130498 = CARTESIAN_POINT ( 'NONE',  ( -21.10320863425827298, -1.337536266937425555, -194.7409926129413122 ) ) ;
#130501 = DIRECTION ( 'NONE',  ( 0.000000000000000000, 0.000000000000000000, -1.000000000000000000 ) ) ;
#130500 = DIRECTION ( 'NONE',  ( 1.000000000000000000, -0.000000000000000000, 0.000000000000000000 ) ) ;
#130499 = VECTOR ( 'NONE', #244870, 1000.000000000000000 ) ;
#130502 = EDGE_LOOP ( 'NONE', ( #129592, #161994, #216404, #101403 ) ) ;
#130503 = CARTESIAN_POINT ( 'NONE',  ( -23.15000000000000213, 4.350000000011156054, -155.1500000000000057 ) ) ;
#130505 = EDGE_CURVE ( 'NONE', #54263, #198296, #186528, .T. ) ;
#130504 = CARTESIAN_POINT ( 'NONE',  ( 19.81427058490527315, 64.33143601963020330, -111.7731074845243739 ) ) ;
#130506 = LINE ( 'NONE', #71849, #145139 ) ;
#130507 = DIRECTION ( 'NONE',  ( -1.000000000000000000, -0.000000000000000000, -0.000000000000000000 ) ) ;
#130508 = ORIENTED_EDGE ( 'NONE', *, *, #145662, .F. ) ;
#130509 = ORIENTED_EDGE ( 'NONE', *, *, #3243, .F. ) ;
#130510 = ADVANCED_FACE ( 'NONE', ( #108275 ), #7901, .F. ) ;
#130512 = AXIS2_PLACEMENT_3D ( 'NONE', #180238, #220641, #1570 ) ;
#130511 = DIRECTION ( 'NONE',  ( 0.000000000000000000, -1.000000000000000000, -6.982962677686266711E-15 ) ) ;
#130513 = ORIENTED_EDGE ( 'NONE', *, *, #210064, .T. ) ;
#130514 = CYLINDRICAL_SURFACE ( 'NONE', #13794, 0.1000000000000028644 ) ;
#130515 = CIRCLE ( 'NONE', #88807, 0.1000000000000052097 ) ;
#130516 = CARTESIAN_POINT ( 'NONE',  ( 21.05000000000000426, 10.56275983746217051, -141.4568139579186550 ) ) ;
#130518 = CARTESIAN_POINT ( 'NONE',  ( -21.08134388332232589, 65.49997743402062156, -241.9491019618814391 ) ) ;
#130517 = VECTOR ( 'NONE', #39388, 1000.000000000000000 ) ;
#130519 = AXIS2_PLACEMENT_3D ( 'NONE', #53341, #156328, #36374 ) ;
#130520 = EDGE_CURVE ( 'NONE', #165658, #73622, #66180, .T. ) ;
#130522 = EDGE_CURVE ( 'NONE', #62499, #204905, #245269, .T. ) ;
#130521 = CARTESIAN_POINT ( 'NONE',  ( -6.099999999999939249, 64.35000000001120668, -25.92310748452479174 ) ) ;
#130523 = ORIENTED_EDGE ( 'NONE', *, *, #87036, .T. ) ;
#130524 = DIRECTION ( 'NONE',  ( 1.000000000000000000, 0.000000000000000000, 0.000000000000000000 ) ) ;
#130525 = EDGE_CURVE ( 'NONE', #82698, #130620, #20409, .T. ) ;
#130526 = DIRECTION ( 'NONE',  ( -3.265361837132813093E-16, -1.000000000000000000, -6.938893903907229955E-15 ) ) ;
#130527 = CARTESIAN_POINT ( 'NONE',  ( -18.52643265882458579, 68.07764576057050476, -224.1679995073710359 ) ) ;
#130528 = CIRCLE ( 'NONE', #159763, 11.70000000000000817 ) ;
#130530 = CYLINDRICAL_SURFACE ( 'NONE', #74852, 12.87499999999999822 ) ;
#130529 = AXIS2_PLACEMENT_3D ( 'NONE', #51090, #128101, #109803 ) ;
#130531 = CARTESIAN_POINT ( 'NONE',  ( -18.79999999999999716, -11.65000000000000036, 32.89999999999999858 ) ) ;
#130532 = DIRECTION ( 'NONE',  ( 1.000000000000000000, -3.265361837132813093E-16, -2.280189983783949500E-30 ) ) ;
#130533 = ADVANCED_FACE ( 'NONE', ( #105668 ), #143529, .T. ) ;
#130534 = CARTESIAN_POINT ( 'NONE',  ( -16.87333278164146577, 66.11739021543348827, -149.6562752906779110 ) ) ;
#130535 = EDGE_LOOP ( 'NONE', ( #73579, #56449, #15369, #21579 ) ) ;
#130537 = CARTESIAN_POINT ( 'NONE',  ( 18.59999999999998366, 7.021664781911246322, -171.3335654018973173 ) ) ;
#130536 = CARTESIAN_POINT ( 'NONE',  ( -18.79999999999999716, 1.901609089591594470, -11.59510167572422112 ) ) ;
#130538 = ORIENTED_EDGE ( 'NONE', *, *, #156273, .F. ) ;
#130540 = ORIENTED_EDGE ( 'NONE', *, *, #142766, .F. ) ;
#130539 = DIRECTION ( 'NONE',  ( 5.421010862427554711E-16, -0.9770955615653309501, -0.2128009952263636151 ) ) ;
#130541 = EDGE_LOOP ( 'NONE', ( #57720, #252832, #84802, #211731, #158999, #5298 ) ) ;
#130542 = CARTESIAN_POINT ( 'NONE',  ( -16.87036670365549895, 9.989418819312803066, -146.5204398826979855 ) ) ;
#130543 = EDGE_CURVE ( 'NONE', #111624, #200814, #191296, .T. ) ;
#130544 = CARTESIAN_POINT ( 'NONE',  ( 12.25000000000000000, 66.65000000001228386, -153.2731074845244166 ) ) ;
#130545 = CARTESIAN_POINT ( 'NONE',  ( 20.85000000000000142, 76.00000000001244871, -170.0231074845243597 ) ) ;
#130546 = AXIS2_PLACEMENT_3D ( 'NONE', #89342, #35824, #210590 ) ;
#130547 = CARTESIAN_POINT ( 'NONE',  ( 20.95000000000005258, 64.35000000001119247, -6.123107484524794586 ) ) ;
#130548 = VERTEX_POINT ( 'NONE', #109531 ) ;
#130549 = CARTESIAN_POINT ( 'NONE',  ( 21.05000000000000071, 69.45934304831143891, -203.4231074845244223 ) ) ;
#130550 = CARTESIAN_POINT ( 'NONE',  ( 18.49999999999999289, 10.49142135624846617, -158.7500000000000284 ) ) ;
#130551 = TOROIDAL_SURFACE ( 'NONE', #209673, 12.77499999999999858, 0.1000000000000000056 ) ;
#130552 = ORIENTED_EDGE ( 'NONE', *, *, #23536, .T. ) ;
#130553 = CIRCLE ( 'NONE', #188821, 0.1000000000000024342 ) ;
#130555 = EDGE_CURVE ( 'NONE', #234543, #102393, #78809, .T. ) ;
#130554 = CARTESIAN_POINT ( 'NONE',  ( 23.15000000000000213, -9.499999999988848032, -143.8939691226524644 ) ) ;
#130556 = AXIS2_PLACEMENT_3D ( 'NONE', #226028, #26601, #126965 ) ;
#130557 = EDGE_LOOP ( 'NONE', ( #207881, #22302, #46410, #215626 ) ) ;
#130558 = DIRECTION ( 'NONE',  ( -1.000000000000000000, 0.000000000000000000, 0.000000000000000000 ) ) ;
#130559 = EDGE_LOOP ( 'NONE', ( #127166, #81316, #205960, #97254, #21035, #106148, #14689, #146880, #234888, #41233, #11918 ) ) ;
#130560 = CARTESIAN_POINT ( 'NONE',  ( 18.50016250449482413, 65.70233904877112252, -97.54874109119650427 ) ) ;
#130561 = ORIENTED_EDGE ( 'NONE', *, *, #43524, .T. ) ;
#130562 = CARTESIAN_POINT ( 'NONE',  ( -22.39999999999999858, 76.10085836911117951, -181.7726746080137445 ) ) ;
#130563 = CARTESIAN_POINT ( 'NONE',  ( 20.99551997958380056, 64.25000000001175238, -76.37144834683515171 ) ) ;
#130564 = DIRECTION ( 'NONE',  ( -1.000000000000000000, -0.000000000000000000, -0.000000000000000000 ) ) ;
#130565 = CARTESIAN_POINT ( 'NONE',  ( 20.94999999999999929, 43.53458741986633385, -253.2342671440096922 ) ) ;
#130566 = AXIS2_PLACEMENT_3D ( 'NONE', #60925, #217422, #63489 ) ;
#130567 = AXIS2_PLACEMENT_3D ( 'NONE', #34231, #113731, #135845 ) ;
#130568 = CARTESIAN_POINT ( 'NONE',  ( 18.43630871534869797, -9.679800874791796517, -73.66063206798409624 ) ) ;
#130569 = CYLINDRICAL_SURFACE ( 'NONE', #101700, 0.1000000000000054040 ) ;
#130570 = CIRCLE ( 'NONE', #188847, 0.1000000000000072220 ) ;
#130571 = EDGE_LOOP ( 'NONE', ( #218942, #170887, #149606 ) ) ;
#130572 = DIRECTION ( 'NONE',  ( 1.000000000000000000, 0.000000000000000000, 0.000000000000000000 ) ) ;
#130573 = ORIENTED_EDGE ( 'NONE', *, *, #126282, .F. ) ;
#130575 = CARTESIAN_POINT ( 'NONE',  ( -20.54999999999999716, 2.400000000011155432, -53.77537807723790309 ) ) ;
#130574 = PLANE ( 'NONE',  #77812 ) ;
#130576 = ADVANCED_FACE ( 'NONE', ( #246486 ), #103932, .F. ) ;
#130577 = ORIENTED_EDGE ( 'NONE', *, *, #117105, .T. ) ;
#130578 = LINE ( 'NONE', #63213, #255608 ) ;
#130579 = LINE ( 'NONE', #211417, #234760 ) ;
#130580 = AXIS2_PLACEMENT_3D ( 'NONE', #121625, #64195, #165878 ) ;
#130581 = DIRECTION ( 'NONE',  ( 0.000000000000000000, -6.608470384673580212E-15, 1.000000000000000000 ) ) ;
#130582 = CARTESIAN_POINT ( 'NONE',  ( 20.95520789717937404, 59.00725844674948917, -225.7706358438024949 ) ) ;
#130583 = AXIS2_PLACEMENT_3D ( 'NONE', #146091, #106962, #163117 ) ;
#130584 = ORIENTED_EDGE ( 'NONE', *, *, #127295, .F. ) ;
#130586 = ORIENTED_EDGE ( 'NONE', *, *, #112639, .T. ) ;
#130585 = CARTESIAN_POINT ( 'NONE',  ( 23.15000000000000213, 81.75190851390706825, -227.2043352493130612 ) ) ;
#130587 = ADVANCED_FACE ( 'NONE', ( #106966 ), #87402, .F. ) ;
#130588 = EDGE_CURVE ( 'NONE', #129962, #233085, #84811, .T. ) ;
#130589 = AXIS2_PLACEMENT_3D ( 'NONE', #114458, #51893, #251395 ) ;
#130591 = DIRECTION ( 'NONE',  ( 0.000000000000000000, -0.9126074666063545004, -0.4088369013363783999 ) ) ;
#130590 = DIRECTION ( 'NONE',  ( 0.000000000000000000, 0.000000000000000000, 1.000000000000000000 ) ) ;
#130593 = ORIENTED_EDGE ( 'NONE', *, *, #126595, .T. ) ;
#130592 = CARTESIAN_POINT ( 'NONE',  ( 19.97071067811864609, 16.69779891432240149, -222.5912266955230621 ) ) ;
#130594 = CIRCLE ( 'NONE', #230569, 4.099999999999992539 ) ;
#130595 = EDGE_CURVE ( 'NONE', #238186, #232528, #203739, .T. ) ;
#130596 = EDGE_CURVE ( 'NONE', #216161, #86809, #157998, .T. ) ;
#130597 = AXIS2_PLACEMENT_3D ( 'NONE', #33855, #134177, #55904 ) ;
#130598 = AXIS2_PLACEMENT_3D ( 'NONE', #111140, #228536, #91579 ) ;
#130599 = PRODUCT ( 'Snap Open Cable Crossbars 10', 'Snap Open Cable Crossbars 10', '', ( #90053 ) ) ;
#130600 = ORIENTED_EDGE ( 'NONE', *, *, #223473, .F. ) ;
#130601 = EDGE_CURVE ( 'NONE', #181805, #159653, #91329, .T. ) ;
#130602 = EDGE_CURVE ( 'NONE', #172993, #101735, #116455, .T. ) ;
#130603 = VECTOR ( 'NONE', #125782, 1000.000000000000000 ) ;
#130604 = PLANE ( 'NONE',  #122745 ) ;
#130605 = DIRECTION ( 'NONE',  ( -0.000000000000000000, 0.5283051335749948674, -0.8490545835447252943 ) ) ;
#130606 = VERTEX_POINT ( 'NONE', #228223 ) ;
#130607 = CARTESIAN_POINT ( 'NONE',  ( 18.39999999999999858, -9.682403433465241349, -174.1568433774127982 ) ) ;
#130608 = ORIENTED_EDGE ( 'NONE', *, *, #215929, .T. ) ;
#130609 = EDGE_CURVE ( 'NONE', #137344, #87320, #166355, .T. ) ;
#130610 = CARTESIAN_POINT ( 'NONE',  ( -21.55000000000000426, 52.80902093404626640, -233.8693558107618173 ) ) ;
#130611 = CYLINDRICAL_SURFACE ( 'NONE', #243274, 0.1000000000000028644 ) ;
#130612 = AXIS2_PLACEMENT_3D ( 'NONE', #109606, #247842, #225675 ) ;
#130613 = ORIENTED_EDGE ( 'NONE', *, *, #107926, .T. ) ;
#130614 = CYLINDRICAL_SURFACE ( 'NONE', #37651, 0.1000000000000006162 ) ;
#130615 = VECTOR ( 'NONE', #114623, 1000.000000000000000 ) ;
#130616 = ORIENTED_EDGE ( 'NONE', *, *, #180464, .F. ) ;
#130617 = DIRECTION ( 'NONE',  ( 0.000000000000000000, -1.000000000000000000, 0.000000000000000000 ) ) ;
#130618 = VECTOR ( 'NONE', #68461, 999.9999999999998863 ) ;
#130619 = EDGE_CURVE ( 'NONE', #88139, #96681, #52125, .T. ) ;
#130620 = VERTEX_POINT ( 'NONE', #135510 ) ;
#130622 = AXIS2_PLACEMENT_3D ( 'NONE', #216109, #41363, #98696 ) ;
#130621 = B_SPLINE_CURVE_WITH_KNOTS ( 'NONE', 3,
 ( #165211, #246040, #229047, #9989, #50371, #124809, #28305, #46528, #129919, #67394, #209468, #204322, #205606, #107801, #105187, #127373, #184767, #88210, #6117 ),
 .UNSPECIFIED., .F., .F.,
 ( 4, 3, 3, 3, 3, 3, 4 ),
 ( -2.000416914672224079E-06, 0.000000000000000000, 4.714008503745887858E-05, 9.979203887778508822E-05, 0.0001372215519229591648, 0.0001635031576220990037, 0.0001900083748504206697 ),
 .UNSPECIFIED. ) ;
#130623 = EDGE_LOOP ( 'NONE', ( #224587, #29788, #231490, #54433, #184915, #239970, #251311, #61136, #92635, #169406, #39403, #145390, #229448, #250801, #19, #28730, #66594, #162612 ) ) ;
#130624 = CARTESIAN_POINT ( 'NONE',  ( 20.21494484322136387, 18.87362850034901385, -229.4702142578394728 ) ) ;
#130625 = EDGE_LOOP ( 'NONE', ( #134377, #207101, #184646, #161452, #179528 ) ) ;
#130626 = CARTESIAN_POINT ( 'NONE',  ( -19.89999999999999858, 4.611773100472912112, 22.11686199900910665 ) ) ;
#130627 = EDGE_LOOP ( 'NONE', ( #47144, #98527, #145244, #224525 ) ) ;
#130629 = VERTEX_POINT ( 'NONE', #251629 ) ;
#130628 = DIRECTION ( 'NONE',  ( 1.000000000000000000, 0.000000000000000000, 0.000000000000000000 ) ) ;
#130630 = EDGE_CURVE ( 'NONE', #227113, #36387, #175968, .T. ) ;
#130631 = ADVANCED_FACE ( 'NONE', ( #195533 ), #14330, .T. ) ;
#130632 = ORIENTED_EDGE ( 'NONE', *, *, #216392, .T. ) ;
#130633 = DIRECTION ( 'NONE',  ( -1.000000000000000000, 0.000000000000000000, 0.000000000000000000 ) ) ;
#130634 = ORIENTED_EDGE ( 'NONE', *, *, #129148, .F. ) ;
#130637 = EDGE_LOOP ( 'NONE', ( #256289, #83351, #64506, #233777 ) ) ;
#130636 = EDGE_LOOP ( 'NONE', ( #96215, #84139, #239520, #181556 ) ) ;
#130635 = DIRECTION ( 'NONE',  ( 0.000000000000000000, 0.9126074666063660468, 0.4088369013363524762 ) ) ;
#130639 = ORIENTED_EDGE ( 'NONE', *, *, #96111, .F. ) ;
#130638 = AXIS2_PLACEMENT_3D ( 'NONE', #231041, #190629, #91512 ) ;
#130640 = AXIS2_PLACEMENT_3D ( 'NONE', #211744, #215569, #134735 ) ;
#130641 = CIRCLE ( 'NONE', #243069, 0.09999999999999939493 ) ;
#130642 = VECTOR ( 'NONE', #202824, 1000.000000000000000 ) ;
#130643 = FACE_OUTER_BOUND ( 'NONE', #92251, .T. ) ;
#130644 = ORIENTED_EDGE ( 'NONE', *, *, #7611, .F. ) ;
#130645 = CARTESIAN_POINT ( 'NONE',  ( -21.07928932188134041, 69.67148334361398554, -203.6220026301790540 ) ) ;
#130647 = VERTEX_POINT ( 'NONE', #131676 ) ;
#130646 = CARTESIAN_POINT ( 'NONE',  ( 20.94999999999999929, 1.115600667400684642E-11, -200.9999999999999432 ) ) ;
#130648 = DIRECTION ( 'NONE',  ( 1.000000000000000000, -0.000000000000000000, -0.000000000000000000 ) ) ;
#130649 = ORIENTED_EDGE ( 'NONE', *, *, #183333, .T. ) ;
#130650 = FACE_OUTER_BOUND ( 'NONE', #141000, .T. ) ;
#130651 = CYLINDRICAL_SURFACE ( 'NONE', #185631, 0.09999999999999939493 ) ;
#130652 = ORIENTED_EDGE ( 'NONE', *, *, #124131, .F. ) ;
#130653 = DIRECTION ( 'NONE',  ( -1.000000000000000000, 0.000000000000000000, 0.000000000000000000 ) ) ;
#130654 = DIRECTION ( 'NONE',  ( 1.836970198721029934E-16, -1.000000000000000000, -0.000000000000000000 ) ) ;
#130655 = ORIENTED_EDGE ( 'NONE', *, *, #18746, .T. ) ;
#130657 = ORIENTED_EDGE ( 'NONE', *, *, #86631, .T. ) ;
#130656 = DIRECTION ( 'NONE',  ( 0.000000000000000000, -1.000000000000000000, 0.000000000000000000 ) ) ;
#130658 = DIRECTION ( 'NONE',  ( -1.116774769942150098E-16, 1.000000000000000000, 0.000000000000000000 ) ) ;
#130660 = ORIENTED_EDGE ( 'NONE', *, *, #197992, .T. ) ;
#130659 = ORIENTED_EDGE ( 'NONE', *, *, #120242, .T. ) ;
#130661 = ORIENTED_EDGE ( 'NONE', *, *, #90539, .F. ) ;
#130662 = FACE_OUTER_BOUND ( 'NONE', #249969, .T. ) ;
#130663 = ORIENTED_EDGE ( 'NONE', *, *, #48956, .T. ) ;
#130664 = EDGE_LOOP ( 'NONE', ( #35751, #198405, #31215, #194264, #68977 ) ) ;
#130665 = CARTESIAN_POINT ( 'NONE',  ( -23.25000000000000000, 2.000000000011154189, -147.2246219227621111 ) ) ;
#130666 = EDGE_LOOP ( 'NONE', ( #121481, #188730, #133427, #135495 ) ) ;
#130667 = DIRECTION ( 'NONE',  ( 1.000000000000000000, -0.000000000000000000, 0.000000000000000000 ) ) ;
#130668 = DIRECTION ( 'NONE',  ( 0.000000000000000000, -0.5283051335750404975, 0.8490545835446967615 ) ) ;
#130669 = ORIENTED_EDGE ( 'NONE', *, *, #201013, .F. ) ;
#130670 = ADVANCED_FACE ( 'NONE', ( #211215 ), #249712, .T. ) ;
#130671 = B_SPLINE_CURVE_WITH_KNOTS ( 'NONE', 3,
 ( #63339, #142863, #159913, #81598, #162476, #221131, #257638, #20399, #222395, #43800 ),
 .UNSPECIFIED., .F., .F.,
 ( 4, 3, 3, 4 ),
 ( 7.757919228897728493E-18, 0.0002000000000002884074, 0.001000000000045107602, 0.001967863649472132576 ),
 .UNSPECIFIED. ) ;
#130672 = ORIENTED_EDGE ( 'NONE', *, *, #137999, .T. ) ;
#130673 = DIRECTION ( 'NONE',  ( 1.000000000000000000, 1.875376730785737719E-16, 0.000000000000000000 ) ) ;
#130674 = EDGE_CURVE ( 'NONE', #70072, #83264, #85647, .T. ) ;
#130675 = VECTOR ( 'NONE', #74834, 1000.000000000000000 ) ;
#130676 = ORIENTED_EDGE ( 'NONE', *, *, #68031, .F. ) ;
#130677 = AXIS2_PLACEMENT_3D ( 'NONE', #205894, #130197, #32437 ) ;
#130678 = CIRCLE ( 'NONE', #43218, 0.1000000000000028783 ) ;
#130679 = EDGE_CURVE ( 'NONE', #107290, #135886, #242835, .T. ) ;
#130680 = DIRECTION ( 'NONE',  ( 0.000000000000000000, -0.8777080977375132376, 0.4791956752371582251 ) ) ;
#130681 = EDGE_CURVE ( 'NONE', #127304, #104858, #120554, .T. ) ;
#130682 = EDGE_LOOP ( 'NONE', ( #55843, #199655, #96408, #183291, #19198 ) ) ;
#130683 = CARTESIAN_POINT ( 'NONE',  ( 22.45305468355010348, -0.1008583690885486023, -122.2504328765103168 ) ) ;
#130685 = VERTEX_POINT ( 'NONE', #173430 ) ;
#130684 = DIRECTION ( 'NONE',  ( 0.000000000000000000, -7.026728003956695223E-15, 1.000000000000000000 ) ) ;
#130686 = CARTESIAN_POINT ( 'NONE',  ( 21.09610168723072832, 0.03358950690266722383, -127.6210442847752233 ) ) ;
#130687 = CARTESIAN_POINT ( 'NONE',  ( -20.64999999999999858, 68.85000000001254250, -182.3731074845244109 ) ) ;
#130688 = CARTESIAN_POINT ( 'NONE',  ( -17.01764560440165397, 12.43531352655448430, -211.3405985066852395 ) ) ;
#130689 = CARTESIAN_POINT ( 'NONE',  ( 23.14999999999999858, 71.18691588786205671, -57.58158972800053022 ) ) ;
#130690 = DIRECTION ( 'NONE',  ( 1.000000000000000000, -0.000000000000000000, -0.000000000000000000 ) ) ;
#130691 = LINE ( 'NONE', #12064, #24272 ) ;
#130692 = DIRECTION ( 'NONE',  ( 1.000000000000000000, 0.000000000000000000, 0.000000000000000000 ) ) ;
#130693 = CIRCLE ( 'NONE', #168163, 7.900000000000003908 ) ;
#130694 = CIRCLE ( 'NONE', #218162, 0.1000000000000074579 ) ;
#130695 = ORIENTED_EDGE ( 'NONE', *, *, #125661, .T. ) ;
#130696 = ADVANCED_FACE ( 'NONE', ( #232084 ), #228866, .F. ) ;
#130697 = EDGE_CURVE ( 'NONE', #195345, #184179, #174710, .T. ) ;
#130698 = AXIS2_PLACEMENT_3D ( 'NONE', #152107, #172971, #132524 ) ;
#130699 = CIRCLE ( 'NONE', #197329, 0.09999999999998898659 ) ;
#130700 = ORIENTED_EDGE ( 'NONE', *, *, #202453, .T. ) ;
#130702 = VERTEX_POINT ( 'NONE', #55968 ) ;
#130701 = CARTESIAN_POINT ( 'NONE',  ( -16.77683809663752257, 33.06517536918362055, -220.7872234046467952 ) ) ;
#130703 = ORIENTED_EDGE ( 'NONE', *, *, #209059, .T. ) ;
#130704 = FACE_OUTER_BOUND ( 'NONE', #91504, .T. ) ;
#130705 = DIRECTION ( 'NONE',  ( 0.000000000000000000, -0.1350103645451904977, -0.9908441862701596881 ) ) ;
#130707 = CARTESIAN_POINT ( 'NONE',  ( 20.94999999999999929, 67.42187159639590277, -195.4898302452107544 ) ) ;
#130706 = DIRECTION ( 'NONE',  ( -0.000000000000000000, 0.1335171055202901413, 0.9910465087640860649 ) ) ;
#130708 = ORIENTED_EDGE ( 'NONE', *, *, #119070, .T. ) ;
#130709 = B_SPLINE_CURVE_WITH_KNOTS ( 'NONE', 3,
 ( #18285, #216485, #17022, #37876, #45555, #183784, #26000, #245038 ),
 .UNSPECIFIED., .F., .F.,
 ( 4, 2, 2, 4 ),
 ( 0.000000000000000000, 0.0001049670497869849457, 0.0002099340995739698915, 0.0004198681991479773505 ),
 .UNSPECIFIED. ) ;
#130710 = ORIENTED_EDGE ( 'NONE', *, *, #152435, .F. ) ;
#130711 = AXIS2_PLACEMENT_3D ( 'NONE', #236869, #179492, #139016 ) ;
#130712 = AXIS2_PLACEMENT_3D ( 'NONE', #27114, #46618, #166625 ) ;
#130713 = ADVANCED_FACE ( 'NONE', ( #215064 ), #36462, .F. ) ;
#130715 = AXIS2_PLACEMENT_3D ( 'NONE', #62576, #123837, #198222 ) ;
#130714 = CARTESIAN_POINT ( 'NONE',  ( 18.40000000000000213, -9.499999999988840926, -40.49936209718013913 ) ) ;
#130716 = ADVANCED_FACE ( 'NONE', ( #54705 ), #134230, .T. ) ;
#130717 = FACE_OUTER_BOUND ( 'NONE', #157201, .T. ) ;
#130719 = ORIENTED_EDGE ( 'NONE', *, *, #198996, .F. ) ;
#130718 = TOROIDAL_SURFACE ( 'NONE', #26702, 2.699999999999999734, 0.1000000000000000056 ) ;
#130720 = ORIENTED_EDGE ( 'NONE', *, *, #187472, .F. ) ;
#130721 = FACE_OUTER_BOUND ( 'NONE', #133306, .T. ) ;
#130722 = DIRECTION ( 'NONE',  ( 1.000000000000000000, -7.304098846218134667E-16, -5.100424963727256530E-30 ) ) ;
#130723 = DIRECTION ( 'NONE',  ( -0.000000000000000000, -0.9876197685951252359, -0.1568667991644863424 ) ) ;
#130724 = CIRCLE ( 'NONE', #184888, 0.1999999999999987899 ) ;
#130725 = CARTESIAN_POINT ( 'NONE',  ( -22.50000000000000000, 76.00000000001195133, -103.1231074845243114 ) ) ;
#130727 = ORIENTED_EDGE ( 'NONE', *, *, #215303, .T. ) ;
#130726 = DIRECTION ( 'NONE',  ( 0.000000000000000000, -0.01283462868042125823, -0.9999176327611367654 ) ) ;
#130728 = DIRECTION ( 'NONE',  ( -0.000000000000000000, 0.1298341882520009927, 0.9915357197604854900 ) ) ;
#130729 = EDGE_CURVE ( 'NONE', #156660, #162125, #16884, .T. ) ;
#130730 = CARTESIAN_POINT ( 'NONE',  ( -20.85000000000000142, 45.93315328338058379, -256.6017782078560003 ) ) ;
#130731 = AXIS2_PLACEMENT_3D ( 'NONE', #109430, #88582, #188991 ) ;
#130732 = LINE ( 'NONE', #246820, #145919 ) ;
#130733 = CARTESIAN_POINT ( 'NONE',  ( 18.54147908293617064, 85.46326165794005192, -95.97415858776851394 ) ) ;
#130735 = VERTEX_POINT ( 'NONE', #91279 ) ;
#130734 = TOROIDAL_SURFACE ( 'NONE', #97385, 11.65000000000000036, 0.1000000000000000056 ) ;
#130736 = CARTESIAN_POINT ( 'NONE',  ( -18.59999999999999787, 9.150000000011157653, -54.65000000000000568 ) ) ;
#130737 = ADVANCED_FACE ( 'NONE', ( #151259 ), #230802, .F. ) ;
#130738 = CARTESIAN_POINT ( 'NONE',  ( 22.39999999999999858, 7.591056067193225232, -199.2444047917219052 ) ) ;
#130739 = VECTOR ( 'NONE', #202984, 1000.000000000000000 ) ;
#130741 = DIRECTION ( 'NONE',  ( 0.000000000000000000, -1.000000000000000000, 0.000000000000000000 ) ) ;
#130740 = CARTESIAN_POINT ( 'NONE',  ( 20.94999999999999929, 0.000000000000000000, 0.000000000000000000 ) ) ;
#130742 = CARTESIAN_POINT ( 'NONE',  ( 18.59999999999998721, 19.85039924724470950, -169.7803030578013477 ) ) ;
#130743 = DIRECTION ( 'NONE',  ( 1.000000000000000000, 0.000000000000000000, 0.000000000000000000 ) ) ;
#130745 = EDGE_CURVE ( 'NONE', #253599, #111006, #178835, .T. ) ;
#130744 = DIRECTION ( 'NONE',  ( 0.000000000000000000, -0.1298341882519953583, -0.9915357197604862671 ) ) ;
#130746 = PLANE ( 'NONE',  #222708 ) ;
#130747 = FACE_OUTER_BOUND ( 'NONE', #191368, .T. ) ;
#130748 = LINE ( 'NONE', #192033, #35270 ) ;
#130749 = EDGE_LOOP ( 'NONE', ( #3799, #204913, #31153, #177829 ) ) ;
#130750 = EDGE_LOOP ( 'NONE', ( #123406, #63714, #102888, #243860 ) ) ;
#130751 = ORIENTED_EDGE ( 'NONE', *, *, #235822, .F. ) ;
#130752 = DIRECTION ( 'NONE',  ( 0.000000000000000000, 0.9908441862701596881, 0.1350103645451904977 ) ) ;
#130753 = CARTESIAN_POINT ( 'NONE',  ( -21.59142135623730852, 68.15000000001187175, -90.67310748452436542 ) ) ;
#130754 = ORIENTED_EDGE ( 'NONE', *, *, #203629, .T. ) ;
#130755 = ADVANCED_FACE ( 'NONE', ( #81929 ), #200643, .T. ) ;
#130756 = ORIENTED_EDGE ( 'NONE', *, *, #182375, .F. ) ;
#130757 = EDGE_CURVE ( 'NONE', #40198, #244668, #83069, .T. ) ;
#130758 = VECTOR ( 'NONE', #81744, 1000.000000000000000 ) ;
#130759 = CIRCLE ( 'NONE', #243174, 0.1999999999999996503 ) ;
#130760 = ORIENTED_EDGE ( 'NONE', *, *, #48944, .F. ) ;
#130761 = CIRCLE ( 'NONE', #93156, 0.1000000000000069167 ) ;
#130762 = DIRECTION ( 'NONE',  ( 0.000000000000000000, 1.000000000000000000, 6.982962677686266711E-15 ) ) ;
#130763 = ORIENTED_EDGE ( 'NONE', *, *, #130681, .T. ) ;
#130764 = CARTESIAN_POINT ( 'NONE',  ( -23.25000000000000000, -8.999999999988844479, -90.60603087734760663 ) ) ;
#130765 = DIRECTION ( 'NONE',  ( 1.000000000000000000, 0.000000000000000000, 0.000000000000000000 ) ) ;
#130766 = CIRCLE ( 'NONE', #93160, 0.1000000000000028644 ) ;
#130767 = LINE ( 'NONE', #150348, #220758 ) ;
#130768 = DIRECTION ( 'NONE',  ( 0.000000000000000000, -0.8660254037844247188, 0.5000000000000245359 ) ) ;
#130770 = ORIENTED_EDGE ( 'NONE', *, *, #63995, .F. ) ;
#130769 = CARTESIAN_POINT ( 'NONE',  ( 21.05000000000000071, 76.00000000001244871, -170.0231074845243597 ) ) ;
#130772 = CARTESIAN_POINT ( 'NONE',  ( 21.09787244211732826, 8.775370707348422172, -79.23925338431750731 ) ) ;
#130771 = DIRECTION ( 'NONE',  ( -1.836970198721029934E-16, 1.000000000000000000, 0.000000000000000000 ) ) ;
#130773 = LINE ( 'NONE', #193331, #206971 ) ;
#130774 = ORIENTED_EDGE ( 'NONE', *, *, #157825, .F. ) ;
#130775 = CARTESIAN_POINT ( 'NONE',  ( 15.52844286134407525, 66.62433047358628357, -120.6553174751384461 ) ) ;
#130776 = CIRCLE ( 'NONE', #193156, 0.4000000000000033529 ) ;
#130777 = CARTESIAN_POINT ( 'NONE',  ( 21.14999999999999858, 59.16775194334852017, -221.0793150863668473 ) ) ;
#130778 = CARTESIAN_POINT ( 'NONE',  ( 21.04999999999999716, -0.03753606327451285835, -60.66772772606437059 ) ) ;
#130779 = ORIENTED_EDGE ( 'NONE', *, *, #103304, .F. ) ;
#130780 = DIRECTION ( 'NONE',  ( 0.000000000000000000, 0.000000000000000000, -1.000000000000000000 ) ) ;
#130781 = AXIS2_PLACEMENT_3D ( 'NONE', #140443, #182161, #141731 ) ;
#130782 = CARTESIAN_POINT ( 'NONE',  ( -20.54999999999999716, 4.250000000000000000, -12.25000000000000000 ) ) ;
#130783 = VERTEX_POINT ( 'NONE', #141940 ) ;
#130784 = AXIS2_PLACEMENT_3D ( 'NONE', #234536, #191600, #35100 ) ;
#130785 = DIRECTION ( 'NONE',  ( 0.000000000000000000, 0.000000000000000000, -1.000000000000000000 ) ) ;
#130786 = DIRECTION ( 'NONE',  ( 0.000000000000000000, 0.8814952561688430555, -0.4721928772777346239 ) ) ;
#130787 = PLANE ( 'NONE',  #174120 ) ;
#130788 = ORIENTED_EDGE ( 'NONE', *, *, #201013, .T. ) ;
#130789 = CIRCLE ( 'NONE', #47572, 11.74999999999999822 ) ;
#130790 = ORIENTED_EDGE ( 'NONE', *, *, #223282, .T. ) ;
#130791 = DIRECTION ( 'NONE',  ( -0.000000000000000000, -6.982962677686266711E-15, 1.000000000000000000 ) ) ;
#130793 = AXIS2_PLACEMENT_3D ( 'NONE', #142835, #183280, #120765 ) ;
#130792 = CARTESIAN_POINT ( 'NONE',  ( 20.85000000000000142, 80.69087520990402140, -192.8618289658565743 ) ) ;
#130794 = CARTESIAN_POINT ( 'NONE',  ( 20.93302460841142931, 65.68434038414410736, -164.4866880726065972 ) ) ;
#130795 = CARTESIAN_POINT ( 'NONE',  ( 18.54999999999999716, 8.750000000011182166, -143.2500000000000284 ) ) ;
#130796 = EDGE_CURVE ( 'NONE', #84065, #197300, #198064, .T. ) ;
#130798 = FACE_OUTER_BOUND ( 'NONE', #106675, .T. ) ;
#130797 = CARTESIAN_POINT ( 'NONE',  ( -20.64999999999999858, 7.150000000011155876, -155.1500000000000057 ) ) ;
#130799 = DIRECTION ( 'NONE',  ( -1.000000000000000000, 0.000000000000000000, 0.000000000000000000 ) ) ;
#130800 = CYLINDRICAL_SURFACE ( 'NONE', #55981, 0.1000000000000028644 ) ;
#130801 = CARTESIAN_POINT ( 'NONE',  ( 21.00000000000000000, 9.750000000011153745, -155.1500000000000057 ) ) ;
#130802 = CIRCLE ( 'NONE', #55756, 0.1000000000000124678 ) ;
#130803 = ORIENTED_EDGE ( 'NONE', *, *, #70226, .T. ) ;
#130804 = CARTESIAN_POINT ( 'NONE',  ( 18.59999999999999432, 74.83729825007360148, -61.42310748452432989 ) ) ;
#130805 = AXIS2_PLACEMENT_3D ( 'NONE', #29013, #227160, #205011 ) ;
#130807 = EDGE_LOOP ( 'NONE', ( #177508, #114529, #167271, #151815 ) ) ;
#130806 = CARTESIAN_POINT ( 'NONE',  ( -23.15000000000000213, 64.35000000001254250, -182.1731074845244507 ) ) ;
#130808 = VECTOR ( 'NONE', #125696, 1000.000000000000000 ) ;
#130809 = FACE_OUTER_BOUND ( 'NONE', #148280, .T. ) ;
#130810 = FACE_OUTER_BOUND ( 'NONE', #179422, .T. ) ;
#130811 = CYLINDRICAL_SURFACE ( 'NONE', #54448, 0.1000000000000001443 ) ;
#130812 = CARTESIAN_POINT ( 'NONE',  ( -16.79270642812296188, 66.05375578307388196, -123.8620407630872648 ) ) ;
#130813 = EDGE_CURVE ( 'NONE', #223187, #86704, #37343, .T. ) ;
#130814 = CARTESIAN_POINT ( 'NONE',  ( 20.94999999999999929, 7.128833340094563376, -233.7327013124401276 ) ) ;
#130816 = ORIENTED_EDGE ( 'NONE', *, *, #118085, .T. ) ;
#130815 = CARTESIAN_POINT ( 'NONE',  ( -18.40000000000000213, 64.52683809664910086, -56.97310748452440521 ) ) ;
#130818 = DIRECTION ( 'NONE',  ( 0.000000000000000000, 0.000000000000000000, -1.000000000000000000 ) ) ;
#130817 = APPLICATION_CONTEXT ( 'automotive_design' ) ;
#130819 = CARTESIAN_POINT ( 'NONE',  ( -21.59142135623730852, 7.850000000011158718, -188.6499999999999488 ) ) ;
#130820 = DIRECTION ( 'NONE',  ( 1.000000000000000000, 7.304098846218135653E-16, 0.000000000000000000 ) ) ;
#130821 = DIRECTION ( 'NONE',  ( 0.000000000000000000, -0.1350103645451974088, 0.9908441862701587999 ) ) ;
#130822 = EDGE_LOOP ( 'NONE', ( #141659, #124241, #182246, #252719 ) ) ;
#130823 = FACE_OUTER_BOUND ( 'NONE', #149554, .T. ) ;
#130824 = EDGE_CURVE ( 'NONE', #204044, #253445, #19441, .T. ) ;
#130826 = EDGE_CURVE ( 'NONE', #251611, #91084, #138079, .T. ) ;
#130825 = VERTEX_POINT ( 'NONE', #139356 ) ;
#130827 = CARTESIAN_POINT ( 'NONE',  ( 22.49999999999999645, 75.90000000001276703, -215.1726782920691505 ) ) ;
#130829 = VERTEX_POINT ( 'NONE', #136803 ) ;
#130828 = TOROIDAL_SURFACE ( 'NONE', #164158, 0.2000000000000000111, 0.1000000000000000056 ) ;
#130830 = CARTESIAN_POINT ( 'NONE',  ( -22.59999999999999787, 7.128833340093095217, -233.7327013124392749 ) ) ;
#130831 = AXIS2_PLACEMENT_3D ( 'NONE', #148204, #45255, #246030 ) ;
#130832 = AXIS2_PLACEMENT_3D ( 'NONE', #254747, #55274, #197379 ) ;
#130833 = ORIENTED_EDGE ( 'NONE', *, *, #224414, .T. ) ;
#130834 = CARTESIAN_POINT ( 'NONE',  ( 22.60000000000000142, 1.115600667400684642E-11, -100.5000000000000284 ) ) ;
#130835 = CARTESIAN_POINT ( 'NONE',  ( -23.15000000000000213, 11.65000000001115588, -21.75000000000000355 ) ) ;
#130836 = EDGE_CURVE ( 'NONE', #103016, #253481, #37741, .T. ) ;
#130837 =( BOUNDED_CURVE ( )  B_SPLINE_CURVE ( 3, ( #198041, #141919, #83203, #216322 ),
 .UNSPECIFIED., .F., .F. ) 
 B_SPLINE_CURVE_WITH_KNOTS ( ( 4, 4 ),
 ( 1.570796326794901665, 3.141592653589802886 ),
 .UNSPECIFIED. ) 
 CURVE ( )  GEOMETRIC_REPRESENTATION_ITEM ( )  RATIONAL_B_SPLINE_CURVE ( ( 1.000000000000000000, 0.8047378541243639383, 0.8047378541243639383, 1.000000000000000000 ) ) 
 REPRESENTATION_ITEM ( '' )  );
#130838 = CARTESIAN_POINT ( 'NONE',  ( -20.64999999999999858, 71.65000000001222702, -148.8731074845244109 ) ) ;
#130839 = VERTEX_POINT ( 'NONE', #102788 ) ;
#130840 = DIRECTION ( 'NONE',  ( 1.734723475976817823E-14, 0.9126074666063771490, 0.4088369013363281623 ) ) ;
#130841 = CARTESIAN_POINT ( 'NONE',  ( -20.94999999999994600, 66.15000000001120384, -4.523107484524794053 ) ) ;
#130842 = LINE ( 'NONE', #173877, #170663 ) ;
#130843 = DIRECTION ( 'NONE',  ( 0.000000000000000000, -1.000000000000000000, 8.673617379884042375E-16 ) ) ;
#130844 = CARTESIAN_POINT ( 'NONE',  ( -16.90128866880176162, 66.04620422280905245, -115.6604313011357306 ) ) ;
#130845 = ORIENTED_EDGE ( 'NONE', *, *, #20959, .T. ) ;
#130846 = CARTESIAN_POINT ( 'NONE',  ( 18.60000000000000142, -9.399999999988782662, -74.29725975966333351 ) ) ;
#130847 = ORIENTED_EDGE ( 'NONE', *, *, #251298, .F. ) ;
#130848 = EDGE_LOOP ( 'NONE', ( #60603, #183201, #132179, #179462 ) ) ;
#130849 = ORIENTED_EDGE ( 'NONE', *, *, #20543, .T. ) ;
#130850 = CIRCLE ( 'NONE', #251467, 1.749999999999998002 ) ;
#130851 = CARTESIAN_POINT ( 'NONE',  ( -21.64999999999999858, 10.04999999999998295, -20.85000000000000142 ) ) ;
#130852 = ORIENTED_EDGE ( 'NONE', *, *, #13706, .F. ) ;
#130853 = EDGE_CURVE ( 'NONE', #57106, #111888, #8113, .T. ) ;
#130854 = CARTESIAN_POINT ( 'NONE',  ( 23.24999999999999645, 1.115600667400684642E-11, -67.00000000000000000 ) ) ;
#130855 = LINE ( 'NONE', #51289, #51791 ) ;
#130856 = DIRECTION ( 'NONE',  ( 1.000000000000000000, 0.000000000000000000, 0.000000000000000000 ) ) ;
#130857 = EDGE_LOOP ( 'NONE', ( #119426, #251046, #15782, #247491 ) ) ;
#130858 = FACE_BOUND ( 'NONE', #64080, .T. ) ;
#130859 = CARTESIAN_POINT ( 'NONE',  ( 23.14999999999999858, 5.500000000011153745, -155.0947339810869323 ) ) ;
#130860 = CARTESIAN_POINT ( 'NONE',  ( -23.25000000000000000, -10.82118976317943826, -206.5294079347637819 ) ) ;
#130861 = ORIENTED_EDGE ( 'NONE', *, *, #83790, .F. ) ;
#130863 = ORIENTED_EDGE ( 'NONE', *, *, #45803, .T. ) ;
#130862 = FACE_OUTER_BOUND ( 'NONE', #132653, .T. ) ;
#130864 = CARTESIAN_POINT ( 'NONE',  ( 22.47071067811865319, 7.720074744509199505, -33.40090754529740025 ) ) ;
#130866 = EDGE_CURVE ( 'NONE', #55107, #111978, #87194, .T. ) ;
#130865 = CARTESIAN_POINT ( 'NONE',  ( -20.64999999999999858, 66.23941198528750363, -222.8935984851895853 ) ) ;
#130867 = AXIS2_PLACEMENT_3D ( 'NONE', #179626, #3524, #158791 ) ;
#130868 = ORIENTED_EDGE ( 'NONE', *, *, #21175, .F. ) ;
#130870 = DIRECTION ( 'NONE',  ( 1.000000000000000000, 0.000000000000000000, 0.000000000000000000 ) ) ;
#130869 = VECTOR ( 'NONE', #8850, 1000.000000000000114 ) ;
#130871 = CARTESIAN_POINT ( 'NONE',  ( -18.37013991200266005, 40.35975918565798537, -235.2922552195464618 ) ) ;
#130872 = DIRECTION ( 'NONE',  ( 0.7070776581709139474, 0.2891032514073391679, -0.6453375049857563717 ) ) ;
#130873 = ORIENTED_EDGE ( 'NONE', *, *, #203575, .T. ) ;
#130874 = DIRECTION ( 'NONE',  ( 0.000000000000000000, 0.8814952561688429444, -0.4721928772777345684 ) ) ;
#130875 = CARTESIAN_POINT ( 'NONE',  ( 21.05000000000000071, 64.40000000001248281, -176.9513107147999449 ) ) ;
#130876 = CARTESIAN_POINT ( 'NONE',  ( 18.49999999999999645, 76.00000000001195133, -103.0231074845243171 ) ) ;
#130877 = EDGE_CURVE ( 'NONE', #222999, #243219, #153916, .T. ) ;
#130878 = CIRCLE ( 'NONE', #172635, 0.09999999999998898659 ) ;
#130879 = CIRCLE ( 'NONE', #68354, 0.09999999999998898659 ) ;
#130880 = TOROIDAL_SURFACE ( 'NONE', #164224, 0.2000000000000000111, 0.1000000000000000056 ) ;
#130881 = ORIENTED_EDGE ( 'NONE', *, *, #61959, .T. ) ;
#130882 = CARTESIAN_POINT ( 'NONE',  ( 21.12400247839514122, 65.27851195598221068, -191.2731074845244166 ) ) ;
#130883 = AXIS2_PLACEMENT_3D ( 'NONE', #77712, #72621, #153472 ) ;
#130884 = ADVANCED_FACE ( 'NONE', ( #158976 ), #42849, .F. ) ;
#130886 = ADVANCED_FACE ( 'NONE', ( #40318 ), #119842, .F. ) ;
#130885 = VECTOR ( 'NONE', #169024, 1000.000000000000000 ) ;
#130887 = ORIENTED_EDGE ( 'NONE', *, *, #52279, .T. ) ;
#130888 = CARTESIAN_POINT ( 'NONE',  ( 21.05000000000000071, 76.00000000001165290, -69.52310748452431710 ) ) ;
#130889 = LINE ( 'NONE', #150475, #83259 ) ;
#130891 = VERTEX_POINT ( 'NONE', #39013 ) ;
#130890 = DIRECTION ( 'NONE',  ( 0.000000000000000000, -4.440892098500611173E-15, -1.000000000000000000 ) ) ;
#130892 = CARTESIAN_POINT ( 'NONE',  ( -21.45000000000000284, 68.29142135624952914, -148.7731074845244166 ) ) ;
#130893 = DIRECTION ( 'NONE',  ( -1.000000000000000000, 3.265361837132813093E-16, 2.280189983783949500E-30 ) ) ;
#130895 = EDGE_CURVE ( 'NONE', #5925, #27502, #101489, .T. ) ;
#130894 = FACE_BOUND ( 'NONE', #91929, .T. ) ;
#130897 = EDGE_CURVE ( 'NONE', #29497, #196290, #199371, .T. ) ;
#130896 = CARTESIAN_POINT ( 'NONE',  ( -18.59999999999999787, -9.399999999988851940, -73.88204184817267617 ) ) ;
#130898 = CARTESIAN_POINT ( 'NONE',  ( -18.59999999999999787, 77.73670573947964613, -125.0056848969006182 ) ) ;
#130899 = VECTOR ( 'NONE', #17244, 999.9999999999998863 ) ;
#130900 = CYLINDRICAL_SURFACE ( 'NONE', #243066, 2.000000000000003553 ) ;
#130901 = CIRCLE ( 'NONE', #147473, 2.000000000000001776 ) ;
#130902 = CARTESIAN_POINT ( 'NONE',  ( 23.24999999999999289, 11.75000000001116263, -33.60000000000000142 ) ) ;
#130904 = ORIENTED_EDGE ( 'NONE', *, *, #82897, .T. ) ;
#130903 = FACE_OUTER_BOUND ( 'NONE', #71104, .T. ) ;
#130905 = AXIS2_PLACEMENT_3D ( 'NONE', #243130, #46209, #102298 ) ;
#130906 = EDGE_CURVE ( 'NONE', #191184, #141149, #239771, .T. ) ;
#130907 = AXIS2_PLACEMENT_3D ( 'NONE', #51887, #11520, #131445 ) ;
#130908 = EDGE_CURVE ( 'NONE', #8126, #185121, #116628, .T. ) ;
#130910 = ADVANCED_FACE ( 'NONE', ( #31965 ), #48925, .T. ) ;
#130909 = EDGE_CURVE ( 'NONE', #59204, #25443, #253784, .T. ) ;
#130911 = CYLINDRICAL_SURFACE ( 'NONE', #159978, 0.09999999999999939493 ) ;
#130912 = CIRCLE ( 'NONE', #135168, 0.09999999999999939493 ) ;
#130913 = CARTESIAN_POINT ( 'NONE',  ( -2.995603634470829482E-16, 6.650000000011155876, -155.1500000000000057 ) ) ;
#130914 = CARTESIAN_POINT ( 'NONE',  ( 23.25000000000000000, 87.75000000001143974, -39.12310748452424747 ) ) ;
#130915 = FACE_OUTER_BOUND ( 'NONE', #7776, .T. ) ;
#130916 = AXIS2_PLACEMENT_3D ( 'NONE', #50417, #27060, #146955 ) ;
#130918 = ORIENTED_EDGE ( 'NONE', *, *, #195070, .T. ) ;
#130917 = AXIS2_PLACEMENT_3D ( 'NONE', #50687, #168144, #228082 ) ;
#130919 = AXIS2_PLACEMENT_3D ( 'NONE', #257463, #215806, #78863 ) ;
#130920 = EDGE_CURVE ( 'NONE', #206475, #77283, #154085, .T. ) ;
#130921 = DIRECTION ( 'NONE',  ( 1.000000000000000000, 0.000000000000000000, -0.000000000000000000 ) ) ;
#130922 = DIRECTION ( 'NONE',  ( 1.000000000000000000, 0.000000000000000000, 0.000000000000000000 ) ) ;
#130923 = ORIENTED_EDGE ( 'NONE', *, *, #223054, .T. ) ;
#130924 = ADVANCED_FACE ( 'NONE', ( #131035 ), #179637, .T. ) ;
#130925 = EDGE_CURVE ( 'NONE', #239517, #219834, #111091, .T. ) ;
#130926 = DIRECTION ( 'NONE',  ( 0.000000000000000000, -0.4088369013363280513, 0.9126074666063769270 ) ) ;
#130927 =( BOUNDED_CURVE ( )  B_SPLINE_CURVE ( 3, ( #114030, #174065, #171489, #151916 ),
 .UNSPECIFIED., .F., .F. ) 
 B_SPLINE_CURVE_WITH_KNOTS ( ( 4, 4 ),
 ( 4.712388980384689674, 6.231880751915386263 ),
 .UNSPECIFIED. ) 
 CURVE ( )  GEOMETRIC_REPRESENTATION_ITEM ( )  RATIONAL_B_SPLINE_CURVE ( ( 1.000000000000000000, 0.8166740347213228279, 0.8166740347213228279, 1.000000000000000000 ) ) 
 REPRESENTATION_ITEM ( '' )  );
#130928 = CARTESIAN_POINT ( 'NONE',  ( -16.93226657140833069, 9.999543822735571297, -79.57871311097366629 ) ) ;
#130929 = ADVANCED_FACE ( 'NONE', ( #168932 ), #145639, .T. ) ;
#130930 = EDGE_LOOP ( 'NONE', ( #140157, #244323, #97787, #138343 ) ) ;
#130931 = CARTESIAN_POINT ( 'NONE',  ( -16.86337532320261801, 66.02003279578825357, -190.9720319535072406 ) ) ;
#130932 = EDGE_LOOP ( 'NONE', ( #257832, #204403, #241682, #173828 ) ) ;
#130933 = CARTESIAN_POINT ( 'NONE',  ( 20.95512820512820440, 65.37615131630018084, -124.3731074845243825 ) ) ;
#130935 = ORIENTED_EDGE ( 'NONE', *, *, #129521, .F. ) ;
#130934 = DIRECTION ( 'NONE',  ( -0.000000000000000000, -0.1298341882520022694, -0.9915357197604853789 ) ) ;
#130936 = EDGE_CURVE ( 'NONE', #215603, #115618, #237428, .T. ) ;
#130937 = FACE_OUTER_BOUND ( 'NONE', #135954, .T. ) ;
#130938 = ORIENTED_EDGE ( 'NONE', *, *, #245413, .F. ) ;
#130939 = AXIS2_PLACEMENT_3D ( 'NONE', #133316, #197123, #56321 ) ;
#130940 = DIRECTION ( 'NONE',  ( 1.000000000000000000, 0.000000000000000000, 0.000000000000000000 ) ) ;
#130941 = ORIENTED_EDGE ( 'NONE', *, *, #37329, .T. ) ;
#130942 = AXIS2_PLACEMENT_3D ( 'NONE', #99145, #58, #39222 ) ;
#130944 = ORIENTED_EDGE ( 'NONE', *, *, #114741, .T. ) ;
#130943 = EDGE_LOOP ( 'NONE', ( #257514, #187270, #239671, #86752 ) ) ;
#130945 = CARTESIAN_POINT ( 'NONE',  ( -18.39999999999999858, -9.600000000000004974, -40.10018939122204529 ) ) ;
#130947 = ORIENTED_EDGE ( 'NONE', *, *, #91206, .F. ) ;
#130946 = CARTESIAN_POINT ( 'NONE',  ( 21.05000000000000071, 1.115600667400684642E-11, -100.5000000000000426 ) ) ;
#130948 = CIRCLE ( 'NONE', #35128, 0.09999999999998898659 ) ;
#130949 = CARTESIAN_POINT ( 'NONE',  ( 20.94983749550516450, 65.70233904876990039, -64.04874109119681691 ) ) ;
#130950 = ORIENTED_EDGE ( 'NONE', *, *, #145008, .T. ) ;
#130951 = VECTOR ( 'NONE', #214319, 1000.000000000000000 ) ;
#130952 = TOROIDAL_SURFACE ( 'NONE', #35137, 6.258578643762712446, 0.1000000000000000056 ) ;
#130953 = ORIENTED_EDGE ( 'NONE', *, *, #46570, .T. ) ;
#130954 = CARTESIAN_POINT ( 'NONE',  ( 18.59999999999999787, 74.14897176987143723, -158.3691942151018850 ) ) ;
#130955 = PLANE ( 'NONE',  #26379 ) ;
#130956 = CARTESIAN_POINT ( 'NONE',  ( -18.45140287520620248, 38.03325571449392584, -261.0487029501068150 ) ) ;
#130957 = ORIENTED_EDGE ( 'NONE', *, *, #237116, .F. ) ;
#130958 = TOROIDAL_SURFACE ( 'NONE', #122611, 11.65000000000000036, 0.1000000000000000056 ) ;
#130959 = CARTESIAN_POINT ( 'NONE',  ( -18.50000000000000000, 7.120270961708746960, -104.1595630418393768 ) ) ;
#130960 = CARTESIAN_POINT ( 'NONE',  ( 21.09793522318413395, 65.27537548979879034, -57.28381661354728038 ) ) ;
#130961 = CARTESIAN_POINT ( 'NONE',  ( -20.05000000000000426, 9.250000000011157297, -45.85000000000000142 ) ) ;
#130962 = CIRCLE ( 'NONE', #135027, 0.1000000000000033362 ) ;
#130963 = ORIENTED_EDGE ( 'NONE', *, *, #246257, .T. ) ;
#130964 = LINE ( 'NONE', #14890, #208531 ) ;
#130965 = CIRCLE ( 'NONE', #18549, 0.1000000000000028644 ) ;
#130966 = DIRECTION ( 'NONE',  ( 0.000000000000000000, 0.000000000000000000, -1.000000000000000000 ) ) ;
#130967 = CARTESIAN_POINT ( 'NONE',  ( 22.39999999999999858, 68.20922040163900135, -170.1231074845244109 ) ) ;
#130969 = DIRECTION ( 'NONE',  ( -0.000000000000000000, 0.8814952561688430555, -0.4721928772777346239 ) ) ;
#130968 = AXIS2_PLACEMENT_3D ( 'NONE', #163765, #102459, #127201 ) ;
#130970 = ORIENTED_EDGE ( 'NONE', *, *, #143841, .T. ) ;
#130971 = CARTESIAN_POINT ( 'NONE',  ( 22.49999999999999645, 0.04562336060750230710, -55.34949566145051847 ) ) ;
#130972 = ORIENTED_EDGE ( 'NONE', *, *, #34730, .F. ) ;
#130973 = DIRECTION ( 'NONE',  ( 0.000000000000000000, 0.1678971852675816834, 0.9858045116447902156 ) ) ;
#130974 = ORIENTED_EDGE ( 'NONE', *, *, #205976, .T. ) ;
#130975 = DIRECTION ( 'NONE',  ( 1.000000000000000000, 2.952720810173289112E-16, -0.000000000000000000 ) ) ;
#130976 = CARTESIAN_POINT ( 'NONE',  ( 18.39999999999999858, -9.682403433465241349, -107.1568433774128408 ) ) ;
#130977 = ORIENTED_EDGE ( 'NONE', *, *, #246795, .T. ) ;
#130978 = ORIENTED_EDGE ( 'NONE', *, *, #124441, .T. ) ;
#130979 = LINE ( 'NONE', #210520, #103116 ) ;
#130980 = LINE ( 'NONE', #12342, #154370 ) ;
#130981 = VERTEX_POINT ( 'NONE', #24592 ) ;
#130982 = VECTOR ( 'NONE', #226023, 1000.000000000000000 ) ;
#130983 = DIRECTION ( 'NONE',  ( 1.000000000000000000, 0.000000000000000000, 0.000000000000000000 ) ) ;
#130984 = CARTESIAN_POINT ( 'NONE',  ( -18.52643265882458579, 65.68026841930881687, -63.97257401318892533 ) ) ;
#130985 = ORIENTED_EDGE ( 'NONE', *, *, #153653, .F. ) ;
#130986 = AXIS2_PLACEMENT_3D ( 'NONE', #155739, #94441, #157015 ) ;
#130987 = EDGE_CURVE ( 'NONE', #248593, #10221, #91904, .T. ) ;
#130988 = ADVANCED_FACE ( 'NONE', ( #104076 ), #148043, .T. ) ;
#130990 = ORIENTED_EDGE ( 'NONE', *, *, #135713, .F. ) ;
#130989 = CIRCLE ( 'NONE', #222546, 0.1000000000000055844 ) ;
#130991 = VECTOR ( 'NONE', #122844, 1000.000000000000114 ) ;
#130992 = LINE ( 'NONE', #250919, #251613 ) ;
#130993 = EDGE_CURVE ( 'NONE', #209903, #141605, #20790, .T. ) ;
#130994 = CARTESIAN_POINT ( 'NONE',  ( -20.64999999999999858, 9.593045456726526865, -211.4478935133083439 ) ) ;
#130995 = ADVANCED_FACE ( 'NONE', ( #153205 ), #172780, .F. ) ;
#130996 = DIRECTION ( 'NONE',  ( -0.000000000000000000, 0.000000000000000000, -1.000000000000000000 ) ) ;
#130997 = VERTEX_POINT ( 'NONE', #257341 ) ;
#130998 = FACE_OUTER_BOUND ( 'NONE', #135792, .T. ) ;
#130999 = DIRECTION ( 'NONE',  ( 0.000000000000000000, -7.304098846218085561E-15, 1.000000000000000000 ) ) ;
#131001 = CARTESIAN_POINT ( 'NONE',  ( 19.92426406871192412, 64.25000000001220712, -145.1731074845244507 ) ) ;
#131000 = CARTESIAN_POINT ( 'NONE',  ( 18.59999999999999787, -11.74999999999999289, -24.85000000000000142 ) ) ;
#131002 = CARTESIAN_POINT ( 'NONE',  ( -21.29999999999995808, 1.115600667400684642E-11, -138.0500000000000114 ) ) ;
#131003 = FACE_OUTER_BOUND ( 'NONE', #101173, .T. ) ;
#131004 = CARTESIAN_POINT ( 'NONE',  ( 20.94999999999999574, 7.939498413483247141, -209.7295111514051200 ) ) ;
#131005 = FACE_OUTER_BOUND ( 'NONE', #252179, .T. ) ;
#131006 = ORIENTED_EDGE ( 'NONE', *, *, #163953, .T. ) ;
#131007 = EDGE_CURVE ( 'NONE', #54485, #89738, #70860, .T. ) ;
#131008 = EDGE_CURVE ( 'NONE', #48243, #93865, #213139, .T. ) ;
#131009 = ORIENTED_EDGE ( 'NONE', *, *, #234430, .F. ) ;
#131010 = VECTOR ( 'NONE', #75683, 1000.000000000000000 ) ;
#131011 = ORIENTED_EDGE ( 'NONE', *, *, #206951, .T. ) ;
#131012 = CYLINDRICAL_SURFACE ( 'NONE', #119351, 7.899999999999990585 ) ;
#131013 = DIRECTION ( 'NONE',  ( 0.000000000000000000, 0.000000000000000000, 1.000000000000000000 ) ) ;
#131014 = ORIENTED_EDGE ( 'NONE', *, *, #41744, .F. ) ;
#131015 =( NAMED_UNIT ( * ) SI_UNIT ( $, .STERADIAN. ) SOLID_ANGLE_UNIT ( ) );
#131016 = DIRECTION ( 'NONE',  ( 0.000000000000000000, 0.06430067914209719460, -0.9979305700607958851 ) ) ;
#131017 = CARTESIAN_POINT ( 'NONE',  ( -16.87331047859649757, 63.08573235307424198, -213.1276215869287967 ) ) ;
#131018 = EDGE_CURVE ( 'NONE', #111525, #251571, #237253, .T. ) ;
#131019 = DIRECTION ( 'NONE',  ( 0.000000000000000000, 0.000000000000000000, -1.000000000000000000 ) ) ;
#131020 = ORIENTED_EDGE ( 'NONE', *, *, #171576, .T. ) ;
#131021 = ORIENTED_EDGE ( 'NONE', *, *, #114815, .T. ) ;
#131023 = CARTESIAN_POINT ( 'NONE',  ( 12.25000000000000000, 66.65000000001228386, -153.2731074845244166 ) ) ;
#131022 = AXIS2_PLACEMENT_3D ( 'NONE', #149223, #125776, #226133 ) ;
#131024 = MECHANICAL_DESIGN_GEOMETRIC_PRESENTATION_REPRESENTATION (  '', ( #255886 ), #114278 ) ;
#131025 = DIRECTION ( 'NONE',  ( 0.000000000000000000, 0.1350103645451876666, -0.9908441862701600211 ) ) ;
#131026 = ORIENTED_EDGE ( 'NONE', *, *, #139811, .T. ) ;
#131027 = FACE_OUTER_BOUND ( 'NONE', #22999, .T. ) ;
#131029 = ORIENTED_EDGE ( 'NONE', *, *, #118793, .F. ) ;
#131028 = DIRECTION ( 'NONE',  ( -1.000000000000000000, 5.467925025959462129E-15, -3.427148797533442008E-14 ) ) ;
#131030 = CARTESIAN_POINT ( 'NONE',  ( -21.29999999999995808, 76.00000000001165290, -69.52310748452431710 ) ) ;
#131031 = EDGE_CURVE ( 'NONE', #112125, #57514, #115319, .T. ) ;
#131033 = ORIENTED_EDGE ( 'NONE', *, *, #169238, .F. ) ;
#131032 = DIRECTION ( 'NONE',  ( -1.000000000000000000, 0.000000000000000000, 0.000000000000000000 ) ) ;
#131034 = CARTESIAN_POINT ( 'NONE',  ( -18.50000324121759121, 10.29307482169070376, -72.45864214669403225 ) ) ;
#131035 = FACE_OUTER_BOUND ( 'NONE', #208679, .T. ) ;
#131036 = FACE_OUTER_BOUND ( 'NONE', #222070, .T. ) ;
#131037 = ADVANCED_FACE ( 'NONE', ( #16256 ), #37102, .F. ) ;
#131038 = CARTESIAN_POINT ( 'NONE',  ( -22.50000000000000000, 55.96169194136206215, -232.9023299069559130 ) ) ;
#131040 = CARTESIAN_POINT ( 'NONE',  ( 20.41140022480589522, 10.41043084241237615, -108.1150013036349549 ) ) ;
#131039 = DIRECTION ( 'NONE',  ( 1.000000000000000000, -0.000000000000000000, -0.000000000000000000 ) ) ;
#131041 = DIRECTION ( 'NONE',  ( 0.000000000000000000, 0.8412123295017488456, 0.5407049257166434142 ) ) ;
#131042 = CIRCLE ( 'NONE', #201769, 0.09999999999998898659 ) ;
#131043 = DIRECTION ( 'NONE',  ( 1.000000000000000000, 7.304098846218134667E-16, -4.607487905232622991E-31 ) ) ;
#131044 = CARTESIAN_POINT ( 'NONE',  ( 21.09107601085592165, 1.537665657181535694, -230.6930743813777838 ) ) ;
#131045 = CARTESIAN_POINT ( 'NONE',  ( -16.91049119928364775, 44.10653343834928819, -235.3119000738687134 ) ) ;
#131046 = CIRCLE ( 'NONE', #51921, 11.79999999999999716 ) ;
#131047 = VERTEX_POINT ( 'NONE', #94467 ) ;
#131048 = AXIS2_PLACEMENT_3D ( 'NONE', #99723, #137572, #81442 ) ;
#131049 = EDGE_CURVE ( 'NONE', #29639, #206018, #258046, .T. ) ;
#131050 = DIRECTION ( 'NONE',  ( 0.000000000000000000, 0.1290532225515392817, 0.9916376685811522096 ) ) ;
#131051 = ORIENTED_EDGE ( 'NONE', *, *, #208423, .T. ) ;
#131052 = CARTESIAN_POINT ( 'NONE',  ( -17.11825945287481332, 51.48671849539696410, -231.8960919591225718 ) ) ;
#131053 = ORIENTED_EDGE ( 'NONE', *, *, #4620, .F. ) ;
#131054 = DIRECTION ( 'NONE',  ( -0.000000000000000000, 1.000000000000000000, -0.000000000000000000 ) ) ;
#131055 = CARTESIAN_POINT ( 'NONE',  ( 20.94999999999999929, 82.09643798151613225, -215.4278993322501208 ) ) ;
#131056 = ADVANCED_FACE ( 'NONE', ( #232726 ), #134859, .T. ) ;
#131057 = VERTEX_POINT ( 'NONE', #112764 ) ;
#131058 = EDGE_CURVE ( 'NONE', #41292, #5669, #183262, .T. ) ;
#131059 = DIRECTION ( 'NONE',  ( -1.000000000000000000, 2.952720810173289112E-16, 2.061873921506763405E-30 ) ) ;
#131060 = CIRCLE ( 'NONE', #51351, 0.09999999999999939493 ) ;
#131061 = ORIENTED_EDGE ( 'NONE', *, *, #632, .F. ) ;
#131062 = VECTOR ( 'NONE', #138289, 1000.000000000000000 ) ;
#131063 = VERTEX_POINT ( 'NONE', #194885 ) ;
#131064 = AXIS2_PLACEMENT_3D ( 'NONE', #233628, #77105, #197039 ) ;
#131065 = FACE_OUTER_BOUND ( 'NONE', #106813, .T. ) ;
#131066 = CARTESIAN_POINT ( 'NONE',  ( 21.05000000000000071, 10.72371681401022592, -41.09439923588420385 ) ) ;
#131067 = CARTESIAN_POINT ( 'NONE',  ( -18.59999999999999787, 74.16465844978787914, -158.3679561919613832 ) ) ;
#131068 = AXIS2_PLACEMENT_3D ( 'NONE', #55762, #135322, #115775 ) ;
#131069 = FACE_OUTER_BOUND ( 'NONE', #25900, .T. ) ;
#131070 = DIRECTION ( 'NONE',  ( 1.000000000000000000, 0.000000000000000000, 0.000000000000000000 ) ) ;
#131071 = ADVANCED_FACE ( 'NONE', ( #253539 ), #176607, .F. ) ;
#131073 = CARTESIAN_POINT ( 'NONE',  ( 18.58685178364170199, 85.40673308381690276, -196.3986870154365363 ) ) ;
#131072 = FACE_OUTER_BOUND ( 'NONE', #234462, .T. ) ;
#131074 = FACE_OUTER_BOUND ( 'NONE', #91131, .T. ) ;
#131076 = EDGE_LOOP ( 'NONE', ( #149596, #251184, #233053 ) ) ;
#131075 = DIRECTION ( 'NONE',  ( -2.561896900575095617E-15, -0.9901894034181603077, -0.1397316906016231042 ) ) ;
#131077 = CARTESIAN_POINT ( 'NONE',  ( -22.59999999999999787, 11.74956712350054744, -100.3991416309013260 ) ) ;
#131078 = CARTESIAN_POINT ( 'NONE',  ( -22.50000000000000000, 31.80488924422933295, -238.9605610896540213 ) ) ;
#131079 = VERTEX_POINT ( 'NONE', #76186 ) ;
#131080 = CARTESIAN_POINT ( 'NONE',  ( -18.52186455168970625, -9.481018481431632949, -174.5250164779141073 ) ) ;
#131081 = AXIS2_PLACEMENT_3D ( 'NONE', #48095, #127647, #207195 ) ;
#131082 = CARTESIAN_POINT ( 'NONE',  ( 21.04999999999908411, 8.776282895301829257, -146.1579090026525307 ) ) ;
#131083 = DIRECTION ( 'NONE',  ( 0.000000000000000000, 1.000000000000000000, 0.000000000000000000 ) ) ;
#131084 = AXIS2_PLACEMENT_3D ( 'NONE', #239596, #38833, #139175 ) ;
#131085 = ORIENTED_EDGE ( 'NONE', *, *, #205887, .F. ) ;
#131086 = CIRCLE ( 'NONE', #193636, 0.09999999999998712696 ) ;
#131087 = CARTESIAN_POINT ( 'NONE',  ( -20.94999999999999929, 76.00000000001126921, -203.5231074845248997 ) ) ;
#131088 = AXIS2_PLACEMENT_3D ( 'NONE', #152915, #212864, #116339 ) ;
#131089 = PLANE ( 'NONE',  #140095 ) ;
#131090 = DIRECTION ( 'NONE',  ( 1.000000000000000000, 7.304098846218134667E-16, -0.000000000000000000 ) ) ;
#131091 = ORIENTED_EDGE ( 'NONE', *, *, #144208, .T. ) ;
#131092 = ORIENTED_EDGE ( 'NONE', *, *, #86128, .T. ) ;
#131093 = CIRCLE ( 'NONE', #18670, 0.09999999999998898659 ) ;
#131094 = DIRECTION ( 'NONE',  ( 1.000000000000000000, -0.000000000000000000, -0.000000000000000000 ) ) ;
#131095 = VECTOR ( 'NONE', #64762, 1000.000000000000000 ) ;
#131096 = DIRECTION ( 'NONE',  ( -1.000000000000000000, -0.000000000000000000, -0.000000000000000000 ) ) ;
#131097 = CARTESIAN_POINT ( 'NONE',  ( -18.59999999999999787, 44.47083028126616000, -247.4212268238128161 ) ) ;
#131098 = CARTESIAN_POINT ( 'NONE',  ( -23.25000000000000000, 1.910280373842930812, -87.86863214480109718 ) ) ;
#131099 = ORIENTED_EDGE ( 'NONE', *, *, #194473, .F. ) ;
#131100 = CIRCLE ( 'NONE', #18675, 11.90000000000000213 ) ;
#131101 = AXIS2_PLACEMENT_3D ( 'NONE', #81787, #161381, #221315 ) ;
#131102 = CARTESIAN_POINT ( 'NONE',  ( 21.05000000000000071, 65.27628289530485972, -170.0231074845244166 ) ) ;
#131103 = DIRECTION ( 'NONE',  ( -1.000000000000000000, -0.000000000000000000, 0.000000000000000000 ) ) ;
#131104 = CARTESIAN_POINT ( 'NONE',  ( 20.12500000000000000, 9.750000000011153745, -75.11177128211431864 ) ) ;
#131105 = DIRECTION ( 'NONE',  ( 1.000000000000000000, -0.000000000000000000, -0.000000000000000000 ) ) ;
#131106 = ORIENTED_EDGE ( 'NONE', *, *, #228730, .F. ) ;
#131107 = CARTESIAN_POINT ( 'NONE',  ( 20.90851465518106167, 10.32532329026770590, -39.06993430183595706 ) ) ;
#131109 = ORIENTED_EDGE ( 'NONE', *, *, #32969, .F. ) ;
#131108 = CARTESIAN_POINT ( 'NONE',  ( -17.29838795460011625, 65.62845014205002769, -192.1278487671402786 ) ) ;
#131110 = CARTESIAN_POINT ( 'NONE',  ( 22.49436431346199683, 31.83493791481901880, -238.9466831125989756 ) ) ;
#131111 = CARTESIAN_POINT ( 'NONE',  ( -22.39999999999999858, 68.20922040163854660, -103.0231074845243739 ) ) ;
#131112 = EDGE_CURVE ( 'NONE', #97884, #39296, #77454, .T. ) ;
#131113 = LINE ( 'NONE', #30764, #217004 ) ;
#131114 = ORIENTED_EDGE ( 'NONE', *, *, #64050, .F. ) ;
#131115 = DIRECTION ( 'NONE',  ( -1.000000000000000000, 2.952720810173289112E-16, 2.061873921506763405E-30 ) ) ;
#131116 = CARTESIAN_POINT ( 'NONE',  ( -20.54999999999999716, 1.115600667400684642E-11, -87.62500000000005684 ) ) ;
#131117 = CARTESIAN_POINT ( 'NONE',  ( 20.85000000000000142, 87.65000000001190017, -103.0231074845242176 ) ) ;
#131118 = VERTEX_POINT ( 'NONE', #233982 ) ;
#131119 = DIRECTION ( 'NONE',  ( 0.000000000000000000, 0.9770955615653313941, 0.2128009952263603677 ) ) ;
#131120 = CIRCLE ( 'NONE', #118679, 0.09999999999998898659 ) ;
#131121 = DIRECTION ( 'NONE',  ( 0.000000000000000000, 0.000000000000000000, -1.000000000000000000 ) ) ;
#131123 = EDGE_CURVE ( 'NONE', #13885, #191690, #244091, .T. ) ;
#131122 = CARTESIAN_POINT ( 'NONE',  ( -20.85000000000000142, 64.35000000001214460, -136.5231074845244166 ) ) ;
#131124 = EDGE_CURVE ( 'NONE', #179546, #212939, #62472, .T. ) ;
#131126 = AXIS2_PLACEMENT_3D ( 'NONE', #239658, #220092, #20625 ) ;
#131125 = DIRECTION ( 'NONE',  ( -0.000000000000000000, -0.9770955615653316162, -0.2128009952263604232 ) ) ;
#131127 = AXIS2_PLACEMENT_3D ( 'NONE', #168799, #205284, #85323 ) ;
#131128 = CARTESIAN_POINT ( 'NONE',  ( 21.05000000000000071, 6.257814610487288043, -167.4022097086911742 ) ) ;
#131129 = DIRECTION ( 'NONE',  ( 0.000000000000000000, -0.1495327102803078179, 0.9887567792719429427 ) ) ;
#131130 = ORIENTED_EDGE ( 'NONE', *, *, #229262, .F. ) ;
#131131 = ORIENTED_EDGE ( 'NONE', *, *, #77273, .T. ) ;
#131132 = AXIS2_PLACEMENT_3D ( 'NONE', #111057, #134451, #109761 ) ;
#131133 = DIRECTION ( 'NONE',  ( -0.000000000000000000, -1.000000000000000000, 0.000000000000000000 ) ) ;
#131134 = DIRECTION ( 'NONE',  ( 0.000000000000000000, 0.8814952561688429444, -0.4721928772777345684 ) ) ;
#131135 = CIRCLE ( 'NONE', #147710, 0.09999999999999939493 ) ;
#131136 = DIRECTION ( 'NONE',  ( 0.000000000000000000, 0.000000000000000000, -1.000000000000000000 ) ) ;
#131137 = EDGE_CURVE ( 'NONE', #60014, #122058, #141310, .T. ) ;
#131138 = LINE ( 'NONE', #214518, #174498 ) ;
#131139 = LINE ( 'NONE', #110288, #218230 ) ;
#131141 = AXIS2_PLACEMENT_3D ( 'NONE', #126883, #185566, #244239 ) ;
#131140 = DIRECTION ( 'NONE',  ( 0.000000000000000000, 0.000000000000000000, -1.000000000000000000 ) ) ;
#131142 = DIRECTION ( 'NONE',  ( -1.000000000000000000, -2.808674667590276147E-16, -1.035613708381807261E-15 ) ) ;
#131143 = VECTOR ( 'NONE', #248121, 1000.000000000000000 ) ;
#131144 = LINE ( 'NONE', #172893, #103749 ) ;
#131145 = DIRECTION ( 'NONE',  ( 0.000000000000000000, 0.000000000000000000, -1.000000000000000000 ) ) ;
#131146 = ORIENTED_EDGE ( 'NONE', *, *, #155150, .F. ) ;
#131147 = DIRECTION ( 'NONE',  ( 0.000000000000000000, -0.6728971962616697722, 0.7397360091702875895 ) ) ;
#131148 = VERTEX_POINT ( 'NONE', #179184 ) ;
#131149 = EDGE_CURVE ( 'NONE', #19956, #695, #87383, .T. ) ;
#131150 = DIRECTION ( 'NONE',  ( -1.000000000000000000, 0.000000000000000000, 0.000000000000000000 ) ) ;
#131151 = EDGE_CURVE ( 'NONE', #98428, #16612, #199854, .T. ) ;
#131153 = VECTOR ( 'NONE', #153136, 1000.000000000000114 ) ;
#131152 = CARTESIAN_POINT ( 'NONE',  ( -20.64999999999999858, 73.60000000001151932, -49.24772940728643533 ) ) ;
#131154 = LINE ( 'NONE', #32085, #207288 ) ;
#131155 = CARTESIAN_POINT ( 'NONE',  ( 21.09706851349342216, 22.05831724336241351, -231.7743849847716149 ) ) ;
#131156 = CARTESIAN_POINT ( 'NONE',  ( 20.94999999999999929, 1.115600667400684642E-11, -97.60000000000005116 ) ) ;
#131157 = LINE ( 'NONE', #138519, #255820 ) ;
#131158 = EDGE_LOOP ( 'NONE', ( #35301, #63636, #248716 ) ) ;
#131159 = DIRECTION ( 'NONE',  ( 0.000000000000000000, 0.1350103645451876666, -0.9908441862701600211 ) ) ;
#131160 = FACE_OUTER_BOUND ( 'NONE', #1394, .T. ) ;
#131161 = DIRECTION ( 'NONE',  ( 0.000000000000000000, 0.000000000000000000, 1.000000000000000000 ) ) ;
#131163 = EDGE_CURVE ( 'NONE', #8515, #109777, #22674, .T. ) ;
#131162 = FACE_OUTER_BOUND ( 'NONE', #116012, .T. ) ;
#131164 = CARTESIAN_POINT ( 'NONE',  ( 21.05000000000000071, 60.06173988932783203, -221.3217724115915814 ) ) ;
#131165 = CIRCLE ( 'NONE', #181270, 0.09999999999999939493 ) ;
#131166 = AXIS2_PLACEMENT_3D ( 'NONE', #110963, #245350, #225754 ) ;
#131167 = EDGE_LOOP ( 'NONE', ( #139264, #20465, #40087, #60881 ) ) ;
#131168 = CARTESIAN_POINT ( 'NONE',  ( -20.54999999999999716, 29.14863708059993286, -237.4168895852561434 ) ) ;
#131169 = DIRECTION ( 'NONE',  ( 7.589415207398576792E-15, -1.000000000000000000, -0.000000000000000000 ) ) ;
#131170 = ORIENTED_EDGE ( 'NONE', *, *, #185900, .T. ) ;
#131171 = ORIENTED_EDGE ( 'NONE', *, *, #35396, .F. ) ;
#131172 = DIRECTION ( 'NONE',  ( 0.000000000000000000, 0.000000000000000000, -1.000000000000000000 ) ) ;
#131173 = CARTESIAN_POINT ( 'NONE',  ( 21.05000000000000782, 11.25362009860280921, -210.9838939269090474 ) ) ;
#131174 = EDGE_CURVE ( 'NONE', #215885, #206475, #249891, .T. ) ;
#131175 = ORIENTED_EDGE ( 'NONE', *, *, #38248, .F. ) ;
#131176 = CARTESIAN_POINT ( 'NONE',  ( 18.47135592147663274, -9.471088613254405431, -174.1835949398439993 ) ) ;
#131177 = CARTESIAN_POINT ( 'NONE',  ( 20.94999999999999929, 8.926614585098253229, -41.97168301922312850 ) ) ;
#131178 = ORIENTED_EDGE ( 'NONE', *, *, #180528, .F. ) ;
#131179 = CIRCLE ( 'NONE', #22884, 0.5000000000000013323 ) ;
#131180 = CARTESIAN_POINT ( 'NONE',  ( -23.15000000000000213, 2.000000000011154189, -53.77537807723790309 ) ) ;
#131181 = ADVANCED_FACE ( 'NONE', ( #160894 ), #241694, .F. ) ;
#131182 = EDGE_LOOP ( 'NONE', ( #207986, #211909, #220757, #52710 ) ) ;
#131183 = CARTESIAN_POINT ( 'NONE',  ( -21.05000000000000071, 11.75000000001115552, -160.4851942293460638 ) ) ;
#131184 = DIRECTION ( 'NONE',  ( 0.000000000000000000, 0.000000000000000000, 1.000000000000000000 ) ) ;
#131186 = EDGE_LOOP ( 'NONE', ( #155548, #165827, #19634, #190403 ) ) ;
#131185 = CARTESIAN_POINT ( 'NONE',  ( -18.59999999999999787, -14.35849056603774976, -0.4952830188679671064 ) ) ;
#131187 = FACE_OUTER_BOUND ( 'NONE', #38246, .T. ) ;
#131189 = UNCERTAINTY_MEASURE_WITH_UNIT (LENGTH_MEASURE( 1.000000000000000082E-05 ), #9804, 'distance_accuracy_value', 'NONE');
#131188 = CARTESIAN_POINT ( 'NONE',  ( 18.59999999999999787, 77.25000000001209344, -128.7226267301092548 ) ) ;
#131190 = EDGE_CURVE ( 'NONE', #195194, #60391, #8303, .T. ) ;
#131192 = EDGE_CURVE ( 'NONE', #67383, #194499, #240416, .T. ) ;
#131191 = CARTESIAN_POINT ( 'NONE',  ( -20.94999027547553894, 65.70673848566998743, -131.0638252334829588 ) ) ;
#131193 = CARTESIAN_POINT ( 'NONE',  ( -18.50000000000000000, 66.65000000001205649, -124.1731074845243654 ) ) ;
#131194 = FACE_OUTER_BOUND ( 'NONE', #201214, .T. ) ;
#131195 = SPHERICAL_SURFACE ( 'NONE', #142727, 0.1000000000000000056 ) ;
#131196 = DIRECTION ( 'NONE',  ( 1.000000000000000000, 0.000000000000000000, 0.000000000000000000 ) ) ;
#131198 = ORIENTED_EDGE ( 'NONE', *, *, #245112, .F. ) ;
#131197 = DIRECTION ( 'NONE',  ( 0.000000000000000000, -0.9654727137038715545, -0.2605042016806676242 ) ) ;
#131199 = ORIENTED_EDGE ( 'NONE', *, *, #212941, .F. ) ;
#131201 = CARTESIAN_POINT ( 'NONE',  ( -18.39999999999999858, 58.58048437606812087, -223.8992190685246157 ) ) ;
#131200 = DIRECTION ( 'NONE',  ( 0.000000000000000000, 0.000000000000000000, 1.000000000000000000 ) ) ;
#131203 = ORIENTED_EDGE ( 'NONE', *, *, #76413, .F. ) ;
#131202 = FACE_OUTER_BOUND ( 'NONE', #136425, .T. ) ;
#131204 = VERTEX_POINT ( 'NONE', #121771 ) ;
#131205 = CARTESIAN_POINT ( 'NONE',  ( -18.39999999999999858, 77.17949092533254429, -241.9177572069595783 ) ) ;
#131206 = DIRECTION ( 'NONE',  ( 0.000000000000000000, 0.8753622295931610120, -0.4834676483506316624 ) ) ;
#131208 = EDGE_CURVE ( 'NONE', #143461, #109066, #241524, .T. ) ;
#131207 = ADVANCED_FACE ( 'NONE', ( #3062 ), #49975, .T. ) ;
#131209 = AXIS2_PLACEMENT_3D ( 'NONE', #53946, #151796, #154380 ) ;
#131210 = VECTOR ( 'NONE', #39083, 1000.000000000000000 ) ;
#131211 = EDGE_CURVE ( 'NONE', #141892, #162009, #63044, .T. ) ;
#131212 = DIRECTION ( 'NONE',  ( 2.952720810173289112E-16, 1.000000000000000000, 6.982962677686266711E-15 ) ) ;
#131213 = CARTESIAN_POINT ( 'NONE',  ( 20.00000000000000355, 11.75000000001116263, -58.14999999999999858 ) ) ;
#131214 = CARTESIAN_POINT ( 'NONE',  ( -18.56579813702275672, 67.49234744263520724, -195.4268335588911327 ) ) ;
#131215 = EDGE_CURVE ( 'NONE', #196436, #204472, #83857, .T. ) ;
#131216 = DIRECTION ( 'NONE',  ( 0.000000000000000000, -0.9770955615653313941, -0.2128009952263603677 ) ) ;
#131218 = ORIENTED_EDGE ( 'NONE', *, *, #204945, .F. ) ;
#131217 = EDGE_CURVE ( 'NONE', #129010, #209135, #145143, .T. ) ;
#131219 = ORIENTED_EDGE ( 'NONE', *, *, #98216, .T. ) ;
#131220 = CARTESIAN_POINT ( 'NONE',  ( -23.15000000000000213, 1.115626384983466744E-11, -64.90000000000000568 ) ) ;
#131221 = VECTOR ( 'NONE', #136374, 1000.000000000000114 ) ;
#131222 = CIRCLE ( 'NONE', #227085, 0.09999999999999469036 ) ;
#131223 = ORIENTED_EDGE ( 'NONE', *, *, #51546, .F. ) ;
#131224 = EDGE_CURVE ( 'NONE', #23701, #255533, #64349, .T. ) ;
#131225 = CARTESIAN_POINT ( 'NONE',  ( 19.97071067811864609, 64.27928932189283273, -44.77310748452440237 ) ) ;
#131227 = EDGE_CURVE ( 'NONE', #14506, #131663, #143864, .T. ) ;
#131226 = EDGE_LOOP ( 'NONE', ( #67448, #114197, #248197, #153675 ) ) ;
#131228 = CARTESIAN_POINT ( 'NONE',  ( -21.65000000000000213, 7.708578643773852157, -155.1500000000000057 ) ) ;
#131229 = AXIS2_PLACEMENT_3D ( 'NONE', #47678, #25582, #245910 ) ;
#131230 = VECTOR ( 'NONE', #50050, 1000.000000000000000 ) ;
#131231 = CYLINDRICAL_SURFACE ( 'NONE', #26206, 0.09999999999999935330 ) ;
#131232 =( GEOMETRIC_REPRESENTATION_CONTEXT ( 3 ) GLOBAL_UNCERTAINTY_ASSIGNED_CONTEXT ( ( #225138 ) ) GLOBAL_UNIT_ASSIGNED_CONTEXT ( ( #185556, #129436, #30352 ) ) REPRESENTATION_CONTEXT ( 'NONE', 'WORKASPACE' ) );
#131233 = EDGE_CURVE ( 'NONE', #69371, #217944, #149965, .T. ) ;
#131234 = LINE ( 'NONE', #89529, #248147 ) ;
#131235 = EDGE_LOOP ( 'NONE', ( #206156, #192786, #185590 ) ) ;
#131236 = LINE ( 'NONE', #253738, #204683 ) ;
#131237 = VERTEX_POINT ( 'NONE', #120495 ) ;
#131238 = EDGE_CURVE ( 'NONE', #51100, #94008, #85148, .T. ) ;
#131239 = CARTESIAN_POINT ( 'NONE',  ( 18.59999999999999787, 74.95904887477786360, -233.7774272632847783 ) ) ;
#131240 = ADVANCED_FACE ( 'NONE', ( #244245 ), #39673, .T. ) ;
#131241 = CARTESIAN_POINT ( 'NONE',  ( -20.85000000000000142, 67.32498692201720303, -236.1680459564915679 ) ) ;
#131243 = VERTEX_POINT ( 'NONE', #70793 ) ;
#131242 = EDGE_CURVE ( 'NONE', #205304, #111888, #169914, .T. ) ;
#131244 = CARTESIAN_POINT ( 'NONE',  ( -21.05000000000000071, 1.261786168576181755, -108.5864989635455089 ) ) ;
#131245 = ORIENTED_EDGE ( 'NONE', *, *, #50223, .T. ) ;
#131247 = ORIENTED_EDGE ( 'NONE', *, *, #54820, .T. ) ;
#131246 = DIRECTION ( 'NONE',  ( 0.000000000000000000, 0.000000000000000000, -1.000000000000000000 ) ) ;
#131248 = CARTESIAN_POINT ( 'NONE',  ( -20.15000000000000568, 66.70857864377468616, -115.2731074845243597 ) ) ;
#131250 = ORIENTED_EDGE ( 'NONE', *, *, #96677, .F. ) ;
#131249 = AXIS2_PLACEMENT_3D ( 'NONE', #177167, #237110, #19346 ) ;
#131251 = CIRCLE ( 'NONE', #226937, 0.09999999999998898659 ) ;
#131252 = ORIENTED_EDGE ( 'NONE', *, *, #184548, .T. ) ;
#131253 = CIRCLE ( 'NONE', #102003, 12.77500000000000924 ) ;
#131254 = DIRECTION ( 'NONE',  ( 0.000000000000000000, -6.547589603894034005E-15, 1.000000000000000000 ) ) ;
#131255 = ORIENTED_EDGE ( 'NONE', *, *, #218296, .F. ) ;
#131256 = EDGE_CURVE ( 'NONE', #109697, #43253, #168637, .T. ) ;
#131257 = CARTESIAN_POINT ( 'NONE',  ( 21.05000000000000071, 18.71171618620643429, -229.8673829423568691 ) ) ;
#131258 = FACE_OUTER_BOUND ( 'NONE', #162033, .T. ) ;
#131259 = ADVANCED_FACE ( 'NONE', ( #111180 ), #29116, .T. ) ;
#131260 = CARTESIAN_POINT ( 'NONE',  ( 18.53317502108576420, 67.49276774653023381, -195.4544018784149841 ) ) ;
#131261 = TOROIDAL_SURFACE ( 'NONE', #102018, 7.800000000000000711, 0.1000000000000000056 ) ;
#131262 = CIRCLE ( 'NONE', #68730, 12.87499999999999289 ) ;
#131263 = ORIENTED_EDGE ( 'NONE', *, *, #155308, .F. ) ;
#131264 = CARTESIAN_POINT ( 'NONE',  ( -20.94999999999999574, 62.98661795304985844, -207.1103002134591122 ) ) ;
#131265 = CARTESIAN_POINT ( 'NONE',  ( 18.41416235934319090, 86.89640087696875526, -199.6396878666313626 ) ) ;
#131266 = CARTESIAN_POINT ( 'NONE',  ( 21.14999999999999858, 6.540656951712400691, -33.50000000000000000 ) ) ;
#131267 = EDGE_LOOP ( 'NONE', ( #4707, #77070, #151515, #56093 ) ) ;
#131268 = DIRECTION ( 'NONE',  ( 0.000000000000000000, 0.000000000000000000, 1.000000000000000000 ) ) ;
#131269 = ORIENTED_EDGE ( 'NONE', *, *, #227642, .T. ) ;
#131270 = DIRECTION ( 'NONE',  ( 0.000000000000000000, -6.982962677686266711E-15, 1.000000000000000000 ) ) ;
#131271 = ORIENTED_EDGE ( 'NONE', *, *, #165739, .F. ) ;
#131272 = VECTOR ( 'NONE', #13593, 1000.000000000000000 ) ;
#131273 = AXIS2_PLACEMENT_3D ( 'NONE', #75974, #56389, #13441 ) ;
#131274 = LINE ( 'NONE', #53013, #80290 ) ;
#131275 = DIRECTION ( 'NONE',  ( -1.000000000000000000, 0.000000000000000000, 0.000000000000000000 ) ) ;
#131277 = EDGE_LOOP ( 'NONE', ( #49967, #154097, #197469, #214444 ) ) ;
#131276 = CARTESIAN_POINT ( 'NONE',  ( 21.05000000000000071, -11.74999999998883560, -131.1000000000000227 ) ) ;
#131278 = CARTESIAN_POINT ( 'NONE',  ( -20.54999999999999716, 74.05981308412400210, -90.19398827347099257 ) ) ;
#131279 = ORIENTED_EDGE ( 'NONE', *, *, #213195, .F. ) ;
#131280 = AXIS2_PLACEMENT_3D ( 'NONE', #200878, #22262, #23572 ) ;
#131281 = CIRCLE ( 'NONE', #164615, 14.20833333333333748 ) ;
#131282 = LINE ( 'NONE', #234222, #2649 ) ;
#131283 = CARTESIAN_POINT ( 'NONE',  ( -16.88783316861809780, 9.950000000011137047, -113.2522640419798279 ) ) ;
#131284 = ORIENTED_EDGE ( 'NONE', *, *, #242103, .F. ) ;
#131285 = EDGE_CURVE ( 'NONE', #163114, #76314, #190745, .T. ) ;
#131286 = DIRECTION ( 'NONE',  ( 0.000000000000000000, 0.000000000000000000, -1.000000000000000000 ) ) ;
#131287 = LINE ( 'NONE', #13921, #127412 ) ;
#131288 = VERTEX_POINT ( 'NONE', #109873 ) ;
#131289 = CARTESIAN_POINT ( 'NONE',  ( -16.93339986808596365, 10.00510392857707487, -146.5659936718128904 ) ) ;
#131290 = EDGE_CURVE ( 'NONE', #82665, #167448, #112356, .T. ) ;
#131291 = ORIENTED_EDGE ( 'NONE', *, *, #215702, .T. ) ;
#131292 = DIRECTION ( 'NONE',  ( -0.000000000000000000, -0.4721928772777346239, -0.8814952561688430555 ) ) ;
#131293 = CARTESIAN_POINT ( 'NONE',  ( 22.48660254037844197, 11.65000000001116298, -167.4499999999999602 ) ) ;
#131296 = EDGE_LOOP ( 'NONE', ( #179723, #22914, #62623, #154343 ) ) ;
#131295 = ORIENTED_EDGE ( 'NONE', *, *, #158306, .T. ) ;
#131294 = DIRECTION ( 'NONE',  ( 1.000000000000000000, 0.000000000000000000, -0.000000000000000000 ) ) ;
#131297 = CARTESIAN_POINT ( 'NONE',  ( 21.87500000000000355, 9.750000000011153745, -188.6499999999999488 ) ) ;
#131298 = LINE ( 'NONE', #137699, #219114 ) ;
#131299 = AXIS2_PLACEMENT_3D ( 'NONE', #167532, #163658, #85361 ) ;
#131300 = CARTESIAN_POINT ( 'NONE',  ( -20.94999999999999929, 77.16270174994961906, -61.62310748452431142 ) ) ;
#131302 = LINE ( 'NONE', #231709, #37981 ) ;
#131301 = DIRECTION ( 'NONE',  ( -0.000000000000000000, 1.000000000000000000, 6.982962677686267499E-15 ) ) ;
#131304 = EDGE_CURVE ( 'NONE', #207105, #198340, #175116, .T. ) ;
#131303 = CARTESIAN_POINT ( 'NONE',  ( -23.25000000000000000, 2.272311100394799332, -217.9150152700588592 ) ) ;
#131305 = AXIS2_PLACEMENT_3D ( 'NONE', #164601, #85020, #163317 ) ;
#131306 = FACE_OUTER_BOUND ( 'NONE', #98969, .T. ) ;
#131307 = FACE_OUTER_BOUND ( 'NONE', #145264, .T. ) ;
#131308 = DIRECTION ( 'NONE',  ( -1.000000000000000000, 0.000000000000000000, 0.000000000000000000 ) ) ;
#131309 = ORIENTED_EDGE ( 'NONE', *, *, #95989, .F. ) ;
#131311 = ORIENTED_EDGE ( 'NONE', *, *, #84950, .T. ) ;
#131310 = AXIS2_PLACEMENT_3D ( 'NONE', #1363, #237431, #40555 ) ;
#131312 = CARTESIAN_POINT ( 'NONE',  ( 18.49999999999998934, 56.14960075277809182, -67.24280442672311153 ) ) ;
#131313 = CIRCLE ( 'NONE', #106348, 0.09999999999998898659 ) ;
#131315 = ORIENTED_EDGE ( 'NONE', *, *, #109099, .T. ) ;
#131314 = CARTESIAN_POINT ( 'NONE',  ( 22.39999999999999503, 31.89597452117651244, -238.9192857152811484 ) ) ;
#131316 = ORIENTED_EDGE ( 'NONE', *, *, #6288, .T. ) ;
#131317 = DIRECTION ( 'NONE',  ( 1.000000000000000000, 0.000000000000000000, 0.000000000000000000 ) ) ;
#131318 = ORIENTED_EDGE ( 'NONE', *, *, #47806, .T. ) ;
#131319 = DIRECTION ( 'NONE',  ( 0.000000000000000000, 0.8814952561688444987, -0.4721928772777320149 ) ) ;
#131320 = VECTOR ( 'NONE', #61735, 1000.000000000000000 ) ;
#131321 = AXIS2_PLACEMENT_3D ( 'NONE', #248781, #209644, #225331 ) ;
#131322 = ORIENTED_EDGE ( 'NONE', *, *, #107833, .T. ) ;
#131323 = CIRCLE ( 'NONE', #214709, 0.2000000000000057288 ) ;
#131324 = DIRECTION ( 'NONE',  ( -1.000000000000000000, 0.000000000000000000, 0.000000000000000000 ) ) ;
#131325 = DIRECTION ( 'NONE',  ( -0.000000000000000000, 0.1350103645451649625, -0.9908441862701631297 ) ) ;
#131327 = VERTEX_POINT ( 'NONE', #27820 ) ;
#131326 = ORIENTED_EDGE ( 'NONE', *, *, #116503, .T. ) ;
#131328 = ORIENTED_EDGE ( 'NONE', *, *, #226265, .T. ) ;
#131329 = EDGE_LOOP ( 'NONE', ( #13229, #160472, #121174, #255973, #220129 ) ) ;
#131330 = ORIENTED_EDGE ( 'NONE', *, *, #13951, .T. ) ;
#131331 = CARTESIAN_POINT ( 'NONE',  ( 20.84999999999999787, 11.75000000000000355, -26.58085275404129888 ) ) ;
#131332 = CARTESIAN_POINT ( 'NONE',  ( 21.14999999999999858, 43.45833571831320796, -234.7657887233443716 ) ) ;
#131333 = CARTESIAN_POINT ( 'NONE',  ( -12.25000000000000178, 9.350000000011139178, -184.2499999999999716 ) ) ;
#131335 = ORIENTED_EDGE ( 'NONE', *, *, #145404, .F. ) ;
#131334 = CARTESIAN_POINT ( 'NONE',  ( -20.64999999999999858, -9.499999999988846255, -124.1060308773475924 ) ) ;
#131336 = DIRECTION ( 'NONE',  ( -3.469446951953605354E-14, 1.000000000000000000, 0.000000000000000000 ) ) ;
#131337 = CARTESIAN_POINT ( 'NONE',  ( -20.64999999999999858, 4.350000000011156054, -155.1500000000000057 ) ) ;
#131339 = VERTEX_POINT ( 'NONE', #30371 ) ;
#131338 = CARTESIAN_POINT ( 'NONE',  ( -16.92132318717937522, 60.91662537786660181, -221.0641526825682490 ) ) ;
#131340 = CARTESIAN_POINT ( 'NONE',  ( -23.15000000000000213, 51.38014393322265505, -230.1906178717505611 ) ) ;
#131341 = VERTEX_POINT ( 'NONE', #249413 ) ;
#131342 = LINE ( 'NONE', #214727, #141074 ) ;
#131343 = EDGE_CURVE ( 'NONE', #105461, #42156, #150315, .T. ) ;
#131344 = ORIENTED_EDGE ( 'NONE', *, *, #197839, .F. ) ;
#131345 = DIRECTION ( 'NONE',  ( 1.000000000000000000, 0.000000000000000000, 0.000000000000000000 ) ) ;
#131346 = DIRECTION ( 'NONE',  ( 0.000000000000000000, 0.000000000000000000, 1.000000000000000000 ) ) ;
#131347 = EDGE_CURVE ( 'NONE', #182252, #56847, #227260, .T. ) ;
#131348 = ORIENTED_EDGE ( 'NONE', *, *, #15828, .F. ) ;
#131350 = CARTESIAN_POINT ( 'NONE',  ( -18.42637059832564006, -9.496945461878548045, -140.6090773097999147 ) ) ;
#131349 = CARTESIAN_POINT ( 'NONE',  ( -18.59999999999999787, 64.35000000001259934, -191.3731074845244393 ) ) ;
#131351 = CARTESIAN_POINT ( 'NONE',  ( -18.50000000000000000, 77.16412189325286874, -61.80825939895269272 ) ) ;
#131352 = CIRCLE ( 'NONE', #214738, 0.1000000000000028644 ) ;
#131353 = SPHERICAL_SURFACE ( 'NONE', #213923, 0.1000000000000000056 ) ;
#131354 = TOROIDAL_SURFACE ( 'NONE', #235395, 0.2000000000000000111, 0.1000000000000000056 ) ;
#131355 = DIRECTION ( 'NONE',  ( 0.000000000000000000, 6.982962677686266711E-15, -1.000000000000000000 ) ) ;
#131356 = ORIENTED_EDGE ( 'NONE', *, *, #197187, .T. ) ;
#131357 = ORIENTED_EDGE ( 'NONE', *, *, #50112, .T. ) ;
#131358 = EDGE_CURVE ( 'NONE', #9091, #37194, #171028, .T. ) ;
#131359 = SPHERICAL_SURFACE ( 'NONE', #80430, 0.1000000000000000056 ) ;
#131360 = CARTESIAN_POINT ( 'NONE',  ( 18.49999999999999645, 77.16270174995034381, -161.9231074845243370 ) ) ;
#131361 = ORIENTED_EDGE ( 'NONE', *, *, #167570, .F. ) ;
#131362 = CYLINDRICAL_SURFACE ( 'NONE', #114192, 0.09999999999999939493 ) ;
#131363 = ORIENTED_EDGE ( 'NONE', *, *, #115016, .F. ) ;
#131364 = CARTESIAN_POINT ( 'NONE',  ( -22.39999999999999858, 68.20922040163897293, -170.0231074845243882 ) ) ;
#131365 = DIRECTION ( 'NONE',  ( 0.000000000000000000, -0.8700118002898321601, 0.4930308989875230030 ) ) ;
#131366 = ADVANCED_FACE ( 'NONE', ( #48623 ), #12101, .F. ) ;
#131367 = DIRECTION ( 'NONE',  ( 0.000000000000000000, -7.147358527629766941E-15, 1.000000000000000000 ) ) ;
#131368 = ORIENTED_EDGE ( 'NONE', *, *, #125863, .T. ) ;
#131369 = ADVANCED_FACE ( 'NONE', ( #86437 ), #235984, .T. ) ;
#131370 = DIRECTION ( 'NONE',  ( -1.000000000000000000, 0.000000000000000000, -0.000000000000000000 ) ) ;
#131371 = CIRCLE ( 'NONE', #143831, 14.30833333333334245 ) ;
#131372 = ORIENTED_EDGE ( 'NONE', *, *, #66446, .T. ) ;
#131373 = ORIENTED_EDGE ( 'NONE', *, *, #12537, .F. ) ;
#131374 = VERTEX_POINT ( 'NONE', #132019 ) ;
#131375 = DIRECTION ( 'NONE',  ( 0.000000000000000000, -0.000000000000000000, 1.000000000000000000 ) ) ;
#131376 = CARTESIAN_POINT ( 'NONE',  ( 12.25000000000000178, 66.65000000001154490, -53.00158811269929515 ) ) ;
#131377 = CIRCLE ( 'NONE', #123189, 12.97499999999999964 ) ;
#131378 = CARTESIAN_POINT ( 'NONE',  ( -21.11927991906891222, 0.009083679485028296058, -127.5515068815085158 ) ) ;
#131379 = DIRECTION ( 'NONE',  ( 0.000000000000000000, 0.000000000000000000, -1.000000000000000000 ) ) ;
#131380 = DIRECTION ( 'NONE',  ( 0.000000000000000000, 1.000000000000000000, 0.000000000000000000 ) ) ;
#131381 = EDGE_CURVE ( 'NONE', #16167, #245180, #145835, .T. ) ;
#131383 = FACE_OUTER_BOUND ( 'NONE', #127364, .T. ) ;
#131382 = DIRECTION ( 'NONE',  ( 0.000000000000000000, -0.2128009952263605065, 0.9770955615653315052 ) ) ;
#131384 = ORIENTED_EDGE ( 'NONE', *, *, #186560, .T. ) ;
#131385 = DIRECTION ( 'NONE',  ( 0.000000000000000000, 1.000000000000000000, 0.000000000000000000 ) ) ;
#131386 = ORIENTED_EDGE ( 'NONE', *, *, #96901, .F. ) ;
#131387 = CARTESIAN_POINT ( 'NONE',  ( -12.93407622233968368, 9.417789466963366607, -149.3573845439769343 ) ) ;
#131388 = ORIENTED_EDGE ( 'NONE', *, *, #7963, .T. ) ;
#131389 = ORIENTED_EDGE ( 'NONE', *, *, #112576, .F. ) ;
#131390 = CARTESIAN_POINT ( 'NONE',  ( -16.93521499325732549, 66.00521388020798952, -48.61599894343083861 ) ) ;
#131391 = CARTESIAN_POINT ( 'NONE',  ( -18.59999999999999787, 1.162701749949165642, -175.5999999999999659 ) ) ;
#131392 = LINE ( 'NONE', #148404, #141826 ) ;
#131393 = DIRECTION ( 'NONE',  ( 0.000000000000000000, 6.982962677686266711E-15, -1.000000000000000000 ) ) ;
#131394 = AXIS2_PLACEMENT_3D ( 'NONE', #236790, #2023, #38610 ) ;
#131395 = MECHANICAL_DESIGN_GEOMETRIC_PRESENTATION_REPRESENTATION (  '', ( #85560 ), #164720 ) ;
#131396 = CARTESIAN_POINT ( 'NONE',  ( 20.94999999999999929, 76.00000000001170974, -69.52310748452431710 ) ) ;
#131397 = ORIENTED_EDGE ( 'NONE', *, *, #194001, .T. ) ;
#131398 = ORIENTED_EDGE ( 'NONE', *, *, #141405, .F. ) ;
#131399 = DIRECTION ( 'NONE',  ( 0.000000000000000000, -1.000000000000000000, 0.000000000000000000 ) ) ;
#131400 = VERTEX_POINT ( 'NONE', #156753 ) ;
#131401 = CARTESIAN_POINT ( 'NONE',  ( -18.59999999999999787, -1.162701749926853712, -142.0000000000000284 ) ) ;
#131402 = VERTEX_POINT ( 'NONE', #251964 ) ;
#131403 = DIRECTION ( 'NONE',  ( -3.890533409366484652E-14, 0.9579639084728162057, 0.2868887416115976086 ) ) ;
#131404 = PLANE ( 'NONE',  #208762 ) ;
#131405 = DIRECTION ( 'NONE',  ( 0.000000000000000000, 0.2128009952263604787, -0.9770955615653315052 ) ) ;
#131406 = CYLINDRICAL_SURFACE ( 'NONE', #142501, 0.1000000000000055844 ) ;
#131407 = ORIENTED_EDGE ( 'NONE', *, *, #149346, .T. ) ;
#131408 = CARTESIAN_POINT ( 'NONE',  ( -23.15000000000000213, 64.35000000001205933, -124.3731074845243825 ) ) ;
#131409 = DIRECTION ( 'NONE',  ( -1.000000000000000000, 0.000000000000000000, 0.000000000000000000 ) ) ;
#131410 = DIRECTION ( 'NONE',  ( -0.000000000000000000, 0.1298341882520009927, 0.9915357197604854900 ) ) ;
#131411 = DIRECTION ( 'NONE',  ( 0.000000000000000000, -1.000000000000000000, 0.000000000000000000 ) ) ;
#131412 = DIRECTION ( 'NONE',  ( 0.000000000000000000, -0.4721928772777356231, -0.8814952561688425003 ) ) ;
#131413 = VECTOR ( 'NONE', #51402, 1000.000000000000000 ) ;
#131414 = DIRECTION ( 'NONE',  ( 0.000000000000000000, 6.982962677686266711E-15, -1.000000000000000000 ) ) ;
#131415 = AXIS2_PLACEMENT_3D ( 'NONE', #140503, #220062, #120989 ) ;
#131416 = VECTOR ( 'NONE', #14717, 999.9999999999998863 ) ;
#131417 = AXIS2_PLACEMENT_3D ( 'NONE', #236161, #216598, #197019 ) ;
#131418 = EDGE_CURVE ( 'NONE', #141019, #113112, #154204, .T. ) ;
#131419 = ORIENTED_EDGE ( 'NONE', *, *, #144102, .F. ) ;
#131420 = COLOUR_RGB ( '', 0.40784314, 0.44705882, 0.49803922) ;
#131421 = CARTESIAN_POINT ( 'NONE',  ( 21.05000000000000071, -0.09999999998884338825, -160.9593430482987344 ) ) ;
#131422 = VERTEX_POINT ( 'NONE', #254507 ) ;
#131423 = CARTESIAN_POINT ( 'NONE',  ( 15.39793903038208001, 66.61031399435661626, -154.3502639781730750 ) ) ;
#131424 = EDGE_CURVE ( 'NONE', #1104, #124170, #52462, .T. ) ;
#131425 = FACE_OUTER_BOUND ( 'NONE', #111776, .T. ) ;
#131426 = DIRECTION ( 'NONE',  ( 0.000000000000000000, 0.8660254037844378194, 0.5000000000000016653 ) ) ;
#131427 = CARTESIAN_POINT ( 'NONE',  ( -18.59999999999999787, 77.16412189325360771, -162.1082593989527254 ) ) ;
#131428 = CARTESIAN_POINT ( 'NONE',  ( 21.14999999999999503, -0.1008583690875562017, -122.2504328765106294 ) ) ;
#131429 = ORIENTED_EDGE ( 'NONE', *, *, #216702, .F. ) ;
#131430 = DIRECTION ( 'NONE',  ( 0.000000000000000000, -0.8777080977375715243, 0.4791956752370512551 ) ) ;
#131431 = CARTESIAN_POINT ( 'NONE',  ( 21.12802099929860944, 67.21944740978983646, -124.2749174995927461 ) ) ;
#131432 = EDGE_CURVE ( 'NONE', #167581, #20467, #187572, .T. ) ;
#131433 = ADVANCED_FACE ( 'NONE', ( #134565 ), #177603, .F. ) ;
#131434 = LINE ( 'NONE', #54462, #239737 ) ;
#131435 = DIRECTION ( 'NONE',  ( 0.000000000000000000, 0.4930308989875230585, 0.8700118002898322711 ) ) ;
#131436 = AXIS2_PLACEMENT_3D ( 'NONE', #98514, #62021, #155997 ) ;
#131437 = B_SPLINE_CURVE_WITH_KNOTS ( 'NONE', 3,
 ( #89830, #87258, #108131, #186398, #187687, #188951, #7753, #9028, #110692, #70318 ),
 .UNSPECIFIED., .F., .F.,
 ( 4, 3, 3, 4 ),
 ( 1.886399917053072492E-15, 3.877043166999333273E-05, 7.336897548476527698E-05, 7.659383120239750958E-05 ),
 .UNSPECIFIED. ) ;
#131438 = CARTESIAN_POINT ( 'NONE',  ( -20.94999999999999929, -11.48912529306490349, -170.3999999999999773 ) ) ;
#131439 =( GEOMETRIC_REPRESENTATION_CONTEXT ( 3 ) GLOBAL_UNCERTAINTY_ASSIGNED_CONTEXT ( ( #50349 ) ) GLOBAL_UNIT_ASSIGNED_CONTEXT ( ( #161166, #159896, #101126 ) ) REPRESENTATION_CONTEXT ( 'NONE', 'WORKASPACE' ) );
#131440 = AXIS2_PLACEMENT_3D ( 'NONE', #130255, #235774, #196645 ) ;
#131441 = VERTEX_POINT ( 'NONE', #17230 ) ;
#131442 = ORIENTED_EDGE ( 'NONE', *, *, #251710, .T. ) ;
#131443 = DIRECTION ( 'NONE',  ( -1.000000000000000000, 7.304098846218134667E-16, 4.217023435051625732E-16 ) ) ;
#131444 = DIRECTION ( 'NONE',  ( -3.469446951953515108E-14, 1.000000000000000000, 0.000000000000000000 ) ) ;
#131445 = DIRECTION ( 'NONE',  ( 0.000000000000000000, -0.9908441862701596881, -0.1350103645451904977 ) ) ;
#131446 = LINE ( 'NONE', #194011, #93034 ) ;
#131447 = FACE_OUTER_BOUND ( 'NONE', #163999, .T. ) ;
#131448 = AXIS2_PLACEMENT_3D ( 'NONE', #13486, #250794, #173883 ) ;
#131449 = EDGE_CURVE ( 'NONE', #140899, #91127, #58521, .T. ) ;
#131450 = ORIENTED_EDGE ( 'NONE', *, *, #74924, .T. ) ;
#131451 = CYLINDRICAL_SURFACE ( 'NONE', #134670, 4.049999999999998046 ) ;
#131452 = AXIS2_PLACEMENT_3D ( 'NONE', #14491, #213947, #256870 ) ;
#131453 = EDGE_CURVE ( 'NONE', #198318, #43558, #255778, .T. ) ;
#131454 = CIRCLE ( 'NONE', #247972, 0.1000000000000000472 ) ;
#131455 = CARTESIAN_POINT ( 'NONE',  ( 20.94999999999999929, -11.64999999998883595, -64.10000000000000853 ) ) ;
#131456 = VERTEX_POINT ( 'NONE', #14674 ) ;
#131457 = LINE ( 'NONE', #171909, #179735 ) ;
#131458 = AXIS2_PLACEMENT_3D ( 'NONE', #143144, #107886, #222681 ) ;
#131459 = VERTEX_POINT ( 'NONE', #192018 ) ;
#131461 = VERTEX_POINT ( 'NONE', #13366 ) ;
#131460 = CIRCLE ( 'NONE', #152530, 0.2000000000000118627 ) ;
#131462 = EDGE_CURVE ( 'NONE', #175543, #109393, #36811, .T. ) ;
#131463 = ORIENTED_EDGE ( 'NONE', *, *, #256841, .F. ) ;
#131464 = EDGE_CURVE ( 'NONE', #129700, #36910, #12783, .T. ) ;
#131465 = CARTESIAN_POINT ( 'NONE',  ( 23.24999999999999645, 1.115600667400684642E-11, -67.00000000000004263 ) ) ;
#131466 = ADVANCED_FACE ( 'NONE', ( #116328 ), #117594, .T. ) ;
#131467 = AXIS2_PLACEMENT_3D ( 'NONE', #48402, #147514, #49696 ) ;
#131468 = FACE_OUTER_BOUND ( 'NONE', #79741, .T. ) ;
#131469 = CARTESIAN_POINT ( 'NONE',  ( 21.13461538461538680, 10.61458296203670848, -112.7500000000000142 ) ) ;
#131470 = AXIS2_PLACEMENT_3D ( 'NONE', #235989, #135599, #62181 ) ;
#131471 = DIRECTION ( 'NONE',  ( 0.000000000000000000, 0.000000000000000000, 1.000000000000000000 ) ) ;
#131472 = DIRECTION ( 'NONE',  ( 1.000000000000000000, 0.000000000000000000, 0.000000000000000000 ) ) ;
#131473 = DIRECTION ( 'NONE',  ( 0.000000000000000000, -1.000000000000000000, 0.000000000000000000 ) ) ;
#131474 = DIRECTION ( 'NONE',  ( -1.000000000000000000, 0.000000000000000000, -0.000000000000000000 ) ) ;
#131476 = CARTESIAN_POINT ( 'NONE',  ( -23.15000000000000213, 76.00000000001264766, -199.3731074845243540 ) ) ;
#131475 = DIRECTION ( 'NONE',  ( -0.000000000000000000, -0.4088369013363281068, 0.9126074666063770380 ) ) ;
#131477 = DIRECTION ( 'NONE',  ( -1.000000000000000000, 0.000000000000000000, 0.000000000000000000 ) ) ;
#131478 = CARTESIAN_POINT ( 'NONE',  ( 20.95512820512820440, 22.03025613173516462, -231.6455594930189648 ) ) ;
#131479 = CARTESIAN_POINT ( 'NONE',  ( 22.49999999999999645, 0.08880997639808871358, -155.8502370819680323 ) ) ;
#131480 = DIRECTION ( 'NONE',  ( 0.000000000000000000, 6.577889128801591149E-15, -1.000000000000000000 ) ) ;
#131481 = ORIENTED_EDGE ( 'NONE', *, *, #213156, .F. ) ;
#131482 = CARTESIAN_POINT ( 'NONE',  ( -18.36527282682040507, -9.500000599999188111, -40.42214896449912942 ) ) ;
#131483 = DIRECTION ( 'NONE',  ( -2.561896900575096011E-15, -0.5907332058517279494, 0.8068669527897025517 ) ) ;
#131484 = FACE_OUTER_BOUND ( 'NONE', #93342, .T. ) ;
#131485 = DIRECTION ( 'NONE',  ( -1.000000000000000000, -0.000000000000000000, -0.000000000000000000 ) ) ;
#131486 = DIRECTION ( 'NONE',  ( 1.000000000000000000, 0.000000000000000000, 0.000000000000000000 ) ) ;
#131487 = FACE_OUTER_BOUND ( 'NONE', #210511, .T. ) ;
#131488 = ORIENTED_EDGE ( 'NONE', *, *, #240118, .F. ) ;
#131489 = VERTEX_POINT ( 'NONE', #234984 ) ;
#131490 = AXIS2_PLACEMENT_3D ( 'NONE', #68409, #90522, #12309 ) ;
#131491 = EDGE_CURVE ( 'NONE', #243191, #100689, #129284, .T. ) ;
#131492 = FACE_OUTER_BOUND ( 'NONE', #118065, .T. ) ;
#131493 = ORIENTED_EDGE ( 'NONE', *, *, #133728, .T. ) ;
#131494 = CARTESIAN_POINT ( 'NONE',  ( -18.79999999999999716, -11.75000000000000000, 30.09999999999999787 ) ) ;
#131495 = CYLINDRICAL_SURFACE ( 'NONE', #47270, 0.1000000000000028644 ) ;
#131496 = AXIS2_PLACEMENT_3D ( 'NONE', #32169, #169126, #111679 ) ;
#131497 = AXIS2_PLACEMENT_3D ( 'NONE', #33835, #169490, #50751 ) ;
#131498 = ORIENTED_EDGE ( 'NONE', *, *, #28924, .F. ) ;
#131499 = DIRECTION ( 'NONE',  ( 1.000000000000000000, -3.265361837132813093E-16, -2.280189983783949500E-30 ) ) ;
#131500 = ADVANCED_FACE ( 'NONE', ( #232430 ), #133313, .T. ) ;
#131501 = ORIENTED_EDGE ( 'NONE', *, *, #185782, .F. ) ;
#131503 = CIRCLE ( 'NONE', #123146, 0.09999999999998898659 ) ;
#131502 = CARTESIAN_POINT ( 'NONE',  ( -23.15000000000000213, 71.75000000001253397, -182.3731074845244109 ) ) ;
#131505 = CIRCLE ( 'NONE', #19074, 3.900000000000000355 ) ;
#131504 = CARTESIAN_POINT ( 'NONE',  ( 20.94999999999999929, 85.00000000001149658, -45.91707660717670336 ) ) ;
#131506 = DIRECTION ( 'NONE',  ( 0.000000000000000000, 0.3970902486047481750, -0.9177795674686920480 ) ) ;
#131507 = EDGE_CURVE ( 'NONE', #88666, #71915, #220842, .T. ) ;
#131508 = CARTESIAN_POINT ( 'NONE',  ( 23.14999999999999858, 0.000000000000000000, 0.000000000000000000 ) ) ;
#131509 = LINE ( 'NONE', #108106, #126483 ) ;
#131510 = CARTESIAN_POINT ( 'NONE',  ( -22.39999999999999503, 1.115541036281197940E-11, -59.20922040162664501 ) ) ;
#131511 = AXIS2_PLACEMENT_3D ( 'NONE', #257736, #202628, #4420 ) ;
#131512 = FACE_OUTER_BOUND ( 'NONE', #141626, .T. ) ;
#131513 = LINE ( 'NONE', #94943, #20578 ) ;
#131514 = ADVANCED_FACE ( 'NONE', ( #34238 ), #162604, .F. ) ;
#131516 = EDGE_LOOP ( 'NONE', ( #213860, #171286, #28548, #181376 ) ) ;
#131515 = CARTESIAN_POINT ( 'NONE',  ( 18.52326479938708914, -0.8637711017511672251, -242.3455657282801781 ) ) ;
#131518 = DIRECTION ( 'NONE',  ( 1.020425574104004196E-15, 1.210927747993693964E-31, 1.000000000000000000 ) ) ;
#131517 = DIRECTION ( 'NONE',  ( 0.000000000000000000, 0.000000000000000000, 1.000000000000000000 ) ) ;
#131519 = EDGE_LOOP ( 'NONE', ( #75347, #181184, #68741, #225210, #44091, #125836, #114846, #106481, #235184, #99697, #22263, #74056, #23344, #75304 ) ) ;
#131521 = ORIENTED_EDGE ( 'NONE', *, *, #227280, .T. ) ;
#131520 = DIRECTION ( 'NONE',  ( -1.000000000000000000, -0.000000000000000000, 0.000000000000000000 ) ) ;
#131522 = ORIENTED_EDGE ( 'NONE', *, *, #208554, .T. ) ;
#131523 = CARTESIAN_POINT ( 'NONE',  ( 20.94999999999999574, 5.900000000011102586, -77.21909976465646253 ) ) ;
#131524 = DIRECTION ( 'NONE',  ( 1.000000000000000000, 0.000000000000000000, 0.000000000000000000 ) ) ;
#131525 = ADVANCED_FACE ( 'NONE', ( #56318 ), #120203, .F. ) ;
#131526 = EDGE_CURVE ( 'NONE', #143126, #213407, #158348, .T. ) ;
#131527 = CARTESIAN_POINT ( 'NONE',  ( 22.39999999999999503, 76.00000000001173817, -81.17267829206912211 ) ) ;
#131528 = FACE_OUTER_BOUND ( 'NONE', #177384, .T. ) ;
#131530 = DIRECTION ( 'NONE',  ( -1.000000000000000000, 0.000000000000000000, 0.000000000000000000 ) ) ;
#131529 = CIRCLE ( 'NONE', #15022, 11.79999999999999893 ) ;
#131531 = DIRECTION ( 'NONE',  ( -4.408576920032448588E-17, 0.1350103645451876666, 0.9908441862701600211 ) ) ;
#131532 = CARTESIAN_POINT ( 'NONE',  ( 23.04999999999999716, 67.17743825834591576, -160.7731074845244166 ) ) ;
#131533 = DIRECTION ( 'NONE',  ( 0.000000000000000000, -1.000000000000000000, -6.982962677686266711E-15 ) ) ;
#131534 = ORIENTED_EDGE ( 'NONE', *, *, #216857, .F. ) ;
#131535 = ORIENTED_EDGE ( 'NONE', *, *, #212079, .F. ) ;
#131536 = PLANE ( 'NONE',  #2032 ) ;
#131537 = VECTOR ( 'NONE', #99927, 1000.000000000000114 ) ;
#131538 = AXIS2_PLACEMENT_3D ( 'NONE', #2414, #162814, #203198 ) ;
#131539 = ADVANCED_FACE ( 'NONE', ( #61479 ), #234444, .T. ) ;
#131540 = ORIENTED_EDGE ( 'NONE', *, *, #105260, .F. ) ;
#131541 = VECTOR ( 'NONE', #55151, 1000.000000000000000 ) ;
#131543 = CARTESIAN_POINT ( 'NONE',  ( -21.37071067811865532, 44.53876154244880325, -237.1775198342045314 ) ) ;
#131542 = AXIS2_PLACEMENT_3D ( 'NONE', #89981, #192954, #134237 ) ;
#131545 = EDGE_CURVE ( 'NONE', #31765, #185054, #83454, .T. ) ;
#131544 = EDGE_LOOP ( 'NONE', ( #117750, #213066, #38014, #8433 ) ) ;
#131546 = CARTESIAN_POINT ( 'NONE',  ( 18.59999996954842771, -9.523204137858824581, -40.38304171191644087 ) ) ;
#131547 = CARTESIAN_POINT ( 'NONE',  ( -20.85000000000000142, 77.26327546522965406, -162.1212428177779543 ) ) ;
#131548 = CARTESIAN_POINT ( 'NONE',  ( 21.05000000000000071, 75.47649400317826007, -205.4533772768803317 ) ) ;
#131549 = EDGE_CURVE ( 'NONE', #137582, #51105, #79185, .T. ) ;
#131550 = CARTESIAN_POINT ( 'NONE',  ( -23.25000000000000355, 11.75000000001113953, -109.7500000000000426 ) ) ;
#131551 = CARTESIAN_POINT ( 'NONE',  ( 21.78635804494511419, 75.90099493450505008, -210.5587689696775442 ) ) ;
#131552 = ORIENTED_EDGE ( 'NONE', *, *, #166072, .F. ) ;
#131553 = CARTESIAN_POINT ( 'NONE',  ( -18.31331870001089612, -9.536294719169530865, -207.8685786909852879 ) ) ;
#131554 = DIRECTION ( 'NONE',  ( 0.000000000000000000, 0.9394191166662618775, 0.3427706569150580362 ) ) ;
#131555 = CARTESIAN_POINT ( 'NONE',  ( 21.00000000000000000, 66.25000000001199396, -115.2731074845243597 ) ) ;
#131556 = ADVANCED_FACE ( 'NONE', ( #142287 ), #101857, .T. ) ;
#131557 = FACE_OUTER_BOUND ( 'NONE', #207185, .T. ) ;
#131558 = DIRECTION ( 'NONE',  ( 0.000000000000000000, -6.454785026890510900E-15, 1.000000000000000000 ) ) ;
#131559 = DIRECTION ( 'NONE',  ( 0.000000000000000000, -0.9126074666063729302, -0.4088369013363370996 ) ) ;
#131561 = ORIENTED_EDGE ( 'NONE', *, *, #141209, .F. ) ;
#131560 = ADVANCED_FACE ( 'NONE', ( #203554 ), #39377, .F. ) ;
#131562 = CIRCLE ( 'NONE', #19126, 0.09999999999999130418 ) ;
#131564 = FACE_OUTER_BOUND ( 'NONE', #43996, .T. ) ;
#131563 = DIRECTION ( 'NONE',  ( 1.000000000000000000, -0.000000000000000000, -0.000000000000000000 ) ) ;
#131565 = EDGE_LOOP ( 'NONE', ( #27149, #49863, #70524, #150680 ) ) ;
#131568 = ORIENTED_EDGE ( 'NONE', *, *, #191230, .T. ) ;
#131567 = CARTESIAN_POINT ( 'NONE',  ( 20.95289811251229750, 67.10683199555371914, -161.5212979906058877 ) ) ;
#131566 = DIRECTION ( 'NONE',  ( 0.000000000000000000, -0.9770955615653316162, -0.2128009952263604232 ) ) ;
#131569 = B_SPLINE_CURVE_WITH_KNOTS ( 'NONE', 3,
 ( #54136, #94545, #150685, #30762 ),
 .UNSPECIFIED., .F., .F.,
 ( 4, 4 ),
 ( 0.000000000000000000, 7.713889350929433657E-05 ),
 .UNSPECIFIED. ) ;
#131570 = PLANE ( 'NONE',  #122775 ) ;
#131571 = EDGE_CURVE ( 'NONE', #94150, #45697, #245801, .T. ) ;
#131572 = DIRECTION ( 'NONE',  ( 1.000000000000000000, 0.000000000000000000, 0.000000000000000000 ) ) ;
#131573 = VECTOR ( 'NONE', #98413, 1000.000000000000000 ) ;
#131574 = EDGE_LOOP ( 'NONE', ( #1137, #40497, #87773, #29699 ) ) ;
#131575 = CARTESIAN_POINT ( 'NONE',  ( -19.99999999999999645, 11.61130914238355771, 16.50000000000000000 ) ) ;
#131577 = CARTESIAN_POINT ( 'NONE',  ( -23.25000000000000000, 1.115600667400684642E-11, -67.00000000000004263 ) ) ;
#131576 = DIRECTION ( 'NONE',  ( 0.000000000000000000, 0.000000000000000000, -1.000000000000000000 ) ) ;
#131578 = ADVANCED_FACE ( 'NONE', ( #181441 ), #37725, .F. ) ;
#131580 = ORIENTED_EDGE ( 'NONE', *, *, #109988, .F. ) ;
#131579 = CARTESIAN_POINT ( 'NONE',  ( -20.64999999999999858, 47.91013932883114990, -242.3192343197862044 ) ) ;
#131581 = EDGE_LOOP ( 'NONE', ( #39270, #141817, #116309, #235177 ) ) ;
#131582 = FACE_OUTER_BOUND ( 'NONE', #233719, .T. ) ;
#131583 = CYLINDRICAL_SURFACE ( 'NONE', #93919, 0.09999999999998898659 ) ;
#131584 = AXIS2_PLACEMENT_3D ( 'NONE', #77406, #40904, #197370 ) ;
#131585 = CYLINDRICAL_SURFACE ( 'NONE', #138517, 0.09999999999999986677 ) ;
#131586 = ORIENTED_EDGE ( 'NONE', *, *, #69902, .F. ) ;
#131587 = LINE ( 'NONE', #209854, #172809 ) ;
#131588 = LINE ( 'NONE', #190299, #89334 ) ;
#131589 = VERTEX_POINT ( 'NONE', #82289 ) ;
#131590 = CARTESIAN_POINT ( 'NONE',  ( 20.74625933824081869, 60.89740640166220231, -225.2731031595071443 ) ) ;
#131591 = DIRECTION ( 'NONE',  ( 0.000000000000000000, 0.000000000000000000, -1.000000000000000000 ) ) ;
#131592 = ORIENTED_EDGE ( 'NONE', *, *, #202823, .T. ) ;
#131593 = VECTOR ( 'NONE', #164353, 1000.000000000000000 ) ;
#131594 = CARTESIAN_POINT ( 'NONE',  ( -21.55000000000000071, 65.67360898266123570, -213.5186389139583980 ) ) ;
#131595 = CARTESIAN_POINT ( 'NONE',  ( -21.05000000000000071, 7.128833340093095217, -233.7327013124392749 ) ) ;
#131596 = VECTOR ( 'NONE', #223580, 1000.000000000000000 ) ;
#131597 = CIRCLE ( 'NONE', #139953, 0.1000000000000028644 ) ;
#131598 = AXIS2_PLACEMENT_3D ( 'NONE', #147001, #33540, #226527 ) ;
#131599 = ORIENTED_EDGE ( 'NONE', *, *, #194510, .F. ) ;
#131600 = ORIENTED_EDGE ( 'NONE', *, *, #17791, .T. ) ;
#131601 = DIRECTION ( 'NONE',  ( -0.000000000000000000, -6.982962677686266711E-15, 1.000000000000000000 ) ) ;
#131602 = ADVANCED_FACE ( 'NONE', ( #19797 ), #133378, .T. ) ;
#131603 = EDGE_LOOP ( 'NONE', ( #215101, #255149, #118483, #249070, #249442 ) ) ;
#131605 = ORIENTED_EDGE ( 'NONE', *, *, #251693, .F. ) ;
#131604 = CARTESIAN_POINT ( 'NONE',  ( -11.60000000000000320, -8.250000000000007105, 15.00000000000000355 ) ) ;
#131606 = EDGE_LOOP ( 'NONE', ( #28689, #91547, #112502, #100651 ) ) ;
#131609 = VERTEX_POINT ( 'NONE', #199725 ) ;
#131608 = ORIENTED_EDGE ( 'NONE', *, *, #65565, .F. ) ;
#131607 = DIRECTION ( 'NONE',  ( 0.000000000000000000, 0.000000000000000000, 1.000000000000000000 ) ) ;
#131610 = DIRECTION ( 'NONE',  ( -1.000000000000000000, 0.000000000000000000, 0.000000000000000000 ) ) ;
#131611 = ORIENTED_EDGE ( 'NONE', *, *, #245738, .T. ) ;
#131612 = DIRECTION ( 'NONE',  ( 0.000000000000000000, 0.000000000000000000, -1.000000000000000000 ) ) ;
#131614 = EDGE_CURVE ( 'NONE', #77088, #208877, #21094, .T. ) ;
#131613 = DIRECTION ( 'NONE',  ( 0.000000000000000000, 0.9770955615653313941, 0.2128009952263603677 ) ) ;
#131615 = TOROIDAL_SURFACE ( 'NONE', #6723, 12.97499999999999787, 0.1000000000000000056 ) ;
#131616 = CARTESIAN_POINT ( 'NONE',  ( -23.25000000000000000, 1.115650265596050101E-11, -96.45000000000003126 ) ) ;
#131617 = FACE_OUTER_BOUND ( 'NONE', #108465, .T. ) ;
#131618 = CARTESIAN_POINT ( 'NONE',  ( -20.94999999999999929, 28.71379363806100571, -258.2416688332294825 ) ) ;
#131620 = ORIENTED_EDGE ( 'NONE', *, *, #91700, .F. ) ;
#131619 = CIRCLE ( 'NONE', #123243, 0.09999999999999939493 ) ;
#131621 = VERTEX_POINT ( 'NONE', #1488 ) ;
#131622 = ORIENTED_EDGE ( 'NONE', *, *, #42636, .T. ) ;
#131623 = DIRECTION ( 'NONE',  ( -1.836970198721029934E-16, -1.000000000000000000, -6.982962677686266711E-15 ) ) ;
#131625 = ORIENTED_EDGE ( 'NONE', *, *, #213297, .F. ) ;
#131624 = CARTESIAN_POINT ( 'NONE',  ( 21.72449340488910607, 65.71604372252143378, -182.6731074845244223 ) ) ;
#131627 = FACE_OUTER_BOUND ( 'NONE', #82207, .T. ) ;
#131626 = AXIS2_PLACEMENT_3D ( 'NONE', #96529, #255575, #91429 ) ;
#131629 = ORIENTED_EDGE ( 'NONE', *, *, #186099, .T. ) ;
#131628 = CARTESIAN_POINT ( 'NONE',  ( 20.05000000000002913, 28.93140779147706354, -237.1870821964558900 ) ) ;
#131630 =( BOUNDED_SURFACE ( )  B_SPLINE_SURFACE ( 3, 2, ( 
 ( #23855, #98181, #69388 ),
 ( #124222, #145043, #185468 ),
 ( #125492, #186765, #168518 ),
 ( #224581, #10685, #189326 ),
 ( #108493, #27717, #208879 ),
 ( #203747, #86329, #148922 ) ),
 .UNSPECIFIED., .F., .F., .F. ) 
 B_SPLINE_SURFACE_WITH_KNOTS ( ( 4, 2, 4 ),
 ( 3, 3 ),
 ( 0.0001300404313046778129, 0.0003183318589266858375, 0.0005066232865486938351 ),
 ( 0.000000000000000000, 1.000000000000000000 ),
 .UNSPECIFIED. ) 
 GEOMETRIC_REPRESENTATION_ITEM ( )  RATIONAL_B_SPLINE_SURFACE ( (
 ( 1.000000000000000000, 0.7071067811865352493, 1.000000000000000000),
 ( 1.000000000000000000, 0.7625113560543027580, 1.000000000000000000),
 ( 1.000000000000000000, 0.8126073484685780723, 1.000000000000000000),
 ( 1.000000000000000000, 0.8923049332735644157, 1.000000000000000000),
 ( 1.000000000000000000, 0.9231914937767029539, 1.000000000000000000),
 ( 1.000000000000000000, 0.9238795325112919565, 1.000000000000000000) ) ) 
 REPRESENTATION_ITEM ( '' )  SURFACE ( )  );
#131631 = ORIENTED_EDGE ( 'NONE', *, *, #34645, .F. ) ;
#131632 = DIRECTION ( 'NONE',  ( 0.000000000000000000, 0.2617529984165031243, 0.9651348961777157509 ) ) ;
#131633 = VECTOR ( 'NONE', #126065, 1000.000000000000000 ) ;
#131634 = CIRCLE ( 'NONE', #177468, 0.1000000000000124678 ) ;
#131635 = ORIENTED_EDGE ( 'NONE', *, *, #64339, .T. ) ;
#131636 = CARTESIAN_POINT ( 'NONE',  ( -16.84793658983456410, 9.950000000011197443, -180.2336466778095314 ) ) ;
#131637 = DIRECTION ( 'NONE',  ( -0.000000000000000000, -0.4856429311786365499, -0.8741572761215353760 ) ) ;
#131640 = ORIENTED_EDGE ( 'NONE', *, *, #165972, .T. ) ;
#131639 = ORIENTED_EDGE ( 'NONE', *, *, #116598, .F. ) ;
#131638 = AXIS2_PLACEMENT_3D ( 'NONE', #157316, #742, #141570 ) ;
#131641 = ORIENTED_EDGE ( 'NONE', *, *, #255068, .F. ) ;
#131642 = CARTESIAN_POINT ( 'NONE',  ( -21.07928932188134041, 30.84304088367084162, -252.0482413927653340 ) ) ;
#131643 = CIRCLE ( 'NONE', #156806, 0.1000000000000028644 ) ;
#131644 = VERTEX_POINT ( 'NONE', #182725 ) ;
#131646 =( BOUNDED_CURVE ( )  B_SPLINE_CURVE ( 3, ( #70169, #7598, #68876, #187546 ),
 .UNSPECIFIED., .F., .F. ) 
 B_SPLINE_CURVE_WITH_KNOTS ( ( 4, 4 ),
 ( 4.712388980384690562, 6.283185307179586232 ),
 .UNSPECIFIED. ) 
 CURVE ( )  GEOMETRIC_REPRESENTATION_ITEM ( )  RATIONAL_B_SPLINE_CURVE ( ( 1.000000000000000000, 0.8047378541243652705, 0.8047378541243652705, 1.000000000000000000 ) ) 
 REPRESENTATION_ITEM ( '' )  );
#131645 = AXIS2_PLACEMENT_3D ( 'NONE', #187294, #11215, #131147 ) ;
#131647 = ORIENTED_EDGE ( 'NONE', *, *, #9369, .F. ) ;
#131648 = CARTESIAN_POINT ( 'NONE',  ( 23.14999999999999858, 71.18691588786307989, -191.5815897280005800 ) ) ;
#131649 = ORIENTED_EDGE ( 'NONE', *, *, #125809, .T. ) ;
#131650 = FACE_OUTER_BOUND ( 'NONE', #52574, .T. ) ;
#131651 = AXIS2_PLACEMENT_3D ( 'NONE', #156007, #200246, #197664 ) ;
#131653 = CARTESIAN_POINT ( 'NONE',  ( 20.94999999999999929, 5.850000000011156942, -190.8675027757220448 ) ) ;
#131652 = CARTESIAN_POINT ( 'NONE',  ( -21.05000000000000071, 0.000000000000000000, -33.50000000000000000 ) ) ;
#131654 = DIRECTION ( 'NONE',  ( 0.000000000000000000, -0.9126074666063660468, -0.4088369013363524762 ) ) ;
#131655 = DIRECTION ( 'NONE',  ( -0.000000000000000000, 0.000000000000000000, 1.000000000000000000 ) ) ;
#131656 = ORIENTED_EDGE ( 'NONE', *, *, #196119, .F. ) ;
#131657 = ADVANCED_FACE ( 'NONE', ( #160606 ), #204269, .T. ) ;
#131658 = EDGE_LOOP ( 'NONE', ( #219561, #15949, #181062, #5193 ) ) ;
#131659 = CARTESIAN_POINT ( 'NONE',  ( 18.50000000000000355, 85.42107434499847329, -96.19863542509438048 ) ) ;
#131660 = DIRECTION ( 'NONE',  ( 0.000000000000000000, -0.9797463026583741463, -0.2002428086779789451 ) ) ;
#131661 = LINE ( 'NONE', #226905, #149496 ) ;
#131662 = ADVANCED_FACE ( 'NONE', ( #242669 ), #41934, .F. ) ;
#131663 = VERTEX_POINT ( 'NONE', #49614 ) ;
#131664 =( BOUNDED_CURVE ( )  B_SPLINE_CURVE ( 3, ( #233027, #131331, #213430, #34832 ),
 .UNSPECIFIED., .F., .F. ) 
 B_SPLINE_CURVE_WITH_KNOTS ( ( 4, 4 ),
 ( 4.712388980384690562, 6.283185307179586232 ),
 .UNSPECIFIED. ) 
 CURVE ( )  GEOMETRIC_REPRESENTATION_ITEM ( )  RATIONAL_B_SPLINE_CURVE ( ( 1.000000000000000000, 0.8047378541243652705, 0.8047378541243652705, 1.000000000000000000 ) ) 
 REPRESENTATION_ITEM ( '' )  );
#131665 = LINE ( 'NONE', #70452, #67994 ) ;
#131666 = CARTESIAN_POINT ( 'NONE',  ( -18.59999999999999787, 1.835341550235567887, -78.55515129256302487 ) ) ;
#131667 = ORIENTED_EDGE ( 'NONE', *, *, #39800, .F. ) ;
#131668 = ORIENTED_EDGE ( 'NONE', *, *, #198490, .T. ) ;
#131669 = EDGE_CURVE ( 'NONE', #92812, #62695, #166732, .T. ) ;
#131670 = CARTESIAN_POINT ( 'NONE',  ( -17.11825945287482753, 10.05000000001113847, -180.2499999999999716 ) ) ;
#131671 = DIRECTION ( 'NONE',  ( 0.000000000000000000, 0.8814952561688429444, -0.4721928772777345684 ) ) ;
#131672 = EDGE_LOOP ( 'NONE', ( #119529, #43523 ) ) ;
#131673 = CARTESIAN_POINT ( 'NONE',  ( -18.40000000000000213, 70.35000000001180354, -78.77310748452434552 ) ) ;
#131674 = ORIENTED_EDGE ( 'NONE', *, *, #129521, .T. ) ;
#131675 = DIRECTION ( 'NONE',  ( -1.000000000000000000, -7.304098846218164250E-16, 4.217023435051628197E-16 ) ) ;
#131676 = CARTESIAN_POINT ( 'NONE',  ( -23.25000000000000000, 5.354661166737471056, -213.3684367965233832 ) ) ;
#131678 = CARTESIAN_POINT ( 'NONE',  ( -20.54999999999999716, 68.85000000001180354, -81.87310748452436826 ) ) ;
#131677 = CARTESIAN_POINT ( 'NONE',  ( -21.05000000000000071, 0.5876173420563349792, -209.1618981382189588 ) ) ;
#131679 = EDGE_CURVE ( 'NONE', #17700, #257458, #41819, .T. ) ;
#131680 = CARTESIAN_POINT ( 'NONE',  ( 20.04142135391667168, 11.75000000001116263, -91.70250686562992826 ) ) ;
#131681 = AXIS2_PLACEMENT_3D ( 'NONE', #160134, #35071, #97531 ) ;
#131682 = CARTESIAN_POINT ( 'NONE',  ( -20.54999999999999716, 1.115600667400684642E-11, -113.4750000000000369 ) ) ;
#131683 = FACE_OUTER_BOUND ( 'NONE', #253230, .T. ) ;
#131684 = AXIS2_PLACEMENT_3D ( 'NONE', #3610, #6173, #83112 ) ;
#131685 = CARTESIAN_POINT ( 'NONE',  ( 21.05000000000000071, -9.499999999988848032, -110.3939691226524786 ) ) ;
#131686 = CIRCLE ( 'NONE', #115122, 0.5000000000000004441 ) ;
#131687 = AXIS2_PLACEMENT_3D ( 'NONE', #10988, #133503, #76093 ) ;
#131688 = EDGE_CURVE ( 'NONE', #224619, #167256, #237613, .T. ) ;
#131690 = ORIENTED_EDGE ( 'NONE', *, *, #98565, .T. ) ;
#131689 = FACE_OUTER_BOUND ( 'NONE', #92536, .T. ) ;
#131691 = CIRCLE ( 'NONE', #139861, 0.2000000000000118627 ) ;
#131693 = VERTEX_POINT ( 'NONE', #84848 ) ;
#131692 = EDGE_LOOP ( 'NONE', ( #150959, #238553, #195552, #138686 ) ) ;
#131694 = VERTEX_POINT ( 'NONE', #208711 ) ;
#131695 = CARTESIAN_POINT ( 'NONE',  ( 22.49436431346199683, 0.06690352972226094874, 11.64995094765345840 ) ) ;
#131696 = SPHERICAL_SURFACE ( 'NONE', #161906, 0.1000000000000000056 ) ;
#131697 = EDGE_CURVE ( 'NONE', #195203, #177395, #243957, .T. ) ;
#131699 = CARTESIAN_POINT ( 'NONE',  ( -20.64999999999999858, 71.65000000001207070, -124.1731074845243228 ) ) ;
#131698 = CARTESIAN_POINT ( 'NONE',  ( -16.83794479845801462, 66.07364258066102991, -182.8266627803020867 ) ) ;
#131700 = CARTESIAN_POINT ( 'NONE',  ( 13.40000000000000036, -11.65000000000000036, 15.00000000000000355 ) ) ;
#131701 = VERTEX_POINT ( 'NONE', #165734 ) ;
#131702 = CARTESIAN_POINT ( 'NONE',  ( -20.90000000000000213, 6.356682116888462630, 11.91686199900910381 ) ) ;
#131703 = AXIS2_PLACEMENT_3D ( 'NONE', #90399, #8322, #47411 ) ;
#131704 = ORIENTED_EDGE ( 'NONE', *, *, #129959, .F. ) ;
#131705 = ORIENTED_EDGE ( 'NONE', *, *, #77474, .F. ) ;
#131706 = CARTESIAN_POINT ( 'NONE',  ( -21.05000000000000071, -0.09999996530009948315, 6.477552182493442778 ) ) ;
#131707 = CIRCLE ( 'NONE', #69547, 11.70000000000000284 ) ;
#131708 = DIRECTION ( 'NONE',  ( -3.265361837132813093E-16, -0.9651348961777157509, 0.2617529984165031243 ) ) ;
#131709 = DIRECTION ( 'NONE',  ( 1.000000000000000000, 0.000000000000000000, 0.000000000000000000 ) ) ;
#131710 = ORIENTED_EDGE ( 'NONE', *, *, #120504, .T. ) ;
#131711 = CARTESIAN_POINT ( 'NONE',  ( -23.15000000000000213, 1.115600667400684642E-11, -100.5000000000000426 ) ) ;
#131712 = CARTESIAN_POINT ( 'NONE',  ( -18.40000000000000213, 11.48667500176882861, -124.7500000000000284 ) ) ;
#131713 = ORIENTED_EDGE ( 'NONE', *, *, #15903, .T. ) ;
#131714 = ORIENTED_EDGE ( 'NONE', *, *, #58195, .F. ) ;
#131715 = FACE_OUTER_BOUND ( 'NONE', #120900, .T. ) ;
#131716 = CYLINDRICAL_SURFACE ( 'NONE', #227088, 0.09999999999999939493 ) ;
#131717 = DIRECTION ( 'NONE',  ( 1.000000000000000000, 0.000000000000000000, 0.000000000000000000 ) ) ;
#131718 = DIRECTION ( 'NONE',  ( 0.000000000000000000, 0.000000000000000000, 1.000000000000000000 ) ) ;
#131719 = DIRECTION ( 'NONE',  ( 6.938893903907222067E-15, 1.000000000000000000, 6.982962677686266711E-15 ) ) ;
#131720 = DIRECTION ( 'NONE',  ( 0.000000000000000000, 0.000000000000000000, -1.000000000000000000 ) ) ;
#131721 = ORIENTED_EDGE ( 'NONE', *, *, #94673, .T. ) ;
#131722 = DIRECTION ( 'NONE',  ( 1.000000000000000000, 7.492892343619937423E-30, -1.073024830501117725E-15 ) ) ;
#131724 = ADVANCED_FACE ( 'NONE', ( #167032 ), #30083, .F. ) ;
#131723 = CARTESIAN_POINT ( 'NONE',  ( -21.46681500593267700, 6.857511159395789591, -33.50000000000000711 ) ) ;
#131726 = CARTESIAN_POINT ( 'NONE',  ( -20.97625342178436014, 11.60000000083177696, -174.4282032298017384 ) ) ;
#131725 = DIRECTION ( 'NONE',  ( 1.000000000000000000, 0.000000000000000000, 0.000000000000000000 ) ) ;
#131727 = FACE_OUTER_BOUND ( 'NONE', #84451, .T. ) ;
#131728 = FACE_OUTER_BOUND ( 'NONE', #132528, .T. ) ;
#131729 = DIRECTION ( 'NONE',  ( 0.000000000000000000, -7.116814260417668513E-15, 1.000000000000000000 ) ) ;
#131730 = CARTESIAN_POINT ( 'NONE',  ( -23.15000000000000213, 1.115600667400684642E-11, -67.00000000000000000 ) ) ;
#131731 = AXIS2_PLACEMENT_3D ( 'NONE', #240449, #241729, #61815 ) ;
#131734 = VERTEX_POINT ( 'NONE', #226970 ) ;
#131733 = AXIS2_PLACEMENT_3D ( 'NONE', #257358, #115340, #237861 ) ;
#131732 = CARTESIAN_POINT ( 'NONE',  ( -23.15000000000000213, 1.115650265596050101E-11, -129.9500000000000171 ) ) ;
#131735 = AXIS2_PLACEMENT_3D ( 'NONE', #7747, #106821, #67710 ) ;
#131736 = AXIS2_PLACEMENT_3D ( 'NONE', #121143, #20744, #100229 ) ;
#131737 = EDGE_CURVE ( 'NONE', #233936, #87492, #216748, .T. ) ;
#131738 = DIRECTION ( 'NONE',  ( 0.000000000000000000, 0.000000000000000000, -1.000000000000000000 ) ) ;
#131739 = EDGE_CURVE ( 'NONE', #190057, #96187, #25240, .T. ) ;
#131740 = AXIS2_PLACEMENT_3D ( 'NONE', #63404, #103801, #237256 ) ;
#131741 = EDGE_CURVE ( 'NONE', #76432, #61312, #154443, .T. ) ;
#131742 = CARTESIAN_POINT ( 'NONE',  ( 13.43663047529820709, 9.446645344706402270, -85.41080645610021804 ) ) ;
#131743 = DIRECTION ( 'NONE',  ( -3.890533409366483389E-14, 0.8127272543710891695, -0.5826443254700338636 ) ) ;
#131744 = AXIS2_PLACEMENT_3D ( 'NONE', #125307, #26214, #229548 ) ;
#131745 = DIRECTION ( 'NONE',  ( 1.000000000000000000, 0.000000000000000000, 0.000000000000000000 ) ) ;
#131746 = CARTESIAN_POINT ( 'NONE',  ( -18.59999999999999787, -1.249999999988843369, -41.50000000000000000 ) ) ;
#131747 = CARTESIAN_POINT ( 'NONE',  ( 21.05000000000000071, 5.850000000011105428, -110.6324972242780120 ) ) ;
#131748 = AXIS2_PLACEMENT_3D ( 'NONE', #100058, #3544, #2252 ) ;
#131749 = ORIENTED_EDGE ( 'NONE', *, *, #221140, .F. ) ;
#131750 = FACE_OUTER_BOUND ( 'NONE', #184476, .T. ) ;
#131752 = ORIENTED_EDGE ( 'NONE', *, *, #22415, .F. ) ;
#131751 = CARTESIAN_POINT ( 'NONE',  ( 18.59999999999999076, 69.45000000001181206, -81.87310748452435405 ) ) ;
#131753 = CARTESIAN_POINT ( 'NONE',  ( 18.49999999999999289, 69.55000000001150795, -48.37310748452436826 ) ) ;
#131754 = EDGE_CURVE ( 'NONE', #102722, #156184, #206125, .T. ) ;
#131755 = CARTESIAN_POINT ( 'NONE',  ( -23.25000000000000000, 1.115600667400684642E-11, -67.00000000000000000 ) ) ;
#131756 = ORIENTED_EDGE ( 'NONE', *, *, #207373, .T. ) ;
#131757 = CARTESIAN_POINT ( 'NONE',  ( 23.24999999999999645, 73.90000000001170122, -69.52310748452431710 ) ) ;
#131758 = ADVANCED_FACE ( 'NONE', ( #5318 ), #199459, .T. ) ;
#131759 = APPLICATION_PROTOCOL_DEFINITION ( 'draft international standard', 'automotive_design', 1998, #182240 ) ;
#131760 = EDGE_CURVE ( 'NONE', #142448, #87242, #100206, .T. ) ;
#131761 = CARTESIAN_POINT ( 'NONE',  ( -23.15000000000000213, 1.925233644870972816, -180.2302435331260995 ) ) ;
#131762 = CARTESIAN_POINT ( 'NONE',  ( 22.48970261584622321, 64.35000000001166143, -69.57847697274181087 ) ) ;
#131763 = ORIENTED_EDGE ( 'NONE', *, *, #85909, .F. ) ;
#131764 = DIRECTION ( 'NONE',  ( 0.5932847527679310229, -0.8049926720990042694, 0.000000000000000000 ) ) ;
#131765 = CYLINDRICAL_SURFACE ( 'NONE', #737, 0.09999999999999939493 ) ;
#131766 = CIRCLE ( 'NONE', #177598, 0.09999999999999939493 ) ;
#131767 = ADVANCED_FACE ( 'NONE', ( #246523 ), #71213, .F. ) ;
#131768 = DIRECTION ( 'NONE',  ( 1.000000000000000000, 0.000000000000000000, -1.020425574104004196E-15 ) ) ;
#131769 = EDGE_LOOP ( 'NONE', ( #197332, #16297, #63498, #246484, #174679, #257854 ) ) ;
#131770 = ORIENTED_EDGE ( 'NONE', *, *, #52499, .T. ) ;
#131771 = ADVANCED_FACE ( 'NONE', ( #47024 ), #134266, .F. ) ;
#131772 = ADVANCED_FACE ( 'NONE', ( #255465 ), #191728, .T. ) ;
#131773 = AXIS2_PLACEMENT_3D ( 'NONE', #55355, #73707, #115365 ) ;
#131774 = FACE_OUTER_BOUND ( 'NONE', #110224, .T. ) ;
#131775 = DIRECTION ( 'NONE',  ( 1.000000000000000000, 0.000000000000000000, -0.000000000000000000 ) ) ;
#131776 = CARTESIAN_POINT ( 'NONE',  ( -20.54999999999999716, -9.399999999988846611, -191.1060308773475356 ) ) ;
#131777 = DIRECTION ( 'NONE',  ( -1.000000000000000000, 0.000000000000000000, 0.000000000000000000 ) ) ;
#131779 = CARTESIAN_POINT ( 'NONE',  ( -20.64999999999999858, 21.39147882631411335, -233.2615922652120730 ) ) ;
#131778 = DIRECTION ( 'NONE',  ( 0.000000000000000000, 0.2128009952263585081, -0.9770955615653320603 ) ) ;
#131780 = CARTESIAN_POINT ( 'NONE',  ( -21.08035267497491816, 75.91731137523639461, -176.3548143243073980 ) ) ;
#131781 = FACE_OUTER_BOUND ( 'NONE', #184110, .T. ) ;
#131782 = FACE_OUTER_BOUND ( 'NONE', #188032, .T. ) ;
#131783 = AXIS2_PLACEMENT_3D ( 'NONE', #200095, #20180, #237926 ) ;
#131784 = VERTEX_POINT ( 'NONE', #16921 ) ;
#131785 = AXIS2_PLACEMENT_3D ( 'NONE', #236815, #13938, #34806 ) ;
#131787 = VERTEX_POINT ( 'NONE', #133019 ) ;
#131786 = CARTESIAN_POINT ( 'NONE',  ( -16.89268316805466341, 12.41449167011727361, -211.2369018264743090 ) ) ;
#131788 = DIRECTION ( 'NONE',  ( 1.073024830501117725E-15, 6.982962677686266711E-15, -1.000000000000000000 ) ) ;
#131789 = CYLINDRICAL_SURFACE ( 'NONE', #115828, 2.000000000000012879 ) ;
#131791 = CARTESIAN_POINT ( 'NONE',  ( -18.40000000000000213, 43.53670602441511051, -233.9623419884299551 ) ) ;
#131790 = DIRECTION ( 'NONE',  ( 0.000000000000000000, 0.2617529984165031243, 0.9651348961777157509 ) ) ;
#131792 = EDGE_CURVE ( 'NONE', #179647, #114189, #35367, .T. ) ;
#131793 = EDGE_LOOP ( 'NONE', ( #103422, #190319, #83782, #6225 ) ) ;
#131794 = CARTESIAN_POINT ( 'NONE',  ( -18.50000000000000000, 4.324939842317335525, -212.0862480289983409 ) ) ;
#131796 = ADVANCED_FACE ( 'NONE', ( #14372 ), #112713, .F. ) ;
#131795 = CARTESIAN_POINT ( 'NONE',  ( 19.97071067811865674, 64.27928932189330169, -111.8731074845243825 ) ) ;
#131797 = CARTESIAN_POINT ( 'NONE',  ( -21.05000000000000071, 69.58633726514277384, -102.9375146211624497 ) ) ;
#131798 = CARTESIAN_POINT ( 'NONE',  ( 21.14999999999999858, 6.390846877240206503, -199.6081416912452653 ) ) ;
#131799 = EDGE_LOOP ( 'NONE', ( #27332, #122086, #140308, #50870 ) ) ;
#131800 = ORIENTED_EDGE ( 'NONE', *, *, #165431, .T. ) ;
#131801 = EDGE_CURVE ( 'NONE', #59416, #44364, #146017, .T. ) ;
#131802 = CYLINDRICAL_SURFACE ( 'NONE', #138544, 0.09999999999998898659 ) ;
#131803 = ORIENTED_EDGE ( 'NONE', *, *, #129233, .F. ) ;
#131804 = LINE ( 'NONE', #47111, #155494 ) ;
#131805 = AXIS2_PLACEMENT_3D ( 'NONE', #35580, #218014, #118954 ) ;
#131806 = CARTESIAN_POINT ( 'NONE',  ( -18.40000000000000213, 64.52683809664982562, -78.82293673299012937 ) ) ;
#131807 = AXIS2_PLACEMENT_3D ( 'NONE', #153108, #17404, #132215 ) ;
#131808 = DIRECTION ( 'NONE',  ( 0.000000000000000000, 0.8660254037844420383, -0.4999999999999943379 ) ) ;
#131810 = EDGE_LOOP ( 'NONE', ( #2882, #254026, #170592 ) ) ;
#131809 = AXIS2_PLACEMENT_3D ( 'NONE', #105503, #88519, #185077 ) ;
#131811 = CARTESIAN_POINT ( 'NONE',  ( -17.11825945287482753, 9.949999999999983302, -12.75000000000000178 ) ) ;
#131812 = AXIS2_PLACEMENT_3D ( 'NONE', #207908, #149216, #245731 ) ;
#131813 = CARTESIAN_POINT ( 'NONE',  ( -20.64999999999999858, 76.00000000001170974, -69.52310748452431710 ) ) ;
#131814 = AXIS2_PLACEMENT_3D ( 'NONE', #132293, #252233, #95723 ) ;
#131815 = CARTESIAN_POINT ( 'NONE',  ( -18.50000000000000000, 68.00366762990590530, -224.2307594727497815 ) ) ;
#131816 = EDGE_CURVE ( 'NONE', #79663, #140018, #96123, .T. ) ;
#131817 = CARTESIAN_POINT ( 'NONE',  ( 21.05000000000000071, 62.24653955602229161, -247.9500786234238490 ) ) ;
#131818 = DIRECTION ( 'NONE',  ( -0.000000000000000000, 0.000000000000000000, 1.000000000000000000 ) ) ;
#131819 = CARTESIAN_POINT ( 'NONE',  ( 18.49999999999998934, 6.450000000011156587, -77.01702717044007329 ) ) ;
#131820 = CARTESIAN_POINT ( 'NONE',  ( -16.77431908686106965, 66.05419424549425855, -149.1872682668742129 ) ) ;
#131821 = EDGE_CURVE ( 'NONE', #211078, #198094, #108609, .T. ) ;
#131822 = ORIENTED_EDGE ( 'NONE', *, *, #173086, .F. ) ;
#131824 = DIRECTION ( 'NONE',  ( 0.000000000000000000, -1.000000000000000000, -6.982962677686266711E-15 ) ) ;
#131823 = FACE_OUTER_BOUND ( 'NONE', #23226, .T. ) ;
#131825 = ORIENTED_EDGE ( 'NONE', *, *, #116472, .F. ) ;
#131827 = VERTEX_POINT ( 'NONE', #190435 ) ;
#131826 = DIRECTION ( 'NONE',  ( -0.000000000000000000, -0.000000000000000000, 1.000000000000000000 ) ) ;
#131828 = AXIS2_PLACEMENT_3D ( 'NONE', #162140, #125558, #103400 ) ;
#131829 = ORIENTED_EDGE ( 'NONE', *, *, #220936, .F. ) ;
#131830 = CARTESIAN_POINT ( 'NONE',  ( -20.85000000000000142, 11.65000000001115232, -67.00000000000000000 ) ) ;
#131831 = AXIS2_PLACEMENT_3D ( 'NONE', #245577, #43526, #203863 ) ;
#131832 = CARTESIAN_POINT ( 'NONE',  ( 15.75000000000000000, 66.65000000001229807, -153.1573643172505683 ) ) ;
#131833 = VECTOR ( 'NONE', #145567, 1000.000000000000000 ) ;
#131834 = CARTESIAN_POINT ( 'NONE',  ( 18.49999999999999289, 65.55993210786641612, -78.25598973563684524 ) ) ;
#131835 = DIRECTION ( 'NONE',  ( 1.000000000000000000, -1.335000415235278971E-16, 2.979993593738921214E-16 ) ) ;
#131836 = ORIENTED_EDGE ( 'NONE', *, *, #42073, .F. ) ;
#131837 = ADVANCED_FACE ( 'NONE', ( #74353 ), #91318, .T. ) ;
#131838 = DIRECTION ( 'NONE',  ( -1.000000000000000000, 0.000000000000000000, -0.000000000000000000 ) ) ;
#131839 = CARTESIAN_POINT ( 'NONE',  ( -23.25000000000000000, 66.45861426436469799, -222.8494355952551018 ) ) ;
#131840 = EDGE_CURVE ( 'NONE', #161509, #130891, #153908, .T. ) ;
#131841 = ORIENTED_EDGE ( 'NONE', *, *, #90883, .T. ) ;
#131842 = DIRECTION ( 'NONE',  ( 1.000000000000000000, 0.000000000000000000, 0.000000000000000000 ) ) ;
#131843 = EDGE_CURVE ( 'NONE', #59716, #77719, #254337, .T. ) ;
#131844 = AXIS2_PLACEMENT_3D ( 'NONE', #215963, #37364, #257611 ) ;
#131845 = DIRECTION ( 'NONE',  ( 0.000000000000000000, -1.000000000000000000, 0.000000000000000000 ) ) ;
#131846 = ORIENTED_EDGE ( 'NONE', *, *, #220452, .T. ) ;
#131847 = DIRECTION ( 'NONE',  ( 1.000000000000000000, -3.469446951953718318E-14, 2.003086131649645455E-14 ) ) ;
#131848 = EDGE_CURVE ( 'NONE', #200243, #31922, #213825, .T. ) ;
#131849 = ORIENTED_EDGE ( 'NONE', *, *, #150753, .F. ) ;
#131850 = CARTESIAN_POINT ( 'NONE',  ( 18.50000972452444969, 65.70673848566960373, -97.56382523348291613 ) ) ;
#131853 = ADVANCED_FACE ( 'NONE', ( #176009 ), #95161, .F. ) ;
#131852 = EDGE_CURVE ( 'NONE', #94754, #79539, #194292, .T. ) ;
#131851 = VERTEX_POINT ( 'NONE', #114730 ) ;
#131854 = CARTESIAN_POINT ( 'NONE',  ( 23.15000000000000213, 84.66355140188112216, -112.5472086025915388 ) ) ;
#131855 = DIRECTION ( 'NONE',  ( 0.000000000000000000, 0.8814952561688437216, -0.4721928772777334582 ) ) ;
#131856 = CARTESIAN_POINT ( 'NONE',  ( 21.04999999999999716, 76.01681986839737704, -75.83053270408971969 ) ) ;
#131857 = DIRECTION ( 'NONE',  ( 1.000000000000000000, 0.000000000000000000, 0.000000000000000000 ) ) ;
#131858 = CIRCLE ( 'NONE', #23570, 0.1000000000000124678 ) ;
#131859 = TOROIDAL_SURFACE ( 'NONE', #31927, 12.77500000000000036, 0.1000000000000000056 ) ;
#131860 = CIRCLE ( 'NONE', #152744, 0.09999999999999971412 ) ;
#131861 = AXIS2_PLACEMENT_3D ( 'NONE', #228469, #104613, #245463 ) ;
#131862 = DIRECTION ( 'NONE',  ( 1.000000000000000000, 0.000000000000000000, -0.000000000000000000 ) ) ;
#131863 = CARTESIAN_POINT ( 'NONE',  ( 18.49999999999999645, -9.480686695267818820, -73.94111516875784673 ) ) ;
#131864 = CARTESIAN_POINT ( 'NONE',  ( 21.72449340488910607, 10.28395627750226815, -154.8500000000000227 ) ) ;
#131866 = ORIENTED_EDGE ( 'NONE', *, *, #172144, .F. ) ;
#131865 = EDGE_CURVE ( 'NONE', #212805, #63849, #29533, .T. ) ;
#131868 = ADVANCED_FACE ( 'NONE', ( #119887 ), #162862, .F. ) ;
#131867 = DIRECTION ( 'NONE',  ( 0.000000000000000000, -0.1290532225515392262, -0.9916376685811520986 ) ) ;
#131869 = ORIENTED_EDGE ( 'NONE', *, *, #165761, .F. ) ;
#131872 = ORIENTED_EDGE ( 'NONE', *, *, #256992, .T. ) ;
#131871 = DIRECTION ( 'NONE',  ( 1.000000000000000000, 0.000000000000000000, 0.000000000000000000 ) ) ;
#131870 = DIRECTION ( 'NONE',  ( -1.836970198721029934E-16, -0.4088369013363281068, 0.9126074666063770380 ) ) ;
#131873 = CIRCLE ( 'NONE', #127598, 0.1000000000000067224 ) ;
#131874 = ORIENTED_EDGE ( 'NONE', *, *, #93257, .F. ) ;
#131875 = DIRECTION ( 'NONE',  ( 1.000000000000000000, 1.394253735153569469E-16, 2.602809386958778209E-16 ) ) ;
#131876 = LINE ( 'NONE', #10652, #59949 ) ;
#131877 = DIRECTION ( 'NONE',  ( 0.000000000000000000, 1.000000000000000000, 0.000000000000000000 ) ) ;
#131878 = ADVANCED_FACE ( 'NONE', ( #59857 ), #37905, .T. ) ;
#131879 = CARTESIAN_POINT ( 'NONE',  ( 21.15000000000003055, 77.16254490893143725, -44.02310748452479316 ) ) ;
#131880 = ORIENTED_EDGE ( 'NONE', *, *, #64882, .T. ) ;
#131882 = ORIENTED_EDGE ( 'NONE', *, *, #253283, .T. ) ;
#131881 = DIRECTION ( 'NONE',  ( 1.000000000000000000, -0.000000000000000000, 0.000000000000000000 ) ) ;
#131883 = VECTOR ( 'NONE', #115032, 1000.000000000000000 ) ;
#131884 = EDGE_CURVE ( 'NONE', #66775, #194152, #23361, .T. ) ;
#131886 = CARTESIAN_POINT ( 'NONE',  ( 18.49999999999999289, 15.53922597307774822, -223.0482397989536310 ) ) ;
#131885 = DIRECTION ( 'NONE',  ( 0.000000000000000000, 0.000000000000000000, -1.000000000000000000 ) ) ;
#131887 = AXIS2_PLACEMENT_3D ( 'NONE', #211193, #191666, #173405 ) ;
#131888 = EDGE_CURVE ( 'NONE', #108252, #226867, #83622, .T. ) ;
#131890 = ORIENTED_EDGE ( 'NONE', *, *, #71450, .F. ) ;
#131889 = CARTESIAN_POINT ( 'NONE',  ( -16.89146115310545682, 9.951443245667611848, -154.8548224189542566 ) ) ;
#131891 = AXIS2_PLACEMENT_3D ( 'NONE', #204579, #66366, #5069 ) ;
#131892 = EDGE_LOOP ( 'NONE', ( #123169, #223672, #173923, #45374 ) ) ;
#131893 = CARTESIAN_POINT ( 'NONE',  ( -22.39999999999999858, 65.19201463318205469, -243.3742797652979561 ) ) ;
#131894 = VERTEX_POINT ( 'NONE', #58581 ) ;
#131895 = CARTESIAN_POINT ( 'NONE',  ( 18.59999999999999076, 69.55000000001187743, -93.00608031408432907 ) ) ;
#131896 = ORIENTED_EDGE ( 'NONE', *, *, #244932, .T. ) ;
#131897 = AXIS2_PLACEMENT_3D ( 'NONE', #118163, #79001, #197683 ) ;
#131899 = EDGE_CURVE ( 'NONE', #24117, #97198, #221505, .T. ) ;
#131898 = CARTESIAN_POINT ( 'NONE',  ( -18.49999999999999289, -9.419084502802128611, -107.3299078070254069 ) ) ;
#131900 = LINE ( 'NONE', #231026, #110017 ) ;
#131901 = VERTEX_POINT ( 'NONE', #122435 ) ;
#131902 = DIRECTION ( 'NONE',  ( 1.000000000000000000, -2.952720810173289112E-16, -2.061873921506763405E-30 ) ) ;
#131903 = PRODUCT_DEFINITION_CONTEXT ( 'detailed design', #130817, 'design' ) ;
#131904 = EDGE_CURVE ( 'NONE', #257751, #225759, #179851, .T. ) ;
#131905 = AXIS2_PLACEMENT_3D ( 'NONE', #116358, #195899, #17257 ) ;
#131906 = AXIS2_PLACEMENT_3D ( 'NONE', #121785, #5639, #180460 ) ;
#131907 = DIRECTION ( 'NONE',  ( 0.000000000000000000, -1.000000000000000000, 0.000000000000000000 ) ) ;
#131908 = AXIS2_PLACEMENT_3D ( 'NONE', #195055, #239301, #157221 ) ;
#131909 = AXIS2_PLACEMENT_3D ( 'NONE', #108326, #9215, #168341 ) ;
#131910 = ORIENTED_EDGE ( 'NONE', *, *, #33601, .T. ) ;
#131911 = ORIENTED_EDGE ( 'NONE', *, *, #166895, .F. ) ;
#131912 = CARTESIAN_POINT ( 'NONE',  ( 18.39999999999999858, -9.519327731081283162, -107.4729763765593589 ) ) ;
#131913 = ORIENTED_EDGE ( 'NONE', *, *, #75022, .T. ) ;
#131915 = EDGE_CURVE ( 'NONE', #2887, #3181, #46238, .T. ) ;
#131914 = CARTESIAN_POINT ( 'NONE',  ( -13.40000000000000213, -8.250000000000007105, 12.40000000000000391 ) ) ;
#131916 = ORIENTED_EDGE ( 'NONE', *, *, #256781, .T. ) ;
#131917 = ORIENTED_EDGE ( 'NONE', *, *, #86220, .T. ) ;
#131918 = ORIENTED_EDGE ( 'NONE', *, *, #177473, .F. ) ;
#131919 = CARTESIAN_POINT ( 'NONE',  ( 21.14999999999999858, 11.21344753582741127, -211.1973313526253833 ) ) ;
#131920 = EDGE_LOOP ( 'NONE', ( #180317, #115899, #1720, #114781 ) ) ;
#131923 = ORIENTED_EDGE ( 'NONE', *, *, #129473, .F. ) ;
#131922 = ORIENTED_EDGE ( 'NONE', *, *, #231621, .T. ) ;
#131921 = DIRECTION ( 'NONE',  ( -1.000000000000000000, -0.000000000000000000, 0.000000000000000000 ) ) ;
#131924 = TOROIDAL_SURFACE ( 'NONE', #198555, 0.2000000000000000111, 0.1000000000000000056 ) ;
#131925 = CARTESIAN_POINT ( 'NONE',  ( -20.94999999999999929, 76.00000000001237765, -170.0231074845243597 ) ) ;
#131926 = AXIS2_PLACEMENT_3D ( 'NONE', #134265, #213824, #80708 ) ;
#131927 = CIRCLE ( 'NONE', #23639, 0.1000000000000028644 ) ;
#131928 = ORIENTED_EDGE ( 'NONE', *, *, #198714, .F. ) ;
#131929 = EDGE_CURVE ( 'NONE', #187169, #152529, #245987, .T. ) ;
#131930 = AXIS2_PLACEMENT_3D ( 'NONE', #50043, #249548, #70929 ) ;
#131931 = DIRECTION ( 'NONE',  ( -0.000000000000000000, -6.982962677686266711E-15, 1.000000000000000000 ) ) ;
#131932 = ORIENTED_EDGE ( 'NONE', *, *, #170528, .T. ) ;
#131933 = DIRECTION ( 'NONE',  ( 0.000000000000000000, 0.2617529984165032908, 0.9651348961777156399 ) ) ;
#131935 = ORIENTED_EDGE ( 'NONE', *, *, #231145, .T. ) ;
#131934 = DIRECTION ( 'NONE',  ( -1.000000000000000000, 0.000000000000000000, 0.000000000000000000 ) ) ;
#131936 = CARTESIAN_POINT ( 'NONE',  ( 23.24999999999999289, 11.75000000001116263, -122.2500000000000284 ) ) ;
#131937 = ORIENTED_EDGE ( 'NONE', *, *, #160132, .T. ) ;
#131938 = DIRECTION ( 'NONE',  ( 1.000000000000000000, 0.000000000000000000, -0.000000000000000000 ) ) ;
#131939 = DIRECTION ( 'NONE',  ( 0.000000000000000000, 6.982962677686266711E-15, -1.000000000000000000 ) ) ;
#131940 = ORIENTED_EDGE ( 'NONE', *, *, #28964, .T. ) ;
#131941 = DIRECTION ( 'NONE',  ( 2.952720810173289112E-16, 1.000000000000000000, 6.530723674265620862E-15 ) ) ;
#131942 = ORIENTED_EDGE ( 'NONE', *, *, #207887, .T. ) ;
#131944 = ORIENTED_EDGE ( 'NONE', *, *, #13473, .F. ) ;
#131943 = CARTESIAN_POINT ( 'NONE',  ( -22.39999999999999858, 76.00000000001222134, -148.1726782920690937 ) ) ;
#131945 = DIRECTION ( 'NONE',  ( 1.000000000000000000, 0.000000000000000000, 0.000000000000000000 ) ) ;
#131947 = ORIENTED_EDGE ( 'NONE', *, *, #204216, .T. ) ;
#131946 = ORIENTED_EDGE ( 'NONE', *, *, #125325, .T. ) ;
#131948 = ORIENTED_EDGE ( 'NONE', *, *, #106870, .F. ) ;
#131949 = CARTESIAN_POINT ( 'NONE',  ( 23.15000000000000213, 20.40049075128452216, -254.1715885023028250 ) ) ;
#131950 = ORIENTED_EDGE ( 'NONE', *, *, #206835, .F. ) ;
#131951 = VERTEX_POINT ( 'NONE', #100269 ) ;
#131952 = DIRECTION ( 'NONE',  ( -0.000000000000000000, 0.4791956752371485107, 0.8777080977375185666 ) ) ;
#131953 = ORIENTED_EDGE ( 'NONE', *, *, #109596, .T. ) ;
#131954 = LINE ( 'NONE', #232368, #239803 ) ;
#131955 = AXIS2_PLACEMENT_3D ( 'NONE', #132736, #177012, #135266 ) ;
#131956 = DIRECTION ( 'NONE',  ( 0.000000000000000000, 0.2128009952263602289, -0.9770955615653316162 ) ) ;
#131957 = ORIENTED_EDGE ( 'NONE', *, *, #73558, .F. ) ;
#131958 = ADVANCED_FACE ( 'NONE', ( #97696 ), #40365, .T. ) ;
#131959 = EDGE_LOOP ( 'NONE', ( #20748, #97163, #10392, #173112 ) ) ;
#131960 = AXIS2_PLACEMENT_3D ( 'NONE', #75061, #133711, #136253 ) ;
#131961 = LINE ( 'NONE', #134511, #71477 ) ;
#131962 = ORIENTED_EDGE ( 'NONE', *, *, #124201, .F. ) ;
#131963 = CIRCLE ( 'NONE', #140325, 0.09999999999999939493 ) ;
#131964 = CIRCLE ( 'NONE', #69632, 12.97499999999999964 ) ;
#131965 = AXIS2_PLACEMENT_3D ( 'NONE', #96758, #101897, #116371 ) ;
#131966 = DIRECTION ( 'NONE',  ( -0.000000000000000000, -0.000000000000000000, 1.000000000000000000 ) ) ;
#131967 = TOROIDAL_SURFACE ( 'NONE', #165288, 4.099999999999999645, 0.1000000000000000056 ) ;
#131968 = ORIENTED_EDGE ( 'NONE', *, *, #69669, .F. ) ;
#131969 = ORIENTED_EDGE ( 'NONE', *, *, #156283, .F. ) ;
#131970 = EDGE_CURVE ( 'NONE', #116815, #104317, #187740, .T. ) ;
#131971 = CYLINDRICAL_SURFACE ( 'NONE', #83586, 12.87499999999999822 ) ;
#131972 = AXIS2_PLACEMENT_3D ( 'NONE', #60843, #98655, #62148 ) ;
#131974 = EDGE_LOOP ( 'NONE', ( #38959, #98577, #126516, #41297 ) ) ;
#131973 = DIRECTION ( 'NONE',  ( 1.000000000000000000, 0.000000000000000000, 0.000000000000000000 ) ) ;
#131975 = CARTESIAN_POINT ( 'NONE',  ( -23.25000000000000000, -1.164121893230052995, -74.91484808557160591 ) ) ;
#131976 = FACE_OUTER_BOUND ( 'NONE', #66417, .T. ) ;
#131977 = CARTESIAN_POINT ( 'NONE',  ( -20.64999999999999858, 4.350000000011156054, -188.7499999999999716 ) ) ;
#131978 = CARTESIAN_POINT ( 'NONE',  ( -33.72168855820451938, 66.05000000001223270, -149.1731074845243654 ) ) ;
#131979 = EDGE_CURVE ( 'NONE', #236913, #241424, #116991, .T. ) ;
#131980 = DIRECTION ( 'NONE',  ( 0.000000000000000000, -0.9999176327611369874, 0.01283462868041984617 ) ) ;
#131981 = CARTESIAN_POINT ( 'NONE',  ( 21.05000000000000071, 76.00000000001192291, -105.0231074845243029 ) ) ;
#131982 = DIRECTION ( 'NONE',  ( -1.000000000000000000, 0.000000000000000000, 0.000000000000000000 ) ) ;
#131983 = CARTESIAN_POINT ( 'NONE',  ( 18.49362639424868604, 38.16301648980600447, -261.0688944849867426 ) ) ;
#131984 = DIRECTION ( 'NONE',  ( -2.952720810173289112E-16, 1.000000000000000000, -0.000000000000000000 ) ) ;
#131986 = EDGE_CURVE ( 'NONE', #81658, #59275, #192024, .T. ) ;
#131985 = CIRCLE ( 'NONE', #15683, 0.09999999999999892308 ) ;
#131987 = VERTEX_POINT ( 'NONE', #98976 ) ;
#131988 = CIRCLE ( 'NONE', #156959, 0.1000000000000028644 ) ;
#131989 = EDGE_CURVE ( 'NONE', #257935, #99184, #17052, .T. ) ;
#131992 = ORIENTED_EDGE ( 'NONE', *, *, #37492, .T. ) ;
#131991 = VERTEX_POINT ( 'NONE', #143268 ) ;
#131990 = CIRCLE ( 'NONE', #27977, 0.09999999999998802902 ) ;
#131993 = ORIENTED_EDGE ( 'NONE', *, *, #58508, .T. ) ;
#131994 = ADVANCED_FACE ( 'NONE', ( #177302 ), #141922, .T. ) ;
#131995 = VECTOR ( 'NONE', #115183, 1000.000000000000000 ) ;
#131996 = CARTESIAN_POINT ( 'NONE',  ( 23.14999999999999503, 6.650000000011155876, -146.1500000000000341 ) ) ;
#131997 = DIRECTION ( 'NONE',  ( 0.000000000000000000, 0.000000000000000000, -1.000000000000000000 ) ) ;
#131998 = ADVANCED_FACE ( 'NONE', ( #121182 ), #200689, .F. ) ;
#131999 = AXIS2_PLACEMENT_3D ( 'NONE', #77155, #120184, #155460 ) ;
#132001 = CARTESIAN_POINT ( 'NONE',  ( 21.10257677756356998, 1.500471753121898510, -230.6894370601294497 ) ) ;
#132000 = CARTESIAN_POINT ( 'NONE',  ( -18.59999999999999787, 64.35000000001222986, -148.6731074845244507 ) ) ;
#132002 = EDGE_LOOP ( 'NONE', ( #3756, #44237, #68859, #176548, #227015 ) ) ;
#132003 = ORIENTED_EDGE ( 'NONE', *, *, #96629, .F. ) ;
#132004 = CARTESIAN_POINT ( 'NONE',  ( 18.51565452909389009, -9.352859338825282975, -40.69490932123330396 ) ) ;
#132005 = EDGE_CURVE ( 'NONE', #102497, #137660, #118597, .T. ) ;
#132006 = CARTESIAN_POINT ( 'NONE',  ( 18.49999999999999289, 6.450000000011156587, -155.7499999999999716 ) ) ;
#132007 = DIRECTION ( 'NONE',  ( 0.000000000000000000, 0.000000000000000000, 1.000000000000000000 ) ) ;
#132008 = ORIENTED_EDGE ( 'NONE', *, *, #100793, .T. ) ;
#132009 = VERTEX_POINT ( 'NONE', #168015 ) ;
#132010 = AXIS2_PLACEMENT_3D ( 'NONE', #5279, #161845, #64002 ) ;
#132011 = DIRECTION ( 'NONE',  ( 1.000000000000000000, 0.000000000000000000, 0.000000000000000000 ) ) ;
#132012 = CIRCLE ( 'NONE', #102758, 0.09999999999999939493 ) ;
#132013 = CARTESIAN_POINT ( 'NONE',  ( 21.15000000000005542, 74.63923853664559260, -43.99645795275012006 ) ) ;
#132015 = ORIENTED_EDGE ( 'NONE', *, *, #176999, .T. ) ;
#132014 = CYLINDRICAL_SURFACE ( 'NONE', #89617, 0.1000000000000028644 ) ;
#132016 = SPHERICAL_SURFACE ( 'NONE', #52740, 0.1000000000000000056 ) ;
#132017 = CARTESIAN_POINT ( 'NONE',  ( -20.94999999999999929, 74.63912941282028157, -161.9501095574334215 ) ) ;
#132018 = CARTESIAN_POINT ( 'NONE',  ( 21.05000000000000071, -11.29603075033528192, -30.45210084033612929 ) ) ;
#132019 = CARTESIAN_POINT ( 'NONE',  ( -20.90000000000000213, 1.212568896937007645, -7.900000000000000355 ) ) ;
#132020 = ORIENTED_EDGE ( 'NONE', *, *, #185338, .F. ) ;
#132021 = CARTESIAN_POINT ( 'NONE',  ( 18.59999999999999076, -1.835859311432481045, -179.0044391687985410 ) ) ;
#132022 = DIRECTION ( 'NONE',  ( 1.000000000000000000, 1.541880601228652843E-16, 2.878400969107353907E-16 ) ) ;
#132024 = EDGE_CURVE ( 'NONE', #633, #70740, #207110, .T. ) ;
#132023 = CARTESIAN_POINT ( 'NONE',  ( -23.25000000000000000, 43.08613539620618837, -254.3146655184800409 ) ) ;
#132026 = DIRECTION ( 'NONE',  ( 0.000000000000000000, 0.9126074666063660468, 0.4088369013363524762 ) ) ;
#132025 = CARTESIAN_POINT ( 'NONE',  ( -16.77683809663752257, 66.05416425680790837, -123.8591584654201512 ) ) ;
#132027 = CARTESIAN_POINT ( 'NONE',  ( -22.10000000000000142, -11.65000000000000036, -15.00000000000000000 ) ) ;
#132028 = DIRECTION ( 'NONE',  ( -1.000000000000000000, 7.304098846218134667E-16, 5.100424963727256530E-30 ) ) ;
#132029 = AXIS2_PLACEMENT_3D ( 'NONE', #46019, #61740, #85114 ) ;
#132030 = CARTESIAN_POINT ( 'NONE',  ( 18.59999999999999432, 5.699452464332755319, -87.95772604343019907 ) ) ;
#132031 = DIRECTION ( 'NONE',  ( 1.000000000000000000, -0.000000000000000000, -0.000000000000000000 ) ) ;
#132032 = CARTESIAN_POINT ( 'NONE',  ( -20.54999999999999716, 85.00000000001179501, -79.41707660717668205 ) ) ;
#132033 = ORIENTED_EDGE ( 'NONE', *, *, #63569, .F. ) ;
#132034 = ORIENTED_EDGE ( 'NONE', *, *, #176301, .F. ) ;
#132035 = VECTOR ( 'NONE', #70082, 1000.000000000000114 ) ;
#132036 = ORIENTED_EDGE ( 'NONE', *, *, #54348, .T. ) ;
#132037 = ADVANCED_FACE ( 'NONE', ( #205810 ), #79371, .T. ) ;
#132038 = CARTESIAN_POINT ( 'NONE',  ( 0.8999999999999993561, -8.279289321881350361, 29.97071067811866030 ) ) ;
#132039 = DIRECTION ( 'NONE',  ( -1.000000000000000000, 0.000000000000000000, 0.000000000000000000 ) ) ;
#132040 = ORIENTED_EDGE ( 'NONE', *, *, #165648, .F. ) ;
#132041 = DIRECTION ( 'NONE',  ( 0.000000000000000000, 0.000000000000000000, -1.000000000000000000 ) ) ;
#132042 = VECTOR ( 'NONE', #108801, 1000.000000000000000 ) ;
#132043 = AXIS2_PLACEMENT_3D ( 'NONE', #211484, #228493, #49834 ) ;
#132044 = ORIENTED_EDGE ( 'NONE', *, *, #24282, .T. ) ;
#132045 = SHAPE_REPRESENTATION_RELATIONSHIP ( 'NONE' , 'NONE' ,  #53611, #241103 ) ;
#132046 = CIRCLE ( 'NONE', #202769, 0.09999999999999939493 ) ;
#132047 = AXIS2_PLACEMENT_3D ( 'NONE', #242342, #186233, #47988 ) ;
#132048 = ORIENTED_EDGE ( 'NONE', *, *, #124434, .T. ) ;
#132049 = CARTESIAN_POINT ( 'NONE',  ( 21.05000000000000071, 76.02138556594995578, -109.3280685972088691 ) ) ;
#132050 = ORIENTED_EDGE ( 'NONE', *, *, #236537, .T. ) ;
#132051 = AXIS2_PLACEMENT_3D ( 'NONE', #70423, #71689, #190351 ) ;
#132052 = EDGE_CURVE ( 'NONE', #17019, #192537, #244936, .T. ) ;
#132053 = DIRECTION ( 'NONE',  ( 1.000000000000000000, 0.000000000000000000, 0.000000000000000000 ) ) ;
#132054 = CARTESIAN_POINT ( 'NONE',  ( -16.80469485234342741, 30.16733359419953686, -234.7950599053594658 ) ) ;
#132055 = DIRECTION ( 'NONE',  ( 0.000000000000000000, 0.8660254037844420383, -0.4999999999999943379 ) ) ;
#132056 = LINE ( 'NONE', #112507, #79076 ) ;
#132057 = CARTESIAN_POINT ( 'NONE',  ( 23.24999999999999289, 56.06656052939784729, -228.0911609752645290 ) ) ;
#132059 = ORIENTED_EDGE ( 'NONE', *, *, #173309, .F. ) ;
#132058 = CARTESIAN_POINT ( 'NONE',  ( -16.85697194749117145, 29.93552328732817003, -234.7090115389776201 ) ) ;
#132061 = CARTESIAN_POINT ( 'NONE',  ( -22.50000000000000000, 10.71943444926882449, -226.8179467668883547 ) ) ;
#132060 = DIRECTION ( 'NONE',  ( 0.000000000000000000, 0.4088369013361243254, -0.9126074666064684093 ) ) ;
#132062 = CARTESIAN_POINT ( 'NONE',  ( -18.40000000000000568, 64.58541674041244107, -149.1731074845244507 ) ) ;
#132063 = EDGE_CURVE ( 'NONE', #44319, #63693, #196103, .T. ) ;
#132064 = CARTESIAN_POINT ( 'NONE',  ( 12.25000000000000000, 66.65000000001204228, -119.7731074845243739 ) ) ;
#132065 = DIRECTION ( 'NONE',  ( 0.000000000000000000, 1.000000000000000000, 1.321694076934707365E-14 ) ) ;
#132066 = CARTESIAN_POINT ( 'NONE',  ( -21.37071067811865532, 67.92928932189387581, -182.3731074845244393 ) ) ;
#132068 = ORIENTED_EDGE ( 'NONE', *, *, #49358, .T. ) ;
#132067 = CIRCLE ( 'NONE', #73273, 0.1000000000000001860 ) ;
#132069 = AXIS2_PLACEMENT_3D ( 'NONE', #28242, #107740, #81725 ) ;
#132070 = EDGE_CURVE ( 'NONE', #79207, #172948, #84375, .T. ) ;
#132071 = SURFACE_STYLE_USAGE ( .BOTH. , #52516 ) ;
#132072 = FACE_OUTER_BOUND ( 'NONE', #58758, .T. ) ;
#132073 = ADVANCED_FACE ( 'NONE', ( #108003 ), #233531, .T. ) ;
#132074 = ADVANCED_BREP_SHAPE_REPRESENTATION ( '', ( #197609, #2425 ), #27429 ) ;
#132075 = DIRECTION ( 'NONE',  ( 0.000000000000000000, -0.000000000000000000, 1.000000000000000000 ) ) ;
#132076 = EDGE_CURVE ( 'NONE', #227951, #181985, #109266, .T. ) ;
#132077 = VERTEX_POINT ( 'NONE', #149721 ) ;
#132078 = AXIS2_PLACEMENT_3D ( 'NONE', #182772, #82337, #61533 ) ;
#132079 = CARTESIAN_POINT ( 'NONE',  ( 21.05000000000000071, -0.09999999998884338825, -134.0000000000000000 ) ) ;
#132080 = EDGE_CURVE ( 'NONE', #84007, #51091, #17237, .T. ) ;
#132081 = DIRECTION ( 'NONE',  ( -1.000000000000000000, 0.000000000000000000, 0.000000000000000000 ) ) ;
#132082 = DIRECTION ( 'NONE',  ( 0.000000000000000000, 0.000000000000000000, -1.000000000000000000 ) ) ;
#132083 = EDGE_LOOP ( 'NONE', ( #199682, #38699, #36719, #189555 ) ) ;
#132084 = ORIENTED_EDGE ( 'NONE', *, *, #13196, .T. ) ;
#132085 = CARTESIAN_POINT ( 'NONE',  ( 20.95289811251229750, 10.49866850695357989, -207.4146053197192998 ) ) ;
#132086 = CARTESIAN_POINT ( 'NONE',  ( 21.05000000000000071, 76.00000000001213607, -136.5231074845243313 ) ) ;
#132087 = CARTESIAN_POINT ( 'NONE',  ( 21.05000000000000071, 86.52890073500824997, -209.5906233940697234 ) ) ;
#132089 = CARTESIAN_POINT ( 'NONE',  ( -21.52071067811865746, 68.22071067813094203, -157.6731074845243938 ) ) ;
#132088 = LINE ( 'NONE', #211637, #9270 ) ;
#132090 = AXIS2_PLACEMENT_3D ( 'NONE', #48049, #204556, #7654 ) ;
#132091 = AXIS2_PLACEMENT_3D ( 'NONE', #166722, #247510, #246231 ) ;
#132092 = CARTESIAN_POINT ( 'NONE',  ( 20.85000000000000142, 77.36242903720570041, -162.1342262366031548 ) ) ;
#132094 = AXIS2_PLACEMENT_3D ( 'NONE', #39549, #74827, #78621 ) ;
#132093 = DIRECTION ( 'NONE',  ( -0.000000000000000000, 1.000000000000000000, 6.982962677686266711E-15 ) ) ;
#132095 = AXIS2_PLACEMENT_3D ( 'NONE', #190447, #92592, #255477 ) ;
#132096 = CARTESIAN_POINT ( 'NONE',  ( -20.54999999999999716, 68.85000000001151932, -48.37310748452436826 ) ) ;
#132097 = VERTEX_POINT ( 'NONE', #127565 ) ;
#132098 = CARTESIAN_POINT ( 'NONE',  ( -18.34374000495059676, 11.47316190337362940, -191.7499999999999716 ) ) ;
#132099 = ADVANCED_FACE ( 'NONE', ( #166723 ), #187562, .F. ) ;
#132101 = ORIENTED_EDGE ( 'NONE', *, *, #238694, .F. ) ;
#132100 = CARTESIAN_POINT ( 'NONE',  ( -23.15000000000000213, 36.65892442174935439, -249.5511627012433848 ) ) ;
#132102 = CARTESIAN_POINT ( 'NONE',  ( 23.25000000000000000, 6.550000000011156231, -45.85000000000000142 ) ) ;
#132103 = DIRECTION ( 'NONE',  ( -1.000000000000000000, -0.000000000000000000, -0.000000000000000000 ) ) ;
#132105 = CARTESIAN_POINT ( 'NONE',  ( -18.54270223418607699, -0.8403597433258389593, -242.3672582601704164 ) ) ;
#132104 = LINE ( 'NONE', #209070, #229428 ) ;
#132106 = DIRECTION ( 'NONE',  ( 1.000000000000000000, -0.000000000000000000, -0.000000000000000000 ) ) ;
#132107 = EDGE_CURVE ( 'NONE', #175179, #173016, #125386, .T. ) ;
#132108 = CARTESIAN_POINT ( 'NONE',  ( 20.85000000000000142, 11.75000000001115907, -194.2161343370218560 ) ) ;
#132110 = ORIENTED_EDGE ( 'NONE', *, *, #6367, .F. ) ;
#132109 = CARTESIAN_POINT ( 'NONE',  ( 20.85000000000000142, 11.65000000001115943, -167.5000000000000284 ) ) ;
#132111 = DIRECTION ( 'NONE',  ( 1.000000000000000000, 0.000000000000000000, 0.000000000000000000 ) ) ;
#132113 = ADVANCED_FACE ( 'NONE', ( #125008 ), #106694, .F. ) ;
#132112 = CYLINDRICAL_SURFACE ( 'NONE', #191170, 12.87499999999999822 ) ;
#132114 = CARTESIAN_POINT ( 'NONE',  ( 22.59999999999999432, 11.74956712350054744, -66.89914163090132604 ) ) ;
#132115 = EDGE_LOOP ( 'NONE', ( #146424, #138387, #221973, #94541 ) ) ;
#132116 = DIRECTION ( 'NONE',  ( -0.000000000000000000, -0.9770955615653310611, -0.2128009952263620608 ) ) ;
#132117 = ORIENTED_EDGE ( 'NONE', *, *, #84046, .F. ) ;
#132118 = AXIS2_PLACEMENT_3D ( 'NONE', #242516, #183829, #143416 ) ;
#132119 = ADVANCED_FACE ( 'NONE', ( #6317 ), #196272, .T. ) ;
#132121 = VECTOR ( 'NONE', #205187, 1000.000000000000000 ) ;
#132120 = CARTESIAN_POINT ( 'NONE',  ( 18.59999999999999432, -1.162701749926853712, -142.1000000000000227 ) ) ;
#132122 = ORIENTED_EDGE ( 'NONE', *, *, #12069, .F. ) ;
#132123 = PLANE ( 'NONE',  #134394 ) ;
#132124 = EDGE_LOOP ( 'NONE', ( #181170, #173238, #136308, #209853 ) ) ;
#132126 = CARTESIAN_POINT ( 'NONE',  ( 21.00000000000000000, 66.25000000001186606, -90.67310748452437963 ) ) ;
#132125 = AXIS2_PLACEMENT_3D ( 'NONE', #58062, #119355, #240579 ) ;
#132127 = FACE_OUTER_BOUND ( 'NONE', #256165, .T. ) ;
#132128 = DIRECTION ( 'NONE',  ( 0.000000000000000000, -6.938893903907222067E-15, 1.000000000000000000 ) ) ;
#132129 = VERTEX_POINT ( 'NONE', #204519 ) ;
#132130 = LINE ( 'NONE', #34342, #229421 ) ;
#132131 = EDGE_CURVE ( 'NONE', #248722, #137467, #246232, .T. ) ;
#132132 = CARTESIAN_POINT ( 'NONE',  ( -18.59999999999999787, 1.115600667400684642E-11, -100.5000000000000426 ) ) ;
#132133 = LINE ( 'NONE', #35637, #95593 ) ;
#132134 = DIRECTION ( 'NONE',  ( 1.000000000000000000, 0.000000000000000000, 0.000000000000000000 ) ) ;
#132135 = DIRECTION ( 'NONE',  ( 0.000000000000000000, -0.9955484899852801162, 0.09425075112713271475 ) ) ;
#132136 = TOROIDAL_SURFACE ( 'NONE', #111294, 1.900000000000002576, 0.1000000000000000056 ) ;
#132137 = ORIENTED_EDGE ( 'NONE', *, *, #162712, .T. ) ;
#132138 = EDGE_LOOP ( 'NONE', ( #38777, #155883, #24501, #227844 ) ) ;
#132140 = EDGE_LOOP ( 'NONE', ( #30277, #105729, #24737, #111786 ) ) ;
#132139 = CARTESIAN_POINT ( 'NONE',  ( -23.25000000000000000, 85.00000000001179501, -79.41707660717668205 ) ) ;
#132141 = EDGE_LOOP ( 'NONE', ( #202849, #65879, #200863, #65441 ) ) ;
#132142 = DIRECTION ( 'NONE',  ( 0.000000000000000000, -0.000000000000000000, -1.000000000000000000 ) ) ;
#132143 = CARTESIAN_POINT ( 'NONE',  ( -16.87383368123029825, 66.05000000001261640, -190.8731074845244393 ) ) ;
#132144 = CARTESIAN_POINT ( 'NONE',  ( -20.90000000000000213, 0.000000000000000000, 0.000000000000000000 ) ) ;
#132145 = CARTESIAN_POINT ( 'NONE',  ( -20.64999999999999858, 74.00000000001156764, -56.29848556176223440 ) ) ;
#132146 = ORIENTED_EDGE ( 'NONE', *, *, #218457, .F. ) ;
#132147 = CARTESIAN_POINT ( 'NONE',  ( -23.25000000000000355, 65.95000000001152785, -48.77310748452439526 ) ) ;
#132148 = CARTESIAN_POINT ( 'NONE',  ( 18.47149038651512143, -9.671457157995547504, -140.6727863347384186 ) ) ;
#132149 = ORIENTED_EDGE ( 'NONE', *, *, #131285, .T. ) ;
#132150 = ADVANCED_FACE ( 'NONE', ( #234354 ), #96297, .T. ) ;
#132152 = ORIENTED_EDGE ( 'NONE', *, *, #132614, .F. ) ;
#132151 = CARTESIAN_POINT ( 'NONE',  ( 18.49999999999998934, 6.550000000011156231, -54.65000000000000568 ) ) ;
#132153 = CYLINDRICAL_SURFACE ( 'NONE', #144371, 0.09999999999998898659 ) ;
#132154 = CARTESIAN_POINT ( 'NONE',  ( -16.87331047859649757, 9.950000000011138823, -54.35000000000000142 ) ) ;
#132155 = CIRCLE ( 'NONE', #7227, 11.64999999999999325 ) ;
#132156 = EDGE_CURVE ( 'NONE', #83407, #160572, #83803, .T. ) ;
#132157 = CIRCLE ( 'NONE', #186331, 0.09999999999999799327 ) ;
#132158 = ORIENTED_EDGE ( 'NONE', *, *, #243323, .T. ) ;
#132159 = VECTOR ( 'NONE', #119827, 1000.000000000000000 ) ;
#132160 = ORIENTED_EDGE ( 'NONE', *, *, #21735, .F. ) ;
#132162 = DIRECTION ( 'NONE',  ( 0.000000000000000000, 0.000000000000000000, 1.000000000000000000 ) ) ;
#132161 = PRODUCT_DEFINITION_FORMATION_WITH_SPECIFIED_SOURCE ( 'ANY', '', #247102, .NOT_KNOWN. ) ;
#132163 = EDGE_CURVE ( 'NONE', #80026, #60977, #112892, .T. ) ;
#132164 = DIRECTION ( 'NONE',  ( 1.836970198721029934E-16, 1.000000000000000000, 6.982962677686266711E-15 ) ) ;
#132167 = EDGE_CURVE ( 'NONE', #159251, #126285, #191421, .T. ) ;
#132166 = ORIENTED_EDGE ( 'NONE', *, *, #120242, .F. ) ;
#132165 = AXIS2_PLACEMENT_3D ( 'NONE', #193564, #169213, #57874 ) ;
#132168 = PLANE ( 'NONE',  #343 ) ;
#132169 = AXIS2_PLACEMENT_3D ( 'NONE', #33629, #193948, #15319 ) ;
#132170 = DIRECTION ( 'NONE',  ( -0.000000000000000000, 0.000000000000000000, -1.000000000000000000 ) ) ;
#132171 = DIRECTION ( 'NONE',  ( -1.836970198721029934E-16, 1.000000000000000000, 0.000000000000000000 ) ) ;
#132172 = AXIS2_PLACEMENT_3D ( 'NONE', #136584, #196569, #97444 ) ;
#132173 = EDGE_CURVE ( 'NONE', #206325, #46365, #130120, .T. ) ;
#132175 = EDGE_CURVE ( 'NONE', #248318, #57247, #229602, .T. ) ;
#132174 = CIRCLE ( 'NONE', #32239, 11.64999999999999325 ) ;
#132176 = VERTEX_POINT ( 'NONE', #253913 ) ;
#132177 = DIRECTION ( 'NONE',  ( -0.000000000000000000, 1.000000000000000000, 0.000000000000000000 ) ) ;
#132178 = CIRCLE ( 'NONE', #11375, 0.1000000000000019901 ) ;
#132179 = ORIENTED_EDGE ( 'NONE', *, *, #82692, .T. ) ;
#132180 = VECTOR ( 'NONE', #251813, 1000.000000000000000 ) ;
#132181 = CARTESIAN_POINT ( 'NONE',  ( -18.46902351632711614, -9.509470118669717920, -174.4864539342572698 ) ) ;
#132182 = CARTESIAN_POINT ( 'NONE',  ( 18.59999999999999787, -11.74999999998883737, -91.85000000000003695 ) ) ;
#132184 = EDGE_LOOP ( 'NONE', ( #104630, #187579, #122945, #108787 ) ) ;
#132183 = CARTESIAN_POINT ( 'NONE',  ( -20.64999999999999858, 7.150000000011155876, -121.6500000000000341 ) ) ;
#132185 = CYLINDRICAL_SURFACE ( 'NONE', #244949, 0.09999999999999939493 ) ;
#132187 = VECTOR ( 'NONE', #88578, 1000.000000000000114 ) ;
#132186 = CARTESIAN_POINT ( 'NONE',  ( 21.07189867249812210, 65.27501972991842649, -57.31065604224765764 ) ) ;
#132188 = FACE_OUTER_BOUND ( 'NONE', #165263, .T. ) ;
#132189 = CARTESIAN_POINT ( 'NONE',  ( -16.94226253665225101, 9.949999999999983302, -20.55326540438422711 ) ) ;
#132190 = DIRECTION ( 'NONE',  ( 0.000000000000000000, 0.4930308989875575865, 0.8700118002898125091 ) ) ;
#132191 = CARTESIAN_POINT ( 'NONE',  ( -18.59999999999999787, 64.35000000001198828, -115.1731074845243796 ) ) ;
#132193 = ADVANCED_FACE ( 'NONE', ( #212252 ), #56231, .T. ) ;
#132192 = DIRECTION ( 'NONE',  ( 0.000000000000000000, 0.8814952561688476074, -0.4721928772777262417 ) ) ;
#132195 = ORIENTED_EDGE ( 'NONE', *, *, #215826, .F. ) ;
#132194 = DIRECTION ( 'NONE',  ( -1.000000000000000000, 2.952720810173289112E-16, 2.061873921506763405E-30 ) ) ;
#132196 = ADVANCED_FACE ( 'NONE', ( #93566 ), #131404, .F. ) ;
#132197 = AXIS2_PLACEMENT_3D ( 'NONE', #44141, #79389, #158977 ) ;
#132198 = AXIS2_PLACEMENT_3D ( 'NONE', #71465, #50567, #32348 ) ;
#132199 = CARTESIAN_POINT ( 'NONE',  ( 21.14999999999999858, 64.35000000001245724, -181.7731074845244450 ) ) ;
#132200 = PLANE ( 'NONE',  #215381 ) ;
#132202 = EDGE_CURVE ( 'NONE', #148979, #206404, #129636, .T. ) ;
#132201 = DIRECTION ( 'NONE',  ( -1.000000000000000000, -0.000000000000000000, 0.000000000000000000 ) ) ;
#132203 = ORIENTED_EDGE ( 'NONE', *, *, #256353, .T. ) ;
#132204 = AXIS2_PLACEMENT_3D ( 'NONE', #103125, #203533, #181420 ) ;
#132205 = DIRECTION ( 'NONE',  ( -1.000000000000000000, 0.000000000000000000, 0.000000000000000000 ) ) ;
#132206 = AXIS2_PLACEMENT_3D ( 'NONE', #238799, #219216, #229511 ) ;
#132207 = DIRECTION ( 'NONE',  ( 1.000000000000000000, -0.000000000000000000, -0.000000000000000000 ) ) ;
#132208 = EDGE_CURVE ( 'NONE', #231817, #64423, #252629, .T. ) ;
#132210 = VERTEX_POINT ( 'NONE', #114420 ) ;
#132209 = VECTOR ( 'NONE', #118627, 1000.000000000000000 ) ;
#132211 = DIRECTION ( 'NONE',  ( 1.000000000000000000, -3.265361837132813093E-16, -2.280189983783949500E-30 ) ) ;
#132213 = CARTESIAN_POINT ( 'NONE',  ( -22.40000000000000568, 59.71212129423881976, -233.8158665866019987 ) ) ;
#132212 = CIRCLE ( 'NONE', #78229, 0.2000000000000005107 ) ;
#132214 = ORIENTED_EDGE ( 'NONE', *, *, #5849, .T. ) ;
#132215 = DIRECTION ( 'NONE',  ( 0.7071067811865127117, 0.7071067811865821007, 0.000000000000000000 ) ) ;
#132216 = ORIENTED_EDGE ( 'NONE', *, *, #143468, .T. ) ;
#132217 = EDGE_CURVE ( 'NONE', #8209, #96344, #104657, .T. ) ;
#132218 = CARTESIAN_POINT ( 'NONE',  ( 21.05000012384953223, 65.37127970113643016, -124.3451301544889702 ) ) ;
#132220 = VERTEX_POINT ( 'NONE', #150530 ) ;
#132219 = CARTESIAN_POINT ( 'NONE',  ( -20.64999999999999858, 74.07476635515278929, -190.7928639513982318 ) ) ;
#132221 = AXIS2_PLACEMENT_3D ( 'NONE', #185483, #207632, #70700 ) ;
#132222 = DIRECTION ( 'NONE',  ( -0.000000000000000000, -6.982962677686266711E-15, 1.000000000000000000 ) ) ;
#132223 = ORIENTED_EDGE ( 'NONE', *, *, #24345, .F. ) ;
#132224 = CARTESIAN_POINT ( 'NONE',  ( -18.40000000000000213, 11.47316190337364183, -57.67405393319205587 ) ) ;
#132225 = TOROIDAL_SURFACE ( 'NONE', #19822, 0.2000000000000000111, 0.1000000000000000056 ) ;
#132226 = CIRCLE ( 'NONE', #36394, 0.09999999999999986677 ) ;
#132227 = VERTEX_POINT ( 'NONE', #50125 ) ;
#132229 = ORIENTED_EDGE ( 'NONE', *, *, #242926, .T. ) ;
#132228 = ORIENTED_EDGE ( 'NONE', *, *, #210180, .F. ) ;
#132230 = CARTESIAN_POINT ( 'NONE',  ( 20.85000000000000142, -1.851617760457748618, -112.1031897196037050 ) ) ;
#132231 = AXIS2_PLACEMENT_3D ( 'NONE', #219711, #38525, #101007 ) ;
#132233 = ORIENTED_EDGE ( 'NONE', *, *, #89728, .T. ) ;
#132232 = CARTESIAN_POINT ( 'NONE',  ( 21.05000000000000071, -11.48912529306489994, -63.89999999999999858 ) ) ;
#132234 = CARTESIAN_POINT ( 'NONE',  ( 20.93302460841142931, 65.68434038414338261, -63.98668807260656166 ) ) ;
#132235 = VERTEX_POINT ( 'NONE', #149258 ) ;
#132236 = CIRCLE ( 'NONE', #223802, 11.80000000000000426 ) ;
#132237 = ORIENTED_EDGE ( 'NONE', *, *, #44138, .T. ) ;
#132238 = CARTESIAN_POINT ( 'NONE',  ( -20.00857864376270001, 66.65000000001253966, -182.2731074845244166 ) ) ;
#132239 = DIRECTION ( 'NONE',  ( 0.000000000000000000, -1.000000000000000000, -6.982962677686265922E-15 ) ) ;
#132240 = DIRECTION ( 'NONE',  ( 0.000000000000000000, 0.000000000000000000, 1.000000000000000000 ) ) ;
#132241 = VERTEX_POINT ( 'NONE', #90532 ) ;
#132242 = CARTESIAN_POINT ( 'NONE',  ( -18.59117750673697245, 65.66751761918692409, -130.9282609406112670 ) ) ;
#132243 = CARTESIAN_POINT ( 'NONE',  ( -18.43473496883415663, -9.494952410988144464, -74.04587157222827898 ) ) ;
#132244 = CARTESIAN_POINT ( 'NONE',  ( -18.60000000000000142, -8.150000000000005684, 32.89999999999999858 ) ) ;
#132245 = AXIS2_PLACEMENT_3D ( 'NONE', #154610, #214541, #55438 ) ;
#132246 = ORIENTED_EDGE ( 'NONE', *, *, #29802, .F. ) ;
#132247 = CARTESIAN_POINT ( 'NONE',  ( -21.55000000000000426, 7.708578643773852157, -45.85000000000000142 ) ) ;
#132248 = CARTESIAN_POINT ( 'NONE',  ( -18.50000000000000000, 73.32445833535280144, -249.6821150215233160 ) ) ;
#132249 = FACE_OUTER_BOUND ( 'NONE', #111704, .T. ) ;
#132250 = EDGE_LOOP ( 'NONE', ( #119118, #214513, #156732, #143463 ) ) ;
#132251 = ORIENTED_EDGE ( 'NONE', *, *, #235445, .F. ) ;
#132252 = FACE_OUTER_BOUND ( 'NONE', #61071, .T. ) ;
#132254 = ORIENTED_EDGE ( 'NONE', *, *, #211364, .T. ) ;
#132253 = AXIS2_PLACEMENT_3D ( 'NONE', #245376, #27640, #146249 ) ;
#132255 = DIRECTION ( 'NONE',  ( 0.000000000000000000, 0.9126074666063769270, 0.4088369013363280513 ) ) ;
#132256 = CARTESIAN_POINT ( 'NONE',  ( -20.94999999999999929, 87.65000000001192859, -106.0231074845242176 ) ) ;
#132257 = ORIENTED_EDGE ( 'NONE', *, *, #16329, .F. ) ;
#132258 = ORIENTED_EDGE ( 'NONE', *, *, #140460, .T. ) ;
#132259 = DIRECTION ( 'NONE',  ( 1.000000000000000000, 0.000000000000000000, 0.000000000000000000 ) ) ;
#132260 = CARTESIAN_POINT ( 'NONE',  ( -20.94999999999999929, -11.48912529306489994, -164.4000000000000057 ) ) ;
#132261 = ORIENTED_EDGE ( 'NONE', *, *, #108995, .F. ) ;
#132262 = ORIENTED_EDGE ( 'NONE', *, *, #160971, .F. ) ;
#132263 = LINE ( 'NONE', #12344, #156240 ) ;
#132264 = CARTESIAN_POINT ( 'NONE',  ( -23.25000000000000355, 64.25000000001233502, -160.7731074845244450 ) ) ;
#132265 = ORIENTED_EDGE ( 'NONE', *, *, #54609, .T. ) ;
#132266 = ADVANCED_FACE ( 'NONE', ( #5851 ), #137991, .F. ) ;
#132267 = CIRCLE ( 'NONE', #174013, 0.09999999999998898659 ) ;
#132268 = VECTOR ( 'NONE', #128233, 1000.000000000000000 ) ;
#132269 = AXIS2_PLACEMENT_3D ( 'NONE', #125965, #68578, #6013 ) ;
#132270 = ORIENTED_EDGE ( 'NONE', *, *, #172059, .T. ) ;
#132271 = CARTESIAN_POINT ( 'NONE',  ( -20.85000000000000142, 77.36242903720570041, -162.1342262366031548 ) ) ;
#132272 = CARTESIAN_POINT ( 'NONE',  ( -20.94999999999999929, 70.10000000001213039, -126.3040077198679398 ) ) ;
#132273 = DIRECTION ( 'NONE',  ( -1.000000000000000000, 3.151514657663852580E-16, -8.547182517843351137E-17 ) ) ;
#132275 = ORIENTED_EDGE ( 'NONE', *, *, #48208, .T. ) ;
#132274 = FACE_OUTER_BOUND ( 'NONE', #169664, .T. ) ;
#132276 = LINE ( 'NONE', #17465, #232620 ) ;
#132277 = EDGE_CURVE ( 'NONE', #220426, #14895, #71401, .T. ) ;
#132278 = DIRECTION ( 'NONE',  ( 2.952720810173289112E-16, -1.000000000000000000, 0.000000000000000000 ) ) ;
#132279 = CARTESIAN_POINT ( 'NONE',  ( 18.50000000000000000, 85.50000000001189449, -95.99103808782457747 ) ) ;
#132282 = CARTESIAN_POINT ( 'NONE',  ( 20.94999999999999929, 88.41227409416215721, -173.0231074845242745 ) ) ;
#132281 = AXIS2_PLACEMENT_3D ( 'NONE', #257870, #121011, #156293 ) ;
#132280 = DIRECTION ( 'NONE',  ( -1.000000000000000000, -0.000000000000000000, -0.000000000000000000 ) ) ;
#132283 = CARTESIAN_POINT ( 'NONE',  ( 20.94999999999999929, 68.87972903831482085, -166.3635444426850825 ) ) ;
#132284 = CARTESIAN_POINT ( 'NONE',  ( -17.29158576265544056, 65.63525233399367664, -58.10586572931656946 ) ) ;
#132285 = AXIS2_PLACEMENT_3D ( 'NONE', #134035, #250148, #173227 ) ;
#132286 = DIRECTION ( 'NONE',  ( 1.000000000000000000, 0.000000000000000000, 0.000000000000000000 ) ) ;
#132287 = DIRECTION ( 'NONE',  ( 0.000000000000000000, 0.000000000000000000, -1.000000000000000000 ) ) ;
#132288 = ORIENTED_EDGE ( 'NONE', *, *, #24096, .F. ) ;
#132289 = AXIS2_PLACEMENT_3D ( 'NONE', #244426, #87896, #89202 ) ;
#132290 = EDGE_CURVE ( 'NONE', #156141, #208842, #226162, .T. ) ;
#132291 = ORIENTED_EDGE ( 'NONE', *, *, #234994, .F. ) ;
#132292 = EDGE_CURVE ( 'NONE', #168738, #136655, #158886, .T. ) ;
#132293 = CARTESIAN_POINT ( 'NONE',  ( -20.64999999999999858, 68.85000000001222986, -148.8731074845244109 ) ) ;
#132294 = ADVANCED_FACE ( 'NONE', ( #106232 ), #26744, .F. ) ;
#132295 = CARTESIAN_POINT ( 'NONE',  ( 23.14999999999999503, 11.65000000001116298, -88.75000000000004263 ) ) ;
#132296 = ORIENTED_EDGE ( 'NONE', *, *, #140396, .F. ) ;
#132297 = SHAPE_REPRESENTATION_RELATIONSHIP ( 'NONE' , 'NONE' ,  #26974, #13839 ) ;
#132298 = CARTESIAN_POINT ( 'NONE',  ( -16.88853107394619357, 63.08565309574376556, -213.1245576704256735 ) ) ;
#132299 = CIRCLE ( 'NONE', #28299, 0.09999999999999510669 ) ;
#132300 = FACE_OUTER_BOUND ( 'NONE', #169216, .T. ) ;
#132301 = ORIENTED_EDGE ( 'NONE', *, *, #244179, .F. ) ;
#132302 = EDGE_LOOP ( 'NONE', ( #232830, #182642, #52058, #190209 ) ) ;
#132303 = VECTOR ( 'NONE', #119409, 1000.000000000000000 ) ;
#132304 = DIRECTION ( 'NONE',  ( 0.000000000000000000, 0.000000000000000000, 1.000000000000000000 ) ) ;
#132305 = DIRECTION ( 'NONE',  ( 1.000000000000000000, 0.000000000000000000, 0.000000000000000000 ) ) ;
#132306 = VERTEX_POINT ( 'NONE', #185793 ) ;
#132307 = EDGE_CURVE ( 'NONE', #75643, #13417, #249635, .T. ) ;
#132308 = DIRECTION ( 'NONE',  ( -4.448008912761042820E-16, -1.000000000000000000, -7.116814260417668513E-15 ) ) ;
#132310 = ORIENTED_EDGE ( 'NONE', *, *, #156087, .F. ) ;
#132309 = DIRECTION ( 'NONE',  ( -1.000000000000000000, 0.000000000000000000, -0.000000000000000000 ) ) ;
#132311 = DIRECTION ( 'NONE',  ( -0.000000000000000000, -0.000000000000000000, 1.000000000000000000 ) ) ;
#132312 = AXIS2_PLACEMENT_3D ( 'NONE', #168720, #4441, #143954 ) ;
#132314 = ORIENTED_EDGE ( 'NONE', *, *, #42884, .T. ) ;
#132313 = DIRECTION ( 'NONE',  ( 1.836970198721029934E-16, -1.000000000000000000, -0.000000000000000000 ) ) ;
#132315 = CARTESIAN_POINT ( 'NONE',  ( -21.05000000000000071, 9.997527148596390134, -228.1702915402975691 ) ) ;
#132316 = CARTESIAN_POINT ( 'NONE',  ( 20.04142135623730070, 11.65000000001115943, -188.8499999999999659 ) ) ;
#132317 = CARTESIAN_POINT ( 'NONE',  ( 23.14999999999999858, 65.65271564877468791, -222.5736063831752176 ) ) ;
#132319 = EDGE_CURVE ( 'NONE', #4212, #13417, #142108, .T. ) ;
#132318 = DIRECTION ( 'NONE',  ( 0.000000000000000000, -0.2128009952263485993, 0.9770955615653341697 ) ) ;
#132320 = AXIS2_PLACEMENT_3D ( 'NONE', #203357, #9003, #204620 ) ;
#132322 = CARTESIAN_POINT ( 'NONE',  ( 20.12518398540832365, 9.975088720679844201, -108.4966682524699593 ) ) ;
#132321 = CARTESIAN_POINT ( 'NONE',  ( -16.87683809663752399, 33.06517536918362055, -220.7872234046467952 ) ) ;
#132323 = DIRECTION ( 'NONE',  ( 0.000000000000000000, -0.4088369013363280513, 0.9126074666063769270 ) ) ;
#132324 = CARTESIAN_POINT ( 'NONE',  ( -23.15000000000000213, 85.00000000001261924, -193.6291383618718385 ) ) ;
#132325 = VECTOR ( 'NONE', #91791, 1000.000000000000000 ) ;
#132326 = AXIS2_PLACEMENT_3D ( 'NONE', #129757, #131039, #192309 ) ;
#132327 = CARTESIAN_POINT ( 'NONE',  ( 21.05000000000000071, 1.622572661691780382, -230.6714771550865350 ) ) ;
#132328 = LINE ( 'NONE', #227578, #130289 ) ;
#132329 = CIRCLE ( 'NONE', #28320, 0.1000000000000055844 ) ;
#132330 = ORIENTED_EDGE ( 'NONE', *, *, #139548, .F. ) ;
#132331 = FACE_OUTER_BOUND ( 'NONE', #143798, .T. ) ;
#132332 = VECTOR ( 'NONE', #68169, 1000.000000000000000 ) ;
#132333 = ORIENTED_EDGE ( 'NONE', *, *, #253030, .T. ) ;
#132334 = LINE ( 'NONE', #216689, #156114 ) ;
#132335 = ORIENTED_EDGE ( 'NONE', *, *, #10680, .T. ) ;
#132337 = DIRECTION ( 'NONE',  ( 1.000000000000000000, 0.000000000000000000, 0.000000000000000000 ) ) ;
#132336 = AXIS2_PLACEMENT_3D ( 'NONE', #158387, #177929, #59203 ) ;
#132338 = B_SPLINE_CURVE_WITH_KNOTS ( 'NONE', 3,
 ( #251356, #119245, #21442, #72765, #198757, #20143, #250085, #183068, #24005, #5672, #4407, #26569, #225996, #66957, #162235, #222151 ),
 .UNSPECIFIED., .F., .F.,
 ( 4, 3, 3, 3, 3, 4 ),
 ( 0.000000000000000000, 1.810570668010599751E-05, 2.740575833571215353E-05, 4.256816319435558806E-05, 5.213463471025249507E-05, 6.641585710717949479E-05 ),
 .UNSPECIFIED. ) ;
#132339 = ORIENTED_EDGE ( 'NONE', *, *, #145280, .F. ) ;
#132340 = CARTESIAN_POINT ( 'NONE',  ( -21.04999999999999716, 30.86294145740712125, -252.1314134296355007 ) ) ;
#132341 =( NAMED_UNIT ( * ) PLANE_ANGLE_UNIT ( ) SI_UNIT ( $, .RADIAN. ) );
#132342 = AXIS2_PLACEMENT_3D ( 'NONE', #179000, #218059, #19901 ) ;
#132343 = VERTEX_POINT ( 'NONE', #86660 ) ;
#132344 = CIRCLE ( 'NONE', #86537, 0.1000000000000001305 ) ;
#132345 = VERTEX_POINT ( 'NONE', #204061 ) ;
#132346 = ADVANCED_BREP_SHAPE_REPRESENTATION ( '', ( #112300, #2425 ), #227291 ) ;
#132347 = EDGE_CURVE ( 'NONE', #37772, #143461, #4718, .T. ) ;
#132349 = CARTESIAN_POINT ( 'NONE',  ( -23.15000000000000213, 1.115600667400684642E-11, -100.5000000000000426 ) ) ;
#132348 = CIRCLE ( 'NONE', #211469, 0.9750000000000036415 ) ;
#132350 = CARTESIAN_POINT ( 'NONE',  ( -16.78055652883087134, 66.05322308388622332, -56.86231564693196106 ) ) ;
#132351 = FACE_OUTER_BOUND ( 'NONE', #193173, .T. ) ;
#132353 = EDGE_CURVE ( 'NONE', #27978, #106685, #168821, .T. ) ;
#132352 = AXIS2_PLACEMENT_3D ( 'NONE', #180372, #60406, #219477 ) ;
#132354 = CARTESIAN_POINT ( 'NONE',  ( 12.26145404764308822, 26.51259657475388920, -233.5074718021644458 ) ) ;
#132355 = DIRECTION ( 'NONE',  ( 0.000000000000000000, -0.9964539953858966292, -0.08413937888696096379 ) ) ;
#132356 = CIRCLE ( 'NONE', #78366, 0.1000000000000028644 ) ;
#132357 =( BOUNDED_SURFACE ( )  B_SPLINE_SURFACE ( 3, 2, ( 
 ( #191764, #27559, #126616 ),
 ( #225679, #249152, #70530 ),
 ( #151341, #247848, #107036 ),
 ( #148763, #186608, #10533 ) ),
 .UNSPECIFIED., .F., .F., .F. ) 
 B_SPLINE_SURFACE_WITH_KNOTS ( ( 4, 4 ),
 ( 3, 3 ),
 ( 4.712388980384689674, 5.765869716888459173 ),
 ( 0.000000000000000000, 1.000000000000000000 ),
 .UNSPECIFIED. ) 
 GEOMETRIC_REPRESENTATION_ITEM ( )  RATIONAL_B_SPLINE_SURFACE ( (
 ( 1.000000000000000000, 0.7071067811865719976, 1.000000000000000000),
 ( 1.000000000000000000, 0.7953136715913269317, 1.000000000000000000),
 ( 1.000000000000000000, 0.8646876308615392137, 1.000000000000000000),
 ( 1.000000000000000000, 0.8984936768950618768, 1.000000000000000000) ) ) 
 REPRESENTATION_ITEM ( '' )  SURFACE ( )  );
#132359 = DIRECTION ( 'NONE',  ( -0.000000000000000000, 0.000000000000000000, 1.000000000000000000 ) ) ;
#132358 = DIRECTION ( 'NONE',  ( -1.000000000000000000, 0.000000000000000000, 0.000000000000000000 ) ) ;
#132360 = CARTESIAN_POINT ( 'NONE',  ( -15.39946565075090668, 9.389534562357859215, -82.67480930438999565 ) ) ;
#132362 = VERTEX_POINT ( 'NONE', #207950 ) ;
#132361 = DIRECTION ( 'NONE',  ( -0.7071067811865127117, -0.7071067811865821007, 0.000000000000000000 ) ) ;
#132363 = CARTESIAN_POINT ( 'NONE',  ( 22.45305468355011058, 76.10085836911193269, -148.2726746080140288 ) ) ;
#132364 = AXIS2_PLACEMENT_3D ( 'NONE', #75165, #12619, #17707 ) ;
#132365 = EDGE_CURVE ( 'NONE', #248967, #73243, #29719, .T. ) ;
#132366 = DIRECTION ( 'NONE',  ( 0.000000000000000000, -0.2128009952263613669, 0.9770955615653312831 ) ) ;
#132367 = EDGE_CURVE ( 'NONE', #46048, #182093, #79551, .T. ) ;
#132368 = EDGE_LOOP ( 'NONE', ( #18424, #124941, #203205, #124989, #114966, #168545, #3057 ) ) ;
#132369 = CARTESIAN_POINT ( 'NONE',  ( -18.40000000000000568, -9.499999999988851584, -174.4993620971800681 ) ) ;
#132370 = CARTESIAN_POINT ( 'NONE',  ( -21.14999999999999858, 69.74218538953626023, -170.1208977758331855 ) ) ;
#132371 = LINE ( 'NONE', #154541, #104001 ) ;
#132372 = ORIENTED_EDGE ( 'NONE', *, *, #130059, .T. ) ;
#132373 = EDGE_CURVE ( 'NONE', #239657, #117118, #175455, .T. ) ;
#132374 = DIRECTION ( 'NONE',  ( 0.000000000000000000, 0.2617529984165035128, 0.9651348961777155289 ) ) ;
#132375 = EDGE_CURVE ( 'NONE', #217944, #95060, #108813, .T. ) ;
#132376 = VECTOR ( 'NONE', #193589, 1000.000000000000000 ) ;
#132377 = FACE_OUTER_BOUND ( 'NONE', #94521, .T. ) ;
#132378 = FACE_OUTER_BOUND ( 'NONE', #38739, .T. ) ;
#132381 = ADVANCED_FACE ( 'NONE', ( #11011 ), #71011, .F. ) ;
#132380 = EDGE_CURVE ( 'NONE', #246321, #253143, #225475, .T. ) ;
#132379 =( GEOMETRIC_REPRESENTATION_CONTEXT ( 3 ) GLOBAL_UNCERTAINTY_ASSIGNED_CONTEXT ( ( #62308 ) ) GLOBAL_UNIT_ASSIGNED_CONTEXT ( ( #137322, #197303, #39565 ) ) REPRESENTATION_CONTEXT ( 'NONE', 'WORKASPACE' ) );
#132383 = ORIENTED_EDGE ( 'NONE', *, *, #31353, .T. ) ;
#132382 = AXIS2_PLACEMENT_3D ( 'NONE', #64708, #68569, #125954 ) ;
#132384 = ORIENTED_EDGE ( 'NONE', *, *, #72617, .F. ) ;
#132385 = CARTESIAN_POINT ( 'NONE',  ( 22.50046968637449751, 64.11207000662210476, -247.1836817737965077 ) ) ;
#132386 = DIRECTION ( 'NONE',  ( 0.000000000000000000, -0.8371762388950346745, -0.5469332180710581026 ) ) ;
#132387 = CARTESIAN_POINT ( 'NONE',  ( 20.94999999999999929, 5.850000000011105428, -43.63249722427796939 ) ) ;
#132388 = FACE_OUTER_BOUND ( 'NONE', #247046, .T. ) ;
#132389 = ORIENTED_EDGE ( 'NONE', *, *, #92151, .T. ) ;
#132390 = CARTESIAN_POINT ( 'NONE',  ( 20.94999999999999929, 36.65892442174935439, -249.5511627012433848 ) ) ;
#132391 = EDGE_CURVE ( 'NONE', #232370, #90864, #50514, .T. ) ;
#132392 = DIRECTION ( 'NONE',  ( -1.000000000000000000, 3.265361837132813093E-16, 2.280189983783949500E-30 ) ) ;
#132393 = AXIS2_PLACEMENT_3D ( 'NONE', #66271, #90956, #170559 ) ;
#132394 = CARTESIAN_POINT ( 'NONE',  ( 20.95512820512820440, 8.876151316299271343, -75.55862899514100661 ) ) ;
#132395 = DIRECTION ( 'NONE',  ( -1.000000000000000000, 0.000000000000000000, 0.000000000000000000 ) ) ;
#132396 = CIRCLE ( 'NONE', #236437, 0.2000000000000057288 ) ;
#132397 = EDGE_CURVE ( 'NONE', #49989, #200718, #121310, .T. ) ;
#132398 = EDGE_CURVE ( 'NONE', #23721, #141610, #146196, .T. ) ;
#132399 = VERTEX_POINT ( 'NONE', #30518 ) ;
#132400 = DIRECTION ( 'NONE',  ( 1.000000000000000000, 0.000000000000000000, 0.000000000000000000 ) ) ;
#132401 = AXIS2_PLACEMENT_3D ( 'NONE', #82548, #85113, #143827 ) ;
#132402 = EDGE_CURVE ( 'NONE', #65805, #89456, #144579, .T. ) ;
#132404 = EDGE_LOOP ( 'NONE', ( #11678, #188606, #94697, #65833 ) ) ;
#132403 = CARTESIAN_POINT ( 'NONE',  ( -17.78241384945274461, 65.14442424721148939, -193.2740698120442744 ) ) ;
#132405 = LINE ( 'NONE', #251048, #209924 ) ;
#132406 = DIRECTION ( 'NONE',  ( 1.000000000000000000, 0.000000000000000000, 0.000000000000000000 ) ) ;
#132407 = CARTESIAN_POINT ( 'NONE',  ( 20.85000000000000142, 45.93315328338058379, -256.6017782078560003 ) ) ;
#132408 = CARTESIAN_POINT ( 'NONE',  ( 23.24999999999999289, 71.85000000001214460, -136.5231074845243029 ) ) ;
#132409 = DIRECTION ( 'NONE',  ( 0.000000000000000000, 0.000000000000000000, 1.000000000000000000 ) ) ;
#132410 = EDGE_CURVE ( 'NONE', #70695, #227218, #167092, .T. ) ;
#132411 = ORIENTED_EDGE ( 'NONE', *, *, #69293, .F. ) ;
#132412 = CARTESIAN_POINT ( 'NONE',  ( 21.30000000000002558, 1.115600667400684642E-11, -129.9500000000000171 ) ) ;
#132413 = ADVANCED_FACE ( 'NONE', ( #33111 ), #153057, .F. ) ;
#132414 = AXIS2_PLACEMENT_3D ( 'NONE', #132584, #238082, #36057 ) ;
#132415 = LINE ( 'NONE', #167712, #175890 ) ;
#132416 = DIRECTION ( 'NONE',  ( 0.000000000000000000, -1.000000000000000000, -6.982962677686266711E-15 ) ) ;
#132417 = VERTEX_POINT ( 'NONE', #93035 ) ;
#132418 = CARTESIAN_POINT ( 'NONE',  ( 21.72449340488910252, 65.71604372252116377, -157.3731074845244393 ) ) ;
#132419 = DIRECTION ( 'NONE',  ( 0.000000000000000000, 0.9126074666063660468, 0.4088369013363524762 ) ) ;
#132420 = DIRECTION ( 'NONE',  ( 1.000000000000000000, -0.000000000000000000, -0.000000000000000000 ) ) ;
#132421 = TOROIDAL_SURFACE ( 'NONE', #86592, 0.2000000000000000111, 0.1000000000000000056 ) ;
#132422 = TOROIDAL_SURFACE ( 'NONE', #3212, 0.6000000000000015321, 0.1000000000000000056 ) ;
#132423 = DIRECTION ( 'NONE',  ( 1.000000000000000000, 0.000000000000000000, 0.000000000000000000 ) ) ;
#132424 = AXIS2_PLACEMENT_3D ( 'NONE', #110047, #190908, #12261 ) ;
#132425 = CARTESIAN_POINT ( 'NONE',  ( -18.59999999999999787, 9.350000000011156942, -146.3500000000000227 ) ) ;
#132426 = AXIS2_PLACEMENT_3D ( 'NONE', #85433, #81584, #120777 ) ;
#132427 = CARTESIAN_POINT ( 'NONE',  ( 12.33938619321248176, 9.360723793997193454, -184.8139271946066913 ) ) ;
#132428 = ORIENTED_EDGE ( 'NONE', *, *, #235735, .F. ) ;
#132429 = ORIENTED_EDGE ( 'NONE', *, *, #213042, .T. ) ;
#132430 = CARTESIAN_POINT ( 'NONE',  ( -18.50000000000000711, -9.419203418015495544, -141.2477858104287236 ) ) ;
#132431 = CARTESIAN_POINT ( 'NONE',  ( -20.95613430942438882, 38.11298866354308501, -236.0245638395625463 ) ) ;
#132432 = CARTESIAN_POINT ( 'NONE',  ( -23.25000000000000000, -1.835859311432481045, -78.50443916879852679 ) ) ;
#132433 = CYLINDRICAL_SURFACE ( 'NONE', #175908, 1.500000000000001332 ) ;
#132434 = VECTOR ( 'NONE', #229961, 1000.000000000000000 ) ;
#132435 = DIRECTION ( 'NONE',  ( 0.000000000000000000, 0.000000000000000000, 1.000000000000000000 ) ) ;
#132436 = CARTESIAN_POINT ( 'NONE',  ( -16.93970660449832621, 10.01284139164672915, -113.0522817357944945 ) ) ;
#132437 = VECTOR ( 'NONE', #151417, 1000.000000000000000 ) ;
#132438 = VERTEX_POINT ( 'NONE', #229978 ) ;
#132439 = EDGE_LOOP ( 'NONE', ( #43799, #58853, #215919, #206974 ) ) ;
#132440 = DIRECTION ( 'NONE',  ( 1.000000000000000000, -2.952720810173289112E-16, -2.061873921506763405E-30 ) ) ;
#132441 = DIRECTION ( 'NONE',  ( 0.000000000000000000, -6.938893903907222067E-15, 1.000000000000000000 ) ) ;
#132443 = ORIENTED_EDGE ( 'NONE', *, *, #127036, .F. ) ;
#132442 = CARTESIAN_POINT ( 'NONE',  ( 21.14999999999999858, 8.786607556611267356, -79.25000000000004263 ) ) ;
#132444 = DIRECTION ( 'NONE',  ( -7.304098846218134667E-16, -1.000000000000000000, 0.000000000000000000 ) ) ;
#132445 = CARTESIAN_POINT ( 'NONE',  ( 21.14999999999999858, 22.07612373182271881, -231.7717111801312342 ) ) ;
#132446 = CARTESIAN_POINT ( 'NONE',  ( 18.58725287972292506, 85.56662691070313542, -62.70060267875840765 ) ) ;
#132447 = DIRECTION ( 'NONE',  ( 0.000000000000000000, 0.000000000000000000, -1.000000000000000000 ) ) ;
#132448 = ORIENTED_EDGE ( 'NONE', *, *, #33405, .F. ) ;
#132449 = DIRECTION ( 'NONE',  ( 2.342056488767301376E-15, 0.3896596508880124654, 0.9209589331071350582 ) ) ;
#132450 = EDGE_CURVE ( 'NONE', #89497, #62775, #212858, .T. ) ;
#132451 = CARTESIAN_POINT ( 'NONE',  ( 18.49999999999999289, 65.79142135624951493, -145.3731074845244109 ) ) ;
#132452 = DIRECTION ( 'NONE',  ( 0.000000000000000000, 1.000000000000000000, 0.000000000000000000 ) ) ;
#132453 = AXIS2_PLACEMENT_3D ( 'NONE', #1561, #99368, #121560 ) ;
#132454 = AXIS2_PLACEMENT_3D ( 'NONE', #120259, #22423, #23719 ) ;
#132455 = CIRCLE ( 'NONE', #20046, 4.049999999999998046 ) ;
#132456 = EDGE_CURVE ( 'NONE', #179549, #97681, #246169, .T. ) ;
#132457 = CIRCLE ( 'NONE', #44974, 0.09999999999999939493 ) ;
#132458 = CARTESIAN_POINT ( 'NONE',  ( 20.94999999999999929, 6.550000000011156231, -79.15000000000004832 ) ) ;
#132459 = ORIENTED_EDGE ( 'NONE', *, *, #237801, .F. ) ;
#132460 =( BOUNDED_SURFACE ( )  B_SPLINE_SURFACE ( 3, 2, ( 
 ( #93364, #68681, #210751 ),
 ( #230307, #30862, #9985 ),
 ( #90787, #172954, #229044 ),
 ( #252426, #170396, #72545 ) ),
 .UNSPECIFIED., .F., .F., .F. ) 
 B_SPLINE_SURFACE_WITH_KNOTS ( ( 4, 4 ),
 ( 3, 3 ),
 ( -3.469446951953614189E-18, 0.001979672783031568434 ),
 ( 0.000000000000000000, 1.000000000000000000 ),
 .UNSPECIFIED. ) 
 GEOMETRIC_REPRESENTATION_ITEM ( )  RATIONAL_B_SPLINE_SURFACE ( (
 ( 1.000000000000000000, 0.7103081912008257781, 1.000000000000000000),
 ( 1.000000000000000000, 0.7104998333563169455, 1.000000000000000000),
 ( 1.000000000000000000, 0.7107238315751489566, 1.000000000000000000),
 ( 1.000000000000000000, 0.7110073749541068189, 1.000000000000000000) ) ) 
 REPRESENTATION_ITEM ( '' )  SURFACE ( )  );
#132461 = CARTESIAN_POINT ( 'NONE',  ( -18.50000000000000000, -1.135018845899022466, -108.2169768834323662 ) ) ;
#132463 = ADVANCED_FACE ( 'NONE', ( #232578 ), #113884, .T. ) ;
#132462 = CARTESIAN_POINT ( 'NONE',  ( -21.05000000000000071, 76.00000000001189449, -95.12310748452431142 ) ) ;
#132465 = EDGE_CURVE ( 'NONE', #198148, #91918, #21338, .T. ) ;
#132464 = EDGE_LOOP ( 'NONE', ( #165224, #150950, #193025, #89794 ) ) ;
#132466 = VERTEX_POINT ( 'NONE', #74802 ) ;
#132467 = CARTESIAN_POINT ( 'NONE',  ( -18.59999999999999787, 78.21362219944482774, -231.2727646510690533 ) ) ;
#132468 = CARTESIAN_POINT ( 'NONE',  ( -0.8999999999999430678, 67.65000000001118963, -5.981686128287480919 ) ) ;
#132469 = ORIENTED_EDGE ( 'NONE', *, *, #220901, .F. ) ;
#132470 = AXIS2_PLACEMENT_3D ( 'NONE', #188213, #25304, #49981 ) ;
#132471 = CARTESIAN_POINT ( 'NONE',  ( 18.46163235739458131, -9.480150806907193584, -174.1576105398774814 ) ) ;
#132472 = DIRECTION ( 'NONE',  ( 1.000000000000000000, -0.000000000000000000, -0.000000000000000000 ) ) ;
#132473 = AXIS2_PLACEMENT_3D ( 'NONE', #182844, #218068, #44598 ) ;
#132474 = VERTEX_POINT ( 'NONE', #154344 ) ;
#132475 = EDGE_CURVE ( 'NONE', #19956, #73870, #9023, .T. ) ;
#132476 = CIRCLE ( 'NONE', #20068, 0.09999999999999939493 ) ;
#132477 = EDGE_CURVE ( 'NONE', #126714, #220134, #31814, .T. ) ;
#132478 = DIRECTION ( 'NONE',  ( 0.000000000000000000, -0.1350103645451807555, -0.9908441862701610203 ) ) ;
#132479 = ORIENTED_EDGE ( 'NONE', *, *, #29737, .T. ) ;
#132480 = CARTESIAN_POINT ( 'NONE',  ( 21.13614978966382196, 76.00000000001217870, -143.0222121863580753 ) ) ;
#132481 = DIRECTION ( 'NONE',  ( -3.265361837132813093E-16, -1.000000000000000000, -6.982962677686266711E-15 ) ) ;
#132483 = ORIENTED_EDGE ( 'NONE', *, *, #240401, .F. ) ;
#132482 = CARTESIAN_POINT ( 'NONE',  ( -17.01825945287481545, 66.05000000001201954, -115.7731074845243597 ) ) ;
#132484 = CARTESIAN_POINT ( 'NONE',  ( 21.05000000000000071, -8.999999999988842703, -157.6060308773475640 ) ) ;
#132485 = CARTESIAN_POINT ( 'NONE',  ( -18.40000000000000213, 11.48667500176882328, -176.7499999999999716 ) ) ;
#132486 = DIRECTION ( 'NONE',  ( 0.000000000000000000, -0.9651348961777379554, 0.2617529984164210233 ) ) ;
#132487 = DIRECTION ( 'NONE',  ( 0.000000000000000000, 0.000000000000000000, -1.000000000000000000 ) ) ;
#132488 = DIRECTION ( 'NONE',  ( 1.000000000000000000, -0.000000000000000000, -0.000000000000000000 ) ) ;
#132489 = CARTESIAN_POINT ( 'NONE',  ( 22.57320508075687115, 11.75000000001115552, -100.5000000000000284 ) ) ;
#132490 = DIRECTION ( 'NONE',  ( -1.000000000000000000, 0.000000000000000000, 0.000000000000000000 ) ) ;
#132493 = VERTEX_POINT ( 'NONE', #160745 ) ;
#132492 = EDGE_CURVE ( 'NONE', #95948, #106770, #255905, .T. ) ;
#132491 = LINE ( 'NONE', #150771, #165451 ) ;
#132494 = ORIENTED_EDGE ( 'NONE', *, *, #214438, .F. ) ;
#132496 = CARTESIAN_POINT ( 'NONE',  ( 21.14999999999999858, 64.35000000001164722, -69.42310748452440805 ) ) ;
#132495 = LINE ( 'NONE', #69976, #199694 ) ;
#132498 = VERTEX_POINT ( 'NONE', #240264 ) ;
#132497 = CARTESIAN_POINT ( 'NONE',  ( -23.25000000000000000, 0.000000000000000000, -4.049999999999998934 ) ) ;
#132499 = CIRCLE ( 'NONE', #207707, 12.87500000000000000 ) ;
#132500 = EDGE_LOOP ( 'NONE', ( #208915, #119818, #43395, #241647 ) ) ;
#132501 = EDGE_CURVE ( 'NONE', #254397, #138780, #233873, .T. ) ;
#132502 = CARTESIAN_POINT ( 'NONE',  ( -23.15000000000000213, 87.48912529308852015, -173.1231074845242688 ) ) ;
#132504 = CARTESIAN_POINT ( 'NONE',  ( 20.94999999999999929, 69.45000000001206786, -126.5060803140843291 ) ) ;
#132503 = AXIS2_PLACEMENT_3D ( 'NONE', #61693, #122960, #202489 ) ;
#132505 = AXIS2_PLACEMENT_3D ( 'NONE', #128910, #233163, #111924 ) ;
#132506 = DIRECTION ( 'NONE',  ( 1.000000000000000000, 0.000000000000000000, 0.000000000000000000 ) ) ;
#132507 = CARTESIAN_POINT ( 'NONE',  ( 19.81427058490557158, 11.66856398039207932, -58.25000000000000000 ) ) ;
#132509 = DIRECTION ( 'NONE',  ( 0.000000000000000000, -0.1350103645451807555, -0.9908441862701610203 ) ) ;
#132508 = AXIS2_PLACEMENT_3D ( 'NONE', #158140, #18587, #159389 ) ;
#132511 = EDGE_CURVE ( 'NONE', #230638, #82836, #167272, .T. ) ;
#132510 = DIRECTION ( 'NONE',  ( 1.000000000000000000, -0.000000000000000000, -0.000000000000000000 ) ) ;
#132512 = EDGE_CURVE ( 'NONE', #248708, #121929, #163164, .T. ) ;
#132513 = CARTESIAN_POINT ( 'NONE',  ( -23.15000000000000213, 1.999999999999998224, -13.22462192276210224 ) ) ;
#132514 = ORIENTED_EDGE ( 'NONE', *, *, #63148, .F. ) ;
#132515 = ORIENTED_EDGE ( 'NONE', *, *, #139916, .T. ) ;
#132516 = CARTESIAN_POINT ( 'NONE',  ( -20.64999999999999858, 85.00000000001251976, -179.9170766071767389 ) ) ;
#132517 = ADVANCED_FACE ( 'NONE', ( #121615 ), #117731, .F. ) ;
#132518 = AXIS2_PLACEMENT_3D ( 'NONE', #195751, #250552, #191906 ) ;
#132519 = CIRCLE ( 'NONE', #115965, 0.5000000000000004441 ) ;
#132520 = ORIENTED_EDGE ( 'NONE', *, *, #221537, .F. ) ;
#132521 = DIRECTION ( 'NONE',  ( -0.000000000000000000, 6.982962677686266711E-15, -1.000000000000000000 ) ) ;
#132522 = EDGE_LOOP ( 'NONE', ( #22647, #100379, #63893 ) ) ;
#132524 = DIRECTION ( 'NONE',  ( -1.000000000000000000, 0.000000000000000000, 0.000000000000000000 ) ) ;
#132523 = AXIS2_PLACEMENT_3D ( 'NONE', #257501, #140163, #181887 ) ;
#132525 = CIRCLE ( 'NONE', #3315, 0.09999999999999864553 ) ;
#132526 = CARTESIAN_POINT ( 'NONE',  ( -21.64999999999999858, 51.86416507299303902, -232.4940334956133938 ) ) ;
#132527 = CARTESIAN_POINT ( 'NONE',  ( -20.85000000000000142, 6.933893972137497030, -70.78564583437358237 ) ) ;
#132528 = EDGE_LOOP ( 'NONE', ( #218790, #242084, #69199, #230353, #19884, #256606, #9932, #127032, #167303, #167714 ) ) ;
#132529 = EDGE_CURVE ( 'NONE', #46680, #186401, #196448, .T. ) ;
#132530 = CARTESIAN_POINT ( 'NONE',  ( -21.05000000000000071, -11.64999999999999858, -30.50000000000000000 ) ) ;
#132531 = EDGE_LOOP ( 'NONE', ( #184192, #14523, #147683, #241595 ) ) ;
#132532 = CARTESIAN_POINT ( 'NONE',  ( -18.59999999999999787, 79.19526988099229925, -196.1889237952725296 ) ) ;
#132533 = DIRECTION ( 'NONE',  ( 0.000000000000000000, 0.5273008465187821736, -0.8496786552930323255 ) ) ;
#132534 = EDGE_CURVE ( 'NONE', #225338, #158894, #78596, .T. ) ;
#132535 = ORIENTED_EDGE ( 'NONE', *, *, #52880, .F. ) ;
#132536 = LINE ( 'NONE', #112975, #256710 ) ;
#132537 = AXIS2_PLACEMENT_3D ( 'NONE', #35326, #154007, #173570 ) ;
#132538 = ORIENTED_EDGE ( 'NONE', *, *, #120823, .F. ) ;
#132540 = ORIENTED_EDGE ( 'NONE', *, *, #147895, .T. ) ;
#132539 = DIRECTION ( 'NONE',  ( -1.000000000000000000, 0.000000000000000000, 0.000000000000000000 ) ) ;
#132541 = CARTESIAN_POINT ( 'NONE',  ( -20.94999999999999929, 64.36312671090738036, -42.84486669784926249 ) ) ;
#132542 = CIRCLE ( 'NONE', #120105, 12.87499999999999822 ) ;
#132543 = ORIENTED_EDGE ( 'NONE', *, *, #170377, .T. ) ;
#132544 = TOROIDAL_SURFACE ( 'NONE', #78362, 0.2000000000000000111, 0.1000000000000000056 ) ;
#132545 = ORIENTED_EDGE ( 'NONE', *, *, #13020, .T. ) ;
#132546 = MECHANICAL_DESIGN_GEOMETRIC_PRESENTATION_REPRESENTATION (  '', ( #190849 ), #32634 ) ;
#132547 = TOROIDAL_SURFACE ( 'NONE', #70219, 0.2000000000000000111, 0.1000000000000000056 ) ;
#132548 = VECTOR ( 'NONE', #232945, 1000.000000000000000 ) ;
#132549 = DIRECTION ( 'NONE',  ( 1.000000000000000000, 0.000000000000000000, -0.000000000000000000 ) ) ;
#132550 = VERTEX_POINT ( 'NONE', #155618 ) ;
#132552 = CIRCLE ( 'NONE', #224121, 11.64999999999999503 ) ;
#132551 = DIRECTION ( 'NONE',  ( 1.000000000000000000, 0.000000000000000000, 0.000000000000000000 ) ) ;
#132553 = DIRECTION ( 'NONE',  ( 0.000000000000000000, 0.9770955615653313941, 0.2128009952263606452 ) ) ;
#132554 = DIRECTION ( 'NONE',  ( 0.000000000000000000, -8.881784197001266523E-15, 1.000000000000000000 ) ) ;
#132555 = FACE_OUTER_BOUND ( 'NONE', #62236, .T. ) ;
#132556 = DIRECTION ( 'NONE',  ( 0.000000000000000000, 0.8814952561688427224, -0.4721928772777352346 ) ) ;
#132557 = ORIENTED_EDGE ( 'NONE', *, *, #153047, .T. ) ;
#132558 = CARTESIAN_POINT ( 'NONE',  ( -21.05000000000000071, 62.99095723518624368, -207.1734234082435080 ) ) ;
#132559 = CARTESIAN_POINT ( 'NONE',  ( -22.50000000000000000, 64.25000000001165290, -69.52310748452438816 ) ) ;
#132560 = CARTESIAN_POINT ( 'NONE',  ( 21.07971444708685738, 6.329792081637703127, -33.41217656368210243 ) ) ;
#132561 = VERTEX_POINT ( 'NONE', #40797 ) ;
#132562 = DIRECTION ( 'NONE',  ( 0.000000000000000000, 0.8814952561688444987, -0.4721928772777320149 ) ) ;
#132564 = ORIENTED_EDGE ( 'NONE', *, *, #250532, .T. ) ;
#132563 = AXIS2_PLACEMENT_3D ( 'NONE', #218804, #40212, #102691 ) ;
#132566 = CIRCLE ( 'NONE', #119946, 0.5000000000000004441 ) ;
#132565 = CARTESIAN_POINT ( 'NONE',  ( 21.05000000000000071, 76.00000000001210765, -132.4231074845243370 ) ) ;
#132567 = ORIENTED_EDGE ( 'NONE', *, *, #78594, .T. ) ;
#132568 = CIRCLE ( 'NONE', #244987, 0.09999999999999123479 ) ;
#132569 = DIRECTION ( 'NONE',  ( 0.000000000000000000, 6.467318590049456648E-15, -1.000000000000000000 ) ) ;
#132570 = DIRECTION ( 'NONE',  ( 1.000000000000000000, -0.000000000000000000, 0.000000000000000000 ) ) ;
#132572 = ORIENTED_EDGE ( 'NONE', *, *, #237473, .F. ) ;
#132571 = CARTESIAN_POINT ( 'NONE',  ( -16.82542659449996592, 44.22818387756893088, -235.2743865959531036 ) ) ;
#132573 = CARTESIAN_POINT ( 'NONE',  ( 20.95512820512820440, 8.876151316299271343, -75.55862899514100661 ) ) ;
#132574 = VERTEX_POINT ( 'NONE', #120344 ) ;
#132575 = CARTESIAN_POINT ( 'NONE',  ( -20.96428641293861617, 36.19089144327093521, -235.9708266132235792 ) ) ;
#132576 = TOROIDAL_SURFACE ( 'NONE', #74166, 0.4000000000000012990, 0.1000000000000000056 ) ;
#132577 = FACE_OUTER_BOUND ( 'NONE', #257628, .T. ) ;
#132578 = AXIS2_PLACEMENT_3D ( 'NONE', #230698, #14229, #172034 ) ;
#132579 = ORIENTED_EDGE ( 'NONE', *, *, #243414, .T. ) ;
#132580 = FACE_OUTER_BOUND ( 'NONE', #146570, .T. ) ;
#132581 = CARTESIAN_POINT ( 'NONE',  ( -21.29999999999995808, 76.00000000001240608, -174.0731074845243711 ) ) ;
#132582 = VECTOR ( 'NONE', #65396, 1000.000000000000000 ) ;
#132583 = ORIENTED_EDGE ( 'NONE', *, *, #192364, .T. ) ;
#132584 = CARTESIAN_POINT ( 'NONE',  ( -20.54999999999999716, 7.128833340094563376, -233.7327013124401276 ) ) ;
#132585 = EDGE_LOOP ( 'NONE', ( #156254, #210979 ) ) ;
#132586 = CIRCLE ( 'NONE', #16095, 3.899999999999987033 ) ;
#132587 = CARTESIAN_POINT ( 'NONE',  ( 15.51872946208854920, 9.376580978055097049, -118.1269462470119862 ) ) ;
#132588 = CARTESIAN_POINT ( 'NONE',  ( 18.59999999999999076, 65.79142135624952914, -148.6731074845244223 ) ) ;
#132589 = EDGE_CURVE ( 'NONE', #141892, #126094, #254643, .T. ) ;
#132590 = VECTOR ( 'NONE', #107557, 1000.000000000000000 ) ;
#132593 = ORIENTED_EDGE ( 'NONE', *, *, #257364, .F. ) ;
#132592 = ORIENTED_EDGE ( 'NONE', *, *, #237275, .F. ) ;
#132591 = LINE ( 'NONE', #167892, #64015 ) ;
#132594 = ADVANCED_FACE ( 'NONE', ( #56455 ), #19711, .T. ) ;
#132595 = PLANE ( 'NONE',  #20428 ) ;
#132597 = EDGE_CURVE ( 'NONE', #59200, #63323, #88093, .T. ) ;
#132596 = AXIS2_PLACEMENT_3D ( 'NONE', #99639, #21447, #240467 ) ;
#132598 = DIRECTION ( 'NONE',  ( 1.000000000000000000, 0.000000000000000000, 0.000000000000000000 ) ) ;
#132599 = DIRECTION ( 'NONE',  ( 0.000000000000000000, -0.2128009952263604510, 0.9770955615653315052 ) ) ;
#132600 = CIRCLE ( 'NONE', #232587, 0.09999999999999939493 ) ;
#132602 = CARTESIAN_POINT ( 'NONE',  ( -23.25000000000000000, 0.000000000000000000, -33.50000000000000000 ) ) ;
#132601 = CARTESIAN_POINT ( 'NONE',  ( 18.59999999999999076, 10.20857864377385127, -54.85000000000000142 ) ) ;
#132603 = CARTESIAN_POINT ( 'NONE',  ( -20.54999999999999716, 73.50000000001223555, -149.7477294072864709 ) ) ;
#132604 = CYLINDRICAL_SURFACE ( 'NONE', #240188, 4.049999999999997158 ) ;
#132605 = FACE_OUTER_BOUND ( 'NONE', #72995, .T. ) ;
#132606 = AXIS2_PLACEMENT_3D ( 'NONE', #126482, #48227, #228163 ) ;
#132607 = DIRECTION ( 'NONE',  ( 1.000000000000000000, -0.000000000000000000, -0.000000000000000000 ) ) ;
#132608 = EDGE_LOOP ( 'NONE', ( #124714, #162466, #139171, #237070 ) ) ;
#132609 = ORIENTED_EDGE ( 'NONE', *, *, #119450, .F. ) ;
#132610 = CARTESIAN_POINT ( 'NONE',  ( -18.39999999999999858, -9.599999999988849453, -107.1001893912220879 ) ) ;
#132612 = VERTEX_POINT ( 'NONE', #99431 ) ;
#132611 = CARTESIAN_POINT ( 'NONE',  ( 21.05000000000000426, 10.72371710471867701, -175.0944173916130637 ) ) ;
#132613 = ORIENTED_EDGE ( 'NONE', *, *, #9599, .F. ) ;
#132614 = EDGE_CURVE ( 'NONE', #170796, #183504, #242233, .T. ) ;
#132615 = DIRECTION ( 'NONE',  ( -1.000000000000000000, 0.000000000000000000, -0.000000000000000000 ) ) ;
#132616 = EDGE_LOOP ( 'NONE', ( #116916, #62676, #55933 ) ) ;
#132617 = FACE_OUTER_BOUND ( 'NONE', #237468, .T. ) ;
#132618 = VECTOR ( 'NONE', #55783, 1000.000000000000227 ) ;
#132619 = EDGE_LOOP ( 'NONE', ( #195792, #72275, #58107, #25232 ) ) ;
#132620 = CARTESIAN_POINT ( 'NONE',  ( -18.59999999999999787, 77.83534155023627932, -91.46795619196132066 ) ) ;
#132622 = ORIENTED_EDGE ( 'NONE', *, *, #156072, .F. ) ;
#132621 = ORIENTED_EDGE ( 'NONE', *, *, #84103, .T. ) ;
#132623 = ORIENTED_EDGE ( 'NONE', *, *, #138648, .F. ) ;
#132624 = ORIENTED_EDGE ( 'NONE', *, *, #174713, .F. ) ;
#132625 = EDGE_LOOP ( 'NONE', ( #73900, #31913, #110436, #166641, #194361 ) ) ;
#132626 = CARTESIAN_POINT ( 'NONE',  ( -18.40000000000000213, 70.35000000001224407, -149.1731074845243938 ) ) ;
#132627 = PLANE ( 'NONE',  #194939 ) ;
#132628 = CARTESIAN_POINT ( 'NONE',  ( -12.48127053791144903, 9.376580978055093496, -185.1269462470118867 ) ) ;
#132630 = ORIENTED_EDGE ( 'NONE', *, *, #207385, .T. ) ;
#132629 = DIRECTION ( 'NONE',  ( 0.000000000000000000, 1.265107689135680095E-16, -1.000000000000000000 ) ) ;
#132631 = ADVANCED_FACE ( 'NONE', ( #180281 ), #229777, .F. ) ;
#132632 = EDGE_CURVE ( 'NONE', #92460, #99525, #159071, .T. ) ;
#132633 = DIRECTION ( 'NONE',  ( -0.000000000000000000, 6.982962677686266711E-15, -1.000000000000000000 ) ) ;
#132634 = DIRECTION ( 'NONE',  ( -3.469446951953635015E-14, 1.000000000000000000, 0.000000000000000000 ) ) ;
#132636 = EDGE_LOOP ( 'NONE', ( #39671, #160525, #256346, #125161 ) ) ;
#132635 = DIRECTION ( 'NONE',  ( 0.000000000000000000, -0.8814952561688430555, 0.4721928772777346239 ) ) ;
#132637 = FACE_OUTER_BOUND ( 'NONE', #174176, .T. ) ;
#132638 = ORIENTED_EDGE ( 'NONE', *, *, #251024, .F. ) ;
#132639 = DIRECTION ( 'NONE',  ( 0.000000000000000000, 0.000000000000000000, -1.000000000000000000 ) ) ;
#132640 = ORIENTED_EDGE ( 'NONE', *, *, #164508, .T. ) ;
#132641 = DIRECTION ( 'NONE',  ( 0.000000000000000000, -0.2617529984164915779, -0.9651348961777189706 ) ) ;
#132642 = DIRECTION ( 'NONE',  ( 0.000000000000000000, -0.1350103645451945777, 0.9908441862701590219 ) ) ;
#132643 = EDGE_CURVE ( 'NONE', #220753, #208402, #204825, .T. ) ;
#132644 = ORIENTED_EDGE ( 'NONE', *, *, #6170, .F. ) ;
#132645 = AXIS2_PLACEMENT_3D ( 'NONE', #255226, #33718, #211031 ) ;
#132648 = DIRECTION ( 'NONE',  ( 1.000000000000000000, 0.000000000000000000, 0.000000000000000000 ) ) ;
#132647 = AXIS2_PLACEMENT_3D ( 'NONE', #205074, #9460, #245518 ) ;
#132646 = DIRECTION ( 'NONE',  ( 0.000000000000000000, 0.000000000000000000, 1.000000000000000000 ) ) ;
#132649 = VECTOR ( 'NONE', #177950, 1000.000000000000114 ) ;
#132650 = CARTESIAN_POINT ( 'NONE',  ( 18.59999999999996945, 18.41524492703432614, -237.0006385043383546 ) ) ;
#132651 = CARTESIAN_POINT ( 'NONE',  ( 18.54999999999999716, 67.25000000001149658, -48.67310748452438673 ) ) ;
#132652 = DIRECTION ( 'NONE',  ( 0.000000000000000000, 0.8700118002898393765, -0.4930308989875104575 ) ) ;
#132653 = EDGE_LOOP ( 'NONE', ( #26408, #221420, #180559, #251788 ) ) ;
#132654 = EDGE_LOOP ( 'NONE', ( #133205, #220702, #252984, #147935 ) ) ;
#132655 = CARTESIAN_POINT ( 'NONE',  ( 21.04999999999999716, 8.871279685995645536, -8.558628995140946216 ) ) ;
#132656 = VECTOR ( 'NONE', #123080, 1000.000000000000000 ) ;
#132657 = DIRECTION ( 'NONE',  ( 1.000000000000000000, 0.000000000000000000, 0.000000000000000000 ) ) ;
#132658 = ORIENTED_EDGE ( 'NONE', *, *, #47858, .T. ) ;
#132659 = DIRECTION ( 'NONE',  ( 0.000000000000000000, 0.9770955615653313941, 0.2128009952263603677 ) ) ;
#132660 = ORIENTED_EDGE ( 'NONE', *, *, #154771, .F. ) ;
#132661 = CARTESIAN_POINT ( 'NONE',  ( -20.85000000000000142, 76.00000000001142553, -36.02310748452432421 ) ) ;
#132662 = CARTESIAN_POINT ( 'NONE',  ( 21.13461538461538325, 60.21941965847794620, -221.1573116214326831 ) ) ;
#132663 = DIRECTION ( 'NONE',  ( -0.000000000000000000, 0.7397360091702708251, 0.6728971962616883129 ) ) ;
#132664 = EDGE_CURVE ( 'NONE', #21197, #175346, #22508, .T. ) ;
#132665 = CIRCLE ( 'NONE', #20239, 0.4000000000000010214 ) ;
#132666 = CIRCLE ( 'NONE', #207687, 11.80000000000000426 ) ;
#132667 = ORIENTED_EDGE ( 'NONE', *, *, #100045, .F. ) ;
#132668 = AXIS2_PLACEMENT_3D ( 'NONE', #232236, #212662, #56119 ) ;
#132669 = CARTESIAN_POINT ( 'NONE',  ( -18.69999999999999929, 1.885425182446137438, -11.49641995933507843 ) ) ;
#132670 = ORIENTED_EDGE ( 'NONE', *, *, #154423, .T. ) ;
#132671 = AXIS2_PLACEMENT_3D ( 'NONE', #237181, #215042, #234601 ) ;
#132672 = ORIENTED_EDGE ( 'NONE', *, *, #103197, .F. ) ;
#132673 = EDGE_LOOP ( 'NONE', ( #224702, #149059, #65819, #240911 ) ) ;
#132674 = EDGE_CURVE ( 'NONE', #187202, #17763, #104553, .T. ) ;
#132675 = DIRECTION ( 'NONE',  ( -2.602085213965226419E-14, -0.000000000000000000, 1.000000000000000000 ) ) ;
#132676 = DIRECTION ( 'NONE',  ( -1.000000000000000000, -0.000000000000000000, -0.000000000000000000 ) ) ;
#132677 = DIRECTION ( 'NONE',  ( 1.000000000000000000, 0.000000000000000000, 0.000000000000000000 ) ) ;
#132678 = EDGE_CURVE ( 'NONE', #75171, #137789, #92396, .T. ) ;
#132679 = CARTESIAN_POINT ( 'NONE',  ( 21.05000000000000071, 85.00000000001179501, -79.41707660717668205 ) ) ;
#132680 = CARTESIAN_POINT ( 'NONE',  ( -16.86379686415369150, 9.975217759253158789, -20.93338988909028231 ) ) ;
#132682 = CARTESIAN_POINT ( 'NONE',  ( 21.05000000000000071, 8.776282895292474961, -12.15000000000000036 ) ) ;
#132681 = CYLINDRICAL_SURFACE ( 'NONE', #257748, 12.87499999999999822 ) ;
#132684 = ORIENTED_EDGE ( 'NONE', *, *, #33724, .T. ) ;
#132683 = DIRECTION ( 'NONE',  ( 0.000000000000000000, 0.1455152366551500653, 0.9893560106964507384 ) ) ;
#132685 = DIRECTION ( 'NONE',  ( 0.000000000000000000, 0.000000000000000000, 1.000000000000000000 ) ) ;
#132686 = ORIENTED_EDGE ( 'NONE', *, *, #20835, .F. ) ;
#132687 = EDGE_CURVE ( 'NONE', #235411, #112587, #84993, .T. ) ;
#132688 = CARTESIAN_POINT ( 'NONE',  ( -19.99999999999999645, 5.645774302107834153, 15.47947886955507890 ) ) ;
#132689 = EDGE_CURVE ( 'NONE', #209650, #5593, #154795, .T. ) ;
#132690 = ORIENTED_EDGE ( 'NONE', *, *, #252022, .T. ) ;
#132691 = ORIENTED_EDGE ( 'NONE', *, *, #73864, .T. ) ;
#132692 = DIRECTION ( 'NONE',  ( 1.000000000000000000, -0.000000000000000000, -0.000000000000000000 ) ) ;
#132693 = DIRECTION ( 'NONE',  ( -1.000000000000000000, -0.000000000000000000, -0.000000000000000000 ) ) ;
#132694 = CARTESIAN_POINT ( 'NONE',  ( -16.94389599337535657, 66.00880201025478300, -48.63075228632278169 ) ) ;
#132695 = DIRECTION ( 'NONE',  ( 0.000000000000000000, -0.1455152366551522025, -0.9893560106964505163 ) ) ;
#132696 = AXIS2_PLACEMENT_3D ( 'NONE', #216603, #120114, #142202 ) ;
#132697 = AXIS2_PLACEMENT_3D ( 'NONE', #131152, #208149, #129860 ) ;
#132698 = EDGE_CURVE ( 'NONE', #154024, #24047, #208932, .T. ) ;
#132699 = CARTESIAN_POINT ( 'NONE',  ( 20.93975676684922504, 18.37846419038447010, -236.9325101954432853 ) ) ;
#132700 = EDGE_CURVE ( 'NONE', #246051, #254405, #107148, .T. ) ;
#132701 = ORIENTED_EDGE ( 'NONE', *, *, #137107, .T. ) ;
#132702 = ORIENTED_EDGE ( 'NONE', *, *, #140015, .T. ) ;
#132703 = CARTESIAN_POINT ( 'NONE',  ( 18.59999999999999076, 11.65000000000000391, -24.85000000000000142 ) ) ;
#132704 = ORIENTED_EDGE ( 'NONE', *, *, #237450, .F. ) ;
#132705 = CARTESIAN_POINT ( 'NONE',  ( -18.79999999999999716, 1.212568896937007645, -8.000000000000000000 ) ) ;
#132706 = FACE_OUTER_BOUND ( 'NONE', #88230, .T. ) ;
#132707 = ORIENTED_EDGE ( 'NONE', *, *, #123947, .F. ) ;
#132709 = LINE ( 'NONE', #133968, #232070 ) ;
#132708 = AXIS2_PLACEMENT_3D ( 'NONE', #112255, #169690, #190517 ) ;
#132711 = EDGE_CURVE ( 'NONE', #39467, #257268, #101987, .T. ) ;
#132710 = DIRECTION ( 'NONE',  ( 0.000000000000000000, -7.026728003956683390E-15, 1.000000000000000000 ) ) ;
#132712 = DIRECTION ( 'NONE',  ( 0.000000000000000000, -0.8814952561688430555, 0.4721928772777346239 ) ) ;
#132713 = DIRECTION ( 'NONE',  ( 0.000000000000000000, 0.000000000000000000, 1.000000000000000000 ) ) ;
#132714 = ORIENTED_EDGE ( 'NONE', *, *, #132163, .F. ) ;
#132715 = FACE_OUTER_BOUND ( 'NONE', #59425, .T. ) ;
#132716 = ADVANCED_FACE ( 'NONE', ( #66755 ), #63174, .F. ) ;
#132717 = DIRECTION ( 'NONE',  ( -1.000000000000000000, 0.000000000000000000, 0.000000000000000000 ) ) ;
#132718 = TOROIDAL_SURFACE ( 'NONE', #57666, 0.4000000000000015210, 0.1000000000000000056 ) ;
#132719 = FACE_OUTER_BOUND ( 'NONE', #185130, .T. ) ;
#132720 = TOROIDAL_SURFACE ( 'NONE', #186891, 12.97499999999999609, 0.1000000000000000056 ) ;
#132721 = EDGE_CURVE ( 'NONE', #222558, #120061, #2931, .T. ) ;
#132722 = EDGE_CURVE ( 'NONE', #249163, #2024, #38250, .T. ) ;
#132723 = AXIS2_PLACEMENT_3D ( 'NONE', #69035, #127716, #28660 ) ;
#132724 = ORIENTED_EDGE ( 'NONE', *, *, #163986, .T. ) ;
#132725 = AXIS2_PLACEMENT_3D ( 'NONE', #140771, #100329, #23422 ) ;
#132726 = EDGE_CURVE ( 'NONE', #55232, #162084, #108961, .T. ) ;
#132727 = DIRECTION ( 'NONE',  ( 0.000000000000000000, 0.000000000000000000, 1.000000000000000000 ) ) ;
#132728 = VERTEX_POINT ( 'NONE', #6770 ) ;
#132729 = CARTESIAN_POINT ( 'NONE',  ( 20.94999999999999929, 8.985508020264692419, -211.4778645542876347 ) ) ;
#132730 = CARTESIAN_POINT ( 'NONE',  ( -16.94107738177414291, 14.24304960796391306, -219.3391119284832484 ) ) ;
#132731 = DIRECTION ( 'NONE',  ( 0.000000000000000000, 0.8700118002898322711, -0.4930308989875231140 ) ) ;
#132732 = EDGE_CURVE ( 'NONE', #3545, #88741, #46589, .T. ) ;
#132734 = VECTOR ( 'NONE', #180449, 1000.000000000000000 ) ;
#132733 = DIRECTION ( 'NONE',  ( 0.000000000000000000, 0.9316174814283056937, 0.3634403228828368970 ) ) ;
#132735 = DIRECTION ( 'NONE',  ( 0.000000000000000000, 1.734723475976817507E-14, 1.000000000000000000 ) ) ;
#132736 = CARTESIAN_POINT ( 'NONE',  ( -20.64999999999999858, 7.150000000000000355, -12.34999999999999964 ) ) ;
#132737 = VECTOR ( 'NONE', #193051, 1000.000000000000114 ) ;
#132738 = EDGE_CURVE ( 'NONE', #83518, #146218, #86280, .T. ) ;
#132739 = ORIENTED_EDGE ( 'NONE', *, *, #76889, .F. ) ;
#132740 = DIRECTION ( 'NONE',  ( 0.000000000000000000, 0.000000000000000000, -1.000000000000000000 ) ) ;
#132741 = DIRECTION ( 'NONE',  ( 0.000000000000000000, -0.3488585713686159218, -0.9371753822965306346 ) ) ;
#132743 = ADVANCED_FACE ( 'NONE', ( #43343 ), #165865, .T. ) ;
#132742 = DIRECTION ( 'NONE',  ( 1.000000000000000000, 0.000000000000000000, 0.000000000000000000 ) ) ;
#132744 = CARTESIAN_POINT ( 'NONE',  ( -23.25000000000000000, 1.115649040949250830E-11, -130.1000000000000512 ) ) ;
#132745 = AXIS2_PLACEMENT_3D ( 'NONE', #105491, #142077, #183785 ) ;
#132746 = DIRECTION ( 'NONE',  ( 1.000000000000000000, 0.000000000000000000, 0.000000000000000000 ) ) ;
#132747 = TOROIDAL_SURFACE ( 'NONE', #153628, 0.2000000000000000111, 0.1000000000000000056 ) ;
#132748 = AXIS2_PLACEMENT_3D ( 'NONE', #224453, #246585, #104486 ) ;
#132750 = ORIENTED_EDGE ( 'NONE', *, *, #194776, .F. ) ;
#132749 = VECTOR ( 'NONE', #121141, 1000.000000000000000 ) ;
#132751 = EDGE_LOOP ( 'NONE', ( #187686, #631, #224616, #165623 ) ) ;
#132752 = CARTESIAN_POINT ( 'NONE',  ( 23.15000000000000213, 23.68770167995059239, -252.8127582590406348 ) ) ;
#132753 =( GEOMETRIC_REPRESENTATION_CONTEXT ( 3 ) GLOBAL_UNCERTAINTY_ASSIGNED_CONTEXT ( ( #86912 ) ) GLOBAL_UNIT_ASSIGNED_CONTEXT ( ( #166978, #65264, #186512 ) ) REPRESENTATION_CONTEXT ( 'NONE', 'WORKASPACE' ) );
#132754 = CYLINDRICAL_SURFACE ( 'NONE', #121875, 11.75000000000001066 ) ;
#132755 = DIRECTION ( 'NONE',  ( 0.000000000000000000, 0.000000000000000000, -1.000000000000000000 ) ) ;
#132756 = CARTESIAN_POINT ( 'NONE',  ( 12.25000000000000000, 66.65000000001185754, -86.27310748452437394 ) ) ;
#132757 = CARTESIAN_POINT ( 'NONE',  ( 21.14999999999999858, 44.33733722763473395, -236.4833033074485513 ) ) ;
#132758 = EDGE_CURVE ( 'NONE', #89464, #186471, #188090, .T. ) ;
#132759 = AXIS2_PLACEMENT_3D ( 'NONE', #244205, #61738, #184247 ) ;
#132760 = VERTEX_POINT ( 'NONE', #242807 ) ;
#132761 = CARTESIAN_POINT ( 'NONE',  ( -15.75000000000000355, 13.18880795147152440, -215.2702608532411830 ) ) ;
#132762 = CARTESIAN_POINT ( 'NONE',  ( -23.25000000000000000, 76.10085836911075319, -114.7726746080137019 ) ) ;
#132763 = ORIENTED_EDGE ( 'NONE', *, *, #56439, .F. ) ;
#132764 = FACE_OUTER_BOUND ( 'NONE', #59528, .T. ) ;
#132765 = PRODUCT_DEFINITION_SHAPE ( 'NONE', 'NONE',  #5427 ) ;
#132766 = DIRECTION ( 'NONE',  ( -0.000000000000000000, -6.982962677686266711E-15, 1.000000000000000000 ) ) ;
#132767 = VECTOR ( 'NONE', #104938, 1000.000000000000000 ) ;
#132768 = AXIS2_PLACEMENT_3D ( 'NONE', #24994, #224442, #221855 ) ;
#132769 = AXIS2_PLACEMENT_3D ( 'NONE', #2588, #202093, #82108 ) ;
#132770 = ORIENTED_EDGE ( 'NONE', *, *, #45512, .F. ) ;
#132771 = DIRECTION ( 'NONE',  ( 0.000000000000000000, -1.000000000000000000, 0.000000000000000000 ) ) ;
#132772 = ORIENTED_EDGE ( 'NONE', *, *, #161823, .F. ) ;
#132773 = DIRECTION ( 'NONE',  ( -1.000000000000000000, 4.625929269271478222E-14, 0.000000000000000000 ) ) ;
#132774 = DIRECTION ( 'NONE',  ( -1.000000000000000000, -2.952720810173289112E-16, 0.000000000000000000 ) ) ;
#132775 = DIRECTION ( 'NONE',  ( -3.035766082959430086E-14, 0.8814952561688430555, -0.4721928772777346239 ) ) ;
#132776 = DIRECTION ( 'NONE',  ( -1.000000000000000000, 0.000000000000000000, -0.000000000000000000 ) ) ;
#132778 = CIRCLE ( 'NONE', #95164, 7.900000000000010125 ) ;
#132777 = FACE_OUTER_BOUND ( 'NONE', #59261, .T. ) ;
#132779 = CARTESIAN_POINT ( 'NONE',  ( 23.24999999999999645, 64.25000000001161027, -60.27310748452440947 ) ) ;
#132780 = CYLINDRICAL_SURFACE ( 'NONE', #180670, 0.09999999999999939493 ) ;
#132781 = AXIS2_PLACEMENT_3D ( 'NONE', #144986, #8075, #68034 ) ;
#132783 = CARTESIAN_POINT ( 'NONE',  ( -20.00857864376270001, 61.53642629385834795, -221.5144953033309321 ) ) ;
#132782 = DIRECTION ( 'NONE',  ( 0.000000000000000000, 0.000000000000000000, -1.000000000000000000 ) ) ;
#132784 = EDGE_CURVE ( 'NONE', #174818, #13368, #150332, .T. ) ;
#132785 = DIRECTION ( 'NONE',  ( 0.000000000000000000, 0.000000000000000000, -1.000000000000000000 ) ) ;
#132786 = CARTESIAN_POINT ( 'NONE',  ( 21.04999999999999716, 22.00620749460749082, -231.7459716400360605 ) ) ;
#132787 = DIRECTION ( 'NONE',  ( 0.000000000000000000, 1.000000000000000000, 6.982962677686266711E-15 ) ) ;
#132788 = ORIENTED_EDGE ( 'NONE', *, *, #32906, .T. ) ;
#132789 = EDGE_CURVE ( 'NONE', #67859, #189017, #112305, .T. ) ;
#132790 = DIRECTION ( 'NONE',  ( 0.000000000000000000, 1.000000000000000000, 0.000000000000000000 ) ) ;
#132791 = CARTESIAN_POINT ( 'NONE',  ( -20.94999999999999929, 0.000000000000000000, -33.50000000000000000 ) ) ;
#132792 = CARTESIAN_POINT ( 'NONE',  ( 20.04142135623730070, 11.75000000001115907, -158.6500000000000057 ) ) ;
#132793 = AXIS2_PLACEMENT_3D ( 'NONE', #68511, #7229, #168937 ) ;
#132794 = CARTESIAN_POINT ( 'NONE',  ( -20.54999999999999716, 9.350000000011156942, -146.2500000000000284 ) ) ;
#132796 = EDGE_CURVE ( 'NONE', #5506, #144728, #193124, .T. ) ;
#132795 = FACE_OUTER_BOUND ( 'NONE', #39853, .T. ) ;
#132797 = CARTESIAN_POINT ( 'NONE',  ( 18.69999999999999929, -9.849999999999996092, 31.39999999999999858 ) ) ;
#132798 = ADVANCED_FACE ( 'NONE', ( #187986 ), #25768, .T. ) ;
#132799 = ORIENTED_EDGE ( 'NONE', *, *, #179217, .F. ) ;
#132800 = TOROIDAL_SURFACE ( 'NONE', #178601, 0.2000000000000000111, 0.1000000000000000056 ) ;
#132801 = AXIS2_PLACEMENT_3D ( 'NONE', #230216, #51542, #213203 ) ;
#132802 = CARTESIAN_POINT ( 'NONE',  ( 20.94999999999999929, 18.18127959618848877, -237.5711165786817389 ) ) ;
#132803 = VECTOR ( 'NONE', #6849, 1000.000000000000000 ) ;
#132804 = ORIENTED_EDGE ( 'NONE', *, *, #69969, .T. ) ;
#132805 = CARTESIAN_POINT ( 'NONE',  ( -20.94999999999999929, 38.25685495413521409, -235.9601135138701693 ) ) ;
#132806 = EDGE_LOOP ( 'NONE', ( #232035, #58409, #95901, #221959 ) ) ;
#132807 = CARTESIAN_POINT ( 'NONE',  ( -20.85000000000000142, 87.65000000001214175, -136.5231074845242745 ) ) ;
#132808 = ORIENTED_EDGE ( 'NONE', *, *, #43834, .T. ) ;
#132809 = DIRECTION ( 'NONE',  ( -2.952720810173289112E-16, -0.9651348961777159730, 0.2617529984165024026 ) ) ;
#132810 = CARTESIAN_POINT ( 'NONE',  ( 20.97462148592276776, 67.12526242356146611, -124.2684631527937000 ) ) ;
#132812 = DIRECTION ( 'NONE',  ( 0.000000000000000000, 0.9999631594459053030, 0.008583690987162899758 ) ) ;
#132811 = AXIS2_PLACEMENT_3D ( 'NONE', #78900, #95908, #60629 ) ;
#132813 = DIRECTION ( 'NONE',  ( 0.000000000000000000, -0.5826443254699606999, -0.8127272543711416830 ) ) ;
#132814 = CARTESIAN_POINT ( 'NONE',  ( -16.78493832629887450, 9.945835743204147761, -12.66394901910421567 ) ) ;
#132815 = DIRECTION ( 'NONE',  ( 0.000000000000000000, 0.2128009952263602844, -0.9770955615653315052 ) ) ;
#132816 = DIRECTION ( 'NONE',  ( -1.000000000000000000, 0.000000000000000000, -0.000000000000000000 ) ) ;
#132817 = ORIENTED_EDGE ( 'NONE', *, *, #185360, .T. ) ;
#132819 = DIRECTION ( 'NONE',  ( -1.000000000000000000, -2.952720810173289112E-16, 0.000000000000000000 ) ) ;
#132818 = DIRECTION ( 'NONE',  ( 1.000000000000000000, 0.000000000000000000, 0.000000000000000000 ) ) ;
#132820 = ORIENTED_EDGE ( 'NONE', *, *, #95897, .T. ) ;
#132822 = ORIENTED_EDGE ( 'NONE', *, *, #139069, .T. ) ;
#132821 = DIRECTION ( 'NONE',  ( -0.000000000000000000, 0.07893460099012301889, -0.9968797965484754720 ) ) ;
#132823 = ORIENTED_EDGE ( 'NONE', *, *, #241848, .F. ) ;
#132824 = EDGE_CURVE ( 'NONE', #13549, #120967, #172316, .T. ) ;
#132825 = CYLINDRICAL_SURFACE ( 'NONE', #41539, 2.600000000000000089 ) ;
#132826 = LINE ( 'NONE', #152405, #80223 ) ;
#132827 = CARTESIAN_POINT ( 'NONE',  ( 23.24999999999999645, 11.75000000001113953, -54.34999999999999432 ) ) ;
#132828 = FACE_OUTER_BOUND ( 'NONE', #212983, .T. ) ;
#132829 = DIRECTION ( 'NONE',  ( 0.000000000000000000, 1.000000000000000000, 6.982962677686266711E-15 ) ) ;
#132830 = DIRECTION ( 'NONE',  ( 1.000000000000000000, 0.000000000000000000, 0.000000000000000000 ) ) ;
#132832 = EDGE_CURVE ( 'NONE', #19242, #64247, #6646, .T. ) ;
#132831 = DIRECTION ( 'NONE',  ( 0.000000000000000000, -0.1350103645451876666, -0.9908441862701600211 ) ) ;
#132833 = EDGE_CURVE ( 'NONE', #200975, #95684, #192366, .T. ) ;
#132834 = DIRECTION ( 'NONE',  ( -0.000000000000000000, 1.000000000000000000, -0.000000000000000000 ) ) ;
#132835 = ORIENTED_EDGE ( 'NONE', *, *, #207734, .F. ) ;
#132836 = VERTEX_POINT ( 'NONE', #111007 ) ;
#132837 = AXIS2_PLACEMENT_3D ( 'NONE', #24901, #67847, #66580 ) ;
#132838 = CARTESIAN_POINT ( 'NONE',  ( 20.04999999999999716, 67.25000000001158185, -60.27310748452438816 ) ) ;
#132839 = AXIS2_PLACEMENT_3D ( 'NONE', #181790, #47395, #125659 ) ;
#132840 = CIRCLE ( 'NONE', #20413, 0.1999999999999893807 ) ;
#132841 = ORIENTED_EDGE ( 'NONE', *, *, #10501, .T. ) ;
#132842 = DIRECTION ( 'NONE',  ( 0.000000000000000000, 0.000000000000000000, 1.000000000000000000 ) ) ;
#132843 = ORIENTED_EDGE ( 'NONE', *, *, #241004, .T. ) ;
#132844 = FACE_OUTER_BOUND ( 'NONE', #107462, .T. ) ;
#132845 = EDGE_CURVE ( 'NONE', #128703, #30986, #615, .T. ) ;
#132846 = AXIS2_PLACEMENT_3D ( 'NONE', #206457, #27857, #107348 ) ;
#132847 = DIRECTION ( 'NONE',  ( -0.000000000000000000, 0.4721928772777345684, 0.8814952561688429444 ) ) ;
#132848 = CYLINDRICAL_SURFACE ( 'NONE', #255340, 0.09999999999999939493 ) ;
#132849 = CARTESIAN_POINT ( 'NONE',  ( 23.14999999999999147, 67.23127455305841238, -235.8551265064783991 ) ) ;
#132850 = EDGE_CURVE ( 'NONE', #164668, #130548, #11320, .T. ) ;
#132851 = DIRECTION ( 'NONE',  ( 2.952720810173289112E-16, 1.000000000000000000, 6.982962677686266711E-15 ) ) ;
#132852 = ORIENTED_EDGE ( 'NONE', *, *, #113015, .T. ) ;
#132853 = ADVANCED_FACE ( 'NONE', ( #10631 ), #213020, .F. ) ;
#132854 = CARTESIAN_POINT ( 'NONE',  ( -18.41817142474042512, -9.498703066590925559, -207.6039654876369696 ) ) ;
#132855 = AXIS2_PLACEMENT_3D ( 'NONE', #201980, #23370, #178592 ) ;
#132856 = CARTESIAN_POINT ( 'NONE',  ( 18.79999999999999716, 6.742993295648862961, 9.658650260582458458 ) ) ;
#132858 = CIRCLE ( 'NONE', #82732, 12.77499999999999503 ) ;
#132857 = CARTESIAN_POINT ( 'NONE',  ( -21.05000000000000071, -11.74999999998884448, -63.89999999999999858 ) ) ;
#132859 = EDGE_CURVE ( 'NONE', #4716, #235019, #179720, .T. ) ;
#132860 = FACE_OUTER_BOUND ( 'NONE', #117185, .T. ) ;
#132861 = VERTEX_POINT ( 'NONE', #30204 ) ;
#132863 = DIRECTION ( 'NONE',  ( 0.000000000000000000, 0.9126074666064177832, 0.4088369013362369020 ) ) ;
#132862 = CARTESIAN_POINT ( 'NONE',  ( -21.46681500593282621, 6.857511159395651035, -134.0000000000000000 ) ) ;
#132864 = ORIENTED_EDGE ( 'NONE', *, *, #57747, .F. ) ;
#132867 = VERTEX_POINT ( 'NONE', #1309 ) ;
#132866 = DIRECTION ( 'NONE',  ( 0.000000000000000000, 0.8814952561688437216, -0.4721928772777334582 ) ) ;
#132865 = CARTESIAN_POINT ( 'NONE',  ( -23.15000000000000213, -6.438379425586759908, -212.1495692908769684 ) ) ;
#132868 = AXIS2_PLACEMENT_3D ( 'NONE', #106000, #222091, #242960 ) ;
#132869 = DIRECTION ( 'NONE',  ( -1.000000000000000000, 2.952720810173289112E-16, 2.061873921506763405E-30 ) ) ;
#132870 = CARTESIAN_POINT ( 'NONE',  ( -20.54999999999999716, 1.115600667400684642E-11, -102.4000000000000483 ) ) ;
#132871 = ORIENTED_EDGE ( 'NONE', *, *, #202124, .T. ) ;
#132872 = DIRECTION ( 'NONE',  ( 0.000000000000000000, 0.000000000000000000, 1.000000000000000000 ) ) ;
#132873 = EDGE_CURVE ( 'NONE', #129083, #133788, #133910, .T. ) ;
#132874 = LINE ( 'NONE', #214958, #44712 ) ;
#132875 = PLANE ( 'NONE',  #138396 ) ;
#132877 = ORIENTED_EDGE ( 'NONE', *, *, #134450, .F. ) ;
#132876 = CARTESIAN_POINT ( 'NONE',  ( 20.85000000000000142, 87.75000000001215028, -139.5231074845243029 ) ) ;
#132878 = ORIENTED_EDGE ( 'NONE', *, *, #190558, .T. ) ;
#132879 = DIRECTION ( 'NONE',  ( 0.000000000000000000, 0.1298341882520022694, 0.9915357197604852679 ) ) ;
#132880 = CARTESIAN_POINT ( 'NONE',  ( 18.48536876927986228, -9.463527249856182877, -74.04861826508293632 ) ) ;
#132881 = DIRECTION ( 'NONE',  ( -1.000000000000000000, 0.000000000000000000, 0.000000000000000000 ) ) ;
#132882 = AXIS2_PLACEMENT_3D ( 'NONE', #183597, #166633, #6223 ) ;
#132883 = CIRCLE ( 'NONE', #53757, 0.1000000000000055844 ) ;
#132884 = CARTESIAN_POINT ( 'NONE',  ( 23.14999999999999503, 6.450000000011156587, -155.7499999999999716 ) ) ;
#132885 = ORIENTED_EDGE ( 'NONE', *, *, #254879, .F. ) ;
#132886 = CARTESIAN_POINT ( 'NONE',  ( 18.50000000000000000, 85.40000000001190017, -95.72584772486095517 ) ) ;
#132887 = LINE ( 'NONE', #134143, #122427 ) ;
#132888 = CARTESIAN_POINT ( 'NONE',  ( -18.59999999999999787, -1.162701749926853712, -175.5999999999999659 ) ) ;
#132889 = CIRCLE ( 'NONE', #53763, 7.800000000000001599 ) ;
#132890 = VERTEX_POINT ( 'NONE', #199558 ) ;
#132891 = CARTESIAN_POINT ( 'NONE',  ( 18.49999999999999289, 65.79142135624982757, -178.8731074845244109 ) ) ;
#132892 = CARTESIAN_POINT ( 'NONE',  ( -22.59999999999999787, 67.23127455305841238, -235.8551265064783991 ) ) ;
#132893 = ORIENTED_EDGE ( 'NONE', *, *, #12563, .T. ) ;
#132895 = AXIS2_PLACEMENT_3D ( 'NONE', #56649, #257391, #119244 ) ;
#132894 = DIRECTION ( 'NONE',  ( 0.000000000000000000, 1.000000000000000000, 0.000000000000000000 ) ) ;
#132896 = SPHERICAL_SURFACE ( 'NONE', #52195, 0.1000000000000000056 ) ;
#132897 = AXIS2_PLACEMENT_3D ( 'NONE', #223483, #5707, #86526 ) ;
#132898 = EDGE_CURVE ( 'NONE', #202477, #246051, #34182, .T. ) ;
#132899 = ORIENTED_EDGE ( 'NONE', *, *, #182170, .T. ) ;
#132900 = ORIENTED_EDGE ( 'NONE', *, *, #140919, .T. ) ;
#132901 = AXIS2_PLACEMENT_3D ( 'NONE', #19904, #156864, #117700 ) ;
#132902 = ORIENTED_EDGE ( 'NONE', *, *, #165966, .T. ) ;
#132904 = ORIENTED_EDGE ( 'NONE', *, *, #93439, .T. ) ;
#132903 = CARTESIAN_POINT ( 'NONE',  ( -23.39999999999994529, 77.83551161375991967, -47.52760213295649550 ) ) ;
#132905 = EDGE_CURVE ( 'NONE', #204898, #131243, #156594, .T. ) ;
#132906 = CIRCLE ( 'NONE', #191180, 0.09999999999999939493 ) ;
#132907 = AXIS2_PLACEMENT_3D ( 'NONE', #71526, #15394, #152353 ) ;
#132910 = ORIENTED_EDGE ( 'NONE', *, *, #227, .T. ) ;
#132909 = ORIENTED_EDGE ( 'NONE', *, *, #187947, .T. ) ;
#132908 = CARTESIAN_POINT ( 'NONE',  ( -21.14999999999999858, 87.65000000001238334, -170.0231074845242745 ) ) ;
#132911 = ADVANCED_FACE ( 'NONE', ( #136983 ), #100403, .F. ) ;
#132912 = ADVANCED_FACE ( 'NONE', ( #97828 ), #171729, .T. ) ;
#132913 = CARTESIAN_POINT ( 'NONE',  ( 18.79999999999999716, 0.000000000000000000, 0.000000000000000000 ) ) ;
#132914 = ORIENTED_EDGE ( 'NONE', *, *, #74493, .F. ) ;
#132915 = CARTESIAN_POINT ( 'NONE',  ( 20.85000000000000142, 68.87972903831482085, -166.3635444426850825 ) ) ;
#132916 = DIRECTION ( 'NONE',  ( 1.000000000000000000, -7.049440681616512959E-16, 1.911869773728117674E-16 ) ) ;
#132917 = CARTESIAN_POINT ( 'NONE',  ( 21.05000000000000071, 76.00000000001142553, -36.02310748452432421 ) ) ;
#132918 = AXIS2_PLACEMENT_3D ( 'NONE', #41609, #195549, #215085 ) ;
#132919 = DIRECTION ( 'NONE',  ( -7.304098846218136639E-16, -0.4721928772777346239, -0.8814952561688430555 ) ) ;
#132921 = ORIENTED_EDGE ( 'NONE', *, *, #143594, .T. ) ;
#132920 = AXIS2_PLACEMENT_3D ( 'NONE', #97759, #78218, #157812 ) ;
#132922 = AXIS2_PLACEMENT_3D ( 'NONE', #166682, #164088, #25870 ) ;
#132923 = VERTEX_POINT ( 'NONE', #95292 ) ;
#132924 = AXIS2_PLACEMENT_3D ( 'NONE', #256691, #36442, #233359 ) ;
#132925 = VERTEX_POINT ( 'NONE', #117431 ) ;
#132926 = CYLINDRICAL_SURFACE ( 'NONE', #245582, 0.09999999999999939493 ) ;
#132928 = ORIENTED_EDGE ( 'NONE', *, *, #78318, .F. ) ;
#132927 = CARTESIAN_POINT ( 'NONE',  ( -20.94999999999994600, 67.82483145523551116, -25.59432346794077162 ) ) ;
#132929 = DIRECTION ( 'NONE',  ( 0.000000000000000000, 0.000000000000000000, -1.000000000000000000 ) ) ;
#132930 = ORIENTED_EDGE ( 'NONE', *, *, #29459, .T. ) ;
#132931 = EDGE_CURVE ( 'NONE', #185202, #246608, #134086, .T. ) ;
#132932 = AXIS2_PLACEMENT_3D ( 'NONE', #226586, #106631, #8847 ) ;
#132933 = EDGE_LOOP ( 'NONE', ( #232048, #233976, #241991, #21440 ) ) ;
#132934 = CARTESIAN_POINT ( 'NONE',  ( -18.39999999999999858, 64.52683809665015247, -194.1971614177164724 ) ) ;
#132935 = ADVANCED_FACE ( 'NONE', ( #18323 ), #162907, .T. ) ;
#132937 = ORIENTED_EDGE ( 'NONE', *, *, #234189, .T. ) ;
#132936 = PRODUCT_DEFINITION ( 'UNKNOWN', '', #169630, #42672 ) ;
#132938 = DIRECTION ( 'NONE',  ( -1.000000000000000000, -0.000000000000000000, -0.000000000000000000 ) ) ;
#132939 = CYLINDRICAL_SURFACE ( 'NONE', #181938, 7.899999999999995914 ) ;
#132940 = AXIS2_PLACEMENT_3D ( 'NONE', #100945, #593, #119291 ) ;
#132942 = ORIENTED_EDGE ( 'NONE', *, *, #150324, .T. ) ;
#132941 = VERTEX_POINT ( 'NONE', #238657 ) ;
#132943 = VERTEX_POINT ( 'NONE', #39200 ) ;
#132944 = DIRECTION ( 'NONE',  ( 0.000000000000000000, -1.000000000000000000, -6.982962677686265922E-15 ) ) ;
#132945 = ORIENTED_EDGE ( 'NONE', *, *, #174829, .T. ) ;
#132946 = VERTEX_POINT ( 'NONE', #80842 ) ;
#132947 = ADVANCED_FACE ( 'NONE', ( #179981 ), #160436, .T. ) ;
#132948 = CARTESIAN_POINT ( 'NONE',  ( 22.39999999999999503, 68.20922040163929978, -203.5231074845243882 ) ) ;
#132950 = EDGE_LOOP ( 'NONE', ( #1980, #163807, #196665, #254050 ) ) ;
#132949 = DIRECTION ( 'NONE',  ( 4.239556034732056743E-17, -0.1298341882520022972, -0.9915357197604853789 ) ) ;
#132951 = ADVANCED_FACE ( 'NONE', ( #239953 ), #254841, .F. ) ;
#132952 = DIRECTION ( 'NONE',  ( 0.000000000000000000, 0.000000000000000000, -1.000000000000000000 ) ) ;
#132953 = ADVANCED_FACE ( 'NONE', ( #114859 ), #254345, .F. ) ;
#132955 = LINE ( 'NONE', #170837, #48374 ) ;
#132954 = DIRECTION ( 'NONE',  ( 1.000000000000000000, 0.000000000000000000, 0.000000000000000000 ) ) ;
#132956 = DIRECTION ( 'NONE',  ( -1.000000000000000000, 0.000000000000000000, 0.000000000000000000 ) ) ;
#132957 = DIRECTION ( 'NONE',  ( -0.7071067811865019426, 0.2890913453341708572, -0.6453109281989138912 ) ) ;
#132958 = ORIENTED_EDGE ( 'NONE', *, *, #119169, .F. ) ;
#132959 = CIRCLE ( 'NONE', #182859, 0.8750000000000007772 ) ;
#132960 = TOROIDAL_SURFACE ( 'NONE', #241296, 0.4000000000000005773, 0.1000000000000000056 ) ;
#132961 = VERTEX_POINT ( 'NONE', #56148 ) ;
#132962 = CARTESIAN_POINT ( 'NONE',  ( 20.94999999999999574, 77.16270174995064224, -195.4231074845243370 ) ) ;
#132963 = DIRECTION ( 'NONE',  ( 0.000000000000000000, -1.000000000000000000, -6.982962677686265922E-15 ) ) ;
#132964 = CARTESIAN_POINT ( 'NONE',  ( -23.15000000000000213, 2.600000000000000089, -13.22462192276210224 ) ) ;
#132965 = CIRCLE ( 'NONE', #166299, 0.2000000000000057288 ) ;
#132966 = ORIENTED_EDGE ( 'NONE', *, *, #7114, .F. ) ;
#132967 = CARTESIAN_POINT ( 'NONE',  ( -23.15000000000000213, 4.150000000011156764, -45.85000000000000142 ) ) ;
#132968 = VECTOR ( 'NONE', #198717, 1000.000000000000000 ) ;
#132969 = B_SPLINE_CURVE_WITH_KNOTS ( 'NONE', 3,
 ( #158567, #159845, #239367, #60705, #219787, #200238, #21612, #184510, #202800, #106248 ),
 .UNSPECIFIED., .F., .F.,
 ( 4, 3, 3, 4 ),
 ( 0.000000000000000000, 0.0002000000000008537104, 0.001000000000082977483, 0.001967863649483329782 ),
 .UNSPECIFIED. ) ;
#132970 = CARTESIAN_POINT ( 'NONE',  ( -16.94445028196807002, 51.64060657411747712, -231.8906364537310196 ) ) ;
#132971 = DIRECTION ( 'NONE',  ( -1.000000000000000000, -0.000000000000000000, -0.000000000000000000 ) ) ;
#132972 = EDGE_LOOP ( 'NONE', ( #157925, #204151, #28665, #237437 ) ) ;
#132973 = ORIENTED_EDGE ( 'NONE', *, *, #174246, .F. ) ;
#132974 = DIRECTION ( 'NONE',  ( 0.000000000000000000, 1.000000000000000000, 6.982962677686266711E-15 ) ) ;
#132975 = CARTESIAN_POINT ( 'NONE',  ( -16.81095280782811230, 66.05000000001207638, -123.8731074845252493 ) ) ;
#132976 = VERTEX_POINT ( 'NONE', #236084 ) ;
#132977 = CARTESIAN_POINT ( 'NONE',  ( -18.41353343127311959, -9.499999999988849808, -174.5320693966996259 ) ) ;
#132978 = ORIENTED_EDGE ( 'NONE', *, *, #97833, .F. ) ;
#132979 = CARTESIAN_POINT ( 'NONE',  ( 18.46932045258648358, -9.670685200254535374, -140.6738603729967565 ) ) ;
#132980 = CARTESIAN_POINT ( 'NONE',  ( -16.77779411440718249, 9.946101447118758543, -154.8369425829954764 ) ) ;
#132982 = CARTESIAN_POINT ( 'NONE',  ( -21.07928932188134397, -1.250084634896337921, -194.7953894783290423 ) ) ;
#132981 = DIRECTION ( 'NONE',  ( 0.000000000000000000, 0.000000000000000000, -1.000000000000000000 ) ) ;
#132984 = AXIS2_PLACEMENT_3D ( 'NONE', #136567, #156177, #235671 ) ;
#132983 = CARTESIAN_POINT ( 'NONE',  ( 18.79999999999999716, 1.350000000000000089, 16.40000000000000213 ) ) ;
#132985 = CARTESIAN_POINT ( 'NONE',  ( 18.50000324121758055, 65.70692517833265356, -164.5644653378304554 ) ) ;
#132986 = EDGE_CURVE ( 'NONE', #231766, #211151, #250807, .T. ) ;
#132987 = CARTESIAN_POINT ( 'NONE',  ( 21.05000000000000071, -0.09999999998884338825, -26.95934304829875927 ) ) ;
#132988 = TOROIDAL_SURFACE ( 'NONE', #174717, 3.899999999999999467, 0.1000000000000000056 ) ;
#132990 = EDGE_LOOP ( 'NONE', ( #45972, #133712, #93094, #243670 ) ) ;
#132989 = CYLINDRICAL_SURFACE ( 'NONE', #219021, 11.79999999999999716 ) ;
#132991 = VECTOR ( 'NONE', #31534, 1000.000000000000000 ) ;
#132993 = ORIENTED_EDGE ( 'NONE', *, *, #74093, .F. ) ;
#132992 = EDGE_LOOP ( 'NONE', ( #18560, #206895, #26643, #91057 ) ) ;
#132994 = ORIENTED_EDGE ( 'NONE', *, *, #207502, .F. ) ;
#132995 = EDGE_CURVE ( 'NONE', #52403, #67483, #196630, .T. ) ;
#132996 = CARTESIAN_POINT ( 'NONE',  ( 22.42196299218230493, 0.002441673987300593818, 11.64961170264947121 ) ) ;
#132997 = DIRECTION ( 'NONE',  ( 0.000000000000000000, 0.000000000000000000, -1.000000000000000000 ) ) ;
#132999 = CARTESIAN_POINT ( 'NONE',  ( 22.39999999999999503, 7.790779598373379855, 0.000000000000000000 ) ) ;
#132998 = CARTESIAN_POINT ( 'NONE',  ( -16.80100914604134843, 66.05685090590898767, -182.7060633572368147 ) ) ;
#133000 = DIRECTION ( 'NONE',  ( -1.000000000000000000, -0.000000000000000000, 0.000000000000000000 ) ) ;
#133001 = ORIENTED_EDGE ( 'NONE', *, *, #82764, .F. ) ;
#133002 = EDGE_CURVE ( 'NONE', #51801, #19242, #123854, .T. ) ;
#133003 = DIRECTION ( 'NONE',  ( 0.000000000000000000, -0.6728971962617483760, 0.7397360091702162022 ) ) ;
#133004 = VERTEX_POINT ( 'NONE', #105524 ) ;
#133005 = ORIENTED_EDGE ( 'NONE', *, *, #74434, .T. ) ;
#133006 = DIRECTION ( 'NONE',  ( 0.7071067811865475727, -0.7071067811865475727, 0.000000000000000000 ) ) ;
#133007 = CARTESIAN_POINT ( 'NONE',  ( -22.47120815636973745, 0.02890382191504723905, -88.85006801124653464 ) ) ;
#133008 = VECTOR ( 'NONE', #187344, 1000.000000000000000 ) ;
#133009 = DIRECTION ( 'NONE',  ( 0.000000000000000000, 0.000000000000000000, -1.000000000000000000 ) ) ;
#133010 = ADVANCED_FACE ( 'NONE', ( #43033 ), #66439, .F. ) ;
#133011 = DIRECTION ( 'NONE',  ( 2.952720810173289112E-16, 1.000000000000000000, 6.982962677686266711E-15 ) ) ;
#133012 = ADVANCED_FACE ( 'NONE', ( #63871 ), #185102, .T. ) ;
#133013 = ORIENTED_EDGE ( 'NONE', *, *, #9093, .T. ) ;
#133014 = ORIENTED_EDGE ( 'NONE', *, *, #163862, .T. ) ;
#133015 = DIRECTION ( 'NONE',  ( -0.000000000000000000, 0.9770955615653313941, 0.2128009952263603954 ) ) ;
#133016 = CARTESIAN_POINT ( 'NONE',  ( -18.46902351632713035, -9.509470118669714367, -40.48645393425731953 ) ) ;
#133017 = CARTESIAN_POINT ( 'NONE',  ( -21.05000000000000071, 61.95000000001162022, -64.00941241376342816 ) ) ;
#133018 = DIRECTION ( 'NONE',  ( 0.000000000000000000, 0.9126074666063813678, 0.4088369013363182813 ) ) ;
#133019 = CARTESIAN_POINT ( 'NONE',  ( -23.25000000000000000, 1.910280373842936141, -79.63136785519898808 ) ) ;
#133020 = CARTESIAN_POINT ( 'NONE',  ( 19.90000000000000924, 4.611773100472912112, 22.11686199900910665 ) ) ;
#133021 = CARTESIAN_POINT ( 'NONE',  ( -21.53699400380027029, 6.787711793208516475, -33.50000000000000711 ) ) ;
#133023 = FACE_OUTER_BOUND ( 'NONE', #210870, .T. ) ;
#133022 = CARTESIAN_POINT ( 'NONE',  ( -18.50000000000000000, 64.25000000001199396, -115.1731074845243796 ) ) ;
#133024 = CARTESIAN_POINT ( 'NONE',  ( 18.39999999999998082, 11.47316190337362585, -76.25000000000004263 ) ) ;
#133025 = DIRECTION ( 'NONE',  ( 1.000000000000000000, -0.000000000000000000, -0.000000000000000000 ) ) ;
#133026 = AXIS2_PLACEMENT_3D ( 'NONE', #238478, #76834, #177258 ) ;
#133027 = PLANE ( 'NONE',  #228723 ) ;
#133028 = DIRECTION ( 'NONE',  ( 0.000000000000000000, -7.056502275159890043E-15, 1.000000000000000000 ) ) ;
#133029 = TOROIDAL_SURFACE ( 'NONE', #49626, 12.77500000000000036, 0.1000000000000000056 ) ;
#133030 = AXIS2_PLACEMENT_3D ( 'NONE', #14955, #214412, #233977 ) ;
#133032 = ORIENTED_EDGE ( 'NONE', *, *, #38254, .T. ) ;
#133031 = CARTESIAN_POINT ( 'NONE',  ( -20.64999999999999858, 68.85000000001186038, -90.77310748452435973 ) ) ;
#133033 = EDGE_CURVE ( 'NONE', #211306, #234821, #204992, .T. ) ;
#133034 = ADVANCED_FACE ( 'NONE', ( #220390 ), #165550, .T. ) ;
#133035 = CIRCLE ( 'NONE', #108085, 0.1000000000000028644 ) ;
#133036 = EDGE_CURVE ( 'NONE', #94760, #81005, #87261, .T. ) ;
#133037 = DIRECTION ( 'NONE',  ( -1.000000000000000000, 0.000000000000000000, 0.000000000000000000 ) ) ;
#133038 = CARTESIAN_POINT ( 'NONE',  ( -22.57320508075687115, 64.25000000001193712, -103.0231074845243739 ) ) ;
#133039 = CIRCLE ( 'NONE', #165801, 0.09999999999998898659 ) ;
#133040 = AXIS2_PLACEMENT_3D ( 'NONE', #29795, #225368, #8911 ) ;
#133041 = EDGE_CURVE ( 'NONE', #141325, #96628, #202103, .T. ) ;
#133043 = AXIS2_PLACEMENT_3D ( 'NONE', #150774, #193753, #212048 ) ;
#133042 = DIRECTION ( 'NONE',  ( 1.000000000000000000, 0.000000000000000000, 0.000000000000000000 ) ) ;
#133045 = EDGE_CURVE ( 'NONE', #95398, #176651, #30087, .T. ) ;
#133044 = DIRECTION ( 'NONE',  ( 0.000000000000000000, -7.147358527629759053E-15, 1.000000000000000000 ) ) ;
#133046 = FACE_OUTER_BOUND ( 'NONE', #103386, .T. ) ;
#133047 = CIRCLE ( 'NONE', #20623, 0.1000000000000043771 ) ;
#133048 = DIRECTION ( 'NONE',  ( -1.000000000000000000, 0.000000000000000000, -0.000000000000000000 ) ) ;
#133049 = CARTESIAN_POINT ( 'NONE',  ( -21.05000000000000071, 0.000000000000000000, 0.000000000000000000 ) ) ;
#133050 = DIRECTION ( 'NONE',  ( 1.000000000000000000, 0.000000000000000000, 0.000000000000000000 ) ) ;
#133051 = ORIENTED_EDGE ( 'NONE', *, *, #162388, .F. ) ;
#133052 = DIRECTION ( 'NONE',  ( 0.000000000000000000, 1.000000000000000000, 0.000000000000000000 ) ) ;
#133054 = ORIENTED_EDGE ( 'NONE', *, *, #43489, .T. ) ;
#133053 = DIRECTION ( 'NONE',  ( 2.710505431213777355E-16, -1.000000000000000000, 0.000000000000000000 ) ) ;
#133055 = DIRECTION ( 'NONE',  ( 0.000000000000000000, -1.000000000000000000, 0.000000000000000000 ) ) ;
#133056 = ADVANCED_FACE ( 'NONE', ( #122577 ), #209115, .T. ) ;
#133057 = VERTEX_POINT ( 'NONE', #46851 ) ;
#133058 = LINE ( 'NONE', #212597, #238561 ) ;
#133059 = EDGE_CURVE ( 'NONE', #229988, #107904, #25964, .T. ) ;
#133060 = PRODUCT_CONTEXT ( 'NONE', #177321, 'mechanical' ) ;
#133061 = DIRECTION ( 'NONE',  ( -0.000000000000000000, 0.4088369013363281068, -0.9126074666063770380 ) ) ;
#133062 = CARTESIAN_POINT ( 'NONE',  ( -23.15000000000000213, 11.75000000001115552, -121.8500000000000227 ) ) ;
#133063 = ORIENTED_EDGE ( 'NONE', *, *, #75342, .F. ) ;
#133064 = LINE ( 'NONE', #195620, #196116 ) ;
#133065 = CARTESIAN_POINT ( 'NONE',  ( -18.59999999999999787, 1.851028230152016674, -45.15391326942249606 ) ) ;
#133066 = CARTESIAN_POINT ( 'NONE',  ( 23.25000000000000000, 87.75000000001173817, -72.62310748452422615 ) ) ;
#133067 = ORIENTED_EDGE ( 'NONE', *, *, #224720, .T. ) ;
#133068 = ORIENTED_EDGE ( 'NONE', *, *, #249655, .F. ) ;
#133069 = CARTESIAN_POINT ( 'NONE',  ( -20.64999999999999858, 76.00000000001126921, -203.5231074845248997 ) ) ;
#133070 = CARTESIAN_POINT ( 'NONE',  ( -20.94999999999999929, 1.115600667400684642E-11, -175.3999999999999773 ) ) ;
#133071 = DIRECTION ( 'NONE',  ( 0.000000000000000000, -1.000000000000000000, -6.982962677686266711E-15 ) ) ;
#133072 = LINE ( 'NONE', #34005, #132737 ) ;
#133074 = CARTESIAN_POINT ( 'NONE',  ( -21.55000000000000426, 68.25000000001158185, -57.17310748452437963 ) ) ;
#133073 = DIRECTION ( 'NONE',  ( 0.000000000000000000, -0.7035695228903320331, -0.7106264324241468033 ) ) ;
#133075 = CARTESIAN_POINT ( 'NONE',  ( -21.07933241753356413, 75.90662040959315959, -176.3517534329041041 ) ) ;
#133076 = FACE_OUTER_BOUND ( 'NONE', #88232, .T. ) ;
#133077 = DIRECTION ( 'NONE',  ( 1.000000000000000000, -0.000000000000000000, -0.000000000000000000 ) ) ;
#133078 = VECTOR ( 'NONE', #2844, 1000.000000000000000 ) ;
#133079 = VERTEX_POINT ( 'NONE', #3896 ) ;
#133080 = ADVANCED_FACE ( 'NONE', ( #204646 ), #92582, .F. ) ;
#133082 = ORIENTED_EDGE ( 'NONE', *, *, #104855, .F. ) ;
#133081 = CARTESIAN_POINT ( 'NONE',  ( 12.60873083341397916, 62.83289218956782207, -216.2009511582251378 ) ) ;
#133083 = CARTESIAN_POINT ( 'NONE',  ( 5.999999999999997335, -11.65000000000000036, 13.90000000000000213 ) ) ;
#133084 = CIRCLE ( 'NONE', #103996, 0.5000000000000014433 ) ;
#133085 = DIRECTION ( 'NONE',  ( 0.000000000000000000, -0.9126074666063753726, -0.4088369013363320481 ) ) ;
#133086 = CARTESIAN_POINT ( 'NONE',  ( -18.59999999999999787, 38.29773864426885410, -236.0513742605307925 ) ) ;
#133087 = ORIENTED_EDGE ( 'NONE', *, *, #52301, .F. ) ;
#133088 = FACE_OUTER_BOUND ( 'NONE', #43074, .T. ) ;
#133089 = DIRECTION ( 'NONE',  ( -1.000000000000000000, 0.000000000000000000, -0.000000000000000000 ) ) ;
#133090 = CARTESIAN_POINT ( 'NONE',  ( -21.09107601085561257, 69.63612202465176892, -103.0624146492415178 ) ) ;
#133091 = DIRECTION ( 'NONE',  ( -0.000000000000000000, -0.4088369013363281623, 0.9126074666063771490 ) ) ;
#133092 = ORIENTED_EDGE ( 'NONE', *, *, #5128, .F. ) ;
#133093 = AXIS2_PLACEMENT_3D ( 'NONE', #107010, #86146, #250388 ) ;
#133094 = AXIS2_PLACEMENT_3D ( 'NONE', #55746, #194038, #153665 ) ;
#133095 = VERTEX_POINT ( 'NONE', #45593 ) ;
#133096 = CARTESIAN_POINT ( 'NONE',  ( 18.49999999999999645, -1.866714910057309273, -11.75267524628200633 ) ) ;
#133097 = ORIENTED_EDGE ( 'NONE', *, *, #210093, .T. ) ;
#133098 = EDGE_CURVE ( 'NONE', #187599, #215584, #105008, .T. ) ;
#133099 = LINE ( 'NONE', #212644, #22194 ) ;
#133100 = TOROIDAL_SURFACE ( 'NONE', #208126, 0.9750000000000019762, 0.1000000000000000056 ) ;
#133101 = LINE ( 'NONE', #113531, #39631 ) ;
#133102 = VECTOR ( 'NONE', #116735, 1000.000000000000000 ) ;
#133104 = VECTOR ( 'NONE', #182732, 1000.000000000000000 ) ;
#133103 = CARTESIAN_POINT ( 'NONE',  ( 21.04999999999999716, 8.894723818388550640, -142.4870843231475703 ) ) ;
#133105 = CIRCLE ( 'NONE', #53976, 0.09999999999998807065 ) ;
#133106 = AXIS2_PLACEMENT_3D ( 'NONE', #180925, #2260, #55799 ) ;
#133107 = ORIENTED_EDGE ( 'NONE', *, *, #80264, .F. ) ;
#133108 = DIRECTION ( 'NONE',  ( 0.000000000000000000, 0.000000000000000000, -1.000000000000000000 ) ) ;
#133109 = VECTOR ( 'NONE', #17810, 1000.000000000000000 ) ;
#133110 = CARTESIAN_POINT ( 'NONE',  ( 21.05000000000000071, 5.900000000011162093, -157.2809002353436654 ) ) ;
#133111 = CARTESIAN_POINT ( 'NONE',  ( 19.75857864376268935, 11.65000000000000391, -24.75000000000000000 ) ) ;
#133112 = DIRECTION ( 'NONE',  ( 1.000000000000000000, -0.000000000000000000, -0.000000000000000000 ) ) ;
#133113 = CARTESIAN_POINT ( 'NONE',  ( 21.11825140030089898, 65.53721733114183223, -242.0739286986531908 ) ) ;
#133115 = CARTESIAN_POINT ( 'NONE',  ( 22.39999999999999858, 0.1000000000111554016, -92.70922040162665212 ) ) ;
#133114 = CARTESIAN_POINT ( 'NONE',  ( 18.59999999999999076, 76.00000000001190870, -103.0231074845243029 ) ) ;
#133116 = CARTESIAN_POINT ( 'NONE',  ( -16.97683809663752186, 66.05000000001224691, -149.9254715027207396 ) ) ;
#133117 = ORIENTED_EDGE ( 'NONE', *, *, #25457, .T. ) ;
#133119 = DIRECTION ( 'NONE',  ( 0.000000000000000000, -0.000000000000000000, -1.000000000000000000 ) ) ;
#133118 = DIRECTION ( 'NONE',  ( 0.000000000000000000, 0.1350103645451945777, -0.9908441862701591329 ) ) ;
#133120 = ORIENTED_EDGE ( 'NONE', *, *, #62322, .F. ) ;
#133122 = ORIENTED_EDGE ( 'NONE', *, *, #189274, .T. ) ;
#133121 = DIRECTION ( 'NONE',  ( 1.000000000000000000, 0.000000000000000000, 0.000000000000000000 ) ) ;
#133123 = ORIENTED_EDGE ( 'NONE', *, *, #240391, .T. ) ;
#133124 = DIRECTION ( 'NONE',  ( -0.000000000000000000, -0.3427706569149662763, 0.9394191166662954062 ) ) ;
#133125 = CARTESIAN_POINT ( 'NONE',  ( 15.69410316191959254, 66.64325398293399871, -152.8197477631602226 ) ) ;
#133126 = DIRECTION ( 'NONE',  ( 0.000000000000000000, -2.498001805406600196E-13, -1.000000000000000000 ) ) ;
#133127 = DIRECTION ( 'NONE',  ( -1.000000000000000000, -0.000000000000000000, -0.000000000000000000 ) ) ;
#133128 = ORIENTED_EDGE ( 'NONE', *, *, #223610, .F. ) ;
#133129 = DIRECTION ( 'NONE',  ( 0.000000000000000000, 0.000000000000000000, 1.000000000000000000 ) ) ;
#133130 = FACE_OUTER_BOUND ( 'NONE', #145059, .T. ) ;
#133131 = ORIENTED_EDGE ( 'NONE', *, *, #182801, .T. ) ;
#133132 = TOROIDAL_SURFACE ( 'NONE', #58277, 3.899999999999999467, 0.1000000000000000056 ) ;
#133133 = DIRECTION ( 'NONE',  ( 0.000000000000000000, -1.000000000000000000, -6.982962677686266711E-15 ) ) ;
#133134 = CIRCLE ( 'NONE', #257976, 11.65000000000000213 ) ;
#133135 = EDGE_CURVE ( 'NONE', #104349, #148687, #44320, .T. ) ;
#133136 = DIRECTION ( 'NONE',  ( 1.000000000000000000, -3.265361837132813093E-16, -2.280189983783949500E-30 ) ) ;
#133137 = ORIENTED_EDGE ( 'NONE', *, *, #79651, .F. ) ;
#133138 = CARTESIAN_POINT ( 'NONE',  ( -21.05000000000000071, 76.00000000001162448, -66.62310748452433984 ) ) ;
#133139 = VECTOR ( 'NONE', #17240, 1000.000000000000000 ) ;
#133140 = EDGE_LOOP ( 'NONE', ( #167297, #45306, #67084 ) ) ;
#133141 = CARTESIAN_POINT ( 'NONE',  ( 18.52643265882457868, 65.68026841930898740, -97.47257401318893244 ) ) ;
#133142 = ORIENTED_EDGE ( 'NONE', *, *, #46394, .T. ) ;
#133143 = DIRECTION ( 'NONE',  ( 1.000000000000000000, 2.885090398161910739E-16, 6.283419270304611573E-17 ) ) ;
#133144 = EDGE_CURVE ( 'NONE', #98368, #149939, #192550, .T. ) ;
#133145 = FACE_OUTER_BOUND ( 'NONE', #167798, .T. ) ;
#133146 = DIRECTION ( 'NONE',  ( -0.000000000000000000, -6.982962677686266711E-15, 1.000000000000000000 ) ) ;
#133147 = EDGE_CURVE ( 'NONE', #154121, #239256, #5145, .T. ) ;
#133148 = DIRECTION ( 'NONE',  ( 0.000000000000000000, -7.172728831056617961E-15, 1.000000000000000000 ) ) ;
#133149 = VECTOR ( 'NONE', #251073, 1000.000000000000000 ) ;
#133150 = CIRCLE ( 'NONE', #66513, 0.09999999999999939493 ) ;
#133151 = LINE ( 'NONE', #127051, #204533 ) ;
#133153 = ADVANCED_FACE ( 'NONE', ( #65143 ), #125142, .F. ) ;
#133152 = B_SPLINE_CURVE_WITH_KNOTS ( 'NONE', 3,
 ( #178983, #156842, #236344, #58959, #177690, #199810, #18591 ),
 .UNSPECIFIED., .F., .F.,
 ( 4, 3, 4 ),
 ( 0.000000000000000000, 1.860045280645600797E-05, 5.251155757304835946E-05 ),
 .UNSPECIFIED. ) ;
#133154 = CARTESIAN_POINT ( 'NONE',  ( 18.33996824403467940, -9.569639859420588479, -73.81906563751665828 ) ) ;
#133155 = CARTESIAN_POINT ( 'NONE',  ( 21.05000000000000071, 76.00000000001229239, -157.8731074845243540 ) ) ;
#133156 = ORIENTED_EDGE ( 'NONE', *, *, #254265, .T. ) ;
#133158 = DIRECTION ( 'NONE',  ( 3.616040088954490704E-32, 7.105427357601001859E-15, -1.000000000000000000 ) ) ;
#133157 = VECTOR ( 'NONE', #146703, 1000.000000000000000 ) ;
#133159 = ORIENTED_EDGE ( 'NONE', *, *, #214338, .T. ) ;
#133162 = ORIENTED_EDGE ( 'NONE', *, *, #232768, .T. ) ;
#133161 = DIRECTION ( 'NONE',  ( 0.000000000000000000, -0.000000000000000000, 1.000000000000000000 ) ) ;
#133160 = DIRECTION ( 'NONE',  ( -0.000000000000000000, 0.000000000000000000, 1.000000000000000000 ) ) ;
#133163 = ORIENTED_EDGE ( 'NONE', *, *, #96245, .F. ) ;
#133164 = PLANE ( 'NONE',  #255798 ) ;
#133165 = CARTESIAN_POINT ( 'NONE',  ( 23.24999999999999645, -3.899999999988843502, -134.0000000000000284 ) ) ;
#133166 = DIRECTION ( 'NONE',  ( 1.000000000000000000, -0.000000000000000000, -0.000000000000000000 ) ) ;
#133167 = CARTESIAN_POINT ( 'NONE',  ( 20.95512820512820440, 58.98414156600839675, -225.6766266970810477 ) ) ;
#133168 = ORIENTED_EDGE ( 'NONE', *, *, #54155, .T. ) ;
#133170 = ORIENTED_EDGE ( 'NONE', *, *, #94094, .T. ) ;
#133169 = DIRECTION ( 'NONE',  ( 0.000000000000000000, 6.982962677686266711E-15, -1.000000000000000000 ) ) ;
#133171 = EDGE_CURVE ( 'NONE', #256381, #172386, #50875, .T. ) ;
#133172 =( BOUNDED_SURFACE ( )  B_SPLINE_SURFACE ( 3, 2, ( 
 ( #17945, #162613, #177058 ),
 ( #83025, #157510, #58337 ),
 ( #80452, #178341, #57055 ),
 ( #137881, #136602, #79194 ),
 ( #139156, #160061, #119640 ),
 ( #140457, #37536, #199163 ) ),
 .UNSPECIFIED., .F., .F., .F. ) 
 B_SPLINE_SURFACE_WITH_KNOTS ( ( 4, 2, 4 ),
 ( 3, 3 ),
 ( 0.0001792624049599592486, 0.0003686986002124714528, 0.0005581347954649836570 ),
 ( 0.000000000000000000, 1.000000000000000000 ),
 .UNSPECIFIED. ) 
 GEOMETRIC_REPRESENTATION_ITEM ( )  RATIONAL_B_SPLINE_SURFACE ( (
 ( 1.000000000000000000, 0.9238795325112837409, 1.000000000000000000),
 ( 1.000000000000000000, 0.9229318695238861725, 1.000000000000000000),
 ( 1.000000000000000000, 0.8926288119230176843, 1.000000000000000000),
 ( 1.000000000000000000, 0.8123777807271899132, 1.000000000000000000),
 ( 1.000000000000000000, 0.7629087100931073451, 1.000000000000000000),
 ( 1.000000000000000000, 0.7071067811865475727, 1.000000000000000000) ) ) 
 REPRESENTATION_ITEM ( '' )  SURFACE ( )  );
#133174 = CARTESIAN_POINT ( 'NONE',  ( -16.91256925476572093, 66.01426884188440170, -190.9907499735296881 ) ) ;
#133173 = DIRECTION ( 'NONE',  ( 0.000000000000000000, 0.000000000000000000, 1.000000000000000000 ) ) ;
#133176 = ORIENTED_EDGE ( 'NONE', *, *, #154139, .T. ) ;
#133175 = DIRECTION ( 'NONE',  ( 0.000000000000000000, -1.000000000000000000, 0.000000000000000000 ) ) ;
#133177 = AXIS2_PLACEMENT_3D ( 'NONE', #227728, #131196, #129907 ) ;
#133178 = AXIS2_PLACEMENT_3D ( 'NONE', #198563, #194750, #179048 ) ;
#133179 = ORIENTED_EDGE ( 'NONE', *, *, #238745, .T. ) ;
#133180 = B_SPLINE_CURVE_WITH_KNOTS ( 'NONE', 3,
 ( #5656, #128211, #245592, #147779, #33009, #209027, #206456, #29152, #108639, #227297 ),
 .UNSPECIFIED., .F., .F.,
 ( 4, 2, 2, 2, 4 ),
 ( 5.248391470688752094E-16, 9.930191194500769870E-05, 0.0001986038238894905622, 0.0003972076477784563164, 0.0007944152955563376804 ),
 .UNSPECIFIED. ) ;
#133181 = CARTESIAN_POINT ( 'NONE',  ( 22.49533356619864222, 11.65000000631534149, -167.4348774196771501 ) ) ;
#133182 = DIRECTION ( 'NONE',  ( 1.000000000000000000, 0.000000000000000000, -0.000000000000000000 ) ) ;
#133183 = VERTEX_POINT ( 'NONE', #109396 ) ;
#133184 = CARTESIAN_POINT ( 'NONE',  ( 23.14999999999999503, 23.34004772283015683, -229.2004250369967338 ) ) ;
#133185 = ORIENTED_EDGE ( 'NONE', *, *, #75736, .F. ) ;
#133186 =( BOUNDED_SURFACE ( )  B_SPLINE_SURFACE ( 3, 2, ( 
 ( #118739, #83412, #100414 ),
 ( #219087, #198248, #79570 ),
 ( #159159, #40511, #22208 ),
 ( #241254, #80856, #78293 ) ),
 .UNSPECIFIED., .F., .F., .F. ) 
 B_SPLINE_SURFACE_WITH_KNOTS ( ( 4, 4 ),
 ( 3, 3 ),
 ( -2.710505431213761085E-20, 0.0003124336117481265837 ),
 ( 0.000000000000000000, 1.000000000000000000 ),
 .UNSPECIFIED. ) 
 GEOMETRIC_REPRESENTATION_ITEM ( )  RATIONAL_B_SPLINE_SURFACE ( (
 ( 1.000000000000000000, 0.7040654476015975050, 1.000000000000000000),
 ( 1.000000000000000000, 0.7039193538782316795, 1.000000000000000000),
 ( 1.000000000000000000, 0.7089171279145296545, 1.000000000000000000),
 ( 1.000000000000000000, 0.7071067811865506814, 1.000000000000000000) ) ) 
 REPRESENTATION_ITEM ( '' )  SURFACE ( )  );
#133187 = CARTESIAN_POINT ( 'NONE',  ( -18.34374000495059676, 11.47316190337362940, -158.2500000000000284 ) ) ;
#133188 = SPHERICAL_SURFACE ( 'NONE', #172424, 0.1000000000000000056 ) ;
#133189 = ORIENTED_EDGE ( 'NONE', *, *, #29307, .T. ) ;
#133190 = CYLINDRICAL_SURFACE ( 'NONE', #129214, 0.5000000000000008882 ) ;
#133191 = AXIS2_PLACEMENT_3D ( 'NONE', #99706, #41075, #155886 ) ;
#133192 = AXIS2_PLACEMENT_3D ( 'NONE', #254784, #193588, #116610 ) ;
#133193 = CIRCLE ( 'NONE', #154086, 0.1999999999999987899 ) ;
#133194 = CIRCLE ( 'NONE', #20793, 1.500000000000001332 ) ;
#133195 = DIRECTION ( 'NONE',  ( -6.938893903907222856E-15, 1.000000000000000000, 0.000000000000000000 ) ) ;
#133196 =( BOUNDED_SURFACE ( )  B_SPLINE_SURFACE ( 3, 2, ( 
 ( #213378, #209540, #193838 ),
 ( #230387, #252500, #93429 ),
 ( #153469, #135115, #173032 ),
 ( #214665, #71336, #72619 ),
 ( #51718, #36052, #73913 ),
 ( #131283, #70055, #212120 ),
 ( #15206, #169163, #94717 ),
 ( #231687, #248665, #174316 ),
 ( #149590, #253779, #210824 ),
 ( #113011, #75189, #115568 ) ),
 .UNSPECIFIED., .F., .F., .F. ) 
 B_SPLINE_SURFACE_WITH_KNOTS ( ( 4, 2, 2, 2, 4 ),
 ( 3, 3 ),
 ( 0.002161241639767785133, 0.002579950749617447234, 0.002789305304542278284, 0.002893982582004694243, 0.002998659859467109768 ),
 ( 0.000000000000000000, 1.000000000000000000 ),
 .UNSPECIFIED. ) 
 GEOMETRIC_REPRESENTATION_ITEM ( )  RATIONAL_B_SPLINE_SURFACE ( (
 ( 1.000000000000000000, 0.7071067811864923947, 1.000000000000000000),
 ( 1.000000000000000000, 0.7632447400662122350, 1.000000000000000000),
 ( 1.000000000000000000, 0.8158073005111775577, 1.000000000000000000),
 ( 1.000000000000000000, 0.8906973462394580654, 1.000000000000000000),
 ( 1.000000000000000000, 0.9149408947800606873, 1.000000000000000000),
 ( 1.000000000000000000, 0.9493368785275470012, 1.000000000000000000),
 ( 1.000000000000000000, 0.9605194247155928178, 1.000000000000000000),
 ( 1.000000000000000000, 0.9803630264781846293, 1.000000000000000000),
 ( 1.000000000000000000, 0.9900844824270638167, 1.000000000000000000),
 ( 1.000000000000000000, 0.9894588281429246290, 1.000000000000000000) ) ) 
 REPRESENTATION_ITEM ( '' )  SURFACE ( )  );
#133197 = EDGE_CURVE ( 'NONE', #218147, #138152, #129980, .T. ) ;
#133198 = VERTEX_POINT ( 'NONE', #10332 ) ;
#133199 = TOROIDAL_SURFACE ( 'NONE', #237433, 11.70000000000000462, 0.1000000000000000056 ) ;
#133200 = EDGE_LOOP ( 'NONE', ( #227208, #14107, #1269, #106559 ) ) ;
#133201 = EDGE_LOOP ( 'NONE', ( #20524, #228618, #27553, #231359 ) ) ;
#133202 = DIRECTION ( 'NONE',  ( 0.000000000000000000, -1.000000000000000000, -6.982962677686265922E-15 ) ) ;
#133203 = ORIENTED_EDGE ( 'NONE', *, *, #209906, .F. ) ;
#133205 = ORIENTED_EDGE ( 'NONE', *, *, #235110, .F. ) ;
#133204 = CARTESIAN_POINT ( 'NONE',  ( 22.47071067811865319, 75.90090754530939421, -110.7431822290223522 ) ) ;
#133206 = EDGE_CURVE ( 'NONE', #73607, #151273, #67720, .T. ) ;
#133207 = ORIENTED_EDGE ( 'NONE', *, *, #228975, .T. ) ;
#133208 = CARTESIAN_POINT ( 'NONE',  ( -20.54999999999999716, 76.00000000001170974, -69.52310748452431710 ) ) ;
#133209 = AXIS2_PLACEMENT_3D ( 'NONE', #170605, #192689, #190123 ) ;
#133210 = ORIENTED_EDGE ( 'NONE', *, *, #150062, .T. ) ;
#133213 = ORIENTED_EDGE ( 'NONE', *, *, #134347, .T. ) ;
#133212 = EDGE_LOOP ( 'NONE', ( #243881, #101575, #54788 ) ) ;
#133211 = DIRECTION ( 'NONE',  ( -2.915501640297154283E-16, 0.9770955615653317272, 0.2128009952263596460 ) ) ;
#133214 = CIRCLE ( 'NONE', #166554, 0.5000000000000004441 ) ;
#133215 = EDGE_CURVE ( 'NONE', #243888, #9700, #84150, .T. ) ;
#133216 = VERTEX_POINT ( 'NONE', #130246 ) ;
#133217 = AXIS2_PLACEMENT_3D ( 'NONE', #40026, #41306, #19140 ) ;
#133218 = CYLINDRICAL_SURFACE ( 'NONE', #100779, 4.049999999999998046 ) ;
#133219 = ORIENTED_EDGE ( 'NONE', *, *, #220810, .F. ) ;
#133220 = DIRECTION ( 'NONE',  ( 1.000000000000000000, 0.000000000000000000, 0.000000000000000000 ) ) ;
#133221 = EDGE_CURVE ( 'NONE', #41155, #117188, #146721, .T. ) ;
#133223 = ORIENTED_EDGE ( 'NONE', *, *, #201061, .F. ) ;
#133222 = DIRECTION ( 'NONE',  ( -1.000000000000000000, 0.000000000000000000, 0.000000000000000000 ) ) ;
#133224 = DIRECTION ( 'NONE',  ( 0.000000000000000000, -1.000000000000000000, 0.000000000000000000 ) ) ;
#133225 = VERTEX_POINT ( 'NONE', #248940 ) ;
#133227 = ORIENTED_EDGE ( 'NONE', *, *, #28187, .T. ) ;
#133226 = EDGE_CURVE ( 'NONE', #194728, #220627, #70323, .T. ) ;
#133228 = ADVANCED_FACE ( 'NONE', ( #212381 ), #72889, .T. ) ;
#133229 = CARTESIAN_POINT ( 'NONE',  ( -23.15000000000000213, 2.000000000011154189, -154.2753780772379173 ) ) ;
#133230 = ORIENTED_EDGE ( 'NONE', *, *, #191068, .F. ) ;
#133232 = ORIENTED_EDGE ( 'NONE', *, *, #80833, .F. ) ;
#133231 = CARTESIAN_POINT ( 'NONE',  ( -18.59999999999999787, -1.637172712959223952, -78.58215336547205254 ) ) ;
#133233 = VECTOR ( 'NONE', #187337, 1000.000000000000000 ) ;
#133234 = CARTESIAN_POINT ( 'NONE',  ( 19.58285714285715073, 66.98499851036351060, -128.1024546684426468 ) ) ;
#133235 = EDGE_CURVE ( 'NONE', #55374, #7110, #12910, .T. ) ;
#133237 = VERTEX_POINT ( 'NONE', #11615 ) ;
#133236 = ORIENTED_EDGE ( 'NONE', *, *, #150311, .F. ) ;
#133238 = VERTEX_POINT ( 'NONE', #113265 ) ;
#133239 = LINE ( 'NONE', #112403, #211674 ) ;
#133240 = EDGE_LOOP ( 'NONE', ( #185080, #59670, #62083, #126858 ) ) ;
#133241 = ORIENTED_EDGE ( 'NONE', *, *, #22698, .T. ) ;
#133242 = CARTESIAN_POINT ( 'NONE',  ( 23.14999999999999503, 69.35000000001254250, -182.1731074845243938 ) ) ;
#133243 = AXIS2_PLACEMENT_3D ( 'NONE', #226956, #10486, #131709 ) ;
#133244 = VERTEX_POINT ( 'NONE', #110699 ) ;
#133245 = ADVANCED_FACE ( 'NONE', ( #53295 ), #91132, .T. ) ;
#133246 = DIRECTION ( 'NONE',  ( 1.000000000000000000, 0.000000000000000000, 0.000000000000000000 ) ) ;
#133247 = EDGE_CURVE ( 'NONE', #126077, #26209, #200741, .T. ) ;
#133248 = CARTESIAN_POINT ( 'NONE',  ( -13.40000000000000036, -9.650000000000005684, 17.60000000000000497 ) ) ;
#133249 = EDGE_LOOP ( 'NONE', ( #12991, #105372, #172507, #163012 ) ) ;
#133250 = ORIENTED_EDGE ( 'NONE', *, *, #214199, .T. ) ;
#133251 = DIRECTION ( 'NONE',  ( 0.000000000000000000, 0.6728971962617862346, -0.7397360091701815632 ) ) ;
#133253 = VERTEX_POINT ( 'NONE', #48150 ) ;
#133252 = AXIS2_PLACEMENT_3D ( 'NONE', #211033, #14137, #92355 ) ;
#133254 = AXIS2_PLACEMENT_3D ( 'NONE', #59640, #197893, #36285 ) ;
#133255 = DIRECTION ( 'NONE',  ( -3.265361837132813093E-16, 1.000000000000000000, 0.000000000000000000 ) ) ;
#133256 = ORIENTED_EDGE ( 'NONE', *, *, #241541, .F. ) ;
#133257 = EDGE_CURVE ( 'NONE', #17884, #88196, #171999, .T. ) ;
#133258 = ORIENTED_EDGE ( 'NONE', *, *, #219234, .F. ) ;
#133259 = CIRCLE ( 'NONE', #112423, 0.1000000000000054040 ) ;
#133260 = ADVANCED_FACE ( 'NONE', ( #151117 ), #152423, .F. ) ;
#133261 = CARTESIAN_POINT ( 'NONE',  ( 20.84999999999998721, 64.25000000001170974, -69.52310748452438816 ) ) ;
#133263 = ORIENTED_EDGE ( 'NONE', *, *, #22087, .T. ) ;
#133262 = CARTESIAN_POINT ( 'NONE',  ( 18.41789779300671981, 85.50000000001233502, -162.9910378181636474 ) ) ;
#133264 = DIRECTION ( 'NONE',  ( 0.000000000000000000, -0.9908441862701596881, 0.1350103645451899148 ) ) ;
#133265 = CARTESIAN_POINT ( 'NONE',  ( -17.78241384938698744, 32.75037188247295461, -235.1425015842832806 ) ) ;
#133266 = CIRCLE ( 'NONE', #83347, 0.4000000000000114575 ) ;
#133267 = CARTESIAN_POINT ( 'NONE',  ( 20.95520789717937404, 65.42306940062712783, -128.9428745106495171 ) ) ;
#133269 = AXIS2_PLACEMENT_3D ( 'NONE', #150124, #6737, #189238 ) ;
#133268 = DIRECTION ( 'NONE',  ( -0.7071067811865127117, -0.7071067811865821007, 0.000000000000000000 ) ) ;
#133270 = DIRECTION ( 'NONE',  ( 0.000000000000000000, 0.4088369013363241100, -0.9126074666063788143 ) ) ;
#133271 = LINE ( 'NONE', #188107, #194071 ) ;
#133272 = CARTESIAN_POINT ( 'NONE',  ( 21.00000000000000000, 9.749999999999998224, -21.15000000000000213 ) ) ;
#133273 = CARTESIAN_POINT ( 'NONE',  ( 21.14999999999999858, 76.10000000001222986, -148.1726782920690937 ) ) ;
#133274 = FACE_OUTER_BOUND ( 'NONE', #187473, .T. ) ;
#133275 = ADVANCED_FACE ( 'NONE', ( #28650 ), #192811, .T. ) ;
#133276 = CARTESIAN_POINT ( 'NONE',  ( 22.49436431346199683, 75.93309647028996778, -148.1730584321777542 ) ) ;
#133277 = DIRECTION ( 'NONE',  ( 0.000000000000000000, 0.000000000000000000, 1.000000000000000000 ) ) ;
#133278 = ORIENTED_EDGE ( 'NONE', *, *, #23770, .F. ) ;
#133279 = AXIS2_PLACEMENT_3D ( 'NONE', #1191, #81996, #193325 ) ;
#133280 = VECTOR ( 'NONE', #226082, 1000.000000000000000 ) ;
#133281 = CIRCLE ( 'NONE', #141642, 0.1000000000000055705 ) ;
#133282 = AXIS2_PLACEMENT_3D ( 'NONE', #73981, #133908, #236859 ) ;
#133283 = AXIS2_PLACEMENT_3D ( 'NONE', #209463, #129916, #128661 ) ;
#133285 = VERTEX_POINT ( 'NONE', #9030 ) ;
#133284 = ORIENTED_EDGE ( 'NONE', *, *, #161247, .F. ) ;
#133286 = ORIENTED_EDGE ( 'NONE', *, *, #28764, .T. ) ;
#133287 = CIRCLE ( 'NONE', #99378, 5.000000000000000888 ) ;
#133288 = CARTESIAN_POINT ( 'NONE',  ( 21.09610168723072832, 75.96641049312121652, -209.9020631997491364 ) ) ;
#133289 = DIRECTION ( 'NONE',  ( -0.000000000000000000, 6.982962677686266711E-15, -1.000000000000000000 ) ) ;
#133291 = DIRECTION ( 'NONE',  ( 0.000000000000000000, 6.982962677686266711E-15, -1.000000000000000000 ) ) ;
#133290 = CARTESIAN_POINT ( 'NONE',  ( -20.54999999999999716, 68.56901367119438362, -214.3038979092079046 ) ) ;
#133292 = ORIENTED_EDGE ( 'NONE', *, *, #8430, .T. ) ;
#133293 = VERTEX_POINT ( 'NONE', #168152 ) ;
#133294 = EDGE_CURVE ( 'NONE', #176136, #113811, #221557, .T. ) ;
#133295 = SURFACE_STYLE_USAGE ( .BOTH. , #55010 ) ;
#133296 = DIRECTION ( 'NONE',  ( 7.304098846218135653E-16, -0.9770955615653315052, -0.2128009952263603954 ) ) ;
#133297 = FACE_OUTER_BOUND ( 'NONE', #216757, .T. ) ;
#133298 = EDGE_CURVE ( 'NONE', #205408, #91770, #58388, .T. ) ;
#133299 = CARTESIAN_POINT ( 'NONE',  ( -20.54999999999999716, 71.65000000001207070, -124.1731074845243228 ) ) ;
#133300 = ORIENTED_EDGE ( 'NONE', *, *, #23161, .F. ) ;
#133301 = ORIENTED_EDGE ( 'NONE', *, *, #42703, .F. ) ;
#133302 = CARTESIAN_POINT ( 'NONE',  ( -16.87036670365548474, 66.01058118071060221, -149.0435473672224020 ) ) ;
#133303 = DIRECTION ( 'NONE',  ( -1.000000000000000000, -0.000000000000000000, -0.000000000000000000 ) ) ;
#133304 = EDGE_CURVE ( 'NONE', #120342, #73323, #34861, .T. ) ;
#133305 = ADVANCED_FACE ( 'NONE', ( #199227 ), #174580, .F. ) ;
#133306 = EDGE_LOOP ( 'NONE', ( #221032, #131171, #196602, #241847 ) ) ;
#133307 = DIRECTION ( 'NONE',  ( 0.000000000000000000, 0.000000000000000000, -1.000000000000000000 ) ) ;
#133309 = VERTEX_POINT ( 'NONE', #238336 ) ;
#133308 = CARTESIAN_POINT ( 'NONE',  ( 18.39999999999999858, 77.43243075322052960, -241.6948671442531520 ) ) ;
#133310 = CARTESIAN_POINT ( 'NONE',  ( -20.54999999999999716, -8.999999999988844479, -124.1060308773475924 ) ) ;
#133311 = LINE ( 'NONE', #212850, #248269 ) ;
#133312 = ADVANCED_FACE ( 'NONE', ( #139214 ), #254043, .F. ) ;
#133313 = CYLINDRICAL_SURFACE ( 'NONE', #12589, 0.09999999999999609201 ) ;
#133314 = ORIENTED_EDGE ( 'NONE', *, *, #5853, .F. ) ;
#133315 = DIRECTION ( 'NONE',  ( 0.000000000000000000, 0.1575844902526835067, 0.9875055080513738259 ) ) ;
#133316 = CARTESIAN_POINT ( 'NONE',  ( -18.59999999999999787, 9.350000000011156942, -79.15000000000003411 ) ) ;
#133317 = SPHERICAL_SURFACE ( 'NONE', #44408, 0.1000000000000000056 ) ;
#133319 = DIRECTION ( 'NONE',  ( 0.000000000000000000, 0.000000000000000000, 1.000000000000000000 ) ) ;
#133318 = PLANE ( 'NONE',  #190816 ) ;
#133320 = CARTESIAN_POINT ( 'NONE',  ( -18.50000000000000711, 64.35000000001264198, -196.5083017138704236 ) ) ;
#133321 = VECTOR ( 'NONE', #12971, 1000.000000000000000 ) ;
#133322 = LINE ( 'NONE', #15968, #166447 ) ;
#133323 = CARTESIAN_POINT ( 'NONE',  ( 18.59999999999999787, -11.75000000000000000, 6.100000000000001421 ) ) ;
#133324 = CARTESIAN_POINT ( 'NONE',  ( 21.70464131381650219, 7.095358018979006864, -33.50000000000000000 ) ) ;
#133326 = ORIENTED_EDGE ( 'NONE', *, *, #172165, .T. ) ;
#133325 = AXIS2_PLACEMENT_3D ( 'NONE', #96429, #16928, #119894 ) ;
#133327 = EDGE_CURVE ( 'NONE', #82047, #241131, #195394, .T. ) ;
#133328 = EDGE_CURVE ( 'NONE', #81824, #122006, #18002, .T. ) ;
#133329 = VERTEX_POINT ( 'NONE', #98791 ) ;
#133330 = CARTESIAN_POINT ( 'NONE',  ( -23.25000000000000000, 71.65000000001259650, -191.3731074845243825 ) ) ;
#133331 = LINE ( 'NONE', #108626, #161063 ) ;
#133332 = VERTEX_POINT ( 'NONE', #175824 ) ;
#133333 = EDGE_CURVE ( 'NONE', #99212, #11251, #234224, .T. ) ;
#133334 = CARTESIAN_POINT ( 'NONE',  ( 19.90000000000000568, 1.350000000000000089, 0.000000000000000000 ) ) ;
#133335 = ORIENTED_EDGE ( 'NONE', *, *, #131285, .F. ) ;
#133336 = AXIS2_PLACEMENT_3D ( 'NONE', #51753, #251249, #10087 ) ;
#133337 =( LENGTH_UNIT ( ) NAMED_UNIT ( * ) SI_UNIT ( .MILLI., .METRE. ) );
#133338 = ORIENTED_EDGE ( 'NONE', *, *, #107381, .F. ) ;
#133339 = ADVANCED_FACE ( 'NONE', ( #16746 ), #252757, .F. ) ;
#133341 = EDGE_CURVE ( 'NONE', #245454, #141252, #75450, .T. ) ;
#133340 = VECTOR ( 'NONE', #34221, 1000.000000000000000 ) ;
#133342 = ORIENTED_EDGE ( 'NONE', *, *, #154948, .T. ) ;
#133343 = AXIS2_PLACEMENT_3D ( 'NONE', #105724, #164455, #143596 ) ;
#133344 = DIRECTION ( 'NONE',  ( 0.000000000000000000, -0.4930308989875248349, -0.8700118002898312719 ) ) ;
#133345 = LINE ( 'NONE', #48655, #194794 ) ;
#133346 = CARTESIAN_POINT ( 'NONE',  ( -21.05000000000000071, 70.10000000001251408, -180.2422072491807796 ) ) ;
#133347 = EDGE_CURVE ( 'NONE', #75413, #133057, #238524, .T. ) ;
#133348 = DIRECTION ( 'NONE',  ( 0.000000000000000000, 0.000000000000000000, -1.000000000000000000 ) ) ;
#133349 = CARTESIAN_POINT ( 'NONE',  ( -20.54999999999999716, 0.000000000000000000, -33.50000000000000000 ) ) ;
#133351 = ORIENTED_EDGE ( 'NONE', *, *, #170819, .T. ) ;
#133350 = CARTESIAN_POINT ( 'NONE',  ( -18.59999999999999787, 43.02787096365918984, -254.3959382439171577 ) ) ;
#133353 = DIRECTION ( 'NONE',  ( 1.000000000000000000, 0.000000000000000000, 0.000000000000000000 ) ) ;
#133352 = CARTESIAN_POINT ( 'NONE',  ( -20.85000000000000142, -11.74999999998884448, -164.6000000000000227 ) ) ;
#133354 = CARTESIAN_POINT ( 'NONE',  ( -17.11825945287481687, 9.949999999999983302, -20.75000000000000000 ) ) ;
#133355 = EDGE_CURVE ( 'NONE', #71652, #74229, #30253, .T. ) ;
#133356 = CARTESIAN_POINT ( 'NONE',  ( 14.56326696814971200, 66.55335100938319215, -121.4339441886011883 ) ) ;
#133357 = CARTESIAN_POINT ( 'NONE',  ( 23.24999999999999289, 11.75000000001116263, -122.2500000000000284 ) ) ;
#133358 = CARTESIAN_POINT ( 'NONE',  ( -21.06715728752538652, 11.75000000001115197, -40.51480577065400013 ) ) ;
#133359 = ORIENTED_EDGE ( 'NONE', *, *, #60318, .F. ) ;
#133360 = EDGE_CURVE ( 'NONE', #69468, #74968, #216195, .T. ) ;
#133361 =( NAMED_UNIT ( * ) PLANE_ANGLE_UNIT ( ) SI_UNIT ( $, .RADIAN. ) );
#133362 = CARTESIAN_POINT ( 'NONE',  ( -23.25000000000000000, 76.00000000001168132, -65.62310748452431142 ) ) ;
#133363 = CIRCLE ( 'NONE', #145816, 0.09999999999999910349 ) ;
#133364 = AXIS2_PLACEMENT_3D ( 'NONE', #27382, #243812, #65170 ) ;
#133365 = ORIENTED_EDGE ( 'NONE', *, *, #156919, .F. ) ;
#133366 = DIRECTION ( 'NONE',  ( 0.000000000000000000, -0.5273008465187821736, 0.8496786552930323255 ) ) ;
#133367 = VERTEX_POINT ( 'NONE', #233237 ) ;
#133368 = CARTESIAN_POINT ( 'NONE',  ( -20.85000000000000142, -1.164121893230052995, -208.9148480855715775 ) ) ;
#133369 = CYLINDRICAL_SURFACE ( 'NONE', #115893, 0.09999999999999939493 ) ;
#133370 = EDGE_CURVE ( 'NONE', #286, #30493, #246703, .T. ) ;
#133371 = EDGE_LOOP ( 'NONE', ( #176795, #163841, #16169, #225999 ) ) ;
#133372 = ORIENTED_EDGE ( 'NONE', *, *, #220098, .F. ) ;
#133374 = EDGE_CURVE ( 'NONE', #4584, #15317, #36313, .T. ) ;
#133373 = CARTESIAN_POINT ( 'NONE',  ( 20.73486653747088226, 68.75000000001257661, -190.8731074845244109 ) ) ;
#133375 = DIRECTION ( 'NONE',  ( -0.000000000000000000, 0.8660254037844377084, 0.5000000000000016653 ) ) ;
#133376 = AXIS2_PLACEMENT_3D ( 'NONE', #192142, #170037, #188263 ) ;
#133377 = DIRECTION ( 'NONE',  ( 0.000000000000000000, 0.9770955615653551529, 0.2128009952262517601 ) ) ;
#133379 = CARTESIAN_POINT ( 'NONE',  ( -18.46902351632712680, -9.509470118669714367, -140.9864539342573266 ) ) ;
#133378 = TOROIDAL_SURFACE ( 'NONE', #71036, 11.65000000000000036, 0.1000000000000000056 ) ;
#133380 = AXIS2_PLACEMENT_3D ( 'NONE', #235093, #58978, #18605 ) ;
#133383 = CARTESIAN_POINT ( 'NONE',  ( 18.49999999999999289, 10.49142135624846439, -158.8500000000000227 ) ) ;
#133382 = AXIS2_PLACEMENT_3D ( 'NONE', #178250, #257693, #79095 ) ;
#133381 = PLANE ( 'NONE',  #225723 ) ;
#133384 = CARTESIAN_POINT ( 'NONE',  ( -21.59142135623730852, 68.15000000001228386, -157.7731074845244166 ) ) ;
#133385 = LINE ( 'NONE', #212915, #69066 ) ;
#133386 = DIRECTION ( 'NONE',  ( 1.000000000000000000, 0.000000000000000000, 0.000000000000000000 ) ) ;
#133387 = ORIENTED_EDGE ( 'NONE', *, *, #103192, .T. ) ;
#133388 = DIRECTION ( 'NONE',  ( -1.000000000000000000, -0.000000000000000000, -0.000000000000000000 ) ) ;
#133390 = ORIENTED_EDGE ( 'NONE', *, *, #134336, .F. ) ;
#133389 = DIRECTION ( 'NONE',  ( -1.000000000000000000, -0.000000000000000000, -0.000000000000000000 ) ) ;
#133391 = CARTESIAN_POINT ( 'NONE',  ( 20.95052659398289308, 65.52017563223272134, -195.9478687286588183 ) ) ;
#133392 = DIRECTION ( 'NONE',  ( 0.7071067811865127117, 0.7071067811865821007, 0.000000000000000000 ) ) ;
#133394 = DIRECTION ( 'NONE',  ( 4.026293107431335996E-15, -0.09425075112712516523, -0.9955484899852807823 ) ) ;
#133393 = CARTESIAN_POINT ( 'NONE',  ( -23.15000000000000213, -8.999999999988846255, -143.8939691226524644 ) ) ;
#133395 = EDGE_CURVE ( 'NONE', #128191, #194795, #121828, .T. ) ;
#133397 = ORIENTED_EDGE ( 'NONE', *, *, #37735, .F. ) ;
#133396 = CARTESIAN_POINT ( 'NONE',  ( -15.39946565075089779, 62.27203542310181206, -218.2690822304508629 ) ) ;
#133398 = LINE ( 'NONE', #192100, #184162 ) ;
#133399 = DIRECTION ( 'NONE',  ( 1.000000000000000000, 7.304098846218105085E-16, 4.217023435051676515E-16 ) ) ;
#133400 = CARTESIAN_POINT ( 'NONE',  ( -23.25000000000000000, 64.35000000001222986, -148.6731074845244507 ) ) ;
#133401 = DIRECTION ( 'NONE',  ( 1.000000000000000000, 0.000000000000000000, 0.000000000000000000 ) ) ;
#133402 = CARTESIAN_POINT ( 'NONE',  ( -18.55807992284872299, 10.32898536001801304, -139.5826683222764757 ) ) ;
#133403 = ORIENTED_EDGE ( 'NONE', *, *, #177976, .T. ) ;
#133404 = CARTESIAN_POINT ( 'NONE',  ( -21.14999999999999858, 11.65000000001115588, -100.6000000000000369 ) ) ;
#133406 = EDGE_LOOP ( 'NONE', ( #144386, #82372, #85463, #55960 ) ) ;
#133405 = AXIS2_PLACEMENT_3D ( 'NONE', #133671, #33331, #248488 ) ;
#133407 = VECTOR ( 'NONE', #35070, 1000.000000000000000 ) ;
#133408 = DIRECTION ( 'NONE',  ( -2.557131231893036985E-16, 0.8660254037844384856, -0.5000000000000002220 ) ) ;
#133409 = ORIENTED_EDGE ( 'NONE', *, *, #48112, .F. ) ;
#133410 = EDGE_CURVE ( 'NONE', #58209, #127492, #9376, .T. ) ;
#133411 = DIRECTION ( 'NONE',  ( 0.000000000000000000, 0.000000000000000000, -1.000000000000000000 ) ) ;
#133412 = EDGE_LOOP ( 'NONE', ( #181122, #801, #63210, #235764 ) ) ;
#133413 = DIRECTION ( 'NONE',  ( -1.000000000000000000, 0.000000000000000000, 0.000000000000000000 ) ) ;
#133414 = DIRECTION ( 'NONE',  ( 1.000000000000000000, 0.000000000000000000, 0.000000000000000000 ) ) ;
#133415 = FACE_OUTER_BOUND ( 'NONE', #1585, .T. ) ;
#133416 = ORIENTED_EDGE ( 'NONE', *, *, #95761, .T. ) ;
#133417 = CARTESIAN_POINT ( 'NONE',  ( -23.25000000000000000, 76.10000000001222986, -148.1726782920690937 ) ) ;
#133418 = CARTESIAN_POINT ( 'NONE',  ( 23.15000000000000213, -11.48912529306489816, -63.89999999999999858 ) ) ;
#133419 = DIRECTION ( 'NONE',  ( -0.7071067811865389130, -5.024295867788141276E-15, 0.7071067811865561215 ) ) ;
#133420 = CARTESIAN_POINT ( 'NONE',  ( -20.54999999999999716, 7.250000000011155521, -188.6499999999999488 ) ) ;
#133422 = CARTESIAN_POINT ( 'NONE',  ( -23.25000000000000000, 67.74990736105834799, -227.9721689390126755 ) ) ;
#133421 = CIRCLE ( 'NONE', #58570, 0.1000000000000024342 ) ;
#133423 = ORIENTED_EDGE ( 'NONE', *, *, #56258, .T. ) ;
#133424 = CARTESIAN_POINT ( 'NONE',  ( -18.31331870001040940, 85.53629471919306582, -129.6545287935387307 ) ) ;
#133425 = ORIENTED_EDGE ( 'NONE', *, *, #52716, .F. ) ;
#133427 = ORIENTED_EDGE ( 'NONE', *, *, #227507, .F. ) ;
#133426 = CARTESIAN_POINT ( 'NONE',  ( -18.40000000000000213, 28.17589918783267322, -238.5974746063260739 ) ) ;
#133428 = ORIENTED_EDGE ( 'NONE', *, *, #55774, .T. ) ;
#133429 = CARTESIAN_POINT ( 'NONE',  ( 18.46858270002953262, 85.47420267472320177, -196.4210855498204467 ) ) ;
#133430 = DIRECTION ( 'NONE',  ( 1.000000000000000000, 0.000000000000000000, 0.000000000000000000 ) ) ;
#133431 = DIRECTION ( 'NONE',  ( 0.000000000000000000, 0.000000000000000000, -1.000000000000000000 ) ) ;
#133432 = CIRCLE ( 'NONE', #87613, 0.09999999999999939493 ) ;
#133433 = ORIENTED_EDGE ( 'NONE', *, *, #154463, .F. ) ;
#133434 = CARTESIAN_POINT ( 'NONE',  ( -16.86733706339143524, 66.03400947037184210, -48.61999218252569932 ) ) ;
#133435 = CARTESIAN_POINT ( 'NONE',  ( 18.59999999999999432, -1.637172712959223952, -112.0821533654720383 ) ) ;
#133436 = ORIENTED_EDGE ( 'NONE', *, *, #16199, .F. ) ;
#133438 = VERTEX_POINT ( 'NONE', #46539 ) ;
#133437 = CARTESIAN_POINT ( 'NONE',  ( -16.87036670365548474, 66.01058118071034642, -115.5435473672223168 ) ) ;
#133439 = EDGE_CURVE ( 'NONE', #70203, #164631, #126069, .T. ) ;
#133440 = DIRECTION ( 'NONE',  ( 0.000000000000000000, 1.000000000000000000, 0.000000000000000000 ) ) ;
#133441 = CARTESIAN_POINT ( 'NONE',  ( -20.94999999999999929, 87.65000000001235492, -167.1231074845242688 ) ) ;
#133442 = AXIS2_PLACEMENT_3D ( 'NONE', #69942, #245997, #210714 ) ;
#133443 = CIRCLE ( 'NONE', #21036, 11.80000000000000426 ) ;
#133444 = ORIENTED_EDGE ( 'NONE', *, *, #67061, .F. ) ;
#133445 = CARTESIAN_POINT ( 'NONE',  ( -23.25000000000000000, 1.115600667400684642E-11, -113.2750000000000341 ) ) ;
#133446 = CARTESIAN_POINT ( 'NONE',  ( -20.94403535211772294, 18.37039103902859694, -236.9176190769588857 ) ) ;
#133447 = VERTEX_POINT ( 'NONE', #205616 ) ;
#133448 = LINE ( 'NONE', #212984, #12847 ) ;
#133449 = VECTOR ( 'NONE', #246556, 1000.000000000000000 ) ;
#133450 = EDGE_CURVE ( 'NONE', #216916, #73323, #13660, .T. ) ;
#133451 = FACE_OUTER_BOUND ( 'NONE', #72254, .T. ) ;
#133452 = TOROIDAL_SURFACE ( 'NONE', #229324, 11.90000000000000391, 0.1000000000000000056 ) ;
#133453 = AXIS2_PLACEMENT_3D ( 'NONE', #173260, #252725, #54536 ) ;
#133454 = EDGE_CURVE ( 'NONE', #9313, #162761, #974, .T. ) ;
#133455 = DIRECTION ( 'NONE',  ( -1.000000000000000000, 0.000000000000000000, 0.000000000000000000 ) ) ;
#133456 = ADVANCED_FACE ( 'NONE', ( #140507 ), #123534, .T. ) ;
#133457 = CIRCLE ( 'NONE', #21063, 12.87499999999999822 ) ;
#133458 = AXIS2_PLACEMENT_3D ( 'NONE', #77627, #142442, #162035 ) ;
#133459 = ORIENTED_EDGE ( 'NONE', *, *, #171165, .T. ) ;
#133461 = CARTESIAN_POINT ( 'NONE',  ( 21.05000000000000071, 67.22371735104047730, -61.03551510600370023 ) ) ;
#133460 = VECTOR ( 'NONE', #40957, 1000.000000000000000 ) ;
#133462 = EDGE_CURVE ( 'NONE', #60454, #243219, #100911, .T. ) ;
#133463 = VERTEX_POINT ( 'NONE', #225169 ) ;
#133464 = EDGE_CURVE ( 'NONE', #6279, #20693, #242606, .T. ) ;
#133465 = DIRECTION ( 'NONE',  ( 1.000000000000000000, 0.000000000000000000, 0.000000000000000000 ) ) ;
#133466 = CYLINDRICAL_SURFACE ( 'NONE', #74933, 0.09999999999998898659 ) ;
#133468 = EDGE_LOOP ( 'NONE', ( #213703, #148319, #169844, #90428, #107329, #23179 ) ) ;
#133467 = CARTESIAN_POINT ( 'NONE',  ( 21.05000012384916275, 10.62872029888669978, -146.1779773300349632 ) ) ;
#133469 = CARTESIAN_POINT ( 'NONE',  ( -21.05000000000000071, 77.36087058720364951, -61.45010955743335046 ) ) ;
#133470 = LINE ( 'NONE', #112627, #257258 ) ;
#133471 = EDGE_CURVE ( 'NONE', #188436, #173426, #192743, .T. ) ;
#133472 = CARTESIAN_POINT ( 'NONE',  ( 20.99999999999997868, 76.00000000001195133, -103.0231074845243171 ) ) ;
#133473 = CARTESIAN_POINT ( 'NONE',  ( 21.05000000000000071, 65.27628289530457550, -128.8581939154367717 ) ) ;
#133474 = CARTESIAN_POINT ( 'NONE',  ( 21.04999999999999716, 6.441084688482481724, -33.51771943330863479 ) ) ;
#133475 = B_SPLINE_CURVE_WITH_KNOTS ( 'NONE', 3,
 ( #237986, #161042, #184440, #102300, #222257, #244414, #43660, #81458, #201435, #86604, #142734, #22833, #85317, #124488 ),
 .UNSPECIFIED., .F., .F.,
 ( 4, 2, 2, 2, 2, 2, 4 ),
 ( 0.000000000000000000, 2.389617747646589612E-05, 4.779235495293179223E-05, 9.558470990578389560E-05, 0.0001911694198114880752, 0.0003823388396228947811, 0.0007646776792456254140 ),
 .UNSPECIFIED. ) ;
#133476 = DIRECTION ( 'NONE',  ( 0.000000000000000000, 0.9910465087640861759, -0.1335171055202901691 ) ) ;
#133477 = CARTESIAN_POINT ( 'NONE',  ( 18.59999999999999076, 11.75000000001115907, -91.85000000000003695 ) ) ;
#133478 = AXIS2_PLACEMENT_3D ( 'NONE', #18733, #233930, #156987 ) ;
#133480 = ORIENTED_EDGE ( 'NONE', *, *, #83538, .T. ) ;
#133479 = DIRECTION ( 'NONE',  ( 0.000000000000000000, 0.000000000000000000, -1.000000000000000000 ) ) ;
#133481 = ADVANCED_FACE ( 'NONE', ( #81798 ), #82858, .T. ) ;
#133482 = FACE_OUTER_BOUND ( 'NONE', #6250, .T. ) ;
#133483 = CARTESIAN_POINT ( 'NONE',  ( 20.94999999999999574, 87.75000000001264766, -200.6231074845242688 ) ) ;
#133484 = CYLINDRICAL_SURFACE ( 'NONE', #159731, 0.1000000000000052097 ) ;
#133485 = EDGE_LOOP ( 'NONE', ( #112400, #230876, #186880, #6946 ) ) ;
#133486 = DIRECTION ( 'NONE',  ( 1.000000000000000000, 0.000000000000000000, 0.000000000000000000 ) ) ;
#133487 = AXIS2_PLACEMENT_3D ( 'NONE', #240002, #219125, #40551 ) ;
#133488 = EDGE_CURVE ( 'NONE', #246033, #217539, #184777, .T. ) ;
#133489 = CARTESIAN_POINT ( 'NONE',  ( 18.59999999999999432, 77.16270174995010223, -128.4231074845242802 ) ) ;
#133490 = AXIS2_PLACEMENT_3D ( 'NONE', #239698, #58457, #37663 ) ;
#133491 = LINE ( 'NONE', #211754, #257371 ) ;
#133492 = ORIENTED_EDGE ( 'NONE', *, *, #257404, .F. ) ;
#133493 = VECTOR ( 'NONE', #25913, 1000.000000000000000 ) ;
#133494 = FACE_OUTER_BOUND ( 'NONE', #13066, .T. ) ;
#133495 = CARTESIAN_POINT ( 'NONE',  ( -16.93262454970420094, 10.00202046794151300, -79.57292377376273862 ) ) ;
#133496 = EDGE_CURVE ( 'NONE', #154400, #50342, #80258, .T. ) ;
#133498 = ORIENTED_EDGE ( 'NONE', *, *, #100459, .F. ) ;
#133497 = CIRCLE ( 'NONE', #158475, 0.09999999999999939493 ) ;
#133499 = CARTESIAN_POINT ( 'NONE',  ( -20.85000000000000142, 76.00000000001244871, -170.0231074845243597 ) ) ;
#133500 = ORIENTED_EDGE ( 'NONE', *, *, #236081, .F. ) ;
#133502 = EDGE_LOOP ( 'NONE', ( #175037, #122957 ) ) ;
#133501 = CARTESIAN_POINT ( 'NONE',  ( -23.15000000000000213, 85.00000000001188027, -93.12913836187181005 ) ) ;
#133503 = DIRECTION ( 'NONE',  ( 0.000000000000000000, -0.9893560106964500722, 0.1455152366551550613 ) ) ;
#133504 = ORIENTED_EDGE ( 'NONE', *, *, #209051, .F. ) ;
#133505 = CIRCLE ( 'NONE', #21114, 0.1000000000000028644 ) ;
#133506 = DIRECTION ( 'NONE',  ( 0.000000000000000000, -0.9667078373770160438, -0.2558827019433957961 ) ) ;
#133507 = EDGE_LOOP ( 'NONE', ( #95395, #204224, #55686, #88058 ) ) ;
#133509 = VERTEX_POINT ( 'NONE', #43989 ) ;
#133508 = VERTEX_POINT ( 'NONE', #4832 ) ;
#133510 = CARTESIAN_POINT ( 'NONE',  ( -23.15000000000000213, 25.94586868676353575, -241.5435999122864530 ) ) ;
#133512 = ORIENTED_EDGE ( 'NONE', *, *, #160758, .F. ) ;
#133511 = FACE_OUTER_BOUND ( 'NONE', #156689, .T. ) ;
#133513 = EDGE_CURVE ( 'NONE', #163114, #49440, #19114, .T. ) ;
#133514 = DIRECTION ( 'NONE',  ( 1.000000000000000000, 0.000000000000000000, 0.000000000000000000 ) ) ;
#133515 = AXIS2_PLACEMENT_3D ( 'NONE', #221490, #102823, #203229 ) ;
#133516 = VERTEX_POINT ( 'NONE', #242183 ) ;
#133517 = ADVANCED_FACE ( 'NONE', ( #6129 ), #145644, .F. ) ;
#133518 = AXIS2_PLACEMENT_3D ( 'NONE', #197698, #242925, #116892 ) ;
#133519 = ORIENTED_EDGE ( 'NONE', *, *, #9904, .T. ) ;
#133520 = PLANE ( 'NONE',  #70472 ) ;
#133521 = DIRECTION ( 'NONE',  ( 0.000000000000000000, 0.4088369013363281623, -0.9126074666063771490 ) ) ;
#133522 = EDGE_CURVE ( 'NONE', #67031, #20238, #67643, .T. ) ;
#133523 = DIRECTION ( 'NONE',  ( -1.000000000000000000, 0.000000000000000000, 0.000000000000000000 ) ) ;
#133524 = ORIENTED_EDGE ( 'NONE', *, *, #210694, .F. ) ;
#133525 = CARTESIAN_POINT ( 'NONE',  ( 20.94999999999999929, -7.176961358819842651, -212.6889627706600834 ) ) ;
#133526 = DIRECTION ( 'NONE',  ( -0.000000000000000000, -0.000000000000000000, -1.000000000000000000 ) ) ;
#133527 = CARTESIAN_POINT ( 'NONE',  ( -18.59999999999999787, 77.16412189325305349, -95.30825939895268561 ) ) ;
#133529 = VERTEX_POINT ( 'NONE', #50381 ) ;
#133528 = EDGE_CURVE ( 'NONE', #229458, #220002, #146912, .T. ) ;
#133531 = EDGE_CURVE ( 'NONE', #9423, #98837, #163508, .T. ) ;
#133530 = CARTESIAN_POINT ( 'NONE',  ( -23.25000000000000000, 5.950000000000010836, -23.19429769496518645 ) ) ;
#133532 = LINE ( 'NONE', #214355, #223593 ) ;
#133533 = SURFACE_STYLE_USAGE ( .BOTH. , #33195 ) ;
#133534 = AXIS2_PLACEMENT_3D ( 'NONE', #233270, #213676, #235794 ) ;
#133535 = ORIENTED_EDGE ( 'NONE', *, *, #100002, .T. ) ;
#133536 = CARTESIAN_POINT ( 'NONE',  ( -16.97092634996651839, 14.21295061030198781, -219.2636457483668835 ) ) ;
#133537 = ORIENTED_EDGE ( 'NONE', *, *, #98856, .F. ) ;
#133538 = CARTESIAN_POINT ( 'NONE',  ( -18.40000000000000213, -7.817436562502988906, -209.8389866834999111 ) ) ;
#133539 = VERTEX_POINT ( 'NONE', #129927 ) ;
#133540 = CARTESIAN_POINT ( 'NONE',  ( -13.22483237240078857, 24.96309550270879640, -232.5807238286746497 ) ) ;
#133541 = EDGE_CURVE ( 'NONE', #173788, #84389, #47819, .T. ) ;
#133542 = ORIENTED_EDGE ( 'NONE', *, *, #55506, .T. ) ;
#133543 = ORIENTED_EDGE ( 'NONE', *, *, #32363, .F. ) ;
#133544 = DIRECTION ( 'NONE',  ( 0.000000000000000000, 1.000000000000000000, 0.000000000000000000 ) ) ;
#133545 = FACE_OUTER_BOUND ( 'NONE', #235054, .T. ) ;
#133546 = ORIENTED_EDGE ( 'NONE', *, *, #245838, .T. ) ;
#133547 = ORIENTED_EDGE ( 'NONE', *, *, #78740, .T. ) ;
#133548 = DIRECTION ( 'NONE',  ( 0.000000000000000000, -6.982962677686266711E-15, 1.000000000000000000 ) ) ;
#133549 = CARTESIAN_POINT ( 'NONE',  ( -20.85000000000000142, 0.000000000000000000, -33.50000000000000000 ) ) ;
#133550 = ORIENTED_EDGE ( 'NONE', *, *, #34626, .F. ) ;
#133551 = VECTOR ( 'NONE', #85608, 1000.000000000000000 ) ;
#133552 = AXIS2_PLACEMENT_3D ( 'NONE', #254216, #33955, #76870 ) ;
#133553 = AXIS2_PLACEMENT_3D ( 'NONE', #85189, #6971, #227302 ) ;
#133554 = EDGE_LOOP ( 'NONE', ( #152457, #187427, #30459, #62539 ) ) ;
#133555 = AXIS2_PLACEMENT_3D ( 'NONE', #73736, #75027, #72448 ) ;
#133556 = CARTESIAN_POINT ( 'NONE',  ( -20.64999999999999858, 1.925233644859816629, -12.73024353312613144 ) ) ;
#133557 = LINE ( 'NONE', #194847, #34579 ) ;
#133558 = ADVANCED_FACE ( 'NONE', ( #49117 ), #171678, .T. ) ;
#133559 = EDGE_CURVE ( 'NONE', #251678, #160550, #224552, .T. ) ;
#133560 = SHAPE_REPRESENTATION ( 'Moving End Attachment Flange', ( #2425 ), #197867 ) ;
#133561 = DIRECTION ( 'NONE',  ( 0.000000000000000000, -0.1575844902526687130, -0.9875055080513762684 ) ) ;
#133563 = EDGE_LOOP ( 'NONE', ( #246670, #245887, #109576, #233897, #93128, #23320 ) ) ;
#133562 = CARTESIAN_POINT ( 'NONE',  ( 20.04142135623730070, 11.65000000000000391, -21.35000000000000142 ) ) ;
#133564 = DIRECTION ( 'NONE',  ( 0.000000000000000000, 1.000000000000000000, 0.000000000000000000 ) ) ;
#133565 = CIRCLE ( 'NONE', #294, 0.2000000000000057288 ) ;
#133566 = CARTESIAN_POINT ( 'NONE',  ( 23.24999999999999289, 6.450000000011156587, -112.8500000000000369 ) ) ;
#133567 = DIRECTION ( 'NONE',  ( -0.000000000000000000, -0.4721928772777346239, -0.8814952561688430555 ) ) ;
#133569 = DIRECTION ( 'NONE',  ( 0.000000000000000000, -1.000000000000000000, -8.717686153663073805E-15 ) ) ;
#133568 = LINE ( 'NONE', #34496, #190053 ) ;
#133570 = DIRECTION ( 'NONE',  ( 0.000000000000000000, 0.9994937237965558774, 0.03181660087586650476 ) ) ;
#133571 = CYLINDRICAL_SURFACE ( 'NONE', #152913, 0.09999999999999939493 ) ;
#133572 = ADVANCED_FACE ( 'NONE', ( #68697 ), #7420, .T. ) ;
#133573 = DIRECTION ( 'NONE',  ( 0.000000000000000000, 0.5859227990963362664, 0.8103668758649469339 ) ) ;
#133574 = DIRECTION ( 'NONE',  ( 0.000000000000000000, 0.000000000000000000, -1.000000000000000000 ) ) ;
#133575 = EDGE_LOOP ( 'NONE', ( #175461, #104257, #63637 ) ) ;
#133577 = ORIENTED_EDGE ( 'NONE', *, *, #186956, .F. ) ;
#133576 = DIRECTION ( 'NONE',  ( -1.000000000000000000, -0.000000000000000000, -0.000000000000000000 ) ) ;
#133578 = CIRCLE ( 'NONE', #241900, 11.89999999999999325 ) ;
#133579 = CARTESIAN_POINT ( 'NONE',  ( 18.59999999999999432, 77.29973367124300410, -146.4949779616548824 ) ) ;
#133580 = DIRECTION ( 'NONE',  ( 0.000000000000000000, 6.982962677686266711E-15, -1.000000000000000000 ) ) ;
#133581 = VERTEX_POINT ( 'NONE', #12594 ) ;
#133582 = CIRCLE ( 'NONE', #154472, 0.1000000000000024342 ) ;
#133583 =( LENGTH_UNIT ( ) NAMED_UNIT ( * ) SI_UNIT ( .MILLI., .METRE. ) );
#133584 = DIRECTION ( 'NONE',  ( 1.000000000000000000, 0.000000000000000000, 0.000000000000000000 ) ) ;
#133585 = EDGE_CURVE ( 'NONE', #67142, #122573, #251157, .T. ) ;
#133586 = ORIENTED_EDGE ( 'NONE', *, *, #167176, .T. ) ;
#133587 = CARTESIAN_POINT ( 'NONE',  ( 21.05933563467872105, 60.07238536843232168, -221.2794350522829632 ) ) ;
#133588 = CARTESIAN_POINT ( 'NONE',  ( -23.25000000000000000, 73.40000000001151648, -49.24772940728643533 ) ) ;
#133589 = VECTOR ( 'NONE', #96739, 1000.000000000000000 ) ;
#133590 = EDGE_CURVE ( 'NONE', #255181, #99209, #196823, .T. ) ;
#133591 = CARTESIAN_POINT ( 'NONE',  ( -13.40000000000000213, -8.350000000000003197, 10.95857864376269042 ) ) ;
#133593 = VERTEX_POINT ( 'NONE', #226451 ) ;
#133592 = CARTESIAN_POINT ( 'NONE',  ( -20.15000000000000568, 9.291421356237307805, -21.25000000000000000 ) ) ;
#133594 = CARTESIAN_POINT ( 'NONE',  ( -21.08035267497491816, 75.91731137523616724, -142.8548143243073696 ) ) ;
#133596 = EDGE_LOOP ( 'NONE', ( #4282, #129580, #239954, #207939 ) ) ;
#133595 = CARTESIAN_POINT ( 'NONE',  ( -23.15000000000000213, 1.115600667400684642E-11, -165.5000000000000284 ) ) ;
#133598 = EDGE_CURVE ( 'NONE', #196513, #117921, #72559, .T. ) ;
#133597 = SPHERICAL_SURFACE ( 'NONE', #45970, 0.1000000000000000056 ) ;
#133599 = CARTESIAN_POINT ( 'NONE',  ( 18.79999999999999716, 11.49641995933507843, 1.885425182446133885 ) ) ;
#133600 = DIRECTION ( 'NONE',  ( 0.000000000000000000, -0.5773469543544729188, -0.8164989248600478255 ) ) ;
#133601 = CARTESIAN_POINT ( 'NONE',  ( -20.85000000000000142, -1.164121893230052995, -108.2148480855716457 ) ) ;
#133603 = DIRECTION ( 'NONE',  ( 1.000000000000000000, -3.265361837132813093E-16, -2.280189983783949500E-30 ) ) ;
#133602 = DIRECTION ( 'NONE',  ( 0.000000000000000000, 0.000000000000000000, -1.000000000000000000 ) ) ;
#133605 = EDGE_CURVE ( 'NONE', #240102, #231259, #117723, .T. ) ;
#133604 = CARTESIAN_POINT ( 'NONE',  ( 21.05000000000000071, 5.400000000011154988, -54.59473398108690390 ) ) ;
#133607 = CYLINDRICAL_SURFACE ( 'NONE', #24803, 0.09999999999999939493 ) ;
#133606 = CIRCLE ( 'NONE', #42062, 0.09999999999999939493 ) ;
#133608 = CARTESIAN_POINT ( 'NONE',  ( -18.31572283045109018, 85.54843783089823717, -163.1724818334656959 ) ) ;
#133609 = DIRECTION ( 'NONE',  ( -5.603264701231743991E-32, 1.897661533703520143E-16, -1.000000000000000000 ) ) ;
#133610 = DIRECTION ( 'NONE',  ( 1.000000000000000000, 0.000000000000000000, -0.000000000000000000 ) ) ;
#133611 = CONICAL_SURFACE ( 'NONE', #17119, 4.049999999999998046, 0.7853981633974604915 ) ;
#133612 = VERTEX_POINT ( 'NONE', #166539 ) ;
#133613 = ADVANCED_FACE ( 'NONE', ( #150794 ), #109087, .F. ) ;
#133615 = CARTESIAN_POINT ( 'NONE',  ( 23.15000000000000213, -11.74999999999999289, -21.35000000000000142 ) ) ;
#133614 = AXIS2_PLACEMENT_3D ( 'NONE', #245397, #247942, #146275 ) ;
#133617 = EDGE_CURVE ( 'NONE', #40138, #206496, #27028, .T. ) ;
#133616 = ADVANCED_FACE ( 'NONE', ( #210767 ), #191237, .T. ) ;
#133618 = EDGE_LOOP ( 'NONE', ( #230248, #141903, #64221, #77874 ) ) ;
#133619 = AXIS2_PLACEMENT_3D ( 'NONE', #1210, #138156, #97733 ) ;
#133620 = EDGE_LOOP ( 'NONE', ( #29056, #109660, #50763, #240582 ) ) ;
#133621 = DIRECTION ( 'NONE',  ( 1.000000000000000000, 0.000000000000000000, 0.000000000000000000 ) ) ;
#133622 = CARTESIAN_POINT ( 'NONE',  ( -16.87036670365548474, 9.989418819312801290, -121.4795601173020856 ) ) ;
#133623 = ORIENTED_EDGE ( 'NONE', *, *, #192373, .T. ) ;
#133624 = CIRCLE ( 'NONE', #208488, 0.2000000000000057288 ) ;
#133625 = VERTEX_POINT ( 'NONE', #106504 ) ;
#133626 = CARTESIAN_POINT ( 'NONE',  ( -18.59999999999999787, 6.846123162363745074, -137.7377262668498759 ) ) ;
#133628 = ORIENTED_EDGE ( 'NONE', *, *, #161271, .F. ) ;
#133627 = AXIS2_PLACEMENT_3D ( 'NONE', #54139, #252334, #51545 ) ;
#133629 = EDGE_CURVE ( 'NONE', #16708, #182252, #186076, .T. ) ;
#133631 = EDGE_CURVE ( 'NONE', #15770, #129072, #38608, .T. ) ;
#133630 = AXIS2_PLACEMENT_3D ( 'NONE', #43052, #65163, #245095 ) ;
#133632 = CIRCLE ( 'NONE', #12861, 0.5000000000000013323 ) ;
#133633 = EDGE_LOOP ( 'NONE', ( #256034, #107204 ) ) ;
#133634 = AXIS2_PLACEMENT_3D ( 'NONE', #195253, #118257, #159973 ) ;
#133635 = CIRCLE ( 'NONE', #21251, 0.9000000000000014655 ) ;
#133636 = DIRECTION ( 'NONE',  ( 1.000000000000000000, 0.000000000000000000, 0.000000000000000000 ) ) ;
#133637 = CARTESIAN_POINT ( 'NONE',  ( -16.77683809663752257, 66.05416425680742520, -56.85915846542017960 ) ) ;
#133638 = CARTESIAN_POINT ( 'NONE',  ( 21.05000000000000071, 86.48473784507378070, -209.3714211149925575 ) ) ;
#133639 = CARTESIAN_POINT ( 'NONE',  ( 21.05000000000000071, 1.115600667400684642E-11, -134.0000000000000000 ) ) ;
#133640 = CARTESIAN_POINT ( 'NONE',  ( 14.22821877134046886, 9.456028260507917338, -15.01119803506572659 ) ) ;
#133641 = ADVANCED_FACE ( 'NONE', ( #135057 ), #217654, .T. ) ;
#133643 = SURFACE_STYLE_FILL_AREA ( #121499 ) ;
#133642 = DIRECTION ( 'NONE',  ( 1.186688945009010077E-16, -1.000000000000000000, -0.000000000000000000 ) ) ;
#133644 = CARTESIAN_POINT ( 'NONE',  ( 18.59999999999999432, 10.49142135624846617, -58.25000000000000000 ) ) ;
#133646 = VERTEX_POINT ( 'NONE', #253729 ) ;
#133645 = LINE ( 'NONE', #232764, #217350 ) ;
#133648 = CARTESIAN_POINT ( 'NONE',  ( -21.30740335185485890, 65.41956451911318027, -242.1572894605589283 ) ) ;
#133647 = FACE_OUTER_BOUND ( 'NONE', #169762, .T. ) ;
#133649 = CARTESIAN_POINT ( 'NONE',  ( -20.64999999999999858, 2.500000000011156409, -180.7246219227620543 ) ) ;
#133650 = ORIENTED_EDGE ( 'NONE', *, *, #150360, .T. ) ;
#133651 = CARTESIAN_POINT ( 'NONE',  ( -18.50000000000000000, 46.62132166459547733, -243.0426574061995950 ) ) ;
#133652 = CARTESIAN_POINT ( 'NONE',  ( 21.05000000000000071, 0.000000000000000000, -33.50000000000000000 ) ) ;
#133653 = DIRECTION ( 'NONE',  ( 0.000000000000000000, -0.8660254037844384856, 0.5000000000000002220 ) ) ;
#133654 = ORIENTED_EDGE ( 'NONE', *, *, #184450, .T. ) ;
#133655 = EDGE_CURVE ( 'NONE', #101761, #83713, #30429, .T. ) ;
#133656 = AXIS2_PLACEMENT_3D ( 'NONE', #222703, #49215, #24548 ) ;
#133657 = LINE ( 'NONE', #37146, #166233 ) ;
#133658 = EDGE_CURVE ( 'NONE', #113044, #224195, #147118, .T. ) ;
#133659 = DIRECTION ( 'NONE',  ( 1.000000000000000000, -0.000000000000000000, 0.000000000000000000 ) ) ;
#133660 = CARTESIAN_POINT ( 'NONE',  ( 13.43443725621852636, 66.55344247693932402, -87.93316553017848491 ) ) ;
#133661 = ORIENTED_EDGE ( 'NONE', *, *, #118604, .T. ) ;
#133662 = ORIENTED_EDGE ( 'NONE', *, *, #198126, .F. ) ;
#133663 = DIRECTION ( 'NONE',  ( -1.000000000000000000, 0.000000000000000000, -0.000000000000000000 ) ) ;
#133664 = DIRECTION ( 'NONE',  ( -1.000000000000000000, 0.000000000000000000, 0.000000000000000000 ) ) ;
#133665 = DIRECTION ( 'NONE',  ( 0.000000000000000000, -0.9908441862701791170, 0.1350103645450472789 ) ) ;
#133667 = ADVANCED_FACE ( 'NONE', ( #75141 ), #130363, .F. ) ;
#133666 = CARTESIAN_POINT ( 'NONE',  ( 23.15000000000000213, -8.999999999988842703, -57.10603087734755690 ) ) ;
#133668 = ORIENTED_EDGE ( 'NONE', *, *, #222561, .F. ) ;
#133669 = CIRCLE ( 'NONE', #21276, 0.1000000000000028644 ) ;
#133670 = CARTESIAN_POINT ( 'NONE',  ( 15.52844286134407881, 47.30686838571505604, -234.5075185885025633 ) ) ;
#133671 = CARTESIAN_POINT ( 'NONE',  ( 20.99999999999999645, 66.25000000001264766, -194.2731074845244166 ) ) ;
#133673 = EDGE_CURVE ( 'NONE', #194433, #168461, #97004, .T. ) ;
#133672 = CARTESIAN_POINT ( 'NONE',  ( 18.59999999999999432, 77.16270174995034381, -161.9231074845243370 ) ) ;
#133674 = DIRECTION ( 'NONE',  ( 0.000000000000000000, 0.9651348961777157509, -0.2617529984165031243 ) ) ;
#133675 = AXIS2_PLACEMENT_3D ( 'NONE', #231363, #110108, #192239 ) ;
#133676 = CARTESIAN_POINT ( 'NONE',  ( -21.64999999999999858, 9.350000000011133849, -109.7500000000000426 ) ) ;
#133677 = CIRCLE ( 'NONE', #42122, 0.09999999999999939493 ) ;
#133679 = EDGE_LOOP ( 'NONE', ( #247162, #196061, #243658, #92252 ) ) ;
#133678 = CARTESIAN_POINT ( 'NONE',  ( 20.94999999999999929, 85.40000000001148805, -45.91707660717669626 ) ) ;
#133680 = CARTESIAN_POINT ( 'NONE',  ( -21.07928932188134041, 69.67148334361908724, -170.1220026301787982 ) ) ;
#133681 = CARTESIAN_POINT ( 'NONE',  ( 13.40000000000005898, 67.75000000001118394, -21.02310748452479316 ) ) ;
#133682 = CYLINDRICAL_SURFACE ( 'NONE', #179368, 11.80000000000000426 ) ;
#133683 = DIRECTION ( 'NONE',  ( 0.000000000000000000, 8.326672684688666480E-14, 1.000000000000000000 ) ) ;
#133684 = EDGE_CURVE ( 'NONE', #58899, #6554, #95939, .T. ) ;
#133685 = CARTESIAN_POINT ( 'NONE',  ( -23.25000000000000000, 69.06610602788505560, -32.23746165015079868 ) ) ;
#133687 = EDGE_LOOP ( 'NONE', ( #125042, #33832, #11853, #19867 ) ) ;
#133686 = DIRECTION ( 'NONE',  ( 0.000000000000000000, 0.4721928772777551075, 0.8814952561688320642 ) ) ;
#133688 = CARTESIAN_POINT ( 'NONE',  ( -20.64999999999999858, 71.65000000001207070, -124.1731074845243228 ) ) ;
#133689 = DIRECTION ( 'NONE',  ( 0.000000000000000000, 0.000000000000000000, 1.000000000000000000 ) ) ;
#133690 = CARTESIAN_POINT ( 'NONE',  ( 21.14999999999999503, -11.64999999998883595, -55.25000000000004974 ) ) ;
#133691 = VERTEX_POINT ( 'NONE', #213319 ) ;
#133692 = FACE_OUTER_BOUND ( 'NONE', #156668, .T. ) ;
#133693 = DIRECTION ( 'NONE',  ( 0.000000000000000000, -0.4721928772777346239, -0.8814952561688430555 ) ) ;
#133694 = CARTESIAN_POINT ( 'NONE',  ( 20.94999999999997442, 43.02787096365918984, -254.3959382439171577 ) ) ;
#133695 = DIRECTION ( 'NONE',  ( 1.000000000000000000, 0.000000000000000000, 0.000000000000000000 ) ) ;
#133697 = CIRCLE ( 'NONE', #137774, 0.09999999999999992228 ) ;
#133696 = DIRECTION ( 'NONE',  ( 0.000000000000000000, 0.000000000000000000, -1.000000000000000000 ) ) ;
#133699 = AXIS2_PLACEMENT_3D ( 'NONE', #123331, #64626, #183301 ) ;
#133698 = FACE_OUTER_BOUND ( 'NONE', #224289, .T. ) ;
#133700 = VERTEX_POINT ( 'NONE', #13859 ) ;
#133701 = ORIENTED_EDGE ( 'NONE', *, *, #27449, .T. ) ;
#133702 = AXIS2_PLACEMENT_3D ( 'NONE', #75491, #153770, #256604 ) ;
#133703 = CARTESIAN_POINT ( 'NONE',  ( -16.87331047859651179, 66.05000000001207638, -123.8731074845243683 ) ) ;
#133704 = DIRECTION ( 'NONE',  ( 1.000000000000000000, 0.000000000000000000, 0.000000000000000000 ) ) ;
#133705 = CARTESIAN_POINT ( 'NONE',  ( -20.64999999999999858, 76.00000000001190870, -103.0231074845243029 ) ) ;
#133706 = DIRECTION ( 'NONE',  ( 0.000000000000000000, 0.5273008465188072647, -0.8496786552930167824 ) ) ;
#133707 = CARTESIAN_POINT ( 'NONE',  ( -18.59999999999999787, 5.949999999999945111, -10.30570230503485796 ) ) ;
#133708 = LINE ( 'NONE', #75059, #34200 ) ;
#133709 = CIRCLE ( 'NONE', #167077, 0.1999999999999987899 ) ;
#133710 = DIRECTION ( 'NONE',  ( 1.000000000000000000, 0.000000000000000000, 0.000000000000000000 ) ) ;
#133711 = DIRECTION ( 'NONE',  ( -1.000000000000000000, 0.000000000000000000, -0.000000000000000000 ) ) ;
#133712 = ORIENTED_EDGE ( 'NONE', *, *, #115090, .T. ) ;
#133713 = CARTESIAN_POINT ( 'NONE',  ( 18.49999999999999645, 74.26374286841490857, -158.4544551555068779 ) ) ;
#133714 = ORIENTED_EDGE ( 'NONE', *, *, #36519, .F. ) ;
#133715 = CYLINDRICAL_SURFACE ( 'NONE', #38224, 0.09999999999999939493 ) ;
#133716 = CARTESIAN_POINT ( 'NONE',  ( -21.65000000000000213, 68.75000000001232081, -157.3731074845244109 ) ) ;
#133717 = DIRECTION ( 'NONE',  ( 0.000000000000000000, 0.9963347912923393723, -0.08553936906741056723 ) ) ;
#133719 = VERTEX_POINT ( 'NONE', #252445 ) ;
#133718 = DIRECTION ( 'NONE',  ( 0.000000000000000000, 0.000000000000000000, 1.000000000000000000 ) ) ;
#133720 = CARTESIAN_POINT ( 'NONE',  ( -22.49231231312463208, 11.64998490367728223, 0.06105288760136910742 ) ) ;
#133721 = SPHERICAL_SURFACE ( 'NONE', #81189, 0.1000000000000000056 ) ;
#133722 = CARTESIAN_POINT ( 'NONE',  ( 18.41815437325352178, 85.49870985315310179, -62.91916164572214143 ) ) ;
#133723 = ORIENTED_EDGE ( 'NONE', *, *, #116945, .T. ) ;
#133724 = FACE_OUTER_BOUND ( 'NONE', #126580, .T. ) ;
#133725 = AXIS2_PLACEMENT_3D ( 'NONE', #41109, #116762, #80170 ) ;
#133726 = DIRECTION ( 'NONE',  ( 0.000000000000000000, 1.000000000000000000, 6.982962677686266711E-15 ) ) ;
#133728 = EDGE_CURVE ( 'NONE', #237228, #2978, #47145, .T. ) ;
#133727 = AXIS2_PLACEMENT_3D ( 'NONE', #201733, #217426, #77928 ) ;
#133729 = CARTESIAN_POINT ( 'NONE',  ( 22.50000000000000000, 75.90000000001245439, -181.6726782920691505 ) ) ;
#133730 = CARTESIAN_POINT ( 'NONE',  ( 18.39999999999999858, 73.22794484573502416, -249.6559397216816478 ) ) ;
#133731 = AXIS2_PLACEMENT_3D ( 'NONE', #173179, #66655, #5358 ) ;
#133732 = FACE_OUTER_BOUND ( 'NONE', #174675, .T. ) ;
#133733 = AXIS2_PLACEMENT_3D ( 'NONE', #51247, #211656, #94248 ) ;
#133734 = ORIENTED_EDGE ( 'NONE', *, *, #200081, .T. ) ;
#133735 = CARTESIAN_POINT ( 'NONE',  ( -22.60000000000080789, 75.95218301954683682, -148.2731299156770319 ) ) ;
#133736 = CARTESIAN_POINT ( 'NONE',  ( -20.64999999999999858, 1.999999999999998224, -13.22462192276210224 ) ) ;
#133737 = EDGE_LOOP ( 'NONE', ( #5260, #180735, #254248, #168204 ) ) ;
#133738 = CARTESIAN_POINT ( 'NONE',  ( -23.15000000000000213, 87.75000000001165290, -69.52310748452424605 ) ) ;
#133739 = CARTESIAN_POINT ( 'NONE',  ( 23.14999999999998437, 11.75000000001115552, -67.00000000000004263 ) ) ;
#133740 = CARTESIAN_POINT ( 'NONE',  ( 22.39999999999999858, 68.20922040163827660, -69.62310748452438247 ) ) ;
#133742 = ADVANCED_FACE ( 'NONE', ( #158522 ), #126272, .T. ) ;
#133741 = AXIS2_PLACEMENT_3D ( 'NONE', #143312, #162913, #62508 ) ;
#133743 = ADVANCED_FACE ( 'NONE', ( #136331 ), #196996, .T. ) ;
#133744 = ORIENTED_EDGE ( 'NONE', *, *, #163797, .T. ) ;
#133745 = CARTESIAN_POINT ( 'NONE',  ( 18.50000000000000355, -9.421074344976293702, -174.3244720594309456 ) ) ;
#133746 = CARTESIAN_POINT ( 'NONE',  ( 21.05000000000000071, 61.16604239671103471, -234.3115055913011417 ) ) ;
#133747 = ORIENTED_EDGE ( 'NONE', *, *, #219455, .F. ) ;
#133748 = ADVANCED_FACE ( 'NONE', ( #172969 ), #84537, .F. ) ;
#133749 = ORIENTED_EDGE ( 'NONE', *, *, #87254, .F. ) ;
#133750 = EDGE_CURVE ( 'NONE', #231870, #186109, #17931, .T. ) ;
#133751 = DIRECTION ( 'NONE',  ( -0.000000000000000000, -0.9126074666063770380, -0.4088369013363281068 ) ) ;
#133752 = CARTESIAN_POINT ( 'NONE',  ( 21.05000000000000071, 1.115600667400684642E-11, -202.8999999999999773 ) ) ;
#133753 = AXIS2_PLACEMENT_3D ( 'NONE', #179920, #1240, #44251 ) ;
#133755 = VERTEX_POINT ( 'NONE', #212069 ) ;
#133754 = CARTESIAN_POINT ( 'NONE',  ( -18.50000000000000000, 5.341242989991647150, 9.806650206488024324 ) ) ;
#133756 = CARTESIAN_POINT ( 'NONE',  ( -23.25000000000000000, 45.99141771592758943, -256.5205054824189119 ) ) ;
#133758 = CARTESIAN_POINT ( 'NONE',  ( -20.94999999999999929, 11.70000000001115126, -160.7450018504814011 ) ) ;
#133757 = UNCERTAINTY_MEASURE_WITH_UNIT (LENGTH_MEASURE( 1.000000000000000082E-05 ), #103423, 'distance_accuracy_value', 'NONE');
#133759 = ADVANCED_FACE ( 'NONE', ( #116804 ), #33460, .F. ) ;
#133760 = CARTESIAN_POINT ( 'NONE',  ( -20.85000000000000142, 65.66751761918692409, -130.9282609406112670 ) ) ;
#133761 = DIRECTION ( 'NONE',  ( 0.000000000000000000, 0.9333616406058473647, 0.3589373870824282275 ) ) ;
#133762 = DIRECTION ( 'NONE',  ( -4.391705002472929091E-16, 1.000000000000000000, 0.000000000000000000 ) ) ;
#133763 = VECTOR ( 'NONE', #39747, 1000.000000000000000 ) ;
#133764 = CYLINDRICAL_SURFACE ( 'NONE', #197088, 0.09999999999999939493 ) ;
#133765 = CARTESIAN_POINT ( 'NONE',  ( -16.77732147278574715, 66.05403306743885139, -157.3595987276486312 ) ) ;
#133767 = VERTEX_POINT ( 'NONE', #236733 ) ;
#133766 = FACE_OUTER_BOUND ( 'NONE', #136112, .T. ) ;
#133768 = ORIENTED_EDGE ( 'NONE', *, *, #164212, .T. ) ;
#133770 = CARTESIAN_POINT ( 'NONE',  ( -16.85722902420148372, 51.51341344488079699, -231.9937090867831273 ) ) ;
#133769 = DIRECTION ( 'NONE',  ( 2.940209281316622495E-16, -1.000000000000000000, -5.880418562633244990E-15 ) ) ;
#133771 = EDGE_CURVE ( 'NONE', #206711, #12050, #138698, .T. ) ;
#133773 = EDGE_LOOP ( 'NONE', ( #230817, #156815, #36098, #113353 ) ) ;
#133772 = CYLINDRICAL_SURFACE ( 'NONE', #255677, 0.09999999999999939493 ) ;
#133774 = VECTOR ( 'NONE', #32167, 1000.000000000000227 ) ;
#133775 = VERTEX_POINT ( 'NONE', #34726 ) ;
#133776 = CARTESIAN_POINT ( 'NONE',  ( 23.14999999999999503, 11.75000000001116263, -193.9851942293460070 ) ) ;
#133777 = CYLINDRICAL_SURFACE ( 'NONE', #155504, 0.09999999999999939493 ) ;
#133778 = AXIS2_PLACEMENT_3D ( 'NONE', #160931, #104755, #99623 ) ;
#133779 = EDGE_CURVE ( 'NONE', #24049, #237661, #55314, .T. ) ;
#133780 = CARTESIAN_POINT ( 'NONE',  ( 23.24999999999999645, 76.00000000001267608, -203.5231074845243597 ) ) ;
#133781 = AXIS2_PLACEMENT_3D ( 'NONE', #19516, #199448, #155196 ) ;
#133782 = CARTESIAN_POINT ( 'NONE',  ( 23.24999999999997513, 62.92003201576280702, -207.2439188921395612 ) ) ;
#133783 = CARTESIAN_POINT ( 'NONE',  ( 21.05000000000000071, 6.093673009692411213, -199.5727803633481301 ) ) ;
#133784 = CIRCLE ( 'NONE', #50572, 0.5000000000000004441 ) ;
#133785 = EDGE_CURVE ( 'NONE', #161742, #173882, #184522, .T. ) ;
#133786 = DIRECTION ( 'NONE',  ( -0.000000000000000000, 0.1350103645451876666, 0.9908441862701600211 ) ) ;
#133787 = EDGE_LOOP ( 'NONE', ( #48371, #33849, #237358, #76684 ) ) ;
#133788 = VERTEX_POINT ( 'NONE', #99776 ) ;
#133789 = DIRECTION ( 'NONE',  ( -0.7071067811865474617, -0.6909108974501236844, -0.1504730267678055788 ) ) ;
#133790 = CIRCLE ( 'NONE', #46478, 0.09999999999999799327 ) ;
#133791 = ORIENTED_EDGE ( 'NONE', *, *, #147130, .T. ) ;
#133792 = DIRECTION ( 'NONE',  ( 0.000000000000000000, 0.2617529984164856383, 0.9651348961777204138 ) ) ;
#133794 = ORIENTED_EDGE ( 'NONE', *, *, #150042, .F. ) ;
#133793 = VECTOR ( 'NONE', #120036, 1000.000000000000000 ) ;
#133795 = CARTESIAN_POINT ( 'NONE',  ( -23.25000000000000000, 64.35000000001195986, -110.0379132551783385 ) ) ;
#133796 = CIRCLE ( 'NONE', #8916, 0.1000000000000029060 ) ;
#133797 = DIRECTION ( 'NONE',  ( -0.5932847527679298016, -0.8049926720990051576, -5.621233785078291429E-15 ) ) ;
#133798 = FACE_OUTER_BOUND ( 'NONE', #5828, .T. ) ;
#133799 = ORIENTED_EDGE ( 'NONE', *, *, #71201, .T. ) ;
#133800 = CARTESIAN_POINT ( 'NONE',  ( 18.59999999999997655, 1.115600667400684642E-11, -67.00000000000000000 ) ) ;
#133801 = ORIENTED_EDGE ( 'NONE', *, *, #221241, .F. ) ;
#133802 = DIRECTION ( 'NONE',  ( 0.000000000000000000, 0.2128009952263603677, -0.9770955615653315052 ) ) ;
#133803 = FACE_OUTER_BOUND ( 'NONE', #159738, .T. ) ;
#133804 = VERTEX_POINT ( 'NONE', #26386 ) ;
#133805 = LINE ( 'NONE', #114251, #106713 ) ;
#133806 = ORIENTED_EDGE ( 'NONE', *, *, #25632, .F. ) ;
#133809 = ORIENTED_EDGE ( 'NONE', *, *, #215991, .F. ) ;
#133808 = DIRECTION ( 'NONE',  ( 1.000000000000000000, 0.000000000000000000, 0.000000000000000000 ) ) ;
#133807 = CARTESIAN_POINT ( 'NONE',  ( -18.50000000000000000, 22.19492904189240079, -246.0046379724989549 ) ) ;
#133810 = VECTOR ( 'NONE', #205199, 1000.000000000000000 ) ;
#133811 = CARTESIAN_POINT ( 'NONE',  ( 23.40000000000005187, 84.00000000001119815, -34.86056257560453986 ) ) ;
#133812 = CIRCLE ( 'NONE', #13054, 0.1000000000000028644 ) ;
#133814 = EDGE_LOOP ( 'NONE', ( #163274, #231514, #16847 ) ) ;
#133813 = AXIS2_PLACEMENT_3D ( 'NONE', #209351, #9870, #184651 ) ;
#133815 = AXIS2_PLACEMENT_3D ( 'NONE', #248863, #148480, #28582 ) ;
#133816 = EDGE_CURVE ( 'NONE', #226125, #208704, #101272, .T. ) ;
#133817 = ORIENTED_EDGE ( 'NONE', *, *, #123759, .F. ) ;
#133818 = EDGE_CURVE ( 'NONE', #160208, #40304, #88896, .T. ) ;
#133819 = CARTESIAN_POINT ( 'NONE',  ( 21.53699400384692808, 3.391009845873812292E-12, 6.787711793240010394 ) ) ;
#133820 = VERTEX_POINT ( 'NONE', #240602 ) ;
#133821 = SPHERICAL_SURFACE ( 'NONE', #43430, 0.1000000000000000056 ) ;
#133822 = ADVANCED_FACE ( 'NONE', ( #28988 ), #155356, .F. ) ;
#133823 = CARTESIAN_POINT ( 'NONE',  ( 22.41477678272288188, 64.18116553293013737, -247.0983321412288660 ) ) ;
#133824 = EDGE_CURVE ( 'NONE', #22410, #17786, #209474, .T. ) ;
#133825 = FACE_OUTER_BOUND ( 'NONE', #108651, .T. ) ;
#133826 = DIRECTION ( 'NONE',  ( -1.000000000000000000, -0.000000000000000000, 0.000000000000000000 ) ) ;
#133827 = CARTESIAN_POINT ( 'NONE',  ( -16.91256925476571382, 66.01426884188389010, -123.9907499735296454 ) ) ;
#133829 = ORIENTED_EDGE ( 'NONE', *, *, #194513, .T. ) ;
#133828 = ADVANCED_FACE ( 'NONE', ( #60659 ), #230315, .T. ) ;
#133830 = CYLINDRICAL_SURFACE ( 'NONE', #185833, 0.09999999999999933942 ) ;
#133831 = CARTESIAN_POINT ( 'NONE',  ( -20.85000000000000142, 64.25000000001195133, -109.8069731475024753 ) ) ;
#133832 = CARTESIAN_POINT ( 'NONE',  ( -20.99780126800952829, 11.60538868788763089, -160.5873525717050541 ) ) ;
#133833 = EDGE_CURVE ( 'NONE', #13316, #32896, #47196, .T. ) ;
#133834 = ORIENTED_EDGE ( 'NONE', *, *, #211451, .F. ) ;
#133835 = CARTESIAN_POINT ( 'NONE',  ( -20.54999999999999716, 76.00000000001126921, -203.5231074845248997 ) ) ;
#133837 = EDGE_CURVE ( 'NONE', #17786, #183689, #81490, .T. ) ;
#133836 = ORIENTED_EDGE ( 'NONE', *, *, #199872, .T. ) ;
#133838 = DIRECTION ( 'NONE',  ( 0.000000000000000000, -1.000000000000000000, 0.000000000000000000 ) ) ;
#133839 = ORIENTED_EDGE ( 'NONE', *, *, #206039, .F. ) ;
#133840 = FACE_OUTER_BOUND ( 'NONE', #19316, .T. ) ;
#133841 = FACE_OUTER_BOUND ( 'NONE', #179008, .T. ) ;
#133842 = ADVANCED_FACE ( 'NONE', ( #206299 ), #120681, .F. ) ;
#133844 = ORIENTED_EDGE ( 'NONE', *, *, #199747, .F. ) ;
#133843 = DIRECTION ( 'NONE',  ( 1.000000000000000000, 0.000000000000000000, 0.000000000000000000 ) ) ;
#133845 = DIRECTION ( 'NONE',  ( -0.000000000000000000, 0.9875055080513808203, -0.1575844902526395142 ) ) ;
#133846 = ORIENTED_EDGE ( 'NONE', *, *, #246388, .T. ) ;
#133847 = AXIS2_PLACEMENT_3D ( 'NONE', #232972, #133845, #213372 ) ;
#133848 = CARTESIAN_POINT ( 'NONE',  ( 20.95000000000005258, 65.15000000001120384, -3.023107484524792277 ) ) ;
#133849 = EDGE_CURVE ( 'NONE', #251542, #140576, #213567, .T. ) ;
#133850 = DIRECTION ( 'NONE',  ( 0.000000000000000000, 0.000000000000000000, -1.000000000000000000 ) ) ;
#133851 = EDGE_LOOP ( 'NONE', ( #57551, #31695, #162668, #173446 ) ) ;
#133852 = CARTESIAN_POINT ( 'NONE',  ( -22.47071067811865319, 0.09909245471376178227, -126.2799252555019649 ) ) ;
#133853 = FACE_OUTER_BOUND ( 'NONE', #120863, .T. ) ;
#133855 = EDGE_LOOP ( 'NONE', ( #210102, #184237 ) ) ;
#133854 = ADVANCED_FACE ( 'NONE', ( #227129 ), #80204, .T. ) ;
#133856 = CARTESIAN_POINT ( 'NONE',  ( -16.94037747912386038, 10.01353938249748410, -146.5511309579755164 ) ) ;
#133857 = ORIENTED_EDGE ( 'NONE', *, *, #231304, .F. ) ;
#133858 = ADVANCED_FACE ( 'NONE', ( #68067 ), #217835, .F. ) ;
#133860 = CARTESIAN_POINT ( 'NONE',  ( 23.24999999999999289, -4.149999999988843058, -33.50000000000000000 ) ) ;
#133859 = AXIS2_PLACEMENT_3D ( 'NONE', #48653, #47356, #23984 ) ;
#133861 = DIRECTION ( 'NONE',  ( -1.000000000000000000, 2.171475777237622503E-16, -9.970532993647777410E-16 ) ) ;
#133862 = EDGE_CURVE ( 'NONE', #101718, #41950, #226190, .T. ) ;
#133863 = ADVANCED_FACE ( 'NONE', ( #21567 ), #101090, .T. ) ;
#133865 = ORIENTED_EDGE ( 'NONE', *, *, #186595, .F. ) ;
#133864 = CARTESIAN_POINT ( 'NONE',  ( -21.14999999999999858, -0.09999999998884338825, -88.85042919245522341 ) ) ;
#133866 = CARTESIAN_POINT ( 'NONE',  ( 20.94999999999999929, 1.115600667400684642E-11, -204.9999999999999716 ) ) ;
#133867 = DIRECTION ( 'NONE',  ( 0.000000000000000000, 0.000000000000000000, -1.000000000000000000 ) ) ;
#133868 = CARTESIAN_POINT ( 'NONE',  ( -21.05000000000000071, 34.01125473725046078, -243.8802146427659352 ) ) ;
#133870 = CARTESIAN_POINT ( 'NONE',  ( -22.47886152344871036, 75.96249906115076556, -181.6730961275722507 ) ) ;
#133869 = CARTESIAN_POINT ( 'NONE',  ( 20.94999999999999574, 42.96458825698139350, -239.5490660745215337 ) ) ;
#133871 = CARTESIAN_POINT ( 'NONE',  ( 20.85000000000000142, -1.749999999999999778, -45.11895003862225195 ) ) ;
#133872 = DIRECTION ( 'NONE',  ( 0.000000000000000000, 0.4999999999999088507, -0.8660254037844913322 ) ) ;
#133873 = VECTOR ( 'NONE', #118254, 1000.000000000000000 ) ;
#133874 = CARTESIAN_POINT ( 'NONE',  ( -22.57320508075687115, 11.75000000000000000, 0.000000000000000000 ) ) ;
#133875 = VECTOR ( 'NONE', #68186, 1000.000000000000000 ) ;
#133876 = DIRECTION ( 'NONE',  ( 1.000000000000000000, 0.000000000000000000, 0.000000000000000000 ) ) ;
#133878 = ORIENTED_EDGE ( 'NONE', *, *, #32695, .T. ) ;
#133877 = AXIS2_PLACEMENT_3D ( 'NONE', #123791, #200755, #65093 ) ;
#133879 = EDGE_LOOP ( 'NONE', ( #216951, #120338, #100534, #82290 ) ) ;
#133880 = LINE ( 'NONE', #231718, #20931 ) ;
#133882 = VERTEX_POINT ( 'NONE', #161078 ) ;
#133881 = LINE ( 'NONE', #191328, #233504 ) ;
#133883 = ORIENTED_EDGE ( 'NONE', *, *, #137221, .F. ) ;
#133884 = DIRECTION ( 'NONE',  ( -3.265361837132813093E-16, 1.000000000000000000, 0.000000000000000000 ) ) ;
#133885 =( BOUNDED_CURVE ( )  B_SPLINE_CURVE ( 3, ( #138237, #195695, #178707, #212673 ),
 .UNSPECIFIED., .F., .F. ) 
 B_SPLINE_CURVE_WITH_KNOTS ( ( 4, 4 ),
 ( 1.570796326794896558, 3.141592653589793116 ),
 .UNSPECIFIED. ) 
 CURVE ( )  GEOMETRIC_REPRESENTATION_ITEM ( )  RATIONAL_B_SPLINE_CURVE ( ( 1.000000000000000000, 0.8047378541243649375, 0.8047378541243649375, 1.000000000000000000 ) ) 
 REPRESENTATION_ITEM ( '' )  );
#133886 = ORIENTED_EDGE ( 'NONE', *, *, #24101, .T. ) ;
#133887 = FACE_OUTER_BOUND ( 'NONE', #193609, .T. ) ;
#133888 = ORIENTED_EDGE ( 'NONE', *, *, #185484, .F. ) ;
#133889 = CIRCLE ( 'NONE', #108948, 0.5999999999999987566 ) ;
#133890 = DIRECTION ( 'NONE',  ( 0.000000000000000000, -0.9908441862701596881, -0.1350103645451901924 ) ) ;
#133892 = ORIENTED_EDGE ( 'NONE', *, *, #223183, .F. ) ;
#133891 = EDGE_LOOP ( 'NONE', ( #39291, #124251, #36676, #184642 ) ) ;
#133893 = ORIENTED_EDGE ( 'NONE', *, *, #164203, .F. ) ;
#133894 = EDGE_LOOP ( 'NONE', ( #61034, #13500, #193601 ) ) ;
#133895 = ORIENTED_EDGE ( 'NONE', *, *, #176869, .T. ) ;
#133896 = DIRECTION ( 'NONE',  ( 0.000000000000000000, 0.000000000000000000, -1.000000000000000000 ) ) ;
#133897 = CARTESIAN_POINT ( 'NONE',  ( 21.14261333020286315, 43.45739530927919247, -234.7636895383062949 ) ) ;
#133898 = ORIENTED_EDGE ( 'NONE', *, *, #51948, .F. ) ;
#133899 = DIRECTION ( 'NONE',  ( -0.000000000000000000, 0.1686199900910312910, -0.9856811345164826488 ) ) ;
#133901 = VERTEX_POINT ( 'NONE', #207596 ) ;
#133900 = CARTESIAN_POINT ( 'NONE',  ( 20.95265033839679347, 10.51225083247831371, -141.5657637560299804 ) ) ;
#133902 = DIRECTION ( 'NONE',  ( 0.000000000000000000, 0.000000000000000000, -1.000000000000000000 ) ) ;
#133903 = ORIENTED_EDGE ( 'NONE', *, *, #211216, .T. ) ;
#133904 = LINE ( 'NONE', #233040, #103620 ) ;
#133906 = EDGE_LOOP ( 'NONE', ( #219490, #75571, #16441, #242663 ) ) ;
#133905 = CARTESIAN_POINT ( 'NONE',  ( 21.07964655665547582, 8.774889614989714204, -112.7219165829640843 ) ) ;
#133907 = DIRECTION ( 'NONE',  ( 0.000000000000000000, -0.4088369013363276072, 0.9126074666063772600 ) ) ;
#133909 = EDGE_CURVE ( 'NONE', #37861, #144467, #134447, .T. ) ;
#133908 = DIRECTION ( 'NONE',  ( 0.000000000000000000, -0.5000000000000004441, -0.8660254037844384856 ) ) ;
#133910 = CIRCLE ( 'NONE', #21513, 0.09999999999999939493 ) ;
#133911 = AXIS2_PLACEMENT_3D ( 'NONE', #11182, #209372, #52857 ) ;
#133912 = ORIENTED_EDGE ( 'NONE', *, *, #93140, .F. ) ;
#133914 = DIRECTION ( 'NONE',  ( 0.000000000000000000, 0.000000000000000000, -1.000000000000000000 ) ) ;
#133913 = CARTESIAN_POINT ( 'NONE',  ( -16.91049119928362643, 9.950000000011135270, -121.3817203931908750 ) ) ;
#133915 = EDGE_CURVE ( 'NONE', #218291, #152832, #109514, .T. ) ;
#133916 = LINE ( 'NONE', #128802, #89084 ) ;
#133917 = DIRECTION ( 'NONE',  ( 0.000000000000000000, 0.8127272543710951647, -0.5826443254700255370 ) ) ;
#133918 = DIRECTION ( 'NONE',  ( -0.000000000000000000, 0.8814952561688430555, -0.4721928772777346239 ) ) ;
#133919 = ORIENTED_EDGE ( 'NONE', *, *, #82329, .F. ) ;
#133920 = ORIENTED_EDGE ( 'NONE', *, *, #246893, .T. ) ;
#133921 = ADVANCED_FACE ( 'NONE', ( #129324 ), #38004, .F. ) ;
#133922 = CARTESIAN_POINT ( 'NONE',  ( 21.05000000000000071, -8.999999999988844479, -43.39396912265245021 ) ) ;
#133924 = EDGE_CURVE ( 'NONE', #151423, #145620, #25126, .T. ) ;
#133923 = CARTESIAN_POINT ( 'NONE',  ( -20.94999999999999929, 42.15997144203495139, -239.2817429668763793 ) ) ;
#133925 = ORIENTED_EDGE ( 'NONE', *, *, #108673, .T. ) ;
#133926 = LINE ( 'NONE', #10140, #93341 ) ;
#133927 = ORIENTED_EDGE ( 'NONE', *, *, #32695, .F. ) ;
#133928 = FACE_OUTER_BOUND ( 'NONE', #90163, .T. ) ;
#133929 = FACE_OUTER_BOUND ( 'NONE', #85423, .T. ) ;
#133930 = TOROIDAL_SURFACE ( 'NONE', #125557, 12.97499999999999609, 0.1000000000000000056 ) ;
#133931 = VERTEX_POINT ( 'NONE', #92753 ) ;
#133932 = FACE_OUTER_BOUND ( 'NONE', #84266, .T. ) ;
#133933 = ORIENTED_EDGE ( 'NONE', *, *, #217995, .F. ) ;
#133934 = ORIENTED_EDGE ( 'NONE', *, *, #214175, .T. ) ;
#133935 = EDGE_CURVE ( 'NONE', #117760, #116862, #231020, .T. ) ;
#133936 = ORIENTED_EDGE ( 'NONE', *, *, #93102, .F. ) ;
#133937 = LINE ( 'NONE', #176958, #50446 ) ;
#133938 = CARTESIAN_POINT ( 'NONE',  ( 14.56326696814972088, 66.55335100938272319, -54.43394418860123096 ) ) ;
#133939 = LINE ( 'NONE', #34885, #138240 ) ;
#133940 = CARTESIAN_POINT ( 'NONE',  ( 23.15000000000000213, -11.64999999998883595, -155.7499999999999716 ) ) ;
#133941 = CARTESIAN_POINT ( 'NONE',  ( 12.60873083341396672, 66.61042836546560864, -118.7054667721552477 ) ) ;
#133942 = AXIS2_PLACEMENT_3D ( 'NONE', #182016, #109793, #32881 ) ;
#133944 = LINE ( 'NONE', #213485, #111647 ) ;
#133943 = CARTESIAN_POINT ( 'NONE',  ( 22.49066049874202022, -3.113992299531016528, -228.1819822047424680 ) ) ;
#133946 = EDGE_LOOP ( 'NONE', ( #29604, #9107, #46278, #44469 ) ) ;
#133945 = DIRECTION ( 'NONE',  ( 0.000000000000000000, 0.2617529984165152257, 0.9651348961777124202 ) ) ;
#133947 = FACE_OUTER_BOUND ( 'NONE', #40620, .T. ) ;
#133948 = ORIENTED_EDGE ( 'NONE', *, *, #53352, .F. ) ;
#133949 = CARTESIAN_POINT ( 'NONE',  ( -14.45443560709635911, 9.450592112144859058, -149.0561883188084096 ) ) ;
#133950 = ORIENTED_EDGE ( 'NONE', *, *, #10553, .F. ) ;
#133951 = ORIENTED_EDGE ( 'NONE', *, *, #98361, .T. ) ;
#133952 = CARTESIAN_POINT ( 'NONE',  ( -16.93440969289731157, 9.995185175825110235, -46.09123418501079783 ) ) ;
#133953 = CARTESIAN_POINT ( 'NONE',  ( 20.94999999999999574, -1.261786168553869603, -175.5864989635454378 ) ) ;
#133954 = EDGE_CURVE ( 'NONE', #176884, #159030, #105396, .T. ) ;
#133955 = CARTESIAN_POINT ( 'NONE',  ( 20.85000000000000142, -1.135018845899022466, -74.71697688343232358 ) ) ;
#133956 = AXIS2_PLACEMENT_3D ( 'NONE', #164925, #183212, #145350 ) ;
#133957 = ADVANCED_FACE ( 'NONE', ( #251835 ), #73242, .F. ) ;
#133958 = CYLINDRICAL_SURFACE ( 'NONE', #196542, 0.4999999999999944489 ) ;
#133959 = CIRCLE ( 'NONE', #46460, 0.1000000000000133560 ) ;
#133960 = ORIENTED_EDGE ( 'NONE', *, *, #148291, .F. ) ;
#133961 = ORIENTED_EDGE ( 'NONE', *, *, #62543, .F. ) ;
#133962 = AXIS2_PLACEMENT_3D ( 'NONE', #137838, #98687, #136553 ) ;
#133963 = CARTESIAN_POINT ( 'NONE',  ( -21.00857864376268935, 38.23914636435921466, -236.1324109481172684 ) ) ;
#133964 = ORIENTED_EDGE ( 'NONE', *, *, #39456, .F. ) ;
#133965 = DIRECTION ( 'NONE',  ( 1.000000000000000000, -0.000000000000000000, 0.000000000000000000 ) ) ;
#133966 = LINE ( 'NONE', #15338, #32174 ) ;
#133967 = ORIENTED_EDGE ( 'NONE', *, *, #188411, .F. ) ;
#133968 = CARTESIAN_POINT ( 'NONE',  ( -20.94999999999999929, 14.05000000001115623, -39.01369507076099552 ) ) ;
#133969 = DIRECTION ( 'NONE',  ( 0.000000000000000000, 0.000000000000000000, 1.000000000000000000 ) ) ;
#133970 = LINE ( 'NONE', #11482, #61287 ) ;
#133972 = EDGE_CURVE ( 'NONE', #75721, #20774, #80439, .T. ) ;
#133971 = CARTESIAN_POINT ( 'NONE',  ( 20.94999999999999929, 64.35000000001195986, -109.8647081744214233 ) ) ;
#133973 = ORIENTED_EDGE ( 'NONE', *, *, #81450, .F. ) ;
#133974 = AXIS2_PLACEMENT_3D ( 'NONE', #115309, #74937, #192297 ) ;
#133975 = ADVANCED_FACE ( 'NONE', ( #148902 ), #228444, .T. ) ;
#133977 = CIRCLE ( 'NONE', #96544, 0.1000000000000028644 ) ;
#133976 = DIRECTION ( 'NONE',  ( 1.000000000000000000, 0.000000000000000000, 0.000000000000000000 ) ) ;
#133978 = DIRECTION ( 'NONE',  ( 0.000000000000000000, 0.000000000000000000, 1.000000000000000000 ) ) ;
#133980 = ADVANCED_FACE ( 'NONE', ( #49783 ), #74536, .F. ) ;
#133979 = AXIS2_PLACEMENT_3D ( 'NONE', #38860, #120977, #200489 ) ;
#133981 = DIRECTION ( 'NONE',  ( -0.000000000000000000, -1.265107689135680095E-16, 1.000000000000000000 ) ) ;
#133982 = AXIS2_PLACEMENT_3D ( 'NONE', #169127, #33472, #247332 ) ;
#133983 = EDGE_LOOP ( 'NONE', ( #144757, #62393, #119091, #7868 ) ) ;
#133984 =( BOUNDED_SURFACE ( )  B_SPLINE_SURFACE ( 3, 2, ( 
 ( #56470, #19952, #4209 ),
 ( #105863, #45916, #104576 ),
 ( #40814, #242826, #245415 ),
 ( #181596, #85012, #142444 ) ),
 .UNSPECIFIED., .F., .F., .T. ) 
 B_SPLINE_SURFACE_WITH_KNOTS ( ( 4, 4 ),
 ( 3, 3 ),
 ( 0.0008258556059633580639, 0.0009616864997632887033 ),
 ( 0.000000000000000000, 1.000000000000000000 ),
 .UNSPECIFIED. ) 
 GEOMETRIC_REPRESENTATION_ITEM ( )  RATIONAL_B_SPLINE_SURFACE ( (
 ( 1.000000000000000000, 0.9152888060719308605, 1.000000000000000000),
 ( 1.000000000000000000, 0.9327727094137928665, 1.000000000000000000),
 ( 1.000000000000000000, 0.9369023509258854743, 1.000000000000000000),
 ( 1.000000000000000000, 0.9246339933864360372, 1.000000000000000000) ) ) 
 REPRESENTATION_ITEM ( '' )  SURFACE ( )  );
#133985 = DIRECTION ( 'NONE',  ( 0.000000000000000000, -0.1568667991644355497, -0.9876197685951332295 ) ) ;
#133986 = ORIENTED_EDGE ( 'NONE', *, *, #250416, .T. ) ;
#133987 = PLANE ( 'NONE',  #18278 ) ;
#133988 = EDGE_CURVE ( 'NONE', #229099, #255159, #63737, .T. ) ;
#133989 = AXIS2_PLACEMENT_3D ( 'NONE', #16762, #194120, #235779 ) ;
#133990 = CARTESIAN_POINT ( 'NONE',  ( -16.93589915522259304, 14.23555534794845023, -219.3310829164208542 ) ) ;
#133991 = CARTESIAN_POINT ( 'NONE',  ( -12.25000000000000178, 9.350000000011139178, -117.2500000000000284 ) ) ;
#133992 = CARTESIAN_POINT ( 'NONE',  ( -21.05000000000000071, 86.48473784507379492, -209.3714211149925575 ) ) ;
#133993 = CARTESIAN_POINT ( 'NONE',  ( 21.05000000000000071, 86.30329675166747450, -209.4258251677035787 ) ) ;
#133994 = CARTESIAN_POINT ( 'NONE',  ( -21.14999999999999858, 6.540656951712397138, -167.4999999999999716 ) ) ;
#133995 = ORIENTED_EDGE ( 'NONE', *, *, #101296, .T. ) ;
#133996 = CARTESIAN_POINT ( 'NONE',  ( -16.93230518875208190, 65.99924963859221805, -123.9473291364228658 ) ) ;
#133997 = EDGE_CURVE ( 'NONE', #229756, #134466, #163880, .T. ) ;
#133998 = CARTESIAN_POINT ( 'NONE',  ( -20.64999999999999858, 1.999999999999998224, -13.22462192276210224 ) ) ;
#133999 = CARTESIAN_POINT ( 'NONE',  ( 21.53752568617667862, 10.24627015979879197, -227.7034273308927084 ) ) ;
#134000 = DIRECTION ( 'NONE',  ( 1.000000000000000000, 7.304098846218105085E-16, 4.217023435051677501E-16 ) ) ;
#134001 = CIRCLE ( 'NONE', #159161, 0.09999999999998898659 ) ;
#134002 = AXIS2_PLACEMENT_3D ( 'NONE', #172227, #32714, #147478 ) ;
#134003 = DIRECTION ( 'NONE',  ( 0.000000000000000000, -0.9908441862701600211, 0.1350103645451876944 ) ) ;
#134004 = CIRCLE ( 'NONE', #117267, 11.65000000000000036 ) ;
#134005 = AXIS2_PLACEMENT_3D ( 'NONE', #70493, #125299, #150015 ) ;
#134006 = ORIENTED_EDGE ( 'NONE', *, *, #159555, .T. ) ;
#134007 = ORIENTED_EDGE ( 'NONE', *, *, #79249, .T. ) ;
#134008 = LINE ( 'NONE', #34953, #76067 ) ;
#134009 = DIRECTION ( 'NONE',  ( 0.000000000000000000, 0.000000000000000000, -1.000000000000000000 ) ) ;
#134010 = DIRECTION ( 'NONE',  ( 0.000000000000000000, 0.000000000000000000, -1.000000000000000000 ) ) ;
#134011 = ORIENTED_EDGE ( 'NONE', *, *, #74069, .F. ) ;
#134012 = DIRECTION ( 'NONE',  ( 0.000000000000000000, 0.4999999999999949485, -0.8660254037844415942 ) ) ;
#134013 = B_SPLINE_CURVE_WITH_KNOTS ( 'NONE', 3,
 ( #4531, #5807, #164907, #50085, #202744, #206598, #108777 ),
 .UNSPECIFIED., .F., .F.,
 ( 4, 3, 4 ),
 ( 0.000000000000000000, 3.357501770814783759E-05, 5.199112466349758733E-05 ),
 .UNSPECIFIED. ) ;
#134014 = DIRECTION ( 'NONE',  ( -1.000000000000000000, -0.000000000000000000, -0.000000000000000000 ) ) ;
#134015 = ORIENTED_EDGE ( 'NONE', *, *, #133257, .T. ) ;
#134016 = CARTESIAN_POINT ( 'NONE',  ( 20.94999999999999929, 70.50000000001230660, -157.6178414656113205 ) ) ;
#134017 = DIRECTION ( 'NONE',  ( 2.952720810173289112E-16, -1.000000000000000000, 0.000000000000000000 ) ) ;
#134018 = CIRCLE ( 'NONE', #117474, 11.65000000000000746 ) ;
#134019 = ORIENTED_EDGE ( 'NONE', *, *, #230944, .F. ) ;
#134020 = CARTESIAN_POINT ( 'NONE',  ( -20.97625342178429975, 12.80863705740234693, -205.3010250806640329 ) ) ;
#134021 = EDGE_LOOP ( 'NONE', ( #132640, #156933, #34028, #112819 ) ) ;
#134022 = CARTESIAN_POINT ( 'NONE',  ( -16.89021194854739605, 9.950000000011137047, -154.7425681316044006 ) ) ;
#134023 = DIRECTION ( 'NONE',  ( 0.000000000000000000, 0.000000000000000000, -1.000000000000000000 ) ) ;
#134024 = DIRECTION ( 'NONE',  ( 4.504528286903032433E-15, -0.1298341882520124002, -0.9915357197604841577 ) ) ;
#134025 = CARTESIAN_POINT ( 'NONE',  ( 21.05000000000000071, -1.162701749938009677, -7.900000000000000355 ) ) ;
#134026 = CARTESIAN_POINT ( 'NONE',  ( 18.59999999999999076, 69.55000000001253113, -182.2731074845244166 ) ) ;
#134027 = DIRECTION ( 'NONE',  ( 1.000000000000000000, 0.000000000000000000, 0.000000000000000000 ) ) ;
#134028 = DIRECTION ( 'NONE',  ( 0.000000000000000000, 0.000000000000000000, -1.000000000000000000 ) ) ;
#134029 = DIRECTION ( 'NONE',  ( 1.000000000000000000, -2.952720810173289112E-16, -2.061873921506763405E-30 ) ) ;
#134031 = CARTESIAN_POINT ( 'NONE',  ( 18.59999999999999076, 1.835341550235567887, -112.0551512925630249 ) ) ;
#134030 = LINE ( 'NONE', #3172, #99365 ) ;
#134032 = CARTESIAN_POINT ( 'NONE',  ( -21.44999999999999929, 44.96555909964510533, -237.8856228368455845 ) ) ;
#134033 = EDGE_CURVE ( 'NONE', #91127, #6368, #80646, .T. ) ;
#134034 = CARTESIAN_POINT ( 'NONE',  ( -23.15000000000000213, -11.48912529306489994, -164.4000000000000057 ) ) ;
#134035 = CARTESIAN_POINT ( 'NONE',  ( -21.14999999999999858, 75.90220970870339556, -142.7809220950004203 ) ) ;
#134036 = ORIENTED_EDGE ( 'NONE', *, *, #175460, .T. ) ;
#134037 = DIRECTION ( 'NONE',  ( 0.000000000000000000, 0.2128009952263485993, -0.9770955615653341697 ) ) ;
#134038 = DIRECTION ( 'NONE',  ( 1.000000000000000000, 0.000000000000000000, 0.000000000000000000 ) ) ;
#134039 = DIRECTION ( 'NONE',  ( -6.938893903907222067E-15, 1.000000000000000000, 2.891205793294679805E-16 ) ) ;
#134040 = AXIS2_PLACEMENT_3D ( 'NONE', #218999, #181186, #3814 ) ;
#134041 = ORIENTED_EDGE ( 'NONE', *, *, #178943, .T. ) ;
#134042 = DIRECTION ( 'NONE',  ( 0.000000000000000000, -0.8660254037844383745, 0.5000000000000003331 ) ) ;
#134043 = CARTESIAN_POINT ( 'NONE',  ( -20.64999999999999858, 68.85000000001180354, -81.87310748452436826 ) ) ;
#134045 = EDGE_CURVE ( 'NONE', #141916, #90926, #193114, .T. ) ;
#134044 = CARTESIAN_POINT ( 'NONE',  ( 23.24999999999999645, 36.65892442174935439, -249.5511627012433848 ) ) ;
#134046 = ORIENTED_EDGE ( 'NONE', *, *, #251909, .F. ) ;
#134047 = EDGE_CURVE ( 'NONE', #44736, #141516, #53644, .T. ) ;
#134048 = EDGE_CURVE ( 'NONE', #85698, #27052, #59793, .T. ) ;
#134049 = DIRECTION ( 'NONE',  ( 0.000000000000000000, 0.4930308989874980785, 0.8700118002898462599 ) ) ;
#134050 = ORIENTED_EDGE ( 'NONE', *, *, #69433, .T. ) ;
#134051 = CARTESIAN_POINT ( 'NONE',  ( 23.14999999999999858, -3.999999999988843147, -100.5000000000000426 ) ) ;
#134052 = CARTESIAN_POINT ( 'NONE',  ( -22.59999999999999787, 1.115600667400684642E-11, -134.0000000000000000 ) ) ;
#134053 = AXIS2_PLACEMENT_3D ( 'NONE', #74377, #116050, #174772 ) ;
#134054 = VECTOR ( 'NONE', #131375, 1000.000000000000000 ) ;
#134055 = TOROIDAL_SURFACE ( 'NONE', #171514, 7.800000000000000711, 0.1000000000000000056 ) ;
#134056 = ORIENTED_EDGE ( 'NONE', *, *, #213643, .F. ) ;
#134057 = DIRECTION ( 'NONE',  ( -1.000000000000000000, 0.000000000000000000, 0.000000000000000000 ) ) ;
#134058 = EDGE_CURVE ( 'NONE', #75872, #99952, #233575, .T. ) ;
#134059 = ORIENTED_EDGE ( 'NONE', *, *, #52623, .F. ) ;
#134060 = DIRECTION ( 'NONE',  ( -0.000000000000000000, -0.8814952561688430555, 0.4721928772777346239 ) ) ;
#134061 = FACE_OUTER_BOUND ( 'NONE', #161598, .T. ) ;
#134063 = CARTESIAN_POINT ( 'NONE',  ( -21.14999999999999858, 11.75000000001115552, -73.72613063605923855 ) ) ;
#134062 = PRODUCT_DEFINITION_CONTEXT ( 'detailed design', #192501, 'design' ) ;
#134064 = DIRECTION ( 'NONE',  ( 2.428612866367594051E-13, 0.4205162045344795763, -0.9072850278296868964 ) ) ;
#134065 = DIRECTION ( 'NONE',  ( 1.000000000000000000, 0.000000000000000000, 0.000000000000000000 ) ) ;
#134066 = CARTESIAN_POINT ( 'NONE',  ( -15.15766958671843412, 46.89553527312529724, -234.6535825622729874 ) ) ;
#134067 = CIRCLE ( 'NONE', #13476, 0.09999999999998898659 ) ;
#134068 = CARTESIAN_POINT ( 'NONE',  ( -20.94999999999999929, 11.70000000001115126, -194.2450018504813443 ) ) ;
#134069 = CARTESIAN_POINT ( 'NONE',  ( 21.05000000000000071, 67.23127455305835554, -235.8551265064784559 ) ) ;
#134071 = ORIENTED_EDGE ( 'NONE', *, *, #62780, .F. ) ;
#134070 = CARTESIAN_POINT ( 'NONE',  ( 21.07928932188134397, 69.67148334361864670, -103.1220026301787414 ) ) ;
#134072 = EDGE_LOOP ( 'NONE', ( #10191, #96033, #63979, #160834 ) ) ;
#134074 = CARTESIAN_POINT ( 'NONE',  ( -21.00219873199078435, 64.39461131213502654, -62.61046005622981880 ) ) ;
#134073 = CARTESIAN_POINT ( 'NONE',  ( -23.15000000000000213, 70.10000000001197407, -113.2422072491807086 ) ) ;
#134075 = ORIENTED_EDGE ( 'NONE', *, *, #61616, .T. ) ;
#134077 = VERTEX_POINT ( 'NONE', #20964 ) ;
#134076 = DIRECTION ( 'NONE',  ( -0.000000000000000000, 0.9770955615653316162, 0.2128009952263604232 ) ) ;
#134078 = ORIENTED_EDGE ( 'NONE', *, *, #240644, .T. ) ;
#134079 = DIRECTION ( 'NONE',  ( -0.000000000000000000, 1.156482317317873105E-15, 1.000000000000000000 ) ) ;
#134080 = EDGE_CURVE ( 'NONE', #207709, #103697, #196985, .T. ) ;
#134081 = LINE ( 'NONE', #93685, #38142 ) ;
#134082 = CARTESIAN_POINT ( 'NONE',  ( -16.87331047859649757, 9.950000000011138823, -121.3500000000000369 ) ) ;
#134083 = DIRECTION ( 'NONE',  ( 3.616040088954497272E-32, -1.224646799147352961E-16, 1.000000000000000000 ) ) ;
#134084 = CARTESIAN_POINT ( 'NONE',  ( 21.14999999999998082, 78.57160958314655375, -238.9307242378722833 ) ) ;
#134085 = CARTESIAN_POINT ( 'NONE',  ( -21.14999999999999858, 41.42187432231295219, -260.1830396872097140 ) ) ;
#134086 = CIRCLE ( 'NONE', #67452, 0.1000000000000028644 ) ;
#134087 = AXIS2_PLACEMENT_3D ( 'NONE', #108701, #150416, #73460 ) ;
#134088 = ADVANCED_FACE ( 'NONE', ( #137030 ), #200856, .F. ) ;
#134090 = AXIS2_PLACEMENT_3D ( 'NONE', #240495, #46139, #121844 ) ;
#134089 = CYLINDRICAL_SURFACE ( 'NONE', #114543, 11.75000000000000178 ) ;
#134091 = ORIENTED_EDGE ( 'NONE', *, *, #232392, .F. ) ;
#134092 = ORIENTED_EDGE ( 'NONE', *, *, #74097, .T. ) ;
#134093 = DIRECTION ( 'NONE',  ( 0.000000000000000000, 0.000000000000000000, -1.000000000000000000 ) ) ;
#134094 = ORIENTED_EDGE ( 'NONE', *, *, #28625, .F. ) ;
#134095 = CARTESIAN_POINT ( 'NONE',  ( 18.39999999999999503, 64.52683809664929981, -78.77310748452438816 ) ) ;
#134096 = ORIENTED_EDGE ( 'NONE', *, *, #98448, .T. ) ;
#134097 = CARTESIAN_POINT ( 'NONE',  ( 18.39999999999999858, -9.500000000000000000, -40.10018939122205239 ) ) ;
#134098 = DIRECTION ( 'NONE',  ( 1.000000000000000000, 0.000000000000000000, 0.000000000000000000 ) ) ;
#134099 = CARTESIAN_POINT ( 'NONE',  ( -23.25000000000000000, 71.65000000001228386, -157.6731074845243938 ) ) ;
#134100 = CARTESIAN_POINT ( 'NONE',  ( 18.59999999999999076, 76.00000000001170974, -69.52310748452431710 ) ) ;
#134101 = FACE_OUTER_BOUND ( 'NONE', #248213, .T. ) ;
#134102 = VERTEX_POINT ( 'NONE', #139571 ) ;
#134103 = CARTESIAN_POINT ( 'NONE',  ( 18.39999999999999503, 64.25000000001199396, -112.2731074845243739 ) ) ;
#134104 = LINE ( 'NONE', #49774, #63067 ) ;
#134105 = DIRECTION ( 'NONE',  ( -1.652117596168391700E-15, 1.000000000000000000, 6.982962677686266711E-15 ) ) ;
#134106 = CARTESIAN_POINT ( 'NONE',  ( 23.24999999999999289, 12.71802988599559647, -223.5105008658000258 ) ) ;
#134107 = DIRECTION ( 'NONE',  ( -1.000000000000000000, 0.000000000000000000, 0.000000000000000000 ) ) ;
#134108 = EDGE_LOOP ( 'NONE', ( #200853, #46538, #242408, #26776, #83147 ) ) ;
#134110 = CARTESIAN_POINT ( 'NONE',  ( 18.59999999999999076, 7.675662554762638479, -241.7139905447625381 ) ) ;
#134109 = FACE_OUTER_BOUND ( 'NONE', #241510, .T. ) ;
#134111 = ORIENTED_EDGE ( 'NONE', *, *, #174089, .F. ) ;
#134114 = ORIENTED_EDGE ( 'NONE', *, *, #191615, .F. ) ;
#134113 = DIRECTION ( 'NONE',  ( 0.000000000000000000, 0.000000000000000000, -1.000000000000000000 ) ) ;
#134112 = FACE_OUTER_BOUND ( 'NONE', #218410, .T. ) ;
#134115 = CIRCLE ( 'NONE', #121681, 0.09999999999999939493 ) ;
#134116 = CARTESIAN_POINT ( 'NONE',  ( 22.39999999999999503, 11.65000000001116298, -167.3999999999999773 ) ) ;
#134117 = EDGE_CURVE ( 'NONE', #27358, #71853, #30623, .T. ) ;
#134118 = DIRECTION ( 'NONE',  ( 0.000000000000000000, 0.000000000000000000, 1.000000000000000000 ) ) ;
#134119 = ORIENTED_EDGE ( 'NONE', *, *, #46221, .F. ) ;
#134121 = EDGE_CURVE ( 'NONE', #54936, #90288, #215281, .T. ) ;
#134120 = DIRECTION ( 'NONE',  ( -1.000000000000000000, -2.952720810173289112E-16, 0.000000000000000000 ) ) ;
#134122 = AXIS2_PLACEMENT_3D ( 'NONE', #254128, #216290, #16837 ) ;
#134123 = FACE_OUTER_BOUND ( 'NONE', #39756, .T. ) ;
#134124 = EDGE_CURVE ( 'NONE', #12219, #233644, #138336, .T. ) ;
#134125 = CARTESIAN_POINT ( 'NONE',  ( -17.01764560440421903, 9.949999999999983302, -12.74999999921389104 ) ) ;
#134126 = EDGE_CURVE ( 'NONE', #180230, #220173, #197180, .T. ) ;
#134128 = ORIENTED_EDGE ( 'NONE', *, *, #170498, .F. ) ;
#134127 = DIRECTION ( 'NONE',  ( 1.875376730785737966E-16, 0.4088369013363281068, -0.9126074666063770380 ) ) ;
#134129 = AXIS2_PLACEMENT_3D ( 'NONE', #138118, #242367, #22062 ) ;
#134130 = VECTOR ( 'NONE', #74528, 1000.000000000000000 ) ;
#134132 = ORIENTED_EDGE ( 'NONE', *, *, #136231, .T. ) ;
#134131 = EDGE_CURVE ( 'NONE', #241878, #225548, #217824, .T. ) ;
#134133 = AXIS2_PLACEMENT_3D ( 'NONE', #240027, #200886, #255680 ) ;
#134134 = AXIS2_PLACEMENT_3D ( 'NONE', #6870, #228504, #150256 ) ;
#134135 = DIRECTION ( 'NONE',  ( 1.000000000000000000, 0.000000000000000000, 0.000000000000000000 ) ) ;
#134136 = CARTESIAN_POINT ( 'NONE',  ( -21.59142135623730852, 62.86143984866549062, -221.9774629907318229 ) ) ;
#134137 = CARTESIAN_POINT ( 'NONE',  ( 21.05000000000000071, 85.50000000001179501, -79.41707660717668205 ) ) ;
#134138 = EDGE_CURVE ( 'NONE', #3363, #85598, #63925, .T. ) ;
#134139 = DIRECTION ( 'NONE',  ( -1.000000000000000000, 0.000000000000000000, 0.000000000000000000 ) ) ;
#134142 = EDGE_CURVE ( 'NONE', #190074, #2351, #22237, .T. ) ;
#134141 = EDGE_CURVE ( 'NONE', #248967, #200038, #199598, .T. ) ;
#134140 = EDGE_LOOP ( 'NONE', ( #51483, #236739, #194235, #207290 ) ) ;
#134143 = CARTESIAN_POINT ( 'NONE',  ( 21.05000000000005400, 64.35000000001119247, -51.02310748452479316 ) ) ;
#134144 = CARTESIAN_POINT ( 'NONE',  ( 23.24999999999999645, 5.000000000011153745, -88.09473398108696074 ) ) ;
#134145 = EDGE_CURVE ( 'NONE', #219183, #121041, #72312, .T. ) ;
#134146 = ORIENTED_EDGE ( 'NONE', *, *, #170001, .T. ) ;
#134147 = LINE ( 'NONE', #29956, #121244 ) ;
#134148 = AXIS2_PLACEMENT_3D ( 'NONE', #183668, #28478, #102808 ) ;
#134149 = CARTESIAN_POINT ( 'NONE',  ( -21.14999999999999858, 1.115600667400684642E-11, -88.85042919245522341 ) ) ;
#134150 = EDGE_CURVE ( 'NONE', #253241, #43496, #37953, .T. ) ;
#134151 = EDGE_LOOP ( 'NONE', ( #245482, #252550, #38490, #239778 ) ) ;
#134152 = CIRCLE ( 'NONE', #34424, 0.09999999999999938105 ) ;
#134153 = DIRECTION ( 'NONE',  ( 0.000000000000000000, 6.608470384673536035E-15, -1.000000000000000000 ) ) ;
#134154 = DIRECTION ( 'NONE',  ( -1.000000000000000000, 0.000000000000000000, 0.000000000000000000 ) ) ;
#134155 = ADVANCED_FACE ( 'NONE', ( #101721 ), #12871, .T. ) ;
#134158 = EDGE_CURVE ( 'NONE', #40973, #209179, #218012, .T. ) ;
#134157 = DIRECTION ( 'NONE',  ( 1.000000000000000000, 0.000000000000000000, 0.000000000000000000 ) ) ;
#134156 = AXIS2_PLACEMENT_3D ( 'NONE', #98971, #157751, #163803 ) ;
#134159 = ORIENTED_EDGE ( 'NONE', *, *, #182108, .F. ) ;
#134160 = EDGE_LOOP ( 'NONE', ( #58689, #252450, #224244, #19928 ) ) ;
#134161 = AXIS2_PLACEMENT_3D ( 'NONE', #88110, #236630, #114117 ) ;
#134162 = EDGE_CURVE ( 'NONE', #88008, #77088, #43082, .T. ) ;
#134163 = FACE_OUTER_BOUND ( 'NONE', #224047, .T. ) ;
#134164 = EDGE_LOOP ( 'NONE', ( #253993, #195336, #90234, #2343 ) ) ;
#134166 = ORIENTED_EDGE ( 'NONE', *, *, #87942, .F. ) ;
#134165 = DIRECTION ( 'NONE',  ( 0.000000000000000000, 0.000000000000000000, -1.000000000000000000 ) ) ;
#134167 = ADVANCED_FACE ( 'NONE', ( #96588 ), #255643, .F. ) ;
#134170 = ORIENTED_EDGE ( 'NONE', *, *, #118475, .T. ) ;
#134169 = VERTEX_POINT ( 'NONE', #126448 ) ;
#134168 = DIRECTION ( 'NONE',  ( 2.557131231893037478E-16, 0.8660254037844420383, -0.4999999999999943379 ) ) ;
#134171 = EDGE_CURVE ( 'NONE', #67224, #78967, #127748, .T. ) ;
#134172 = FACE_OUTER_BOUND ( 'NONE', #150223, .T. ) ;
#134173 = CARTESIAN_POINT ( 'NONE',  ( -16.87333278164151196, 12.45100533682980348, -211.7293307750952920 ) ) ;
#134174 = CIRCLE ( 'NONE', #55052, 0.4000000000000114575 ) ;
#134175 = FACE_OUTER_BOUND ( 'NONE', #141887, .T. ) ;
#134176 = CIRCLE ( 'NONE', #21780, 0.1000000000000028644 ) ;
#134177 = DIRECTION ( 'NONE',  ( -1.073024830501117725E-15, 0.000000000000000000, 1.000000000000000000 ) ) ;
#134178 = AXIS2_PLACEMENT_3D ( 'NONE', #63722, #140694, #157748 ) ;
#134179 = VERTEX_POINT ( 'NONE', #186440 ) ;
#134180 = ORIENTED_EDGE ( 'NONE', *, *, #187735, .T. ) ;
#134181 = ORIENTED_EDGE ( 'NONE', *, *, #185522, .T. ) ;
#134182 = DIRECTION ( 'NONE',  ( 1.000000000000000000, 0.000000000000000000, 0.000000000000000000 ) ) ;
#134184 = ORIENTED_EDGE ( 'NONE', *, *, #203332, .T. ) ;
#134183 = DIRECTION ( 'NONE',  ( 0.000000000000000000, 0.8741572761215442577, -0.4856429311786202851 ) ) ;
#134185 = CARTESIAN_POINT ( 'NONE',  ( 0.8999999999999992450, -8.350000000000004974, 21.95857864376269220 ) ) ;
#134186 = VERTEX_POINT ( 'NONE', #65188 ) ;
#134187 = EDGE_CURVE ( 'NONE', #217454, #51561, #250788, .T. ) ;
#134188 = DIRECTION ( 'NONE',  ( 0.000000000000000000, 0.000000000000000000, -1.000000000000000000 ) ) ;
#134189 = EDGE_LOOP ( 'NONE', ( #132852, #144934, #228542, #177224 ) ) ;
#134190 = LINE ( 'NONE', #233328, #170946 ) ;
#134191 = ORIENTED_EDGE ( 'NONE', *, *, #66866, .T. ) ;
#134192 = DIRECTION ( 'NONE',  ( -1.000000000000000000, 0.000000000000000000, -1.734723475976817507E-14 ) ) ;
#134193 = CARTESIAN_POINT ( 'NONE',  ( 20.94999999999999929, 76.00000000001246292, -172.0231074845243597 ) ) ;
#134194 = AXIS2_PLACEMENT_3D ( 'NONE', #86121, #9185, #147415 ) ;
#134196 = ORIENTED_EDGE ( 'NONE', *, *, #43999, .F. ) ;
#134195 = ORIENTED_EDGE ( 'NONE', *, *, #37800, .F. ) ;
#134197 = ORIENTED_EDGE ( 'NONE', *, *, #153156, .T. ) ;
#134198 = FACE_OUTER_BOUND ( 'NONE', #151191, .T. ) ;
#134199 = ORIENTED_EDGE ( 'NONE', *, *, #96790, .F. ) ;
#134200 = EDGE_LOOP ( 'NONE', ( #168145, #142328, #162732, #134872 ) ) ;
#134201 = DIRECTION ( 'NONE',  ( 1.000000000000000000, -1.875376730785737719E-16, -1.309568571767809260E-30 ) ) ;
#134203 = ORIENTED_EDGE ( 'NONE', *, *, #173317, .F. ) ;
#134202 = DIRECTION ( 'NONE',  ( -1.000000000000000000, 0.000000000000000000, -0.000000000000000000 ) ) ;
#134204 = CARTESIAN_POINT ( 'NONE',  ( 21.30000000000002558, 1.148907358139439339E-11, -201.0000000000015064 ) ) ;
#134206 = CYLINDRICAL_SURFACE ( 'NONE', #94337, 0.1000000000000098310 ) ;
#134205 = CARTESIAN_POINT ( 'NONE',  ( -22.39999999999999858, 64.35000000001214460, -136.6231074845243825 ) ) ;
#134207 = DIRECTION ( 'NONE',  ( 0.000000000000000000, 0.000000000000000000, 1.000000000000000000 ) ) ;
#134208 = CARTESIAN_POINT ( 'NONE',  ( -18.39999999999999858, 11.47316190337362762, -42.82594606680797256 ) ) ;
#134209 = DIRECTION ( 'NONE',  ( 0.000000000000000000, 0.000000000000000000, -1.000000000000000000 ) ) ;
#134210 = VERTEX_POINT ( 'NONE', #183857 ) ;
#134211 = ORIENTED_EDGE ( 'NONE', *, *, #39954, .T. ) ;
#134213 = EDGE_CURVE ( 'NONE', #257328, #132760, #117517, .T. ) ;
#134212 = DIRECTION ( 'NONE',  ( 1.000000000000000000, 7.304098846218133681E-16, 4.639676173203992654E-30 ) ) ;
#134214 = ORIENTED_EDGE ( 'NONE', *, *, #156228, .F. ) ;
#134215 = CARTESIAN_POINT ( 'NONE',  ( -23.25000000000000000, 77.02083669383561926, -199.7590813894317989 ) ) ;
#134216 = EDGE_CURVE ( 'NONE', #225601, #41121, #130553, .T. ) ;
#134217 = AXIS2_PLACEMENT_3D ( 'NONE', #59252, #196233, #76282 ) ;
#134218 = FACE_OUTER_BOUND ( 'NONE', #236176, .T. ) ;
#134219 = CARTESIAN_POINT ( 'NONE',  ( -18.59999999999999787, 18.51199663233067483, -231.2535697180530292 ) ) ;
#134220 = ORIENTED_EDGE ( 'NONE', *, *, #257494, .F. ) ;
#134221 = ORIENTED_EDGE ( 'NONE', *, *, #94426, .F. ) ;
#134222 = EDGE_CURVE ( 'NONE', #87571, #86852, #159785, .T. ) ;
#134223 = DIRECTION ( 'NONE',  ( 1.000000000000000000, 0.000000000000000000, 0.000000000000000000 ) ) ;
#134225 = EDGE_CURVE ( 'NONE', #62775, #99799, #241284, .T. ) ;
#134224 = DIRECTION ( 'NONE',  ( 0.000000000000000000, -0.4999999999999543698, -0.8660254037844650199 ) ) ;
#134226 = ORIENTED_EDGE ( 'NONE', *, *, #117301, .F. ) ;
#134227 = CARTESIAN_POINT ( 'NONE',  ( 18.50000000000000000, -7.785976468740638090, -209.8926132507865816 ) ) ;
#134228 = ORIENTED_EDGE ( 'NONE', *, *, #87371, .F. ) ;
#134229 = CARTESIAN_POINT ( 'NONE',  ( -21.05000000000000426, 6.332272273946814245, -100.5375360632857138 ) ) ;
#134230 = PLANE ( 'NONE',  #45522 ) ;
#134232 = CARTESIAN_POINT ( 'NONE',  ( -21.05000000000000071, -1.300857950936794571, -194.8777500463866659 ) ) ;
#134231 = CYLINDRICAL_SURFACE ( 'NONE', #44895, 0.09999999999999520384 ) ;
#134233 = ADVANCED_FACE ( 'NONE', ( #242541 ), #182595, .T. ) ;
#134234 = CARTESIAN_POINT ( 'NONE',  ( -18.39999999999999858, 13.19494617735151465, -207.6708402378485516 ) ) ;
#134235 = DIRECTION ( 'NONE',  ( 0.000000000000000000, -1.000000000000000000, 0.000000000000000000 ) ) ;
#134236 = AXIS2_PLACEMENT_3D ( 'NONE', #222496, #24346, #64730 ) ;
#134237 = DIRECTION ( 'NONE',  ( 0.000000000000000000, 0.000000000000000000, -1.000000000000000000 ) ) ;
#134238 = CIRCLE ( 'NONE', #151016, 3.999999999999999112 ) ;
#134239 = EDGE_CURVE ( 'NONE', #31326, #117566, #38994, .T. ) ;
#134241 = EDGE_LOOP ( 'NONE', ( #60940, #79848, #198545, #63749, #173075, #197337, #247783, #11552, #220257, #80985 ) ) ;
#134240 = ORIENTED_EDGE ( 'NONE', *, *, #136531, .F. ) ;
#134242 = EDGE_LOOP ( 'NONE', ( #185466, #185808, #243710, #56881 ) ) ;
#134243 = CARTESIAN_POINT ( 'NONE',  ( -18.59999999999999787, 77.85161776048053639, -57.91991776492063337 ) ) ;
#134244 = CARTESIAN_POINT ( 'NONE',  ( 22.46250603428203618, 0.02114417613880632471, 11.64986309734008074 ) ) ;
#134245 = CARTESIAN_POINT ( 'NONE',  ( -18.39999999999999858, -9.499999999988849808, -107.5320693966997112 ) ) ;
#134247 = DIRECTION ( 'NONE',  ( 0.000000000000000000, -0.9667078373770113808, -0.2558827019434133376 ) ) ;
#134246 = CARTESIAN_POINT ( 'NONE',  ( -16.87372397896795562, 66.11940046337079480, -183.1723829744886700 ) ) ;
#134248 = DIRECTION ( 'NONE',  ( 1.000000000000000000, 0.000000000000000000, 0.000000000000000000 ) ) ;
#134249 = EDGE_LOOP ( 'NONE', ( #68895, #38348, #62952, #96531 ) ) ;
#134250 = CARTESIAN_POINT ( 'NONE',  ( 21.53752568617679586, 69.21319212550768896, -69.62208194579503129 ) ) ;
#134251 = ORIENTED_EDGE ( 'NONE', *, *, #182471, .F. ) ;
#134252 = ORIENTED_EDGE ( 'NONE', *, *, #54897, .T. ) ;
#134253 = DIRECTION ( 'NONE',  ( -1.000000000000000000, 0.000000000000000000, 0.000000000000000000 ) ) ;
#134254 = DIRECTION ( 'NONE',  ( 1.000000000000000000, -0.000000000000000000, -0.000000000000000000 ) ) ;
#134255 = DIRECTION ( 'NONE',  ( 0.000000000000000000, 0.000000000000000000, -1.000000000000000000 ) ) ;
#134256 = EDGE_CURVE ( 'NONE', #174999, #175804, #23542, .T. ) ;
#134257 = CARTESIAN_POINT ( 'NONE',  ( 23.14999999999999858, 70.40000000001150227, -48.42837350343745584 ) ) ;
#134258 = FACE_OUTER_BOUND ( 'NONE', #256055, .T. ) ;
#134259 = ORIENTED_EDGE ( 'NONE', *, *, #174488, .F. ) ;
#134260 = ORIENTED_EDGE ( 'NONE', *, *, #58752, .F. ) ;
#134261 = FACE_OUTER_BOUND ( 'NONE', #129766, .T. ) ;
#134262 = AXIS2_PLACEMENT_3D ( 'NONE', #139541, #1311, #57436 ) ;
#134263 = CYLINDRICAL_SURFACE ( 'NONE', #211349, 0.09999999999999939493 ) ;
#134264 = DIRECTION ( 'NONE',  ( 1.000000000000000000, 0.000000000000000000, 0.000000000000000000 ) ) ;
#134265 = CARTESIAN_POINT ( 'NONE',  ( -20.54999999999999716, 4.350000000011156054, -54.64999999999999858 ) ) ;
#134266 = CYLINDRICAL_SURFACE ( 'NONE', #133552, 0.1000000000000002554 ) ;
#134268 = EDGE_CURVE ( 'NONE', #7048, #49647, #26082, .T. ) ;
#134267 = CARTESIAN_POINT ( 'NONE',  ( -16.87331047859649757, 63.08573235307424198, -213.1276215869287967 ) ) ;
#134269 = DIRECTION ( 'NONE',  ( -0.000000000000000000, -6.982962677686266711E-15, 1.000000000000000000 ) ) ;
#134270 = B_SPLINE_CURVE_WITH_KNOTS ( 'NONE', 3,
 ( #43603, #26628, #68308, #203952, #44888, #244353, #65730, #67014 ),
 .UNSPECIFIED., .F., .F.,
 ( 4, 2, 2, 4 ),
 ( 0.000000000000000000, 0.0002114466876441986436, 0.0003171700314663001880, 0.0004228933752884017866 ),
 .UNSPECIFIED. ) ;
#134273 = DIRECTION ( 'NONE',  ( 1.000000000000000000, 0.000000000000000000, 0.000000000000000000 ) ) ;
#134272 = AXIS2_PLACEMENT_3D ( 'NONE', #217474, #114551, #74175 ) ;
#134271 = CYLINDRICAL_SURFACE ( 'NONE', #136979, 0.09999999999999939493 ) ;
#134275 = CARTESIAN_POINT ( 'NONE',  ( -21.14999999999999858, 64.35000000001166143, -69.52310748452438816 ) ) ;
#134274 = AXIS2_PLACEMENT_3D ( 'NONE', #182818, #104508, #4149 ) ;
#134276 = EDGE_CURVE ( 'NONE', #106654, #251285, #138881, .T. ) ;
#134277 = AXIS2_PLACEMENT_3D ( 'NONE', #33058, #175137, #177683 ) ;
#134278 = DIRECTION ( 'NONE',  ( 0.000000000000000000, 0.000000000000000000, -1.000000000000000000 ) ) ;
#134279 = CYLINDRICAL_SURFACE ( 'NONE', #103766, 0.1000000000000001305 ) ;
#134280 = CARTESIAN_POINT ( 'NONE',  ( -23.15000000000000213, 64.25000000001179501, -81.67310748452440805 ) ) ;
#134282 = ORIENTED_EDGE ( 'NONE', *, *, #112790, .T. ) ;
#134281 = DIRECTION ( 'NONE',  ( -0.000000000000000000, -0.000000000000000000, 1.000000000000000000 ) ) ;
#134283 = EDGE_CURVE ( 'NONE', #171719, #53585, #222099, .T. ) ;
#134284 = DIRECTION ( 'NONE',  ( -1.000000000000000000, 7.510212038922847255E-17, -1.676432719286211941E-16 ) ) ;
#134285 = VERTEX_POINT ( 'NONE', #142158 ) ;
#134286 = EDGE_CURVE ( 'NONE', #187280, #131489, #103020, .T. ) ;
#134287 = EDGE_CURVE ( 'NONE', #131118, #180615, #71754, .T. ) ;
#134288 = DIRECTION ( 'NONE',  ( 0.000000000000000000, 0.000000000000000000, -1.000000000000000000 ) ) ;
#134289 = CARTESIAN_POINT ( 'NONE',  ( 18.69999999999999929, -8.350000000000004974, 10.95857864376269575 ) ) ;
#134290 = EDGE_CURVE ( 'NONE', #75413, #176760, #104988, .T. ) ;
#134291 = CARTESIAN_POINT ( 'NONE',  ( -20.94999999999999929, 0.2561057921033771945, -100.4651035583277405 ) ) ;
#134293 = VECTOR ( 'NONE', #189587, 1000.000000000000000 ) ;
#134292 = CARTESIAN_POINT ( 'NONE',  ( -21.05000000000000071, 1.115600667400684642E-11, -167.5000000000000284 ) ) ;
#134294 = CIRCLE ( 'NONE', #88493, 7.900000000000007461 ) ;
#134295 = DIRECTION ( 'NONE',  ( 0.000000000000000000, -0.2617529984165152257, -0.9651348961777124202 ) ) ;
#134296 = LINE ( 'NONE', #237278, #182689 ) ;
#134297 = DIRECTION ( 'NONE',  ( 0.000000000000000000, 0.000000000000000000, -1.000000000000000000 ) ) ;
#134298 = EDGE_LOOP ( 'NONE', ( #216924, #41125, #210688, #9474 ) ) ;
#134300 = ORIENTED_EDGE ( 'NONE', *, *, #197311, .F. ) ;
#134299 = CARTESIAN_POINT ( 'NONE',  ( -20.94999999999999929, 77.16270174995010223, -128.4231074845242802 ) ) ;
#134301 = DIRECTION ( 'NONE',  ( 0.000000000000000000, 0.9654727137038715545, -0.2605042016806676242 ) ) ;
#134302 = ADVANCED_FACE ( 'NONE', ( #84715 ), #147296, .T. ) ;
#134303 = AXIS2_PLACEMENT_3D ( 'NONE', #67172, #107568, #149299 ) ;
#134304 = CYLINDRICAL_SURFACE ( 'NONE', #28784, 0.1000000000000124678 ) ;
#134305 = CARTESIAN_POINT ( 'NONE',  ( -22.59066674512241235, 31.82725254005515936, -238.8404961800037256 ) ) ;
#134306 = ORIENTED_EDGE ( 'NONE', *, *, #23322, .F. ) ;
#134307 = CARTESIAN_POINT ( 'NONE',  ( -16.80621392010917958, 66.05779742250486208, -190.8335155191072374 ) ) ;
#134308 = VECTOR ( 'NONE', #123405, 1000.000000000000000 ) ;
#134309 = APPLICATION_PROTOCOL_DEFINITION ( 'draft international standard', 'automotive_design', 1998, #70691 ) ;
#134310 = DIRECTION ( 'NONE',  ( 1.000000000000000000, 0.000000000000000000, 0.000000000000000000 ) ) ;
#134312 = VECTOR ( 'NONE', #230356, 1000.000000000000000 ) ;
#134311 = CARTESIAN_POINT ( 'NONE',  ( -22.39999999999999858, 11.65000000001115588, -133.9000000000000057 ) ) ;
#134313 = ORIENTED_EDGE ( 'NONE', *, *, #131453, .T. ) ;
#134314 = VECTOR ( 'NONE', #195476, 1000.000000000000114 ) ;
#134315 = DIRECTION ( 'NONE',  ( 1.186688945009009831E-16, -0.4721928772777346239, -0.8814952561688430555 ) ) ;
#134316 = DIRECTION ( 'NONE',  ( 0.000000000000000000, -1.000000000000000000, -6.982962677686266711E-15 ) ) ;
#134317 = CIRCLE ( 'NONE', #21911, 12.97499999999999964 ) ;
#134318 = TOROIDAL_SURFACE ( 'NONE', #26023, 0.2000000000000000111, 0.1000000000000000056 ) ;
#134319 = DIRECTION ( 'NONE',  ( 1.000000000000000000, 3.265361837132813093E-16, -0.000000000000000000 ) ) ;
#134320 = EDGE_LOOP ( 'NONE', ( #140778, #235857 ) ) ;
#134321 = ORIENTED_EDGE ( 'NONE', *, *, #5341, .T. ) ;
#134323 = VECTOR ( 'NONE', #168963, 1000.000000000000114 ) ;
#134322 = DIRECTION ( 'NONE',  ( 0.000000000000000000, -0.000000000000000000, 1.000000000000000000 ) ) ;
#134325 = AXIS2_PLACEMENT_3D ( 'NONE', #96454, #100306, #138151 ) ;
#134324 = DIRECTION ( 'NONE',  ( -0.000000000000000000, 0.8660254037844383745, -0.5000000000000003331 ) ) ;
#134326 = CARTESIAN_POINT ( 'NONE',  ( -20.64999999999999858, 65.86663596189677605, -213.5709895136416776 ) ) ;
#134327 = FACE_OUTER_BOUND ( 'NONE', #62792, .T. ) ;
#134329 = CARTESIAN_POINT ( 'NONE',  ( -23.25000000000000000, 64.25000000001215028, -136.5231074845243597 ) ) ;
#134328 = DIRECTION ( 'NONE',  ( -1.000000000000000000, -0.000000000000000000, -0.000000000000000000 ) ) ;
#134330 = CIRCLE ( 'NONE', #50935, 0.09999999999999939493 ) ;
#134331 = CYLINDRICAL_SURFACE ( 'NONE', #252568, 11.75000000000001066 ) ;
#134332 = SPHERICAL_SURFACE ( 'NONE', #10409, 0.1000000000000000056 ) ;
#134333 = CARTESIAN_POINT ( 'NONE',  ( 22.57320508075687115, 11.75000000001115552, -100.5000000000000284 ) ) ;
#134334 = CARTESIAN_POINT ( 'NONE',  ( -13.39999999999994529, 67.65000000001118963, -25.06452884076210452 ) ) ;
#134335 = EDGE_LOOP ( 'NONE', ( #147664, #48796, #97615, #163353 ) ) ;
#134336 = EDGE_CURVE ( 'NONE', #221411, #13648, #255400, .T. ) ;
#134337 = ORIENTED_EDGE ( 'NONE', *, *, #28131, .T. ) ;
#134338 = LINE ( 'NONE', #16997, #185331 ) ;
#134339 = VECTOR ( 'NONE', #23567, 1000.000000000000000 ) ;
#134340 = DIRECTION ( 'NONE',  ( -1.000000000000000000, 0.000000000000000000, 0.000000000000000000 ) ) ;
#134341 = DIRECTION ( 'NONE',  ( -1.000000000000000000, 2.952720810173289112E-16, 2.061873921506763405E-30 ) ) ;
#134342 = AXIS2_PLACEMENT_3D ( 'NONE', #87816, #209078, #70883 ) ;
#134343 = FACE_OUTER_BOUND ( 'NONE', #16303, .T. ) ;
#134344 = DIRECTION ( 'NONE',  ( 1.000000000000000000, 0.000000000000000000, 0.000000000000000000 ) ) ;
#134347 = EDGE_CURVE ( 'NONE', #108159, #10047, #88842, .T. ) ;
#134346 = CARTESIAN_POINT ( 'NONE',  ( 15.07585980824112859, 13.06404166453376980, -216.7291753257208029 ) ) ;
#134345 = CIRCLE ( 'NONE', #121907, 0.1000000000000024342 ) ;
#134348 = ORIENTED_EDGE ( 'NONE', *, *, #67528, .F. ) ;
#134349 = EDGE_LOOP ( 'NONE', ( #202839, #244159, #244240, #53971, #155123, #211504, #222612, #184393, #118566 ) ) ;
#134350 = EDGE_CURVE ( 'NONE', #42984, #224632, #110734, .T. ) ;
#134351 = EDGE_CURVE ( 'NONE', #105032, #29024, #248983, .T. ) ;
#134352 = CARTESIAN_POINT ( 'NONE',  ( 23.24999999999999645, 8.822561741677553471, -42.75000000000000000 ) ) ;
#134353 = VERTEX_POINT ( 'NONE', #211125 ) ;
#134354 = DIRECTION ( 'NONE',  ( 1.000000000000000000, 0.000000000000000000, 0.000000000000000000 ) ) ;
#134355 = AXIS2_PLACEMENT_3D ( 'NONE', #11206, #88130, #244661 ) ;
#134356 = AXIS2_PLACEMENT_3D ( 'NONE', #169403, #212357, #168125 ) ;
#134357 = CARTESIAN_POINT ( 'NONE',  ( 18.59999999999999076, 68.87972903831482085, -166.3635444426850825 ) ) ;
#134358 = VECTOR ( 'NONE', #204203, 1000.000000000000000 ) ;
#134359 = PLANE ( 'NONE',  #152499 ) ;
#134360 = ORIENTED_EDGE ( 'NONE', *, *, #60783, .T. ) ;
#134361 = CARTESIAN_POINT ( 'NONE',  ( 23.24999999999997513, 64.25000000001175238, -76.53791325517833855 ) ) ;
#134362 = ADVANCED_FACE ( 'NONE', ( #108184 ), #190294, .T. ) ;
#134363 = DIRECTION ( 'NONE',  ( -1.000000000000000000, -0.000000000000000000, -0.000000000000000000 ) ) ;
#134364 = CARTESIAN_POINT ( 'NONE',  ( -18.39999999999999858, 64.52683809664983983, -160.6971614177164724 ) ) ;
#134365 = CARTESIAN_POINT ( 'NONE',  ( 21.59780538579341780, 75.90102133041420984, -143.3701980144675474 ) ) ;
#134366 = DIRECTION ( 'NONE',  ( 0.000000000000000000, 1.000000000000000000, -6.308085367188393199E-16 ) ) ;
#134368 = DIRECTION ( 'NONE',  ( 0.000000000000000000, -0.9126074666063769270, -0.4088369013363280513 ) ) ;
#134367 = CARTESIAN_POINT ( 'NONE',  ( 21.00000000000000000, 66.25000000001199396, -115.2731074845243597 ) ) ;
#134369 = CARTESIAN_POINT ( 'NONE',  ( -16.82542659449977762, 66.06550010858478572, -149.2677430845504318 ) ) ;
#134370 = ORIENTED_EDGE ( 'NONE', *, *, #135998, .F. ) ;
#134371 = AXIS2_PLACEMENT_3D ( 'NONE', #244568, #65945, #145466 ) ;
#134373 = CARTESIAN_POINT ( 'NONE',  ( -16.83199318825828072, 66.06935387203084531, -115.7955222963151698 ) ) ;
#134372 = DIRECTION ( 'NONE',  ( 1.000000000000000000, -0.000000000000000000, -0.000000000000000000 ) ) ;
#134374 = ORIENTED_EDGE ( 'NONE', *, *, #29199, .T. ) ;
#134376 = ORIENTED_EDGE ( 'NONE', *, *, #157163, .F. ) ;
#134375 = DIRECTION ( 'NONE',  ( -1.000000000000000000, 0.000000000000000000, -0.000000000000000000 ) ) ;
#134377 = ORIENTED_EDGE ( 'NONE', *, *, #142683, .F. ) ;
#134378 = DIRECTION ( 'NONE',  ( -1.073024830501117725E-15, 6.982962677686266711E-15, -1.000000000000000000 ) ) ;
#134379 = DIRECTION ( 'NONE',  ( 0.000000000000000000, -1.445602896647342861E-16, 1.000000000000000000 ) ) ;
#134380 = CARTESIAN_POINT ( 'NONE',  ( 20.94999999999999929, 1.115600667400684642E-11, -167.5000000000000284 ) ) ;
#134381 = LINE ( 'NONE', #17043, #162602 ) ;
#134382 = AXIS2_PLACEMENT_3D ( 'NONE', #187927, #131790, #10576 ) ;
#134383 = EDGE_LOOP ( 'NONE', ( #163660, #50753, #214889, #205899 ) ) ;
#134384 = EDGE_CURVE ( 'NONE', #126771, #176941, #171713, .T. ) ;
#134385 = EDGE_CURVE ( 'NONE', #190309, #57548, #113430, .T. ) ;
#134386 = CARTESIAN_POINT ( 'NONE',  ( -23.15000000000000213, 1.148907358139439339E-11, -201.0000000000015064 ) ) ;
#134387 = ORIENTED_EDGE ( 'NONE', *, *, #22705, .T. ) ;
#134388 = FACE_OUTER_BOUND ( 'NONE', #163548, .T. ) ;
#134389 = EDGE_CURVE ( 'NONE', #65545, #110864, #204981, .T. ) ;
#134390 = DIRECTION ( 'NONE',  ( 0.000000000000000000, 0.000000000000000000, -1.000000000000000000 ) ) ;
#134391 = ORIENTED_EDGE ( 'NONE', *, *, #117028, .T. ) ;
#134392 = ORIENTED_EDGE ( 'NONE', *, *, #136801, .F. ) ;
#134393 = DIRECTION ( 'NONE',  ( 0.000000000000000000, -0.9126074666063769270, -0.4088369013363280513 ) ) ;
#134394 = AXIS2_PLACEMENT_3D ( 'NONE', #73462, #211672, #29216 ) ;
#134395 = VERTEX_POINT ( 'NONE', #109438 ) ;
#134396 = CARTESIAN_POINT ( 'NONE',  ( 20.73486653747088582, 42.13647595316533057, -239.1530172309881550 ) ) ;
#134397 = ORIENTED_EDGE ( 'NONE', *, *, #70003, .T. ) ;
#134398 = DIRECTION ( 'NONE',  ( 0.000000000000000000, -1.000000000000000000, 0.000000000000000000 ) ) ;
#134399 = CARTESIAN_POINT ( 'NONE',  ( -18.50000000000000355, 77.26327546522863088, -28.12124281777790813 ) ) ;
#134400 = DIRECTION ( 'NONE',  ( 0.000000000000000000, 0.9654727137038715545, -0.2605042016806676242 ) ) ;
#134401 = CARTESIAN_POINT ( 'NONE',  ( 21.05000000000000071, 76.00000000001193712, -107.0231074845243029 ) ) ;
#134402 = EDGE_CURVE ( 'NONE', #52066, #24624, #230117, .T. ) ;
#134404 = CIRCLE ( 'NONE', #138501, 0.09999999999999911737 ) ;
#134403 = CARTESIAN_POINT ( 'NONE',  ( -22.47071067811865319, 0.09909245471376171288, -25.77992525550194003 ) ) ;
#134405 = CARTESIAN_POINT ( 'NONE',  ( 21.05000000000000071, 6.650000000011155876, -43.34382208968312966 ) ) ;
#134406 = DIRECTION ( 'NONE',  ( 0.000000000000000000, 0.000000000000000000, -1.000000000000000000 ) ) ;
#134407 = ORIENTED_EDGE ( 'NONE', *, *, #160692, .T. ) ;
#134409 = CARTESIAN_POINT ( 'NONE',  ( 23.14999999999999147, 1.115600667400684642E-11, -33.50000000000000000 ) ) ;
#134408 = CARTESIAN_POINT ( 'NONE',  ( 23.14999999999999503, 64.25000000001253397, -182.2731074845244450 ) ) ;
#134411 = ORIENTED_EDGE ( 'NONE', *, *, #53113, .T. ) ;
#134410 = AXIS2_PLACEMENT_3D ( 'NONE', #233222, #14175, #54552 ) ;
#134414 = ORIENTED_EDGE ( 'NONE', *, *, #41822, .T. ) ;
#134413 = CARTESIAN_POINT ( 'NONE',  ( 22.57320508075687115, 64.25000000001215028, -136.5231074845243597 ) ) ;
#134412 = CARTESIAN_POINT ( 'NONE',  ( 21.05000000000000071, 11.65000000001115943, -67.10000000000005116 ) ) ;
#134415 = ORIENTED_EDGE ( 'NONE', *, *, #28494, .F. ) ;
#134416 = DIRECTION ( 'NONE',  ( -1.000000000000000000, 0.000000000000000000, -0.000000000000000000 ) ) ;
#134417 = LINE ( 'NONE', #229700, #209825 ) ;
#134419 = FACE_OUTER_BOUND ( 'NONE', #226849, .T. ) ;
#134418 = VECTOR ( 'NONE', #239481, 1000.000000000000000 ) ;
#134420 = ADVANCED_FACE ( 'NONE', ( #228132 ), #33817, .F. ) ;
#134421 = CARTESIAN_POINT ( 'NONE',  ( 21.05000000000005400, 84.00000000001119815, -37.18565239344504647 ) ) ;
#134422 = ORIENTED_EDGE ( 'NONE', *, *, #154504, .F. ) ;
#134424 = EDGE_LOOP ( 'NONE', ( #144221, #122535, #51405, #36006 ) ) ;
#134423 = CARTESIAN_POINT ( 'NONE',  ( -18.50000000000000000, 70.05000000001193428, -92.71740517948948934 ) ) ;
#134425 = ADVANCED_FACE ( 'NONE', ( #252802 ), #52028, .T. ) ;
#134427 = CARTESIAN_POINT ( 'NONE',  ( 23.15000000000000213, 87.65000000001144542, -39.02310748452423894 ) ) ;
#134426 = DIRECTION ( 'NONE',  ( 0.000000000000000000, 0.000000000000000000, 1.000000000000000000 ) ) ;
#134428 = ADVANCED_FACE ( 'NONE', ( #250250 ), #231993, .F. ) ;
#134430 = ORIENTED_EDGE ( 'NONE', *, *, #233129, .T. ) ;
#134429 = CARTESIAN_POINT ( 'NONE',  ( 20.04142135623730070, 64.25000000001148237, -44.87310748452440379 ) ) ;
#134431 = VECTOR ( 'NONE', #42838, 1000.000000000000000 ) ;
#134432 = AXIS2_PLACEMENT_3D ( 'NONE', #146966, #210811, #132562 ) ;
#134433 = ORIENTED_EDGE ( 'NONE', *, *, #165233, .T. ) ;
#134435 = ADVANCED_FACE ( 'NONE', ( #91177 ), #131585, .F. ) ;
#134434 = CARTESIAN_POINT ( 'NONE',  ( 20.95052659398289308, 11.85180822207893669, -206.1716151108944644 ) ) ;
#134436 = CARTESIAN_POINT ( 'NONE',  ( -21.65000000000000213, 60.96553306590055854, -220.9452142459683159 ) ) ;
#134438 = EDGE_CURVE ( 'NONE', #7468, #247780, #71929, .T. ) ;
#134437 = EDGE_LOOP ( 'NONE', ( #143478, #94284, #111594, #113327 ) ) ;
#134439 = CARTESIAN_POINT ( 'NONE',  ( -21.04999999999994387, 69.83923505573476120, -35.48358590217651454 ) ) ;
#134440 = VERTEX_POINT ( 'NONE', #113304 ) ;
#134441 = CIRCLE ( 'NONE', #217828, 0.5000000000000004441 ) ;
#134442 = DIRECTION ( 'NONE',  ( 0.000000000000000000, 0.8814952561688442767, -0.4721928772777324035 ) ) ;
#134443 = DIRECTION ( 'NONE',  ( 0.000000000000000000, 1.000000000000000000, 0.000000000000000000 ) ) ;
#134444 = ORIENTED_EDGE ( 'NONE', *, *, #23202, .T. ) ;
#134445 = DIRECTION ( 'NONE',  ( 1.000000000000000000, 0.000000000000000000, 0.000000000000000000 ) ) ;
#134446 = CIRCLE ( 'NONE', #171922, 0.1000000000000072220 ) ;
#134447 = CIRCLE ( 'NONE', #251147, 7.720710678118663850 ) ;
#134448 = AXIS2_PLACEMENT_3D ( 'NONE', #110649, #70274, #11569 ) ;
#134449 = VECTOR ( 'NONE', #10119, 1000.000000000000000 ) ;
#134450 = EDGE_CURVE ( 'NONE', #48019, #70426, #55127, .T. ) ;
#134451 = DIRECTION ( 'NONE',  ( 0.000000000000000000, -0.1332476588733589040, 0.9910827722268049644 ) ) ;
#134452 = EDGE_CURVE ( 'NONE', #83517, #118873, #153773, .T. ) ;
#134453 = EDGE_CURVE ( 'NONE', #12588, #251277, #196805, .T. ) ;
#134454 = ORIENTED_EDGE ( 'NONE', *, *, #76117, .T. ) ;
#134455 = ORIENTED_EDGE ( 'NONE', *, *, #141554, .T. ) ;
#134456 = FACE_OUTER_BOUND ( 'NONE', #85915, .T. ) ;
#134457 = VERTEX_POINT ( 'NONE', #230701 ) ;
#134458 = EDGE_CURVE ( 'NONE', #79058, #133293, #155161, .T. ) ;
#134459 = ORIENTED_EDGE ( 'NONE', *, *, #245555, .T. ) ;
#134461 = ORIENTED_EDGE ( 'NONE', *, *, #135624, .T. ) ;
#134460 = CARTESIAN_POINT ( 'NONE',  ( -23.25000000000000000, 65.66751761918692409, -130.9282609406112670 ) ) ;
#134463 = EDGE_CURVE ( 'NONE', #160017, #43253, #63514, .T. ) ;
#134462 = ORIENTED_EDGE ( 'NONE', *, *, #122767, .F. ) ;
#134464 = DIRECTION ( 'NONE',  ( -1.000000000000000000, -0.000000000000000000, -0.000000000000000000 ) ) ;
#134466 = VERTEX_POINT ( 'NONE', #157611 ) ;
#134465 = EDGE_CURVE ( 'NONE', #145757, #255780, #84314, .T. ) ;
#134469 = ORIENTED_EDGE ( 'NONE', *, *, #220639, .F. ) ;
#134468 = VERTEX_POINT ( 'NONE', #37641 ) ;
#134467 = CARTESIAN_POINT ( 'NONE',  ( -23.15000000000000213, 1.115651490242849210E-11, -163.3499999999999943 ) ) ;
#134470 = EDGE_CURVE ( 'NONE', #163431, #227883, #146701, .T. ) ;
#134471 = CIRCLE ( 'NONE', #1197, 0.09999999999999771572 ) ;
#134472 = ORIENTED_EDGE ( 'NONE', *, *, #212615, .F. ) ;
#134473 = PLANE ( 'NONE',  #75886 ) ;
#134474 = ORIENTED_EDGE ( 'NONE', *, *, #201955, .F. ) ;
#134475 = CIRCLE ( 'NONE', #226048, 0.2000000000000057288 ) ;
#134476 = B_SPLINE_CURVE_WITH_KNOTS ( 'NONE', 3,
 ( #148644, #70415, #149934, #228175, #130334, #229455, #170815, #71681, #151207, #187322 ),
 .UNSPECIFIED., .F., .F.,
 ( 4, 2, 2, 2, 4 ),
 ( 0.000000000000000000, 0.0001584437871625818894, 0.0002376656807438358356, 0.0002772766275344235335, 0.0003168875743250112315 ),
 .UNSPECIFIED. ) ;
#134477 = CARTESIAN_POINT ( 'NONE',  ( -16.93589915522259304, 10.00862525870701347, -154.9405601019603296 ) ) ;
#134478 = AXIS2_PLACEMENT_3D ( 'NONE', #95418, #175006, #215358 ) ;
#134480 = ORIENTED_EDGE ( 'NONE', *, *, #240732, .T. ) ;
#134479 = DIRECTION ( 'NONE',  ( 0.000000000000000000, 0.000000000000000000, -1.000000000000000000 ) ) ;
#134481 = LINE ( 'NONE', #229752, #233904 ) ;
#134482 = VERTEX_POINT ( 'NONE', #16795 ) ;
#134483 = EDGE_CURVE ( 'NONE', #38660, #54887, #119741, .T. ) ;
#134484 = EDGE_LOOP ( 'NONE', ( #103936, #84161, #159640, #248279 ) ) ;
#134485 = EDGE_CURVE ( 'NONE', #102962, #148888, #26132, .T. ) ;
#134486 = AXIS2_PLACEMENT_3D ( 'NONE', #56046, #153944, #15700 ) ;
#134487 = CARTESIAN_POINT ( 'NONE',  ( 22.39999999999999503, 1.115541036281197940E-11, -159.7092204016265669 ) ) ;
#134488 = CARTESIAN_POINT ( 'NONE',  ( 18.51024323315077069, 18.37846419038448431, -236.9325101954433137 ) ) ;
#134489 = CIRCLE ( 'NONE', #105435, 11.65000000000000036 ) ;
#134491 = ORIENTED_EDGE ( 'NONE', *, *, #194535, .T. ) ;
#134490 = AXIS2_PLACEMENT_3D ( 'NONE', #2384, #42820, #157678 ) ;
#134492 = EDGE_LOOP ( 'NONE', ( #138169, #140470, #226592, #204986 ) ) ;
#134493 = DIRECTION ( 'NONE',  ( 0.000000000000000000, -6.982962677686266711E-15, 1.000000000000000000 ) ) ;
#134494 = CARTESIAN_POINT ( 'NONE',  ( 21.14999999999999858, 10.71339244341104013, -146.2500000000000284 ) ) ;
#134495 = VECTOR ( 'NONE', #215882, 1000.000000000000000 ) ;
#134497 = ORIENTED_EDGE ( 'NONE', *, *, #201590, .F. ) ;
#134496 = ORIENTED_EDGE ( 'NONE', *, *, #73536, .T. ) ;
#134498 = ORIENTED_EDGE ( 'NONE', *, *, #216957, .F. ) ;
#134499 = DIRECTION ( 'NONE',  ( 1.000000000000000000, 0.000000000000000000, 0.000000000000000000 ) ) ;
#134500 = EDGE_LOOP ( 'NONE', ( #11360, #161898, #10186, #154341 ) ) ;
#134501 = EDGE_LOOP ( 'NONE', ( #50432, #26682, #94245, #256180 ) ) ;
#134502 = CARTESIAN_POINT ( 'NONE',  ( 21.14999999999999858, 6.650000000011155876, -112.6500000000000341 ) ) ;
#134503 = ORIENTED_EDGE ( 'NONE', *, *, #15609, .T. ) ;
#134504 = DIRECTION ( 'NONE',  ( -1.000000000000000000, 0.000000000000000000, -0.000000000000000000 ) ) ;
#134505 = TOROIDAL_SURFACE ( 'NONE', #138583, 0.2000000000000000111, 0.1000000000000000056 ) ;
#134506 = LINE ( 'NONE', #40606, #44300 ) ;
#134508 = ORIENTED_EDGE ( 'NONE', *, *, #42912, .F. ) ;
#134507 = AXIS2_PLACEMENT_3D ( 'NONE', #78917, #123214, #243154 ) ;
#134509 = ORIENTED_EDGE ( 'NONE', *, *, #205952, .F. ) ;
#134510 = CIRCLE ( 'NONE', #251036, 0.1000000000000052097 ) ;
#134512 = EDGE_CURVE ( 'NONE', #166015, #117026, #180069, .T. ) ;
#134511 = CARTESIAN_POINT ( 'NONE',  ( 18.50000000000000000, -9.499999999988842703, -107.5320693966997112 ) ) ;
#134513 = ORIENTED_EDGE ( 'NONE', *, *, #62653, .F. ) ;
#134514 = EDGE_CURVE ( 'NONE', #239889, #26637, #177163, .T. ) ;
#134515 = VECTOR ( 'NONE', #179733, 1000.000000000000000 ) ;
#134516 = VECTOR ( 'NONE', #81101, 1000.000000000000000 ) ;
#134517 = VECTOR ( 'NONE', #123237, 1000.000000000000114 ) ;
#134518 = AXIS2_PLACEMENT_3D ( 'NONE', #128230, #89089, #167379 ) ;
#134519 = DIRECTION ( 'NONE',  ( 0.000000000000000000, -0.000000000000000000, -1.000000000000000000 ) ) ;
#134520 = ORIENTED_EDGE ( 'NONE', *, *, #121240, .T. ) ;
#134521 = ORIENTED_EDGE ( 'NONE', *, *, #57040, .T. ) ;
#134522 = CARTESIAN_POINT ( 'NONE',  ( -23.25000000000000000, 80.82423061532404063, -192.8091306798888525 ) ) ;
#134524 = ORIENTED_EDGE ( 'NONE', *, *, #134213, .F. ) ;
#134523 = CARTESIAN_POINT ( 'NONE',  ( 18.45036689428336629, 85.49018414334112492, -163.0104116570379915 ) ) ;
#134525 = DIRECTION ( 'NONE',  ( -1.000000000000000000, 2.952720810173289112E-16, 2.061873921506763405E-30 ) ) ;
#134526 = DIRECTION ( 'NONE',  ( 0.000000000000000000, -7.056502275159890832E-15, 1.000000000000000000 ) ) ;
#134527 = CARTESIAN_POINT ( 'NONE',  ( -22.39999999999999858, 64.35000000001214460, -136.6231074845243825 ) ) ;
#134528 = CARTESIAN_POINT ( 'NONE',  ( -20.94999999999999929, 44.06843597547145208, -258.9974126733344519 ) ) ;
#134529 = CARTESIAN_POINT ( 'NONE',  ( -23.15000000000000213, 76.00000000001267608, -203.5231074845243597 ) ) ;
#134530 = DIRECTION ( 'NONE',  ( 0.000000000000000000, 0.000000000000000000, 1.000000000000000000 ) ) ;
#134531 = CARTESIAN_POINT ( 'NONE',  ( 21.05933563467872105, 65.27547528793097342, -157.8294597355684630 ) ) ;
#134532 = CARTESIAN_POINT ( 'NONE',  ( -16.77683809663752257, 66.05416425680809311, -149.1870565036286109 ) ) ;
#134533 = CARTESIAN_POINT ( 'NONE',  ( 22.42196299218230493, 75.99755832602491523, -148.1727191871737830 ) ) ;
#134534 = CARTESIAN_POINT ( 'NONE',  ( 23.14999999999999503, 23.42819724844704155, -229.2476443247244902 ) ) ;
#134535 = EDGE_CURVE ( 'NONE', #204996, #24660, #151033, .T. ) ;
#134536 = VECTOR ( 'NONE', #228121, 1000.000000000000000 ) ;
#134538 = ORIENTED_EDGE ( 'NONE', *, *, #96442, .T. ) ;
#134537 = CIRCLE ( 'NONE', #22155, 0.09999999999999939493 ) ;
#134539 = AXIS2_PLACEMENT_3D ( 'NONE', #175537, #33479, #152123 ) ;
#134540 = AXIS2_PLACEMENT_3D ( 'NONE', #249012, #49514, #131607 ) ;
#134542 = VERTEX_POINT ( 'NONE', #40216 ) ;
#134541 = EDGE_LOOP ( 'NONE', ( #200621, #211275, #83483, #168685 ) ) ;
#134543 = EDGE_LOOP ( 'NONE', ( #80786, #24439, #21087, #553 ) ) ;
#134544 = FACE_OUTER_BOUND ( 'NONE', #47012, .T. ) ;
#134545 = CARTESIAN_POINT ( 'NONE',  ( -18.59999999999999787, -1.162701749926853712, -108.6000000000000227 ) ) ;
#134547 = FACE_OUTER_BOUND ( 'NONE', #11735, .T. ) ;
#134546 = CARTESIAN_POINT ( 'NONE',  ( 18.59999999999999076, -1.835859311443637010, -45.00443916879852679 ) ) ;
#134548 = ORIENTED_EDGE ( 'NONE', *, *, #66326, .T. ) ;
#134549 = VERTEX_POINT ( 'NONE', #140555 ) ;
#134550 = CARTESIAN_POINT ( 'NONE',  ( 23.14999999999999503, 11.65000000001116298, -21.75000000000000355 ) ) ;
#134551 = LINE ( 'NONE', #15945, #20937 ) ;
#134552 = LINE ( 'NONE', #92868, #72250 ) ;
#134553 = DIRECTION ( 'NONE',  ( 0.000000000000000000, -1.000000000000000000, 0.000000000000000000 ) ) ;
#134554 = ORIENTED_EDGE ( 'NONE', *, *, #20944, .T. ) ;
#134555 = ORIENTED_EDGE ( 'NONE', *, *, #23851, .F. ) ;
#134556 = DIRECTION ( 'NONE',  ( 0.000000000000000000, -0.1686199900910857752, 0.9856811345164735449 ) ) ;
#134557 = CARTESIAN_POINT ( 'NONE',  ( -21.05000000000000071, 75.90220970870363715, -176.2809220950004487 ) ) ;
#134558 = AXIS2_PLACEMENT_3D ( 'NONE', #102270, #82708, #226078 ) ;
#134559 = ORIENTED_EDGE ( 'NONE', *, *, #33269, .T. ) ;
#134560 = FACE_OUTER_BOUND ( 'NONE', #111054, .T. ) ;
#134562 = ORIENTED_EDGE ( 'NONE', *, *, #76155, .T. ) ;
#134561 = DIRECTION ( 'NONE',  ( 0.000000000000000000, 0.000000000000000000, 1.000000000000000000 ) ) ;
#134563 = DIRECTION ( 'NONE',  ( 1.000000000000000000, 0.000000000000000000, 0.000000000000000000 ) ) ;
#134564 = CARTESIAN_POINT ( 'NONE',  ( 21.13736287352038445, 19.08223167578460533, -231.0074083443886366 ) ) ;
#134565 = FACE_OUTER_BOUND ( 'NONE', #147516, .T. ) ;
#134566 = ORIENTED_EDGE ( 'NONE', *, *, #10949, .F. ) ;
#134567 = CARTESIAN_POINT ( 'NONE',  ( -21.05000000000000071, 5.850000000011105428, -110.6324972242780120 ) ) ;
#134569 = EDGE_CURVE ( 'NONE', #76393, #91770, #199269, .T. ) ;
#134568 = FACE_OUTER_BOUND ( 'NONE', #113057, .T. ) ;
#134570 = LINE ( 'NONE', #13371, #86051 ) ;
#134572 = CARTESIAN_POINT ( 'NONE',  ( -20.94999999999999929, 47.95459712139159336, -246.5019368548292675 ) ) ;
#134571 = LINE ( 'NONE', #15965, #249242 ) ;
#134573 = CARTESIAN_POINT ( 'NONE',  ( 23.25000000000000000, -11.88052908492543480, -191.5620167057819287 ) ) ;
#134574 = EDGE_CURVE ( 'NONE', #182833, #71184, #57154, .T. ) ;
#134575 = CARTESIAN_POINT ( 'NONE',  ( -16.89268316805465986, 9.951721813253337601, -121.3557524785455826 ) ) ;
#134576 = CARTESIAN_POINT ( 'NONE',  ( 18.39999999999999858, 85.68240343348880117, -163.3662641071115047 ) ) ;
#134577 = DIRECTION ( 'NONE',  ( 0.000000000000000000, -6.982962677686266711E-15, 1.000000000000000000 ) ) ;
#134578 = AXIS2_PLACEMENT_3D ( 'NONE', #26707, #205299, #207911 ) ;
#134579 = ORIENTED_EDGE ( 'NONE', *, *, #237754, .F. ) ;
#134580 = AXIS2_PLACEMENT_3D ( 'NONE', #156542, #152689, #236037 ) ;
#134581 = VERTEX_POINT ( 'NONE', #257894 ) ;
#134582 = EDGE_CURVE ( 'NONE', #22326, #161169, #152109, .T. ) ;
#134583 = DIRECTION ( 'NONE',  ( 0.8049926720990051576, 0.5932847527679298016, -0.000000000000000000 ) ) ;
#134584 = VERTEX_POINT ( 'NONE', #238379 ) ;
#134585 = EDGE_CURVE ( 'NONE', #112680, #224378, #100901, .T. ) ;
#134586 = FACE_OUTER_BOUND ( 'NONE', #230931, .T. ) ;
#134587 = VERTEX_POINT ( 'NONE', #194151 ) ;
#134588 = AXIS2_PLACEMENT_3D ( 'NONE', #40753, #17317, #78543 ) ;
#134589 = ADVANCED_FACE ( 'NONE', ( #98835 ), #159232, .T. ) ;
#134590 = ORIENTED_EDGE ( 'NONE', *, *, #181399, .F. ) ;
#134591 = CARTESIAN_POINT ( 'NONE',  ( 22.00356870068118553, 65.33245486358892151, -242.8564489551373811 ) ) ;
#134592 = EDGE_LOOP ( 'NONE', ( #60549, #40040, #78024, #95861 ) ) ;
#134593 = AXIS2_PLACEMENT_3D ( 'NONE', #232912, #178066, #155944 ) ;
#134594 = CARTESIAN_POINT ( 'NONE',  ( 18.52130828395272033, -7.769407441232962341, -209.8812647411876071 ) ) ;
#134595 = CARTESIAN_POINT ( 'NONE',  ( -20.94999999999999929, 87.65000000001191438, -103.0231074845242176 ) ) ;
#134596 = DIRECTION ( 'NONE',  ( 1.000000000000000000, -0.000000000000000000, 0.000000000000000000 ) ) ;
#134597 = AXIS2_PLACEMENT_3D ( 'NONE', #55878, #172046, #254093 ) ;
#134598 = LINE ( 'NONE', #77205, #249557 ) ;
#134600 = ORIENTED_EDGE ( 'NONE', *, *, #146748, .T. ) ;
#134599 = DIRECTION ( 'NONE',  ( 0.000000000000000000, 0.000000000000000000, 1.000000000000000000 ) ) ;
#134602 = CARTESIAN_POINT ( 'NONE',  ( 19.87657994471988587, 11.75000000001115019, -192.2657881246250042 ) ) ;
#134601 = CARTESIAN_POINT ( 'NONE',  ( -20.64999999999999858, -9.000000000000003553, -9.893969122652444881 ) ) ;
#134603 = EDGE_CURVE ( 'NONE', #221804, #120003, #55868, .T. ) ;
#134604 = CARTESIAN_POINT ( 'NONE',  ( -17.05016517656120811, 9.949999999999983302, -20.82730200400101239 ) ) ;
#134605 = LINE ( 'NONE', #235024, #119077 ) ;
#134606 = CARTESIAN_POINT ( 'NONE',  ( -12.24999999999999289, 9.350000000011130297, -117.0185689574026213 ) ) ;
#134607 = CARTESIAN_POINT ( 'NONE',  ( -21.14999999999999503, 11.75000000001115197, -40.41914724595876862 ) ) ;
#134608 = ORIENTED_EDGE ( 'NONE', *, *, #143887, .F. ) ;
#134609 = AXIS2_PLACEMENT_3D ( 'NONE', #4959, #178526, #158964 ) ;
#134610 = SHAPE_REPRESENTATION_RELATIONSHIP ( 'NONE' , 'NONE' ,  #61981, #29580 ) ;
#134612 = FACE_OUTER_BOUND ( 'NONE', #224005, .T. ) ;
#134611 = VECTOR ( 'NONE', #170141, 1000.000000000000000 ) ;
#134613 = CIRCLE ( 'NONE', #38784, 11.69999999999998863 ) ;
#134614 = ORIENTED_EDGE ( 'NONE', *, *, #6187, .F. ) ;
#134615 = PLANE ( 'NONE',  #193912 ) ;
#134616 = ORIENTED_EDGE ( 'NONE', *, *, #81305, .T. ) ;
#134617 = CARTESIAN_POINT ( 'NONE',  ( -22.50000000000000000, 67.23127455305841238, -235.8551265064783991 ) ) ;
#134618 = AXIS2_PLACEMENT_3D ( 'NONE', #117898, #119204, #198726 ) ;
#134619 = FACE_OUTER_BOUND ( 'NONE', #185140, .T. ) ;
#134620 = ORIENTED_EDGE ( 'NONE', *, *, #202244, .T. ) ;
#134621 = ORIENTED_EDGE ( 'NONE', *, *, #220763, .F. ) ;
#134622 = AXIS2_PLACEMENT_3D ( 'NONE', #29188, #89105, #49984 ) ;
#134623 = VECTOR ( 'NONE', #177476, 1000.000000000000000 ) ;
#134624 = VECTOR ( 'NONE', #148173, 1000.000000000000000 ) ;
#134625 = CIRCLE ( 'NONE', #26339, 11.80000000000000959 ) ;
#134626 = DIRECTION ( 'NONE',  ( 0.000000000000000000, 1.000000000000000000, 6.982962677686267499E-15 ) ) ;
#134627 = DIRECTION ( 'NONE',  ( 0.000000000000000000, -0.5000000000000078826, -0.8660254037844340447 ) ) ;
#134628 = CARTESIAN_POINT ( 'NONE',  ( -16.92973740335347443, 66.00749618554451104, -90.42916651972677755 ) ) ;
#134630 = DIRECTION ( 'NONE',  ( 0.000000000000000000, -0.9651348961777157509, 0.2617529984165031243 ) ) ;
#134629 = CARTESIAN_POINT ( 'NONE',  ( -21.00023020733502932, 76.00000000001219291, -142.9139767297926369 ) ) ;
#134631 = CYLINDRICAL_SURFACE ( 'NONE', #195031, 0.5000000000000004441 ) ;
#134632 = CYLINDRICAL_SURFACE ( 'NONE', #235086, 12.87499999999999822 ) ;
#134633 = CARTESIAN_POINT ( 'NONE',  ( 21.05000000000000071, 30.73075574124490217, -252.3164853687435709 ) ) ;
#134634 = ORIENTED_EDGE ( 'NONE', *, *, #36201, .F. ) ;
#134635 = LINE ( 'NONE', #34308, #198103 ) ;
#134636 = EDGE_CURVE ( 'NONE', #65554, #187942, #88450, .T. ) ;
#134638 = VERTEX_POINT ( 'NONE', #96288 ) ;
#134637 = DIRECTION ( 'NONE',  ( 0.000000000000000000, -1.000000000000000000, -0.000000000000000000 ) ) ;
#134639 = LINE ( 'NONE', #235061, #47749 ) ;
#134640 = CARTESIAN_POINT ( 'NONE',  ( 18.49999999999999289, 10.29270135741298731, -206.4573618871519045 ) ) ;
#134642 = DIRECTION ( 'NONE',  ( -1.000000000000000000, 0.000000000000000000, 0.000000000000000000 ) ) ;
#134641 = FACE_OUTER_BOUND ( 'NONE', #158270, .T. ) ;
#134644 = ORIENTED_EDGE ( 'NONE', *, *, #60463, .T. ) ;
#134643 = CARTESIAN_POINT ( 'NONE',  ( -21.05000000000000071, 74.73821383144760944, -195.4366085209788935 ) ) ;
#134645 = DIRECTION ( 'NONE',  ( 0.000000000000000000, 0.000000000000000000, 1.000000000000000000 ) ) ;
#134646 = DIRECTION ( 'NONE',  ( -1.000000000000000000, 0.000000000000000000, -0.000000000000000000 ) ) ;
#134647 = CARTESIAN_POINT ( 'NONE',  ( 18.59999999999999787, -9.849999999999994316, 30.09999999999999787 ) ) ;
#134649 = EDGE_CURVE ( 'NONE', #111962, #106794, #175869, .T. ) ;
#134648 = CARTESIAN_POINT ( 'NONE',  ( -20.94999999999999929, 18.14639373905162145, -237.6648341169113792 ) ) ;
#134650 = ORIENTED_EDGE ( 'NONE', *, *, #193610, .T. ) ;
#134651 = DIRECTION ( 'NONE',  ( 1.000000000000000000, 2.885090398161910739E-16, 6.283419270304611573E-17 ) ) ;
#134652 = ORIENTED_EDGE ( 'NONE', *, *, #124131, .T. ) ;
#134653 = AXIS2_PLACEMENT_3D ( 'NONE', #125406, #167124, #142386 ) ;
#134654 = EDGE_CURVE ( 'NONE', #113056, #236459, #163495, .T. ) ;
#134655 = ADVANCED_FACE ( 'NONE', ( #106552, #121040 ), #4875, .T. ) ;
#134656 = AXIS2_PLACEMENT_3D ( 'NONE', #54734, #114718, #90003 ) ;
#134657 = DIRECTION ( 'NONE',  ( 0.000000000000000000, 0.000000000000000000, 1.000000000000000000 ) ) ;
#134658 = VERTEX_POINT ( 'NONE', #183553 ) ;
#134659 = FACE_OUTER_BOUND ( 'NONE', #235066, .T. ) ;
#134660 = TOROIDAL_SURFACE ( 'NONE', #135233, 4.149999999999999467, 0.1000000000000000056 ) ;
#134661 = ORIENTED_EDGE ( 'NONE', *, *, #99862, .F. ) ;
#134662 = DIRECTION ( 'NONE',  ( 0.000000000000000000, 0.9651348961777148627, -0.2617529984165062329 ) ) ;
#134663 = CYLINDRICAL_SURFACE ( 'NONE', #229200, 0.5000000000000004441 ) ;
#134664 = AXIS2_PLACEMENT_3D ( 'NONE', #183248, #185806, #48861 ) ;
#134665 = AXIS2_PLACEMENT_3D ( 'NONE', #131673, #15615, #52122 ) ;
#134666 = FACE_OUTER_BOUND ( 'NONE', #35949, .T. ) ;
#134667 = ORIENTED_EDGE ( 'NONE', *, *, #218316, .F. ) ;
#134668 = ADVANCED_FACE ( 'NONE', ( #123576 ), #203105, .F. ) ;
#134669 =( BOUNDED_SURFACE ( )  B_SPLINE_SURFACE ( 3, 2, ( 
 ( #256025, #113994, #94434 ),
 ( #52737, #215654, #76151 ),
 ( #112727, #196120, #214387 ),
 ( #253504, #96966, #192276 ),
 ( #56563, #194853, #95713 ),
 ( #74912, #77422, #136103 ) ),
 .UNSPECIFIED., .F., .F., .F. ) 
 B_SPLINE_SURFACE_WITH_KNOTS ( ( 4, 2, 4 ),
 ( 3, 3 ),
 ( 0.0001300404313046550988, 0.0003183318589266533115, 0.0005066232865486515512 ),
 ( 0.000000000000000000, 1.000000000000000000 ),
 .UNSPECIFIED. ) 
 GEOMETRIC_REPRESENTATION_ITEM ( )  RATIONAL_B_SPLINE_SURFACE ( (
 ( 1.000000000000000000, 0.7071067811865597852, 1.000000000000000000),
 ( 1.000000000000000000, 0.7625113560543042013, 1.000000000000000000),
 ( 1.000000000000000000, 0.8126073484684787074, 1.000000000000000000),
 ( 1.000000000000000000, 0.8923049332736151529, 1.000000000000000000),
 ( 1.000000000000000000, 0.9231914937766685370, 1.000000000000000000),
 ( 1.000000000000000000, 0.9238795325112900692, 1.000000000000000000) ) ) 
 REPRESENTATION_ITEM ( '' )  SURFACE ( )  );
#134670 = AXIS2_PLACEMENT_3D ( 'NONE', #34961, #37504, #233152 ) ;
#134671 = EDGE_CURVE ( 'NONE', #172794, #108629, #175997, .T. ) ;
#134672 = CARTESIAN_POINT ( 'NONE',  ( -16.88705144915409306, 9.949999999999983302, -12.93097859471232525 ) ) ;
#134674 = AXIS2_PLACEMENT_3D ( 'NONE', #78666, #198624, #143782 ) ;
#134673 = CARTESIAN_POINT ( 'NONE',  ( -23.25000000000000000, 71.65000000001151648, -48.37310748452435405 ) ) ;
#134675 = CYLINDRICAL_SURFACE ( 'NONE', #54070, 0.09999999999999939493 ) ;
#134676 = AXIS2_PLACEMENT_3D ( 'NONE', #220510, #177561, #21037 ) ;
#134677 = AXIS2_PLACEMENT_3D ( 'NONE', #59921, #199478, #178643 ) ;
#134678 = CARTESIAN_POINT ( 'NONE',  ( 12.93279065517211812, 9.417690691063100417, -18.14160069676457709 ) ) ;
#134679 = CIRCLE ( 'NONE', #34967, 0.1000000000000028644 ) ;
#134680 = CARTESIAN_POINT ( 'NONE',  ( 23.24999999999999645, 50.88295650978584206, -230.3037755757580953 ) ) ;
#134681 = ORIENTED_EDGE ( 'NONE', *, *, #105477, .F. ) ;
#134682 = CARTESIAN_POINT ( 'NONE',  ( -18.39999999999999858, 85.68240343348850274, -129.8662641071115047 ) ) ;
#134683 = EDGE_LOOP ( 'NONE', ( #22989, #200841, #108242, #75803 ) ) ;
#134685 = VERTEX_POINT ( 'NONE', #103979 ) ;
#134684 = CARTESIAN_POINT ( 'NONE',  ( -16.98495255085916611, 65.99443563401746360, -149.1577246907449137 ) ) ;
#134686 = VECTOR ( 'NONE', #43692, 1000.000000000000000 ) ;
#134687 = EDGE_LOOP ( 'NONE', ( #8021, #214989, #101889, #126480 ) ) ;
#134688 = CARTESIAN_POINT ( 'NONE',  ( 22.47007471830798053, 1.116269474027924959E-11, -59.27928934807359695 ) ) ;
#134689 = DIRECTION ( 'NONE',  ( 1.000000000000000000, -0.000000000000000000, -0.000000000000000000 ) ) ;
#134690 = DIRECTION ( 'NONE',  ( 0.000000000000000000, 0.000000000000000000, -1.000000000000000000 ) ) ;
#134691 = ADVANCED_FACE ( 'NONE', ( #2323 ), #96821, .T. ) ;
#134692 = DIRECTION ( 'NONE',  ( 0.000000000000000000, -1.000000000000000000, 0.000000000000000000 ) ) ;
#134693 = ORIENTED_EDGE ( 'NONE', *, *, #204088, .T. ) ;
#134694 = EDGE_CURVE ( 'NONE', #71034, #53701, #38587, .T. ) ;
#134695 = ADVANCED_FACE ( 'NONE', ( #144387 ), #67442, .F. ) ;
#134697 = DIRECTION ( 'NONE',  ( 1.000000000000000000, 0.000000000000000000, 0.000000000000000000 ) ) ;
#134696 = CIRCLE ( 'NONE', #9627, 0.09999999999999939493 ) ;
#134698 = VERTEX_POINT ( 'NONE', #122294 ) ;
#134700 = ORIENTED_EDGE ( 'NONE', *, *, #233119, .F. ) ;
#134699 = DIRECTION ( 'NONE',  ( -1.000000000000000000, 0.000000000000000000, -0.000000000000000000 ) ) ;
#134701 = CARTESIAN_POINT ( 'NONE',  ( 23.15000000000000213, 86.52890073500824997, -209.5906233940697234 ) ) ;
#134702 = CYLINDRICAL_SURFACE ( 'NONE', #135629, 0.09999999999999939493 ) ;
#134703 = DIRECTION ( 'NONE',  ( -1.836970198721029934E-16, 1.000000000000000000, 0.000000000000000000 ) ) ;
#134704 = VERTEX_POINT ( 'NONE', #85686 ) ;
#134705 = CIRCLE ( 'NONE', #126534, 12.87499999999999822 ) ;
#134706 = VERTEX_POINT ( 'NONE', #166579 ) ;
#134707 =( BOUNDED_SURFACE ( )  B_SPLINE_SURFACE ( 3, 2, ( 
 ( #251109, #72513, #52925 ),
 ( #172928, #114186, #174210 ),
 ( #220688, #86277, #124165 ),
 ( #45895, #121613, #84986 ),
 ( #164572, #160743, #244086 ),
 ( #42064, #6767, #65451 ),
 ( #44620, #202403, #142421 ),
 ( #201118, #47153, #144977 ),
 ( #143704, #125443, #105842 ),
 ( #224526, #242803, #23799 ) ),
 .UNSPECIFIED., .F., .F., .F. ) 
 B_SPLINE_SURFACE_WITH_KNOTS ( ( 4, 2, 2, 2, 4 ),
 ( 3, 3 ),
 ( 0.002161241639767785133, 0.002579950749617447234, 0.002789305304542278284, 0.002893982582004694243, 0.002998659859467109768 ),
 ( 0.000000000000000000, 1.000000000000000000 ),
 .UNSPECIFIED. ) 
 GEOMETRIC_REPRESENTATION_ITEM ( )  RATIONAL_B_SPLINE_SURFACE ( (
 ( 1.000000000000000000, 0.7071067811864923947, 1.000000000000000000),
 ( 1.000000000000000000, 0.7632447400664384984, 1.000000000000000000),
 ( 1.000000000000000000, 0.8158073005108742448, 1.000000000000000000),
 ( 1.000000000000000000, 0.8906973462396178265, 1.000000000000000000),
 ( 1.000000000000000000, 0.9149408947802152303, 1.000000000000000000),
 ( 1.000000000000000000, 0.9493368785274697297, 1.000000000000000000),
 ( 1.000000000000000000, 0.9605194247157555765, 1.000000000000000000),
 ( 1.000000000000000000, 0.9803630264780319736, 1.000000000000000000),
 ( 1.000000000000000000, 0.9900844824271819444, 1.000000000000000000),
 ( 1.000000000000000000, 0.9894588281429244070, 1.000000000000000000) ) ) 
 REPRESENTATION_ITEM ( '' )  SURFACE ( )  );
#134708 = AXIS2_PLACEMENT_3D ( 'NONE', #18988, #158538, #170761 ) ;
#134709 = VECTOR ( 'NONE', #890, 1000.000000000000000 ) ;
#134710 = DIRECTION ( 'NONE',  ( 0.000000000000000000, 0.000000000000000000, -1.000000000000000000 ) ) ;
#134711 = VERTEX_POINT ( 'NONE', #45319 ) ;
#134712 = DIRECTION ( 'NONE',  ( 1.000000000000000000, 0.000000000000000000, 0.000000000000000000 ) ) ;
#134713 = EDGE_CURVE ( 'NONE', #23868, #210308, #101068, .T. ) ;
#134714 = EDGE_CURVE ( 'NONE', #177651, #116965, #246099, .T. ) ;
#134715 = CARTESIAN_POINT ( 'NONE',  ( 12.33938619321247465, 66.63927620602551372, -52.20918028991769688 ) ) ;
#134716 = DIRECTION ( 'NONE',  ( -0.000000000000000000, -0.1298341882519805091, -0.9915357197604881545 ) ) ;
#134717 = EDGE_CURVE ( 'NONE', #33150, #92669, #102695, .T. ) ;
#134718 = TOROIDAL_SURFACE ( 'NONE', #63831, 2.100000000000002309, 0.1000000000000000056 ) ;
#134719 = AXIS2_PLACEMENT_3D ( 'NONE', #249867, #67380, #71254 ) ;
#134720 = CIRCLE ( 'NONE', #247148, 2.000000000000001776 ) ;
#134721 = VECTOR ( 'NONE', #182305, 1000.000000000000000 ) ;
#134722 = ORIENTED_EDGE ( 'NONE', *, *, #52700, .T. ) ;
#134723 = CARTESIAN_POINT ( 'NONE',  ( -18.39999999999999858, 64.52683809664961245, -127.1971614177164156 ) ) ;
#134724 = ORIENTED_EDGE ( 'NONE', *, *, #83007, .T. ) ;
#134725 = DIRECTION ( 'NONE',  ( 1.000000000000000000, -0.000000000000000000, -0.000000000000000000 ) ) ;
#134726 = CARTESIAN_POINT ( 'NONE',  ( -18.59999999999999787, 77.25000000001263345, -195.5231074845243313 ) ) ;
#134728 = ORIENTED_EDGE ( 'NONE', *, *, #229633, .F. ) ;
#134727 = DIRECTION ( 'NONE',  ( 1.000000000000000000, 0.000000000000000000, 0.000000000000000000 ) ) ;
#134729 = LINE ( 'NONE', #229997, #24393 ) ;
#134730 = CARTESIAN_POINT ( 'NONE',  ( 20.99999999999999645, 12.21861431488691707, -211.2854491503459826 ) ) ;
#134731 = CARTESIAN_POINT ( 'NONE',  ( -20.90000000000000213, -1.300000000000000044, -7.800000000000000711 ) ) ;
#134732 = CARTESIAN_POINT ( 'NONE',  ( -16.92989507731676113, 9.949999999999983302, -20.61749893061018923 ) ) ;
#134733 = CARTESIAN_POINT ( 'NONE',  ( 18.49999999999999289, 33.98796489282361932, -236.2185561567993091 ) ) ;
#134734 = EDGE_CURVE ( 'NONE', #62992, #167556, #222652, .T. ) ;
#134735 = DIRECTION ( 'NONE',  ( 1.000000000000000000, 0.000000000000000000, 0.000000000000000000 ) ) ;
#134736 = CARTESIAN_POINT ( 'NONE',  ( -20.94999999999999929, 1.162701749949165642, -41.50000000000000000 ) ) ;
#134738 = VERTEX_POINT ( 'NONE', #21916 ) ;
#134737 = DIRECTION ( 'NONE',  ( -1.000000000000000000, -0.000000000000000000, -0.000000000000000000 ) ) ;
#134739 = EDGE_CURVE ( 'NONE', #33150, #117589, #246869, .T. ) ;
#134740 = EDGE_CURVE ( 'NONE', #141829, #244695, #42883, .T. ) ;
#134741 = EDGE_CURVE ( 'NONE', #109797, #187747, #180992, .T. ) ;
#134742 = DIRECTION ( 'NONE',  ( -0.000000000000000000, 0.01283462868039629209, -0.9999176327611372095 ) ) ;
#134743 = DIRECTION ( 'NONE',  ( 1.000000000000000000, 0.000000000000000000, 0.000000000000000000 ) ) ;
#134744 = EDGE_LOOP ( 'NONE', ( #135506, #179959, #140318, #96334 ) ) ;
#134745 = LINE ( 'NONE', #53944, #137388 ) ;
#134746 = CARTESIAN_POINT ( 'NONE',  ( -23.15000000000000213, 1.115600667400684642E-11, -67.00000000000000000 ) ) ;
#134747 = CARTESIAN_POINT ( 'NONE',  ( -18.59999999999999787, 64.25000000001203659, -114.7731074845243882 ) ) ;
#134748 = EDGE_LOOP ( 'NONE', ( #72008, #7276, #22561, #76024 ) ) ;
#134749 = AXIS2_PLACEMENT_3D ( 'NONE', #233869, #250847, #211750 ) ;
#134751 = EDGE_CURVE ( 'NONE', #146536, #157096, #7469, .T. ) ;
#134750 = DIRECTION ( 'NONE',  ( 1.000000000000000000, -0.000000000000000000, -0.000000000000000000 ) ) ;
#134752 = CIRCLE ( 'NONE', #151565, 0.09999999999998898659 ) ;
#134753 = EDGE_CURVE ( 'NONE', #201487, #167224, #46943, .T. ) ;
#134754 = AXIS2_PLACEMENT_3D ( 'NONE', #127195, #84148, #171183 ) ;
#134755 = CARTESIAN_POINT ( 'NONE',  ( 21.14999999999999503, -0.1008583690875562017, -21.75043287651061164 ) ) ;
#134756 = VERTEX_POINT ( 'NONE', #170453 ) ;
#134757 = CARTESIAN_POINT ( 'NONE',  ( -23.25000000000000000, 74.00000000001199396, -116.2477294072864140 ) ) ;
#134758 = ORIENTED_EDGE ( 'NONE', *, *, #58773, .T. ) ;
#134759 = EDGE_CURVE ( 'NONE', #31326, #144794, #220448, .T. ) ;
#134760 = CARTESIAN_POINT ( 'NONE',  ( 21.07928932188134397, 76.00000000001165290, -69.52310748452431710 ) ) ;
#134761 = ORIENTED_EDGE ( 'NONE', *, *, #42597, .T. ) ;
#134762 = FACE_OUTER_BOUND ( 'NONE', #119853, .T. ) ;
#134763 = EDGE_LOOP ( 'NONE', ( #195563, #221757, #164714, #252753 ) ) ;
#134764 = CARTESIAN_POINT ( 'NONE',  ( 20.94999999999999929, 64.23744694032048130, -224.5446448091673233 ) ) ;
#134765 = ORIENTED_EDGE ( 'NONE', *, *, #350, .T. ) ;
#134767 = ORIENTED_EDGE ( 'NONE', *, *, #238745, .F. ) ;
#134766 = ORIENTED_EDGE ( 'NONE', *, *, #80919, .F. ) ;
#134769 = CARTESIAN_POINT ( 'NONE',  ( -20.94999999999999929, 87.65000000001192859, -105.9231074845242091 ) ) ;
#134768 = VECTOR ( 'NONE', #128328, 1000.000000000000000 ) ;
#134771 = VERTEX_POINT ( 'NONE', #53009 ) ;
#134770 = DIRECTION ( 'NONE',  ( 1.000000000000000000, -1.145314911736513664E-16, 3.106193895438251016E-17 ) ) ;
#134772 = EDGE_CURVE ( 'NONE', #118409, #82068, #38783, .T. ) ;
#134773 = CARTESIAN_POINT ( 'NONE',  ( 20.94999999999999929, 34.98408343502854478, -248.6539962344157004 ) ) ;
#134774 = ORIENTED_EDGE ( 'NONE', *, *, #196590, .F. ) ;
#134775 = VECTOR ( 'NONE', #109725, 1000.000000000000000 ) ;
#134776 = VECTOR ( 'NONE', #21105, 1000.000000000000114 ) ;
#134777 = AXIS2_PLACEMENT_3D ( 'NONE', #230714, #225535, #149902 ) ;
#134778 = EDGE_CURVE ( 'NONE', #102643, #6436, #192725, .T. ) ;
#134779 = VERTEX_POINT ( 'NONE', #51704 ) ;
#134780 = DIRECTION ( 'NONE',  ( 1.000000000000000000, 0.000000000000000000, 0.000000000000000000 ) ) ;
#134781 = CARTESIAN_POINT ( 'NONE',  ( 21.78635804494511419, 75.90099493450402690, -76.55876896967750156 ) ) ;
#134782 = CARTESIAN_POINT ( 'NONE',  ( 21.05000000000000071, 8.826429739517195117, -8.414054712943700665 ) ) ;
#134783 = ORIENTED_EDGE ( 'NONE', *, *, #82000, .T. ) ;
#134784 = FACE_OUTER_BOUND ( 'NONE', #246163, .T. ) ;
#134785 = CYLINDRICAL_SURFACE ( 'NONE', #81355, 0.09999999999998898659 ) ;
#134786 = ADVANCED_FACE ( 'NONE', ( #189968 ), #187410, .F. ) ;
#134787 = DIRECTION ( 'NONE',  ( -1.000000000000000000, 0.000000000000000000, -0.000000000000000000 ) ) ;
#134788 = AXIS2_PLACEMENT_3D ( 'NONE', #190054, #184912, #85773 ) ;
#134789 = VERTEX_POINT ( 'NONE', #208259 ) ;
#134790 = AXIS2_PLACEMENT_3D ( 'NONE', #178482, #256644, #257932 ) ;
#134791 = CARTESIAN_POINT ( 'NONE',  ( 18.49999999999999645, -1.299733671230788756, 9.971870477130599042 ) ) ;
#134792 = CARTESIAN_POINT ( 'NONE',  ( 23.40000000000005187, 82.84256550613280012, -26.34830530078816935 ) ) ;
#134793 = CIRCLE ( 'NONE', #22417, 0.6000000000000033085 ) ;
#134794 = ORIENTED_EDGE ( 'NONE', *, *, #15980, .F. ) ;
#134795 = DIRECTION ( 'NONE',  ( 1.000000000000000000, 0.000000000000000000, 0.000000000000000000 ) ) ;
#134796 = ORIENTED_EDGE ( 'NONE', *, *, #21057, .F. ) ;
#134797 = ORIENTED_EDGE ( 'NONE', *, *, #238324, .T. ) ;
#134798 = FACE_OUTER_BOUND ( 'NONE', #222311, .T. ) ;
#134800 = ORIENTED_EDGE ( 'NONE', *, *, #191258, .F. ) ;
#134799 = VECTOR ( 'NONE', #6499, 1000.000000000000000 ) ;
#134801 = EDGE_LOOP ( 'NONE', ( #69088, #227141, #139174, #34698 ) ) ;
#134802 = DIRECTION ( 'NONE',  ( 0.000000000000000000, -0.9553114395362780620, -0.2956011730205483912 ) ) ;
#134803 = ADVANCED_FACE ( 'NONE', ( #191278 ), #171718, .T. ) ;
#134804 = CARTESIAN_POINT ( 'NONE',  ( -16.93294127766158752, 10.00328010296601988, -188.4299072658292005 ) ) ;
#134805 = ORIENTED_EDGE ( 'NONE', *, *, #245354, .F. ) ;
#134806 = ORIENTED_EDGE ( 'NONE', *, *, #55475, .F. ) ;
#134807 = CARTESIAN_POINT ( 'NONE',  ( -21.55000000000000071, 21.48591740176965814, -233.0852932139783036 ) ) ;
#134808 = VECTOR ( 'NONE', #133077, 1000.000000000000000 ) ;
#134809 = AXIS2_PLACEMENT_3D ( 'NONE', #25671, #127333, #128625 ) ;
#134810 = CYLINDRICAL_SURFACE ( 'NONE', #243999, 0.1000000000000055705 ) ;
#134811 = CIRCLE ( 'NONE', #76573, 5.000000000000004441 ) ;
#134812 = ORIENTED_EDGE ( 'NONE', *, *, #37249, .F. ) ;
#134813 = ORIENTED_EDGE ( 'NONE', *, *, #42546, .F. ) ;
#134814 = CARTESIAN_POINT ( 'NONE',  ( -18.50000000000000000, -1.736257131586239844, -112.0686523290175245 ) ) ;
#134815 = ADVANCED_FACE ( 'NONE', ( #209525 ), #93417, .T. ) ;
#134816 = CARTESIAN_POINT ( 'NONE',  ( 20.94999999999999929, 1.115600667400684642E-11, -100.5000000000000284 ) ) ;
#134817 = CARTESIAN_POINT ( 'NONE',  ( 23.14999999999999858, 76.00000000001170974, -69.52310748452431710 ) ) ;
#134818 = LINE ( 'NONE', #94425, #122469 ) ;
#134819 = CARTESIAN_POINT ( 'NONE',  ( -18.40000000000000213, 11.75000000001113953, -158.2500000000000284 ) ) ;
#134820 = FACE_OUTER_BOUND ( 'NONE', #216716, .T. ) ;
#134821 = FACE_OUTER_BOUND ( 'NONE', #40698, .T. ) ;
#134822 = AXIS2_PLACEMENT_3D ( 'NONE', #253679, #150748, #93329 ) ;
#134824 = CARTESIAN_POINT ( 'NONE',  ( -19.95857864376268864, 5.488301202077012775, 16.50000000000000000 ) ) ;
#134823 = CARTESIAN_POINT ( 'NONE',  ( -16.86578989773641979, 9.984809801258794693, -12.53533511337776574 ) ) ;
#134825 = DIRECTION ( 'NONE',  ( 0.000000000000000000, 0.000000000000000000, -1.000000000000000000 ) ) ;
#134826 = CARTESIAN_POINT ( 'NONE',  ( -16.77431908686106610, 22.98856962916521240, -230.9454472391804813 ) ) ;
#134827 = VECTOR ( 'NONE', #44958, 1000.000000000000000 ) ;
#134828 = CARTESIAN_POINT ( 'NONE',  ( -23.15000000000000213, 67.23127455305835554, -235.8551265064784559 ) ) ;
#134829 = EDGE_CURVE ( 'NONE', #205763, #171197, #12633, .T. ) ;
#134831 = CARTESIAN_POINT ( 'NONE',  ( 20.94999999999999929, 87.48912529308798014, -106.1231074845242262 ) ) ;
#134830 = CIRCLE ( 'NONE', #226410, 0.1000000000000124678 ) ;
#134832 = ORIENTED_EDGE ( 'NONE', *, *, #65551, .T. ) ;
#134833 = VECTOR ( 'NONE', #146282, 1000.000000000000000 ) ;
#134834 = CIRCLE ( 'NONE', #39227, 0.1000000000000028644 ) ;
#134836 = EDGE_LOOP ( 'NONE', ( #65309, #199298 ) ) ;
#134835 = CARTESIAN_POINT ( 'NONE',  ( 23.14999999999999858, 1.115600667400684642E-11, -134.0000000000000284 ) ) ;
#134837 = CARTESIAN_POINT ( 'NONE',  ( -23.25000000000000000, 84.59626168225496201, -112.4732350016745102 ) ) ;
#134838 = AXIS2_PLACEMENT_3D ( 'NONE', #243380, #7342, #144259 ) ;
#134839 = DIRECTION ( 'NONE',  ( 0.000000000000000000, 0.9915357197604862671, -0.1298341882519953583 ) ) ;
#134840 = ORIENTED_EDGE ( 'NONE', *, *, #89034, .T. ) ;
#134841 = TOROIDAL_SURFACE ( 'NONE', #205795, 0.2000000000000000111, 0.1000000000000000056 ) ;
#134842 = FILL_AREA_STYLE_COLOUR ( '', #64427 ) ;
#134843 = CIRCLE ( 'NONE', #22478, 0.09999999999999938105 ) ;
#134844 = DIRECTION ( 'NONE',  ( 0.000000000000000000, 0.000000000000000000, -1.000000000000000000 ) ) ;
#134845 = AXIS2_PLACEMENT_3D ( 'NONE', #150924, #152235, #229185 ) ;
#134846 = DIRECTION ( 'NONE',  ( -1.000000000000000000, -0.000000000000000000, -0.000000000000000000 ) ) ;
#134847 = ORIENTED_EDGE ( 'NONE', *, *, #58815, .T. ) ;
#134848 = CIRCLE ( 'NONE', #226438, 0.09999999999998898659 ) ;
#134849 = DIRECTION ( 'NONE',  ( 0.000000000000000000, -0.2128009952263645033, 0.9770955615653306170 ) ) ;
#134850 = DIRECTION ( 'NONE',  ( -0.8660254037843277963, 0.000000000000000000, 0.5000000000001921796 ) ) ;
#134851 = CARTESIAN_POINT ( 'NONE',  ( -20.54999999999999716, 71.75000000001259082, -191.2731074845243882 ) ) ;
#134853 = VERTEX_POINT ( 'NONE', #13902 ) ;
#134852 = FACE_OUTER_BOUND ( 'NONE', #11460, .T. ) ;
#134854 = CARTESIAN_POINT ( 'NONE',  ( 23.24999999999999645, 15.91777359887373500, -218.8720307647289474 ) ) ;
#134855 = TOROIDAL_SURFACE ( 'NONE', #22497, 0.2000000000000000111, 0.1000000000000000056 ) ;
#134857 = ORIENTED_EDGE ( 'NONE', *, *, #251910, .F. ) ;
#134856 = DIRECTION ( 'NONE',  ( 1.000000000000000000, -0.000000000000000000, -0.000000000000000000 ) ) ;
#134858 = CARTESIAN_POINT ( 'NONE',  ( 22.50000000000000000, 68.25000000001193712, -103.1231074845243540 ) ) ;
#134859 = SPHERICAL_SURFACE ( 'NONE', #133192, 0.1000000000000000056 ) ;
#134860 = EDGE_CURVE ( 'NONE', #28509, #86605, #205339, .T. ) ;
#134861 = CARTESIAN_POINT ( 'NONE',  ( -22.50000000000000000, 11.48087284840413425, -198.4995883060917947 ) ) ;
#134862 = CARTESIAN_POINT ( 'NONE',  ( 21.97500000000000497, 66.25000000001229239, -157.7731074845244166 ) ) ;
#134863 = AXIS2_PLACEMENT_3D ( 'NONE', #10404, #229444, #251559 ) ;
#134865 = LINE ( 'NONE', #38369, #141108 ) ;
#134864 = CARTESIAN_POINT ( 'NONE',  ( -16.77308656112214891, 9.950000000011138823, -154.8498068082977284 ) ) ;
#134866 = DIRECTION ( 'NONE',  ( 2.557131231893036985E-16, -0.8660254037844383745, 0.5000000000000003331 ) ) ;
#134867 = CARTESIAN_POINT ( 'NONE',  ( -21.03571358705754335, 64.25000000001233502, -163.1980006624665123 ) ) ;
#134868 = DIRECTION ( 'NONE',  ( 0.000000000000000000, 0.8814952561688432775, -0.4721928772777344019 ) ) ;
#134869 = DIRECTION ( 'NONE',  ( 0.000000000000000000, 0.9126074666063813678, 0.4088369013363182813 ) ) ;
#134870 = AXIS2_PLACEMENT_3D ( 'NONE', #165665, #88645, #27462 ) ;
#134872 = ORIENTED_EDGE ( 'NONE', *, *, #23779, .F. ) ;
#134871 = AXIS2_PLACEMENT_3D ( 'NONE', #210486, #206622, #107514 ) ;
#134873 = CARTESIAN_POINT ( 'NONE',  ( -23.25000000000000000, 19.97490019448090948, -235.9060780337186145 ) ) ;
#134874 = CIRCLE ( 'NONE', #101557, 0.09999999999999939493 ) ;
#134875 = ORIENTED_EDGE ( 'NONE', *, *, #82200, .F. ) ;
#134876 = ORIENTED_EDGE ( 'NONE', *, *, #245230, .F. ) ;
#134877 = EDGE_CURVE ( 'NONE', #31357, #200607, #146891, .T. ) ;
#134878 = DIRECTION ( 'NONE',  ( -2.840903330521632762E-16, 0.09425075112713271475, 0.9955484899852801162 ) ) ;
#134879 = PLANE ( 'NONE',  #152719 ) ;
#134880 = EDGE_LOOP ( 'NONE', ( #153036, #131373, #173584, #97973 ) ) ;
#134881 = EDGE_CURVE ( 'NONE', #75563, #67142, #51214, .T. ) ;
#134882 = EDGE_LOOP ( 'NONE', ( #6947, #41280, #219458, #172019 ) ) ;
#134883 = CARTESIAN_POINT ( 'NONE',  ( 20.94999999999999929, 8.876614585098254295, -175.8850804788446567 ) ) ;
#134884 = EDGE_CURVE ( 'NONE', #115886, #227071, #155340, .T. ) ;
#134885 = VECTOR ( 'NONE', #1647, 1000.000000000000000 ) ;
#134886 = EDGE_LOOP ( 'NONE', ( #655, #172870, #205212, #174762 ) ) ;
#134887 = CIRCLE ( 'NONE', #242686, 12.87499999999999822 ) ;
#134888 = AXIS2_PLACEMENT_3D ( 'NONE', #128430, #168884, #150567 ) ;
#134889 = ORIENTED_EDGE ( 'NONE', *, *, #206192, .F. ) ;
#134890 = DIRECTION ( 'NONE',  ( -0.000000000000000000, -1.000000000000000000, -0.000000000000000000 ) ) ;
#134891 = CARTESIAN_POINT ( 'NONE',  ( -16.80438519320023616, 66.05022090354323439, -56.87236920360312098 ) ) ;
#134892 = DIRECTION ( 'NONE',  ( 1.000000000000000000, 0.000000000000000000, 0.000000000000000000 ) ) ;
#134893 = DIRECTION ( 'NONE',  ( 0.000000000000000000, 0.000000000000000000, -1.000000000000000000 ) ) ;
#134894 = CARTESIAN_POINT ( 'NONE',  ( 12.93225390519045170, 9.417651958841004145, -15.35878739244042812 ) ) ;
#134896 = FACE_OUTER_BOUND ( 'NONE', #203508, .T. ) ;
#134895 = DIRECTION ( 'NONE',  ( -0.7071067811865475727, 0.2890913453342130457, -0.6453109281988448354 ) ) ;
#134897 = CARTESIAN_POINT ( 'NONE',  ( 21.05000000000000071, 76.10000000001218723, -143.0637644362255401 ) ) ;
#134899 = ORIENTED_EDGE ( 'NONE', *, *, #210392, .F. ) ;
#134898 = CARTESIAN_POINT ( 'NONE',  ( -18.40000000000000213, 11.75000000001113953, -146.6500000000000341 ) ) ;
#134901 = DIRECTION ( 'NONE',  ( -1.000000000000000000, -8.623019343401623015E-17, -8.389849937938898203E-16 ) ) ;
#134900 = DIRECTION ( 'NONE',  ( 0.000000000000000000, 0.000000000000000000, -1.000000000000000000 ) ) ;
#134902 = EDGE_CURVE ( 'NONE', #182665, #183267, #34514, .T. ) ;
#134903 = DIRECTION ( 'NONE',  ( -1.000000000000000000, 0.000000000000000000, 0.000000000000000000 ) ) ;
#134904 = EDGE_LOOP ( 'NONE', ( #246656, #63593, #13105, #43226 ) ) ;
#134905 = FACE_OUTER_BOUND ( 'NONE', #142819, .T. ) ;
#134906 = LINE ( 'NONE', #214461, #233058 ) ;
#134907 = ORIENTED_EDGE ( 'NONE', *, *, #114828, .T. ) ;
#134908 = ADVANCED_FACE ( 'NONE', ( #29638 ), #109125, .T. ) ;
#134909 = FACE_OUTER_BOUND ( 'NONE', #53929, .T. ) ;
#134910 = DIRECTION ( 'NONE',  ( 0.000000000000000000, 0.1350103645451876666, -0.9908441862701600211 ) ) ;
#134911 = DIRECTION ( 'NONE',  ( 0.000000000000000000, -6.982962677686266711E-15, 1.000000000000000000 ) ) ;
#134912 = VERTEX_POINT ( 'NONE', #169151 ) ;
#134913 = ORIENTED_EDGE ( 'NONE', *, *, #78851, .T. ) ;
#134914 = VECTOR ( 'NONE', #181259, 1000.000000000000000 ) ;
#134915 = DIRECTION ( 'NONE',  ( 0.000000000000000000, -1.000000000000000000, 0.000000000000000000 ) ) ;
#134916 = CARTESIAN_POINT ( 'NONE',  ( -18.46154800491008174, -0.7175219691130436672, -242.2550643080716668 ) ) ;
#134917 = SPHERICAL_SURFACE ( 'NONE', #236426, 0.1000000000000000056 ) ;
#134918 = CARTESIAN_POINT ( 'NONE',  ( -20.89878130938411616, 10.32747123227773045, -206.5774032850248716 ) ) ;
#134919 = EDGE_LOOP ( 'NONE', ( #171260, #192045, #17491, #79838 ) ) ;
#134920 = EDGE_CURVE ( 'NONE', #224282, #118480, #159412, .T. ) ;
#134921 = DIRECTION ( 'NONE',  ( 0.000000000000000000, 0.000000000000000000, -1.000000000000000000 ) ) ;
#134922 = DIRECTION ( 'NONE',  ( 0.000000000000000000, -0.9908441862701596881, 0.1350103645451904977 ) ) ;
#134923 = CARTESIAN_POINT ( 'NONE',  ( -18.37013991200266005, 11.49974761622313224, -124.7930230105171461 ) ) ;
#134924 = CYLINDRICAL_SURFACE ( 'NONE', #120026, 0.09999999999999939493 ) ;
#134925 = CIRCLE ( 'NONE', #218140, 0.09999999999999939493 ) ;
#134926 = AXIS2_PLACEMENT_3D ( 'NONE', #37550, #72841, #117075 ) ;
#134927 = CARTESIAN_POINT ( 'NONE',  ( -18.41418431465367433, -9.499999999989068300, -207.6001893912213916 ) ) ;
#134928 = AXIS2_PLACEMENT_3D ( 'NONE', #209973, #189116, #67876 ) ;
#134929 = VECTOR ( 'NONE', #133918, 1000.000000000000000 ) ;
#134930 = EDGE_CURVE ( 'NONE', #44654, #176730, #9544, .T. ) ;
#134932 = EDGE_LOOP ( 'NONE', ( #137484, #237699, #220143, #108156 ) ) ;
#134931 = DIRECTION ( 'NONE',  ( -1.000000000000000000, 2.952720810173289112E-16, 2.061873921506763405E-30 ) ) ;
#134933 = DIRECTION ( 'NONE',  ( 0.000000000000000000, 0.9126074666063769270, 0.4088369013363282733 ) ) ;
#134934 = DIRECTION ( 'NONE',  ( 1.000000000000000000, 0.000000000000000000, 0.000000000000000000 ) ) ;
#134935 = CARTESIAN_POINT ( 'NONE',  ( 18.59999999999999787, 0.000000000000000000, 0.000000000000000000 ) ) ;
#134936 = CARTESIAN_POINT ( 'NONE',  ( 23.14999999999999503, 11.65000000001116298, -193.9851942293460070 ) ) ;
#134937 = DIRECTION ( 'NONE',  ( 0.000000000000000000, 0.000000000000000000, -1.000000000000000000 ) ) ;
#134939 = VERTEX_POINT ( 'NONE', #155995 ) ;
#134938 = CARTESIAN_POINT ( 'NONE',  ( 21.05000000000000071, 1.115600667400684642E-11, -67.00000000000000000 ) ) ;
#134940 = DIRECTION ( 'NONE',  ( 0.000000000000000000, -0.2617529984165031243, -0.9651348961777157509 ) ) ;
#134941 = CARTESIAN_POINT ( 'NONE',  ( -18.59999999999999787, 2.859758780633683273, -208.6670499591424459 ) ) ;
#134942 = LINE ( 'NONE', #155846, #103078 ) ;
#134943 = ADVANCED_FACE ( 'NONE', ( #54288 ), #213362, .T. ) ;
#134944 = EDGE_LOOP ( 'NONE', ( #60126, #97642, #95353, #37386 ) ) ;
#134945 = CARTESIAN_POINT ( 'NONE',  ( 18.59999999999999432, 1.162701749949165642, -75.10000000000003695 ) ) ;
#134946 = DIRECTION ( 'NONE',  ( -7.304098846218201720E-16, 1.000000000000000000, 0.000000000000000000 ) ) ;
#134947 = DIRECTION ( 'NONE',  ( 1.000000000000000000, 0.000000000000000000, -0.000000000000000000 ) ) ;
#134948 = SPHERICAL_SURFACE ( 'NONE', #17093, 0.1000000000000000056 ) ;
#134949 = AXIS2_PLACEMENT_3D ( 'NONE', #250514, #247946, #229682 ) ;
#134950 = EDGE_CURVE ( 'NONE', #110239, #278, #55299, .T. ) ;
#134951 = DIRECTION ( 'NONE',  ( 0.000000000000000000, 0.000000000000000000, 1.000000000000000000 ) ) ;
#134952 = AXIS2_PLACEMENT_3D ( 'NONE', #125976, #86834, #243355 ) ;
#134953 = EDGE_CURVE ( 'NONE', #101113, #72258, #213551, .T. ) ;
#134954 = DIRECTION ( 'NONE',  ( 0.000000000000000000, 1.000000000000000000, -0.000000000000000000 ) ) ;
#134956 = VERTEX_POINT ( 'NONE', #20330 ) ;
#134955 = AXIS2_PLACEMENT_3D ( 'NONE', #86939, #182233, #122254 ) ;
#134957 = ORIENTED_EDGE ( 'NONE', *, *, #221011, .F. ) ;
#134958 = AXIS2_PLACEMENT_3D ( 'NONE', #227812, #46593, #107866 ) ;
#134960 = DIRECTION ( 'NONE',  ( -1.000000000000000000, -2.986185139342066933E-16, 6.665775143889695732E-16 ) ) ;
#134959 = AXIS2_PLACEMENT_3D ( 'NONE', #155556, #255853, #56399 ) ;
#134961 = EDGE_CURVE ( 'NONE', #195497, #223676, #154716, .T. ) ;
#134962 = DIRECTION ( 'NONE',  ( -4.701977403289178058E-30, -2.433019743745433765E-14, 1.000000000000000000 ) ) ;
#134963 = LINE ( 'NONE', #150710, #172531 ) ;
#134964 = CARTESIAN_POINT ( 'NONE',  ( -21.05000000000000071, 44.47083028126616000, -247.4212268238128161 ) ) ;
#134965 = AXIS2_PLACEMENT_3D ( 'NONE', #146730, #108910, #149355 ) ;
#134966 = ADVANCED_FACE ( 'NONE', ( #55546 ), #158563, .F. ) ;
#134967 = AXIS2_PLACEMENT_3D ( 'NONE', #118690, #121282, #221591 ) ;
#134969 = EDGE_CURVE ( 'NONE', #253904, #6455, #116845, .T. ) ;
#134968 = CARTESIAN_POINT ( 'NONE',  ( -21.05000000000000071, 69.45934304831041572, -69.42310748452437963 ) ) ;
#134970 = AXIS2_PLACEMENT_3D ( 'NONE', #159132, #83383, #199539 ) ;
#134971 = CARTESIAN_POINT ( 'NONE',  ( -16.94309007106719633, 9.992226192581140864, -113.1057912825555292 ) ) ;
#134972 = VECTOR ( 'NONE', #180314, 1000.000000000000000 ) ;
#134973 = DIRECTION ( 'NONE',  ( 7.304098846218134667E-16, -0.4088369013363281068, 0.9126074666063770380 ) ) ;
#134974 = ORIENTED_EDGE ( 'NONE', *, *, #225914, .F. ) ;
#134975 = DIRECTION ( 'NONE',  ( 0.000000000000000000, 0.2128009952263485993, -0.9770955615653341697 ) ) ;
#134976 = EDGE_CURVE ( 'NONE', #97541, #23890, #73901, .T. ) ;
#134977 = AXIS2_PLACEMENT_3D ( 'NONE', #242983, #5635, #85162 ) ;
#134978 = ORIENTED_EDGE ( 'NONE', *, *, #75895, .F. ) ;
#134979 = ORIENTED_EDGE ( 'NONE', *, *, #226229, .T. ) ;
#134980 = CARTESIAN_POINT ( 'NONE',  ( -16.92209698673685025, 9.950000000011138823, -154.7893644329461722 ) ) ;
#134981 = CARTESIAN_POINT ( 'NONE',  ( -23.15000000000000213, 25.94586868676353575, -241.5435999122864530 ) ) ;
#134983 = VERTEX_POINT ( 'NONE', #236775 ) ;
#134982 = FACE_OUTER_BOUND ( 'NONE', #182121, .T. ) ;
#134984 = EDGE_CURVE ( 'NONE', #159030, #36331, #238063, .T. ) ;
#134985 = EDGE_CURVE ( 'NONE', #6661, #286, #153454, .T. ) ;
#134987 = VECTOR ( 'NONE', #80878, 1000.000000000000000 ) ;
#134986 = DIRECTION ( 'NONE',  ( 1.000000000000000000, 0.000000000000000000, 0.000000000000000000 ) ) ;
#134988 = DIRECTION ( 'NONE',  ( 0.000000000000000000, 0.8660254037844385966, -0.5000000000000003331 ) ) ;
#134989 = CARTESIAN_POINT ( 'NONE',  ( 18.48413544395646113, 85.66430403363939661, -62.84000249148589745 ) ) ;
#134990 = EDGE_LOOP ( 'NONE', ( #181343, #118370, #130132, #68559 ) ) ;
#134992 = DIRECTION ( 'NONE',  ( -1.000000000000000000, 2.849773892568378313E-16, -7.728835255496647986E-17 ) ) ;
#134991 = CIRCLE ( 'NONE', #164070, 11.70000000000000284 ) ;
#134993 = CARTESIAN_POINT ( 'NONE',  ( 18.49999999999999289, 65.50857864377491069, -145.2731074845243882 ) ) ;
#134994 = LINE ( 'NONE', #232858, #85732 ) ;
#134995 = DIRECTION ( 'NONE',  ( 0.000000000000000000, -0.1350103645451904977, -0.9908441862701596881 ) ) ;
#134996 = VERTEX_POINT ( 'NONE', #176837 ) ;
#134997 = CARTESIAN_POINT ( 'NONE',  ( -16.79184697841823493, 9.948761661669548673, -79.65414227060256280 ) ) ;
#134998 = CARTESIAN_POINT ( 'NONE',  ( -21.44999999999999929, 7.350000000011155166, -121.6500000000000341 ) ) ;
#134999 = ORIENTED_EDGE ( 'NONE', *, *, #36417, .T. ) ;
#135000 = CARTESIAN_POINT ( 'NONE',  ( 21.05000000000000071, -8.730841121484166578, -124.4019252810156928 ) ) ;
#135001 = EDGE_CURVE ( 'NONE', #9598, #186768, #255195, .T. ) ;
#135002 = EDGE_CURVE ( 'NONE', #194499, #221938, #175557, .T. ) ;
#135003 = CYLINDRICAL_SURFACE ( 'NONE', #251378, 0.1000000000000028644 ) ;
#135004 = CARTESIAN_POINT ( 'NONE',  ( 23.14999999999998792, 64.35000000001214460, -136.5231074845243597 ) ) ;
#135005 = CIRCLE ( 'NONE', #168418, 0.1000000000000028644 ) ;
#135006 = EDGE_LOOP ( 'NONE', ( #107794, #29579, #49558, #224771 ) ) ;
#135007 = CARTESIAN_POINT ( 'NONE',  ( 21.05000000000000071, 8.815201804578244094, -41.92053749668480123 ) ) ;
#135008 = AXIS2_PLACEMENT_3D ( 'NONE', #229399, #91157, #172023 ) ;
#135009 = ADVANCED_FACE ( 'NONE', ( #197651 ), #137723, .F. ) ;
#135010 = B_SPLINE_CURVE_WITH_KNOTS ( 'NONE', 3,
 ( #96520, #78253, #118698, #255566, #1, #216489, #37882, #39167, #198208, #56112 ),
 .UNSPECIFIED., .F., .F.,
 ( 4, 2, 2, 2, 4 ),
 ( 0.000000000000000000, 0.0003916577441626798361, 0.0005874866162440179652, 0.0006854010522846884935, 0.0007833154883253590217 ),
 .UNSPECIFIED. ) ;
#135012 = ORIENTED_EDGE ( 'NONE', *, *, #49583, .T. ) ;
#135011 = CIRCLE ( 'NONE', #239102, 1.899999999999999023 ) ;
#135013 =( BOUNDED_CURVE ( )  B_SPLINE_CURVE ( 3, ( #11056, #48892, #131001, #9765 ),
 .UNSPECIFIED., .F., .T. ) 
 B_SPLINE_CURVE_WITH_KNOTS ( ( 4, 4 ),
 ( 0.000000000000000000, 1.570796326794908992 ),
 .UNSPECIFIED. ) 
 CURVE ( )  GEOMETRIC_REPRESENTATION_ITEM ( )  RATIONAL_B_SPLINE_CURVE ( ( 1.000000000000000000, 0.8047378541243619399, 0.8047378541243619399, 1.000000000000000000 ) ) 
 REPRESENTATION_ITEM ( '' )  );
#135014 = AXIS2_PLACEMENT_3D ( 'NONE', #213977, #95307, #256897 ) ;
#135015 = CIRCLE ( 'NONE', #222513, 0.1000000000000002692 ) ;
#135016 = ORIENTED_EDGE ( 'NONE', *, *, #216881, .F. ) ;
#135017 = DIRECTION ( 'NONE',  ( -0.000000000000000000, -0.1350103645451928291, -0.9908441862701594660 ) ) ;
#135018 = CARTESIAN_POINT ( 'NONE',  ( -23.15000000000000213, 1.148907358139439339E-11, -201.0000000000015064 ) ) ;
#135020 = ORIENTED_EDGE ( 'NONE', *, *, #34414, .F. ) ;
#135019 = CARTESIAN_POINT ( 'NONE',  ( -40.23850191057533010, 65.25000000001119815, -51.02310748452479316 ) ) ;
#135021 = LINE ( 'NONE', #133756, #7422 ) ;
#135023 = AXIS2_PLACEMENT_3D ( 'NONE', #185683, #223503, #8341 ) ;
#135022 = CARTESIAN_POINT ( 'NONE',  ( -20.85000000000000142, 14.70949956575304185, -235.9560995168023112 ) ) ;
#135024 = CARTESIAN_POINT ( 'NONE',  ( -21.05000000000000071, 1.115600667400684642E-11, -200.9999999999999432 ) ) ;
#135025 = FACE_OUTER_BOUND ( 'NONE', #123484, .T. ) ;
#135026 = CARTESIAN_POINT ( 'NONE',  ( -21.05000000000000071, 87.29603075034721371, -99.97520832486037534 ) ) ;
#135027 = AXIS2_PLACEMENT_3D ( 'NONE', #13653, #16249, #249699 ) ;
#135028 = EDGE_CURVE ( 'NONE', #197595, #245185, #192757, .T. ) ;
#135029 = DIRECTION ( 'NONE',  ( 1.000000000000000000, 0.000000000000000000, 0.000000000000000000 ) ) ;
#135030 = DIRECTION ( 'NONE',  ( -1.000000000000000000, 0.000000000000000000, 0.000000000000000000 ) ) ;
#135032 = ORIENTED_EDGE ( 'NONE', *, *, #142185, .T. ) ;
#135031 = FACE_OUTER_BOUND ( 'NONE', #125136, .T. ) ;
#135034 = ORIENTED_EDGE ( 'NONE', *, *, #239528, .T. ) ;
#135033 = PLANE ( 'NONE',  #44441 ) ;
#135035 = CARTESIAN_POINT ( 'NONE',  ( -21.14999999999999858, 76.00000000001219291, -143.0637644362255401 ) ) ;
#135036 = AXIS2_PLACEMENT_3D ( 'NONE', #63355, #124637, #141620 ) ;
#135038 = ORIENTED_EDGE ( 'NONE', *, *, #12022, .T. ) ;
#135037 = CARTESIAN_POINT ( 'NONE',  ( 18.59999999999999432, -1.162701749926853712, -108.5000000000000426 ) ) ;
#135039 = EDGE_CURVE ( 'NONE', #32277, #12028, #84520, .T. ) ;
#135040 = VERTEX_POINT ( 'NONE', #241915 ) ;
#135041 = CARTESIAN_POINT ( 'NONE',  ( -18.55807992284872299, 10.32898536001801304, -106.0826683222765041 ) ) ;
#135042 = AXIS2_PLACEMENT_3D ( 'NONE', #93421, #255005, #76426 ) ;
#135043 = CARTESIAN_POINT ( 'NONE',  ( -16.87331047859649757, 30.20632856012693424, -234.8070450048000737 ) ) ;
#135044 = DIRECTION ( 'NONE',  ( 1.000000000000000000, -0.000000000000000000, -0.000000000000000000 ) ) ;
#135045 = EDGE_CURVE ( 'NONE', #44809, #50852, #151214, .T. ) ;
#135046 = DIRECTION ( 'NONE',  ( -1.000000000000000000, 0.000000000000000000, 0.000000000000000000 ) ) ;
#135047 = AXIS2_PLACEMENT_3D ( 'NONE', #196216, #80084, #115395 ) ;
#135048 = CARTESIAN_POINT ( 'NONE',  ( -23.25000000000000000, -0.09999999998884338825, -21.85042919245520210 ) ) ;
#135049 = EDGE_CURVE ( 'NONE', #200243, #134542, #72112, .T. ) ;
#135050 = DIRECTION ( 'NONE',  ( 0.000000000000000000, 0.000000000000000000, 1.000000000000000000 ) ) ;
#135051 = AXIS2_PLACEMENT_3D ( 'NONE', #238101, #179443, #59434 ) ;
#135052 = ORIENTED_EDGE ( 'NONE', *, *, #199185, .F. ) ;
#135053 = ORIENTED_EDGE ( 'NONE', *, *, #37650, .T. ) ;
#135054 = ADVANCED_FACE ( 'NONE', ( #24180 ), #84079, .T. ) ;
#135055 = DIRECTION ( 'NONE',  ( 1.000000000000000000, 0.000000000000000000, 0.000000000000000000 ) ) ;
#135056 = EDGE_LOOP ( 'NONE', ( #246357, #180075, #132966, #65369 ) ) ;
#135057 = FACE_OUTER_BOUND ( 'NONE', #160434, .T. ) ;
#135059 = CIRCLE ( 'NONE', #30885, 11.74999999999999645 ) ;
#135058 = CARTESIAN_POINT ( 'NONE',  ( 18.59117750673696179, 68.11287320386161070, -224.1382462126928488 ) ) ;
#135060 = CIRCLE ( 'NONE', #55759, 0.09999999999999609201 ) ;
#135061 = ADVANCED_FACE ( 'NONE', ( #22904 ), #189545, .T. ) ;
#135062 = AXIS2_PLACEMENT_3D ( 'NONE', #176406, #214233, #115130 ) ;
#135064 = EDGE_CURVE ( 'NONE', #92332, #119361, #184690, .T. ) ;
#135063 = EDGE_CURVE ( 'NONE', #233091, #155368, #26313, .T. ) ;
#135065 = CARTESIAN_POINT ( 'NONE',  ( 15.48841904831874849, 8.561580951692381092, -79.65000000000003411 ) ) ;
#135066 = ORIENTED_EDGE ( 'NONE', *, *, #115913, .F. ) ;
#135067 = CYLINDRICAL_SURFACE ( 'NONE', #219098, 0.09999999999999939493 ) ;
#135068 = ORIENTED_EDGE ( 'NONE', *, *, #213353, .F. ) ;
#135070 = FACE_OUTER_BOUND ( 'NONE', #40287, .T. ) ;
#135069 = SHAPE_REPRESENTATION ( 'Injection Molded Chain Links 15', ( #2425 ), #106268 ) ;
#135071 = ORIENTED_EDGE ( 'NONE', *, *, #211283, .F. ) ;
#135072 = CARTESIAN_POINT ( 'NONE',  ( -20.94999999999994600, 87.75000000001122658, -30.12310748452481235 ) ) ;
#135073 = DIRECTION ( 'NONE',  ( 1.000000000000000000, -0.000000000000000000, -0.000000000000000000 ) ) ;
#135074 = ORIENTED_EDGE ( 'NONE', *, *, #162010, .F. ) ;
#135075 = CARTESIAN_POINT ( 'NONE',  ( 22.39999999999999858, 7.790779598384538929, -66.90000000000004832 ) ) ;
#135076 = ORIENTED_EDGE ( 'NONE', *, *, #84653, .F. ) ;
#135078 = ORIENTED_EDGE ( 'NONE', *, *, #61941, .F. ) ;
#135077 = CARTESIAN_POINT ( 'NONE',  ( 23.15000000000000213, -8.999999999988842703, -90.60603087734760663 ) ) ;
#135079 = EDGE_CURVE ( 'NONE', #163256, #20965, #159839, .T. ) ;
#135080 = CARTESIAN_POINT ( 'NONE',  ( -21.37071067811865532, 8.070710678129811910, -88.15000000000004832 ) ) ;
#135081 = CIRCLE ( 'NONE', #243427, 0.4000000000000114575 ) ;
#135082 = EDGE_CURVE ( 'NONE', #95981, #203190, #148866, .T. ) ;
#135083 = EDGE_LOOP ( 'NONE', ( #80220, #235430, #257250, #66817 ) ) ;
#135084 = B_SPLINE_CURVE_WITH_KNOTS ( 'NONE', 3,
 ( #165660, #245183, #129085, #225582, #46951, #27457, #169536, #9137, #168252, #126514 ),
 .UNSPECIFIED., .F., .F.,
 ( 4, 2, 2, 2, 4 ),
 ( 5.259846352425386116E-16, 9.930191194500028547E-05, 0.0001986038238894745702, 0.0003972076477784231940, 0.0007944152955563411498 ),
 .UNSPECIFIED. ) ;
#135085 = ORIENTED_EDGE ( 'NONE', *, *, #122993, .F. ) ;
#135086 = EDGE_CURVE ( 'NONE', #79128, #241603, #33197, .T. ) ;
#135087 = AXIS2_PLACEMENT_3D ( 'NONE', #34943, #12804, #175725 ) ;
#135088 = DIRECTION ( 'NONE',  ( 0.000000000000000000, -0.4721928772777332917, -0.8814952561688437216 ) ) ;
#135089 = ORIENTED_EDGE ( 'NONE', *, *, #254524, .T. ) ;
#135090 = DIRECTION ( 'NONE',  ( -0.000000000000000000, 0.8660254037844502539, 0.4999999999999799605 ) ) ;
#135091 = CARTESIAN_POINT ( 'NONE',  ( 22.49806830649814060, 64.10711748978857827, -247.0785650319148203 ) ) ;
#135093 = ADVANCED_FACE ( 'NONE', ( #166276 ), #168856, .T. ) ;
#135092 = DIRECTION ( 'NONE',  ( 1.000000000000000000, -0.000000000000000000, -0.000000000000000000 ) ) ;
#135094 = FACE_OUTER_BOUND ( 'NONE', #232153, .T. ) ;
#135095 = LINE ( 'NONE', #239353, #35456 ) ;
#135096 = ADVANCED_FACE ( 'NONE', ( #127111 ), #122171, .F. ) ;
#135097 = ORIENTED_EDGE ( 'NONE', *, *, #141046, .F. ) ;
#135098 = DIRECTION ( 'NONE',  ( 0.000000000000000000, -0.8814952561688425003, 0.4721928772777359007 ) ) ;
#135099 = DIRECTION ( 'NONE',  ( 0.000000000000000000, -0.9908441862701605762, -0.1350103645451835310 ) ) ;
#135100 = CARTESIAN_POINT ( 'NONE',  ( 20.99999999999999645, 9.750000000011137757, -46.15000000000000568 ) ) ;
#135101 = ORIENTED_EDGE ( 'NONE', *, *, #100830, .F. ) ;
#135102 = CARTESIAN_POINT ( 'NONE',  ( 20.84999999999998721, 68.11287320386161070, -224.1382462126928488 ) ) ;
#135103 = ORIENTED_EDGE ( 'NONE', *, *, #225875, .T. ) ;
#135104 = FACE_OUTER_BOUND ( 'NONE', #141948, .T. ) ;
#135105 = ORIENTED_EDGE ( 'NONE', *, *, #9033, .T. ) ;
#135106 = VECTOR ( 'NONE', #100071, 1000.000000000000000 ) ;
#135107 = DIRECTION ( 'NONE',  ( 1.000000000000000000, -0.000000000000000000, -0.000000000000000000 ) ) ;
#135108 = DIRECTION ( 'NONE',  ( 1.000000000000000000, 0.000000000000000000, 0.000000000000000000 ) ) ;
#135110 = ORIENTED_EDGE ( 'NONE', *, *, #88616, .F. ) ;
#135109 = DIRECTION ( 'NONE',  ( 0.000000000000000000, -0.9121259477928120862, 0.4099100576505341209 ) ) ;
#135111 = ADVANCED_FACE ( 'NONE', ( #72294 ), #72287, .T. ) ;
#135112 = CARTESIAN_POINT ( 'NONE',  ( -20.64999999999999858, 68.85000000001156195, -57.17310748452437252 ) ) ;
#135113 = ORIENTED_EDGE ( 'NONE', *, *, #246306, .F. ) ;
#135114 = CARTESIAN_POINT ( 'NONE',  ( -20.95000000000002416, 36.22724532936084074, -235.9903003947922002 ) ) ;
#135115 = CARTESIAN_POINT ( 'NONE',  ( -16.89935556175728948, 9.950000000011010926, -113.6396763628857940 ) ) ;
#135116 = ORIENTED_EDGE ( 'NONE', *, *, #138635, .F. ) ;
#135117 = EDGE_CURVE ( 'NONE', #105944, #129607, #8461, .T. ) ;
#135118 = DIRECTION ( 'NONE',  ( 0.000000000000000000, 6.982962677686266711E-15, -1.000000000000000000 ) ) ;
#135119 = CARTESIAN_POINT ( 'NONE',  ( 20.95392731769792150, 67.11693852082312617, -94.50087950495306188 ) ) ;
#135120 = VERTEX_POINT ( 'NONE', #167555 ) ;
#135122 = DIRECTION ( 'NONE',  ( -7.304098846218134667E-16, -1.000000000000000000, -6.982962677686267499E-15 ) ) ;
#135121 = AXIS2_PLACEMENT_3D ( 'NONE', #110738, #11664, #212429 ) ;
#135123 = CIRCLE ( 'NONE', #176860, 0.2000000000000057288 ) ;
#135124 = ORIENTED_EDGE ( 'NONE', *, *, #135771, .F. ) ;
#135125 = AXIS2_PLACEMENT_3D ( 'NONE', #199406, #40354, #119872 ) ;
#135126 = VECTOR ( 'NONE', #145286, 1000.000000000000000 ) ;
#135127 = CARTESIAN_POINT ( 'NONE',  ( 14.88075390448864965, 9.431689550535256927, -118.7792900322361049 ) ) ;
#135128 = CARTESIAN_POINT ( 'NONE',  ( -21.64999999999999858, 10.05000000001113847, -180.1499999999999773 ) ) ;
#135129 =( GEOMETRIC_REPRESENTATION_CONTEXT ( 3 ) GLOBAL_UNCERTAINTY_ASSIGNED_CONTEXT ( ( #232894 ) ) GLOBAL_UNIT_ASSIGNED_CONTEXT ( ( #248402, #170201, #205399 ) ) REPRESENTATION_CONTEXT ( 'NONE', 'WORKASPACE' ) );
#135130 = ADVANCED_FACE ( 'NONE', ( #89261 ), #73047, .T. ) ;
#135132 = ORIENTED_EDGE ( 'NONE', *, *, #55736, .F. ) ;
#135131 = DIRECTION ( 'NONE',  ( 0.000000000000000000, -6.982962677686266711E-15, 1.000000000000000000 ) ) ;
#135133 = CARTESIAN_POINT ( 'NONE',  ( -21.05000000000000071, 70.15000000001192859, -92.89061026024637613 ) ) ;
#135134 = CARTESIAN_POINT ( 'NONE',  ( -16.93294127766158752, 10.00328010295486081, -20.92990726582922889 ) ) ;
#135135 = VECTOR ( 'NONE', #174586, 1000.000000000000114 ) ;
#135137 = CARTESIAN_POINT ( 'NONE',  ( 0.9000000000000547562, 64.35000000001120668, -10.02310748452479139 ) ) ;
#135136 = CARTESIAN_POINT ( 'NONE',  ( 20.95159278453404283, 8.907896337960204747, -41.98472018510925352 ) ) ;
#135138 = CARTESIAN_POINT ( 'NONE',  ( 20.04142135623730070, 61.57587952878035509, -212.2000740415318774 ) ) ;
#135139 = DIRECTION ( 'NONE',  ( 0.000000000000000000, 0.8814952561688437216, -0.4721928772777331806 ) ) ;
#135140 = DIRECTION ( 'NONE',  ( 5.421010862427554711E-16, 0.9651348961777166391, -0.2617529984164999601 ) ) ;
#135141 = AXIS2_PLACEMENT_3D ( 'NONE', #13984, #173097, #90931 ) ;
#135142 = DIRECTION ( 'NONE',  ( -1.000000000000000000, -1.836970198721029934E-16, -0.000000000000000000 ) ) ;
#135143 = AXIS2_PLACEMENT_3D ( 'NONE', #174933, #176180, #112346 ) ;
#135144 = ORIENTED_EDGE ( 'NONE', *, *, #88836, .F. ) ;
#135145 = VERTEX_POINT ( 'NONE', #50135 ) ;
#135146 = VECTOR ( 'NONE', #156682, 1000.000000000000000 ) ;
#135147 = DIRECTION ( 'NONE',  ( -1.000000000000000000, -0.000000000000000000, -0.000000000000000000 ) ) ;
#135148 = CIRCLE ( 'NONE', #81168, 4.000000000000003553 ) ;
#135150 = ORIENTED_EDGE ( 'NONE', *, *, #71153, .F. ) ;
#135149 = FACE_OUTER_BOUND ( 'NONE', #22235, .T. ) ;
#135151 = ORIENTED_EDGE ( 'NONE', *, *, #163574, .T. ) ;
#135152 = CYLINDRICAL_SURFACE ( 'NONE', #89283, 0.1000000000000013933 ) ;
#135153 = VERTEX_POINT ( 'NONE', #209213 ) ;
#135154 = CARTESIAN_POINT ( 'NONE',  ( 21.14999999999999858, 1.115600667400684642E-11, -21.85042919245520210 ) ) ;
#135155 = AXIS2_PLACEMENT_3D ( 'NONE', #111309, #209111, #69623 ) ;
#135156 = VECTOR ( 'NONE', #179197, 1000.000000000000000 ) ;
#135157 = CIRCLE ( 'NONE', #168557, 0.1000000000000054040 ) ;
#135158 = EDGE_LOOP ( 'NONE', ( #131947, #101926, #243855, #29955 ) ) ;
#135159 = CIRCLE ( 'NONE', #193470, 0.1000000000000019207 ) ;
#135160 = DIRECTION ( 'NONE',  ( 0.000000000000000000, 0.000000000000000000, 1.000000000000000000 ) ) ;
#135161 = DIRECTION ( 'NONE',  ( -0.000000000000000000, 0.8700118002898356018, -0.4930308989875170078 ) ) ;
#135162 = TOROIDAL_SURFACE ( 'NONE', #64462, 4.099999999999999645, 0.1000000000000000056 ) ;
#135164 = VERTEX_POINT ( 'NONE', #231368 ) ;
#135163 = EDGE_LOOP ( 'NONE', ( #23454, #187840, #188375, #144394 ) ) ;
#135165 = ORIENTED_EDGE ( 'NONE', *, *, #106627, .T. ) ;
#135166 = VERTEX_POINT ( 'NONE', #31897 ) ;
#135167 = ORIENTED_EDGE ( 'NONE', *, *, #150456, .F. ) ;
#135169 = CYLINDRICAL_SURFACE ( 'NONE', #180312, 0.09999999999999939493 ) ;
#135168 = AXIS2_PLACEMENT_3D ( 'NONE', #101381, #57147, #59717 ) ;
#135170 = CARTESIAN_POINT ( 'NONE',  ( -21.44999999999999929, 7.150000000011155876, -179.7499999999999716 ) ) ;
#135172 = ORIENTED_EDGE ( 'NONE', *, *, #227232, .F. ) ;
#135171 = DIRECTION ( 'NONE',  ( -0.7071067811865474617, 0.7071067811865474617, 4.937700262164531476E-15 ) ) ;
#135173 = CARTESIAN_POINT ( 'NONE',  ( 18.59999999999999432, 14.85285025691667293, -236.4388300032497057 ) ) ;
#135174 = DIRECTION ( 'NONE',  ( 0.000000000000000000, 0.000000000000000000, -1.000000000000000000 ) ) ;
#135176 = ORIENTED_EDGE ( 'NONE', *, *, #26467, .F. ) ;
#135175 = CYLINDRICAL_SURFACE ( 'NONE', #184952, 0.09999999999999939493 ) ;
#135177 = CARTESIAN_POINT ( 'NONE',  ( -23.15000000000000213, 36.65892442174935439, -249.5511627012433848 ) ) ;
#135178 = ORIENTED_EDGE ( 'NONE', *, *, #127172, .F. ) ;
#135179 = TOROIDAL_SURFACE ( 'NONE', #110062, 4.041421356237307805, 0.1000000000000000056 ) ;
#135180 = DIRECTION ( 'NONE',  ( 0.7071067811865463515, 0.7071067811865487940, 7.587431340288849180E-16 ) ) ;
#135182 = EDGE_LOOP ( 'NONE', ( #242077, #144864, #27422 ) ) ;
#135181 = CARTESIAN_POINT ( 'NONE',  ( 20.73486653747088937, 29.16750423011593440, -236.7463345683714522 ) ) ;
#135183 = CARTESIAN_POINT ( 'NONE',  ( 0.9000000000000549782, 66.35000000001119247, -12.62310748452479281 ) ) ;
#135184 = CARTESIAN_POINT ( 'NONE',  ( -16.94107738177415712, 10.01423928514777550, -113.0500000000000398 ) ) ;
#135185 = ADVANCED_FACE ( 'NONE', ( #52701 ), #30608, .T. ) ;
#135186 = VERTEX_POINT ( 'NONE', #150541 ) ;
#135188 = CARTESIAN_POINT ( 'NONE',  ( -18.59999999999999787, 43.35377423437995503, -245.1717807829448930 ) ) ;
#135187 = DIRECTION ( 'NONE',  ( 0.000000000000000000, 1.000000000000000000, 0.000000000000000000 ) ) ;
#135189 = DIRECTION ( 'NONE',  ( -7.304098846218134667E-16, -1.000000000000000000, 0.000000000000000000 ) ) ;
#135190 = CARTESIAN_POINT ( 'NONE',  ( 20.94999999999999929, 76.00000000001173817, -72.42310748452430857 ) ) ;
#135191 = LINE ( 'NONE', #170545, #176678 ) ;
#135192 = VERTEX_POINT ( 'NONE', #210510 ) ;
#135193 = ORIENTED_EDGE ( 'NONE', *, *, #49468, .T. ) ;
#135194 = LINE ( 'NONE', #75272, #69173 ) ;
#135195 = EDGE_LOOP ( 'NONE', ( #238074, #63410, #12982, #191579, #151491 ) ) ;
#135196 = ORIENTED_EDGE ( 'NONE', *, *, #107230, .T. ) ;
#135197 = ADVANCED_FACE ( 'NONE', ( #111410 ), #4462, .T. ) ;
#135198 = PLANE ( 'NONE',  #148293 ) ;
#135199 = CARTESIAN_POINT ( 'NONE',  ( -20.54999999999999716, 2.500000000011156409, -46.72462192276210402 ) ) ;
#135200 = EDGE_CURVE ( 'NONE', #186782, #18582, #95683, .T. ) ;
#135201 = CIRCLE ( 'NONE', #151811, 0.09999999999999939493 ) ;
#135202 = CIRCLE ( 'NONE', #197935, 11.74999999999999645 ) ;
#135203 = VERTEX_POINT ( 'NONE', #173998 ) ;
#135204 = CARTESIAN_POINT ( 'NONE',  ( -20.54999999999999716, -9.499999999988848032, -43.39396912265245021 ) ) ;
#135205 = VECTOR ( 'NONE', #162343, 1000.000000000000000 ) ;
#135206 = EDGE_CURVE ( 'NONE', #2322, #224755, #232659, .T. ) ;
#135207 = ORIENTED_EDGE ( 'NONE', *, *, #155753, .T. ) ;
#135208 = ORIENTED_EDGE ( 'NONE', *, *, #107769, .F. ) ;
#135209 = ORIENTED_EDGE ( 'NONE', *, *, #126774, .T. ) ;
#135210 = CIRCLE ( 'NONE', #22827, 0.1000000000000072220 ) ;
#135211 = ADVANCED_FACE ( 'NONE', ( #57828 ), #216912, .T. ) ;
#135212 = DIRECTION ( 'NONE',  ( 0.000000000000000000, -0.4930308989875248349, -0.8700118002898312719 ) ) ;
#135213 = DIRECTION ( 'NONE',  ( 0.000000000000000000, 0.000000000000000000, -1.000000000000000000 ) ) ;
#135214 = CIRCLE ( 'NONE', #22828, 0.09999999999999892308 ) ;
#135215 = CARTESIAN_POINT ( 'NONE',  ( -16.90257928357874917, 66.04589317890619782, -56.88682205441069328 ) ) ;
#135217 = EDGE_CURVE ( 'NONE', #103352, #224045, #93111, .T. ) ;
#135216 = DIRECTION ( 'NONE',  ( 1.000000000000000000, 0.000000000000000000, 0.000000000000000000 ) ) ;
#135218 = CARTESIAN_POINT ( 'NONE',  ( 14.22916352759893854, 66.54258906972185628, -118.0231915757780570 ) ) ;
#135220 = CARTESIAN_POINT ( 'NONE',  ( -20.64999999999999858, 0.000000000000000000, -31.50000000000000000 ) ) ;
#135219 = FACE_OUTER_BOUND ( 'NONE', #232524, .T. ) ;
#135222 = ORIENTED_EDGE ( 'NONE', *, *, #38740, .F. ) ;
#135221 = CARTESIAN_POINT ( 'NONE',  ( 23.14999999999999858, 5.000000000011153745, -112.9052660189131245 ) ) ;
#135223 = CARTESIAN_POINT ( 'NONE',  ( -16.89268316805465986, 9.951721813253337601, -154.8557524785455541 ) ) ;
#135224 = ORIENTED_EDGE ( 'NONE', *, *, #88032, .F. ) ;
#135225 = ADVANCED_FACE ( 'NONE', ( #236482 ), #192903, .T. ) ;
#135226 = CARTESIAN_POINT ( 'NONE',  ( -15.70407651835960650, 9.355806591641286474, -150.2911025315461870 ) ) ;
#135227 = EDGE_LOOP ( 'NONE', ( #208705, #179295, #221434, #33284 ) ) ;
#135228 = VERTEX_POINT ( 'NONE', #175272 ) ;
#135229 = DIRECTION ( 'NONE',  ( 0.000000000000000000, 0.000000000000000000, -1.000000000000000000 ) ) ;
#135230 = AXIS2_PLACEMENT_3D ( 'NONE', #242961, #206415, #246815 ) ;
#135231 = CARTESIAN_POINT ( 'NONE',  ( -21.05000000000000071, 6.540656951712399803, -134.0000000000000284 ) ) ;
#135232 = CARTESIAN_POINT ( 'NONE',  ( 20.84999999999999432, -1.164121893241208960, -41.41484808557160591 ) ) ;
#135233 = AXIS2_PLACEMENT_3D ( 'NONE', #73166, #31473, #110978 ) ;
#135234 = CARTESIAN_POINT ( 'NONE',  ( 20.95289811251229750, 8.893168004469750088, -75.50180949391855734 ) ) ;
#135235 = EDGE_CURVE ( 'NONE', #90818, #39258, #192244, .T. ) ;
#135236 = PLANE ( 'NONE',  #84063 ) ;
#135237 = ORIENTED_EDGE ( 'NONE', *, *, #54687, .T. ) ;
#135239 = ORIENTED_EDGE ( 'NONE', *, *, #156055, .T. ) ;
#135238 = EDGE_CURVE ( 'NONE', #143070, #119750, #163863, .T. ) ;
#135240 = SPHERICAL_SURFACE ( 'NONE', #128331, 0.1000000000000000056 ) ;
#135241 = ORIENTED_EDGE ( 'NONE', *, *, #167198, .F. ) ;
#135242 = PLANE ( 'NONE',  #182055 ) ;
#135243 = FACE_OUTER_BOUND ( 'NONE', #59702, .T. ) ;
#135244 = EDGE_LOOP ( 'NONE', ( #57638, #87119, #20138, #249925 ) ) ;
#135245 = EDGE_CURVE ( 'NONE', #2377, #160646, #80424, .T. ) ;
#135246 = DIRECTION ( 'NONE',  ( -1.000000000000000000, -8.674042436075324885E-17, -1.619280515896126624E-16 ) ) ;
#135247 = CIRCLE ( 'NONE', #185150, 0.1000000000000021844 ) ;
#135248 = CARTESIAN_POINT ( 'NONE',  ( -18.47140463609787631, -9.671474685209723532, -207.6727604582740696 ) ) ;
#135249 = EDGE_LOOP ( 'NONE', ( #113452, #135288, #206979, #30304 ) ) ;
#135250 = EDGE_CURVE ( 'NONE', #77835, #214564, #88816, .T. ) ;
#135251 = DIRECTION ( 'NONE',  ( -1.000000000000000000, 3.151514657663852580E-16, -8.547182517843351137E-17 ) ) ;
#135252 = CARTESIAN_POINT ( 'NONE',  ( 23.14999999999998437, 7.128833340093095217, -233.7327013124392749 ) ) ;
#135253 = CARTESIAN_POINT ( 'NONE',  ( -21.14999999893415250, 57.68250670178610306, -226.1736674723211706 ) ) ;
#135254 = AXIS2_PLACEMENT_3D ( 'NONE', #247427, #109192, #70112 ) ;
#135255 = AXIS2_PLACEMENT_3D ( 'NONE', #226543, #230423, #49213 ) ;
#135256 = ORIENTED_EDGE ( 'NONE', *, *, #78419, .F. ) ;
#135257 = AXIS2_PLACEMENT_3D ( 'NONE', #182826, #44582, #4155 ) ;
#135258 = ADVANCED_FACE ( 'NONE', ( #136074 ), #55477, .T. ) ;
#135259 = CARTESIAN_POINT ( 'NONE',  ( 21.05000000000000426, 0.03486800302424813980, -161.2299141363108390 ) ) ;
#135260 = VERTEX_POINT ( 'NONE', #172715 ) ;
#135261 = CARTESIAN_POINT ( 'NONE',  ( -20.94999999999999929, 68.92903212821303782, -99.27654326265604823 ) ) ;
#135262 = CARTESIAN_POINT ( 'NONE',  ( 18.49999999999999645, -1.637172712959225507, -45.08215336547201701 ) ) ;
#135263 = FACE_OUTER_BOUND ( 'NONE', #216418, .T. ) ;
#135264 = DIRECTION ( 'NONE',  ( 0.000000000000000000, 0.000000000000000000, -1.000000000000000000 ) ) ;
#135265 = CARTESIAN_POINT ( 'NONE',  ( -23.25000000000000355, 64.25000000001210765, -127.2731074845243882 ) ) ;
#135266 = DIRECTION ( 'NONE',  ( 0.000000000000000000, 0.000000000000000000, 1.000000000000000000 ) ) ;
#135267 = ORIENTED_EDGE ( 'NONE', *, *, #66709, .T. ) ;
#135268 = CARTESIAN_POINT ( 'NONE',  ( -16.93909480342659890, 66.00692163521051725, -123.9227604678520436 ) ) ;
#135269 = CARTESIAN_POINT ( 'NONE',  ( -23.15000000000000213, 76.00000000001213607, -136.5231074845242745 ) ) ;
#135270 = FACE_OUTER_BOUND ( 'NONE', #40257, .T. ) ;
#135271 = CARTESIAN_POINT ( 'NONE',  ( 23.30000000000000426, -11.79999999999999538, 33.00000000000000000 ) ) ;
#135272 = AXIS2_PLACEMENT_3D ( 'NONE', #41263, #219859, #137744 ) ;
#135273 = CYLINDRICAL_SURFACE ( 'NONE', #24140, 0.1000000000000000194 ) ;
#135274 = EDGE_CURVE ( 'NONE', #31859, #239007, #5604, .T. ) ;
#135275 = ORIENTED_EDGE ( 'NONE', *, *, #22430, .T. ) ;
#135276 = ORIENTED_EDGE ( 'NONE', *, *, #247429, .T. ) ;
#135277 = CARTESIAN_POINT ( 'NONE',  ( -20.94999999999999929, 76.00000000001173817, -73.62310748452429721 ) ) ;
#135278 = CARTESIAN_POINT ( 'NONE',  ( -20.90000000000000213, 6.356682116888462630, 11.91686199900910381 ) ) ;
#135279 = CARTESIAN_POINT ( 'NONE',  ( -21.05000000000000071, 11.60000000001115517, -93.57179676972454274 ) ) ;
#135281 = DIRECTION ( 'NONE',  ( 0.000000000000000000, 0.2128009952263485993, -0.9770955615653340587 ) ) ;
#135280 = VECTOR ( 'NONE', #215172, 1000.000000000000000 ) ;
#135282 = CARTESIAN_POINT ( 'NONE',  ( -16.97683809663752186, 23.64127277249475156, -231.2903243416350847 ) ) ;
#135283 = EDGE_CURVE ( 'NONE', #221285, #35500, #255376, .T. ) ;
#135284 = ORIENTED_EDGE ( 'NONE', *, *, #232504, .F. ) ;
#135285 = CARTESIAN_POINT ( 'NONE',  ( 18.69999999999999929, 7.800000000000000711, -15.00000000000000000 ) ) ;
#135286 = CYLINDRICAL_SURFACE ( 'NONE', #34269, 0.1000000000000001443 ) ;
#135287 = EDGE_CURVE ( 'NONE', #236175, #211977, #180081, .T. ) ;
#135288 = ORIENTED_EDGE ( 'NONE', *, *, #64967, .T. ) ;
#135290 = ADVANCED_FACE ( 'NONE', ( #139935 ), #1345, .T. ) ;
#135289 = DIRECTION ( 'NONE',  ( 0.000000000000000000, 1.000000000000000000, 0.000000000000000000 ) ) ;
#135291 = CARTESIAN_POINT ( 'NONE',  ( -20.54999999999999716, 85.00000000001149658, -45.91707660717669626 ) ) ;
#135292 = EDGE_CURVE ( 'NONE', #67059, #150585, #176354, .T. ) ;
#135293 = AXIS2_PLACEMENT_3D ( 'NONE', #179416, #728, #255017 ) ;
#135294 = AXIS2_PLACEMENT_3D ( 'NONE', #36526, #22081, #216406 ) ;
#135295 = ORIENTED_EDGE ( 'NONE', *, *, #21267, .F. ) ;
#135296 = CARTESIAN_POINT ( 'NONE',  ( -18.34374000495060386, 64.52683809665015247, -194.2731074845244450 ) ) ;
#135297 = ADVANCED_FACE ( 'NONE', ( #199950 ), #62984, .T. ) ;
#135298 = VERTEX_POINT ( 'NONE', #141243 ) ;
#135299 = FACE_OUTER_BOUND ( 'NONE', #215974, .T. ) ;
#135300 = DIRECTION ( 'NONE',  ( -0.000000000000000000, 0.8814952561688430555, -0.4721928772777346239 ) ) ;
#135301 = DIRECTION ( 'NONE',  ( 0.000000000000000000, -0.1568667991644714932, 0.9876197685951274563 ) ) ;
#135302 = CARTESIAN_POINT ( 'NONE',  ( 22.01447462590973814, 75.90096299995289542, -177.2869076857542723 ) ) ;
#135303 = LINE ( 'NONE', #119624, #157217 ) ;
#135304 = FACE_OUTER_BOUND ( 'NONE', #42016, .T. ) ;
#135305 = DIRECTION ( 'NONE',  ( 0.000000000000000000, 0.9968797965484670343, 0.07893460099023182075 ) ) ;
#135306 = FACE_OUTER_BOUND ( 'NONE', #142459, .T. ) ;
#135307 = PLANE ( 'NONE',  #182991 ) ;
#135308 = DIRECTION ( 'NONE',  ( 0.000000000000000000, 0.000000000000000000, 1.000000000000000000 ) ) ;
#135309 = DIRECTION ( 'NONE',  ( -0.000000000000000000, -1.000000000000000000, -6.982962677686266711E-15 ) ) ;
#135310 = CARTESIAN_POINT ( 'NONE',  ( -22.59999999999999787, 11.64957080755595520, -100.4000000000000483 ) ) ;
#135312 = PLANE ( 'NONE',  #103047 ) ;
#135311 = CIRCLE ( 'NONE', #106072, 11.80000000000000426 ) ;
#135313 = ORIENTED_EDGE ( 'NONE', *, *, #27402, .F. ) ;
#135314 = CIRCLE ( 'NONE', #22926, 2.700000000000001066 ) ;
#135315 = CARTESIAN_POINT ( 'NONE',  ( -23.25000000000000000, 1.115600667400684642E-11, -200.9999999999999432 ) ) ;
#135317 = CARTESIAN_POINT ( 'NONE',  ( 23.14999999999999858, 1.115600667400684642E-11, -67.00000000000000000 ) ) ;
#135316 = AXIS2_PLACEMENT_3D ( 'NONE', #29462, #165079, #124678 ) ;
#135318 = AXIS2_PLACEMENT_3D ( 'NONE', #57504, #215313, #116237 ) ;
#135319 = ADVANCED_FACE ( 'NONE', ( #240356 ), #181664, .F. ) ;
#135320 = VERTEX_POINT ( 'NONE', #2995 ) ;
#135322 = DIRECTION ( 'NONE',  ( 1.000000000000000000, 0.000000000000000000, -0.000000000000000000 ) ) ;
#135321 = COLOUR_RGB ( '', 0.66274510, 0.83137255, 0.94901961) ;
#135323 = LINE ( 'NONE', #234426, #187622 ) ;
#135324 = DIRECTION ( 'NONE',  ( 0.000000000000000000, 0.8454177738465993297, 0.5341055959866553016 ) ) ;
#135325 = EDGE_CURVE ( 'NONE', #146767, #157290, #67995, .T. ) ;
#135326 = ADVANCED_FACE ( 'NONE', ( #160830 ), #26499, .F. ) ;
#135327 = ORIENTED_EDGE ( 'NONE', *, *, #50824, .T. ) ;
#135328 = CYLINDRICAL_SURFACE ( 'NONE', #14057, 0.1000000000000013656 ) ;
#135329 = ORIENTED_EDGE ( 'NONE', *, *, #239726, .T. ) ;
#135330 = DIRECTION ( 'NONE',  ( 0.1538461538461656786, -0.4039696218773441982, 0.9017427047373420823 ) ) ;
#135331 = CARTESIAN_POINT ( 'NONE',  ( 20.94999999999999929, 87.65000000001141700, -36.02310748452425315 ) ) ;
#135332 = AXIS2_PLACEMENT_3D ( 'NONE', #173337, #72935, #252804 ) ;
#135333 = VECTOR ( 'NONE', #127478, 1000.000000000000000 ) ;
#135334 = CIRCLE ( 'NONE', #106286, 11.74999999999999645 ) ;
#135335 = ORIENTED_EDGE ( 'NONE', *, *, #33437, .T. ) ;
#135336 = DIRECTION ( 'NONE',  ( 0.000000000000000000, 0.2128009952263604232, -0.9770955615653316162 ) ) ;
#135337 = ORIENTED_EDGE ( 'NONE', *, *, #56042, .T. ) ;
#135338 = LINE ( 'NONE', #238296, #108302 ) ;
#135339 = CARTESIAN_POINT ( 'NONE',  ( 21.12400222705966257, 67.22148809293496186, -124.2731074845243597 ) ) ;
#135341 = CIRCLE ( 'NONE', #173005, 0.09999999999999080458 ) ;
#135340 = LINE ( 'NONE', #134063, #99278 ) ;
#135343 = DIRECTION ( 'NONE',  ( 1.000000000000000000, 0.000000000000000000, 0.000000000000000000 ) ) ;
#135342 = AXIS2_PLACEMENT_3D ( 'NONE', #150758, #51615, #148180 ) ;
#135344 = AXIS2_PLACEMENT_3D ( 'NONE', #244184, #241635, #222040 ) ;
#135345 = CARTESIAN_POINT ( 'NONE',  ( -16.79139129368504513, 9.944944162461677450, -12.67024463282581337 ) ) ;
#135346 = ADVANCED_FACE ( 'NONE', ( #100782 ), #65546, .F. ) ;
#135348 = CIRCLE ( 'NONE', #2063, 0.1000000000000018374 ) ;
#135347 = CARTESIAN_POINT ( 'NONE',  ( -15.06774609480954474, 46.82518482938919391, -234.6773041598980853 ) ) ;
#135349 = DIRECTION ( 'NONE',  ( 0.000000000000000000, -1.000000000000000000, -6.982962677686266711E-15 ) ) ;
#135350 = PLANE ( 'NONE',  #33082 ) ;
#135352 = VERTEX_POINT ( 'NONE', #198642 ) ;
#135351 = CARTESIAN_POINT ( 'NONE',  ( 21.05000000000000071, 69.52244781751849700, -102.9231075192248142 ) ) ;
#135353 = EDGE_LOOP ( 'NONE', ( #35522, #26949, #62256, #87177, #128265 ) ) ;
#135355 = DIRECTION ( 'NONE',  ( 2.557131231893037478E-16, -0.8660254037844385966, 0.5000000000000003331 ) ) ;
#135354 = CARTESIAN_POINT ( 'NONE',  ( -21.05000000000000071, 6.413759733810282526, -0.08561306080396846596 ) ) ;
#135357 = EDGE_LOOP ( 'NONE', ( #246136, #50513, #188286, #63649 ) ) ;
#135356 = DIRECTION ( 'NONE',  ( -1.000000000000000000, -0.000000000000000000, -0.000000000000000000 ) ) ;
#135358 = VERTEX_POINT ( 'NONE', #42157 ) ;
#135359 = DIRECTION ( 'NONE',  ( 2.952720810173289112E-16, -1.000000000000000000, 0.000000000000000000 ) ) ;
#135360 = CARTESIAN_POINT ( 'NONE',  ( 20.11144452914359348, 9.933610851132206321, -175.3902934539515002 ) ) ;
#135361 = AXIS2_PLACEMENT_3D ( 'NONE', #93411, #153447, #54281 ) ;
#135362 = AXIS2_PLACEMENT_3D ( 'NONE', #906, #80438, #239562 ) ;
#135363 = FACE_OUTER_BOUND ( 'NONE', #78585, .T. ) ;
#135364 = CARTESIAN_POINT ( 'NONE',  ( -23.25000000000000000, 71.65000000001155911, -57.17310748452435121 ) ) ;
#135365 = DIRECTION ( 'NONE',  ( 0.000000000000000000, 0.1455152366551500653, 0.9893560106964507384 ) ) ;
#135366 = AXIS2_PLACEMENT_3D ( 'NONE', #119410, #219770, #20321 ) ;
#135367 = CARTESIAN_POINT ( 'NONE',  ( -18.50000000000000000, 3.912899247244609580, -111.9818229730110062 ) ) ;
#135368 = CARTESIAN_POINT ( 'NONE',  ( -20.54999999999999716, 66.65000000001157332, -57.27310748452438816 ) ) ;
#135369 = ADVANCED_FACE ( 'NONE', ( #121701 ), #184207, .T. ) ;
#135370 = CARTESIAN_POINT ( 'NONE',  ( 22.50000000000000000, 1.115600667400684642E-11, -33.50000000000000000 ) ) ;
#135371 = ORIENTED_EDGE ( 'NONE', *, *, #58745, .F. ) ;
#135372 = VERTEX_POINT ( 'NONE', #43427 ) ;
#135373 = EDGE_CURVE ( 'NONE', #10090, #29906, #234583, .T. ) ;
#135374 = CARTESIAN_POINT ( 'NONE',  ( -20.94999999999999929, -11.39257802169451672, -170.5739495798319183 ) ) ;
#135375 = VERTEX_POINT ( 'NONE', #23892 ) ;
#135376 = DIRECTION ( 'NONE',  ( -1.020425574104004196E-15, 0.000000000000000000, 1.000000000000000000 ) ) ;
#135377 = ORIENTED_EDGE ( 'NONE', *, *, #126553, .T. ) ;
#135378 = CARTESIAN_POINT ( 'NONE',  ( 18.43466021071414573, -9.494190690456539627, -40.11706156012773050 ) ) ;
#135379 = EDGE_CURVE ( 'NONE', #246882, #152864, #109675, .T. ) ;
#135380 = ADVANCED_FACE ( 'NONE', ( #223327 ), #99514, .F. ) ;
#135381 = CARTESIAN_POINT ( 'NONE',  ( 21.05000000000000071, 76.00000000001142553, -36.02310748452432421 ) ) ;
#135382 = DIRECTION ( 'NONE',  ( -1.000000000000000000, 0.000000000000000000, -0.000000000000000000 ) ) ;
#135384 = ORIENTED_EDGE ( 'NONE', *, *, #219562, .F. ) ;
#135383 = CARTESIAN_POINT ( 'NONE',  ( -21.12642695952773764, 6.375659922046319927, -33.40109671681064185 ) ) ;
#135385 = DIRECTION ( 'NONE',  ( 0.000000000000000000, 0.000000000000000000, -1.000000000000000000 ) ) ;
#135386 = EDGE_LOOP ( 'NONE', ( #162215, #152051, #255717, #238256 ) ) ;
#135387 = CIRCLE ( 'NONE', #172872, 0.1000000000000000472 ) ;
#135388 = CARTESIAN_POINT ( 'NONE',  ( -23.15000000000000213, 68.62136427087769164, -214.1108709299723500 ) ) ;
#135389 = CARTESIAN_POINT ( 'NONE',  ( -21.05000000000000071, 75.90220970870291239, -75.78092209500043452 ) ) ;
#135390 = VECTOR ( 'NONE', #250881, 1000.000000000000000 ) ;
#135391 = CARTESIAN_POINT ( 'NONE',  ( 20.94999999999999929, 5.850000000011156942, -123.8675027757221159 ) ) ;
#135392 = CARTESIAN_POINT ( 'NONE',  ( -21.52071067811865746, 68.22071067813045886, -81.77310748452435973 ) ) ;
#135393 = CIRCLE ( 'NONE', #39767, 0.09999999999998898659 ) ;
#135394 = ORIENTED_EDGE ( 'NONE', *, *, #29430, .F. ) ;
#135396 = DIRECTION ( 'NONE',  ( 0.000000000000000000, -0.5000000000000078826, -0.8660254037844340447 ) ) ;
#135395 = CARTESIAN_POINT ( 'NONE',  ( 23.50000000000005684, 77.16254490893143725, -43.82310748452479743 ) ) ;
#135397 = EDGE_LOOP ( 'NONE', ( #257950, #229776, #217820, #109826 ) ) ;
#135400 = ORIENTED_EDGE ( 'NONE', *, *, #114243, .F. ) ;
#135399 = CARTESIAN_POINT ( 'NONE',  ( -18.59999999999999787, 11.65000000001115232, -79.15000000000004832 ) ) ;
#135398 = DIRECTION ( 'NONE',  ( 0.000000000000000000, 0.001293682058376932620, 0.9999991631930158498 ) ) ;
#135401 = EDGE_CURVE ( 'NONE', #142601, #93118, #247039, .T. ) ;
#135402 = CARTESIAN_POINT ( 'NONE',  ( -20.94999999999999929, -11.48912529306490349, -170.5999999999999659 ) ) ;
#135403 = EDGE_CURVE ( 'NONE', #95630, #57548, #164665, .T. ) ;
#135404 = VECTOR ( 'NONE', #136032, 1000.000000000000000 ) ;
#135405 = AXIS2_PLACEMENT_3D ( 'NONE', #144539, #63729, #168010 ) ;
#135406 = VERTEX_POINT ( 'NONE', #120432 ) ;
#135407 = DIRECTION ( 'NONE',  ( 0.000000000000000000, 0.000000000000000000, -1.000000000000000000 ) ) ;
#135409 = CARTESIAN_POINT ( 'NONE',  ( -20.54999999999999716, 76.00000000001190870, -103.0231074845243029 ) ) ;
#135408 =( BOUNDED_SURFACE ( )  B_SPLINE_SURFACE ( 3, 2, ( 
 ( #91397, #189215, #31455 ),
 ( #10582, #34025, #170979 ),
 ( #9284, #52242, #131797 ),
 ( #133090, #212635, #113521 ),
 ( #168414, #148808, #228342 ),
 ( #186195, #167940, #147044 ) ),
 .UNSPECIFIED., .F., .F., .F. ) 
 B_SPLINE_SURFACE_WITH_KNOTS ( ( 4, 2, 4 ),
 ( 3, 3 ),
 ( 0.0001300404313046710908, 0.0003183318589266775434, 0.0005066232865486839688 ),
 ( 0.000000000000000000, 1.000000000000000000 ),
 .UNSPECIFIED. ) 
 GEOMETRIC_REPRESENTATION_ITEM ( )  RATIONAL_B_SPLINE_SURFACE ( (
 ( 1.000000000000000000, 0.7071067811865966446, 1.000000000000000000),
 ( 1.000000000000000000, 0.7625113560540166535, 1.000000000000000000),
 ( 1.000000000000000000, 0.8126073484687468262, 1.000000000000000000),
 ( 1.000000000000000000, 0.8923049332733752337, 1.000000000000000000),
 ( 1.000000000000000000, 0.9231914937768672669, 1.000000000000000000),
 ( 1.000000000000000000, 0.9238795325112946211, 1.000000000000000000) ) ) 
 REPRESENTATION_ITEM ( '' )  SURFACE ( )  );
#135410 = DIRECTION ( 'NONE',  ( 1.000000000000000000, 0.000000000000000000, 0.000000000000000000 ) ) ;
#135412 = ORIENTED_EDGE ( 'NONE', *, *, #124882, .F. ) ;
#135411 = LINE ( 'NONE', #177152, #47701 ) ;
#135413 = CIRCLE ( 'NONE', #173257, 2.000000000000001776 ) ;
#135414 = CARTESIAN_POINT ( 'NONE',  ( -20.54999999999999716, 7.150000000011155876, -79.25000000000004263 ) ) ;
#135415 = EDGE_CURVE ( 'NONE', #126778, #143787, #1715, .T. ) ;
#135416 = AXIS2_PLACEMENT_3D ( 'NONE', #126899, #69513, #250685 ) ;
#135417 = VERTEX_POINT ( 'NONE', #71986 ) ;
#135419 = ADVANCED_FACE ( 'NONE', ( #107244 ), #249344, .F. ) ;
#135418 = FACE_OUTER_BOUND ( 'NONE', #52091, .T. ) ;
#135420 = CARTESIAN_POINT ( 'NONE',  ( 18.42595409746875745, -9.499999812554055012, -73.99936235174590138 ) ) ;
#135421 = CARTESIAN_POINT ( 'NONE',  ( -20.90000000000000213, 11.49641995933507843, 1.885425182446133885 ) ) ;
#135422 = AXIS2_PLACEMENT_3D ( 'NONE', #233227, #136649, #77959 ) ;
#135423 = VERTEX_POINT ( 'NONE', #29040 ) ;
#135424 = CARTESIAN_POINT ( 'NONE',  ( -21.00000000000000000, 0.000000000000000000, -7.800000000000000711 ) ) ;
#135425 = EDGE_LOOP ( 'NONE', ( #160503, #18655, #209873, #53018 ) ) ;
#135426 = FACE_OUTER_BOUND ( 'NONE', #105349, .T. ) ;
#135427 = DIRECTION ( 'NONE',  ( 1.000000000000000000, 0.000000000000000000, 0.000000000000000000 ) ) ;
#135428 = SPHERICAL_SURFACE ( 'NONE', #247575, 0.1000000000000000056 ) ;
#135429 = AXIS2_PLACEMENT_3D ( 'NONE', #226567, #47937, #127490 ) ;
#135430 = ORIENTED_EDGE ( 'NONE', *, *, #174793, .T. ) ;
#135431 = EDGE_CURVE ( 'NONE', #60123, #33086, #69425, .T. ) ;
#135432 = CYLINDRICAL_SURFACE ( 'NONE', #79487, 0.1000000000000046685 ) ;
#135433 = DIRECTION ( 'NONE',  ( -0.000000000000000000, 0.8660254037844502539, 0.4999999999999799050 ) ) ;
#135434 = ORIENTED_EDGE ( 'NONE', *, *, #32247, .T. ) ;
#135435 = ADVANCED_FACE ( 'NONE', ( #87669 ), #189363, .T. ) ;
#135436 = CARTESIAN_POINT ( 'NONE',  ( -23.15000000000000213, 1.115600667400684642E-11, -171.6499999999999773 ) ) ;
#135437 = DIRECTION ( 'NONE',  ( 1.000000000000000000, -0.000000000000000000, 0.000000000000000000 ) ) ;
#135438 = LINE ( 'NONE', #235825, #161282 ) ;
#135439 = AXIS2_PLACEMENT_3D ( 'NONE', #134527, #7194, #193247 ) ;
#135440 = ORIENTED_EDGE ( 'NONE', *, *, #48112, .T. ) ;
#135441 = CIRCLE ( 'NONE', #81261, 0.1000000000000057648 ) ;
#135442 = ORIENTED_EDGE ( 'NONE', *, *, #105078, .F. ) ;
#135443 = CARTESIAN_POINT ( 'NONE',  ( -18.59999999999999787, 77.16412189325286874, -61.60825939895269698 ) ) ;
#135444 = EDGE_LOOP ( 'NONE', ( #170831, #26611, #198189, #90779 ) ) ;
#135446 = EDGE_LOOP ( 'NONE', ( #82937, #176838, #172388 ) ) ;
#135445 = CARTESIAN_POINT ( 'NONE',  ( -18.59999999999999787, 77.73670573947940454, -91.50568489690056140 ) ) ;
#135447 = EDGE_CURVE ( 'NONE', #106883, #65528, #31599, .T. ) ;
#135450 = ORIENTED_EDGE ( 'NONE', *, *, #222613, .T. ) ;
#135449 = VERTEX_POINT ( 'NONE', #45986 ) ;
#135448 = FACE_OUTER_BOUND ( 'NONE', #209559, .T. ) ;
#135451 = FACE_OUTER_BOUND ( 'NONE', #121034, .T. ) ;
#135452 = CARTESIAN_POINT ( 'NONE',  ( -16.82055514392383699, 12.41973608413271535, -211.2690732309943371 ) ) ;
#135453 = CARTESIAN_POINT ( 'NONE',  ( 21.09696443733127325, 10.72400988392963228, -112.7347775270482657 ) ) ;
#135454 = CIRCLE ( 'NONE', #39646, 11.74999999999999645 ) ;
#135455 = CARTESIAN_POINT ( 'NONE',  ( 21.05000000000000071, 65.51540711881831669, -196.0663939139407432 ) ) ;
#135456 = CARTESIAN_POINT ( 'NONE',  ( -20.94999999999999929, 68.96868720525620233, -32.41395654629707224 ) ) ;
#135457 = CARTESIAN_POINT ( 'NONE',  ( -20.54999999999999716, 73.50000000001180922, -82.74772940728642823 ) ) ;
#135458 = ORIENTED_EDGE ( 'NONE', *, *, #76582, .F. ) ;
#135459 = ORIENTED_EDGE ( 'NONE', *, *, #187704, .F. ) ;
#135460 = ORIENTED_EDGE ( 'NONE', *, *, #64305, .T. ) ;
#135461 = DIRECTION ( 'NONE',  ( -7.304098846218134667E-16, 1.000000000000000000, 6.982962677686267499E-15 ) ) ;
#135462 = VECTOR ( 'NONE', #205871, 1000.000000000000000 ) ;
#135464 = VERTEX_POINT ( 'NONE', #167258 ) ;
#135463 = DIRECTION ( 'NONE',  ( -2.602085213965226419E-14, -6.982962677686266711E-15, 1.000000000000000000 ) ) ;
#135465 = CARTESIAN_POINT ( 'NONE',  ( 21.05000000000000071, 87.48912529308852015, -173.0231074845243029 ) ) ;
#135466 = ORIENTED_EDGE ( 'NONE', *, *, #142433, .T. ) ;
#135467 = FACE_OUTER_BOUND ( 'NONE', #54962, .T. ) ;
#135468 = ORIENTED_EDGE ( 'NONE', *, *, #193367, .F. ) ;
#135469 = DIRECTION ( 'NONE',  ( -1.000000000000000000, -0.000000000000000000, 0.000000000000000000 ) ) ;
#135470 = ORIENTED_EDGE ( 'NONE', *, *, #150995, .F. ) ;
#135471 = DIRECTION ( 'NONE',  ( 1.000000000000000000, -0.000000000000000000, -0.000000000000000000 ) ) ;
#135472 = SPHERICAL_SURFACE ( 'NONE', #232027, 0.1000000000000000056 ) ;
#135474 = ORIENTED_EDGE ( 'NONE', *, *, #103954, .F. ) ;
#135473 = EDGE_LOOP ( 'NONE', ( #46329, #155419, #54729, #11283 ) ) ;
#135475 = ORIENTED_EDGE ( 'NONE', *, *, #69696, .T. ) ;
#135476 = CARTESIAN_POINT ( 'NONE',  ( -23.49999999999994316, 87.75000000001119815, -43.82310748452479743 ) ) ;
#135477 = ORIENTED_EDGE ( 'NONE', *, *, #95903, .F. ) ;
#135478 = VERTEX_POINT ( 'NONE', #26442 ) ;
#135479 = CARTESIAN_POINT ( 'NONE',  ( 20.94999999999999574, 67.07338541492552508, -195.0514244653012952 ) ) ;
#135481 = VERTEX_POINT ( 'NONE', #8159 ) ;
#135480 = DIRECTION ( 'NONE',  ( 0.000000000000000000, -0.9910827722268041873, 0.1332476588733659539 ) ) ;
#135482 = CARTESIAN_POINT ( 'NONE',  ( 18.59999999999999076, 7.070967871798842452, -37.24656422186831151 ) ) ;
#135484 = CARTESIAN_POINT ( 'NONE',  ( -22.39999999999999858, 12.62988036037870998, -223.4632815780722410 ) ) ;
#135483 = CARTESIAN_POINT ( 'NONE',  ( -18.50000000000000000, 85.50000000001223555, -148.2731074845242460 ) ) ;
#135485 = DIRECTION ( 'NONE',  ( 1.000000000000000000, 0.000000000000000000, 0.000000000000000000 ) ) ;
#135486 = FACE_OUTER_BOUND ( 'NONE', #176517, .T. ) ;
#135487 = CARTESIAN_POINT ( 'NONE',  ( -23.25000000000000000, 76.00000000001244871, -170.0231074845243597 ) ) ;
#135488 = ORIENTED_EDGE ( 'NONE', *, *, #60846, .F. ) ;
#135489 = ORIENTED_EDGE ( 'NONE', *, *, #112028, .T. ) ;
#135490 = CARTESIAN_POINT ( 'NONE',  ( 18.43630871534871218, 85.67980087481485896, -96.36247541654022086 ) ) ;
#135491 = CARTESIAN_POINT ( 'NONE',  ( 18.57071067811864040, 62.96913842657221494, -212.6815504609503762 ) ) ;
#135492 = CARTESIAN_POINT ( 'NONE',  ( -21.05000000000000071, 1.835341550235569663, -179.0551512925629538 ) ) ;
#135493 = EDGE_CURVE ( 'NONE', #26411, #200879, #238874, .T. ) ;
#135494 = AXIS2_PLACEMENT_3D ( 'NONE', #106249, #227493, #107547 ) ;
#135495 = ORIENTED_EDGE ( 'NONE', *, *, #181382, .F. ) ;
#135496 = CARTESIAN_POINT ( 'NONE',  ( -18.50000000000000000, 52.91185528119410719, -244.1460391050142960 ) ) ;
#135497 = CIRCLE ( 'NONE', #118961, 0.1000000000000001860 ) ;
#135498 = CIRCLE ( 'NONE', #106442, 11.65000000000000391 ) ;
#135499 = DIRECTION ( 'NONE',  ( 0.000000000000000000, 0.2128009952263604232, -0.9770955615653316162 ) ) ;
#135500 = ORIENTED_EDGE ( 'NONE', *, *, #94194, .T. ) ;
#135501 = ORIENTED_EDGE ( 'NONE', *, *, #147895, .F. ) ;
#135502 =( BOUNDED_CURVE ( )  B_SPLINE_CURVE ( 3, ( #228571, #70799, #49915, #126895 ),
 .UNSPECIFIED., .F., .T. ) 
 B_SPLINE_CURVE_WITH_KNOTS ( ( 4, 4 ),
 ( 0.3000847527772386725, 0.5517402753107893965 ),
 .UNSPECIFIED. ) 
 CURVE ( )  GEOMETRIC_REPRESENTATION_ITEM ( )  RATIONAL_B_SPLINE_CURVE ( ( 1.000000000000000000, 0.9947294176030464508, 0.9947294176030464508, 1.000000000000000000 ) ) 
 REPRESENTATION_ITEM ( '' )  );
#135503 = CARTESIAN_POINT ( 'NONE',  ( 23.24999999999999645, 29.67396024497139706, -235.8008764811443712 ) ) ;
#135504 = EDGE_CURVE ( 'NONE', #227159, #186480, #9425, .T. ) ;
#135505 = CARTESIAN_POINT ( 'NONE',  ( -21.10000000000000142, 0.000000000000000000, 0.000000000000000000 ) ) ;
#135506 = ORIENTED_EDGE ( 'NONE', *, *, #166314, .T. ) ;
#135507 = CARTESIAN_POINT ( 'NONE',  ( 18.59999999999999432, 0.5663372425336981042, -209.0641885820623997 ) ) ;
#135508 = ORIENTED_EDGE ( 'NONE', *, *, #52376, .F. ) ;
#135509 = DIRECTION ( 'NONE',  ( -0.000000000000000000, -0.000000000000000000, -1.000000000000000000 ) ) ;
#135510 = CARTESIAN_POINT ( 'NONE',  ( -20.64999999999999858, 73.50000000001199396, -116.2477294072864140 ) ) ;
#135512 = CARTESIAN_POINT ( 'NONE',  ( -17.71734398241074260, 65.15764277154693218, -46.29796923151879895 ) ) ;
#135511 = DIRECTION ( 'NONE',  ( 0.000000000000000000, -0.9910827722268055195, 0.1332476588733540468 ) ) ;
#135513 = EDGE_CURVE ( 'NONE', #96344, #172822, #47304, .T. ) ;
#135514 = DIRECTION ( 'NONE',  ( 1.000000000000000000, -0.000000000000000000, -0.000000000000000000 ) ) ;
#135515 = CARTESIAN_POINT ( 'NONE',  ( -18.40000000000000213, 5.650000000011139001, -188.3499999999999659 ) ) ;
#135516 = CARTESIAN_POINT ( 'NONE',  ( 12.25000000000000000, 66.15000000001228386, -153.2731074845244450 ) ) ;
#135517 = AXIS2_PLACEMENT_3D ( 'NONE', #28365, #109127, #184821 ) ;
#135518 =( GEOMETRIC_REPRESENTATION_CONTEXT ( 3 ) GLOBAL_UNCERTAINTY_ASSIGNED_CONTEXT ( ( #253699 ) ) GLOBAL_UNIT_ASSIGNED_CONTEXT ( ( #80301, #60758, #187164 ) ) REPRESENTATION_CONTEXT ( 'NONE', 'WORKASPACE' ) );
#135520 = ORIENTED_EDGE ( 'NONE', *, *, #76943, .F. ) ;
#135519 = ORIENTED_EDGE ( 'NONE', *, *, #80214, .T. ) ;
#135521 = ORIENTED_EDGE ( 'NONE', *, *, #34603, .F. ) ;
#135522 = TOROIDAL_SURFACE ( 'NONE', #106459, 11.65000000000000036, 0.1000000000000000056 ) ;
#135523 = EDGE_CURVE ( 'NONE', #228920, #77088, #222264, .T. ) ;
#135524 = CARTESIAN_POINT ( 'NONE',  ( -16.87331047859651179, 12.41403342719998726, -211.2428889513006993 ) ) ;
#135525 = CARTESIAN_POINT ( 'NONE',  ( -21.05000000000000071, -1.489567864901279792, -194.6304332222954372 ) ) ;
#135527 = EDGE_CURVE ( 'NONE', #173624, #38916, #228496, .T. ) ;
#135526 = DIRECTION ( 'NONE',  ( -1.000000000000000000, -0.000000000000000000, -0.000000000000000000 ) ) ;
#135528 = VECTOR ( 'NONE', #157162, 1000.000000000000000 ) ;
#135529 = CARTESIAN_POINT ( 'NONE',  ( -18.46856557590792391, -9.474215907775336731, -107.6019862408823116 ) ) ;
#135531 = DIRECTION ( 'NONE',  ( 0.000000000000000000, -1.000000000000000000, 0.000000000000000000 ) ) ;
#135530 = CARTESIAN_POINT ( 'NONE',  ( 24.30000000000000071, -12.79999999999999716, -347.0000000000001137 ) ) ;
#135532 = DIRECTION ( 'NONE',  ( 0.000000000000000000, 0.000000000000000000, -1.000000000000000000 ) ) ;
#135533 = EDGE_LOOP ( 'NONE', ( #225884, #191388, #134806, #198192 ) ) ;
#135534 = CIRCLE ( 'NONE', #248163, 0.09999999999999982514 ) ;
#135535 = ADVANCED_FACE ( 'NONE', ( #171124 ), #164413, .T. ) ;
#135536 = CARTESIAN_POINT ( 'NONE',  ( 22.47071067811864609, 68.27992525551361780, -69.62219993922697370 ) ) ;
#135537 = AXIS2_PLACEMENT_3D ( 'NONE', #151441, #113578, #131855 ) ;
#135538 = AXIS2_PLACEMENT_3D ( 'NONE', #142223, #182658, #223043 ) ;
#135539 = EDGE_LOOP ( 'NONE', ( #57128, #54908, #36621, #124822 ) ) ;
#135540 = VERTEX_POINT ( 'NONE', #111099 ) ;
#135541 = CARTESIAN_POINT ( 'NONE',  ( -21.05000000000000071, -9.519327731081284938, -107.4729763765593589 ) ) ;
#135542 = DIRECTION ( 'NONE',  ( -0.000000000000000000, 0.000000000000000000, -1.000000000000000000 ) ) ;
#135543 = CARTESIAN_POINT ( 'NONE',  ( 23.14999999999999858, 5.076932660807364606, -234.1795834024154885 ) ) ;
#135544 = DIRECTION ( 'NONE',  ( 0.000000000000000000, 0.000000000000000000, 1.000000000000000000 ) ) ;
#135545 = VECTOR ( 'NONE', #145072, 1000.000000000000000 ) ;
#135546 = LINE ( 'NONE', #113433, #217191 ) ;
#135547 = VERTEX_POINT ( 'NONE', #12024 ) ;
#135549 = ORIENTED_EDGE ( 'NONE', *, *, #212473, .T. ) ;
#135548 = EDGE_CURVE ( 'NONE', #106243, #251339, #255564, .T. ) ;
#135550 = AXIS2_PLACEMENT_3D ( 'NONE', #141232, #122962, #180363 ) ;
#135551 = DIRECTION ( 'NONE',  ( 0.7070776581708965169, 0.000000000000000000, 0.7071359030027827286 ) ) ;
#135552 = CARTESIAN_POINT ( 'NONE',  ( 19.97071067811864609, 62.37141908057012074, -208.9966201521278037 ) ) ;
#135553 = CARTESIAN_POINT ( 'NONE',  ( -22.47071067811865319, 7.720074744509219933, -33.40090754529740025 ) ) ;
#135554 = LINE ( 'NONE', #53470, #27552 ) ;
#135555 = AXIS2_PLACEMENT_3D ( 'NONE', #20539, #174521, #100020 ) ;
#135556 = CARTESIAN_POINT ( 'NONE',  ( -16.81744102076748959, 9.950000000011138823, -188.3499999999999659 ) ) ;
#135557 = CIRCLE ( 'NONE', #114731, 0.09999999999999939493 ) ;
#135558 = CARTESIAN_POINT ( 'NONE',  ( -23.15000000000000213, 76.00000000001267608, -203.5231074845243597 ) ) ;
#135559 = CARTESIAN_POINT ( 'NONE',  ( 20.27550659511088682, 10.97336462231075416, -208.0769506682813130 ) ) ;
#135561 = DIRECTION ( 'NONE',  ( 1.000000000000000000, 0.000000000000000000, 0.000000000000000000 ) ) ;
#135560 = CARTESIAN_POINT ( 'NONE',  ( -22.46246831459151494, 0.02191216693942996119, 11.64986456120996650 ) ) ;
#135562 = LINE ( 'NONE', #239827, #183206 ) ;
#135563 = ADVANCED_FACE ( 'NONE', ( #177202 ), #196724, .F. ) ;
#135564 = CARTESIAN_POINT ( 'NONE',  ( 23.15000000000000213, 85.60000000001197407, -112.9170766071766820 ) ) ;
#135565 = CARTESIAN_POINT ( 'NONE',  ( 18.59999999999999076, 11.75000000001115907, -175.5999999999999659 ) ) ;
#135566 = CARTESIAN_POINT ( 'NONE',  ( 0.8999999999999993561, -11.75000000000000000, 28.70000000000000284 ) ) ;
#135568 = ORIENTED_EDGE ( 'NONE', *, *, #119760, .T. ) ;
#135567 = CARTESIAN_POINT ( 'NONE',  ( -18.50000000000000000, 64.35000000001247145, -181.7731074845244450 ) ) ;
#135569 = CARTESIAN_POINT ( 'NONE',  ( 20.95035502843362707, 10.47763832678762341, -41.07629970873637859 ) ) ;
#135570 = EDGE_LOOP ( 'NONE', ( #129822, #252205 ) ) ;
#135572 = CIRCLE ( 'NONE', #239644, 0.09999999999998898659 ) ;
#135571 = FACE_OUTER_BOUND ( 'NONE', #148127, .T. ) ;
#135573 = DIRECTION ( 'NONE',  ( 0.000000000000000000, -0.9126074666063545004, -0.4088369013363783999 ) ) ;
#135575 = ORIENTED_EDGE ( 'NONE', *, *, #24902, .F. ) ;
#135574 = AXIS2_PLACEMENT_3D ( 'NONE', #69710, #10997, #72270 ) ;
#135576 = DIRECTION ( 'NONE',  ( 0.000000000000000000, 0.000000000000000000, 1.000000000000000000 ) ) ;
#135577 = CIRCLE ( 'NONE', #160570, 4.041421356237310469 ) ;
#135578 = CARTESIAN_POINT ( 'NONE',  ( 15.39170923737819585, 9.389529397477893724, -84.81710791289373219 ) ) ;
#135579 = CARTESIAN_POINT ( 'NONE',  ( 20.85000000000000142, 78.04167338765999773, -195.9950552943387265 ) ) ;
#135580 = DIRECTION ( 'NONE',  ( 0.000000000000000000, 0.000000000000000000, -1.000000000000000000 ) ) ;
#135581 = CARTESIAN_POINT ( 'NONE',  ( 18.49999999999999289, 10.49142135623730709, -24.74999999999999645 ) ) ;
#135582 = CARTESIAN_POINT ( 'NONE',  ( -23.49999999999994316, 64.25000000001119815, -36.02310748452479316 ) ) ;
#135583 = EDGE_CURVE ( 'NONE', #64123, #932, #2403, .T. ) ;
#135584 = EDGE_CURVE ( 'NONE', #229705, #64043, #89009, .T. ) ;
#135585 = ORIENTED_EDGE ( 'NONE', *, *, #206725, .T. ) ;
#135586 = CARTESIAN_POINT ( 'NONE',  ( 21.05000000000000071, 1.115600667400684642E-11, -67.00000000000004263 ) ) ;
#135588 = ORIENTED_EDGE ( 'NONE', *, *, #197169, .T. ) ;
#135587 = DIRECTION ( 'NONE',  ( 1.000000000000000000, 0.000000000000000000, 0.000000000000000000 ) ) ;
#135589 = CARTESIAN_POINT ( 'NONE',  ( 20.94999999999997442, 77.26327546522965406, -162.1212428177779543 ) ) ;
#135590 = CARTESIAN_POINT ( 'NONE',  ( 20.95512820512820795, 22.89972396243220487, -230.1286587026982033 ) ) ;
#135592 = EDGE_CURVE ( 'NONE', #73858, #257895, #84890, .T. ) ;
#135591 = CARTESIAN_POINT ( 'NONE',  ( -22.50014994443984406, 31.77938584364020258, -238.8622469772241175 ) ) ;
#135594 = EDGE_CURVE ( 'NONE', #33556, #236903, #113958, .T. ) ;
#135593 = CIRCLE ( 'NONE', #23205, 0.09999999999999939493 ) ;
#135595 = ORIENTED_EDGE ( 'NONE', *, *, #232260, .T. ) ;
#135596 = DIRECTION ( 'NONE',  ( 0.000000000000000000, 0.000000000000000000, -1.000000000000000000 ) ) ;
#135597 = CIRCLE ( 'NONE', #10717, 0.09999999999999592548 ) ;
#135598 = SHAPE_DEFINITION_REPRESENTATION ( #107599, #26974 ) ;
#135599 = DIRECTION ( 'NONE',  ( 1.000000000000000000, -2.952720810173289112E-16, -2.061873921506763405E-30 ) ) ;
#135600 = CARTESIAN_POINT ( 'NONE',  ( 23.15000000000000213, -11.74999999998883560, -79.15000000000004832 ) ) ;
#135601 = CIRCLE ( 'NONE', #64695, 0.6000000000000033085 ) ;
#135602 = EDGE_CURVE ( 'NONE', #64951, #17038, #147291, .T. ) ;
#135603 = ORIENTED_EDGE ( 'NONE', *, *, #66136, .T. ) ;
#135604 = DIRECTION ( 'NONE',  ( 0.000000000000000000, -1.000000000000000000, 0.000000000000000000 ) ) ;
#135605 = DIRECTION ( 'NONE',  ( 0.000000000000000000, -0.2128009952267955196, 0.9770955615652368031 ) ) ;
#135606 = EDGE_CURVE ( 'NONE', #68619, #107947, #68180, .T. ) ;
#135608 = EDGE_CURVE ( 'NONE', #247011, #66129, #143170, .T. ) ;
#135607 = EDGE_CURVE ( 'NONE', #35640, #254886, #209844, .T. ) ;
#135609 = CYLINDRICAL_SURFACE ( 'NONE', #28743, 0.1000000000000028644 ) ;
#135610 = ORIENTED_EDGE ( 'NONE', *, *, #71758, .F. ) ;
#135611 = AXIS2_PLACEMENT_3D ( 'NONE', #255987, #223000, #254710 ) ;
#135612 = ORIENTED_EDGE ( 'NONE', *, *, #110, .F. ) ;
#135613 = FACE_OUTER_BOUND ( 'NONE', #121740, .T. ) ;
#135614 = DIRECTION ( 'NONE',  ( -1.000000000000000000, -0.000000000000000000, -0.000000000000000000 ) ) ;
#135615 = LINE ( 'NONE', #215164, #144316 ) ;
#135616 = EDGE_CURVE ( 'NONE', #151457, #56292, #79331, .T. ) ;
#135617 = CARTESIAN_POINT ( 'NONE',  ( -16.87242674293849376, 30.20728960713221767, -234.8075598113715898 ) ) ;
#135618 = SPHERICAL_SURFACE ( 'NONE', #124541, 0.1000000000000000056 ) ;
#135619 = CARTESIAN_POINT ( 'NONE',  ( 20.88420186297724257, 65.66974365629616273, -30.43601455626050978 ) ) ;
#135621 = EDGE_CURVE ( 'NONE', #217587, #68571, #39165, .T. ) ;
#135620 = LINE ( 'NONE', #36578, #56174 ) ;
#135622 = DIRECTION ( 'NONE',  ( 0.000000000000000000, 0.000000000000000000, -1.000000000000000000 ) ) ;
#135624 = EDGE_CURVE ( 'NONE', #107287, #227999, #73292, .T. ) ;
#135623 = DIRECTION ( 'NONE',  ( 1.000000000000000000, 0.000000000000000000, 0.000000000000000000 ) ) ;
#135625 = CIRCLE ( 'NONE', #15418, 0.1000000000000028644 ) ;
#135626 = EDGE_LOOP ( 'NONE', ( #250566, #171141, #217254, #13235, #130135 ) ) ;
#135627 = CIRCLE ( 'NONE', #152236, 0.09999999999998898659 ) ;
#135628 = ORIENTED_EDGE ( 'NONE', *, *, #138512, .T. ) ;
#135629 = AXIS2_PLACEMENT_3D ( 'NONE', #112601, #195997, #192153 ) ;
#135631 = DIRECTION ( 'NONE',  ( 0.000000000000000000, -0.7035695228903320331, -0.7106264324241468033 ) ) ;
#135630 = CIRCLE ( 'NONE', #23239, 11.65000000000000036 ) ;
#135632 = CARTESIAN_POINT ( 'NONE',  ( -17.78241384945712156, 65.14442424720434133, -146.7721451569937585 ) ) ;
#135634 = DIRECTION ( 'NONE',  ( 1.000000000000000000, -0.000000000000000000, 0.000000000000000000 ) ) ;
#135633 = CARTESIAN_POINT ( 'NONE',  ( 23.14999999999999858, 71.00000000001253397, -182.4283735034374843 ) ) ;
#135635 = ADVANCED_FACE ( 'NONE', ( #13291 ), #22413, .T. ) ;
#135636 = DIRECTION ( 'NONE',  ( 1.000000000000000000, 0.000000000000000000, 0.000000000000000000 ) ) ;
#135637 = LINE ( 'NONE', #40439, #195820 ) ;
#135638 = CARTESIAN_POINT ( 'NONE',  ( 12.33938619321247288, 12.83074261044330022, -215.9253900757178428 ) ) ;
#135639 = VERTEX_POINT ( 'NONE', #18087 ) ;
#135640 = EDGE_CURVE ( 'NONE', #31733, #175274, #217557, .T. ) ;
#135641 = ORIENTED_EDGE ( 'NONE', *, *, #77192, .F. ) ;
#135642 = CARTESIAN_POINT ( 'NONE',  ( 20.85000000000000142, 77.13501884592184865, -61.80613060109197932 ) ) ;
#135643 = VERTEX_POINT ( 'NONE', #181037 ) ;
#135644 = CARTESIAN_POINT ( 'NONE',  ( 18.49999999999999289, 64.35000000001191722, -103.0231074845243882 ) ) ;
#135645 = AXIS2_PLACEMENT_3D ( 'NONE', #225945, #145142, #102144 ) ;
#135646 = CARTESIAN_POINT ( 'NONE',  ( 21.14999999999999858, 6.540656951712400691, -167.4999999999999716 ) ) ;
#135647 = AXIS2_PLACEMENT_3D ( 'NONE', #257786, #139146, #97453 ) ;
#135648 = ORIENTED_EDGE ( 'NONE', *, *, #125291, .T. ) ;
#135649 = DIRECTION ( 'NONE',  ( 0.000000000000000000, -0.8814952561688476074, 0.4721928772777262417 ) ) ;
#135650 = VERTEX_POINT ( 'NONE', #118497 ) ;
#135651 = FACE_OUTER_BOUND ( 'NONE', #238653, .T. ) ;
#135652 = DIRECTION ( 'NONE',  ( 1.000000000000000000, 0.000000000000000000, 0.000000000000000000 ) ) ;
#135653 = CARTESIAN_POINT ( 'NONE',  ( -16.93658623642905070, 66.01961832835493738, -123.9112047553951328 ) ) ;
#135654 = DIRECTION ( 'NONE',  ( 0.000000000000000000, 0.9126074666063660468, 0.4088369013363524762 ) ) ;
#135655 = CARTESIAN_POINT ( 'NONE',  ( 21.05000000000000426, 65.48742650828103251, -241.9089677661080771 ) ) ;
#135657 = FACE_OUTER_BOUND ( 'NONE', #185927, .T. ) ;
#135656 = DIRECTION ( 'NONE',  ( 0.000000000000000000, -0.8660254037844420383, 0.4999999999999943379 ) ) ;
#135658 = CARTESIAN_POINT ( 'NONE',  ( -16.88783316861802319, 66.05000000001224691, -149.2753715265037044 ) ) ;
#135659 = VERTEX_POINT ( 'NONE', #152831 ) ;
#135661 = DIRECTION ( 'NONE',  ( 0.000000000000000000, 0.9394191166662618775, 0.3427706569150580362 ) ) ;
#135660 = FACE_OUTER_BOUND ( 'NONE', #247869, .T. ) ;
#135662 = ORIENTED_EDGE ( 'NONE', *, *, #272, .F. ) ;
#135664 = ORIENTED_EDGE ( 'NONE', *, *, #228823, .F. ) ;
#135663 = CARTESIAN_POINT ( 'NONE',  ( -21.05000000000000071, 5.265981236333565222E-16, 4.299999999999956302 ) ) ;
#135665 = AXIS2_PLACEMENT_3D ( 'NONE', #211502, #108547, #250612 ) ;
#135666 = ORIENTED_EDGE ( 'NONE', *, *, #80247, .F. ) ;
#135667 = TOROIDAL_SURFACE ( 'NONE', #1816, 2.100000000000002309, 0.1000000000000000056 ) ;
#135668 = DIRECTION ( 'NONE',  ( -0.000000000000000000, -6.982962677686266711E-15, 1.000000000000000000 ) ) ;
#135669 = DIRECTION ( 'NONE',  ( 1.000000000000000000, -0.000000000000000000, -0.000000000000000000 ) ) ;
#135670 = CARTESIAN_POINT ( 'NONE',  ( -21.04999999999999716, 30.84067272007213134, -252.2516193862038278 ) ) ;
#135671 = CARTESIAN_POINT ( 'NONE',  ( -16.91256925476570672, 22.89123816192538285, -230.8480166193616867 ) ) ;
#135672 = ORIENTED_EDGE ( 'NONE', *, *, #217706, .F. ) ;
#135673 = DIRECTION ( 'NONE',  ( 0.000000000000000000, -6.938893903907222067E-15, 1.000000000000000000 ) ) ;
#135674 = CYLINDRICAL_SURFACE ( 'NONE', #143913, 11.79999999999999361 ) ;
#135675 = ORIENTED_EDGE ( 'NONE', *, *, #153904, .T. ) ;
#135676 = DIRECTION ( 'NONE',  ( -1.000000000000000000, 1.207181226542539700E-16, -2.694675058168174199E-16 ) ) ;
#135677 = EDGE_CURVE ( 'NONE', #206022, #238213, #19384, .T. ) ;
#135679 = VECTOR ( 'NONE', #27441, 1000.000000000000000 ) ;
#135678 = DIRECTION ( 'NONE',  ( -1.000000000000000000, -0.000000000000000000, -0.000000000000000000 ) ) ;
#135680 = ORIENTED_EDGE ( 'NONE', *, *, #202062, .T. ) ;
#135681 = ORIENTED_EDGE ( 'NONE', *, *, #227957, .F. ) ;
#135682 = EDGE_CURVE ( 'NONE', #235224, #257030, #234772, .T. ) ;
#135684 = CARTESIAN_POINT ( 'NONE',  ( -16.90202395485531639, 9.965944544560510820, -188.4030137212579916 ) ) ;
#135683 = PRESENTATION_LAYER_ASSIGNMENT (  '', '', ( #118587 ) ) ;
#135685 = AXIS2_PLACEMENT_3D ( 'NONE', #190142, #91029, #106719 ) ;
#135686 = CIRCLE ( 'NONE', #239758, 0.09999999999999395484 ) ;
#135687 = ORIENTED_EDGE ( 'NONE', *, *, #189191, .T. ) ;
#135688 = CARTESIAN_POINT ( 'NONE',  ( 21.05000000000000071, 5.400000000011154988, -191.1060308773475072 ) ) ;
#135689 = EDGE_LOOP ( 'NONE', ( #193529, #133734, #183939, #240259 ) ) ;
#135690 = CARTESIAN_POINT ( 'NONE',  ( 20.02499999999999858, 14.02742277431099538, -219.5907614236512870 ) ) ;
#135691 = PRESENTATION_LAYER_ASSIGNMENT (  '', '', ( #160686 ) ) ;
#135692 = ADVANCED_FACE ( 'NONE', ( #2362 ), #191085, .T. ) ;
#135693 = EDGE_CURVE ( 'NONE', #24027, #41411, #161479, .T. ) ;
#135694 = DIRECTION ( 'NONE',  ( -1.000000000000000000, -0.000000000000000000, -0.000000000000000000 ) ) ;
#135695 = DIRECTION ( 'NONE',  ( 1.000000000000000000, -0.000000000000000000, -0.000000000000000000 ) ) ;
#135696 = CARTESIAN_POINT ( 'NONE',  ( -23.15000000000000213, 1.115600667400684642E-11, -100.5000000000000284 ) ) ;
#135697 = CARTESIAN_POINT ( 'NONE',  ( -18.50000000000000000, 78.21362219944489880, -231.2727646510690533 ) ) ;
#135698 = CARTESIAN_POINT ( 'NONE',  ( 18.41832399655378083, -9.682403266662738872, -73.65684362002765795 ) ) ;
#135699 = DIRECTION ( 'NONE',  ( 0.7071067811865474617, 0.3338907855510734324, 0.6233112732207618523 ) ) ;
#135700 = ORIENTED_EDGE ( 'NONE', *, *, #143648, .T. ) ;
#135702 = LINE ( 'NONE', #17078, #73091 ) ;
#135701 = FACE_OUTER_BOUND ( 'NONE', #70260, .T. ) ;
#135703 = CIRCLE ( 'NONE', #23323, 11.80000000000000426 ) ;
#135704 = ORIENTED_EDGE ( 'NONE', *, *, #139781, .T. ) ;
#135707 = ORIENTED_EDGE ( 'NONE', *, *, #139614, .T. ) ;
#135706 = DIRECTION ( 'NONE',  ( 0.000000000000000000, 0.000000000000000000, 1.000000000000000000 ) ) ;
#135705 = CARTESIAN_POINT ( 'NONE',  ( 18.59999999999999076, 0.000000000000000000, -33.50000000000000000 ) ) ;
#135708 = COLOUR_RGB ( '', 0.40784314, 0.44705882, 0.49803922) ;
#135709 = EDGE_CURVE ( 'NONE', #32814, #204362, #126624, .T. ) ;
#135710 = ORIENTED_EDGE ( 'NONE', *, *, #213017, .F. ) ;
#135711 = DIRECTION ( 'NONE',  ( -0.000000000000000000, 1.000000000000000000, 6.982962677686266711E-15 ) ) ;
#135713 = EDGE_CURVE ( 'NONE', #129684, #121951, #184860, .T. ) ;
#135712 = AXIS2_PLACEMENT_3D ( 'NONE', #180640, #22872, #59362 ) ;
#135714 = DIRECTION ( 'NONE',  ( 1.000000000000000000, 0.000000000000000000, 0.000000000000000000 ) ) ;
#135715 = DIRECTION ( 'NONE',  ( 0.000000000000000000, 0.000000000000000000, 1.000000000000000000 ) ) ;
#135716 = CARTESIAN_POINT ( 'NONE',  ( -21.05000000000000071, 64.35000000001208775, -129.7392418215462158 ) ) ;
#135717 = ORIENTED_EDGE ( 'NONE', *, *, #161592, .T. ) ;
#135719 = ORIENTED_EDGE ( 'NONE', *, *, #176296, .T. ) ;
#135718 = CARTESIAN_POINT ( 'NONE',  ( -18.69999999999999929, 1.350000000000000089, 22.10000000000000142 ) ) ;
#135720 = VECTOR ( 'NONE', #21211, 1000.000000000000000 ) ;
#135721 = AXIS2_PLACEMENT_3D ( 'NONE', #64818, #85632, #89509 ) ;
#135723 = CARTESIAN_POINT ( 'NONE',  ( 20.95462737510932882, 10.55678195164374067, -7.569950056562293916 ) ) ;
#135722 = DIRECTION ( 'NONE',  ( -0.000000000000000000, -0.2617529984165031243, -0.9651348961777157509 ) ) ;
#135724 = CIRCLE ( 'NONE', #56581, 7.900000000000000355 ) ;
#135726 = ORIENTED_EDGE ( 'NONE', *, *, #105404, .F. ) ;
#135725 = FACE_OUTER_BOUND ( 'NONE', #158253, .T. ) ;
#135727 = EDGE_CURVE ( 'NONE', #141149, #206737, #72474, .T. ) ;
#135728 = ORIENTED_EDGE ( 'NONE', *, *, #215397, .F. ) ;
#135729 = EDGE_CURVE ( 'NONE', #1224, #176884, #84434, .T. ) ;
#135730 = CARTESIAN_POINT ( 'NONE',  ( -23.15000000000000213, 2.000000000011154189, -154.2753780772379173 ) ) ;
#135731 = AXIS2_PLACEMENT_3D ( 'NONE', #248689, #171749, #70076 ) ;
#135732 = CARTESIAN_POINT ( 'NONE',  ( 0.8999999999999993561, -11.65000000000000036, 28.70000000000000284 ) ) ;
#135733 = ORIENTED_EDGE ( 'NONE', *, *, #37696, .T. ) ;
#135734 = DIRECTION ( 'NONE',  ( 0.000000000000000000, 6.982962677686266711E-15, -1.000000000000000000 ) ) ;
#135735 = ORIENTED_EDGE ( 'NONE', *, *, #239391, .T. ) ;
#135736 = AXIS2_PLACEMENT_3D ( 'NONE', #55090, #216758, #62826 ) ;
#135737 = DIRECTION ( 'NONE',  ( -1.000000000000000000, 0.000000000000000000, 0.000000000000000000 ) ) ;
#135738 = DIRECTION ( 'NONE',  ( 1.000000000000000000, 0.000000000000000000, 0.000000000000000000 ) ) ;
#135739 = TOROIDAL_SURFACE ( 'NONE', #89949, 11.65000000000000036, 0.1000000000000000056 ) ;
#135741 = VERTEX_POINT ( 'NONE', #222692 ) ;
#135740 = VECTOR ( 'NONE', #90055, 1000.000000000000000 ) ;
#135742 = EDGE_CURVE ( 'NONE', #48831, #6502, #213924, .T. ) ;
#135743 = DIRECTION ( 'NONE',  ( 1.000000000000000000, 0.000000000000000000, 0.000000000000000000 ) ) ;
#135744 = EDGE_CURVE ( 'NONE', #184180, #79953, #145727, .T. ) ;
#135745 = EDGE_CURVE ( 'NONE', #108629, #251339, #105748, .T. ) ;
#135746 = FACE_OUTER_BOUND ( 'NONE', #207545, .T. ) ;
#135747 = ORIENTED_EDGE ( 'NONE', *, *, #34380, .F. ) ;
#135748 = EDGE_LOOP ( 'NONE', ( #257294, #11347, #106690, #6544 ) ) ;
#135749 = CARTESIAN_POINT ( 'NONE',  ( 20.58091095332355280, 18.80829090936573778, -229.7581893066683278 ) ) ;
#135750 = VERTEX_POINT ( 'NONE', #242262 ) ;
#135751 = ORIENTED_EDGE ( 'NONE', *, *, #184861, .T. ) ;
#135753 = ORIENTED_EDGE ( 'NONE', *, *, #64746, .T. ) ;
#135752 = DIRECTION ( 'NONE',  ( -0.000000000000000000, -0.4791956752371546724, -0.8777080977375153470 ) ) ;
#135754 =( REPRESENTATION_RELATIONSHIP ('NONE','NONE', #36900, #170171 ) REPRESENTATION_RELATIONSHIP_WITH_TRANSFORMATION ( #230567 )SHAPE_REPRESENTATION_RELATIONSHIP( ) );
#135755 = EDGE_CURVE ( 'NONE', #239290, #132343, #186156, .T. ) ;
#135756 = VERTEX_POINT ( 'NONE', #183592 ) ;
#135757 = AXIS2_PLACEMENT_3D ( 'NONE', #155003, #18025, #59697 ) ;
#135758 = DIRECTION ( 'NONE',  ( 0.000000000000000000, 0.000000000000000000, 1.000000000000000000 ) ) ;
#135759 = CIRCLE ( 'NONE', #56464, 0.9000000000000014655 ) ;
#135762 = ORIENTED_EDGE ( 'NONE', *, *, #155446, .T. ) ;
#135761 = VERTEX_POINT ( 'NONE', #85727 ) ;
#135760 = CARTESIAN_POINT ( 'NONE',  ( 23.25000000000000000, 23.40438595358394736, -253.3416554127419431 ) ) ;
#135763 = ADVANCED_FACE ( 'NONE', ( #63635 ), #243554, .T. ) ;
#135764 = VECTOR ( 'NONE', #198059, 1000.000000000000000 ) ;
#135765 = AXIS2_PLACEMENT_3D ( 'NONE', #252153, #132222, #193494 ) ;
#135766 = ORIENTED_EDGE ( 'NONE', *, *, #214676, .F. ) ;
#135767 = CARTESIAN_POINT ( 'NONE',  ( -23.15000000000000213, 64.25000000001199396, -115.1731074845243796 ) ) ;
#135768 = LINE ( 'NONE', #191941, #42563 ) ;
#135769 = ORIENTED_EDGE ( 'NONE', *, *, #4276, .T. ) ;
#135770 = DIRECTION ( 'NONE',  ( -1.836970198721029934E-16, -1.000000000000000000, -6.982962677686266711E-15 ) ) ;
#135771 = EDGE_CURVE ( 'NONE', #216625, #74147, #3655, .T. ) ;
#135773 = VERTEX_POINT ( 'NONE', #83159 ) ;
#135772 = FACE_OUTER_BOUND ( 'NONE', #194564, .T. ) ;
#135774 = CARTESIAN_POINT ( 'NONE',  ( 20.94999999999999929, 70.50000000001180922, -81.92837350343744163 ) ) ;
#135775 = ORIENTED_EDGE ( 'NONE', *, *, #154041, .T. ) ;
#135776 = AXIS2_PLACEMENT_3D ( 'NONE', #134529, #217915, #197080 ) ;
#135777 = ORIENTED_EDGE ( 'NONE', *, *, #85801, .F. ) ;
#135778 = SURFACE_STYLE_USAGE ( .BOTH. , #180066 ) ;
#135779 = VECTOR ( 'NONE', #83918, 1000.000000000000000 ) ;
#135780 = EDGE_LOOP ( 'NONE', ( #126234, #250292, #182111, #149579 ) ) ;
#135781 = EDGE_LOOP ( 'NONE', ( #185905, #137717, #81882, #251054 ) ) ;
#135782 = CARTESIAN_POINT ( 'NONE',  ( -16.93440969289731157, 9.995185175825108459, -180.0912341850107623 ) ) ;
#135783 = DIRECTION ( 'NONE',  ( -1.000000000000000000, 2.952720810173289112E-16, 2.061873921506763405E-30 ) ) ;
#135785 = ORIENTED_EDGE ( 'NONE', *, *, #107150, .F. ) ;
#135784 = VERTEX_POINT ( 'NONE', #143154 ) ;
#135786 = ORIENTED_EDGE ( 'NONE', *, *, #151015, .T. ) ;
#135787 = DIRECTION ( 'NONE',  ( 0.000000000000000000, 0.2617529984164506107, 0.9651348961777299618 ) ) ;
#135788 = VERTEX_POINT ( 'NONE', #203147 ) ;
#135789 = ORIENTED_EDGE ( 'NONE', *, *, #40839, .T. ) ;
#135790 = LINE ( 'NONE', #173705, #46636 ) ;
#135791 = AXIS2_PLACEMENT_3D ( 'NONE', #10073, #28396, #89597 ) ;
#135792 = EDGE_LOOP ( 'NONE', ( #207271, #78607, #241336, #135610 ) ) ;
#135793 = CARTESIAN_POINT ( 'NONE',  ( -16.93970660449832621, 12.45464092817497814, -211.1340361583801268 ) ) ;
#135795 = DIRECTION ( 'NONE',  ( -0.000000000000000000, -6.982962677686266711E-15, 1.000000000000000000 ) ) ;
#135794 = CYLINDRICAL_SURFACE ( 'NONE', #152879, 0.1000000000000028644 ) ;
#135796 = ORIENTED_EDGE ( 'NONE', *, *, #142649, .T. ) ;
#135797 = ORIENTED_EDGE ( 'NONE', *, *, #237285, .T. ) ;
#135798 = DIRECTION ( 'NONE',  ( 5.421010862427554711E-16, -1.000000000000000000, -3.252606517456533024E-15 ) ) ;
#135799 = EDGE_LOOP ( 'NONE', ( #222032, #157844, #123216, #167352 ) ) ;
#135800 = AXIS2_PLACEMENT_3D ( 'NONE', #130419, #208702, #53461 ) ;
#135801 = CIRCLE ( 'NONE', #202459, 0.09999999999999982514 ) ;
#135802 = CIRCLE ( 'NONE', #65089, 0.2000000000000057288 ) ;
#135803 = VECTOR ( 'NONE', #50838, 1000.000000000000000 ) ;
#135804 = DIRECTION ( 'NONE',  ( -1.000000000000000000, 0.000000000000000000, 0.000000000000000000 ) ) ;
#135805 = ORIENTED_EDGE ( 'NONE', *, *, #132005, .F. ) ;
#135806 = EDGE_LOOP ( 'NONE', ( #142768, #194770, #187003, #16893 ) ) ;
#135807 = DIRECTION ( 'NONE',  ( 0.000000000000000000, 0.9126074666063772600, 0.4088369013363273852 ) ) ;
#135808 = ADVANCED_FACE ( 'NONE', ( #104019 ), #159765, .T. ) ;
#135810 = ORIENTED_EDGE ( 'NONE', *, *, #74370, .T. ) ;
#135809 = CARTESIAN_POINT ( 'NONE',  ( 18.54147908293606406, 85.46326165794057772, -162.9741585877686987 ) ) ;
#135811 = DIRECTION ( 'NONE',  ( -1.000000000000000000, 0.000000000000000000, -0.000000000000000000 ) ) ;
#135812 = DIRECTION ( 'NONE',  ( -1.000000000000000000, -0.000000000000000000, -0.000000000000000000 ) ) ;
#135813 = ORIENTED_EDGE ( 'NONE', *, *, #215503, .F. ) ;
#135814 = CARTESIAN_POINT ( 'NONE',  ( -21.37071067811865532, 8.070710678129811910, -155.1500000000000057 ) ) ;
#135815 = CARTESIAN_POINT ( 'NONE',  ( 18.49999999999999289, 33.89981536720674171, -236.1713368690715527 ) ) ;
#135816 = CARTESIAN_POINT ( 'NONE',  ( 18.39999999999999503, 11.47316190337363828, -46.15000000000000568 ) ) ;
#135817 = DIRECTION ( 'NONE',  ( 0.000000000000000000, -0.2128009952263601456, 0.9770955615653316162 ) ) ;
#135818 = EDGE_CURVE ( 'NONE', #7171, #24438, #243142, .T. ) ;
#135819 = DIRECTION ( 'NONE',  ( 0.000000000000000000, -0.8814952561688429444, 0.4721928772777345684 ) ) ;
#135821 = EDGE_CURVE ( 'NONE', #192117, #253488, #51571, .T. ) ;
#135820 = CARTESIAN_POINT ( 'NONE',  ( -20.85000000000000142, 1.115600667400684642E-11, -167.5000000000000284 ) ) ;
#135822 = CARTESIAN_POINT ( 'NONE',  ( -16.87683809663752399, 66.15000000001225544, -149.9254715027207396 ) ) ;
#135823 = CARTESIAN_POINT ( 'NONE',  ( -23.25000000000000000, 0.000000000000000000, -37.40000000000000568 ) ) ;
#135824 = FACE_OUTER_BOUND ( 'NONE', #184217, .T. ) ;
#135825 = AXIS2_PLACEMENT_3D ( 'NONE', #131730, #230856, #211272 ) ;
#135826 = AXIS2_PLACEMENT_3D ( 'NONE', #223104, #82287, #161883 ) ;
#135827 = ORIENTED_EDGE ( 'NONE', *, *, #28942, .F. ) ;
#135829 = VERTEX_POINT ( 'NONE', #119325 ) ;
#135828 = VERTEX_POINT ( 'NONE', #37230 ) ;
#135830 = CIRCLE ( 'NONE', #169194, 12.87499999999999822 ) ;
#135831 = VERTEX_POINT ( 'NONE', #3203 ) ;
#135832 = EDGE_CURVE ( 'NONE', #224073, #122696, #139061, .T. ) ;
#135833 = CARTESIAN_POINT ( 'NONE',  ( -21.13498764882296044, 0.001656394742484908677, -94.00438185652609491 ) ) ;
#135834 = CYLINDRICAL_SURFACE ( 'NONE', #123634, 0.09999999999999939493 ) ;
#135836 = CYLINDRICAL_SURFACE ( 'NONE', #48909, 11.75000000000001066 ) ;
#135835 = DIRECTION ( 'NONE',  ( 2.879366945564059217E-14, -0.9875055080513751582, 0.1575844902526747915 ) ) ;
#135837 = ORIENTED_EDGE ( 'NONE', *, *, #120799, .F. ) ;
#135838 = DIRECTION ( 'NONE',  ( 2.952720810173288619E-16, -1.000000000000000000, 0.000000000000000000 ) ) ;
#135839 = FACE_OUTER_BOUND ( 'NONE', #239118, .T. ) ;
#135840 = CARTESIAN_POINT ( 'NONE',  ( -16.88219499860498374, 9.950206425438745228, -180.1493096901072875 ) ) ;
#135841 = CYLINDRICAL_SURFACE ( 'NONE', #241404, 0.09999999999999939493 ) ;
#135842 = ORIENTED_EDGE ( 'NONE', *, *, #104091, .F. ) ;
#135843 = EDGE_LOOP ( 'NONE', ( #126797, #82734, #104957 ) ) ;
#135844 = VECTOR ( 'NONE', #151233, 1000.000000000000000 ) ;
#135845 = DIRECTION ( 'NONE',  ( 0.000000000000000000, -1.000000000000000000, 0.000000000000000000 ) ) ;
#135846 = VERTEX_POINT ( 'NONE', #116747 ) ;
#135847 = EDGE_CURVE ( 'NONE', #205356, #83334, #239055, .T. ) ;
#135848 = DIRECTION ( 'NONE',  ( 1.000000000000000000, -0.000000000000000000, -0.000000000000000000 ) ) ;
#135849 = LINE ( 'NONE', #4996, #85500 ) ;
#135850 = ADVANCED_FACE ( 'NONE', ( #38508 ), #158476, .T. ) ;
#135851 = CARTESIAN_POINT ( 'NONE',  ( 23.14999999999999503, 6.650000000011155876, -112.7500000000000284 ) ) ;
#135852 = CARTESIAN_POINT ( 'NONE',  ( 20.90000000000000213, -1.885425182446133885, -11.59641995933507808 ) ) ;
#135853 = CARTESIAN_POINT ( 'NONE',  ( -20.85000000000000142, 79.19526988099229925, -196.1889237952725296 ) ) ;
#135854 = VERTEX_POINT ( 'NONE', #141444 ) ;
#135855 = DIRECTION ( 'NONE',  ( -1.000000000000000000, 2.952720810173289112E-16, 2.061873921506763405E-30 ) ) ;
#135856 = LINE ( 'NONE', #35532, #39207 ) ;
#135857 = LINE ( 'NONE', #66620, #58421 ) ;
#135859 = CARTESIAN_POINT ( 'NONE',  ( -21.64999999999999858, 66.65000000001261071, -190.8731074845244393 ) ) ;
#135858 = DIRECTION ( 'NONE',  ( 0.000000000000000000, 0.000000000000000000, 1.000000000000000000 ) ) ;
#135860 = CARTESIAN_POINT ( 'NONE',  ( -20.64999999999999858, 68.75000000001260503, -191.2731074845244166 ) ) ;
#135861 = EDGE_CURVE ( 'NONE', #16840, #213344, #93297, .T. ) ;
#135862 = VECTOR ( 'NONE', #233476, 1000.000000000000000 ) ;
#135863 = CARTESIAN_POINT ( 'NONE',  ( 21.72449340488910252, 23.13575923509592513, -230.6406825367463966 ) ) ;
#135864 = DIRECTION ( 'NONE',  ( 0.000000000000000000, 0.9126074666063773710, 0.4088369013363272741 ) ) ;
#135865 = DIRECTION ( 'NONE',  ( 0.000000000000000000, 0.1335171055202867274, -0.9910465087640866200 ) ) ;
#135866 = AXIS2_PLACEMENT_3D ( 'NONE', #155850, #114121, #132419 ) ;
#135867 = ORIENTED_EDGE ( 'NONE', *, *, #127372, .T. ) ;
#135868 = AXIS2_PLACEMENT_3D ( 'NONE', #192886, #152495, #91216 ) ;
#135869 = VERTEX_POINT ( 'NONE', #17636 ) ;
#135870 = DIRECTION ( 'NONE',  ( 0.000000000000000000, -1.000000000000000000, 0.000000000000000000 ) ) ;
#135871 = VERTEX_POINT ( 'NONE', #77594 ) ;
#135872 = DIRECTION ( 'NONE',  ( 1.000000000000000000, 0.000000000000000000, 0.000000000000000000 ) ) ;
#135873 = EDGE_CURVE ( 'NONE', #111909, #211794, #121904, .T. ) ;
#135874 = B_SPLINE_CURVE_WITH_KNOTS ( 'NONE', 3,
 ( #141448, #44930, #206569, #240560, #82728, #203992, #4498 ),
 .UNSPECIFIED., .F., .F.,
 ( 4, 3, 4 ),
 ( 0.000000000000000000, 0.0009834301579439998740, 0.001767853679402675614 ),
 .UNSPECIFIED. ) ;
#135875 = DIRECTION ( 'NONE',  ( 0.000000000000000000, 0.000000000000000000, 1.000000000000000000 ) ) ;
#135876 = VECTOR ( 'NONE', #64410, 1000.000000000000000 ) ;
#135877 = EDGE_LOOP ( 'NONE', ( #115235, #90963, #51167, #22906, #28053 ) ) ;
#135878 = CARTESIAN_POINT ( 'NONE',  ( 21.12230431290520016, 0.005209851700173377329, -161.0424333467069573 ) ) ;
#135879 = AXIS2_PLACEMENT_3D ( 'NONE', #209486, #206927, #128685 ) ;
#135880 = DIRECTION ( 'NONE',  ( 1.000000000000000000, 0.000000000000000000, 0.000000000000000000 ) ) ;
#135881 = CARTESIAN_POINT ( 'NONE',  ( 23.25000000000000000, -11.74999999998883560, -79.15000000000004832 ) ) ;
#135882 = EDGE_CURVE ( 'NONE', #123921, #239471, #198850, .T. ) ;
#135883 = DIRECTION ( 'NONE',  ( 0.000000000000000000, 0.000000000000000000, -1.000000000000000000 ) ) ;
#135886 = VERTEX_POINT ( 'NONE', #120626 ) ;
#135885 = LINE ( 'NONE', #53805, #225892 ) ;
#135884 = AXIS2_PLACEMENT_3D ( 'NONE', #254323, #234783, #114833 ) ;
#135887 = CARTESIAN_POINT ( 'NONE',  ( 19.97071067811865674, 11.72071067812981937, -192.1499999999999488 ) ) ;
#135888 = CARTESIAN_POINT ( 'NONE',  ( 18.49999999999999645, 1.115600667400684642E-11, -33.50000000000000000 ) ) ;
#135889 = DIRECTION ( 'NONE',  ( 1.000000000000000000, 0.000000000000000000, 0.000000000000000000 ) ) ;
#135890 = AXIS2_PLACEMENT_3D ( 'NONE', #237049, #19285, #257838 ) ;
#135891 = CARTESIAN_POINT ( 'NONE',  ( -19.99999999999999645, 5.454087299794354138, 16.60000000000000142 ) ) ;
#135893 = EDGE_CURVE ( 'NONE', #188307, #238064, #222457, .T. ) ;
#135892 = CARTESIAN_POINT ( 'NONE',  ( -21.05000000000000071, 0.2561057921033771945, -33.46510355832771211 ) ) ;
#135894 = ADVANCED_FACE ( 'NONE', ( #118032 ), #162315, .F. ) ;
#135896 = ORIENTED_EDGE ( 'NONE', *, *, #137352, .F. ) ;
#135895 = AXIS2_PLACEMENT_3D ( 'NONE', #175312, #254765, #50177 ) ;
#135897 = DIRECTION ( 'NONE',  ( 1.000000000000000000, 0.000000000000000000, 0.000000000000000000 ) ) ;
#135898 = FACE_OUTER_BOUND ( 'NONE', #149271, .T. ) ;
#135899 = ORIENTED_EDGE ( 'NONE', *, *, #87112, .F. ) ;
#135900 = DIRECTION ( 'NONE',  ( -1.073024830501117725E-15, -6.982962677686266711E-15, 1.000000000000000000 ) ) ;
#135901 = EDGE_LOOP ( 'NONE', ( #150501, #73265, #41425, #188500 ) ) ;
#135902 = EDGE_CURVE ( 'NONE', #44729, #167145, #151781, .T. ) ;
#135903 = CIRCLE ( 'NONE', #119174, 0.9750000000000036415 ) ;
#135904 = DIRECTION ( 'NONE',  ( 0.000000000000000000, -0.2617529984165031243, -0.9651348961777157509 ) ) ;
#135905 = ADVANCED_FACE ( 'NONE', ( #256189 ), #214116, .T. ) ;
#135906 = CIRCLE ( 'NONE', #173392, 0.09999999999999939493 ) ;
#135907 = AXIS2_PLACEMENT_3D ( 'NONE', #15385, #139129, #213557 ) ;
#135908 = DIRECTION ( 'NONE',  ( 1.000000000000000000, 0.000000000000000000, 0.000000000000000000 ) ) ;
#135909 = DIRECTION ( 'NONE',  ( 0.000000000000000000, -1.000000000000000000, 0.000000000000000000 ) ) ;
#135910 = ORIENTED_EDGE ( 'NONE', *, *, #6350, .F. ) ;
#135911 = ADVANCED_FACE ( 'NONE', ( #239273 ), #157190, .T. ) ;
#135912 = CIRCLE ( 'NONE', #160890, 4.049999999999998046 ) ;
#135913 = ORIENTED_EDGE ( 'NONE', *, *, #99180, .F. ) ;
#135914 = DIRECTION ( 'NONE',  ( 2.557131231893037478E-16, -0.8660254037844385966, 0.5000000000000003331 ) ) ;
#135915 = DIRECTION ( 'NONE',  ( 0.000000000000000000, -0.8660254037844384856, 0.5000000000000003331 ) ) ;
#135916 = ADVANCED_FACE ( 'NONE', ( #98423 ), #140146, .T. ) ;
#135917 = CARTESIAN_POINT ( 'NONE',  ( 18.39999999999999858, 77.26488334054519669, -241.9697969554615611 ) ) ;
#135918 = DIRECTION ( 'NONE',  ( 3.265361837132813093E-16, 1.000000000000000000, 6.982962677686266711E-15 ) ) ;
#135920 = SPHERICAL_SURFACE ( 'NONE', #36913, 0.1000000000000000056 ) ;
#135919 = DIRECTION ( 'NONE',  ( 0.000000000000000000, 1.000000000000000000, 6.982962677686266711E-15 ) ) ;
#135921 = DIRECTION ( 'NONE',  ( 0.000000000000000000, 1.000000000000000000, 0.000000000000000000 ) ) ;
#135923 = EDGE_CURVE ( 'NONE', #66229, #249247, #102285, .T. ) ;
#135922 = CARTESIAN_POINT ( 'NONE',  ( 21.05000000000000071, 65.27628288308574156, -90.84686788338628105 ) ) ;
#135925 = EDGE_CURVE ( 'NONE', #10431, #91860, #139249, .T. ) ;
#135924 = DIRECTION ( 'NONE',  ( 1.000000000000000000, 0.000000000000000000, 0.000000000000000000 ) ) ;
#135926 = ORIENTED_EDGE ( 'NONE', *, *, #224798, .T. ) ;
#135927 = CARTESIAN_POINT ( 'NONE',  ( -18.50000000000000000, -9.499999999988849808, -41.60000000000000142 ) ) ;
#135929 = VERTEX_POINT ( 'NONE', #203987 ) ;
#135928 = DIRECTION ( 'NONE',  ( 2.952720810173289112E-16, 1.000000000000000000, -6.088138035986627436E-46 ) ) ;
#135930 = DIRECTION ( 'NONE',  ( 1.000000000000000000, 7.304098846218134667E-16, -0.000000000000000000 ) ) ;
#135931 = DIRECTION ( 'NONE',  ( 1.000000000000000000, 7.492892343619937423E-30, -1.073024830501117725E-15 ) ) ;
#135933 = CARTESIAN_POINT ( 'NONE',  ( -21.14999999999999858, 65.61575147395463148, -242.1939180743342774 ) ) ;
#135932 = LINE ( 'NONE', #175131, #17675 ) ;
#135934 = ADVANCED_FACE ( 'NONE', ( #4494 ), #146565, .T. ) ;
#135935 = EDGE_LOOP ( 'NONE', ( #153427, #43176, #83364, #201383 ) ) ;
#135937 = CARTESIAN_POINT ( 'NONE',  ( -18.40000000000000213, 11.47316190337364183, -57.67405393319205587 ) ) ;
#135936 = CARTESIAN_POINT ( 'NONE',  ( -23.25000000000000000, 0.000000000000000000, -33.50000000000000000 ) ) ;
#135938 = DIRECTION ( 'NONE',  ( 2.952720810173289112E-16, 1.000000000000000000, 6.938893903907222067E-15 ) ) ;
#135939 = DIRECTION ( 'NONE',  ( -1.000000000000000000, -9.458662978381124901E-16, 5.066746821047763994E-16 ) ) ;
#135940 = CARTESIAN_POINT ( 'NONE',  ( -23.15000000000000213, 64.25000000001277556, -215.2731074845244450 ) ) ;
#135941 = CARTESIAN_POINT ( 'NONE',  ( -18.59999999999999787, 85.48068669529084218, -96.08199231576638510 ) ) ;
#135942 = VERTEX_POINT ( 'NONE', #103583 ) ;
#135943 = CARTESIAN_POINT ( 'NONE',  ( 18.49999999999998934, 69.55000000001159322, -59.50608031408435039 ) ) ;
#135944 = EDGE_CURVE ( 'NONE', #60871, #85465, #18483, .T. ) ;
#135945 = AXIS2_PLACEMENT_3D ( 'NONE', #54264, #215895, #178098 ) ;
#135946 = ORIENTED_EDGE ( 'NONE', *, *, #168727, .T. ) ;
#135947 = EDGE_CURVE ( 'NONE', #5552, #168403, #244394, .T. ) ;
#135948 = AXIS2_PLACEMENT_3D ( 'NONE', #42747, #124856, #45315 ) ;
#135949 = AXIS2_PLACEMENT_3D ( 'NONE', #69500, #210285, #73361 ) ;
#135950 = AXIS2_PLACEMENT_3D ( 'NONE', #118571, #40339, #37754 ) ;
#135951 = EDGE_CURVE ( 'NONE', #149997, #67927, #130901, .T. ) ;
#135952 = DIRECTION ( 'NONE',  ( 0.000000000000000000, 0.000000000000000000, 1.000000000000000000 ) ) ;
#135953 = B_SPLINE_CURVE_WITH_KNOTS ( 'NONE', 3,
 ( #44474, #124010, #104403, #164415, #13062, #250364, #132999 ),
 .UNSPECIFIED., .F., .F.,
 ( 4, 3, 4 ),
 ( 0.000000000000000000, 0.0007844235214594269838, 0.001767853679404345069 ),
 .UNSPECIFIED. ) ;
#135954 = EDGE_LOOP ( 'NONE', ( #101738, #13282, #256788, #167566 ) ) ;
#135955 = ORIENTED_EDGE ( 'NONE', *, *, #226370, .T. ) ;
#135956 = AXIS2_PLACEMENT_3D ( 'NONE', #78380, #79655, #200907 ) ;
#135957 = FACE_OUTER_BOUND ( 'NONE', #31283, .T. ) ;
#135958 = DIRECTION ( 'NONE',  ( 0.000000000000000000, -0.4088369013363280513, 0.9126074666063769270 ) ) ;
#135959 = FACE_OUTER_BOUND ( 'NONE', #144193, .T. ) ;
#135960 = ORIENTED_EDGE ( 'NONE', *, *, #63146, .F. ) ;
#135961 = EDGE_CURVE ( 'NONE', #112332, #173445, #114141, .T. ) ;
#135963 = CIRCLE ( 'NONE', #15183, 0.09999999999999939493 ) ;
#135962 = CARTESIAN_POINT ( 'NONE',  ( -21.53551880898957549, -1.347108827648217044, -194.3495433631890705 ) ) ;
#135964 = CARTESIAN_POINT ( 'NONE',  ( 20.85000000000000142, 76.00000000001244871, -170.0231074845243597 ) ) ;
#135965 = DIRECTION ( 'NONE',  ( 0.000000000000000000, -0.9394191166662962944, -0.3427706569149635563 ) ) ;
#135966 = CARTESIAN_POINT ( 'NONE',  ( -16.94275863006528482, 66.01050395134448934, -115.6314101024477878 ) ) ;
#135967 = ORIENTED_EDGE ( 'NONE', *, *, #222237, .T. ) ;
#135968 = CARTESIAN_POINT ( 'NONE',  ( -18.31572283045112570, 85.54843783089792453, -129.6724818334656675 ) ) ;
#135969 = EDGE_LOOP ( 'NONE', ( #97338, #20120, #31746, #84716 ) ) ;
#135971 = VERTEX_POINT ( 'NONE', #222243 ) ;
#135970 = CARTESIAN_POINT ( 'NONE',  ( -16.94445028196807002, 66.00793639031451221, -149.1304376629428816 ) ) ;
#135972 = ORIENTED_EDGE ( 'NONE', *, *, #182710, .F. ) ;
#135973 = LINE ( 'NONE', #36933, #144715 ) ;
#135974 = CARTESIAN_POINT ( 'NONE',  ( 14.56326696814971555, 66.55335100938374637, -188.4339441886012594 ) ) ;
#135975 = CARTESIAN_POINT ( 'NONE',  ( -23.25000000000000000, -1.164121893230052995, -141.9148480855716343 ) ) ;
#135976 = DIRECTION ( 'NONE',  ( 0.000000000000000000, -7.086529944415886769E-15, 1.000000000000000000 ) ) ;
#135978 = VERTEX_POINT ( 'NONE', #127026 ) ;
#135977 = AXIS2_PLACEMENT_3D ( 'NONE', #251235, #72638, #75210 ) ;
#135979 = DIRECTION ( 'NONE',  ( 0.000000000000000000, -7.109473446599835262E-15, 1.000000000000000000 ) ) ;
#135980 = DIRECTION ( 'NONE',  ( 1.000000000000000000, -3.265361837132813093E-16, -2.280189983783949500E-30 ) ) ;
#135981 = VERTEX_POINT ( 'NONE', #246964 ) ;
#135983 = ORIENTED_EDGE ( 'NONE', *, *, #1437, .F. ) ;
#135982 = DIRECTION ( 'NONE',  ( 0.000000000000000000, -0.8814952561688429444, 0.4721928772777349570 ) ) ;
#135984 = CARTESIAN_POINT ( 'NONE',  ( -23.15000000000000213, 2.500000000011154633, -120.7753780772379315 ) ) ;
#135985 = EDGE_CURVE ( 'NONE', #155667, #36086, #68347, .T. ) ;
#135986 = DIRECTION ( 'NONE',  ( 2.694716079187273439E-16, 0.9651348961777159730, -0.2617529984165023471 ) ) ;
#135987 = AXIS2_PLACEMENT_3D ( 'NONE', #59194, #149071, #5654 ) ;
#135988 = VECTOR ( 'NONE', #52788, 1000.000000000000000 ) ;
#135989 = EDGE_CURVE ( 'NONE', #213407, #140695, #39356, .T. ) ;
#135990 = TOROIDAL_SURFACE ( 'NONE', #73676, 0.4000000000000012990, 0.1000000000000000056 ) ;
#135991 = AXIS2_PLACEMENT_3D ( 'NONE', #184929, #104085, #46686 ) ;
#135992 = DIRECTION ( 'NONE',  ( 1.000000000000000000, 0.000000000000000000, 0.000000000000000000 ) ) ;
#135993 = ORIENTED_EDGE ( 'NONE', *, *, #148583, .F. ) ;
#135994 = FACE_OUTER_BOUND ( 'NONE', #128619, .T. ) ;
#135995 = CARTESIAN_POINT ( 'NONE',  ( 15.57250062127602597, 66.62931007840892050, -51.99664235786332256 ) ) ;
#135996 = DIRECTION ( 'NONE',  ( 1.000000000000000000, -3.265361837132813093E-16, -2.280189983783949500E-30 ) ) ;
#135997 = AXIS2_PLACEMENT_3D ( 'NONE', #170271, #28176, #26890 ) ;
#135998 = EDGE_CURVE ( 'NONE', #169291, #140287, #30978, .T. ) ;
#135999 = CIRCLE ( 'NONE', #227591, 0.09999999999998898659 ) ;
#136000 = AXIS2_PLACEMENT_3D ( 'NONE', #113599, #133166, #236111 ) ;
#136001 = ORIENTED_EDGE ( 'NONE', *, *, #252403, .F. ) ;
#136002 = FACE_OUTER_BOUND ( 'NONE', #193393, .T. ) ;
#136003 = CIRCLE ( 'NONE', #219225, 0.5000000000000004441 ) ;
#136004 = ORIENTED_EDGE ( 'NONE', *, *, #10132, .T. ) ;
#136005 = LINE ( 'NONE', #39535, #172836 ) ;
#136006 = CARTESIAN_POINT ( 'NONE',  ( -33.72168855820451938, 9.950000000011156587, -113.1499999999999773 ) ) ;
#136008 = VERTEX_POINT ( 'NONE', #223535 ) ;
#136007 = DIRECTION ( 'NONE',  ( -0.000000000000000000, -0.9770955615653313941, -0.2128009952263606730 ) ) ;
#136009 = DIRECTION ( 'NONE',  ( 1.000000000000000000, 0.000000000000000000, 0.000000000000000000 ) ) ;
#136010 = DIRECTION ( 'NONE',  ( 0.000000000000000000, 0.000000000000000000, -1.000000000000000000 ) ) ;
#136011 = CARTESIAN_POINT ( 'NONE',  ( 22.48660254037844197, 64.35000000001194564, -103.0731074845243853 ) ) ;
#136012 = DIRECTION ( 'NONE',  ( 0.000000000000000000, 0.9908441862701782288, -0.1350103645450542456 ) ) ;
#136013 = CARTESIAN_POINT ( 'NONE',  ( 21.04999999999999716, 6.300183336278553980, -33.44867256765849106 ) ) ;
#136014 = DIRECTION ( 'NONE',  ( 0.000000000000000000, -0.8814952561688444987, 0.4721928772777320149 ) ) ;
#136015 = CARTESIAN_POINT ( 'NONE',  ( 21.09316766718127667, 6.370153312485569153, -66.96073659768534014 ) ) ;
#136016 = EDGE_LOOP ( 'NONE', ( #72871, #136388, #125772, #176058 ) ) ;
#136017 = VECTOR ( 'NONE', #189712, 1000.000000000000000 ) ;
#136018 = DIRECTION ( 'NONE',  ( 1.000000000000000000, 0.000000000000000000, 0.000000000000000000 ) ) ;
#136019 = DIRECTION ( 'NONE',  ( 0.000000000000000000, -0.5000000000000209832, 0.8660254037844264952 ) ) ;
#136020 = CARTESIAN_POINT ( 'NONE',  ( -18.50000000000000711, 85.42130820975131655, -196.2807442704737753 ) ) ;
#136021 = VECTOR ( 'NONE', #244, 1000.000000000000000 ) ;
#136022 = VERTEX_POINT ( 'NONE', #226098 ) ;
#136023 = EDGE_CURVE ( 'NONE', #51917, #206366, #87871, .T. ) ;
#136024 = CARTESIAN_POINT ( 'NONE',  ( -21.05000000000000071, 87.65000000001266756, -200.6231074845242688 ) ) ;
#136025 = DIRECTION ( 'NONE',  ( 0.000000000000000000, 0.000000000000000000, -1.000000000000000000 ) ) ;
#136026 = EDGE_CURVE ( 'NONE', #133691, #21323, #202704, .T. ) ;
#136027 = CARTESIAN_POINT ( 'NONE',  ( -18.49719636458555883, 85.44636535923967813, -62.45149361464103777 ) ) ;
#136028 = VECTOR ( 'NONE', #76294, 1000.000000000000000 ) ;
#136029 = VERTEX_POINT ( 'NONE', #241830 ) ;
#136030 = AXIS2_PLACEMENT_3D ( 'NONE', #109519, #189072, #89957 ) ;
#136031 = CIRCLE ( 'NONE', #131785, 0.1999999999999987899 ) ;
#136032 = DIRECTION ( 'NONE',  ( -3.265361837132813093E-16, -1.000000000000000000, -6.982962677686266711E-15 ) ) ;
#136033 = CARTESIAN_POINT ( 'NONE',  ( 21.14999999999999503, -0.1008583690875562017, -155.7504328765105868 ) ) ;
#136034 = EDGE_CURVE ( 'NONE', #15348, #64826, #36936, .T. ) ;
#136035 = ORIENTED_EDGE ( 'NONE', *, *, #182360, .F. ) ;
#136036 = DIRECTION ( 'NONE',  ( -1.000000000000000000, 3.265361837132813093E-16, 2.280189983783949500E-30 ) ) ;
#136037 = ORIENTED_EDGE ( 'NONE', *, *, #119647, .F. ) ;
#136038 = LINE ( 'NONE', #215591, #71377 ) ;
#136040 = ORIENTED_EDGE ( 'NONE', *, *, #73564, .F. ) ;
#136039 = FACE_OUTER_BOUND ( 'NONE', #9066, .T. ) ;
#136041 = EDGE_CURVE ( 'NONE', #249313, #30919, #97550, .T. ) ;
#136042 = EDGE_CURVE ( 'NONE', #220397, #206536, #145289, .T. ) ;
#136043 = DIRECTION ( 'NONE',  ( 0.000000000000000000, 0.000000000000000000, -1.000000000000000000 ) ) ;
#136044 = VERTEX_POINT ( 'NONE', #224828 ) ;
#136045 = DIRECTION ( 'NONE',  ( 0.000000000000000000, 0.1350103645451876666, -0.9908441862701600211 ) ) ;
#136046 = ORIENTED_EDGE ( 'NONE', *, *, #137017, .T. ) ;
#136048 = ORIENTED_EDGE ( 'NONE', *, *, #5093, .F. ) ;
#136047 = ORIENTED_EDGE ( 'NONE', *, *, #63315, .T. ) ;
#136049 = DIRECTION ( 'NONE',  ( 0.000000000000000000, 0.000000000000000000, 1.000000000000000000 ) ) ;
#136050 = EDGE_CURVE ( 'NONE', #21586, #237840, #205907, .T. ) ;
#136051 = ORIENTED_EDGE ( 'NONE', *, *, #107843, .F. ) ;
#136052 = DIRECTION ( 'NONE',  ( -0.000000000000000000, -0.000000000000000000, -1.000000000000000000 ) ) ;
#136054 = VERTEX_POINT ( 'NONE', #243114 ) ;
#136053 = CIRCLE ( 'NONE', #161033, 0.09999999999998898659 ) ;
#136055 = AXIS2_PLACEMENT_3D ( 'NONE', #16150, #235172, #14860 ) ;
#136056 = AXIS2_PLACEMENT_3D ( 'NONE', #77177, #233706, #55030 ) ;
#136057 = ORIENTED_EDGE ( 'NONE', *, *, #75615, .F. ) ;
#136058 = AXIS2_PLACEMENT_3D ( 'NONE', #5778, #257829, #256541 ) ;
#136059 = DIRECTION ( 'NONE',  ( 1.000000000000000000, 0.000000000000000000, 0.000000000000000000 ) ) ;
#136060 = EDGE_CURVE ( 'NONE', #215705, #29202, #55859, .T. ) ;
#136061 = DIRECTION ( 'NONE',  ( 0.000000000000000000, 0.000000000000000000, 1.000000000000000000 ) ) ;
#136062 = FACE_OUTER_BOUND ( 'NONE', #101449, .T. ) ;
#136063 = ORIENTED_EDGE ( 'NONE', *, *, #60768, .F. ) ;
#136064 = AXIS2_PLACEMENT_3D ( 'NONE', #213311, #34711, #51651 ) ;
#136065 = SPHERICAL_SURFACE ( 'NONE', #74438, 0.1000000000000000056 ) ;
#136066 = AXIS2_PLACEMENT_3D ( 'NONE', #69478, #231124, #52442 ) ;
#136067 = DIRECTION ( 'NONE',  ( 1.000000000000000000, 0.000000000000000000, 0.000000000000000000 ) ) ;
#136068 = DIRECTION ( 'NONE',  ( 1.000000000000000000, 0.000000000000000000, 0.000000000000000000 ) ) ;
#136069 = VERTEX_POINT ( 'NONE', #144007 ) ;
#136070 = LINE ( 'NONE', #115251, #171144 ) ;
#136071 = CARTESIAN_POINT ( 'NONE',  ( -18.49372193242269802, 38.16337307575515325, -261.0689495423612243 ) ) ;
#136072 = CARTESIAN_POINT ( 'NONE',  ( -20.54999999999999716, 7.150000000011155876, -112.8500000000000369 ) ) ;
#136073 = VERTEX_POINT ( 'NONE', #44927 ) ;
#136074 = FACE_OUTER_BOUND ( 'NONE', #20743, .T. ) ;
#136075 = EDGE_LOOP ( 'NONE', ( #190514, #108714, #111051, #26460 ) ) ;
#136076 = ORIENTED_EDGE ( 'NONE', *, *, #74804, .T. ) ;
#136077 = TOROIDAL_SURFACE ( 'NONE', #202738, 0.2000000000000000111, 0.1000000000000000056 ) ;
#136078 = CONICAL_SURFACE ( 'NONE', #65374, 6.249999999999996447, 0.7853981633974431720 ) ;
#136079 = CIRCLE ( 'NONE', #219308, 0.1000000000000019901 ) ;
#136080 = DIRECTION ( 'NONE',  ( 0.000000000000000000, 6.938893903907222067E-15, -1.000000000000000000 ) ) ;
#136081 = VERTEX_POINT ( 'NONE', #217745 ) ;
#136082 = ORIENTED_EDGE ( 'NONE', *, *, #60620, .F. ) ;
#136083 = CARTESIAN_POINT ( 'NONE',  ( -18.59999999999999787, 69.15387683765929694, -99.28538121767448388 ) ) ;
#136084 = DIRECTION ( 'NONE',  ( 0.000000000000000000, 0.000000000000000000, -1.000000000000000000 ) ) ;
#136085 = EDGE_LOOP ( 'NONE', ( #246701, #200120, #235832, #65228 ) ) ;
#136086 = ORIENTED_EDGE ( 'NONE', *, *, #150197, .F. ) ;
#136087 = CARTESIAN_POINT ( 'NONE',  ( -23.15000000000000213, 2.500000000000000444, -13.22462192276210224 ) ) ;
#136088 = DIRECTION ( 'NONE',  ( 0.000000000000000000, -6.982962677686266711E-15, 1.000000000000000000 ) ) ;
#136089 = VERTEX_POINT ( 'NONE', #179939 ) ;
#136090 = CIRCLE ( 'NONE', #32094, 11.70000000000000284 ) ;
#136091 = ORIENTED_EDGE ( 'NONE', *, *, #183428, .F. ) ;
#136092 = ADVANCED_FACE ( 'NONE', ( #181232 ), #239915, .F. ) ;
#136093 = DIRECTION ( 'NONE',  ( 1.000000000000000000, -4.851622311275597861E-17, 1.082981191754466620E-16 ) ) ;
#136094 = CARTESIAN_POINT ( 'NONE',  ( 21.05000000000000071, 14.05000000001115623, -61.48630492923908974 ) ) ;
#136095 = EDGE_CURVE ( 'NONE', #224941, #94319, #230886, .T. ) ;
#136096 = CARTESIAN_POINT ( 'NONE',  ( 20.85000000000000142, 80.80934863333322937, -192.8037999715871535 ) ) ;
#136097 = DIRECTION ( 'NONE',  ( 1.000000000000000000, 0.000000000000000000, 0.000000000000000000 ) ) ;
#136098 = AXIS2_PLACEMENT_3D ( 'NONE', #34446, #158254, #193502 ) ;
#136099 = CARTESIAN_POINT ( 'NONE',  ( -21.05000000000000071, -12.41227409414968541, -30.59999999999999432 ) ) ;
#136100 = CARTESIAN_POINT ( 'NONE',  ( 21.05000000000000071, 10.72371710471867701, -67.00000000000004263 ) ) ;
#136101 = LINE ( 'NONE', #257307, #139681 ) ;
#136102 = EDGE_CURVE ( 'NONE', #237605, #138314, #138204, .T. ) ;
#136104 = DIRECTION ( 'NONE',  ( 0.000000000000000000, 0.000000000000000000, 1.000000000000000000 ) ) ;
#136103 = CARTESIAN_POINT ( 'NONE',  ( 21.05000000000000071, 75.90220970870248607, -75.78092209500584886 ) ) ;
#136107 = EDGE_CURVE ( 'NONE', #108305, #61048, #22588, .T. ) ;
#136106 = AXIS2_PLACEMENT_3D ( 'NONE', #164437, #243954, #182720 ) ;
#136105 = LINE ( 'NONE', #76153, #240552 ) ;
#136108 = LINE ( 'NONE', #17472, #169486 ) ;
#136109 = DIRECTION ( 'NONE',  ( 0.000000000000000000, -7.086529944415894657E-15, 1.000000000000000000 ) ) ;
#136110 = FACE_OUTER_BOUND ( 'NONE', #92878, .T. ) ;
#136112 = EDGE_LOOP ( 'NONE', ( #33501, #227256, #71441, #228191 ) ) ;
#136111 = AXIS2_PLACEMENT_3D ( 'NONE', #78072, #59775, #16846 ) ;
#136113 =( BOUNDED_CURVE ( )  B_SPLINE_CURVE ( 3, ( #104186, #106758, #122499, #85891 ),
 .UNSPECIFIED., .F., .F. ) 
 B_SPLINE_CURVE_WITH_KNOTS ( ( 4, 4 ),
 ( 1.570796326794908992, 2.617993877991470875 ),
 .UNSPECIFIED. ) 
 CURVE ( )  GEOMETRIC_REPRESENTATION_ITEM ( )  RATIONAL_B_SPLINE_CURVE ( ( 1.000000000000000000, 0.9106836025229650966, 0.9106836025229650966, 1.000000000000000000 ) ) 
 REPRESENTATION_ITEM ( '' )  );
#136115 = ORIENTED_EDGE ( 'NONE', *, *, #38007, .F. ) ;
#136114 = CARTESIAN_POINT ( 'NONE',  ( 23.15000000000000213, 86.27712145182582049, -209.5223386573213702 ) ) ;
#136116 = EDGE_CURVE ( 'NONE', #13808, #121700, #89201, .T. ) ;
#136117 = VECTOR ( 'NONE', #210291, 1000.000000000000000 ) ;
#136118 = CARTESIAN_POINT ( 'NONE',  ( -21.05000000000000071, -11.29603075032412995, -170.5478991596638423 ) ) ;
#136119 = EDGE_CURVE ( 'NONE', #200797, #45011, #47681, .T. ) ;
#136120 = CIRCLE ( 'NONE', #173639, 0.1000000000000028644 ) ;
#136121 = LINE ( 'NONE', #235247, #248649 ) ;
#136122 = ORIENTED_EDGE ( 'NONE', *, *, #227842, .F. ) ;
#136123 = VECTOR ( 'NONE', #177361, 1000.000000000000114 ) ;
#136124 = PRODUCT_RELATED_PRODUCT_CATEGORY ( 'part', '', ( #72353 ) ) ;
#136125 = CARTESIAN_POINT ( 'NONE',  ( -20.54999999999999716, 76.00000000001169553, -67.52310748452430289 ) ) ;
#136126 = DIRECTION ( 'NONE',  ( 0.000000000000000000, 1.000000000000000000, 0.000000000000000000 ) ) ;
#136127 = ORIENTED_EDGE ( 'NONE', *, *, #98211, .F. ) ;
#136128 = VECTOR ( 'NONE', #200123, 1000.000000000000000 ) ;
#136129 = CARTESIAN_POINT ( 'NONE',  ( -20.94999999999999929, 11.75000000001115197, -140.8416006898971489 ) ) ;
#136130 = DIRECTION ( 'NONE',  ( 0.5932847527679299127, 0.8049926720990051576, 4.984624513800587583E-15 ) ) ;
#136131 = ADVANCED_FACE ( 'NONE', ( #20885 ), #160154, .T. ) ;
#136132 = EDGE_CURVE ( 'NONE', #92509, #16880, #47495, .T. ) ;
#136133 = CARTESIAN_POINT ( 'NONE',  ( 18.50000000000000000, 46.96039402156216624, -255.3459641718773128 ) ) ;
#136135 = ORIENTED_EDGE ( 'NONE', *, *, #56859, .T. ) ;
#136134 = CARTESIAN_POINT ( 'NONE',  ( -20.94403535211772294, 67.49374512151688066, -195.5131169347613991 ) ) ;
#136136 = ADVANCED_FACE ( 'NONE', ( #119988 ), #41720, .T. ) ;
#136138 = EDGE_LOOP ( 'NONE', ( #96030, #121690, #124625, #241708 ) ) ;
#136137 = CARTESIAN_POINT ( 'NONE',  ( -18.43634282235119670, 85.67978719993983816, -96.36245559907032998 ) ) ;
#136139 = CARTESIAN_POINT ( 'NONE',  ( -18.69999999999999929, 5.488301202077016328, 16.39999999999999858 ) ) ;
#136140 = CARTESIAN_POINT ( 'NONE',  ( -21.05000000000000071, 72.02722222756958104, -225.1832529173024398 ) ) ;
#136141 = DIRECTION ( 'NONE',  ( -1.020425574104004196E-15, 0.000000000000000000, 1.000000000000000000 ) ) ;
#136142 = DIRECTION ( 'NONE',  ( 0.000000000000000000, 0.000000000000000000, 1.000000000000000000 ) ) ;
#136144 = LINE ( 'NONE', #119193, #58250 ) ;
#136143 = DIRECTION ( 'NONE',  ( 1.000000000000000000, -0.000000000000000000, 0.000000000000000000 ) ) ;
#136145 = DIRECTION ( 'NONE',  ( -1.073024830501117725E-15, -0.000000000000000000, -1.000000000000000000 ) ) ;
#136146 = CARTESIAN_POINT ( 'NONE',  ( -18.79999999999999716, -1.885425182446132997, -11.49641995933507843 ) ) ;
#136147 = CARTESIAN_POINT ( 'NONE',  ( -20.94999999999999929, 7.021664781911246322, -204.8335654018972605 ) ) ;
#136148 = CIRCLE ( 'NONE', #152787, 0.09999999999999939493 ) ;
#136149 = AXIS2_PLACEMENT_3D ( 'NONE', #167342, #169933, #108624 ) ;
#136150 = CARTESIAN_POINT ( 'NONE',  ( 20.94999999999999929, 70.42128727326085880, -228.5349014959848262 ) ) ;
#136151 = AXIS2_PLACEMENT_3D ( 'NONE', #147597, #32831, #191893 ) ;
#136152 = VECTOR ( 'NONE', #64055, 1000.000000000000000 ) ;
#136153 = ORIENTED_EDGE ( 'NONE', *, *, #133862, .T. ) ;
#136154 = FACE_OUTER_BOUND ( 'NONE', #43381, .T. ) ;
#136155 = ORIENTED_EDGE ( 'NONE', *, *, #122672, .F. ) ;
#136156 = VERTEX_POINT ( 'NONE', #57392 ) ;
#136157 = DIRECTION ( 'NONE',  ( 1.000000000000000000, 0.000000000000000000, 0.000000000000000000 ) ) ;
#136158 = ORIENTED_EDGE ( 'NONE', *, *, #52420, .F. ) ;
#136160 = EDGE_CURVE ( 'NONE', #224073, #199876, #99077, .T. ) ;
#136159 = EDGE_LOOP ( 'NONE', ( #116246, #165703, #176817, #78696 ) ) ;
#136161 = CARTESIAN_POINT ( 'NONE',  ( -17.78241384944316650, 10.85557575281093357, -144.2490376724881003 ) ) ;
#136162 = SURFACE_SIDE_STYLE ('',( #56621 ) ) ;
#136163 = CIRCLE ( 'NONE', #111273, 0.9000000000000014655 ) ;
#136164 = AXIS2_PLACEMENT_3D ( 'NONE', #222489, #141686, #25611 ) ;
#136165 = EDGE_LOOP ( 'NONE', ( #235976, #255188, #134496, #65523 ) ) ;
#136166 = ORIENTED_EDGE ( 'NONE', *, *, #55966, .T. ) ;
#136167 = DIRECTION ( 'NONE',  ( 0.000000000000000000, -0.1298341882519953583, -0.9915357197604862671 ) ) ;
#136168 = CARTESIAN_POINT ( 'NONE',  ( -20.64999999999999858, 68.85000000001259934, -191.1731074845243938 ) ) ;
#136169 = CIRCLE ( 'NONE', #57070, 0.09999999999999971412 ) ;
#136170 = CARTESIAN_POINT ( 'NONE',  ( -22.59999999999999787, 1.115600667400684642E-11, -67.00000000000004263 ) ) ;
#136171 = DIRECTION ( 'NONE',  ( 0.000000000000000000, 0.000000000000000000, 1.000000000000000000 ) ) ;
#136172 = CARTESIAN_POINT ( 'NONE',  ( -23.25000000000000355, 64.25000000001256240, -182.6731074845244507 ) ) ;
#136173 = EDGE_CURVE ( 'NONE', #191683, #168277, #10097, .T. ) ;
#136174 = DIRECTION ( 'NONE',  ( -1.000000000000000000, 0.000000000000000000, 0.000000000000000000 ) ) ;
#136175 = LINE ( 'NONE', #80048, #228517 ) ;
#136177 = EDGE_LOOP ( 'NONE', ( #234352, #30205, #91541, #240950, #158619 ) ) ;
#136176 = CARTESIAN_POINT ( 'NONE',  ( 23.14999999999999858, 7.128833340094563376, -233.7327013124401276 ) ) ;
#136179 = CARTESIAN_POINT ( 'NONE',  ( 21.05000000000000071, 4.813084112160684214, -122.0584822434762060 ) ) ;
#136178 = FACE_OUTER_BOUND ( 'NONE', #80803, .T. ) ;
#136180 = CARTESIAN_POINT ( 'NONE',  ( 20.99142135623731065, 11.60000000000000497, -26.57179676972450011 ) ) ;
#136181 =( BOUNDED_CURVE ( )  B_SPLINE_CURVE ( 3, ( #199572, #57447, #237390, #58718 ),
 .UNSPECIFIED., .F., .F. ) 
 B_SPLINE_CURVE_WITH_KNOTS ( ( 4, 4 ),
 ( 4.712388980384690562, 6.283185307179586232 ),
 .UNSPECIFIED. ) 
 CURVE ( )  GEOMETRIC_REPRESENTATION_ITEM ( )  RATIONAL_B_SPLINE_CURVE ( ( 1.000000000000000000, 0.8047378541243652705, 0.8047378541243652705, 1.000000000000000000 ) ) 
 REPRESENTATION_ITEM ( '' )  );
#136182 = ORIENTED_EDGE ( 'NONE', *, *, #91438, .F. ) ;
#136183 = DIRECTION ( 'NONE',  ( 0.000000000000000000, -1.000000000000000000, -7.109473446599835262E-15 ) ) ;
#136185 = ADVANCED_FACE ( 'NONE', ( #37873 ), #117386, .T. ) ;
#136184 = CARTESIAN_POINT ( 'NONE',  ( 21.05000000000000071, 1.115600667400684642E-11, -67.00000000000004263 ) ) ;
#136186 = ORIENTED_EDGE ( 'NONE', *, *, #95765, .T. ) ;
#136188 = CARTESIAN_POINT ( 'NONE',  ( -21.05000000000000071, 87.65000000001269598, -203.5231074845243029 ) ) ;
#136187 = PLANE ( 'NONE',  #45588 ) ;
#136189 = EDGE_CURVE ( 'NONE', #43432, #148962, #18283, .T. ) ;
#136190 = CARTESIAN_POINT ( 'NONE',  ( -21.05000000000000071, 36.65892442174472876, -249.5511627012454596 ) ) ;
#136191 = FACE_OUTER_BOUND ( 'NONE', #89563, .T. ) ;
#136192 = ORIENTED_EDGE ( 'NONE', *, *, #200438, .T. ) ;
#136193 = ORIENTED_EDGE ( 'NONE', *, *, #50045, .T. ) ;
#136194 = ADVANCED_FACE ( 'NONE', ( #161672 ), #31167, .T. ) ;
#136196 = EDGE_CURVE ( 'NONE', #236918, #143411, #193273, .T. ) ;
#136195 = DIRECTION ( 'NONE',  ( 0.000000000000000000, 0.000000000000000000, -1.000000000000000000 ) ) ;
#136197 = PLANE ( 'NONE',  #49058 ) ;
#136198 = CARTESIAN_POINT ( 'NONE',  ( 23.04999999999999716, 8.822561741677553471, -188.3499999999999659 ) ) ;
#136199 = DIRECTION ( 'NONE',  ( -1.000000000000000000, -0.000000000000000000, -0.000000000000000000 ) ) ;
#136200 = ORIENTED_EDGE ( 'NONE', *, *, #189492, .T. ) ;
#136201 = CARTESIAN_POINT ( 'NONE',  ( 14.45204356427542614, 46.53494637834451453, -234.7711487335851928 ) ) ;
#136202 = VECTOR ( 'NONE', #254621, 1000.000000000000000 ) ;
#136203 = CARTESIAN_POINT ( 'NONE',  ( -17.27223548804798270, 10.34539739142601000, -122.6336061791826211 ) ) ;
#136204 = DIRECTION ( 'NONE',  ( 1.000000000000000000, 0.000000000000000000, 0.000000000000000000 ) ) ;
#136205 = AXIS2_PLACEMENT_3D ( 'NONE', #195074, #93371, #76364 ) ;
#136206 = CIRCLE ( 'NONE', #115389, 0.09999999999998898659 ) ;
#136207 = ADVANCED_FACE ( 'NONE', ( #205900 ), #43422, .T. ) ;
#136209 = ADVANCED_FACE ( 'NONE', ( #162953 ), #89379, .F. ) ;
#136208 = DIRECTION ( 'NONE',  ( 0.000000000000000000, 0.000000000000000000, 1.000000000000000000 ) ) ;
#136210 =( BOUNDED_SURFACE ( )  B_SPLINE_SURFACE ( 3, 2, ( 
 ( #50313, #54176, #172900 ),
 ( #33380, #189848, #171603 ),
 ( #231553, #29523, #251086 ),
 ( #211994, #213249, #193708 ),
 ( #112880, #209404, #192420 ),
 ( #174184, #72485, #111598 ) ),
 .UNSPECIFIED., .F., .F., .F. ) 
 B_SPLINE_SURFACE_WITH_KNOTS ( ( 4, 2, 4 ),
 ( 3, 3 ),
 ( 6.719893378900589293E-05, 0.0002757154632485561046, 0.0004842319927081063704 ),
 ( 0.000000000000000000, 1.000000000000000000 ),
 .UNSPECIFIED. ) 
 GEOMETRIC_REPRESENTATION_ITEM ( )  RATIONAL_B_SPLINE_SURFACE ( (
 ( 1.000000000000000000, 0.7250110520819700310, 1.000000000000000000),
 ( 1.000000000000000000, 0.7277932058357532430, 1.000000000000000000),
 ( 1.000000000000000000, 0.7278452872619737279, 1.000000000000000000),
 ( 1.000000000000000000, 0.7221445671547080947, 1.000000000000000000),
 ( 1.000000000000000000, 0.7163662143781105440, 1.000000000000000000),
 ( 1.000000000000000000, 0.7071067811865475727, 1.000000000000000000) ) ) 
 REPRESENTATION_ITEM ( '' )  SURFACE ( )  );
#136211 = DIRECTION ( 'NONE',  ( 1.000000000000000000, 3.265361837132813093E-16, -0.000000000000000000 ) ) ;
#136213 = ORIENTED_EDGE ( 'NONE', *, *, #247830, .T. ) ;
#136212 = CARTESIAN_POINT ( 'NONE',  ( -16.87036670365548474, 51.65495115403913218, -231.7824289814309111 ) ) ;
#136214 = DIRECTION ( 'NONE',  ( 0.000000000000000000, -1.000000000000000000, -0.000000000000000000 ) ) ;
#136215 = AXIS2_PLACEMENT_3D ( 'NONE', #41557, #78077, #101451 ) ;
#136216 = CARTESIAN_POINT ( 'NONE',  ( -16.85697194749132422, 66.09145628588828458, -90.08810321691005640 ) ) ;
#136217 = DIRECTION ( 'NONE',  ( 0.000000000000000000, 0.000000000000000000, 1.000000000000000000 ) ) ;
#136218 = DIRECTION ( 'NONE',  ( 1.000000000000000000, -0.000000000000000000, 0.000000000000000000 ) ) ;
#136219 = EDGE_CURVE ( 'NONE', #36016, #228170, #93666, .T. ) ;
#136220 = VECTOR ( 'NONE', #221198, 1000.000000000000000 ) ;
#136221 = CARTESIAN_POINT ( 'NONE',  ( -18.50000000000000000, 74.36282728704168221, -124.9409541190522930 ) ) ;
#136223 = VERTEX_POINT ( 'NONE', #125105 ) ;
#136222 = DIRECTION ( 'NONE',  ( 1.000000000000000000, 0.000000000000000000, 0.000000000000000000 ) ) ;
#136224 = CARTESIAN_POINT ( 'NONE',  ( 22.48970261584622321, 64.35000000001238618, -170.0784769727418393 ) ) ;
#136225 = DIRECTION ( 'NONE',  ( -1.000000000000000000, -0.000000000000000000, -0.000000000000000000 ) ) ;
#136226 = CARTESIAN_POINT ( 'NONE',  ( -21.14999999999999858, 6.412126976762837494, -199.7058512474018244 ) ) ;
#136227 = EDGE_LOOP ( 'NONE', ( #68790, #52015, #7046, #60310 ) ) ;
#136228 = DIRECTION ( 'NONE',  ( 0.000000000000000000, 0.000000000000000000, -1.000000000000000000 ) ) ;
#136229 = CARTESIAN_POINT ( 'NONE',  ( 0.8999999999999993561, -11.65000000000000036, 23.30000000000000426 ) ) ;
#136230 = CARTESIAN_POINT ( 'NONE',  ( 18.49999999999998934, 6.650000000011155876, -112.8500000000000369 ) ) ;
#136231 = EDGE_CURVE ( 'NONE', #101606, #195198, #27062, .T. ) ;
#136232 = DIRECTION ( 'NONE',  ( 1.000000000000000000, 0.000000000000000000, 0.000000000000000000 ) ) ;
#136233 = ADVANCED_FACE ( 'NONE', ( #242451 ), #235148, .F. ) ;
#136234 = CARTESIAN_POINT ( 'NONE',  ( -20.85000000000000142, -0.3238857010591806307, -167.4575895893140114 ) ) ;
#136235 = AXIS2_PLACEMENT_3D ( 'NONE', #162920, #121245, #142039 ) ;
#136236 = DIRECTION ( 'NONE',  ( -0.000000000000000000, -0.1350103645451876666, 0.9908441862701600211 ) ) ;
#136237 = AXIS2_PLACEMENT_3D ( 'NONE', #95985, #238071, #77702 ) ;
#136238 = ORIENTED_EDGE ( 'NONE', *, *, #118669, .T. ) ;
#136239 = EDGE_LOOP ( 'NONE', ( #61664, #177521, #226152, #225973 ) ) ;
#136240 = EDGE_CURVE ( 'NONE', #52077, #140929, #246322, .T. ) ;
#136241 = AXIS2_PLACEMENT_3D ( 'NONE', #255711, #96647, #17170 ) ;
#136242 = CARTESIAN_POINT ( 'NONE',  ( -1.739115166359751170E-14, 31.44980407958350455, -233.5445995079518866 ) ) ;
#136243 = DIRECTION ( 'NONE',  ( 0.000000000000000000, -0.2128009952264117433, 0.9770955615653204029 ) ) ;
#136244 = CIRCLE ( 'NONE', #57141, 0.09999999999999939493 ) ;
#136245 = DIRECTION ( 'NONE',  ( 1.000000000000000000, 0.000000000000000000, 0.000000000000000000 ) ) ;
#136246 = LINE ( 'NONE', #158443, #209493 ) ;
#136247 = ORIENTED_EDGE ( 'NONE', *, *, #53661, .T. ) ;
#136248 = TOROIDAL_SURFACE ( 'NONE', #7089, 11.70000000000000107, 0.1000000000000000056 ) ;
#136249 = EDGE_CURVE ( 'NONE', #209902, #124124, #39547, .T. ) ;
#136250 = DIRECTION ( 'NONE',  ( 0.000000000000000000, -6.938893903907222067E-15, 1.000000000000000000 ) ) ;
#136251 = DIRECTION ( 'NONE',  ( 0.000000000000000000, 0.8814952561688426114, -0.4721928772777353456 ) ) ;
#136252 = DIRECTION ( 'NONE',  ( 0.000000000000000000, 0.000000000000000000, 1.000000000000000000 ) ) ;
#136253 = DIRECTION ( 'NONE',  ( 0.000000000000000000, 0.000000000000000000, -1.000000000000000000 ) ) ;
#136254 = CIRCLE ( 'NONE', #107058, 9.500000000000001776 ) ;
#136255 = CIRCLE ( 'NONE', #90489, 0.1000000000000028644 ) ;
#136256 = CIRCLE ( 'NONE', #65553, 0.09999999999999939493 ) ;
#136257 = ORIENTED_EDGE ( 'NONE', *, *, #115686, .T. ) ;
#136258 = DIRECTION ( 'NONE',  ( 0.000000000000000000, 0.9126074666063891394, 0.4088369013363010729 ) ) ;
#136259 = ORIENTED_EDGE ( 'NONE', *, *, #4658, .T. ) ;
#136260 = VERTEX_POINT ( 'NONE', #165514 ) ;
#136261 = CARTESIAN_POINT ( 'NONE',  ( -21.05000000000000071, 0.03175835306653384399, -27.24115287692075071 ) ) ;
#136262 = CARTESIAN_POINT ( 'NONE',  ( -21.05000000000000426, 6.497017786443685772, -100.5145456905711256 ) ) ;
#136263 = DIRECTION ( 'NONE',  ( -1.000000000000000000, 0.000000000000000000, 0.000000000000000000 ) ) ;
#136264 = ORIENTED_EDGE ( 'NONE', *, *, #236828, .T. ) ;
#136265 = CARTESIAN_POINT ( 'NONE',  ( -20.64999999999999858, 76.00000000001213607, -136.5231074845243313 ) ) ;
#136266 = DIRECTION ( 'NONE',  ( 1.000000000000000000, 0.000000000000000000, 0.000000000000000000 ) ) ;
#136267 = CARTESIAN_POINT ( 'NONE',  ( -20.85000000000000142, 6.933893972137497030, -204.7856458343735255 ) ) ;
#136268 = ORIENTED_EDGE ( 'NONE', *, *, #243745, .T. ) ;
#136269 = DIRECTION ( 'NONE',  ( -1.000000000000000000, 0.000000000000000000, 0.000000000000000000 ) ) ;
#136270 = AXIS2_PLACEMENT_3D ( 'NONE', #131996, #96683, #176287 ) ;
#136272 = ORIENTED_EDGE ( 'NONE', *, *, #43336, .F. ) ;
#136271 = DIRECTION ( 'NONE',  ( -1.000000000000000000, -3.265361837132813093E-16, 0.000000000000000000 ) ) ;
#136273 = DIRECTION ( 'NONE',  ( 0.2834754621636438876, 0.6737039339378290137, -0.6824695390622222968 ) ) ;
#136274 = CIRCLE ( 'NONE', #190499, 0.1999999999999945155 ) ;
#136275 = CARTESIAN_POINT ( 'NONE',  ( -21.05000000000000071, 8.001317420522642720, -237.7387931148579980 ) ) ;
#136276 = EDGE_CURVE ( 'NONE', #195393, #50748, #226754, .T. ) ;
#136277 = ORIENTED_EDGE ( 'NONE', *, *, #29178, .T. ) ;
#136278 = AXIS2_PLACEMENT_3D ( 'NONE', #135138, #231710, #210851 ) ;
#136279 = CARTESIAN_POINT ( 'NONE',  ( 21.05000000000000071, 20.42498087366621817, -235.1829032864613396 ) ) ;
#136280 = CARTESIAN_POINT ( 'NONE',  ( 23.14999999999999503, 11.65000000001116298, -54.85000000000000142 ) ) ;
#136281 = DIRECTION ( 'NONE',  ( 0.000000000000000000, 0.9126074666064812879, 0.4088369013360954596 ) ) ;
#136282 = ORIENTED_EDGE ( 'NONE', *, *, #248831, .F. ) ;
#136283 = CARTESIAN_POINT ( 'NONE',  ( 21.05000000000005400, 85.52235250936195143, -34.45408804175119144 ) ) ;
#136284 = DIRECTION ( 'NONE',  ( -1.000000000000000000, 0.000000000000000000, 0.000000000000000000 ) ) ;
#136285 = DIRECTION ( 'NONE',  ( 0.000000000000000000, 1.000000000000000000, -0.000000000000000000 ) ) ;
#136286 = AXIS2_PLACEMENT_3D ( 'NONE', #40867, #222008, #21301 ) ;
#136287 = TOROIDAL_SURFACE ( 'NONE', #77862, 11.70000000000000462, 0.1000000000000000056 ) ;
#136288 = EDGE_LOOP ( 'NONE', ( #103676, #135150, #118824, #132261 ) ) ;
#136289 = AXIS2_PLACEMENT_3D ( 'NONE', #78144, #75621, #255462 ) ;
#136290 = DIRECTION ( 'NONE',  ( -1.000000000000000000, 0.000000000000000000, 0.000000000000000000 ) ) ;
#136291 = VECTOR ( 'NONE', #168964, 1000.000000000000000 ) ;
#136292 = EDGE_CURVE ( 'NONE', #80924, #88973, #17921, .T. ) ;
#136293 = EDGE_LOOP ( 'NONE', ( #253998, #1802, #192972 ) ) ;
#136294 = AXIS2_PLACEMENT_3D ( 'NONE', #164047, #165327, #184879 ) ;
#136295 = VERTEX_POINT ( 'NONE', #168115 ) ;
#136296 = FACE_OUTER_BOUND ( 'NONE', #57091, .T. ) ;
#136297 = FACE_OUTER_BOUND ( 'NONE', #141207, .T. ) ;
#136299 = ORIENTED_EDGE ( 'NONE', *, *, #185059, .T. ) ;
#136298 = DIRECTION ( 'NONE',  ( -1.000000000000000000, 0.000000000000000000, 0.000000000000000000 ) ) ;
#136300 = FACE_OUTER_BOUND ( 'NONE', #82901, .T. ) ;
#136301 = FACE_BOUND ( 'NONE', #125501, .T. ) ;
#136302 = PLANE ( 'NONE',  #146098 ) ;
#136303 = CARTESIAN_POINT ( 'NONE',  ( -18.59999999999999787, 64.35000000001230092, -157.8731074845244393 ) ) ;
#136304 = DIRECTION ( 'NONE',  ( -0.000000000000000000, 6.982962677686266711E-15, -1.000000000000000000 ) ) ;
#136305 = DIRECTION ( 'NONE',  ( 1.186688945009009831E-16, -0.4721928772777346239, -0.8814952561688430555 ) ) ;
#136306 = DIRECTION ( 'NONE',  ( 0.000000000000000000, -0.9908441862701596881, 0.1350103645451904977 ) ) ;
#136308 = ORIENTED_EDGE ( 'NONE', *, *, #40544, .F. ) ;
#136307 = CARTESIAN_POINT ( 'NONE',  ( 23.50000000000005684, 74.83745509109094485, -43.82310748452479743 ) ) ;
#136310 = ORIENTED_EDGE ( 'NONE', *, *, #47410, .F. ) ;
#136309 = CARTESIAN_POINT ( 'NONE',  ( 20.02499999999999858, 14.04870287383362992, -219.6884709798078177 ) ) ;
#136312 = CARTESIAN_POINT ( 'NONE',  ( -16.83233564386407366, 51.51243561217257394, -232.0158193348888744 ) ) ;
#136311 = CARTESIAN_POINT ( 'NONE',  ( -16.92973740335368760, 60.88366223094347163, -221.0847067658247056 ) ) ;
#136314 = ORIENTED_EDGE ( 'NONE', *, *, #215485, .T. ) ;
#136313 = DIRECTION ( 'NONE',  ( 0.000000000000000000, 0.000000000000000000, 1.000000000000000000 ) ) ;
#136315 = ORIENTED_EDGE ( 'NONE', *, *, #240097, .T. ) ;
#136316 = DIRECTION ( 'NONE',  ( 0.000000000000000000, 0.000000000000000000, -1.000000000000000000 ) ) ;
#136317 = DIRECTION ( 'NONE',  ( 1.000000000000000000, -0.000000000000000000, 0.000000000000000000 ) ) ;
#136318 = AXIS2_PLACEMENT_3D ( 'NONE', #33715, #111941, #14126 ) ;
#136319 = CYLINDRICAL_SURFACE ( 'NONE', #213449, 0.09999999999999939493 ) ;
#136320 = FACE_OUTER_BOUND ( 'NONE', #128339, .T. ) ;
#136321 = CYLINDRICAL_SURFACE ( 'NONE', #26398, 0.09999999999999543976 ) ;
#136322 = LINE ( 'NONE', #154668, #169625 ) ;
#136323 = DIRECTION ( 'NONE',  ( 0.000000000000000000, 0.000000000000000000, -1.000000000000000000 ) ) ;
#136324 = VERTEX_POINT ( 'NONE', #166818 ) ;
#136325 = ORIENTED_EDGE ( 'NONE', *, *, #177611, .T. ) ;
#136326 = DIRECTION ( 'NONE',  ( 1.000000000000000000, 0.000000000000000000, 0.000000000000000000 ) ) ;
#136327 = ADVANCED_FACE ( 'NONE', ( #187653, #186360 ), #7721, .T. ) ;
#136328 = AXIS2_PLACEMENT_3D ( 'NONE', #173190, #32380, #209700 ) ;
#136329 = CIRCLE ( 'NONE', #178079, 0.09999999999999939493 ) ;
#136330 = VERTEX_POINT ( 'NONE', #48111 ) ;
#136331 = FACE_OUTER_BOUND ( 'NONE', #168175, .T. ) ;
#136332 = CARTESIAN_POINT ( 'NONE',  ( -16.92209698673563878, 51.56352646095744774, -231.9712590729939734 ) ) ;
#136333 = DIRECTION ( 'NONE',  ( 0.000000000000000000, -6.938893903907222067E-15, 1.000000000000000000 ) ) ;
#136334 = CARTESIAN_POINT ( 'NONE',  ( -21.07094088545368038, -1.248309276978958104, -194.8035479807908530 ) ) ;
#136335 = EDGE_CURVE ( 'NONE', #60977, #231942, #207210, .T. ) ;
#136336 = ORIENTED_EDGE ( 'NONE', *, *, #99441, .T. ) ;
#136337 = LINE ( 'NONE', #52974, #115060 ) ;
#136338 = EDGE_LOOP ( 'NONE', ( #11476, #156908, #200282, #47609 ) ) ;
#136339 = ORIENTED_EDGE ( 'NONE', *, *, #220877, .F. ) ;
#136340 = EDGE_CURVE ( 'NONE', #147639, #220201, #99627, .T. ) ;
#136341 = DIRECTION ( 'NONE',  ( -1.000000000000000000, -0.000000000000000000, 0.000000000000000000 ) ) ;
#136342 = CARTESIAN_POINT ( 'NONE',  ( 17.23472005113827876, 65.69211804551110845, -91.56968434459304262 ) ) ;
#136343 = CARTESIAN_POINT ( 'NONE',  ( -16.86757978335471719, 9.965650379045438712, -113.0980046531675356 ) ) ;
#136344 = AXIS2_PLACEMENT_3D ( 'NONE', #238668, #39210, #3912 ) ;
#136345 = ORIENTED_EDGE ( 'NONE', *, *, #178468, .F. ) ;
#136346 = CIRCLE ( 'NONE', #23980, 0.1000000000000028644 ) ;
#136347 = EDGE_CURVE ( 'NONE', #245009, #173882, #172834, .T. ) ;
#136349 = ORIENTED_EDGE ( 'NONE', *, *, #25162, .T. ) ;
#136348 = CARTESIAN_POINT ( 'NONE',  ( 18.39999999999998082, 11.47316190336247033, -9.250000000000000000 ) ) ;
#136350 = DIRECTION ( 'NONE',  ( 1.000000000000000000, 0.000000000000000000, 0.000000000000000000 ) ) ;
#136351 = ORIENTED_EDGE ( 'NONE', *, *, #188224, .F. ) ;
#136352 = AXIS2_PLACEMENT_3D ( 'NONE', #104877, #245721, #107486 ) ;
#136353 = ORIENTED_EDGE ( 'NONE', *, *, #20997, .F. ) ;
#136354 = CARTESIAN_POINT ( 'NONE',  ( 21.46681500597573944, -5.827586677109586333E-16, 6.857511159430853986 ) ) ;
#136355 = ORIENTED_EDGE ( 'NONE', *, *, #49283, .T. ) ;
#136356 = DIRECTION ( 'NONE',  ( 0.000000000000000000, 1.000000000000000000, 0.000000000000000000 ) ) ;
#136357 = EDGE_CURVE ( 'NONE', #119594, #233017, #176896, .T. ) ;
#136358 = DIRECTION ( 'NONE',  ( -0.000000000000000000, -6.982962677686266711E-15, 1.000000000000000000 ) ) ;
#136359 = CARTESIAN_POINT ( 'NONE',  ( 20.94999999999999929, 87.65000000001244018, -170.0231074845242745 ) ) ;
#136360 = FACE_OUTER_BOUND ( 'NONE', #8362, .T. ) ;
#136361 = DIRECTION ( 'NONE',  ( 1.000000000000000000, 1.836970198721029934E-16, 0.000000000000000000 ) ) ;
#136362 = ORIENTED_EDGE ( 'NONE', *, *, #80950, .T. ) ;
#136363 = CARTESIAN_POINT ( 'NONE',  ( -20.85000000000000142, 43.08613539620618837, -254.3146655184800409 ) ) ;
#136364 = CARTESIAN_POINT ( 'NONE',  ( 18.50000000000000000, 86.87843438503968230, -199.3967801207316484 ) ) ;
#136365 = DIRECTION ( 'NONE',  ( 1.000000000000000000, -2.952720810173289112E-16, -2.061873921506763405E-30 ) ) ;
#136366 = VECTOR ( 'NONE', #223086, 1000.000000000000000 ) ;
#136367 = EDGE_LOOP ( 'NONE', ( #52407, #98403, #244655, #42385 ) ) ;
#136368 = CARTESIAN_POINT ( 'NONE',  ( 23.25000000000000000, 78.50726470275242264, -228.6618886302502176 ) ) ;
#136369 = VERTEX_POINT ( 'NONE', #153696 ) ;
#136370 = DIRECTION ( 'NONE',  ( -0.000000000000000000, -0.000000000000000000, -1.000000000000000000 ) ) ;
#136371 = AXIS2_PLACEMENT_3D ( 'NONE', #129668, #111398, #90530 ) ;
#136372 = ORIENTED_EDGE ( 'NONE', *, *, #3794, .T. ) ;
#136373 = DIRECTION ( 'NONE',  ( 0.000000000000000000, -0.9651348961777379554, 0.2617529984164210233 ) ) ;
#136374 = DIRECTION ( 'NONE',  ( 0.000000000000000000, -0.1350103645451876666, -0.9908441862701600211 ) ) ;
#136376 = ORIENTED_EDGE ( 'NONE', *, *, #93452, .T. ) ;
#136375 = DIRECTION ( 'NONE',  ( 0.000000000000000000, 0.000000000000000000, -1.000000000000000000 ) ) ;
#136377 = CYLINDRICAL_SURFACE ( 'NONE', #42283, 0.9000000000000014655 ) ;
#136378 = ORIENTED_EDGE ( 'NONE', *, *, #177467, .F. ) ;
#136379 = AXIS2_PLACEMENT_3D ( 'NONE', #222187, #237923, #217056 ) ;
#136380 = ADVANCED_FACE ( 'NONE', ( #35015 ), #143557, .T. ) ;
#136381 = CARTESIAN_POINT ( 'NONE',  ( 20.94999999999999929, 0.5450571430110628945, -208.9664790259058691 ) ) ;
#136382 = CARTESIAN_POINT ( 'NONE',  ( 21.05000000000000071, 43.51422117117169108, -240.0698702536254530 ) ) ;
#136383 = ORIENTED_EDGE ( 'NONE', *, *, #3775, .T. ) ;
#136384 = CIRCLE ( 'NONE', #24017, 0.1000000000000028644 ) ;
#136385 = ORIENTED_EDGE ( 'NONE', *, *, #96847, .T. ) ;
#136386 = DIRECTION ( 'NONE',  ( -1.000000000000000000, 0.000000000000000000, 0.000000000000000000 ) ) ;
#136387 = LINE ( 'NONE', #154733, #69348 ) ;
#136388 = ORIENTED_EDGE ( 'NONE', *, *, #101668, .T. ) ;
#136389 = CARTESIAN_POINT ( 'NONE',  ( -18.50000000000000000, -9.399999999988850163, -107.7972597596633193 ) ) ;
#136390 = VECTOR ( 'NONE', #132510, 1000.000000000000000 ) ;
#136391 = AXIS2_PLACEMENT_3D ( 'NONE', #190049, #72695, #170540 ) ;
#136392 = CIRCLE ( 'NONE', #153626, 0.1000000000000028644 ) ;
#136393 = ORIENTED_EDGE ( 'NONE', *, *, #148218, .T. ) ;
#136394 = EDGE_CURVE ( 'NONE', #104211, #150814, #229336, .T. ) ;
#136395 = CARTESIAN_POINT ( 'NONE',  ( 22.39999999999999503, 25.97741635855165754, -254.4468634167653249 ) ) ;
#136397 = DIRECTION ( 'NONE',  ( 0.000000000000000000, 0.000000000000000000, -1.000000000000000000 ) ) ;
#136396 = AXIS2_PLACEMENT_3D ( 'NONE', #248718, #116589, #177864 ) ;
#136398 = AXIS2_PLACEMENT_3D ( 'NONE', #208075, #125933, #29458 ) ;
#136399 = EDGE_CURVE ( 'NONE', #18995, #230047, #193466, .T. ) ;
#136401 = ORIENTED_EDGE ( 'NONE', *, *, #231771, .F. ) ;
#136400 = CARTESIAN_POINT ( 'NONE',  ( -20.94999999999999929, 69.20602499728043711, -247.8456586332460176 ) ) ;
#136402 = LINE ( 'NONE', #78998, #82533 ) ;
#136403 = DIRECTION ( 'NONE',  ( 1.000000000000000000, 0.000000000000000000, 0.000000000000000000 ) ) ;
#136404 = DIRECTION ( 'NONE',  ( 0.000000000000000000, 0.000000000000000000, -1.000000000000000000 ) ) ;
#136406 = CARTESIAN_POINT ( 'NONE',  ( -18.50000000000000000, 72.10920423909969657, -225.0008277277438822 ) ) ;
#136405 = CARTESIAN_POINT ( 'NONE',  ( 21.15000000000005542, 86.36484105039212977, -51.23044614117323903 ) ) ;
#136408 = EDGE_CURVE ( 'NONE', #218618, #132210, #190208, .T. ) ;
#136407 = CARTESIAN_POINT ( 'NONE',  ( 21.14999999999999858, -0.09999999998884338825, -26.95934304829875927 ) ) ;
#136409 = CARTESIAN_POINT ( 'NONE',  ( 21.14999999999999858, -1.236118717437887371, -194.8647072476926212 ) ) ;
#136410 = TOROIDAL_SURFACE ( 'NONE', #169814, 4.041421356237307805, 0.1000000000000000056 ) ;
#136411 = CARTESIAN_POINT ( 'NONE',  ( -20.85000000000000142, -11.75000000000000000, -30.59999999999999432 ) ) ;
#136412 = CARTESIAN_POINT ( 'NONE',  ( 20.85000000000000142, 77.83585931145570669, -125.0186683157258329 ) ) ;
#136413 = VECTOR ( 'NONE', #125829, 1000.000000000000000 ) ;
#136414 = ORIENTED_EDGE ( 'NONE', *, *, #207751, .F. ) ;
#136415 = EDGE_LOOP ( 'NONE', ( #229550, #213028, #92960, #60990 ) ) ;
#136417 = DIRECTION ( 'NONE',  ( 0.000000000000000000, -0.2617529984165031243, -0.9651348961777157509 ) ) ;
#136416 = TOROIDAL_SURFACE ( 'NONE', #223734, 12.77500000000000036, 0.1000000000000000056 ) ;
#136418 = CIRCLE ( 'NONE', #248894, 0.1000000000000102612 ) ;
#136420 = EDGE_LOOP ( 'NONE', ( #199349, #88627, #255130, #17100, #251626 ) ) ;
#136419 = CARTESIAN_POINT ( 'NONE',  ( 20.84999999999998721, 11.75000000001115552, -100.5000000000000426 ) ) ;
#136421 = STYLED_ITEM ( 'NONE', ( #127725 ), #190377 ) ;
#136422 = VERTEX_POINT ( 'NONE', #130202 ) ;
#136423 = FACE_OUTER_BOUND ( 'NONE', #175030, .T. ) ;
#136424 = EDGE_CURVE ( 'NONE', #251180, #29639, #234439, .T. ) ;
#136425 = EDGE_LOOP ( 'NONE', ( #185162, #90778, #183690, #159149 ) ) ;
#136426 = DIRECTION ( 'NONE',  ( 1.000000000000000000, 7.049440681616512959E-16, -1.911869773728117674E-16 ) ) ;
#136427 = AXIS2_PLACEMENT_3D ( 'NONE', #156307, #57142, #78005 ) ;
#136428 = ADVANCED_FACE ( 'NONE', ( #113218 ), #252717, .T. ) ;
#136429 = ADVANCED_FACE ( 'NONE', ( #170685 ), #171956, .T. ) ;
#136430 = VERTEX_POINT ( 'NONE', #192770 ) ;
#136431 = SURFACE_SIDE_STYLE ('',( #118184 ) ) ;
#136432 = CARTESIAN_POINT ( 'NONE',  ( -23.25000000000000000, 67.23127455305835554, -235.8551265064784559 ) ) ;
#136434 = ORIENTED_EDGE ( 'NONE', *, *, #246684, .T. ) ;
#136433 = ORIENTED_EDGE ( 'NONE', *, *, #235329, .T. ) ;
#136435 = VERTEX_POINT ( 'NONE', #74132 ) ;
#136436 = CIRCLE ( 'NONE', #40830, 0.1000000000000024342 ) ;
#136437 = CIRCLE ( 'NONE', #211492, 0.1000000000000021289 ) ;
#136438 = ORIENTED_EDGE ( 'NONE', *, *, #247646, .F. ) ;
#136439 = ORIENTED_EDGE ( 'NONE', *, *, #108863, .F. ) ;
#136440 = ADVANCED_FACE ( 'NONE', ( #233200 ), #149810, .T. ) ;
#136441 = PLANE ( 'NONE',  #80303 ) ;
#136442 = CARTESIAN_POINT ( 'NONE',  ( -16.86420534634261514, 30.27630137067296090, -234.8211406191147717 ) ) ;
#136444 = ORIENTED_EDGE ( 'NONE', *, *, #227686, .T. ) ;
#136443 = DIRECTION ( 'NONE',  ( 1.000000000000000000, -0.000000000000000000, 0.000000000000000000 ) ) ;
#136445 = FACE_OUTER_BOUND ( 'NONE', #190863, .T. ) ;
#136446 = ADVANCED_FACE ( 'NONE', ( #194067 ), #31163, .T. ) ;
#136447 = CARTESIAN_POINT ( 'NONE',  ( 12.47034474403011473, 12.53792204840291546, -214.5112614470119183 ) ) ;
#136449 = VERTEX_POINT ( 'NONE', #15427 ) ;
#136448 = DIRECTION ( 'NONE',  ( 0.000000000000000000, 0.2128009952263605620, -0.9770955615653315052 ) ) ;
#136450 = DIRECTION ( 'NONE',  ( 0.000000000000000000, 1.000000000000000000, -0.000000000000000000 ) ) ;
#136452 = EDGE_CURVE ( 'NONE', #218711, #142216, #156054, .T. ) ;
#136451 = ORIENTED_EDGE ( 'NONE', *, *, #93828, .F. ) ;
#136453 = LINE ( 'NONE', #197731, #195759 ) ;
#136455 = ORIENTED_EDGE ( 'NONE', *, *, #29121, .T. ) ;
#136454 = SPHERICAL_SURFACE ( 'NONE', #168664, 0.1000000000000000056 ) ;
#136456 = CIRCLE ( 'NONE', #169855, 11.80000000000000426 ) ;
#136457 = CARTESIAN_POINT ( 'NONE',  ( 22.39999999999999858, 68.20922040163875977, -136.6231074845243540 ) ) ;
#136458 = DIRECTION ( 'NONE',  ( 1.000000000000000000, 0.000000000000000000, 0.000000000000000000 ) ) ;
#136459 = AXIS2_PLACEMENT_3D ( 'NONE', #140660, #162819, #218903 ) ;
#136460 = CARTESIAN_POINT ( 'NONE',  ( -16.92209698673556062, 9.950000000011138823, -87.78936443294738012 ) ) ;
#136461 = ORIENTED_EDGE ( 'NONE', *, *, #147242, .F. ) ;
#136463 = DIRECTION ( 'NONE',  ( 0.000000000000000000, 0.000000000000000000, 1.000000000000000000 ) ) ;
#136462 = DIRECTION ( 'NONE',  ( -0.000000000000000000, -0.000000000000000000, 1.000000000000000000 ) ) ;
#136464 = VECTOR ( 'NONE', #128256, 1000.000000000000000 ) ;
#136465 = CARTESIAN_POINT ( 'NONE',  ( -21.05000000000000071, 1.115600667400684642E-11, -196.9999999999999432 ) ) ;
#136466 = DIRECTION ( 'NONE',  ( 0.000000000000000000, 0.000000000000000000, 1.000000000000000000 ) ) ;
#136467 = DIRECTION ( 'NONE',  ( 0.000000000000000000, 0.000000000000000000, -1.000000000000000000 ) ) ;
#136468 = ORIENTED_EDGE ( 'NONE', *, *, #130374, .F. ) ;
#136469 = VERTEX_POINT ( 'NONE', #188915 ) ;
#136470 = CARTESIAN_POINT ( 'NONE',  ( -18.70000000000000284, -1.311673547813416718, -7.986648289447971116 ) ) ;
#136471 = DIRECTION ( 'NONE',  ( 0.000000000000000000, 0.1495327102803586661, 0.9887567792719350601 ) ) ;
#136473 = ORIENTED_EDGE ( 'NONE', *, *, #128235, .F. ) ;
#136472 = ADVANCED_FACE ( 'NONE', ( #211049 ), #231909, .F. ) ;
#136474 = CARTESIAN_POINT ( 'NONE',  ( -22.50000000000000000, 76.00000000001173817, -81.17267829206912211 ) ) ;
#136475 = ORIENTED_EDGE ( 'NONE', *, *, #252273, .F. ) ;
#136476 = ADVANCED_FACE ( 'NONE', ( #196601 ), #101838, .T. ) ;
#136477 = DIRECTION ( 'NONE',  ( 0.000000000000000000, 0.8814952561688444987, -0.4721928772777320149 ) ) ;
#136478 = CARTESIAN_POINT ( 'NONE',  ( -21.07094088545368393, 75.90110629746020265, -176.3432747064415196 ) ) ;
#136479 = CIRCLE ( 'NONE', #61672, 3.900000000000000355 ) ;
#136480 = AXIS2_PLACEMENT_3D ( 'NONE', #249764, #107677, #166408 ) ;
#136481 = AXIS2_PLACEMENT_3D ( 'NONE', #107345, #65653, #185609 ) ;
#136483 = ADVANCED_FACE ( 'NONE', ( #137901 ), #122740, .T. ) ;
#136482 = VERTEX_POINT ( 'NONE', #180903 ) ;
#136484 = VECTOR ( 'NONE', #244418, 1000.000000000000000 ) ;
#136485 = DIRECTION ( 'NONE',  ( 1.000000000000000000, -0.000000000000000000, 0.000000000000000000 ) ) ;
#136486 = AXIS2_PLACEMENT_3D ( 'NONE', #12694, #252544, #233020 ) ;
#136487 = B_SPLINE_CURVE_WITH_KNOTS ( 'NONE', 3,
 ( #3126, #82650, #241754, #142642, #34835, #136442, #59457, #114346, #257632, #118191 ),
 .UNSPECIFIED., .F., .F.,
 ( 4, 3, 3, 4 ),
 ( 7.632826238684376041E-06, 4.756916949875301682E-05, 9.484459048150192589E-05, 0.0001435500935099878316 ),
 .UNSPECIFIED. ) ;
#136488 = VERTEX_POINT ( 'NONE', #2238 ) ;
#136489 = ORIENTED_EDGE ( 'NONE', *, *, #37492, .F. ) ;
#136490 = ORIENTED_EDGE ( 'NONE', *, *, #70948, .T. ) ;
#136491 = DIRECTION ( 'NONE',  ( -1.000000000000000000, -0.000000000000000000, -0.000000000000000000 ) ) ;
#136492 = DIRECTION ( 'NONE',  ( 0.000000000000000000, 0.9999176327611370985, -0.01283462868041286391 ) ) ;
#136493 = CARTESIAN_POINT ( 'NONE',  ( -16.92132318717937522, 66.03392997600563774, -56.90070085417232804 ) ) ;
#136494 = DIRECTION ( 'NONE',  ( 1.296989514748957922E-15, -0.9887567792719341719, 0.1495327102803664099 ) ) ;
#136495 = CARTESIAN_POINT ( 'NONE',  ( 15.75000000000000000, 66.65000000001204228, -119.6573643172504973 ) ) ;
#136497 = DIRECTION ( 'NONE',  ( 2.694716079187272946E-16, -1.000000000000000000, 0.000000000000000000 ) ) ;
#136496 = CARTESIAN_POINT ( 'NONE',  ( 21.07954640115206502, 0.06600770715081333284, -161.1707123039770408 ) ) ;
#136498 = LINE ( 'NONE', #217320, #54091 ) ;
#136500 = ORIENTED_EDGE ( 'NONE', *, *, #87901, .F. ) ;
#136499 = CARTESIAN_POINT ( 'NONE',  ( 18.59999999999999432, 18.14639373905162145, -237.6648341169113792 ) ) ;
#136501 = CARTESIAN_POINT ( 'NONE',  ( 18.59999999999998721, 69.15387683765952431, -132.7853812176745407 ) ) ;
#136502 = ORIENTED_EDGE ( 'NONE', *, *, #107405, .F. ) ;
#136503 = DIRECTION ( 'NONE',  ( 0.000000000000000000, 0.000000000000000000, -1.000000000000000000 ) ) ;
#136504 = VERTEX_POINT ( 'NONE', #178358 ) ;
#136505 = ORIENTED_EDGE ( 'NONE', *, *, #150368, .T. ) ;
#136506 = CARTESIAN_POINT ( 'NONE',  ( 21.14999999999999858, -0.09999999998884338825, -167.4999999999999716 ) ) ;
#136507 = CIRCLE ( 'NONE', #219716, 0.1000000000000070832 ) ;
#136508 = CARTESIAN_POINT ( 'NONE',  ( -21.04999999999999716, 6.440770893673127162, -134.0175971870084481 ) ) ;
#136510 = EDGE_CURVE ( 'NONE', #222594, #90426, #118644, .T. ) ;
#136509 = CARTESIAN_POINT ( 'NONE',  ( 22.60000000000000142, 76.00000000001213607, -136.5231074845242745 ) ) ;
#136511 = ORIENTED_EDGE ( 'NONE', *, *, #42577, .F. ) ;
#136512 = DIRECTION ( 'NONE',  ( 0.000000000000000000, 0.2128009952263604787, -0.9770955615653315052 ) ) ;
#136513 = ADVANCED_FACE ( 'NONE', ( #179634 ), #64457, .T. ) ;
#136514 = AXIS2_PLACEMENT_3D ( 'NONE', #101969, #159423, #98113 ) ;
#136515 = CARTESIAN_POINT ( 'NONE',  ( 20.94999999999999574, 40.74071615341952679, -237.9411309446948337 ) ) ;
#136516 = ORIENTED_EDGE ( 'NONE', *, *, #121340, .F. ) ;
#136517 = ORIENTED_EDGE ( 'NONE', *, *, #243538, .T. ) ;
#136519 = EDGE_CURVE ( 'NONE', #141640, #206438, #85259, .T. ) ;
#136518 = DIRECTION ( 'NONE',  ( 0.000000000000000000, -0.09425075112712516523, -0.9955484899852807823 ) ) ;
#136520 = ORIENTED_EDGE ( 'NONE', *, *, #138319, .T. ) ;
#136521 = CARTESIAN_POINT ( 'NONE',  ( -16.93262454970420094, 60.86897606381956649, -221.1025001777335888 ) ) ;
#136522 = LINE ( 'NONE', #210953, #240272 ) ;
#136523 = ORIENTED_EDGE ( 'NONE', *, *, #225424, .F. ) ;
#136524 = CARTESIAN_POINT ( 'NONE',  ( 20.94999999999999574, 65.37642973952982572, -196.0311622812938879 ) ) ;
#136525 = DIRECTION ( 'NONE',  ( 0.000000000000000000, 0.9126074666063773710, 0.4088369013363269966 ) ) ;
#136526 = FACE_OUTER_BOUND ( 'NONE', #204378, .T. ) ;
#136527 = ORIENTED_EDGE ( 'NONE', *, *, #210467, .T. ) ;
#136528 = EDGE_CURVE ( 'NONE', #70888, #132861, #239419, .T. ) ;
#136529 = DIRECTION ( 'NONE',  ( 0.000000000000000000, 0.000000000000000000, 1.000000000000000000 ) ) ;
#136531 = EDGE_CURVE ( 'NONE', #73853, #153900, #231068, .T. ) ;
#136530 = FACE_OUTER_BOUND ( 'NONE', #52911, .T. ) ;
#136532 = VECTOR ( 'NONE', #233143, 1000.000000000000114 ) ;
#136534 = CIRCLE ( 'NONE', #36636, 0.09999999999999538425 ) ;
#136533 = CARTESIAN_POINT ( 'NONE',  ( -22.49917693094574034, 25.99238864986915942, -254.2362476092667123 ) ) ;
#136535 = AXIS2_PLACEMENT_3D ( 'NONE', #159996, #239515, #101224 ) ;
#136536 = EDGE_CURVE ( 'NONE', #200569, #235587, #135157, .T. ) ;
#136537 = ORIENTED_EDGE ( 'NONE', *, *, #15510, .T. ) ;
#136539 = EDGE_CURVE ( 'NONE', #193203, #248447, #56050, .T. ) ;
#136538 = ADVANCED_FACE ( 'NONE', ( #41410 ), #235726, .F. ) ;
#136540 = CARTESIAN_POINT ( 'NONE',  ( 21.07928932188134397, 61.09751618602743406, -234.2940654522722639 ) ) ;
#136541 = ORIENTED_EDGE ( 'NONE', *, *, #165084, .F. ) ;
#136542 = CARTESIAN_POINT ( 'NONE',  ( -23.15000000000000213, 76.00000000001244871, -170.0231074845243597 ) ) ;
#136543 = ADVANCED_FACE ( 'NONE', ( #81757 ), #255242, .F. ) ;
#136544 = DIRECTION ( 'NONE',  ( 0.000000000000000000, -6.982962677686266711E-15, 1.000000000000000000 ) ) ;
#136545 = CARTESIAN_POINT ( 'NONE',  ( -18.59999999999999787, -1.851028230140860487, -11.65391326942249250 ) ) ;
#136546 = DIRECTION ( 'NONE',  ( 1.000000000000000000, -0.000000000000000000, -0.000000000000000000 ) ) ;
#136547 = DIRECTION ( 'NONE',  ( 1.000000000000000000, 0.000000000000000000, 0.000000000000000000 ) ) ;
#136548 = ORIENTED_EDGE ( 'NONE', *, *, #25806, .F. ) ;
#136549 = CARTESIAN_POINT ( 'NONE',  ( -16.97092634996628036, 65.99911103366434872, -149.1532502508223672 ) ) ;
#136550 = CARTESIAN_POINT ( 'NONE',  ( -20.64999999999999858, 7.249999999999999112, -12.25000000000000000 ) ) ;
#136551 = CIRCLE ( 'NONE', #40755, 0.09999999999999961697 ) ;
#136552 = CARTESIAN_POINT ( 'NONE',  ( -18.58744394320989102, 77.36894789412127693, -241.7960489703176563 ) ) ;
#136553 = DIRECTION ( 'NONE',  ( -2.940209281316621509E-16, 1.000000000000000000, 0.000000000000000000 ) ) ;
#136554 = CIRCLE ( 'NONE', #24157, 0.1999999999999987899 ) ;
#136555 = EDGE_CURVE ( 'NONE', #19947, #33844, #218537, .T. ) ;
#136556 = ADVANCED_FACE ( 'NONE', ( #136621 ), #79209, .F. ) ;
#136557 = CARTESIAN_POINT ( 'NONE',  ( 20.11144452914042802, 66.06638914889163061, -61.63281403056953422 ) ) ;
#136558 =( BOUNDED_SURFACE ( )  B_SPLINE_SURFACE ( 3, 2, ( 
 ( #65657, #145186, #224722 ),
 ( #9532, #6968, #206459 ),
 ( #89066, #87772, #48659 ),
 ( #30406, #188188, #107349 ),
 ( #186925, #185614, #163483 ),
 ( #8272, #244287, #167363 ) ),
 .UNSPECIFIED., .F., .F., .T. ) 
 B_SPLINE_SURFACE_WITH_KNOTS ( ( 4, 2, 4 ),
 ( 3, 3 ),
 ( 0.0001381104793128072085, 0.0002947094729387660984, 0.0004513084665647249883 ),
 ( 0.000000000000000000, 1.000000000000000000 ),
 .UNSPECIFIED. ) 
 GEOMETRIC_REPRESENTATION_ITEM ( )  RATIONAL_B_SPLINE_SURFACE ( (
 ( 1.000000000000000000, 0.7071067811866307284, 1.000000000000000000),
 ( 1.000000000000000000, 0.6919563088109071947, 1.000000000000000000),
 ( 1.000000000000000000, 0.6959445945703722769, 1.000000000000000000),
 ( 1.000000000000000000, 0.7137882985326097218, 1.000000000000000000),
 ( 1.000000000000000000, 0.7257496306086942406, 1.000000000000000000),
 ( 1.000000000000000000, 0.7250110520819876836, 1.000000000000000000) ) ) 
 REPRESENTATION_ITEM ( '' )  SURFACE ( )  );
#136559 = CIRCLE ( 'NONE', #244902, 0.1000000000000024342 ) ;
#136560 = ORIENTED_EDGE ( 'NONE', *, *, #173175, .T. ) ;
#136561 = ORIENTED_EDGE ( 'NONE', *, *, #38212, .F. ) ;
#136562 = DIRECTION ( 'NONE',  ( 2.952720810173289112E-16, 1.000000000000000000, 6.308085367188367561E-15 ) ) ;
#136563 = DIRECTION ( 'NONE',  ( -1.000000000000000000, -0.000000000000000000, -0.000000000000000000 ) ) ;
#136565 = EDGE_CURVE ( 'NONE', #189309, #50227, #37553, .T. ) ;
#136564 = CARTESIAN_POINT ( 'NONE',  ( -23.15000000000000213, 11.75000000001115552, -146.1500000000000341 ) ) ;
#136566 = CARTESIAN_POINT ( 'NONE',  ( 21.05000000000000426, 58.86930248204848937, -225.7185241593660692 ) ) ;
#136567 = CARTESIAN_POINT ( 'NONE',  ( -20.85000000000000142, 78.48087866980282001, -232.8271061603568910 ) ) ;
#136568 = VERTEX_POINT ( 'NONE', #77935 ) ;
#136569 = ADVANCED_FACE ( 'NONE', ( #98750 ), #40137, .T. ) ;
#136570 = EDGE_CURVE ( 'NONE', #153937, #256858, #31360, .T. ) ;
#136571 = DIRECTION ( 'NONE',  ( 1.000000000000000000, 0.000000000000000000, 0.000000000000000000 ) ) ;
#136572 = EDGE_LOOP ( 'NONE', ( #69645, #59538, #146272, #123987 ) ) ;
#136573 = DIRECTION ( 'NONE',  ( 1.000000000000000000, 0.000000000000000000, 0.000000000000000000 ) ) ;
#136574 = DIRECTION ( 'NONE',  ( 0.000000000000000000, -0.4999999999999413247, 0.8660254037844724584 ) ) ;
#136575 = AXIS2_PLACEMENT_3D ( 'NONE', #140680, #145804, #62439 ) ;
#136576 = VECTOR ( 'NONE', #96925, 1000.000000000000000 ) ;
#136577 = CIRCLE ( 'NONE', #40946, 0.1999999999999945155 ) ;
#136578 = ORIENTED_EDGE ( 'NONE', *, *, #114162, .F. ) ;
#136579 = CARTESIAN_POINT ( 'NONE',  ( -21.05000000000000071, 12.82201439108308527, -205.1891724321641277 ) ) ;
#136580 = VERTEX_POINT ( 'NONE', #66079 ) ;
#136581 = ADVANCED_FACE ( 'NONE', ( #102607 ), #26984, .T. ) ;
#136582 = DIRECTION ( 'NONE',  ( 0.000000000000000000, 0.000000000000000000, 1.000000000000000000 ) ) ;
#136583 = FACE_OUTER_BOUND ( 'NONE', #251158, .T. ) ;
#136584 = CARTESIAN_POINT ( 'NONE',  ( -21.29999999999995808, 1.115600667400684642E-11, -100.5000000000000284 ) ) ;
#136585 = DIRECTION ( 'NONE',  ( -1.000000000000000000, -0.000000000000000000, -0.000000000000000000 ) ) ;
#136586 = CARTESIAN_POINT ( 'NONE',  ( 20.94999999999999929, 6.649999999999999467, -10.01702717044001822 ) ) ;
#136587 = DIRECTION ( 'NONE',  ( 0.000000000000000000, 7.147358527629766941E-15, -1.000000000000000000 ) ) ;
#136588 = DIRECTION ( 'NONE',  ( 0.000000000000000000, 0.000000000000000000, 1.000000000000000000 ) ) ;
#136589 = CARTESIAN_POINT ( 'NONE',  ( -20.94999999999999929, -4.756823075239758225, -233.1486023682345490 ) ) ;
#136590 = EDGE_CURVE ( 'NONE', #235379, #14771, #206292, .T. ) ;
#136591 = LINE ( 'NONE', #216136, #225560 ) ;
#136592 = CARTESIAN_POINT ( 'NONE',  ( -18.40000000000000213, 64.66825945288744037, -190.8731074845244393 ) ) ;
#136593 = LINE ( 'NONE', #137873, #77299 ) ;
#136594 = CARTESIAN_POINT ( 'NONE',  ( 18.50000972452444969, 10.29326151435342851, -206.4592822510414010 ) ) ;
#136595 = VECTOR ( 'NONE', #8108, 1000.000000000000000 ) ;
#136596 = CIRCLE ( 'NONE', #174073, 4.049999999999998046 ) ;
#136597 = CIRCLE ( 'NONE', #169983, 0.09999999999999935330 ) ;
#136598 = DIRECTION ( 'NONE',  ( 1.000000000000000000, 0.000000000000000000, 0.000000000000000000 ) ) ;
#136599 = CARTESIAN_POINT ( 'NONE',  ( 20.94999999999999929, 56.27731819600170837, -227.9967441372480437 ) ) ;
#136600 = AXIS2_PLACEMENT_3D ( 'NONE', #214200, #35585, #254570 ) ;
#136601 = VERTEX_POINT ( 'NONE', #144303 ) ;
#136602 = CARTESIAN_POINT ( 'NONE',  ( 21.05000000000000071, 6.441084688471240050, -0.01771943330862802563 ) ) ;
#136603 = CYLINDRICAL_SURFACE ( 'NONE', #195999, 0.09999999999999939493 ) ;
#136604 = EDGE_CURVE ( 'NONE', #214102, #210483, #231250, .T. ) ;
#136605 = DIRECTION ( 'NONE',  ( 0.000000000000000000, -0.2605042016806740079, 0.9654727137038698892 ) ) ;
#136606 =( BOUNDED_SURFACE ( )  B_SPLINE_SURFACE ( 3, 2, ( 
 ( #28095, #65910, #64613 ),
 ( #204118, #88009, #128453 ),
 ( #103717, #145430, #125865 ),
 ( #185850, #46328, #167598 ),
 ( #247093, #224956, #68483 ),
 ( #86728, #108881, #205394 ) ),
 .UNSPECIFIED., .F., .F., .F. ) 
 B_SPLINE_SURFACE_WITH_KNOTS ( ( 4, 2, 4 ),
 ( 3, 3 ),
 ( 1.570796326794897668, 2.356194490192346169, 3.141592653589794448 ),
 ( 0.000000000000000000, 1.000000000000000000 ),
 .UNSPECIFIED. ) 
 GEOMETRIC_REPRESENTATION_ITEM ( )  RATIONAL_B_SPLINE_SURFACE ( (
 ( 1.000000000000000000, 0.7071067811865597852, 1.000000000000000000),
 ( 1.000000000000000000, 0.6611148371781027100, 1.000000000000000000),
 ( 1.000000000000000000, 0.6092287576693442563, 1.000000000000000000),
 ( 1.000000000000000000, 0.5278258667060597986, 1.000000000000000000),
 ( 1.000000000000000000, 0.4993418825332296973, 1.000000000000000000),
 ( 1.000000000000000000, 0.5000000000000456302, 1.000000000000000000) ) ) 
 REPRESENTATION_ITEM ( '' )  SURFACE ( )  );
#136607 = ORIENTED_EDGE ( 'NONE', *, *, #13120, .T. ) ;
#136608 = CARTESIAN_POINT ( 'NONE',  ( -18.50000000000000000, 1.115600667400684642E-11, -67.00000000000000000 ) ) ;
#136609 = CYLINDRICAL_SURFACE ( 'NONE', #147120, 0.09999999999999939493 ) ;
#136610 = ORIENTED_EDGE ( 'NONE', *, *, #184979, .T. ) ;
#136611 = LINE ( 'NONE', #153692, #105031 ) ;
#136612 = DIRECTION ( 'NONE',  ( -1.000000000000000000, -0.000000000000000000, -0.000000000000000000 ) ) ;
#136613 = CIRCLE ( 'NONE', #232335, 11.90000000000000036 ) ;
#136614 = EDGE_CURVE ( 'NONE', #12940, #59445, #52149, .T. ) ;
#136615 = EDGE_LOOP ( 'NONE', ( #207009, #112050, #197071, #67624 ) ) ;
#136616 = CIRCLE ( 'NONE', #170010, 0.1999999999999997335 ) ;
#136617 = AXIS2_PLACEMENT_3D ( 'NONE', #109194, #250006, #227875 ) ;
#136618 = AXIS2_PLACEMENT_3D ( 'NONE', #2687, #82202, #181366 ) ;
#136620 = ORIENTED_EDGE ( 'NONE', *, *, #257612, .F. ) ;
#136619 = AXIS2_PLACEMENT_3D ( 'NONE', #217496, #38897, #182250 ) ;
#136621 = FACE_OUTER_BOUND ( 'NONE', #183223, .T. ) ;
#136622 = EDGE_LOOP ( 'NONE', ( #110033, #30185, #119092, #40404 ) ) ;
#136623 = CIRCLE ( 'NONE', #157340, 0.5000000000000004441 ) ;
#136624 = FACE_OUTER_BOUND ( 'NONE', #231535, .T. ) ;
#136625 = FACE_OUTER_BOUND ( 'NONE', #127466, .T. ) ;
#136627 = DIRECTION ( 'NONE',  ( 0.000000000000000000, -0.8814952561688437216, 0.4721928772777334582 ) ) ;
#136626 = UNCERTAINTY_MEASURE_WITH_UNIT (LENGTH_MEASURE( 1.000000000000000082E-05 ), #169937, 'distance_accuracy_value', 'NONE');
#136628 = CARTESIAN_POINT ( 'NONE',  ( 21.14999999999999858, 11.65000000001116298, -45.65000000000000568 ) ) ;
#136629 = DIRECTION ( 'NONE',  ( 0.000000000000000000, 0.5907332058517377193, -0.8068669527896954463 ) ) ;
#136630 = DIRECTION ( 'NONE',  ( 1.000000000000000000, 0.000000000000000000, 0.000000000000000000 ) ) ;
#136631 = DIRECTION ( 'NONE',  ( -1.000000000000000000, 7.492892343619937423E-30, -1.073024830501117725E-15 ) ) ;
#136632 = CARTESIAN_POINT ( 'NONE',  ( -22.59999999999999787, 76.00000000001213607, -136.5231074845242745 ) ) ;
#136634 = ORIENTED_EDGE ( 'NONE', *, *, #49097, .F. ) ;
#136633 = CARTESIAN_POINT ( 'NONE',  ( -18.50000000000000000, -9.419203418015493767, -40.74778581042865255 ) ) ;
#136635 = EDGE_LOOP ( 'NONE', ( #34546, #224366, #155096, #63331 ) ) ;
#136637 = CARTESIAN_POINT ( 'NONE',  ( 21.30000000000002558, 1.115600667400684642E-11, -163.4499999999999886 ) ) ;
#136636 = CARTESIAN_POINT ( 'NONE',  ( -20.99142135623731065, 11.60000000001115161, -160.5717967697245285 ) ) ;
#136639 = ORIENTED_EDGE ( 'NONE', *, *, #148283, .F. ) ;
#136638 = FACE_OUTER_BOUND ( 'NONE', #145732, .T. ) ;
#136640 = VERTEX_POINT ( 'NONE', #162627 ) ;
#136641 = DIRECTION ( 'NONE',  ( 0.000000000000000000, 1.000000000000000000, 0.000000000000000000 ) ) ;
#136642 = CIRCLE ( 'NONE', #215921, 0.1000000000000001860 ) ;
#136643 = VECTOR ( 'NONE', #44839, 1000.000000000000114 ) ;
#136644 = CARTESIAN_POINT ( 'NONE',  ( 20.77526135991796608, 8.932009016637321608, -175.9685685427218971 ) ) ;
#136645 = CLOSED_SHELL ( 'NONE', ( #223881, #208176, #101084, #127507, #46716, #253959, #70034, #154768, #171314, #182417, #223770, #196170, #231624, #243606, #54169, #66958, #213600, #54183, #240819, #169205, #67621, #232782, #126788, #7280, #144190, #210679, #145867, #138436, #147317, #27882, #129297, #129769, #183117, #120973, #182456, #210595, #20155, #50176, #15643, #149481, #126088, #178564, #248439, #53666, #250699, #132935, #8152, #232477, #1354, #131539, #38038, #177995, #138305 ) ) ;
#136646 = FACE_OUTER_BOUND ( 'NONE', #101535, .T. ) ;
#136647 = CARTESIAN_POINT ( 'NONE',  ( -18.59999999999999787, 11.65000000001115232, -40.41480577065399871 ) ) ;
#136648 = CARTESIAN_POINT ( 'NONE',  ( 20.84999999999998721, 18.41524492703432614, -237.0006385043383546 ) ) ;
#136649 = DIRECTION ( 'NONE',  ( -4.336808689941751101E-15, -0.03181660087581671820, 0.9994937237965574317 ) ) ;
#136650 = CARTESIAN_POINT ( 'NONE',  ( 23.15000000000000213, 85.50000000001207923, -126.6291383618717816 ) ) ;
#136651 = AXIS2_PLACEMENT_3D ( 'NONE', #171834, #253885, #135213 ) ;
#136652 = EDGE_CURVE ( 'NONE', #238381, #208354, #166499, .T. ) ;
#136653 = CARTESIAN_POINT ( 'NONE',  ( -23.25000000000000000, 62.92003201576280702, -207.2439188921395896 ) ) ;
#136654 = ORIENTED_EDGE ( 'NONE', *, *, #238732, .T. ) ;
#136655 = VERTEX_POINT ( 'NONE', #223853 ) ;
#136656 = CARTESIAN_POINT ( 'NONE',  ( -21.05000000000000071, 1.115649653272650466E-11, -204.9999999999999716 ) ) ;
#136657 = AXIS2_PLACEMENT_3D ( 'NONE', #241475, #2837, #221877 ) ;
#136658 = ORIENTED_EDGE ( 'NONE', *, *, #95176, .T. ) ;
#136659 = DIRECTION ( 'NONE',  ( -7.304098846218134667E-16, 1.000000000000000000, 6.982962677686266711E-15 ) ) ;
#136660 = VERTEX_POINT ( 'NONE', #107775 ) ;
#136661 = CARTESIAN_POINT ( 'NONE',  ( -20.94999999999999929, 79.13126459505528487, -235.8705213229730191 ) ) ;
#136662 = AXIS2_PLACEMENT_3D ( 'NONE', #167291, #246784, #22635 ) ;
#136663 = CARTESIAN_POINT ( 'NONE',  ( 20.05000000000002913, 63.54522198573871350, -221.7484608313106378 ) ) ;
#136664 = DIRECTION ( 'NONE',  ( 0.000000000000000000, -1.000000000000000000, -6.860497997771532351E-15 ) ) ;
#136665 = EDGE_CURVE ( 'NONE', #218718, #142016, #105156, .T. ) ;
#136667 = ORIENTED_EDGE ( 'NONE', *, *, #52388, .T. ) ;
#136666 = CARTESIAN_POINT ( 'NONE',  ( -23.25000000000000000, -9.000000000000001776, -24.20603087734755832 ) ) ;
#136668 = DIRECTION ( 'NONE',  ( 0.000000000000000000, 1.000000000000000000, 0.000000000000000000 ) ) ;
#136669 = ORIENTED_EDGE ( 'NONE', *, *, #178712, .F. ) ;
#136670 = AXIS2_PLACEMENT_3D ( 'NONE', #10771, #150294, #207700 ) ;
#136671 = CARTESIAN_POINT ( 'NONE',  ( -21.14999999999999858, -10.86374996222471268, -206.3339888224507206 ) ) ;
#136672 = EDGE_CURVE ( 'NONE', #12413, #73105, #226952, .T. ) ;
#136673 = CARTESIAN_POINT ( 'NONE',  ( -18.59999999999999787, 102.4393534156129562, -118.3815988770166427 ) ) ;
#136674 = AXIS2_PLACEMENT_3D ( 'NONE', #71147, #185935, #150666 ) ;
#136675 = CARTESIAN_POINT ( 'NONE',  ( -22.47007471830799474, 29.61294623328925013, -252.7076741202934898 ) ) ;
#136676 = FACE_OUTER_BOUND ( 'NONE', #146900, .T. ) ;
#136677 = AXIS2_PLACEMENT_3D ( 'NONE', #183230, #39889, #144073 ) ;
#136678 = DIRECTION ( 'NONE',  ( 0.000000000000000000, -7.147358527629762208E-15, 1.000000000000000000 ) ) ;
#136679 = VERTEX_POINT ( 'NONE', #204293 ) ;
#136680 = CYLINDRICAL_SURFACE ( 'NONE', #94063, 0.09999999999999781286 ) ;
#136681 = EDGE_CURVE ( 'NONE', #183742, #58187, #165185, .T. ) ;
#136682 = ORIENTED_EDGE ( 'NONE', *, *, #194948, .T. ) ;
#136685 = ORIENTED_EDGE ( 'NONE', *, *, #101970, .T. ) ;
#136684 = CARTESIAN_POINT ( 'NONE',  ( -23.25000000000000000, -3.187427350888460076, -228.3200064793908837 ) ) ;
#136683 = DIRECTION ( 'NONE',  ( 0.000000000000000000, 0.000000000000000000, 1.000000000000000000 ) ) ;
#136686 = AXIS2_PLACEMENT_3D ( 'NONE', #161474, #257927, #179743 ) ;
#136687 = CARTESIAN_POINT ( 'NONE',  ( -21.14999999999999858, 60.91865828504416669, -234.1430899377568551 ) ) ;
#136688 = EDGE_CURVE ( 'NONE', #248699, #59743, #106292, .T. ) ;
#136689 = CARTESIAN_POINT ( 'NONE',  ( -22.45305610364635740, -2.598867842139048534, -189.5410128746471798 ) ) ;
#136690 = ORIENTED_EDGE ( 'NONE', *, *, #108147, .F. ) ;
#136691 = CARTESIAN_POINT ( 'NONE',  ( -21.05000000000000071, 70.15000000001266756, -193.3906102602464330 ) ) ;
#136692 = EDGE_CURVE ( 'NONE', #254925, #216004, #28278, .T. ) ;
#136693 = CARTESIAN_POINT ( 'NONE',  ( 20.85000000000000142, 76.00000000001244871, -170.0231074845243597 ) ) ;
#136694 = EDGE_CURVE ( 'NONE', #212250, #20048, #117224, .T. ) ;
#136695 = DIRECTION ( 'NONE',  ( 0.000000000000000000, 0.1350103645451945777, -0.9908441862701591329 ) ) ;
#136697 = ORIENTED_EDGE ( 'NONE', *, *, #119420, .F. ) ;
#136696 = DIRECTION ( 'NONE',  ( 1.000000000000000000, 0.000000000000000000, 0.000000000000000000 ) ) ;
#136698 = CYLINDRICAL_SURFACE ( 'NONE', #247624, 0.09999999999999939493 ) ;
#136699 = EDGE_CURVE ( 'NONE', #100102, #78058, #110411, .T. ) ;
#136700 = ORIENTED_EDGE ( 'NONE', *, *, #243138, .T. ) ;
#136701 = LINE ( 'NONE', #196677, #45268 ) ;
#136702 = DIRECTION ( 'NONE',  ( 0.000000000000000000, -0.03181660087583042251, 0.9994937237965568766 ) ) ;
#136703 = DIRECTION ( 'NONE',  ( -0.7071067811865456854, -0.7071067811865493491, -4.937700262164544098E-15 ) ) ;
#136704 = ORIENTED_EDGE ( 'NONE', *, *, #81865, .T. ) ;
#136705 = DIRECTION ( 'NONE',  ( 0.000000000000000000, 0.000000000000000000, -1.000000000000000000 ) ) ;
#136706 = EDGE_LOOP ( 'NONE', ( #102311, #34178, #257416, #226177, #155190, #242871, #72197, #204792, #91394, #98882, #140563, #146861, #111633, #16184, #193423, #76606, #85748, #107718, #106909, #233582, #144638, #242832, #157979, #55963, #177409, #167962, #210069 ) ) ;
#136707 = CARTESIAN_POINT ( 'NONE',  ( 18.59999999999999076, 6.550000000011156231, -188.7499999999999716 ) ) ;
#136708 = CARTESIAN_POINT ( 'NONE',  ( 20.94999999999999574, 1.162701749949165642, -175.3999999999999773 ) ) ;
#136709 = DIRECTION ( 'NONE',  ( 0.000000000000000000, -0.9126074666063770380, -0.4088369013363281068 ) ) ;
#136710 = ORIENTED_EDGE ( 'NONE', *, *, #57290, .F. ) ;
#136711 = CARTESIAN_POINT ( 'NONE',  ( 21.14999999999999858, 22.98593783141595992, -230.0732594427593938 ) ) ;
#136712 = EDGE_CURVE ( 'NONE', #135186, #109568, #139617, .T. ) ;
#136713 = DIRECTION ( 'NONE',  ( -0.000000000000000000, 1.000000000000000000, 6.352154140967427193E-15 ) ) ;
#136714 = DIRECTION ( 'NONE',  ( -0.000000000000000000, 1.000000000000000000, 2.891205793294679805E-16 ) ) ;
#136715 = ORIENTED_EDGE ( 'NONE', *, *, #89469, .T. ) ;
#136716 = AXIS2_PLACEMENT_3D ( 'NONE', #81095, #283, #160684 ) ;
#136717 = AXIS2_PLACEMENT_3D ( 'NONE', #138467, #218007, #36865 ) ;
#136719 = VECTOR ( 'NONE', #38331, 1000.000000000000000 ) ;
#136718 = DIRECTION ( 'NONE',  ( 0.000000000000000000, 0.5000000000000014433, -0.8660254037844378194 ) ) ;
#136720 = CARTESIAN_POINT ( 'NONE',  ( 18.50000000000000000, -9.499999999988842703, -55.25000000000004974 ) ) ;
#136721 = AXIS2_PLACEMENT_3D ( 'NONE', #90688, #9874, #73728 ) ;
#136722 = DIRECTION ( 'NONE',  ( 1.000000000000000000, 0.000000000000000000, 0.000000000000000000 ) ) ;
#136723 = EDGE_LOOP ( 'NONE', ( #166138, #63641, #70021, #20088 ) ) ;
#136724 = ADVANCED_FACE ( 'NONE', ( #163907 ), #131261, .T. ) ;
#136725 = DIRECTION ( 'NONE',  ( 0.000000000000000000, 1.000000000000000000, 0.000000000000000000 ) ) ;
#136726 = ORIENTED_EDGE ( 'NONE', *, *, #42824, .T. ) ;
#136728 = EDGE_LOOP ( 'NONE', ( #109893, #28387, #166611 ) ) ;
#136727 = CARTESIAN_POINT ( 'NONE',  ( -20.64999999999999858, 71.75000000001186606, -90.77310748452434552 ) ) ;
#136731 = VERTEX_POINT ( 'NONE', #243429 ) ;
#136730 = VERTEX_POINT ( 'NONE', #24418 ) ;
#136729 = DIRECTION ( 'NONE',  ( 0.000000000000000000, -0.000000000000000000, -1.000000000000000000 ) ) ;
#136733 = CIRCLE ( 'NONE', #132470, 0.3999999999999975797 ) ;
#136732 = DIRECTION ( 'NONE',  ( 0.000000000000000000, 0.9126074666063107577, 0.4088369013364760440 ) ) ;
#136734 = CARTESIAN_POINT ( 'NONE',  ( -20.90851465518106167, 65.67467670974367877, -30.45317318268843820 ) ) ;
#136735 = CARTESIAN_POINT ( 'NONE',  ( 18.59999999999999432, -1.637172712959223952, -145.5821533654720383 ) ) ;
#136736 = CIRCLE ( 'NONE', #157643, 0.4000000000000010214 ) ;
#136737 = CARTESIAN_POINT ( 'NONE',  ( -20.94999999999999929, -1.835341550213257733, -179.0551512925629538 ) ) ;
#136738 = DIRECTION ( 'NONE',  ( 0.000000000000000000, 0.4721928772777346239, 0.8814952561688430555 ) ) ;
#136739 = DIRECTION ( 'NONE',  ( -0.000000000000000000, 1.000000000000000000, 0.000000000000000000 ) ) ;
#136740 = ADVANCED_FACE ( 'NONE', ( #85604 ), #226414, .F. ) ;
#136741 = DIRECTION ( 'NONE',  ( 0.000000000000000000, 0.8700118002898356018, -0.4930308989875170078 ) ) ;
#136742 = CIRCLE ( 'NONE', #203412, 0.09999999999999609201 ) ;
#136743 = FACE_OUTER_BOUND ( 'NONE', #67840, .T. ) ;
#136744 = ORIENTED_EDGE ( 'NONE', *, *, #90883, .F. ) ;
#136745 = EDGE_LOOP ( 'NONE', ( #43240, #224562, #185266, #15818 ) ) ;
#136746 = EDGE_LOOP ( 'NONE', ( #33875, #81097, #232030, #62567 ) ) ;
#136747 = CARTESIAN_POINT ( 'NONE',  ( -11.59999999999994458, 64.35000000001120668, -23.72310748452479245 ) ) ;
#136749 = EDGE_LOOP ( 'NONE', ( #49608, #249970, #120562, #28424 ) ) ;
#136748 = DIRECTION ( 'NONE',  ( 0.000000000000000000, 1.000000000000000000, -6.308085367188393199E-16 ) ) ;
#136750 = DIRECTION ( 'NONE',  ( 0.000000000000000000, 0.2128009952263568982, -0.9770955615653323934 ) ) ;
#136751 = ORIENTED_EDGE ( 'NONE', *, *, #12650, .F. ) ;
#136752 = DIRECTION ( 'NONE',  ( 3.469446951953515108E-14, 1.000000000000000000, 0.000000000000000000 ) ) ;
#136753 = EDGE_CURVE ( 'NONE', #220739, #126259, #146878, .T. ) ;
#136754 = ORIENTED_EDGE ( 'NONE', *, *, #135292, .T. ) ;
#136755 = CARTESIAN_POINT ( 'NONE',  ( -18.40000000000000213, 70.35000000001230092, -157.3731074845244109 ) ) ;
#136756 = EDGE_CURVE ( 'NONE', #221411, #183267, #196006, .T. ) ;
#136757 = EDGE_CURVE ( 'NONE', #42612, #163390, #60518, .T. ) ;
#136758 = VERTEX_POINT ( 'NONE', #57748 ) ;
#136759 = DIRECTION ( 'NONE',  ( 0.000000000000000000, -0.000000000000000000, 1.000000000000000000 ) ) ;
#136760 = CARTESIAN_POINT ( 'NONE',  ( -20.94999999999999929, 87.48912529308852015, -173.0231074845243029 ) ) ;
#136761 = AXIS2_PLACEMENT_3D ( 'NONE', #1507, #172819, #52809 ) ;
#136762 = CIRCLE ( 'NONE', #53580, 0.09999999999998898659 ) ;
#136763 = AXIS2_PLACEMENT_3D ( 'NONE', #98715, #105128, #205540 ) ;
#136765 = ORIENTED_EDGE ( 'NONE', *, *, #192191, .T. ) ;
#136764 = EDGE_LOOP ( 'NONE', ( #222127, #8273, #217687, #221189 ) ) ;
#136766 = VERTEX_POINT ( 'NONE', #50341 ) ;
#136767 = DIRECTION ( 'NONE',  ( 0.000000000000000000, -1.000000000000000000, 0.000000000000000000 ) ) ;
#136768 = ORIENTED_EDGE ( 'NONE', *, *, #46126, .F. ) ;
#136769 = VERTEX_POINT ( 'NONE', #212030 ) ;
#136770 = EDGE_CURVE ( 'NONE', #4150, #252923, #77099, .T. ) ;
#136771 = CARTESIAN_POINT ( 'NONE',  ( -20.00857864376270001, 9.350000000011156942, -179.8499999999999659 ) ) ;
#136773 = ORIENTED_EDGE ( 'NONE', *, *, #191410, .F. ) ;
#136772 = DIRECTION ( 'NONE',  ( -1.000000000000000000, 0.000000000000000000, 0.000000000000000000 ) ) ;
#136774 = VECTOR ( 'NONE', #135180, 999.9999999999998863 ) ;
#136776 = DIRECTION ( 'NONE',  ( -3.469446951953515108E-14, 1.000000000000000000, 0.000000000000000000 ) ) ;
#136775 = DIRECTION ( 'NONE',  ( 2.952720810173289112E-16, -1.000000000000000000, 0.000000000000000000 ) ) ;
#136777 = LINE ( 'NONE', #199344, #211598 ) ;
#136778 = CARTESIAN_POINT ( 'NONE',  ( -20.94999999999999929, -11.64999999998884483, -137.0000000000000000 ) ) ;
#136779 = CARTESIAN_POINT ( 'NONE',  ( 22.24259225415828212, 29.78122419289665146, -252.5237351003267179 ) ) ;
#136780 = VERTEX_POINT ( 'NONE', #33414 ) ;
#136781 = ORIENTED_EDGE ( 'NONE', *, *, #140223, .T. ) ;
#136782 = CARTESIAN_POINT ( 'NONE',  ( 18.50000000000000355, 85.48068669529082797, -96.08199231576635668 ) ) ;
#136783 = DIRECTION ( 'NONE',  ( 0.000000000000000000, 6.308085367183347448E-16, 1.000000000000000000 ) ) ;
#136784 = DIRECTION ( 'NONE',  ( 1.000000000000000000, 0.000000000000000000, 0.000000000000000000 ) ) ;
#136785 = ORIENTED_EDGE ( 'NONE', *, *, #9217, .F. ) ;
#136786 = AXIS2_PLACEMENT_3D ( 'NONE', #176826, #253759, #19006 ) ;
#136788 = CARTESIAN_POINT ( 'NONE',  ( 21.00000000000000000, 9.750000000011153745, -155.1500000000000057 ) ) ;
#136787 = AXIS2_PLACEMENT_3D ( 'NONE', #123044, #85153, #202574 ) ;
#136789 = VECTOR ( 'NONE', #204008, 1000.000000000000114 ) ;
#136790 = FACE_OUTER_BOUND ( 'NONE', #73354, .T. ) ;
#136791 = CARTESIAN_POINT ( 'NONE',  ( -14.77738660682464022, 12.45029792656132095, -213.8222050902128331 ) ) ;
#136792 = AXIS2_PLACEMENT_3D ( 'NONE', #181201, #225418, #145889 ) ;
#136793 = ORIENTED_EDGE ( 'NONE', *, *, #97391, .T. ) ;
#136794 = ORIENTED_EDGE ( 'NONE', *, *, #257500, .F. ) ;
#136795 = DIRECTION ( 'NONE',  ( -1.000000000000000000, 0.000000000000000000, 0.000000000000000000 ) ) ;
#136796 = DIRECTION ( 'NONE',  ( 0.000000000000000000, 0.000000000000000000, 1.000000000000000000 ) ) ;
#136798 = EDGE_LOOP ( 'NONE', ( #157737, #110277, #41588, #38664 ) ) ;
#136797 = EDGE_CURVE ( 'NONE', #208213, #216334, #173007, .T. ) ;
#136799 = PLANE ( 'NONE',  #159820 ) ;
#136800 = ORIENTED_EDGE ( 'NONE', *, *, #24095, .T. ) ;
#136801 = EDGE_CURVE ( 'NONE', #121993, #229490, #39720, .T. ) ;
#136802 = DIRECTION ( 'NONE',  ( 1.000000000000000000, 0.000000000000000000, 0.000000000000000000 ) ) ;
#136803 = CARTESIAN_POINT ( 'NONE',  ( 18.52928932188133970, 62.89880023679608456, -212.5588616714909733 ) ) ;
#136805 = DIRECTION ( 'NONE',  ( -1.000000000000000000, 0.000000000000000000, 0.000000000000000000 ) ) ;
#136804 = CARTESIAN_POINT ( 'NONE',  ( -18.50000000000000000, 25.65398771707549841, -256.3298696899526021 ) ) ;
#136806 = AXIS2_PLACEMENT_3D ( 'NONE', #26271, #110931, #7995 ) ;
#136807 = CARTESIAN_POINT ( 'NONE',  ( 23.14999999999999858, 76.00000000001267608, -203.5231074845243597 ) ) ;
#136808 = CARTESIAN_POINT ( 'NONE',  ( 21.12769345151713196, 65.28071232307129890, -90.77562713832689667 ) ) ;
#136809 = EDGE_CURVE ( 'NONE', #22303, #236473, #251141, .T. ) ;
#136810 = AXIS2_PLACEMENT_3D ( 'NONE', #187952, #11899, #211367 ) ;
#136811 = LINE ( 'NONE', #80673, #235766 ) ;
#136814 = EDGE_LOOP ( 'NONE', ( #103231, #160471, #214358, #59381 ) ) ;
#136813 = ORIENTED_EDGE ( 'NONE', *, *, #5020, .T. ) ;
#136812 = TOROIDAL_SURFACE ( 'NONE', #207577, 11.65000000000000036, 0.1000000000000000056 ) ;
#136815 = ORIENTED_EDGE ( 'NONE', *, *, #218319, .T. ) ;
#136816 = CIRCLE ( 'NONE', #70218, 0.09999999999999939493 ) ;
#136817 = AXIS2_PLACEMENT_3D ( 'NONE', #23635, #198380, #161853 ) ;
#136818 = VECTOR ( 'NONE', #224756, 1000.000000000000000 ) ;
#136819 = DIRECTION ( 'NONE',  ( -7.304098846218134667E-16, -1.000000000000000000, 0.000000000000000000 ) ) ;
#136820 = CARTESIAN_POINT ( 'NONE',  ( 22.39999999999999503, 0.000000000000000000, 11.64957080754479968 ) ) ;
#136821 = DIRECTION ( 'NONE',  ( 0.000000000000000000, 0.000000000000000000, 1.000000000000000000 ) ) ;
#136822 = DIRECTION ( 'NONE',  ( 0.000000000000000000, 0.000000000000000000, -1.000000000000000000 ) ) ;
#136823 = AXIS2_PLACEMENT_3D ( 'NONE', #124596, #241955, #183277 ) ;
#136825 = DIRECTION ( 'NONE',  ( 0.000000000000000000, -7.026728003956686545E-15, 1.000000000000000000 ) ) ;
#136824 = CARTESIAN_POINT ( 'NONE',  ( 20.22483756094572271, 9.501904678871314402, -8.139539128714682548 ) ) ;
#136826 = DIRECTION ( 'NONE',  ( 0.000000000000000000, -0.7071067811865473507, -0.7071067811865477948 ) ) ;
#136827 = EDGE_LOOP ( 'NONE', ( #223018, #2998, #35599, #123155 ) ) ;
#136828 = CARTESIAN_POINT ( 'NONE',  ( 21.30000000000002558, 1.115650265596050101E-11, -29.45000000000000284 ) ) ;
#136829 = EDGE_LOOP ( 'NONE', ( #100800, #109625, #49721, #13024 ) ) ;
#136830 = EDGE_LOOP ( 'NONE', ( #177990, #77310 ) ) ;
#136831 = CARTESIAN_POINT ( 'NONE',  ( -21.07954640115405809, 69.67071230398674686, -69.58911519166422011 ) ) ;
#136832 = CARTESIAN_POINT ( 'NONE',  ( -21.44999999999999929, 7.150000000000000355, -12.25000000000000000 ) ) ;
#136833 = DIRECTION ( 'NONE',  ( 1.000000000000000000, -0.000000000000000000, -0.000000000000000000 ) ) ;
#136834 = CARTESIAN_POINT ( 'NONE',  ( 12.29592348164039350, 9.355806591641286474, -83.29110253154621546 ) ) ;
#136835 = EDGE_CURVE ( 'NONE', #225207, #40351, #49077, .T. ) ;
#136836 = AXIS2_PLACEMENT_3D ( 'NONE', #162710, #242220, #158872 ) ;
#136837 = AXIS2_PLACEMENT_3D ( 'NONE', #146189, #66669, #41984 ) ;
#136839 = CLOSED_SHELL ( 'NONE', ( #53945, #90226, #155636, #91001, #98896, #72341, #46396, #254262, #31002, #187655, #174951, #29863, #16471, #250424, #78235, #149163, #85740, #140295, #186484, #213405, #67155, #71970, #246545, #104936, #70461, #109432, #131724, #91741, #168694, #119035, #154394, #158653, #150601, #89461, #186353, #228284, #240482, #190804, #200349, #68602, #74133, #224330, #159942, #165791, #235402, #130375, #194749, #114320, #123938, #174020, #158114, #180073, #1115 ) ) ;
#136838 = CARTESIAN_POINT ( 'NONE',  ( 22.40000000000010161, 1.020945317880167817E-11, -155.7495671075409973 ) ) ;
#136840 = ORIENTED_EDGE ( 'NONE', *, *, #39479, .F. ) ;
#136841 = ORIENTED_EDGE ( 'NONE', *, *, #18429, .F. ) ;
#136842 = CARTESIAN_POINT ( 'NONE',  ( -21.14999999999999858, 11.75000000001115197, -40.28386566297815108 ) ) ;
#136844 = ADVANCED_FACE ( 'NONE', ( #231584 ), #9959, .F. ) ;
#136843 = CARTESIAN_POINT ( 'NONE',  ( 20.27550659511089037, 66.78395627750370522, -182.6731074845244223 ) ) ;
#136845 = ORIENTED_EDGE ( 'NONE', *, *, #144736, .F. ) ;
#136846 = DIRECTION ( 'NONE',  ( 1.000000000000000000, 0.000000000000000000, 0.000000000000000000 ) ) ;
#136847 = CARTESIAN_POINT ( 'NONE',  ( -18.59999999999999787, 74.14897176987101091, -91.36919421510182815 ) ) ;
#136848 = CARTESIAN_POINT ( 'NONE',  ( -16.97048361161167662, 9.950000000011137047, -187.8588843444303507 ) ) ;
#136849 = DIRECTION ( 'NONE',  ( 0.000000000000000000, 1.897661533703519897E-16, -1.000000000000000000 ) ) ;
#136850 = CARTESIAN_POINT ( 'NONE',  ( 21.05000000000000071, 5.850000000011156942, -157.3675027757221017 ) ) ;
#136851 = TOROIDAL_SURFACE ( 'NONE', #36943, 0.4000000000000012990, 0.1000000000000000056 ) ;
#136852 = EDGE_CURVE ( 'NONE', #163445, #198523, #68729, .T. ) ;
#136854 = CARTESIAN_POINT ( 'NONE',  ( 23.04999999999999716, 67.17743825834614313, -182.6731074845244223 ) ) ;
#136853 = DIRECTION ( 'NONE',  ( -0.000000000000000000, 1.000000000000000000, 6.982962677686266711E-15 ) ) ;
#136855 = CARTESIAN_POINT ( 'NONE',  ( -22.50000000000000000, 1.115600667400684642E-11, -33.50000000000000000 ) ) ;
#136856 = AXIS2_PLACEMENT_3D ( 'NONE', #23810, #163297, #165873 ) ;
#136857 = DIRECTION ( 'NONE',  ( 0.000000000000000000, -6.982962677686266711E-15, 1.000000000000000000 ) ) ;
#136859 = ADVANCED_FACE ( 'NONE', ( #90761 ), #127170, .F. ) ;
#136858 = DIRECTION ( 'NONE',  ( 1.000000000000000000, 0.000000000000000000, 0.000000000000000000 ) ) ;
#136861 = CARTESIAN_POINT ( 'NONE',  ( 20.94999999999999929, 65.27628289530437655, -95.35819391543677170 ) ) ;
#136860 = CIRCLE ( 'NONE', #41207, 0.1000000000000000888 ) ;
#136863 = EDGE_LOOP ( 'NONE', ( #234531, #238039, #200323, #170954 ) ) ;
#136862 = CARTESIAN_POINT ( 'NONE',  ( -17.73285935861159501, 10.85798180380402300, -56.75856180978417598 ) ) ;
#136864 = CIRCLE ( 'NONE', #74369, 0.4000000000000045186 ) ;
#136865 = ADVANCED_FACE ( 'NONE', ( #229018 ), #251114, .T. ) ;
#136866 = ADVANCED_FACE ( 'NONE', ( #32117 ), #77313, .F. ) ;
#136867 = DIRECTION ( 'NONE',  ( 0.000000000000000000, 0.000000000000000000, -1.000000000000000000 ) ) ;
#136868 = ORIENTED_EDGE ( 'NONE', *, *, #49005, .T. ) ;
#136869 = VECTOR ( 'NONE', #124005, 1000.000000000000000 ) ;
#136870 = FACE_OUTER_BOUND ( 'NONE', #104759, .T. ) ;
#136871 =( NAMED_UNIT ( * ) PLANE_ANGLE_UNIT ( ) SI_UNIT ( $, .RADIAN. ) );
#136872 = CIRCLE ( 'NONE', #170244, 14.20833333333333748 ) ;
#136873 = AXIS2_PLACEMENT_3D ( 'NONE', #36536, #157785, #74384 ) ;
#136874 = EDGE_LOOP ( 'NONE', ( #192541, #55608, #172379, #144321 ) ) ;
#136875 = CARTESIAN_POINT ( 'NONE',  ( 23.24999999999999289, 69.55000000001186322, -90.67310748452435121 ) ) ;
#136876 = AXIS2_PLACEMENT_3D ( 'NONE', #62002, #63264, #142784 ) ;
#136877 = CARTESIAN_POINT ( 'NONE',  ( -23.25000000000000000, 4.150000000011156764, -45.85000000000000142 ) ) ;
#136878 = DIRECTION ( 'NONE',  ( -3.469446951953612296E-14, -0.9908441862701596881, -0.1350103645451904977 ) ) ;
#136879 = EDGE_CURVE ( 'NONE', #209946, #6520, #147851, .T. ) ;
#136880 = DIRECTION ( 'NONE',  ( 0.000000000000000000, -0.9651348961777157509, 0.2617529984165031243 ) ) ;
#136881 = EDGE_CURVE ( 'NONE', #121164, #9105, #69956, .T. ) ;
#136882 = LINE ( 'NONE', #254241, #211903 ) ;
#136883 = DIRECTION ( 'NONE',  ( 1.000000000000000000, 0.000000000000000000, 0.000000000000000000 ) ) ;
#136884 = ORIENTED_EDGE ( 'NONE', *, *, #36383, .F. ) ;
#136885 = CYLINDRICAL_SURFACE ( 'NONE', #112361, 0.09999999999998898659 ) ;
#136887 = ORIENTED_EDGE ( 'NONE', *, *, #79507, .F. ) ;
#136886 = FACE_OUTER_BOUND ( 'NONE', #87846, .T. ) ;
#136888 = DIRECTION ( 'NONE',  ( 0.000000000000000000, 0.9126074666063385132, 0.4088369013364143156 ) ) ;
#136889 = EDGE_CURVE ( 'NONE', #128159, #38688, #180285, .T. ) ;
#136890 = DIRECTION ( 'NONE',  ( 0.000000000000000000, -1.000000000000000000, -7.272083257015735086E-15 ) ) ;
#136891 = CARTESIAN_POINT ( 'NONE',  ( -22.48660254037843131, 31.85034414784621148, -238.9397275603479898 ) ) ;
#136892 = VERTEX_POINT ( 'NONE', #139851 ) ;
#136893 = DIRECTION ( 'NONE',  ( 0.000000000000000000, 1.000000000000000000, 0.000000000000000000 ) ) ;
#136894 = AXIS2_PLACEMENT_3D ( 'NONE', #238299, #118376, #2243 ) ;
#136895 = APPLICATION_PROTOCOL_DEFINITION ( 'draft international standard', 'automotive_design', 1998, #154098 ) ;
#136896 = EDGE_CURVE ( 'NONE', #79382, #219396, #222841, .T. ) ;
#136897 = LINE ( 'NONE', #251711, #181722 ) ;
#136898 = CARTESIAN_POINT ( 'NONE',  ( -20.65000000000000568, 5.650000000011139001, -76.25000000000004263 ) ) ;
#136899 = ORIENTED_EDGE ( 'NONE', *, *, #118914, .T. ) ;
#136900 = DIRECTION ( 'NONE',  ( 1.000000000000000000, 0.000000000000000000, 0.000000000000000000 ) ) ;
#136901 = CARTESIAN_POINT ( 'NONE',  ( -20.00857864376270001, 61.41373750439892376, -221.5848334931070553 ) ) ;
#136902 = ADVANCED_FACE ( 'NONE', ( #242811 ), #181179, .T. ) ;
#136903 = DIRECTION ( 'NONE',  ( 1.000000000000000000, 7.304098846218134667E-16, 5.100424963727256530E-30 ) ) ;
#136904 = EDGE_LOOP ( 'NONE', ( #107526, #106603, #216284, #30366 ) ) ;
#136905 = ORIENTED_EDGE ( 'NONE', *, *, #227902, .T. ) ;
#136906 = ADVANCED_FACE ( 'NONE', ( #219389 ), #64616, .T. ) ;
#136907 = LINE ( 'NONE', #97750, #43258 ) ;
#136908 = CARTESIAN_POINT ( 'NONE',  ( 18.59999999999999076, 6.650000000011155876, -188.6499999999999488 ) ) ;
#136909 = DIRECTION ( 'NONE',  ( 0.000000000000000000, 0.000000000000000000, 1.000000000000000000 ) ) ;
#136910 = DIRECTION ( 'NONE',  ( 0.000000000000000000, -0.1298341882519953860, -0.9915357197604862671 ) ) ;
#136911 = LINE ( 'NONE', #57356, #40978 ) ;
#136913 = CARTESIAN_POINT ( 'NONE',  ( 21.30000000000002558, 7.128833340093095217, -233.7327013124392749 ) ) ;
#136912 = DIRECTION ( 'NONE',  ( -1.000000000000000000, -0.000000000000000000, -0.000000000000000000 ) ) ;
#136914 = EDGE_CURVE ( 'NONE', #50451, #122095, #56234, .T. ) ;
#136915 = AXIS2_PLACEMENT_3D ( 'NONE', #160375, #199494, #61245 ) ;
#136917 = CARTESIAN_POINT ( 'NONE',  ( 20.89878130938411616, 65.67252876774480796, -30.44570419949946327 ) ) ;
#136916 = AXIS2_PLACEMENT_3D ( 'NONE', #86705, #209244, #30639 ) ;
#136918 = PLANE ( 'NONE',  #156175 ) ;
#136919 = FACE_OUTER_BOUND ( 'NONE', #182206, .T. ) ;
#136920 = TOROIDAL_SURFACE ( 'NONE', #199487, 11.65000000000000036, 0.1000000000000000056 ) ;
#136921 = DIRECTION ( 'NONE',  ( 0.000000000000000000, 0.000000000000000000, -1.000000000000000000 ) ) ;
#136922 = VERTEX_POINT ( 'NONE', #40802 ) ;
#136923 = ORIENTED_EDGE ( 'NONE', *, *, #108141, .T. ) ;
#136924 = DIRECTION ( 'NONE',  ( -3.469446951953515108E-14, 1.000000000000000000, 0.000000000000000000 ) ) ;
#136925 = CARTESIAN_POINT ( 'NONE',  ( 21.07928932188134397, 75.90110485435729970, -75.85162414091763594 ) ) ;
#136927 = DIRECTION ( 'NONE',  ( -1.000000000000000000, 0.000000000000000000, 0.000000000000000000 ) ) ;
#136926 = DIRECTION ( 'NONE',  ( -0.000000000000000000, 1.000000000000000000, -0.000000000000000000 ) ) ;
#136928 = AXIS2_PLACEMENT_3D ( 'NONE', #193625, #150646, #52810 ) ;
#136929 = CYLINDRICAL_SURFACE ( 'NONE', #222634, 0.09999999999998898659 ) ;
#136930 = DIRECTION ( 'NONE',  ( -0.000000000000000000, 0.9770955615653315052, 0.2128009952263602844 ) ) ;
#136931 = EDGE_CURVE ( 'NONE', #250321, #250869, #64189, .T. ) ;
#136932 = CARTESIAN_POINT ( 'NONE',  ( 20.94999999999999929, 8.001317420522637391, -237.7387931148579980 ) ) ;
#136933 = EDGE_LOOP ( 'NONE', ( #214082, #149416, #94485, #47967, #25066 ) ) ;
#136934 = ORIENTED_EDGE ( 'NONE', *, *, #32141, .F. ) ;
#136935 = B_SPLINE_CURVE_WITH_KNOTS ( 'NONE', 3,
 ( #134208, #13021, #177231, #57226 ),
 .UNSPECIFIED., .F., .F.,
 ( 4, 4 ),
 ( 0.000000000000000000, 7.713889350929433657E-05 ),
 .UNSPECIFIED. ) ;
#136936 = CIRCLE ( 'NONE', #91142, 0.1000000000000043493 ) ;
#136937 = TOROIDAL_SURFACE ( 'NONE', #178673, 0.2000000000000000111, 0.1000000000000000056 ) ;
#136939 = AXIS2_PLACEMENT_3D ( 'NONE', #50672, #192787, #36291 ) ;
#136938 = CARTESIAN_POINT ( 'NONE',  ( -22.39999999999999858, -3.275978944802467652, -228.2735455795363748 ) ) ;
#136940 = ORIENTED_EDGE ( 'NONE', *, *, #53851, .F. ) ;
#136941 = DIRECTION ( 'NONE',  ( 0.000000000000000000, 1.734723475976757554E-14, 1.000000000000000000 ) ) ;
#136942 = CARTESIAN_POINT ( 'NONE',  ( 18.43630871534874416, 85.67980087481434737, -29.36247541654018889 ) ) ;
#136943 = ORIENTED_EDGE ( 'NONE', *, *, #26308, .T. ) ;
#136944 = DIRECTION ( 'NONE',  ( -0.000000000000000000, 6.982962677686266711E-15, -1.000000000000000000 ) ) ;
#136945 =( BOUNDED_CURVE ( )  B_SPLINE_CURVE ( 3, ( #137102, #142, #240062, #219193 ),
 .UNSPECIFIED., .F., .F. ) 
 B_SPLINE_CURVE_WITH_KNOTS ( ( 4, 4 ),
 ( 4.712388980384689674, 6.231880751915385375 ),
 .UNSPECIFIED. ) 
 CURVE ( )  GEOMETRIC_REPRESENTATION_ITEM ( )  RATIONAL_B_SPLINE_CURVE ( ( 1.000000000000000000, 0.8166740347213230500, 0.8166740347213230500, 1.000000000000000000 ) ) 
 REPRESENTATION_ITEM ( '' )  );
#136946 = ORIENTED_EDGE ( 'NONE', *, *, #8288, .F. ) ;
#136947 = DIRECTION ( 'NONE',  ( -1.000000000000000000, 0.000000000000000000, 0.000000000000000000 ) ) ;
#136948 = CARTESIAN_POINT ( 'NONE',  ( -20.54999999999999716, 6.757359537351773859, -220.2789794402637824 ) ) ;
#136949 = DIRECTION ( 'NONE',  ( -0.000000000000000000, -0.000000000000000000, -1.000000000000000000 ) ) ;
#136950 = CARTESIAN_POINT ( 'NONE',  ( 21.07928932188134397, 75.90110485435778287, -142.8516241409176075 ) ) ;
#136951 = CARTESIAN_POINT ( 'NONE',  ( -22.39999999999999858, 76.00000000001173817, -81.17267829206912211 ) ) ;
#136953 = CARTESIAN_POINT ( 'NONE',  ( 18.49999999999999289, 65.70729864261026876, -131.0657455973724836 ) ) ;
#136952 = CARTESIAN_POINT ( 'NONE',  ( 20.94999999999999929, 6.550000000011156231, -112.6500000000000341 ) ) ;
#136954 = DIRECTION ( 'NONE',  ( -1.000000000000000000, 0.000000000000000000, 0.000000000000000000 ) ) ;
#136955 = ORIENTED_EDGE ( 'NONE', *, *, #192409, .F. ) ;
#136957 = DIRECTION ( 'NONE',  ( 0.000000000000000000, 0.000000000000000000, -1.000000000000000000 ) ) ;
#136956 = CARTESIAN_POINT ( 'NONE',  ( -18.52328366898031931, 38.02497047517800155, -261.2215128630973027 ) ) ;
#136959 = ORIENTED_EDGE ( 'NONE', *, *, #23549, .T. ) ;
#136958 = AXIS2_PLACEMENT_3D ( 'NONE', #38963, #19390, #40262 ) ;
#136961 = VERTEX_POINT ( 'NONE', #223239 ) ;
#136960 = CARTESIAN_POINT ( 'NONE',  ( -23.15000000000000213, 2.600000000011156054, -46.72462192276210402 ) ) ;
#136962 = ORIENTED_EDGE ( 'NONE', *, *, #217459, .F. ) ;
#136963 = DIRECTION ( 'NONE',  ( 1.000000000000000000, 2.952720810173289112E-16, -0.000000000000000000 ) ) ;
#136964 = CARTESIAN_POINT ( 'NONE',  ( 5.899999999999996803, -11.75000000000000000, 14.00000000000000178 ) ) ;
#136965 = CARTESIAN_POINT ( 'NONE',  ( -18.59999999999999787, 11.75000000001115197, -54.85000000000000142 ) ) ;
#136966 = DIRECTION ( 'NONE',  ( 0.000000000000000000, -1.000000000000000000, 0.000000000000000000 ) ) ;
#136967 = ORIENTED_EDGE ( 'NONE', *, *, #53749, .T. ) ;
#136968 = DIRECTION ( 'NONE',  ( -1.000000000000000000, -0.000000000000000000, -0.000000000000000000 ) ) ;
#136969 = CARTESIAN_POINT ( 'NONE',  ( -18.35235881385853318, 40.40978641300705476, -235.2986935099420975 ) ) ;
#136970 = CIRCLE ( 'NONE', #128786, 0.1000000000000108025 ) ;
#136971 = PLANE ( 'NONE',  #39893 ) ;
#136972 = VERTEX_POINT ( 'NONE', #60320 ) ;
#136973 = CARTESIAN_POINT ( 'NONE',  ( -21.05000000000000071, 74.16465844978765176, -124.9679561919613207 ) ) ;
#136974 = ADVANCED_FACE ( 'NONE', ( #138553 ), #59010, .T. ) ;
#136975 = DIRECTION ( 'NONE',  ( 1.000000000000000000, 0.000000000000000000, 0.000000000000000000 ) ) ;
#136976 = TOROIDAL_SURFACE ( 'NONE', #24009, 7.800000000000000711, 0.1000000000000000056 ) ;
#136977 = VERTEX_POINT ( 'NONE', #104558 ) ;
#136978 = ORIENTED_EDGE ( 'NONE', *, *, #68579, .T. ) ;
#136979 = AXIS2_PLACEMENT_3D ( 'NONE', #116029, #255469, #213829 ) ;
#136980 = CARTESIAN_POINT ( 'NONE',  ( 20.85000000000000142, 71.99422445362657186, -246.4870034924427671 ) ) ;
#136981 = CIRCLE ( 'NONE', #107750, 0.1000000000000133560 ) ;
#136982 = VERTEX_POINT ( 'NONE', #120348 ) ;
#136983 = FACE_OUTER_BOUND ( 'NONE', #96602, .T. ) ;
#136985 = VERTEX_POINT ( 'NONE', #179037 ) ;
#136984 = CIRCLE ( 'NONE', #32986, 1.500000000000001332 ) ;
#136986 = DIRECTION ( 'NONE',  ( 0.000000000000000000, 0.000000000000000000, 1.000000000000000000 ) ) ;
#136987 = CARTESIAN_POINT ( 'NONE',  ( -22.39999999999999858, 7.790779598384560245, -100.5000000000000284 ) ) ;
#136988 = CARTESIAN_POINT ( 'NONE',  ( 21.05000000000390159, 60.86818597347610904, -225.3357246298605219 ) ) ;
#136989 = DIRECTION ( 'NONE',  ( 1.000000000000000000, 0.000000000000000000, 0.000000000000000000 ) ) ;
#136990 = CIRCLE ( 'NONE', #99540, 0.09999999999998898659 ) ;
#136991 = AXIS2_PLACEMENT_3D ( 'NONE', #23420, #19548, #200742 ) ;
#136992 = EDGE_CURVE ( 'NONE', #105589, #151810, #142163, .T. ) ;
#136993 = EDGE_CURVE ( 'NONE', #89321, #31422, #152138, .T. ) ;
#136994 = CARTESIAN_POINT ( 'NONE',  ( -23.15000000000000213, 76.00000000001126921, -203.5231074845248997 ) ) ;
#136995 = AXIS2_PLACEMENT_3D ( 'NONE', #222895, #44285, #203349 ) ;
#136996 = DIRECTION ( 'NONE',  ( 0.9880948137434723000, -0.1538461538461484146, -1.074301950413233906E-15 ) ) ;
#136997 = CYLINDRICAL_SURFACE ( 'NONE', #197394, 0.09999999999999939493 ) ;
#136998 = EDGE_LOOP ( 'NONE', ( #112684, #25483, #178616, #38355 ) ) ;
#137000 = FACE_OUTER_BOUND ( 'NONE', #256945, .T. ) ;
#136999 = CARTESIAN_POINT ( 'NONE',  ( 21.06089410995844702, 22.94958222544119764, -230.0402814468934594 ) ) ;
#137001 = ORIENTED_EDGE ( 'NONE', *, *, #49642, .F. ) ;
#137004 = VERTEX_POINT ( 'NONE', #220693 ) ;
#137003 = DIRECTION ( 'NONE',  ( 1.000000000000000000, 0.000000000000000000, 0.000000000000000000 ) ) ;
#137002 = FACE_OUTER_BOUND ( 'NONE', #168605, .T. ) ;
#137005 = CIRCLE ( 'NONE', #16226, 0.1000000000000013933 ) ;
#137006 = ORIENTED_EDGE ( 'NONE', *, *, #223574, .F. ) ;
#137007 = DIRECTION ( 'NONE',  ( 1.000000000000000000, 0.000000000000000000, 0.000000000000000000 ) ) ;
#137008 = CIRCLE ( 'NONE', #253689, 0.09999999999998898659 ) ;
#137009 = VECTOR ( 'NONE', #230808, 1000.000000000000000 ) ;
#137010 = CARTESIAN_POINT ( 'NONE',  ( 14.11444803880197441, 66.54256847116334939, -155.0231905466248179 ) ) ;
#137011 = STYLED_ITEM ( 'NONE', ( #44436 ), #191235 ) ;
#137012 = CARTESIAN_POINT ( 'NONE',  ( -21.05000000000000071, 12.82677665681128332, -205.1493534351658354 ) ) ;
#137013 = EDGE_CURVE ( 'NONE', #169470, #213112, #189547, .T. ) ;
#137014 = DIRECTION ( 'NONE',  ( 0.5735764363510460484, -0.8191520442889919096, 0.000000000000000000 ) ) ;
#137015 = EDGE_LOOP ( 'NONE', ( #235171, #142852, #95737, #256951 ) ) ;
#137016 = CARTESIAN_POINT ( 'NONE',  ( 20.95289811251229750, 67.10683199555401757, -195.0212979906058877 ) ) ;
#137017 = EDGE_CURVE ( 'NONE', #217227, #72782, #197890, .T. ) ;
#137018 = VECTOR ( 'NONE', #13628, 1000.000000000000000 ) ;
#137019 = LINE ( 'NONE', #217814, #194573 ) ;
#137020 = EDGE_CURVE ( 'NONE', #40869, #179371, #31541, .T. ) ;
#137022 = CARTESIAN_POINT ( 'NONE',  ( -18.40000000000000213, 11.47316190336195341, -24.20017075153427299 ) ) ;
#137021 = CARTESIAN_POINT ( 'NONE',  ( 22.39999999999999503, -1.657885652111590780, -193.3876638332971538 ) ) ;
#137024 = ORIENTED_EDGE ( 'NONE', *, *, #173080, .T. ) ;
#137023 = DIRECTION ( 'NONE',  ( -1.000000000000000000, 0.000000000000000000, 0.000000000000000000 ) ) ;
#137025 = EDGE_CURVE ( 'NONE', #197069, #12386, #64799, .T. ) ;
#137026 = PRODUCT_DEFINITION_SHAPE ( 'NONE', 'NONE',  #171249 ) ;
#137027 = VERTEX_POINT ( 'NONE', #2908 ) ;
#137028 = CIRCLE ( 'NONE', #78734, 12.97499999999998721 ) ;
#137029 = CARTESIAN_POINT ( 'NONE',  ( 20.95556889135987788, 12.00496303110825025, -206.2069893072027469 ) ) ;
#137031 = CIRCLE ( 'NONE', #28746, 0.1000000000000033223 ) ;
#137030 = FACE_OUTER_BOUND ( 'NONE', #138168, .T. ) ;
#137032 = ORIENTED_EDGE ( 'NONE', *, *, #206833, .F. ) ;
#137033 = CARTESIAN_POINT ( 'NONE',  ( -20.85000000000000142, 77.83585931145570669, -125.0186683157258329 ) ) ;
#137034 = EDGE_CURVE ( 'NONE', #182088, #51816, #177282, .T. ) ;
#137035 = ORIENTED_EDGE ( 'NONE', *, *, #189092, .T. ) ;
#137036 = CARTESIAN_POINT ( 'NONE',  ( -21.64999999999999858, 66.65000000001161595, -60.27310748452439526 ) ) ;
#137037 = DIRECTION ( 'NONE',  ( -1.000000000000000000, 3.469446951953635015E-14, 0.000000000000000000 ) ) ;
#137038 = DIRECTION ( 'NONE',  ( -0.000000000000000000, 0.000000000000000000, -1.000000000000000000 ) ) ;
#137039 = VERTEX_POINT ( 'NONE', #79864 ) ;
#137040 = CARTESIAN_POINT ( 'NONE',  ( 18.79999999999999716, -1.467286812112899463, 32.89999999999999858 ) ) ;
#137041 = VECTOR ( 'NONE', #164150, 1000.000000000000227 ) ;
#137042 = VECTOR ( 'NONE', #190256, 1000.000000000000000 ) ;
#137043 = EDGE_CURVE ( 'NONE', #79296, #222594, #151419, .T. ) ;
#137044 = CIRCLE ( 'NONE', #216137, 11.75000000000001066 ) ;
#137045 = CARTESIAN_POINT ( 'NONE',  ( -20.94999999999999929, -11.74999999998884448, -103.4000000000000341 ) ) ;
#137046 = VECTOR ( 'NONE', #107318, 1000.000000000000227 ) ;
#137047 = ORIENTED_EDGE ( 'NONE', *, *, #33590, .T. ) ;
#137048 = ORIENTED_EDGE ( 'NONE', *, *, #96921, .T. ) ;
#137049 = FACE_OUTER_BOUND ( 'NONE', #211630, .T. ) ;
#137050 =( BOUNDED_CURVE ( )  B_SPLINE_CURVE ( 3, ( #242439, #178666, #63823, #143347 ),
 .UNSPECIFIED., .F., .T. ) 
 B_SPLINE_CURVE_WITH_KNOTS ( ( 4, 4 ),
 ( 5.733388419619901200, 5.983100554402348337 ),
 .UNSPECIFIED. ) 
 CURVE ( )  GEOMETRIC_REPRESENTATION_ITEM ( )  RATIONAL_B_SPLINE_CURVE ( ( 1.000000000000000000, 0.9948104011409416580, 0.9948104011409416580, 1.000000000000000000 ) ) 
 REPRESENTATION_ITEM ( '' )  );
#137051 = ORIENTED_EDGE ( 'NONE', *, *, #233616, .T. ) ;
#137052 = ORIENTED_EDGE ( 'NONE', *, *, #15608, .T. ) ;
#137054 = ORIENTED_EDGE ( 'NONE', *, *, #101715, .F. ) ;
#137053 = CARTESIAN_POINT ( 'NONE',  ( 21.59780538579342135, 75.90102133041401089, -109.8701980144675616 ) ) ;
#137055 = ORIENTED_EDGE ( 'NONE', *, *, #159800, .F. ) ;
#137056 = FACE_OUTER_BOUND ( 'NONE', #130557, .T. ) ;
#137057 = VECTOR ( 'NONE', #39102, 1000.000000000000000 ) ;
#137060 = VERTEX_POINT ( 'NONE', #6775 ) ;
#137059 = ORIENTED_EDGE ( 'NONE', *, *, #131865, .T. ) ;
#137058 = LINE ( 'NONE', #195776, #139462 ) ;
#137061 = AXIS2_PLACEMENT_3D ( 'NONE', #235195, #76109, #33181 ) ;
#137062 = ORIENTED_EDGE ( 'NONE', *, *, #97449, .F. ) ;
#137063 = DIRECTION ( 'NONE',  ( 0.000000000000000000, 0.8814952561688430555, -0.4721928772777346239 ) ) ;
#137064 = DIRECTION ( 'NONE',  ( 0.000000000000000000, 0.2617529984165024026, 0.9651348961777158619 ) ) ;
#137065 = ADVANCED_FACE ( 'NONE', ( #164580 ), #224533, .F. ) ;
#137066 = CARTESIAN_POINT ( 'NONE',  ( -16.80891096016305397, 14.16276025102163771, -219.2723308067244830 ) ) ;
#137067 = ADVANCED_FACE ( 'NONE', ( #150160 ), #198092, .T. ) ;
#137068 = ORIENTED_EDGE ( 'NONE', *, *, #229216, .F. ) ;
#137069 = CARTESIAN_POINT ( 'NONE',  ( 20.94999999999999574, 6.350000000000004974, -9.843822089683131438 ) ) ;
#137071 = ORIENTED_EDGE ( 'NONE', *, *, #249540, .F. ) ;
#137070 = DIRECTION ( 'NONE',  ( 0.000000000000000000, 0.000000000000000000, -1.000000000000000000 ) ) ;
#137072 = DIRECTION ( 'NONE',  ( 0.000000000000000000, -1.000000000000000000, -6.982962677686266711E-15 ) ) ;
#137073 = ORIENTED_EDGE ( 'NONE', *, *, #79309, .T. ) ;
#137074 = ADVANCED_FACE ( 'NONE', ( #187990 ), #210128, .T. ) ;
#137075 = EDGE_CURVE ( 'NONE', #181396, #115352, #197886, .T. ) ;
#137076 = ORIENTED_EDGE ( 'NONE', *, *, #42962, .F. ) ;
#137077 = DIRECTION ( 'NONE',  ( 0.000000000000000000, -0.2965989261549410450, -0.9550021345545443019 ) ) ;
#137078 = CARTESIAN_POINT ( 'NONE',  ( -20.94999999999999929, 1.162701749949165642, -175.5999999999999659 ) ) ;
#137079 = EDGE_CURVE ( 'NONE', #225270, #144437, #148016, .T. ) ;
#137080 = ORIENTED_EDGE ( 'NONE', *, *, #175385, .T. ) ;
#137081 = ORIENTED_EDGE ( 'NONE', *, *, #73671, .T. ) ;
#137082 = CARTESIAN_POINT ( 'NONE',  ( -16.93302609847409457, 9.996682520814371031, -180.0863884953625131 ) ) ;
#137084 = ADVANCED_FACE ( 'NONE', ( #146277 ), #101120, .T. ) ;
#137083 = DIRECTION ( 'NONE',  ( 0.000000000000000000, 0.000000000000000000, -1.000000000000000000 ) ) ;
#137085 = EDGE_CURVE ( 'NONE', #239047, #69658, #69331, .T. ) ;
#137087 = EDGE_LOOP ( 'NONE', ( #234138, #208103, #140818, #94344, #68674, #116550, #127714, #29856, #64173, #56898 ) ) ;
#137086 = VERTEX_POINT ( 'NONE', #86283 ) ;
#137088 = VERTEX_POINT ( 'NONE', #26348 ) ;
#137089 = CARTESIAN_POINT ( 'NONE',  ( -18.59999999999999787, 64.35000000001208775, -129.5083017138703667 ) ) ;
#137090 = VERTEX_POINT ( 'NONE', #147572 ) ;
#137091 = ORIENTED_EDGE ( 'NONE', *, *, #235057, .T. ) ;
#137092 = EDGE_CURVE ( 'NONE', #245477, #103483, #131454, .T. ) ;
#137093 = DIRECTION ( 'NONE',  ( 0.000000000000000000, 0.000000000000000000, -1.000000000000000000 ) ) ;
#137094 = VERTEX_POINT ( 'NONE', #10636 ) ;
#137095 = DIRECTION ( 'NONE',  ( 1.000000000000000000, 0.000000000000000000, -0.000000000000000000 ) ) ;
#137097 = CARTESIAN_POINT ( 'NONE',  ( -22.48660254037843487, 64.35000000001268461, -203.5731074845244279 ) ) ;
#137096 = DIRECTION ( 'NONE',  ( 0.000000000000000000, 0.000000000000000000, -1.000000000000000000 ) ) ;
#137098 = ORIENTED_EDGE ( 'NONE', *, *, #119519, .F. ) ;
#137099 = EDGE_CURVE ( 'NONE', #49547, #117646, #109710, .T. ) ;
#137100 = VERTEX_POINT ( 'NONE', #227094 ) ;
#137101 = AXIS2_PLACEMENT_3D ( 'NONE', #230599, #251433, #11558 ) ;
#137102 = CARTESIAN_POINT ( 'NONE',  ( 20.12500000000000000, 9.750000000011153745, -175.6117712821142618 ) ) ;
#137103 = CIRCLE ( 'NONE', #182905, 0.09999999999998898659 ) ;
#137104 = EDGE_CURVE ( 'NONE', #169837, #207406, #207562, .T. ) ;
#137105 = VECTOR ( 'NONE', #118329, 1000.000000000000000 ) ;
#137107 = EDGE_CURVE ( 'NONE', #255276, #190492, #126450, .T. ) ;
#137106 = AXIS2_PLACEMENT_3D ( 'NONE', #21077, #13655, #160588 ) ;
#137108 = ORIENTED_EDGE ( 'NONE', *, *, #114504, .F. ) ;
#137109 = EDGE_CURVE ( 'NONE', #89054, #58722, #56423, .T. ) ;
#137110 = CIRCLE ( 'NONE', #166189, 0.5000000000000004441 ) ;
#137111 = DIRECTION ( 'NONE',  ( 0.000000000000000000, -1.000000000000000000, 0.000000000000000000 ) ) ;
#137112 = ORIENTED_EDGE ( 'NONE', *, *, #83486, .F. ) ;
#137113 = ORIENTED_EDGE ( 'NONE', *, *, #48774, .T. ) ;
#137114 = DIRECTION ( 'NONE',  ( 1.000000000000000000, 0.000000000000000000, 0.000000000000000000 ) ) ;
#137116 = ADVANCED_FACE ( 'NONE', ( #133145 ), #233543, .T. ) ;
#137115 = ORIENTED_EDGE ( 'NONE', *, *, #12869, .T. ) ;
#137117 = CYLINDRICAL_SURFACE ( 'NONE', #226220, 2.000000000000003553 ) ;
#137118 = CARTESIAN_POINT ( 'NONE',  ( -17.22767730082000526, 31.53411859322281785, -235.0653887475340014 ) ) ;
#137119 = ORIENTED_EDGE ( 'NONE', *, *, #136424, .T. ) ;
#137120 = EDGE_CURVE ( 'NONE', #56541, #252739, #194018, .T. ) ;
#137121 = CARTESIAN_POINT ( 'NONE',  ( 21.05000000000000071, 87.48912529308817909, -133.4231074845242233 ) ) ;
#137122 = CARTESIAN_POINT ( 'NONE',  ( 20.04142135623730070, 11.65000000001115943, -121.8500000000000369 ) ) ;
#137124 = DIRECTION ( 'NONE',  ( 0.000000000000000000, -6.982962677686266711E-15, 1.000000000000000000 ) ) ;
#137123 = FACE_OUTER_BOUND ( 'NONE', #135570, .T. ) ;
#137125 = CARTESIAN_POINT ( 'NONE',  ( -20.94999999999994600, 64.35000000001119247, -6.023107484524794941 ) ) ;
#137127 = CARTESIAN_POINT ( 'NONE',  ( 23.14999999999999503, 64.35000000001178933, -81.67310748452439384 ) ) ;
#137126 = AXIS2_PLACEMENT_3D ( 'NONE', #115910, #157639, #190656 ) ;
#137129 = CARTESIAN_POINT ( 'NONE',  ( 21.14999999999999858, 6.257814610487280937, -33.40220970869120265 ) ) ;
#137128 = AXIS2_PLACEMENT_3D ( 'NONE', #61175, #40373, #181143 ) ;
#137130 = CARTESIAN_POINT ( 'NONE',  ( -21.07928932188134041, 36.65892442174472876, -249.5511627012454596 ) ) ;
#137131 = VECTOR ( 'NONE', #27993, 1000.000000000000000 ) ;
#137132 = CARTESIAN_POINT ( 'NONE',  ( 22.47110162079220785, 75.97120258720953245, -148.1730434212086323 ) ) ;
#137133 = LINE ( 'NONE', #212822, #230573 ) ;
#137134 = ORIENTED_EDGE ( 'NONE', *, *, #55787, .F. ) ;
#137135 = VECTOR ( 'NONE', #1483, 1000.000000000000000 ) ;
#137137 = VERTEX_POINT ( 'NONE', #14508 ) ;
#137136 = ORIENTED_EDGE ( 'NONE', *, *, #182377, .F. ) ;
#137138 = ORIENTED_EDGE ( 'NONE', *, *, #199859, .F. ) ;
#137139 = VERTEX_POINT ( 'NONE', #230983 ) ;
#137140 = DIRECTION ( 'NONE',  ( 0.000000000000000000, 0.000000000000000000, -1.000000000000000000 ) ) ;
#137141 = CARTESIAN_POINT ( 'NONE',  ( 21.14999999999999858, 11.65000000001115943, -33.60000000000000142 ) ) ;
#137143 = CARTESIAN_POINT ( 'NONE',  ( -23.25000000000000000, 77.83585931145570669, -125.0186683157258329 ) ) ;
#137142 = DIRECTION ( 'NONE',  ( 0.000000000000000000, 0.2818822000686748708, -0.9594490217225944972 ) ) ;
#137144 = ORIENTED_EDGE ( 'NONE', *, *, #100577, .F. ) ;
#137145 = DIRECTION ( 'NONE',  ( 1.000000000000000000, 0.000000000000000000, -0.000000000000000000 ) ) ;
#137146 = CARTESIAN_POINT ( 'NONE',  ( -21.04999999999994387, 83.98667523412385094, -37.28476067066772970 ) ) ;
#137147 = DIRECTION ( 'NONE',  ( 0.000000000000000000, 0.000000000000000000, -1.000000000000000000 ) ) ;
#137148 = LINE ( 'NONE', #60165, #195625 ) ;
#137149 = ORIENTED_EDGE ( 'NONE', *, *, #121264, .F. ) ;
#137150 = DIRECTION ( 'NONE',  ( -3.440080580676165868E-14, -0.1298341882520124002, -0.9915357197604841577 ) ) ;
#137151 = VERTEX_POINT ( 'NONE', #213967 ) ;
#137152 = DIRECTION ( 'NONE',  ( -1.000000000000000000, 0.000000000000000000, 0.000000000000000000 ) ) ;
#137153 = CYLINDRICAL_SURFACE ( 'NONE', #140408, 0.1000000000000028644 ) ;
#137154 = LINE ( 'NONE', #156751, #181043 ) ;
#137155 = DIRECTION ( 'NONE',  ( -1.000000000000000000, -0.000000000000000000, -0.000000000000000000 ) ) ;
#137156 = DIRECTION ( 'NONE',  ( 0.000000000000000000, 0.5341055959866798375, -0.8454177738465836756 ) ) ;
#137157 = VERTEX_POINT ( 'NONE', #96557 ) ;
#137158 = DIRECTION ( 'NONE',  ( 0.000000000000000000, 0.000000000000000000, 1.000000000000000000 ) ) ;
#137159 = CARTESIAN_POINT ( 'NONE',  ( 18.59999999999999076, 77.14957036958807635, -162.2071950000224092 ) ) ;
#137160 = CARTESIAN_POINT ( 'NONE',  ( -16.81744102076749314, 9.950000000011142376, -146.6500000000000341 ) ) ;
#137161 = EDGE_CURVE ( 'NONE', #107947, #143687, #43959, .T. ) ;
#137163 = DIRECTION ( 'NONE',  ( 0.000000000000000000, -7.056502275159890043E-15, 1.000000000000000000 ) ) ;
#137162 = CARTESIAN_POINT ( 'NONE',  ( -16.80468759584937288, 66.05784632487790020, -123.8330886183227477 ) ) ;
#137164 = DIRECTION ( 'NONE',  ( 1.000000000000000000, 0.000000000000000000, 0.000000000000000000 ) ) ;
#137165 = CARTESIAN_POINT ( 'NONE',  ( 21.08479644141223019, 0.05855444257529528185, -27.15496134226810909 ) ) ;
#137167 = EDGE_CURVE ( 'NONE', #103428, #114980, #91455, .T. ) ;
#137166 = CARTESIAN_POINT ( 'NONE',  ( 18.59999999999999432, 85.48068669529136798, -163.0819923157664562 ) ) ;
#137168 = LINE ( 'NONE', #139718, #35906 ) ;
#137169 = ORIENTED_EDGE ( 'NONE', *, *, #111316, .F. ) ;
#137170 = ORIENTED_EDGE ( 'NONE', *, *, #254640, .T. ) ;
#137171 = EDGE_CURVE ( 'NONE', #147343, #231071, #243873, .T. ) ;
#137172 = CARTESIAN_POINT ( 'NONE',  ( 23.14999999999998437, 0.000000000000000000, 0.000000000000000000 ) ) ;
#137173 = EDGE_CURVE ( 'NONE', #215662, #212264, #218928, .T. ) ;
#137174 = ORIENTED_EDGE ( 'NONE', *, *, #143648, .F. ) ;
#137175 = CARTESIAN_POINT ( 'NONE',  ( 23.15000000000000213, 88.41227409416185878, -139.6231074845242688 ) ) ;
#137176 = AXIS2_PLACEMENT_3D ( 'NONE', #71776, #47031, #87449 ) ;
#137177 = TOROIDAL_SURFACE ( 'NONE', #158081, 7.800000000000000711, 0.1000000000000000056 ) ;
#137178 = CARTESIAN_POINT ( 'NONE',  ( -21.65000000000000213, 68.75000000001202238, -115.6731074845243512 ) ) ;
#137179 = ORIENTED_EDGE ( 'NONE', *, *, #150682, .T. ) ;
#137180 = CIRCLE ( 'NONE', #53796, 0.1000000000000066946 ) ;
#137181 = CARTESIAN_POINT ( 'NONE',  ( 19.75857864376268935, 64.35000000001197407, -111.7731074845243739 ) ) ;
#137183 = ADVANCED_FACE ( 'NONE', ( #53609 ), #19009, .T. ) ;
#137182 = VECTOR ( 'NONE', #77905, 1000.000000000000000 ) ;
#137184 = CIRCLE ( 'NONE', #95486, 0.09999999999999971412 ) ;
#137185 = DIRECTION ( 'NONE',  ( 1.000000000000000000, 0.000000000000000000, 0.000000000000000000 ) ) ;
#137186 = CARTESIAN_POINT ( 'NONE',  ( -20.65000000000000568, 70.35000000001201670, -115.6731074845243370 ) ) ;
#137187 = CYLINDRICAL_SURFACE ( 'NONE', #216200, 0.09999999999999982514 ) ;
#137189 = EDGE_LOOP ( 'NONE', ( #157117, #150316, #161495, #180770, #156801, #34481, #245995, #56473, #48392, #105605, #52666, #146314, #70928, #40526 ) ) ;
#137188 = CARTESIAN_POINT ( 'NONE',  ( -23.25000000000000000, -8.729782940176420425, -238.4538547387928986 ) ) ;
#137191 = DIRECTION ( 'NONE',  ( 0.000000000000000000, 0.9915357197604862671, -0.1298341882519953583 ) ) ;
#137190 = CARTESIAN_POINT ( 'NONE',  ( -20.90000000000000213, 1.901609089591594470, -11.59510167572422112 ) ) ;
#137192 = CIRCLE ( 'NONE', #149879, 0.09999999999999134581 ) ;
#137193 = DIRECTION ( 'NONE',  ( 0.000000000000000000, 0.2617529984165030132, 0.9651348961777158619 ) ) ;
#137194 = CARTESIAN_POINT ( 'NONE',  ( -0.8999999999999993561, -11.75000000000000000, 28.70000000000000284 ) ) ;
#137195 = CARTESIAN_POINT ( 'NONE',  ( 18.43709777086140278, 87.08727414655709254, -199.6327537731849873 ) ) ;
#137196 = CARTESIAN_POINT ( 'NONE',  ( -20.64999999999999858, 68.85000000001254250, -182.3731074845244109 ) ) ;
#137197 = EDGE_LOOP ( 'NONE', ( #193153, #33995, #182223 ) ) ;
#137198 = DIRECTION ( 'NONE',  ( 0.000000000000000000, 0.000000000000000000, 1.000000000000000000 ) ) ;
#137199 = CARTESIAN_POINT ( 'NONE',  ( -11.59999999999994458, 67.75000000001118394, -16.98168612828748181 ) ) ;
#137200 = EDGE_CURVE ( 'NONE', #206950, #374, #156598, .T. ) ;
#137201 = ORIENTED_EDGE ( 'NONE', *, *, #103532, .T. ) ;
#137202 = CARTESIAN_POINT ( 'NONE',  ( 23.14999999999999858, 54.46551753941606222, -236.3409998116131021 ) ) ;
#137203 = EDGE_CURVE ( 'NONE', #118409, #16439, #181362, .T. ) ;
#137205 = VERTEX_POINT ( 'NONE', #154042 ) ;
#137204 = CIRCLE ( 'NONE', #253715, 12.77499999999999503 ) ;
#137206 = CARTESIAN_POINT ( 'NONE',  ( -20.94999999999999929, 44.06843597547145208, -258.9974126733344519 ) ) ;
#137207 = CARTESIAN_POINT ( 'NONE',  ( -23.15000000000000213, 11.60000000001115517, -127.0717967697245143 ) ) ;
#137208 = CARTESIAN_POINT ( 'NONE',  ( -23.15000000000000213, 64.35000000001205933, -124.3731074845243825 ) ) ;
#137209 = ORIENTED_EDGE ( 'NONE', *, *, #58673, .F. ) ;
#137210 = ORIENTED_EDGE ( 'NONE', *, *, #81200, .F. ) ;
#137211 = ADVANCED_FACE ( 'NONE', ( #152738 ), #253074, .T. ) ;
#137212 = ADVANCED_FACE ( 'NONE', ( #250513 ), #211399, .F. ) ;
#137213 = AXIS2_PLACEMENT_3D ( 'NONE', #9038, #192823, #110705 ) ;
#137214 = DIRECTION ( 'NONE',  ( -0.1538461538461484146, -0.9880948137434723000, 0.000000000000000000 ) ) ;
#137215 = DIRECTION ( 'NONE',  ( 0.000000000000000000, -0.000000000000000000, -1.000000000000000000 ) ) ;
#137216 = CARTESIAN_POINT ( 'NONE',  ( -22.10000000000000142, -11.65000000000000036, 32.89999999999999858 ) ) ;
#137217 = CARTESIAN_POINT ( 'NONE',  ( -16.94878442675512886, 66.00827089702086425, -90.41132706016226450 ) ) ;
#137218 = VECTOR ( 'NONE', #94600, 1000.000000000000000 ) ;
#137220 = CARTESIAN_POINT ( 'NONE',  ( 20.94999999999999574, -1.736257131586239844, -45.06865232901750318 ) ) ;
#137219 = FACE_OUTER_BOUND ( 'NONE', #162736, .T. ) ;
#137221 = EDGE_CURVE ( 'NONE', #91231, #193742, #74496, .T. ) ;
#137222 = FACE_OUTER_BOUND ( 'NONE', #80944, .T. ) ;
#137223 = CARTESIAN_POINT ( 'NONE',  ( 21.09793522318408066, 65.27537548979908877, -90.78381661354731591 ) ) ;
#137224 = DIRECTION ( 'NONE',  ( 0.000000000000000000, -7.172728831056617961E-15, 1.000000000000000000 ) ) ;
#137225 = ORIENTED_EDGE ( 'NONE', *, *, #21415, .T. ) ;
#137226 = CARTESIAN_POINT ( 'NONE',  ( 20.04142135623731136, 34.50923130584770604, -235.0700073140421864 ) ) ;
#137227 = VECTOR ( 'NONE', #28827, 1000.000000000000000 ) ;
#137229 = ORIENTED_EDGE ( 'NONE', *, *, #51226, .T. ) ;
#137228 = DIRECTION ( 'NONE',  ( 1.000000000000000000, 0.000000000000000000, 0.000000000000000000 ) ) ;
#137230 = DIRECTION ( 'NONE',  ( 0.000000000000000000, -0.2617529984165031243, -0.9651348961777157509 ) ) ;
#137232 = DIRECTION ( 'NONE',  ( 0.000000000000000000, 0.4721928772777346239, 0.8814952561688430555 ) ) ;
#137231 = CARTESIAN_POINT ( 'NONE',  ( -20.94999999999999929, 79.38304387823771435, -235.9388060597213723 ) ) ;
#137233 = EDGE_LOOP ( 'NONE', ( #102128, #187798, #202478, #162432 ) ) ;
#137235 = DIRECTION ( 'NONE',  ( 1.000000000000000000, 0.000000000000000000, 0.000000000000000000 ) ) ;
#137234 = FACE_OUTER_BOUND ( 'NONE', #162970, .T. ) ;
#137236 = CARTESIAN_POINT ( 'NONE',  ( -20.94999999999999929, 86.32947205150912851, -209.3293116780858156 ) ) ;
#137237 = EDGE_CURVE ( 'NONE', #71501, #44121, #234811, .T. ) ;
#137238 = CARTESIAN_POINT ( 'NONE',  ( -21.05000000000000071, 74.63912941282028157, -161.9501095574334215 ) ) ;
#137239 = CARTESIAN_POINT ( 'NONE',  ( 23.50000000000005684, 64.25000000001119815, -43.82310748452479743 ) ) ;
#137240 = CARTESIAN_POINT ( 'NONE',  ( -21.65000000000000213, 68.29142135624991283, -191.2731074845244166 ) ) ;
#137241 = ORIENTED_EDGE ( 'NONE', *, *, #26272, .F. ) ;
#137242 = DIRECTION ( 'NONE',  ( 0.000000000000000000, 0.000000000000000000, -1.000000000000000000 ) ) ;
#137244 = ORIENTED_EDGE ( 'NONE', *, *, #38628, .T. ) ;
#137243 = AXIS2_PLACEMENT_3D ( 'NONE', #77879, #157470, #118316 ) ;
#137245 = EDGE_CURVE ( 'NONE', #56627, #13982, #57437, .T. ) ;
#137246 = CIRCLE ( 'NONE', #162209, 0.1000000000000012546 ) ;
#137247 = CARTESIAN_POINT ( 'NONE',  ( 20.94999999999999929, 87.39257802171711376, -39.09705706435617856 ) ) ;
#137248 = ORIENTED_EDGE ( 'NONE', *, *, #211260, .T. ) ;
#137249 = SPHERICAL_SURFACE ( 'NONE', #121946, 0.1000000000000000056 ) ;
#137250 = ORIENTED_EDGE ( 'NONE', *, *, #229472, .F. ) ;
#137251 = CARTESIAN_POINT ( 'NONE',  ( -18.40000000000000213, 11.75000000001113953, -46.15000000000000568 ) ) ;
#137252 = DIRECTION ( 'NONE',  ( -1.000000000000000000, 0.000000000000000000, -0.000000000000000000 ) ) ;
#137253 = EDGE_LOOP ( 'NONE', ( #86344, #245904, #191439, #164732 ) ) ;
#137254 = CYLINDRICAL_SURFACE ( 'NONE', #204458, 0.1000000000000028644 ) ;
#137255 = DIRECTION ( 'NONE',  ( 0.000000000000000000, 6.982962677686266711E-15, -1.000000000000000000 ) ) ;
#137256 = DIRECTION ( 'NONE',  ( 0.000000000000000000, 0.3427706569149635007, -0.9394191166662961834 ) ) ;
#137257 = DIRECTION ( 'NONE',  ( 4.239556034732056743E-17, 0.1298341882519953860, 0.9915357197604862671 ) ) ;
#137259 = VECTOR ( 'NONE', #63844, 1000.000000000000000 ) ;
#137258 = FACE_OUTER_BOUND ( 'NONE', #127027, .T. ) ;
#137260 = CARTESIAN_POINT ( 'NONE',  ( 22.49436431346199683, 12.57088205413893434, -223.4317334472834489 ) ) ;
#137261 = EDGE_LOOP ( 'NONE', ( #209216, #210425, #17076, #198004 ) ) ;
#137262 = CARTESIAN_POINT ( 'NONE',  ( -18.50000000000001066, 85.48068669529106955, -129.5819923157664562 ) ) ;
#137263 = ORIENTED_EDGE ( 'NONE', *, *, #135847, .F. ) ;
#137265 = ORIENTED_EDGE ( 'NONE', *, *, #67567, .T. ) ;
#137264 = DIRECTION ( 'NONE',  ( 0.000000000000000000, 0.000000000000000000, -1.000000000000000000 ) ) ;
#137266 = EDGE_LOOP ( 'NONE', ( #154300, #130103, #182948, #225225 ) ) ;
#137267 = DIRECTION ( 'NONE',  ( 1.000000000000000000, -0.000000000000000000, -0.000000000000000000 ) ) ;
#137268 = CARTESIAN_POINT ( 'NONE',  ( 13.22261339317535267, 66.56344716000816675, -188.3451520117641564 ) ) ;
#137269 = CARTESIAN_POINT ( 'NONE',  ( 21.05000000000000071, 76.00000000001173817, -73.62310748452429721 ) ) ;
#137270 = CARTESIAN_POINT ( 'NONE',  ( -20.54999999999999716, 2.500000000011154633, -120.7753780772379315 ) ) ;
#137271 = VERTEX_POINT ( 'NONE', #136987 ) ;
#137272 = DIRECTION ( 'NONE',  ( -0.000000000000000000, -0.000000000000000000, 1.000000000000000000 ) ) ;
#137273 = FACE_OUTER_BOUND ( 'NONE', #99890, .T. ) ;
#137274 = ORIENTED_EDGE ( 'NONE', *, *, #17648, .T. ) ;
#137276 = VERTEX_POINT ( 'NONE', #195712 ) ;
#137275 = FACE_OUTER_BOUND ( 'NONE', #124044, .T. ) ;
#137277 = DIRECTION ( 'NONE',  ( 1.000000000000000000, 0.000000000000000000, 0.000000000000000000 ) ) ;
#137278 = AXIS2_PLACEMENT_3D ( 'NONE', #60594, #18907, #198832 ) ;
#137279 = AXIS2_PLACEMENT_3D ( 'NONE', #216343, #78109, #218900 ) ;
#137280 = CIRCLE ( 'NONE', #233176, 0.1000000000000028644 ) ;
#137282 = AXIS2_PLACEMENT_3D ( 'NONE', #225333, #224059, #46705 ) ;
#137281 = CARTESIAN_POINT ( 'NONE',  ( -16.96982749440708460, 9.950000000011137047, -80.12477840881192037 ) ) ;
#137283 = AXIS2_PLACEMENT_3D ( 'NONE', #73103, #254246, #33984 ) ;
#137284 = DIRECTION ( 'NONE',  ( 0.7070776581709139474, 0.7071359030027652981, 2.946958787807621248E-14 ) ) ;
#137285 = VERTEX_POINT ( 'NONE', #216525 ) ;
#137286 = DIRECTION ( 'NONE',  ( -1.000000000000000000, 7.049440681616512959E-16, -1.911869773728117674E-16 ) ) ;
#137287 = EDGE_CURVE ( 'NONE', #66263, #83634, #6547, .T. ) ;
#137288 = CARTESIAN_POINT ( 'NONE',  ( 18.59999999999999787, -9.523946312306552642, -174.3820279953382624 ) ) ;
#137290 = CARTESIAN_POINT ( 'NONE',  ( -20.94999999999999929, 87.48912529308817909, -133.5231074845242176 ) ) ;
#137289 = APPLICATION_CONTEXT ( 'automotive_design' ) ;
#137291 = CARTESIAN_POINT ( 'NONE',  ( -18.59999999999999787, 11.75000000000000000, 31.39999999999999858 ) ) ;
#137292 = EDGE_CURVE ( 'NONE', #98112, #85621, #160713, .T. ) ;
#137294 = EDGE_CURVE ( 'NONE', #65351, #201212, #120031, .T. ) ;
#137293 = CIRCLE ( 'NONE', #91516, 4.050000000000005151 ) ;
#137295 = AXIS2_PLACEMENT_3D ( 'NONE', #182571, #123874, #140863 ) ;
#137296 = CIRCLE ( 'NONE', #158203, 0.1999999999999987899 ) ;
#137297 = ORIENTED_EDGE ( 'NONE', *, *, #5419, .F. ) ;
#137298 = DIRECTION ( 'NONE',  ( 0.000000000000000000, 0.000000000000000000, 1.000000000000000000 ) ) ;
#137299 = ORIENTED_EDGE ( 'NONE', *, *, #54991, .F. ) ;
#137300 = DIRECTION ( 'NONE',  ( -1.836970198721029934E-16, 1.000000000000000000, 0.000000000000000000 ) ) ;
#137301 = EDGE_CURVE ( 'NONE', #128354, #168945, #161716, .T. ) ;
#137302 = DIRECTION ( 'NONE',  ( 1.000000000000000000, -0.000000000000000000, -0.000000000000000000 ) ) ;
#137304 = ORIENTED_EDGE ( 'NONE', *, *, #63427, .F. ) ;
#137303 = DIRECTION ( 'NONE',  ( 1.000000000000000000, 0.000000000000000000, 0.000000000000000000 ) ) ;
#137305 = DIRECTION ( 'NONE',  ( -1.000000000000000000, 0.000000000000000000, 0.000000000000000000 ) ) ;
#137306 = DIRECTION ( 'NONE',  ( -1.000000000000000000, 0.000000000000000000, -0.000000000000000000 ) ) ;
#137307 = CARTESIAN_POINT ( 'NONE',  ( 18.49999999999999289, 65.79142135624984178, -182.1731074845244223 ) ) ;
#137308 = CARTESIAN_POINT ( 'NONE',  ( 20.85000000000000142, 76.00000000001190870, -103.0231074845243029 ) ) ;
#137309 = CARTESIAN_POINT ( 'NONE',  ( -23.15000000000000213, 87.48912529308779540, -72.52310748452423184 ) ) ;
#137310 = CARTESIAN_POINT ( 'NONE',  ( 18.79999999999999716, 13.48082180182240819, -2.152770446119436354 ) ) ;
#137311 = CARTESIAN_POINT ( 'NONE',  ( -18.50000000000000711, 85.42130820975080496, -129.2807442704737753 ) ) ;
#137313 = ORIENTED_EDGE ( 'NONE', *, *, #44147, .F. ) ;
#137312 = CARTESIAN_POINT ( 'NONE',  ( -22.24259225415828567, 68.50806212944671358, -136.6221733679771830 ) ) ;
#137314 = AXIS2_PLACEMENT_3D ( 'NONE', #128951, #248902, #33742 ) ;
#137315 = FACE_OUTER_BOUND ( 'NONE', #25364, .T. ) ;
#137316 = EDGE_CURVE ( 'NONE', #38307, #246198, #168905, .T. ) ;
#137317 = ADVANCED_FACE ( 'NONE', ( #23502 ), #102980, .F. ) ;
#137318 = SPHERICAL_SURFACE ( 'NONE', #169978, 0.1000000000000000056 ) ;
#137319 = DIRECTION ( 'NONE',  ( -1.000000000000000000, 0.000000000000000000, 0.000000000000000000 ) ) ;
#137320 = VERTEX_POINT ( 'NONE', #199563 ) ;
#137321 = DIRECTION ( 'NONE',  ( -1.000000000000000000, 0.000000000000000000, 0.000000000000000000 ) ) ;
#137323 = EDGE_CURVE ( 'NONE', #41537, #255042, #39, .T. ) ;
#137322 =( LENGTH_UNIT ( ) NAMED_UNIT ( * ) SI_UNIT ( .MILLI., .METRE. ) );
#137324 = VERTEX_POINT ( 'NONE', #80846 ) ;
#137325 = VECTOR ( 'NONE', #152681, 1000.000000000000114 ) ;
#137326 = CARTESIAN_POINT ( 'NONE',  ( -23.15000000000000213, 4.250000000011156409, -54.64999999999999858 ) ) ;
#137327 = AXIS2_PLACEMENT_3D ( 'NONE', #113228, #93669, #130212 ) ;
#137328 = CARTESIAN_POINT ( 'NONE',  ( -22.39999999999999858, 7.790779598373403836, 0.000000000000000000 ) ) ;
#137329 = ORIENTED_EDGE ( 'NONE', *, *, #178345, .T. ) ;
#137330 = AXIS2_PLACEMENT_3D ( 'NONE', #16302, #252301, #119239 ) ;
#137331 = ORIENTED_EDGE ( 'NONE', *, *, #14933, .T. ) ;
#137332 = LINE ( 'NONE', #237737, #38069 ) ;
#137334 = ORIENTED_EDGE ( 'NONE', *, *, #79324, .F. ) ;
#137333 = CARTESIAN_POINT ( 'NONE',  ( 21.05000000000000071, 6.344359042054848352, -133.9851443651061231 ) ) ;
#137335 = AXIS2_PLACEMENT_3D ( 'NONE', #177308, #93879, #74359 ) ;
#137336 = AXIS2_PLACEMENT_3D ( 'NONE', #154008, #215209, #195675 ) ;
#137337 = LINE ( 'NONE', #232631, #19252 ) ;
#137338 = VERTEX_POINT ( 'NONE', #122581 ) ;
#137339 = DIRECTION ( 'NONE',  ( 0.000000000000000000, 0.2558827019434435912, -0.9667078373770033872 ) ) ;
#137340 = ORIENTED_EDGE ( 'NONE', *, *, #104249, .T. ) ;
#137342 = ORIENTED_EDGE ( 'NONE', *, *, #108338, .T. ) ;
#137341 = ORIENTED_EDGE ( 'NONE', *, *, #129883, .F. ) ;
#137343 = CARTESIAN_POINT ( 'NONE',  ( 23.15000000000000213, 87.65000000001269598, -203.5231074845243029 ) ) ;
#137344 = VERTEX_POINT ( 'NONE', #220393 ) ;
#137345 = CARTESIAN_POINT ( 'NONE',  ( -23.15000000000000213, 1.115600667400684642E-11, -33.50000000000000000 ) ) ;
#137346 = ORIENTED_EDGE ( 'NONE', *, *, #44767, .T. ) ;
#137347 = AXIS2_PLACEMENT_3D ( 'NONE', #71126, #108935, #188478 ) ;
#137348 = CIRCLE ( 'NONE', #4260, 12.87499999999999822 ) ;
#137349 =( GEOMETRIC_REPRESENTATION_CONTEXT ( 3 ) GLOBAL_UNCERTAINTY_ASSIGNED_CONTEXT ( ( #92064 ) ) GLOBAL_UNIT_ASSIGNED_CONTEXT ( ( #241416, #223114, #242677 ) ) REPRESENTATION_CONTEXT ( 'NONE', 'WORKASPACE' ) );
#137350 = AXIS2_PLACEMENT_3D ( 'NONE', #114360, #16554, #158645 ) ;
#137351 = CIRCLE ( 'NONE', #124910, 11.64999999999999325 ) ;
#137352 = EDGE_CURVE ( 'NONE', #242494, #95316, #79564, .T. ) ;
#137353 = EDGE_CURVE ( 'NONE', #91403, #225601, #196953, .T. ) ;
#137354 = ORIENTED_EDGE ( 'NONE', *, *, #233220, .T. ) ;
#137356 = CIRCLE ( 'NONE', #16597, 0.09999999999999568956 ) ;
#137355 = CYLINDRICAL_SURFACE ( 'NONE', #124421, 0.09999999999999939493 ) ;
#137357 = FACE_OUTER_BOUND ( 'NONE', #191776, .T. ) ;
#137359 = ORIENTED_EDGE ( 'NONE', *, *, #175404, .F. ) ;
#137358 = CARTESIAN_POINT ( 'NONE',  ( 18.39999999999999503, 64.25000000001261924, -190.8731074845244393 ) ) ;
#137360 = CARTESIAN_POINT ( 'NONE',  ( 20.85000000000000142, 80.78317333349157536, -192.9003134612049166 ) ) ;
#137361 = EDGE_LOOP ( 'NONE', ( #146418, #15794, #185155, #252196 ) ) ;
#137362 = EDGE_CURVE ( 'NONE', #8048, #102057, #198241, .T. ) ;
#137364 = ADVANCED_FACE ( 'NONE', ( #101679 ), #58712, .F. ) ;
#137363 = CARTESIAN_POINT ( 'NONE',  ( 21.05000000000000071, 86.27712145182582049, -209.5223386573213702 ) ) ;
#137365 = CARTESIAN_POINT ( 'NONE',  ( -18.50000000000000355, -9.399999999988814636, -74.29725975966334772 ) ) ;
#137366 = DIRECTION ( 'NONE',  ( 0.000000000000000000, -0.6728971962616697722, 0.7397360091702875895 ) ) ;
#137367 = ORIENTED_EDGE ( 'NONE', *, *, #118417, .F. ) ;
#137368 = CARTESIAN_POINT ( 'NONE',  ( 20.94999999999999929, -1.349153571976048571, -41.28749733558988311 ) ) ;
#137369 = CARTESIAN_POINT ( 'NONE',  ( -21.14999999999994174, 74.83745509109094485, -44.02310748452479316 ) ) ;
#137370 = DIRECTION ( 'NONE',  ( -1.000000000000000000, -0.000000000000000000, 0.000000000000000000 ) ) ;
#137371 = ORIENTED_EDGE ( 'NONE', *, *, #178984, .F. ) ;
#137372 = CARTESIAN_POINT ( 'NONE',  ( -17.05016517656249420, 14.15417143192140514, -219.2328944449856465 ) ) ;
#137373 = ORIENTED_EDGE ( 'NONE', *, *, #151385, .F. ) ;
#137374 = ORIENTED_EDGE ( 'NONE', *, *, #127131, .F. ) ;
#137375 = EDGE_CURVE ( 'NONE', #204353, #46873, #156441, .T. ) ;
#137377 = ADVANCED_FACE ( 'NONE', ( #117436 ), #134318, .T. ) ;
#137376 = EDGE_CURVE ( 'NONE', #102466, #30919, #173205, .T. ) ;
#137378 = DIRECTION ( 'NONE',  ( -1.000000000000000000, -0.000000000000000000, -0.000000000000000000 ) ) ;
#137379 = ORIENTED_EDGE ( 'NONE', *, *, #158573, .T. ) ;
#137380 = EDGE_LOOP ( 'NONE', ( #162770, #24434, #199505, #84467 ) ) ;
#137381 = DIRECTION ( 'NONE',  ( 0.000000000000000000, 0.000000000000000000, 1.000000000000000000 ) ) ;
#137382 = DIRECTION ( 'NONE',  ( -1.000000000000000000, -0.000000000000000000, -0.000000000000000000 ) ) ;
#137383 = EDGE_LOOP ( 'NONE', ( #108144, #152219, #208632 ) ) ;
#137384 = EDGE_CURVE ( 'NONE', #193842, #91133, #150897, .T. ) ;
#137385 = ORIENTED_EDGE ( 'NONE', *, *, #63724, .T. ) ;
#137386 = DIRECTION ( 'NONE',  ( 0.000000000000000000, 0.000000000000000000, -1.000000000000000000 ) ) ;
#137387 = PLANE ( 'NONE',  #48004 ) ;
#137388 = VECTOR ( 'NONE', #187377, 1000.000000000000000 ) ;
#137389 = ORIENTED_EDGE ( 'NONE', *, *, #77773, .F. ) ;
#137390 = EDGE_CURVE ( 'NONE', #190614, #98928, #84206, .T. ) ;
#137391 = AXIS2_PLACEMENT_3D ( 'NONE', #173352, #252824, #112058 ) ;
#137392 = VERTEX_POINT ( 'NONE', #22199 ) ;
#137393 = ADVANCED_FACE ( 'NONE', ( #142121 ), #178727, .F. ) ;
#137394 = ADVANCED_FACE ( 'NONE', ( #247644 ), #142692, .F. ) ;
#137395 = EDGE_LOOP ( 'NONE', ( #35747, #130935, #130538, #228961 ) ) ;
#137396 = AXIS2_PLACEMENT_3D ( 'NONE', #116031, #27219, #63740 ) ;
#137397 = DIRECTION ( 'NONE',  ( 0.000000000000000000, -1.000000000000000000, -6.982962677686266711E-15 ) ) ;
#137398 = EDGE_CURVE ( 'NONE', #96608, #111061, #128992, .T. ) ;
#137399 = DIRECTION ( 'NONE',  ( 1.000000000000000000, 0.000000000000000000, 0.000000000000000000 ) ) ;
#137400 = CARTESIAN_POINT ( 'NONE',  ( -16.78270389226385717, 14.15456323211786582, -219.2470401007283272 ) ) ;
#137401 = CARTESIAN_POINT ( 'NONE',  ( -22.47071067811865319, 0.09909245471376171288, -159.7799252555019223 ) ) ;
#137402 = ADVANCED_FACE ( 'NONE', ( #207255 ), #127858, .T. ) ;
#137403 = DIRECTION ( 'NONE',  ( 0.000000000000000000, 0.000000000000000000, 1.000000000000000000 ) ) ;
#137404 = VECTOR ( 'NONE', #134960, 1000.000000000000000 ) ;
#137405 = DIRECTION ( 'NONE',  ( 0.000000000000000000, 0.000000000000000000, 1.000000000000000000 ) ) ;
#137406 = CARTESIAN_POINT ( 'NONE',  ( 20.90000000000000213, 6.742993295648862961, 9.658650260582458458 ) ) ;
#137407 = AXIS2_PLACEMENT_3D ( 'NONE', #168230, #247721, #7844 ) ;
#137408 = B_SPLINE_CURVE_WITH_KNOTS ( 'NONE', 3,
 ( #20171, #222183, #159682, #99666, #163524, #162261, #239207, #60556, #123123, #117976, #21467, #240493, #63121, #24035, #59236, #197502 ),
 .UNSPECIFIED., .F., .F.,
 ( 4, 3, 3, 3, 3, 4 ),
 ( 0.000000000000000000, 2.372700795694236445E-05, 5.739057815866932760E-05, 9.073899019179894126E-05, 0.0001243544287365692729, 0.0001585386695601185094 ),
 .UNSPECIFIED. ) ;
#137410 = DIRECTION ( 'NONE',  ( 0.000000000000000000, 0.2617529984164506107, 0.9651348961777299618 ) ) ;
#137409 = DIRECTION ( 'NONE',  ( 0.000000000000000000, -0.4930308989875170078, -0.8700118002898356018 ) ) ;
#137412 = ADVANCED_FACE ( 'NONE', ( #49448 ), #252721, .T. ) ;
#137411 = CARTESIAN_POINT ( 'NONE',  ( -16.87683809663752754, 23.48261004695467591, -231.3007506504703770 ) ) ;
#137413 = DIRECTION ( 'NONE',  ( 0.000000000000000000, -0.2818822000685679008, 0.9594490217226259166 ) ) ;
#137414 = DIRECTION ( 'NONE',  ( -0.7071067811865475727, -0.6909108974501237954, -0.1504730267678056066 ) ) ;
#137415 = CIRCLE ( 'NONE', #95899, 4.050000000000014921 ) ;
#137416 = ORIENTED_EDGE ( 'NONE', *, *, #119131, .T. ) ;
#137417 = VERTEX_POINT ( 'NONE', #203392 ) ;
#137418 = EDGE_CURVE ( 'NONE', #50827, #21187, #24780, .T. ) ;
#137419 = DIRECTION ( 'NONE',  ( -1.000000000000000000, -0.000000000000000000, -0.000000000000000000 ) ) ;
#137420 = DIRECTION ( 'NONE',  ( 0.000000000000000000, 0.000000000000000000, 1.000000000000000000 ) ) ;
#137421 = VERTEX_POINT ( 'NONE', #66444 ) ;
#137422 =( NAMED_UNIT ( * ) SI_UNIT ( $, .STERADIAN. ) SOLID_ANGLE_UNIT ( ) );
#137423 = DIRECTION ( 'NONE',  ( 0.000000000000000000, -0.4930308989875248349, -0.8700118002898312719 ) ) ;
#137424 = CIRCLE ( 'NONE', #91661, 2.100000000000004530 ) ;
#137425 = CARTESIAN_POINT ( 'NONE',  ( -16.85718274719460652, 66.02385768539041067, -157.4597611523423666 ) ) ;
#137426 = ORIENTED_EDGE ( 'NONE', *, *, #134535, .T. ) ;
#137427 = FACE_OUTER_BOUND ( 'NONE', #206591, .T. ) ;
#137428 = B_SPLINE_CURVE_WITH_KNOTS ( 'NONE', 3,
 ( #26276, #6696, #165803, #56074, #251733, #255527, #117363, #176078, #174814, #73131 ),
 .UNSPECIFIED., .F., .F.,
 ( 4, 3, 3, 4 ),
 ( 1.894194122894209342E-15, 3.877043167000115254E-05, 7.336897548477166022E-05, 7.659383120240389282E-05 ),
 .UNSPECIFIED. ) ;
#137429 = DIRECTION ( 'NONE',  ( -0.000000000000000000, -0.000000000000000000, 1.000000000000000000 ) ) ;
#137430 = DIRECTION ( 'NONE',  ( 1.000000000000000000, -7.304098846218135653E-16, -2.111765289898286048E-31 ) ) ;
#137431 = DIRECTION ( 'NONE',  ( -0.000000000000000000, -1.000000000000000000, 0.000000000000000000 ) ) ;
#137433 = EDGE_LOOP ( 'NONE', ( #257794, #9437, #9280, #97790 ) ) ;
#137432 = CARTESIAN_POINT ( 'NONE',  ( -18.59999999999999787, 68.87972903831482085, -166.3635444426850825 ) ) ;
#137435 = ORIENTED_EDGE ( 'NONE', *, *, #29543, .F. ) ;
#137434 = FACE_OUTER_BOUND ( 'NONE', #44996, .T. ) ;
#137436 = DIRECTION ( 'NONE',  ( 1.000000000000000000, 0.000000000000000000, 0.000000000000000000 ) ) ;
#137437 = CARTESIAN_POINT ( 'NONE',  ( 21.05933563467872460, 10.72452471208132074, -12.19364774895595538 ) ) ;
#137438 = DIRECTION ( 'NONE',  ( 0.000000000000000000, 0.000000000000000000, -1.000000000000000000 ) ) ;
#137439 = CARTESIAN_POINT ( 'NONE',  ( 18.49999999999999289, 6.450000000000001066, 11.75000000000000000 ) ) ;
#137440 = VECTOR ( 'NONE', #50034, 1000.000000000000000 ) ;
#137441 = ADVANCED_FACE ( 'NONE', ( #87267 ), #217523, .F. ) ;
#137444 = DIRECTION ( 'NONE',  ( -3.265361837132813093E-16, -1.000000000000000000, -6.938893903907222067E-15 ) ) ;
#137443 = VECTOR ( 'NONE', #114028, 1000.000000000000000 ) ;
#137442 = CARTESIAN_POINT ( 'NONE',  ( 20.94999999999999574, 87.48912529308798014, -99.92310748452423752 ) ) ;
#137445 = CARTESIAN_POINT ( 'NONE',  ( -22.50000000000000000, 64.35000000001238618, -170.0231074845244166 ) ) ;
#137446 = DIRECTION ( 'NONE',  ( 0.000000000000000000, 0.000000000000000000, 1.000000000000000000 ) ) ;
#137447 = CIRCLE ( 'NONE', #245802, 12.97499999999999964 ) ;
#137448 = AXIS2_PLACEMENT_3D ( 'NONE', #81648, #240772, #62133 ) ;
#137450 = B_SPLINE_CURVE_WITH_KNOTS ( 'NONE', 3,
 ( #36783, #116296, #176279, #82249, #203525, #100528, #178862, #143535 ),
 .UNSPECIFIED., .F., .F.,
 ( 4, 2, 2, 4 ),
 ( 0.000000000000000000, 0.0001881495939909106339, 0.0002822243909863764405, 0.0003762991879818423013 ),
 .UNSPECIFIED. ) ;
#137449 = DIRECTION ( 'NONE',  ( -0.000000000000000000, 0.8700118002898356018, -0.4930308989875170078 ) ) ;
#137451 = CARTESIAN_POINT ( 'NONE',  ( 22.01447462590973458, 0.09903700007069084210, -160.2361997987700875 ) ) ;
#137452 = EDGE_CURVE ( 'NONE', #22920, #206325, #196869, .T. ) ;
#137453 = CARTESIAN_POINT ( 'NONE',  ( -18.50000000000000000, 9.250000000011157297, -88.35000000000003695 ) ) ;
#137454 = ORIENTED_EDGE ( 'NONE', *, *, #166842, .T. ) ;
#137455 = DIRECTION ( 'NONE',  ( 0.000000000000000000, -0.5000000000000209832, 0.8660254037844264952 ) ) ;
#137456 = VECTOR ( 'NONE', #164166, 1000.000000000000000 ) ;
#137457 = ORIENTED_EDGE ( 'NONE', *, *, #223352, .T. ) ;
#137458 = EDGE_LOOP ( 'NONE', ( #216262, #85626, #59336, #236726 ) ) ;
#137459 = EDGE_CURVE ( 'NONE', #29064, #231902, #45598, .T. ) ;
#137460 = CARTESIAN_POINT ( 'NONE',  ( -18.40000000000000213, 64.52683809664902981, -48.57310748452440663 ) ) ;
#137461 = EDGE_CURVE ( 'NONE', #3992, #152770, #200981, .T. ) ;
#137462 = DIRECTION ( 'NONE',  ( 0.000000000000000000, -1.000000000000000000, -6.982962677686265922E-15 ) ) ;
#137463 = ORIENTED_EDGE ( 'NONE', *, *, #133327, .F. ) ;
#137464 = AXIS2_PLACEMENT_3D ( 'NONE', #108963, #231504, #32033 ) ;
#137465 = ORIENTED_EDGE ( 'NONE', *, *, #48807, .F. ) ;
#137466 = AXIS2_PLACEMENT_3D ( 'NONE', #98587, #231743, #133902 ) ;
#137467 = VERTEX_POINT ( 'NONE', #168156 ) ;
#137468 = ORIENTED_EDGE ( 'NONE', *, *, #178797, .F. ) ;
#137469 = DIRECTION ( 'NONE',  ( 0.000000000000000000, 0.000000000000000000, -1.000000000000000000 ) ) ;
#137470 = CARTESIAN_POINT ( 'NONE',  ( -22.50000000000000000, 1.115600667400684642E-11, -122.3504291924552234 ) ) ;
#137471 = CYLINDRICAL_SURFACE ( 'NONE', #155227, 11.80000000000000426 ) ;
#137472 = CARTESIAN_POINT ( 'NONE',  ( -22.39999999999999503, 7.790779598384560245, -100.4000000000000341 ) ) ;
#137473 = CARTESIAN_POINT ( 'NONE',  ( 15.15590539855246455, 9.410682294267953552, -15.43114344194827581 ) ) ;
#137474 = CARTESIAN_POINT ( 'NONE',  ( -18.50000000000000000, 11.75000000001115197, -21.75000000000000355 ) ) ;
#137475 = CYLINDRICAL_SURFACE ( 'NONE', #78641, 7.900000000000010125 ) ;
#137477 = ORIENTED_EDGE ( 'NONE', *, *, #98510, .T. ) ;
#137476 = DIRECTION ( 'NONE',  ( -3.469446951953612296E-14, -0.9908441862701596881, -0.1350103645451904977 ) ) ;
#137479 = SPHERICAL_SURFACE ( 'NONE', #16869, 0.1000000000000000056 ) ;
#137478 = DIRECTION ( 'NONE',  ( 0.000000000000000000, 0.000000000000000000, 1.000000000000000000 ) ) ;
#137480 = DIRECTION ( 'NONE',  ( 0.000000000000000000, 0.2262561206234166566, 0.9740678456249555195 ) ) ;
#137481 = ORIENTED_EDGE ( 'NONE', *, *, #209252, .F. ) ;
#137482 = CARTESIAN_POINT ( 'NONE',  ( -18.42554971533677133, 8.849916218358112374, -245.4285586339724716 ) ) ;
#137483 = CARTESIAN_POINT ( 'NONE',  ( -18.50000000000000000, 9.350000000000001421, -12.34999999999999964 ) ) ;
#137484 = ORIENTED_EDGE ( 'NONE', *, *, #42333, .T. ) ;
#137486 = DIRECTION ( 'NONE',  ( 0.000000000000000000, 6.982962677686266711E-15, -1.000000000000000000 ) ) ;
#137485 = LINE ( 'NONE', #159647, #20479 ) ;
#137487 = VECTOR ( 'NONE', #253696, 1000.000000000000000 ) ;
#137488 = CYLINDRICAL_SURFACE ( 'NONE', #81809, 0.5000000000000004441 ) ;
#137489 = EDGE_CURVE ( 'NONE', #238715, #150205, #6459, .T. ) ;
#137490 = DIRECTION ( 'NONE',  ( -1.000000000000000000, 0.000000000000000000, -0.000000000000000000 ) ) ;
#137491 = EDGE_LOOP ( 'NONE', ( #232951, #114361, #175, #220916 ) ) ;
#137492 = ORIENTED_EDGE ( 'NONE', *, *, #85711, .F. ) ;
#137493 = CARTESIAN_POINT ( 'NONE',  ( -16.87683809663752399, 23.65833333334447985, -150.7500000000000284 ) ) ;
#137495 = CARTESIAN_POINT ( 'NONE',  ( 23.25000000000000000, -8.596261682242985813, -24.04987248284971812 ) ) ;
#137494 = VECTOR ( 'NONE', #81967, 1000.000000000000114 ) ;
#137496 = CARTESIAN_POINT ( 'NONE',  ( -21.14999999999999858, 76.00000000001237765, -170.0231074845243597 ) ) ;
#137497 = SPHERICAL_SURFACE ( 'NONE', #180305, 0.1000000000000000056 ) ;
#137498 = ORIENTED_EDGE ( 'NONE', *, *, #116228, .F. ) ;
#137499 = EDGE_CURVE ( 'NONE', #228568, #208658, #59272, .T. ) ;
#137500 = CARTESIAN_POINT ( 'NONE',  ( -21.55000000000000071, 68.65000000001199965, -115.3731074845243540 ) ) ;
#137501 = ADVANCED_FACE ( 'NONE', ( #14196, #11619, #50695 ), #112001, .F. ) ;
#137502 = CARTESIAN_POINT ( 'NONE',  ( -17.29838795458689660, 10.37154985796053097, -122.6047412826064829 ) ) ;
#137503 = DIRECTION ( 'NONE',  ( 1.000000000000000000, 0.000000000000000000, 0.000000000000000000 ) ) ;
#137504 = AXIS2_PLACEMENT_3D ( 'NONE', #85912, #147202, #226729 ) ;
#137505 = DIRECTION ( 'NONE',  ( -1.000000000000000000, 0.000000000000000000, 0.000000000000000000 ) ) ;
#137507 = LINE ( 'NONE', #217042, #163507 ) ;
#137506 = AXIS2_PLACEMENT_3D ( 'NONE', #255567, #57401, #239923 ) ;
#137508 = EDGE_CURVE ( 'NONE', #177551, #252063, #46836, .T. ) ;
#137510 = EDGE_LOOP ( 'NONE', ( #86785, #98064, #104763, #45096 ) ) ;
#137509 = DIRECTION ( 'NONE',  ( 0.000000000000000000, 0.000000000000000000, -1.000000000000000000 ) ) ;
#137511 = DIRECTION ( 'NONE',  ( 0.000000000000000000, 0.000000000000000000, -1.000000000000000000 ) ) ;
#137512 = CARTESIAN_POINT ( 'NONE',  ( 21.05000000000000071, 8.776282895303632259, -142.4880007215843705 ) ) ;
#137513 = CARTESIAN_POINT ( 'NONE',  ( -18.59999999999999787, 77.83534155023627932, -91.46795619196132066 ) ) ;
#137514 = CIRCLE ( 'NONE', #245694, 12.77500000000000924 ) ;
#137515 = CARTESIAN_POINT ( 'NONE',  ( -23.25000000000000000, 11.75000000000000000, -33.50000000000000000 ) ) ;
#137516 = CARTESIAN_POINT ( 'NONE',  ( -21.05000000000000071, 0.000000000000000000, -29.40000000000000213 ) ) ;
#137517 = EDGE_CURVE ( 'NONE', #142182, #153937, #100961, .T. ) ;
#137519 = ORIENTED_EDGE ( 'NONE', *, *, #255596, .T. ) ;
#137518 = DIRECTION ( 'NONE',  ( 0.000000000000000000, -0.8814952561688431665, 0.4721928772777346794 ) ) ;
#137520 = DIRECTION ( 'NONE',  ( 0.000000000000000000, 0.000000000000000000, -1.000000000000000000 ) ) ;
#137521 = AXIS2_PLACEMENT_3D ( 'NONE', #118601, #139405, #81984 ) ;
#137522 = EDGE_CURVE ( 'NONE', #51183, #136580, #105071, .T. ) ;
#137523 = CARTESIAN_POINT ( 'NONE',  ( 18.49999999999999289, 64.35000000001147669, -44.67310748452440095 ) ) ;
#137524 = CARTESIAN_POINT ( 'NONE',  ( 21.05000000000000071, 85.40000000001252545, -179.9170766071767389 ) ) ;
#137525 = CIRCLE ( 'NONE', #233432, 0.09999999999999939493 ) ;
#137526 = ORIENTED_EDGE ( 'NONE', *, *, #139117, .T. ) ;
#137527 = DIRECTION ( 'NONE',  ( 0.000000000000000000, 0.000000000000000000, -1.000000000000000000 ) ) ;
#137528 = CARTESIAN_POINT ( 'NONE',  ( 23.14999999999998437, 76.00000000001195133, -103.0231074845243171 ) ) ;
#137529 = DIRECTION ( 'NONE',  ( 0.000000000000000000, 0.000000000000000000, -1.000000000000000000 ) ) ;
#137530 = DIRECTION ( 'NONE',  ( -0.000000000000000000, -0.000000000000000000, -1.000000000000000000 ) ) ;
#137531 = ADVANCED_FACE ( 'NONE', ( #53299 ), #174585, .T. ) ;
#137532 = CARTESIAN_POINT ( 'NONE',  ( 23.14999999999999503, 69.55000000001206217, -124.1731074845243370 ) ) ;
#137534 = CARTESIAN_POINT ( 'NONE',  ( 16.87683809663750267, 66.05000000001187743, -90.37310748452438247 ) ) ;
#137533 = AXIS2_PLACEMENT_3D ( 'NONE', #137474, #17530, #99619 ) ;
#137535 = AXIS2_PLACEMENT_3D ( 'NONE', #184130, #144994, #82439 ) ;
#137537 = ORIENTED_EDGE ( 'NONE', *, *, #88689, .T. ) ;
#137536 = AXIS2_PLACEMENT_3D ( 'NONE', #100276, #179859, #27220 ) ;
#137538 = VERTEX_POINT ( 'NONE', #31211 ) ;
#137539 = VECTOR ( 'NONE', #233980, 1000.000000000000114 ) ;
#137540 = AXIS2_PLACEMENT_3D ( 'NONE', #136850, #15661, #178585 ) ;
#137541 = CARTESIAN_POINT ( 'NONE',  ( -18.59999999999999787, -10.84999999999999076, 33.00000000000000000 ) ) ;
#137542 = DIRECTION ( 'NONE',  ( 1.000000000000000000, 0.000000000000000000, -0.000000000000000000 ) ) ;
#137543 = EDGE_CURVE ( 'NONE', #113056, #78387, #254047, .T. ) ;
#137544 = CARTESIAN_POINT ( 'NONE',  ( -18.50000000000000000, 11.65000000001115232, -155.7499999999999716 ) ) ;
#137545 = CARTESIAN_POINT ( 'NONE',  ( 23.24999999999999289, 6.650000000011155876, -88.15000000000004832 ) ) ;
#137546 = ORIENTED_EDGE ( 'NONE', *, *, #127757, .T. ) ;
#137547 = CYLINDRICAL_SURFACE ( 'NONE', #142549, 0.1000000000000028644 ) ;
#137548 = DIRECTION ( 'NONE',  ( 0.000000000000000000, -6.982962677686266711E-15, 1.000000000000000000 ) ) ;
#137549 = DIRECTION ( 'NONE',  ( -1.000000000000000000, 0.000000000000000000, 0.000000000000000000 ) ) ;
#137550 = DIRECTION ( 'NONE',  ( 0.000000000000000000, 0.08413937888704771384, -0.9964539953858891908 ) ) ;
#137551 = ORIENTED_EDGE ( 'NONE', *, *, #230667, .T. ) ;
#137552 = CARTESIAN_POINT ( 'NONE',  ( -23.15000000000000213, 76.00000000001230660, -157.1481074845243882 ) ) ;
#137553 = ORIENTED_EDGE ( 'NONE', *, *, #139127, .T. ) ;
#137554 = VERTEX_POINT ( 'NONE', #110702 ) ;
#137555 = DIRECTION ( 'NONE',  ( 0.000000000000000000, 1.000000000000000000, 0.000000000000000000 ) ) ;
#137556 = CARTESIAN_POINT ( 'NONE',  ( -21.05000000000000071, 6.413662734880552385, -100.5855928633623790 ) ) ;
#137557 = CARTESIAN_POINT ( 'NONE',  ( 21.14999999999999858, 11.65000000001115943, -112.6500000000000341 ) ) ;
#137558 = EDGE_LOOP ( 'NONE', ( #8839, #193483, #158915, #240355 ) ) ;
#137559 = DIRECTION ( 'NONE',  ( 0.000000000000000000, -0.000000000000000000, -1.000000000000000000 ) ) ;
#137560 = DIRECTION ( 'NONE',  ( 0.000000000000000000, 0.000000000000000000, 1.000000000000000000 ) ) ;
#137561 = FACE_BOUND ( 'NONE', #83724, .T. ) ;
#137562 = VERTEX_POINT ( 'NONE', #175828 ) ;
#137563 = CARTESIAN_POINT ( 'NONE',  ( -18.59999999999999787, 9.350000000000001421, -12.34999999999999964 ) ) ;
#137565 = ORIENTED_EDGE ( 'NONE', *, *, #138206, .T. ) ;
#137564 = CARTESIAN_POINT ( 'NONE',  ( -23.15000000000000213, 64.25000000001206502, -124.3731074845243825 ) ) ;
#137566 = VECTOR ( 'NONE', #110443, 1000.000000000000227 ) ;
#137567 = DIRECTION ( 'NONE',  ( -1.000000000000000000, -0.000000000000000000, 0.000000000000000000 ) ) ;
#137568 = CARTESIAN_POINT ( 'NONE',  ( 21.05000000000000071, -9.499999999988848032, -177.3939691226524076 ) ) ;
#137569 = CIRCLE ( 'NONE', #37659, 0.1000000000000000472 ) ;
#137570 = EDGE_CURVE ( 'NONE', #220040, #26378, #121880, .T. ) ;
#137571 = ORIENTED_EDGE ( 'NONE', *, *, #97017, .F. ) ;
#137572 = DIRECTION ( 'NONE',  ( 0.000000000000000000, 0.2128009952263604232, -0.9770955615653316162 ) ) ;
#137573 = DIRECTION ( 'NONE',  ( 0.000000000000000000, 0.1455152366551700771, 0.9893560106964479628 ) ) ;
#137574 = CARTESIAN_POINT ( 'NONE',  ( 20.94999999999999929, 69.35000000001156195, -57.37310748452436826 ) ) ;
#137575 = ORIENTED_EDGE ( 'NONE', *, *, #244142, .F. ) ;
#137576 = DIRECTION ( 'NONE',  ( 0.000000000000000000, 0.000000000000000000, -1.000000000000000000 ) ) ;
#137577 = EDGE_CURVE ( 'NONE', #224490, #72626, #34412, .T. ) ;
#137578 = CARTESIAN_POINT ( 'NONE',  ( 12.26145404764308644, 48.33210975535352816, -234.0748017065895397 ) ) ;
#137579 = DIRECTION ( 'NONE',  ( -0.000000000000000000, 0.000000000000000000, 1.000000000000000000 ) ) ;
#137580 = AXIS2_PLACEMENT_3D ( 'NONE', #181685, #195173, #215968 ) ;
#137581 = ADVANCED_FACE ( 'NONE', ( #255287 ), #172006, .F. ) ;
#137582 = VERTEX_POINT ( 'NONE', #131547 ) ;
#137583 = EDGE_CURVE ( 'NONE', #145162, #110428, #155222, .T. ) ;
#137584 = ORIENTED_EDGE ( 'NONE', *, *, #95466, .F. ) ;
#137585 = AXIS2_PLACEMENT_3D ( 'NONE', #157739, #133006, #112167 ) ;
#137586 = AXIS2_PLACEMENT_3D ( 'NONE', #61501, #228, #141042 ) ;
#137587 = CIRCLE ( 'NONE', #121083, 0.09999999999999864553 ) ;
#137588 = ORIENTED_EDGE ( 'NONE', *, *, #242838, .T. ) ;
#137589 = CARTESIAN_POINT ( 'NONE',  ( -16.86379686415369150, 9.975217759264314310, -87.93338988909033560 ) ) ;
#137590 = EDGE_CURVE ( 'NONE', #178773, #16075, #234272, .T. ) ;
#137591 = DIRECTION ( 'NONE',  ( -1.000000000000000000, 0.000000000000000000, 0.000000000000000000 ) ) ;
#137592 = ORIENTED_EDGE ( 'NONE', *, *, #232295, .T. ) ;
#137593 = DIRECTION ( 'NONE',  ( -0.000000000000000000, 0.000000000000000000, -1.000000000000000000 ) ) ;
#137594 = ADVANCED_FACE ( 'NONE', ( #252763 ), #74180, .T. ) ;
#137595 = CARTESIAN_POINT ( 'NONE',  ( -23.15000000000000213, 1.115600667400684642E-11, -100.5000000000000426 ) ) ;
#137596 = CARTESIAN_POINT ( 'NONE',  ( -20.85000000000000142, 76.00000000001126921, -203.5231074845248997 ) ) ;
#137597 = FACE_OUTER_BOUND ( 'NONE', #100179, .T. ) ;
#137598 = CARTESIAN_POINT ( 'NONE',  ( -17.29158576265543346, 14.82658187305711373, -220.3713364495094709 ) ) ;
#137600 = ORIENTED_EDGE ( 'NONE', *, *, #90094, .T. ) ;
#137599 = CARTESIAN_POINT ( 'NONE',  ( -16.91256925476571382, 66.01426884188435906, -182.5554649955192019 ) ) ;
#137602 = ORIENTED_EDGE ( 'NONE', *, *, #117614, .F. ) ;
#137601 = DIRECTION ( 'NONE',  ( 1.000000000000000000, -0.000000000000000000, -0.000000000000000000 ) ) ;
#137605 = CARTESIAN_POINT ( 'NONE',  ( -16.77308656112214891, 51.61868662400122787, -231.9465479995465103 ) ) ;
#137604 = FACE_OUTER_BOUND ( 'NONE', #214471, .T. ) ;
#137603 = CIRCLE ( 'NONE', #171004, 0.8750000000000007772 ) ;
#137606 = CIRCLE ( 'NONE', #37701, 0.1000000000000028644 ) ;
#137608 = ORIENTED_EDGE ( 'NONE', *, *, #215335, .F. ) ;
#137607 = CYLINDRICAL_SURFACE ( 'NONE', #191757, 1.500000000000001332 ) ;
#137609 = VERTEX_POINT ( 'NONE', #76694 ) ;
#137610 = DIRECTION ( 'NONE',  ( -0.000000000000000000, -6.982962677686266711E-15, 1.000000000000000000 ) ) ;
#137611 = CARTESIAN_POINT ( 'NONE',  ( -23.25000000000000000, 68.76204065042992397, -214.3562485088912126 ) ) ;
#137613 = EDGE_CURVE ( 'NONE', #188240, #151423, #153737, .T. ) ;
#137612 = DIRECTION ( 'NONE',  ( -0.000000000000000000, -0.000000000000000000, -1.000000000000000000 ) ) ;
#137614 = FACE_OUTER_BOUND ( 'NONE', #131519, .T. ) ;
#137615 = EDGE_CURVE ( 'NONE', #28056, #203988, #75455, .T. ) ;
#137616 = EDGE_CURVE ( 'NONE', #192382, #98928, #205043, .T. ) ;
#137617 = CYLINDRICAL_SURFACE ( 'NONE', #84592, 0.09999999999998898659 ) ;
#137618 = DIRECTION ( 'NONE',  ( 1.000000000000000000, 1.394253735153569469E-16, 2.602809386958778209E-16 ) ) ;
#137619 = CARTESIAN_POINT ( 'NONE',  ( 23.14999999999999858, 64.40000000001248281, -176.9513107147999449 ) ) ;
#137620 = CIRCLE ( 'NONE', #75134, 0.5000000000000014433 ) ;
#137621 = EDGE_LOOP ( 'NONE', ( #213902, #33097, #236171, #109165 ) ) ;
#137622 = ORIENTED_EDGE ( 'NONE', *, *, #122278, .F. ) ;
#137623 = DIRECTION ( 'NONE',  ( 1.000000000000000000, 0.000000000000000000, 0.000000000000000000 ) ) ;
#137624 = EDGE_CURVE ( 'NONE', #148058, #8019, #238194, .T. ) ;
#137625 = VECTOR ( 'NONE', #183061, 999.9999999999998863 ) ;
#137626 = ORIENTED_EDGE ( 'NONE', *, *, #226731, .T. ) ;
#137627 = DIRECTION ( 'NONE',  ( 1.000000000000000000, 0.000000000000000000, 0.000000000000000000 ) ) ;
#137628 = DIRECTION ( 'NONE',  ( -1.000000000000000000, 0.000000000000000000, 0.000000000000000000 ) ) ;
#137629 = CARTESIAN_POINT ( 'NONE',  ( 21.07094088545367327, 75.90110629746020265, -176.3432747064415196 ) ) ;
#137630 = AXIS2_PLACEMENT_3D ( 'NONE', #193665, #12474, #110261 ) ;
#137631 = CARTESIAN_POINT ( 'NONE',  ( 18.49999999999999289, 10.20857864376269575, -24.65000000000000213 ) ) ;
#137632 = ORIENTED_EDGE ( 'NONE', *, *, #63454, .F. ) ;
#137633 = CARTESIAN_POINT ( 'NONE',  ( -23.25000000000000000, 7.668827189579289438, -241.6142244293585009 ) ) ;
#137634 = ORIENTED_EDGE ( 'NONE', *, *, #29084, .F. ) ;
#137635 = FACE_OUTER_BOUND ( 'NONE', #58827, .T. ) ;
#137636 = ORIENTED_EDGE ( 'NONE', *, *, #208106, .F. ) ;
#137637 = CIRCLE ( 'NONE', #129299, 6.329289321881371500 ) ;
#137638 = DIRECTION ( 'NONE',  ( 0.000000000000000000, -0.9126074666063768159, -0.4088369013363282178 ) ) ;
#137639 = EDGE_CURVE ( 'NONE', #205612, #230995, #125949, .T. ) ;
#137640 = FACE_OUTER_BOUND ( 'NONE', #236131, .T. ) ;
#137641 = DIRECTION ( 'NONE',  ( 0.000000000000000000, 0.1618390714546066034, -0.9868171638914225996 ) ) ;
#137642 = ORIENTED_EDGE ( 'NONE', *, *, #170940, .F. ) ;
#137643 = DIRECTION ( 'NONE',  ( 0.000000000000000000, -0.000000000000000000, -1.000000000000000000 ) ) ;
#137645 = EDGE_LOOP ( 'NONE', ( #253477, #199433, #122203, #89113 ) ) ;
#137644 = DIRECTION ( 'NONE',  ( 0.000000000000000000, -1.000000000000000000, 0.000000000000000000 ) ) ;
#137646 = DIRECTION ( 'NONE',  ( -4.336808689942052446E-15, 0.8660254037844445918, 0.4999999999999896194 ) ) ;
#137647 = ORIENTED_EDGE ( 'NONE', *, *, #165022, .T. ) ;
#137648 = EDGE_CURVE ( 'NONE', #30937, #38453, #255071, .T. ) ;
#137650 = FACE_OUTER_BOUND ( 'NONE', #193200, .T. ) ;
#137649 =( BOUNDED_SURFACE ( )  B_SPLINE_SURFACE ( 3, 2, ( 
 ( #131257, #65195, #84719 ),
 ( #185147, #50414, #163040 ),
 ( #164313, #71314, #243829 ),
 ( #249929, #5194, #146010 ) ),
 .UNSPECIFIED., .F., .F., .F. ) 
 B_SPLINE_SURFACE_WITH_KNOTS ( ( 4, 4 ),
 ( 3, 3 ),
 ( 0.0002700421466196672679, 0.0004789321604330734573 ),
 ( 0.000000000000000000, 1.000000000000000000 ),
 .UNSPECIFIED. ) 
 GEOMETRIC_REPRESENTATION_ITEM ( )  RATIONAL_B_SPLINE_SURFACE ( (
 ( 1.000000000000000000, 0.7071067811865475727, 1.000000000000000000),
 ( 1.000000000000000000, 0.7163411249512025014, 1.000000000000000000),
 ( 1.000000000000000000, 0.7221957104841917330, 1.000000000000000000),
 ( 1.000000000000000000, 0.7250110520819895710, 1.000000000000000000) ) ) 
 REPRESENTATION_ITEM ( '' )  SURFACE ( )  );
#137651 = ORIENTED_EDGE ( 'NONE', *, *, #51761, .T. ) ;
#137652 = DIRECTION ( 'NONE',  ( 0.000000000000000000, -0.4999999999999348299, 0.8660254037844762331 ) ) ;
#137654 = CARTESIAN_POINT ( 'NONE',  ( -20.00857864376270001, 11.56851667937982775, -211.1200010790121553 ) ) ;
#137653 = VECTOR ( 'NONE', #16344, 1000.000000000000000 ) ;
#137655 = CARTESIAN_POINT ( 'NONE',  ( 21.05000000000000071, 28.37802281961254991, -258.4449340416662722 ) ) ;
#137656 = DIRECTION ( 'NONE',  ( -1.020425574104004196E-15, -6.982962677686266711E-15, 1.000000000000000000 ) ) ;
#137657 = EDGE_CURVE ( 'NONE', #239783, #80656, #141801, .T. ) ;
#137658 = CARTESIAN_POINT ( 'NONE',  ( -21.14999999999999858, 1.115600667400684642E-11, -60.45934304829880546 ) ) ;
#137659 = TOROIDAL_SURFACE ( 'NONE', #171067, 0.6000000000000013101, 0.1000000000000000056 ) ;
#137660 = VERTEX_POINT ( 'NONE', #19301 ) ;
#137661 = DIRECTION ( 'NONE',  ( -0.000000000000000000, -0.000000000000000000, 1.000000000000000000 ) ) ;
#137662 = FACE_OUTER_BOUND ( 'NONE', #215861, .T. ) ;
#137663 = CARTESIAN_POINT ( 'NONE',  ( -20.95000000000000639, 11.75000000001115019, -160.7161343370219129 ) ) ;
#137664 = AXIS2_PLACEMENT_3D ( 'NONE', #220990, #26681, #166208 ) ;
#137665 = ORIENTED_EDGE ( 'NONE', *, *, #63203, .T. ) ;
#137666 = DIRECTION ( 'NONE',  ( -0.000000000000000000, 1.000000000000000000, -0.000000000000000000 ) ) ;
#137667 = VERTEX_POINT ( 'NONE', #137944 ) ;
#137668 = DIRECTION ( 'NONE',  ( 0.000000000000000000, 0.000000000000000000, -1.000000000000000000 ) ) ;
#137669 = ORIENTED_EDGE ( 'NONE', *, *, #249582, .T. ) ;
#137670 = EDGE_CURVE ( 'NONE', #221119, #211199, #23176, .T. ) ;
#137671 = EDGE_CURVE ( 'NONE', #140349, #143381, #63595, .T. ) ;
#137672 = CARTESIAN_POINT ( 'NONE',  ( -21.14999999999999858, -11.74999999998884448, -100.5000000000000284 ) ) ;
#137673 = CARTESIAN_POINT ( 'NONE',  ( 18.49999999999999289, 6.450000000000001066, -10.01702717044001822 ) ) ;
#137674 = AXIS2_PLACEMENT_3D ( 'NONE', #180472, #53144, #16610 ) ;
#137676 = VERTEX_POINT ( 'NONE', #136663 ) ;
#137675 = DIRECTION ( 'NONE',  ( 0.000000000000000000, 0.000000000000000000, -1.000000000000000000 ) ) ;
#137677 = CYLINDRICAL_SURFACE ( 'NONE', #117299, 0.09999999999999939493 ) ;
#137678 = EDGE_LOOP ( 'NONE', ( #209034, #109968, #229514, #242802 ) ) ;
#137679 = FACE_OUTER_BOUND ( 'NONE', #162015, .T. ) ;
#137680 = ORIENTED_EDGE ( 'NONE', *, *, #225763, .F. ) ;
#137681 = ORIENTED_EDGE ( 'NONE', *, *, #66477, .F. ) ;
#137682 = ADVANCED_FACE ( 'NONE', ( #60982 ), #140512, .F. ) ;
#137683 = CARTESIAN_POINT ( 'NONE',  ( -21.02374657821563275, 11.60000000083177696, -194.0717967701982616 ) ) ;
#137684 = EDGE_LOOP ( 'NONE', ( #198326, #37737, #201395, #94602 ) ) ;
#137685 = DIRECTION ( 'NONE',  ( 0.000000000000000000, 0.4721928772777346239, 0.8814952561688430555 ) ) ;
#137686 = CIRCLE ( 'NONE', #46120, 0.5000000000000013323 ) ;
#137688 = EDGE_CURVE ( 'NONE', #112762, #226125, #216201, .T. ) ;
#137687 = CIRCLE ( 'NONE', #108490, 7.900000000000000355 ) ;
#137689 = ORIENTED_EDGE ( 'NONE', *, *, #125586, .F. ) ;
#137690 = ORIENTED_EDGE ( 'NONE', *, *, #133785, .F. ) ;
#137691 = AXIS2_PLACEMENT_3D ( 'NONE', #128015, #208829, #84995 ) ;
#137692 = CARTESIAN_POINT ( 'NONE',  ( -23.25000000000000355, 62.23844973457045882, -209.3750075427748811 ) ) ;
#137693 = ADVANCED_FACE ( 'NONE', ( #18010 ), #209343, .F. ) ;
#137694 = CIRCLE ( 'NONE', #171095, 0.2000000000000057288 ) ;
#137695 = CIRCLE ( 'NONE', #125266, 0.1000000000000000472 ) ;
#137697 = VERTEX_POINT ( 'NONE', #237066 ) ;
#137696 = DIRECTION ( 'NONE',  ( -1.000000000000000000, 0.000000000000000000, 0.000000000000000000 ) ) ;
#137698 = DIRECTION ( 'NONE',  ( 1.000000000000000000, 0.000000000000000000, 0.000000000000000000 ) ) ;
#137699 = CARTESIAN_POINT ( 'NONE',  ( 20.94999999999999574, -1.249999999988843369, -142.0000000000000284 ) ) ;
#137700 = ADVANCED_FACE ( 'NONE', ( #222605 ), #163564, .F. ) ;
#137701 = CARTESIAN_POINT ( 'NONE',  ( -21.29999999999995808, 76.00000000001270450, -207.5731074845243427 ) ) ;
#137703 = DIRECTION ( 'NONE',  ( 0.000000000000000000, 3.469446951953515108E-14, 1.000000000000000000 ) ) ;
#137702 = CARTESIAN_POINT ( 'NONE',  ( 20.94999999999999574, 8.926614585098251453, -41.97168301922312850 ) ) ;
#137704 = CARTESIAN_POINT ( 'NONE',  ( -21.05000000000000071, 64.35000000001218723, -143.5379132551784096 ) ) ;
#137705 = EDGE_CURVE ( 'NONE', #225321, #22313, #80125, .T. ) ;
#137706 = DIRECTION ( 'NONE',  ( 0.000000000000000000, -0.9910827722268055195, -0.1332476588733540468 ) ) ;
#137707 = VECTOR ( 'NONE', #157450, 1000.000000000000000 ) ;
#137708 = CARTESIAN_POINT ( 'NONE',  ( -20.64999999999999858, 76.00000000001213607, -136.5231074845243313 ) ) ;
#137709 = CIRCLE ( 'NONE', #87827, 2.600000000000000089 ) ;
#137710 = AXIS2_PLACEMENT_3D ( 'NONE', #251360, #135251, #213512 ) ;
#137711 = ORIENTED_EDGE ( 'NONE', *, *, #216471, .F. ) ;
#137712 = CIRCLE ( 'NONE', #21249, 0.1999999999999996503 ) ;
#137714 = VERTEX_POINT ( 'NONE', #28323 ) ;
#137713 = VECTOR ( 'NONE', #45459, 1000.000000000000000 ) ;
#137715 = CARTESIAN_POINT ( 'NONE',  ( 20.94999999999999929, 61.94127660284455317, -221.8315191551248517 ) ) ;
#137717 = ORIENTED_EDGE ( 'NONE', *, *, #137203, .T. ) ;
#137716 = CARTESIAN_POINT ( 'NONE',  ( -21.65000000000000213, 52.72272256579932304, -234.4105091754867942 ) ) ;
#137718 = ORIENTED_EDGE ( 'NONE', *, *, #179991, .T. ) ;
#137719 = FACE_OUTER_BOUND ( 'NONE', #237039, .T. ) ;
#137720 = ORIENTED_EDGE ( 'NONE', *, *, #34162, .T. ) ;
#137721 = DIRECTION ( 'NONE',  ( 0.000000000000000000, 0.000000000000000000, -1.000000000000000000 ) ) ;
#137722 = ADVANCED_FACE ( 'NONE', ( #242188 ), #25718, .T. ) ;
#137723 =( BOUNDED_SURFACE ( )  B_SPLINE_SURFACE ( 3, 2, ( 
 ( #94703, #178122, #59395 ),
 ( #138934, #15191, #218483 ),
 ( #39903, #195124, #174303 ),
 ( #119422, #198938, #253768 ) ),
 .UNSPECIFIED., .F., .F., .F. ) 
 B_SPLINE_SURFACE_WITH_KNOTS ( ( 4, 4 ),
 ( 3, 3 ),
 ( 0.04058434257139474644, 0.04256401539001600925 ),
 ( 0.000000000000000000, 1.000000000000000000 ),
 .UNSPECIFIED. ) 
 GEOMETRIC_REPRESENTATION_ITEM ( )  RATIONAL_B_SPLINE_SURFACE ( (
 ( 1.000000000000000000, 0.7103081912008574195, 1.000000000000000000),
 ( 1.000000000000000000, 0.7104998333553186329, 1.000000000000000000),
 ( 1.000000000000000000, 0.7107238315756846392, 1.000000000000000000),
 ( 1.000000000000000000, 0.7110073749539638222, 1.000000000000000000) ) ) 
 REPRESENTATION_ITEM ( '' )  SURFACE ( )  );
#137724 = ADVANCED_FACE ( 'NONE', ( #67407 ), #80308, .T. ) ;
#137725 = AXIS2_PLACEMENT_3D ( 'NONE', #141895, #40270, #42806 ) ;
#137726 = ORIENTED_EDGE ( 'NONE', *, *, #18121, .F. ) ;
#137727 = FILL_AREA_STYLE_COLOUR ( '', #106458 ) ;
#137728 = DIRECTION ( 'NONE',  ( 1.000000000000000000, 0.000000000000000000, 0.000000000000000000 ) ) ;
#137730 = EDGE_LOOP ( 'NONE', ( #131916, #74649, #147233, #3418 ) ) ;
#137729 = ORIENTED_EDGE ( 'NONE', *, *, #93768, .T. ) ;
#137731 = EDGE_LOOP ( 'NONE', ( #113371, #229235, #39144, #29555, #142187 ) ) ;
#137732 = VERTEX_POINT ( 'NONE', #203062 ) ;
#137733 = DIRECTION ( 'NONE',  ( 1.000000000000000000, 0.000000000000000000, 0.000000000000000000 ) ) ;
#137734 = LINE ( 'NONE', #37390, #63432 ) ;
#137736 = VERTEX_POINT ( 'NONE', #63549 ) ;
#137735 = DIRECTION ( 'NONE',  ( 1.000000000000000000, -1.207181226542539700E-16, 2.694675058168174199E-16 ) ) ;
#137737 = CARTESIAN_POINT ( 'NONE',  ( 15.70340296795548163, 12.60783650272741063, -214.9246183040210383 ) ) ;
#137739 = ORIENTED_EDGE ( 'NONE', *, *, #142811, .T. ) ;
#137738 = LINE ( 'NONE', #79038, #180861 ) ;
#137740 = CARTESIAN_POINT ( 'NONE',  ( -23.25000000000000000, 67.23127455305835554, -235.8551265064784559 ) ) ;
#137741 = VERTEX_POINT ( 'NONE', #107817 ) ;
#137742 = DIRECTION ( 'NONE',  ( 0.000000000000000000, 0.000000000000000000, 1.000000000000000000 ) ) ;
#137743 = CIRCLE ( 'NONE', #29476, 0.1000000000000028644 ) ;
#137745 = ORIENTED_EDGE ( 'NONE', *, *, #52346, .F. ) ;
#137744 = DIRECTION ( 'NONE',  ( 0.000000000000000000, 0.000000000000000000, 1.000000000000000000 ) ) ;
#137746 = DIRECTION ( 'NONE',  ( 0.000000000000000000, -1.000000000000000000, 0.000000000000000000 ) ) ;
#137747 = DIRECTION ( 'NONE',  ( -1.000000000000000000, -0.000000000000000000, -0.000000000000000000 ) ) ;
#137748 = DIRECTION ( 'NONE',  ( 1.000000000000000000, -0.000000000000000000, -0.000000000000000000 ) ) ;
#137749 = VERTEX_POINT ( 'NONE', #47824 ) ;
#137751 = CARTESIAN_POINT ( 'NONE',  ( -21.14999999999999503, 64.25000000001190870, -96.10396023856559111 ) ) ;
#137750 = CARTESIAN_POINT ( 'NONE',  ( -16.88705144915432044, 9.950000000011137047, -46.43097859471209432 ) ) ;
#137752 = CARTESIAN_POINT ( 'NONE',  ( -14.56336952470180357, 66.55335465531658201, -84.61230102842418432 ) ) ;
#137753 = CARTESIAN_POINT ( 'NONE',  ( -21.14999999999999858, 11.65000000001115588, -67.10000000000005116 ) ) ;
#137754 = AXIS2_PLACEMENT_3D ( 'NONE', #79938, #18719, #57824 ) ;
#137755 = EDGE_CURVE ( 'NONE', #44901, #139739, #143078, .T. ) ;
#137756 = DIRECTION ( 'NONE',  ( -1.000000000000000000, -0.000000000000000000, -0.000000000000000000 ) ) ;
#137757 = DIRECTION ( 'NONE',  ( -0.000000000000000000, 1.000000000000000000, 0.000000000000000000 ) ) ;
#137758 = ORIENTED_EDGE ( 'NONE', *, *, #63158, .F. ) ;
#137759 = VERTEX_POINT ( 'NONE', #105204 ) ;
#137760 =( BOUNDED_SURFACE ( )  B_SPLINE_SURFACE ( 3, 2, ( 
 ( #134487, #14590, #176226 ),
 ( #254428, #234906, #95383 ),
 ( #232351, #117515, #255692 ),
 ( #114947, #97917, #56236 ) ),
 .UNSPECIFIED., .F., .F., .F. ) 
 B_SPLINE_SURFACE_WITH_KNOTS ( ( 4, 4 ),
 ( 3, 3 ),
 ( -3.469446951953614189E-18, 0.001979672783031532438 ),
 ( 0.000000000000000000, 1.000000000000000000 ),
 .UNSPECIFIED. ) 
 GEOMETRIC_REPRESENTATION_ITEM ( )  RATIONAL_B_SPLINE_SURFACE ( (
 ( 1.000000000000000000, 0.7103081912008198939, 1.000000000000000000),
 ( 1.000000000000000000, 0.7104998333558532053, 1.000000000000000000),
 ( 1.000000000000000000, 0.7107238315755430857, 1.000000000000000000),
 ( 1.000000000000000000, 0.7110073749539379540, 1.000000000000000000) ) ) 
 REPRESENTATION_ITEM ( '' )  SURFACE ( )  );
#137761 = ORIENTED_EDGE ( 'NONE', *, *, #132052, .T. ) ;
#137763 = VECTOR ( 'NONE', #183355, 1000.000000000000000 ) ;
#137762 = LINE ( 'NONE', #136470, #30424 ) ;
#137764 = DIRECTION ( 'NONE',  ( 0.000000000000000000, 0.000000000000000000, -1.000000000000000000 ) ) ;
#137765 = ORIENTED_EDGE ( 'NONE', *, *, #90525, .T. ) ;
#137766 = ORIENTED_EDGE ( 'NONE', *, *, #92606, .F. ) ;
#137767 = DIRECTION ( 'NONE',  ( 0.000000000000000000, 0.000000000000000000, -1.000000000000000000 ) ) ;
#137768 = DIRECTION ( 'NONE',  ( 0.000000000000000000, 0.9126074666063660468, 0.4088369013363524762 ) ) ;
#137769 = CIRCLE ( 'NONE', #245950, 0.09999999999999939493 ) ;
#137770 = ORIENTED_EDGE ( 'NONE', *, *, #204752, .F. ) ;
#137771 = CARTESIAN_POINT ( 'NONE',  ( -18.39999999999999858, -9.519327731081281385, -73.97297637655937308 ) ) ;
#137772 = FILL_AREA_STYLE_COLOUR ( '', #139589 ) ;
#137773 = EDGE_CURVE ( 'NONE', #112792, #198094, #225703, .T. ) ;
#137774 = AXIS2_PLACEMENT_3D ( 'NONE', #192666, #14031, #115689 ) ;
#137776 = ORIENTED_EDGE ( 'NONE', *, *, #29838, .F. ) ;
#137775 = AXIS2_PLACEMENT_3D ( 'NONE', #203201, #46681, #24595 ) ;
#137777 = VERTEX_POINT ( 'NONE', #24463 ) ;
#137778 = ORIENTED_EDGE ( 'NONE', *, *, #135951, .F. ) ;
#137779 = CIRCLE ( 'NONE', #87878, 0.09999999999999939493 ) ;
#137780 = DIRECTION ( 'NONE',  ( -0.000000000000000000, -6.982962677686266711E-15, 1.000000000000000000 ) ) ;
#137781 = CARTESIAN_POINT ( 'NONE',  ( -20.94999999999999929, 14.80545736607782814, -235.9842437978701639 ) ) ;
#137782 = FACE_OUTER_BOUND ( 'NONE', #226521, .T. ) ;
#137783 = FACE_OUTER_BOUND ( 'NONE', #135056, .T. ) ;
#137784 = CARTESIAN_POINT ( 'NONE',  ( -18.50000000000000000, 9.150000000011157653, -55.25000000000004974 ) ) ;
#137786 = CARTESIAN_POINT ( 'NONE',  ( -18.59999999999999787, -1.687074390080403941, -54.18542703345839584 ) ) ;
#137785 = CARTESIAN_POINT ( 'NONE',  ( 21.05000000000000071, 0.01471785653540256221, -161.1552765959100952 ) ) ;
#137787 = DIRECTION ( 'NONE',  ( 1.000000000000000000, 0.000000000000000000, 0.000000000000000000 ) ) ;
#137789 = VERTEX_POINT ( 'NONE', #184784 ) ;
#137788 = CARTESIAN_POINT ( 'NONE',  ( 13.39999999999999858, -11.75000000000000000, 17.70000000000000639 ) ) ;
#137790 = DIRECTION ( 'NONE',  ( 1.000000000000000000, 1.394253735153569469E-16, 2.602809386958778209E-16 ) ) ;
#137791 = ORIENTED_EDGE ( 'NONE', *, *, #79067, .T. ) ;
#137792 = CARTESIAN_POINT ( 'NONE',  ( 18.59999999999999076, 69.45000000001222418, -148.7731074845244166 ) ) ;
#137793 = VERTEX_POINT ( 'NONE', #126081 ) ;
#137794 = ORIENTED_EDGE ( 'NONE', *, *, #90356, .F. ) ;
#137795 = CARTESIAN_POINT ( 'NONE',  ( -20.94999999999999929, 70.10000000001149090, -46.24220724918073699 ) ) ;
#137796 = DIRECTION ( 'NONE',  ( 0.000000000000000000, 0.8660254037844411501, 0.4999999999999956701 ) ) ;
#137797 = CARTESIAN_POINT ( 'NONE',  ( -21.65000000000000213, 68.29142135624888965, -57.27310748452437394 ) ) ;
#137798 = ORIENTED_EDGE ( 'NONE', *, *, #90470, .T. ) ;
#137799 = VECTOR ( 'NONE', #59707, 1000.000000000000000 ) ;
#137800 = DIRECTION ( 'NONE',  ( 0.000000000000000000, -0.9651348961777157509, 0.2617529984165031243 ) ) ;
#137801 = ORIENTED_EDGE ( 'NONE', *, *, #154477, .T. ) ;
#137802 = ORIENTED_EDGE ( 'NONE', *, *, #15526, .T. ) ;
#137803 = CARTESIAN_POINT ( 'NONE',  ( -18.59999999999999787, 36.65892442174935439, -249.5511627012433848 ) ) ;
#137804 = EDGE_LOOP ( 'NONE', ( #148545, #147149, #191617, #67460 ) ) ;
#137805 = CARTESIAN_POINT ( 'NONE',  ( -21.14999999999994174, 82.74366731733570646, -26.36310895752070138 ) ) ;
#137806 = CARTESIAN_POINT ( 'NONE',  ( -21.05000000000000071, 76.00000000001126921, -203.5231074845248997 ) ) ;
#137807 = ORIENTED_EDGE ( 'NONE', *, *, #80232, .T. ) ;
#137808 = DIRECTION ( 'NONE',  ( 0.000000000000000000, 0.000000000000000000, -1.000000000000000000 ) ) ;
#137809 = B_SPLINE_CURVE_WITH_KNOTS ( 'NONE', 3,
 ( #19337, #180988, #98831, #62314, #119736, #141839, #239673, #41487, #248646, #146963, #148264, #85683, #68735 ),
 .UNSPECIFIED., .F., .F.,
 ( 4, 3, 3, 3, 4 ),
 ( -3.224855718284247652E-06, 4.235164736271501695E-22, 6.199515528661409170E-06, 4.034952380126323066E-05, 7.452715123697944196E-05 ),
 .UNSPECIFIED. ) ;
#137810 = CARTESIAN_POINT ( 'NONE',  ( 23.14999999999999858, 66.37271706025207152, -233.9386508266050839 ) ) ;
#137811 = DIRECTION ( 'NONE',  ( 1.000000000000000000, 3.190570557967288949E-16, 6.948722487160392945E-17 ) ) ;
#137812 = EDGE_LOOP ( 'NONE', ( #251860, #114682, #198499, #217740 ) ) ;
#137813 = DIRECTION ( 'NONE',  ( 0.000000000000000000, 0.000000000000000000, -1.000000000000000000 ) ) ;
#137814 = CIRCLE ( 'NONE', #171200, 0.1000000000000066530 ) ;
#137815 = AXIS2_PLACEMENT_3D ( 'NONE', #258037, #80709, #181135 ) ;
#137817 = DIRECTION ( 'NONE',  ( 1.000000000000000000, 0.000000000000000000, 0.000000000000000000 ) ) ;
#137816 = AXIS2_PLACEMENT_3D ( 'NONE', #236361, #79830, #96817 ) ;
#137818 = EDGE_CURVE ( 'NONE', #15448, #59827, #67882, .T. ) ;
#137819 = CIRCLE ( 'NONE', #29537, 0.09999999999998898659 ) ;
#137820 = CYLINDRICAL_SURFACE ( 'NONE', #249000, 0.09999999999999939493 ) ;
#137821 = EDGE_LOOP ( 'NONE', ( #53016, #177077, #118049, #197031 ) ) ;
#137822 = CIRCLE ( 'NONE', #112898, 0.1000000000000028644 ) ;
#137823 = EDGE_CURVE ( 'NONE', #212713, #100153, #64831, .T. ) ;
#137824 = FACE_OUTER_BOUND ( 'NONE', #164326, .T. ) ;
#137825 = ORIENTED_EDGE ( 'NONE', *, *, #90610, .T. ) ;
#137826 = CARTESIAN_POINT ( 'NONE',  ( -18.59999999999999787, 11.65000000001115232, -188.8499999999999659 ) ) ;
#137827 = CARTESIAN_POINT ( 'NONE',  ( -23.15000000000000213, 64.35000000001150511, -48.17310748452440095 ) ) ;
#137828 = ADVANCED_FACE ( 'NONE', ( #8725 ), #255267, .T. ) ;
#137829 = CARTESIAN_POINT ( 'NONE',  ( 18.59999999999999432, 77.16270174994990327, -94.92310748452430857 ) ) ;
#137830 = CARTESIAN_POINT ( 'NONE',  ( 21.05000000000000071, 34.07612324756792077, -243.5412266404783566 ) ) ;
#137831 = CARTESIAN_POINT ( 'NONE',  ( -20.94999999999994600, 64.35000000001120668, -30.12310748452479103 ) ) ;
#137832 = FACE_OUTER_BOUND ( 'NONE', #89148, .T. ) ;
#137833 = AXIS2_PLACEMENT_3D ( 'NONE', #48067, #88451, #229287 ) ;
#137834 = ORIENTED_EDGE ( 'NONE', *, *, #190932, .T. ) ;
#137835 = DIRECTION ( 'NONE',  ( 1.000000000000000000, 0.000000000000000000, 0.000000000000000000 ) ) ;
#137836 = CYLINDRICAL_SURFACE ( 'NONE', #235644, 0.1000000000000028644 ) ;
#137837 = CARTESIAN_POINT ( 'NONE',  ( -18.50000000000000000, 77.44184265367995579, -241.6694879557322793 ) ) ;
#137838 = CARTESIAN_POINT ( 'NONE',  ( 18.60000000000000497, 1.115600667400684642E-11, -33.50000000000000000 ) ) ;
#137839 = EDGE_CURVE ( 'NONE', #77400, #34312, #59455, .T. ) ;
#137840 = CARTESIAN_POINT ( 'NONE',  ( 20.74897398619119215, 65.40430697834514717, -61.84379602826854239 ) ) ;
#137841 = ORIENTED_EDGE ( 'NONE', *, *, #176201, .F. ) ;
#137842 = ORIENTED_EDGE ( 'NONE', *, *, #227098, .F. ) ;
#137843 = DIRECTION ( 'NONE',  ( 0.000000000000000000, 0.000000000000000000, 1.000000000000000000 ) ) ;
#137844 = CARTESIAN_POINT ( 'NONE',  ( -23.25000000000000000, 76.00000000001267608, -203.5231074845243597 ) ) ;
#137845 = FACE_OUTER_BOUND ( 'NONE', #114860, .T. ) ;
#137846 = CARTESIAN_POINT ( 'NONE',  ( -23.15000000000000213, 64.25000000001237765, -170.0231074845244166 ) ) ;
#137847 = DIRECTION ( 'NONE',  ( 0.000000000000000000, -1.000000000000000000, 0.000000000000000000 ) ) ;
#137848 = EDGE_CURVE ( 'NONE', #203407, #193751, #13714, .T. ) ;
#137849 = TOROIDAL_SURFACE ( 'NONE', #67125, 0.2000000000000000111, 0.1000000000000000056 ) ;
#137850 = ORIENTED_EDGE ( 'NONE', *, *, #175835, .F. ) ;
#137851 = CARTESIAN_POINT ( 'NONE',  ( -18.46856557590792036, 47.01365916724044780, -255.2938488308768115 ) ) ;
#137852 = CARTESIAN_POINT ( 'NONE',  ( 21.05000000000000071, 10.68863688179707694, -222.5873974249509217 ) ) ;
#137853 = AXIS2_PLACEMENT_3D ( 'NONE', #87805, #125668, #246894 ) ;
#137854 = ORIENTED_EDGE ( 'NONE', *, *, #8706, .F. ) ;
#137855 = FACE_OUTER_BOUND ( 'NONE', #142554, .T. ) ;
#137856 = FACE_OUTER_BOUND ( 'NONE', #186115, .T. ) ;
#137857 = TOROIDAL_SURFACE ( 'NONE', #250302, 0.2000000000000000111, 0.1000000000000000056 ) ;
#137858 = CIRCLE ( 'NONE', #29774, 0.09999999999999939493 ) ;
#137859 = ORIENTED_EDGE ( 'NONE', *, *, #212927, .T. ) ;
#137860 = DIRECTION ( 'NONE',  ( 0.000000000000000000, -8.338584948901395817E-15, 1.000000000000000000 ) ) ;
#137861 = AXIS2_PLACEMENT_3D ( 'NONE', #6650, #86166, #230868 ) ;
#137862 = ORIENTED_EDGE ( 'NONE', *, *, #3453, .T. ) ;
#137863 = FACE_OUTER_BOUND ( 'NONE', #246794, .T. ) ;
#137864 = CARTESIAN_POINT ( 'NONE',  ( 21.14999999999999858, 11.65000000001115943, -112.6500000000000341 ) ) ;
#137865 = FACE_OUTER_BOUND ( 'NONE', #121788, .T. ) ;
#137866 = CARTESIAN_POINT ( 'NONE',  ( 18.50000972452444969, 65.70673848566940478, -64.06382523348294455 ) ) ;
#137867 = CARTESIAN_POINT ( 'NONE',  ( 20.94999999999999929, 1.115600667400684642E-11, -134.0000000000000284 ) ) ;
#137868 = CARTESIAN_POINT ( 'NONE',  ( 20.95429693346636313, 18.77218889732035834, -228.0090229569942721 ) ) ;
#137869 = FACE_OUTER_BOUND ( 'NONE', #86663, .T. ) ;
#137870 = DIRECTION ( 'NONE',  ( 1.000000000000000000, -0.000000000000000000, -0.000000000000000000 ) ) ;
#137871 = DIRECTION ( 'NONE',  ( 0.000000000000000000, 1.000000000000000000, 0.000000000000000000 ) ) ;
#137872 = CARTESIAN_POINT ( 'NONE',  ( -21.05000000000000071, 28.50120599808395028, -258.2149742250584268 ) ) ;
#137873 = CARTESIAN_POINT ( 'NONE',  ( -18.59999999999999787, -1.249999999988843369, -208.8004807544150481 ) ) ;
#137874 = CIRCLE ( 'NONE', #92097, 0.1000000000000002692 ) ;
#137875 = AXIS2_PLACEMENT_3D ( 'NONE', #156603, #236095, #57444 ) ;
#137876 = CARTESIAN_POINT ( 'NONE',  ( 21.06089410995816635, 10.72529553213474429, -79.20238073104307830 ) ) ;
#137877 = DIRECTION ( 'NONE',  ( -0.000000000000000000, 1.000000000000000000, 6.982962677686266711E-15 ) ) ;
#137878 = EDGE_CURVE ( 'NONE', #10010, #99209, #165226, .T. ) ;
#137879 = EDGE_LOOP ( 'NONE', ( #17796, #176364, #231236, #202880 ) ) ;
#137880 = AXIS2_PLACEMENT_3D ( 'NONE', #117334, #250414, #32707 ) ;
#137881 = CARTESIAN_POINT ( 'NONE',  ( 21.11833042828132889, 6.445644693855303586, 0.007100509059361484118 ) ) ;
#137882 = DIRECTION ( 'NONE',  ( -1.000000000000000000, 0.000000000000000000, 0.000000000000000000 ) ) ;
#137883 = FACE_OUTER_BOUND ( 'NONE', #192218, .T. ) ;
#137884 = CIRCLE ( 'NONE', #17130, 0.5000000000000004441 ) ;
#137886 = EDGE_CURVE ( 'NONE', #225625, #170631, #208222, .T. ) ;
#137885 = CIRCLE ( 'NONE', #162883, 0.09999999999999939493 ) ;
#137887 = ORIENTED_EDGE ( 'NONE', *, *, #161785, .F. ) ;
#137888 = CARTESIAN_POINT ( 'NONE',  ( 20.94999999999999929, -8.999999999988844479, -177.3939691226524076 ) ) ;
#137889 = CARTESIAN_POINT ( 'NONE',  ( -18.50000000000000000, 42.92545512184477730, -254.1955779480491344 ) ) ;
#137890 = ADVANCED_FACE ( 'NONE', ( #244747 ), #17986, .F. ) ;
#137891 = EDGE_LOOP ( 'NONE', ( #185166, #141037, #204715, #133747 ) ) ;
#137893 = EDGE_CURVE ( 'NONE', #221695, #38211, #92810, .T. ) ;
#137892 = CARTESIAN_POINT ( 'NONE',  ( -16.86379686415369150, 9.975217759264314310, -188.4333898890902503 ) ) ;
#137894 = FACE_OUTER_BOUND ( 'NONE', #185885, .T. ) ;
#137895 = AXIS2_PLACEMENT_3D ( 'NONE', #29493, #251053, #72450 ) ;
#137896 = ORIENTED_EDGE ( 'NONE', *, *, #39429, .T. ) ;
#137897 = AXIS2_PLACEMENT_3D ( 'NONE', #54588, #231974, #216221 ) ;
#137898 = CIRCLE ( 'NONE', #71307, 0.2000000000000057288 ) ;
#137899 = AXIS2_PLACEMENT_3D ( 'NONE', #178332, #75384, #137871 ) ;
#137900 = ORIENTED_EDGE ( 'NONE', *, *, #146853, .T. ) ;
#137901 = FACE_OUTER_BOUND ( 'NONE', #39477, .T. ) ;
#137902 = EDGE_CURVE ( 'NONE', #249989, #170195, #50387, .T. ) ;
#137903 = ORIENTED_EDGE ( 'NONE', *, *, #252897, .F. ) ;
#137904 = EDGE_CURVE ( 'NONE', #172948, #162125, #171682, .T. ) ;
#137905 = CARTESIAN_POINT ( 'NONE',  ( -18.59999999999999787, 6.933893972137497030, -204.7856458343735255 ) ) ;
#137906 = DIRECTION ( 'NONE',  ( -0.000000000000000000, -0.000000000000000000, 1.000000000000000000 ) ) ;
#137907 = DIRECTION ( 'NONE',  ( -0.5932847527679298016, 0.8049926720990051576, 0.000000000000000000 ) ) ;
#137908 = EDGE_CURVE ( 'NONE', #222707, #125903, #154002, .T. ) ;
#137909 = DIRECTION ( 'NONE',  ( 0.000000000000000000, -6.982962677686266711E-15, 1.000000000000000000 ) ) ;
#137910 = CARTESIAN_POINT ( 'NONE',  ( 22.47071067811865319, 36.65892442174472876, -249.5511627012454596 ) ) ;
#137911 = CARTESIAN_POINT ( 'NONE',  ( 18.39999999999999503, 11.75000000001113953, -57.75000000000000711 ) ) ;
#137912 = DIRECTION ( 'NONE',  ( -0.000000000000000000, 0.8660254037844383745, -0.5000000000000003331 ) ) ;
#137913 = DIRECTION ( 'NONE',  ( 0.000000000000000000, -7.086529944415894657E-15, 1.000000000000000000 ) ) ;
#137915 = ORIENTED_EDGE ( 'NONE', *, *, #210, .F. ) ;
#137914 = FACE_OUTER_BOUND ( 'NONE', #249752, .T. ) ;
#137916 = ORIENTED_EDGE ( 'NONE', *, *, #237566, .T. ) ;
#137918 = CARTESIAN_POINT ( 'NONE',  ( -21.14999999999999858, 64.35000000001195986, -103.0231074845244024 ) ) ;
#137917 = CARTESIAN_POINT ( 'NONE',  ( 20.84999999999998721, 65.66751761918648356, -63.92826094061123143 ) ) ;
#137920 = ORIENTED_EDGE ( 'NONE', *, *, #214480, .T. ) ;
#137919 = DIRECTION ( 'NONE',  ( 0.000000000000000000, 0.000000000000000000, -1.000000000000000000 ) ) ;
#137921 = ORIENTED_EDGE ( 'NONE', *, *, #171813, .F. ) ;
#137922 = DIRECTION ( 'NONE',  ( -1.000000000000000000, -2.952720810173289112E-16, 0.000000000000000000 ) ) ;
#137923 = CARTESIAN_POINT ( 'NONE',  ( 20.22483756094572271, 9.501904678881089694, -175.6395391287154268 ) ) ;
#137924 = ADVANCED_FACE ( 'NONE', ( #231635 ), #252448, .F. ) ;
#137926 = EDGE_CURVE ( 'NONE', #241225, #129556, #51284, .T. ) ;
#137925 = DIRECTION ( 'NONE',  ( 0.000000000000000000, 0.000000000000000000, 1.000000000000000000 ) ) ;
#137927 = CARTESIAN_POINT ( 'NONE',  ( 18.47073956224755165, -9.471729412471800558, -7.108685752817913261 ) ) ;
#137928 = CARTESIAN_POINT ( 'NONE',  ( 23.14999999999999503, 52.91185528119409298, -244.1460391050142675 ) ) ;
#137929 = EDGE_CURVE ( 'NONE', #142111, #217887, #159474, .T. ) ;
#137930 = EDGE_CURVE ( 'NONE', #219323, #13885, #201152, .T. ) ;
#137931 = DIRECTION ( 'NONE',  ( 0.000000000000000000, 1.000000000000000000, 0.000000000000000000 ) ) ;
#137932 = LINE ( 'NONE', #217464, #127889 ) ;
#137933 = CIRCLE ( 'NONE', #225221, 0.09999999999999543976 ) ;
#137934 = DIRECTION ( 'NONE',  ( 0.000000000000000000, 0.000000000000000000, 1.000000000000000000 ) ) ;
#137935 = ORIENTED_EDGE ( 'NONE', *, *, #1983, .T. ) ;
#137936 = ORIENTED_EDGE ( 'NONE', *, *, #171891, .F. ) ;
#137937 = LINE ( 'NONE', #237058, #43748 ) ;
#137938 = ORIENTED_EDGE ( 'NONE', *, *, #155649, .T. ) ;
#137939 = CARTESIAN_POINT ( 'NONE',  ( 20.95346350065193519, 8.887177249185651107, -142.5117319470354005 ) ) ;
#137940 = EDGE_LOOP ( 'NONE', ( #26341, #222938, #39084, #98605 ) ) ;
#137941 = DIRECTION ( 'NONE',  ( 0.000000000000000000, 0.000000000000000000, -1.000000000000000000 ) ) ;
#137942 = AXIS2_PLACEMENT_3D ( 'NONE', #162216, #217010, #38392 ) ;
#137943 = EDGE_CURVE ( 'NONE', #73802, #11381, #129932, .T. ) ;
#137944 = CARTESIAN_POINT ( 'NONE',  ( -20.85000000000000142, 43.00579525902548994, -254.2551217332645876 ) ) ;
#137945 = LINE ( 'NONE', #217479, #76894 ) ;
#137946 = EDGE_CURVE ( 'NONE', #59523, #28760, #112964, .T. ) ;
#137948 = VERTEX_POINT ( 'NONE', #209485 ) ;
#137947 = DIRECTION ( 'NONE',  ( -1.000000000000000000, 0.000000000000000000, 0.000000000000000000 ) ) ;
#137949 = CARTESIAN_POINT ( 'NONE',  ( -23.25000000000000000, 11.75000000001115552, -100.5000000000000284 ) ) ;
#137950 = ORIENTED_EDGE ( 'NONE', *, *, #183595, .F. ) ;
#137951 = CARTESIAN_POINT ( 'NONE',  ( 5.900000000000059863, 64.65000000001120384, -25.92310748452479174 ) ) ;
#137952 = CARTESIAN_POINT ( 'NONE',  ( 20.94999999999999574, 18.92285928089247804, -233.3572654221044900 ) ) ;
#137953 = LINE ( 'NONE', #19309, #73094 ) ;
#137954 = EDGE_CURVE ( 'NONE', #90057, #160549, #146969, .T. ) ;
#137955 = CYLINDRICAL_SURFACE ( 'NONE', #508, 0.09999999999999939493 ) ;
#137956 = CARTESIAN_POINT ( 'NONE',  ( 21.05000000000000071, -11.74999999998883560, -164.4000000000000057 ) ) ;
#137957 = ORIENTED_EDGE ( 'NONE', *, *, #125577, .T. ) ;
#137959 = CARTESIAN_POINT ( 'NONE',  ( 18.59999999999999076, 11.65000000001115943, -100.5000000000000426 ) ) ;
#137958 = CIRCLE ( 'NONE', #54765, 0.1000000000000024342 ) ;
#137960 = ORIENTED_EDGE ( 'NONE', *, *, #242373, .F. ) ;
#137963 = ORIENTED_EDGE ( 'NONE', *, *, #55721, .F. ) ;
#137962 = DIRECTION ( 'NONE',  ( 0.000000000000000000, 0.9126074666063774821, 0.4088369013363268301 ) ) ;
#137961 = DIRECTION ( 'NONE',  ( 1.000000000000000000, 0.000000000000000000, 0.000000000000000000 ) ) ;
#137964 = AXIS2_PLACEMENT_3D ( 'NONE', #178190, #182019, #257631 ) ;
#137965 = LINE ( 'NONE', #77997, #251931 ) ;
#137966 = DIRECTION ( 'NONE',  ( -7.304098846218134667E-16, -1.000000000000000000, 0.000000000000000000 ) ) ;
#137967 = ORIENTED_EDGE ( 'NONE', *, *, #225652, .T. ) ;
#137968 = CARTESIAN_POINT ( 'NONE',  ( 20.85000000000000142, -0.3238857010703366512, -33.45758958931398297 ) ) ;
#137969 = DIRECTION ( 'NONE',  ( 1.000000000000000000, 0.000000000000000000, 0.000000000000000000 ) ) ;
#137970 = CARTESIAN_POINT ( 'NONE',  ( -16.92209698673604024, 9.949999999999983302, -12.71063556705198039 ) ) ;
#137972 = ORIENTED_EDGE ( 'NONE', *, *, #32224, .T. ) ;
#137971 = CARTESIAN_POINT ( 'NONE',  ( 23.24999999999999645, 7.187745831299792165, -211.5611048126997389 ) ) ;
#137973 = EDGE_CURVE ( 'NONE', #219130, #60211, #117765, .T. ) ;
#137974 = LINE ( 'NONE', #21906, #255770 ) ;
#137975 = ORIENTED_EDGE ( 'NONE', *, *, #234430, .T. ) ;
#137976 = EDGE_CURVE ( 'NONE', #110957, #224935, #251023, .T. ) ;
#137977 = CARTESIAN_POINT ( 'NONE',  ( -16.94878442675512531, 9.991729103002162660, -180.1117804243620810 ) ) ;
#137978 = CARTESIAN_POINT ( 'NONE',  ( 21.53752568617683849, 60.65518257771599764, -234.1741829020553780 ) ) ;
#137979 = DIRECTION ( 'NONE',  ( 0.000000000000000000, -0.9656312546561486299, -0.2599159095384356855 ) ) ;
#137980 = ORIENTED_EDGE ( 'NONE', *, *, #89213, .F. ) ;
#137981 = CARTESIAN_POINT ( 'NONE',  ( -20.64999999999999858, 1.115600667400684642E-11, -167.5000000000000284 ) ) ;
#137982 = ORIENTED_EDGE ( 'NONE', *, *, #134961, .T. ) ;
#137983 = ADVANCED_FACE ( 'NONE', ( #54253 ), #71287, .F. ) ;
#137984 = ADVANCED_FACE ( 'NONE', ( #51670 ), #131231, .T. ) ;
#137985 = DIRECTION ( 'NONE',  ( 0.000000000000000000, 0.000000000000000000, 1.000000000000000000 ) ) ;
#137986 = DIRECTION ( 'NONE',  ( 0.000000000000000000, 0.000000000000000000, -1.000000000000000000 ) ) ;
#137987 = EDGE_LOOP ( 'NONE', ( #4630, #175991, #164677, #216902 ) ) ;
#137988 = CARTESIAN_POINT ( 'NONE',  ( -21.05000000000000071, 1.115600667400684642E-11, -200.9999999999999432 ) ) ;
#137989 = EDGE_CURVE ( 'NONE', #68795, #2625, #251160, .T. ) ;
#137990 = CARTESIAN_POINT ( 'NONE',  ( 20.94999999999999574, 69.45000000001206786, -126.6792853948412159 ) ) ;
#137991 = CONICAL_SURFACE ( 'NONE', #58882, 4.299999999999970512, 0.7853981633974466137 ) ;
#137992 = CIRCLE ( 'NONE', #225476, 11.75000000000001066 ) ;
#137993 = CYLINDRICAL_SURFACE ( 'NONE', #220814, 12.87499999999999822 ) ;
#137994 = ORIENTED_EDGE ( 'NONE', *, *, #233798, .T. ) ;
#137995 = AXIS2_PLACEMENT_3D ( 'NONE', #158728, #94861, #218652 ) ;
#137996 = FACE_OUTER_BOUND ( 'NONE', #4846, .T. ) ;
#137997 = DIRECTION ( 'NONE',  ( 0.000000000000000000, -7.487053152578127080E-15, 1.000000000000000000 ) ) ;
#137998 = CARTESIAN_POINT ( 'NONE',  ( -23.25000000000000355, 11.75000000001113953, -42.75000000000000000 ) ) ;
#137999 = EDGE_CURVE ( 'NONE', #186169, #197596, #30490, .T. ) ;
#138000 = ORIENTED_EDGE ( 'NONE', *, *, #166607, .F. ) ;
#138001 = EDGE_CURVE ( 'NONE', #175396, #232247, #213627, .T. ) ;
#138002 = FACE_OUTER_BOUND ( 'NONE', #87097, .T. ) ;
#138003 = ORIENTED_EDGE ( 'NONE', *, *, #74145, .T. ) ;
#138005 = EDGE_LOOP ( 'NONE', ( #96324, #179310, #243249, #143228 ) ) ;
#138004 = CARTESIAN_POINT ( 'NONE',  ( -21.05000000000000071, 72.02722222756959525, -225.1832529173024398 ) ) ;
#138006 = EDGE_CURVE ( 'NONE', #35640, #25250, #159799, .T. ) ;
#138007 = CIRCLE ( 'NONE', #121498, 0.1000000000000033362 ) ;
#138010 = ORIENTED_EDGE ( 'NONE', *, *, #234578, .T. ) ;
#138009 = ORIENTED_EDGE ( 'NONE', *, *, #228526, .T. ) ;
#138008 = CARTESIAN_POINT ( 'NONE',  ( -21.13498764882296044, 0.001656394731329963003, 6.495618143473942396 ) ) ;
#138011 = DIRECTION ( 'NONE',  ( 1.000000000000000000, -0.000000000000000000, -0.000000000000000000 ) ) ;
#138012 = CARTESIAN_POINT ( 'NONE',  ( -20.93975676684922504, 65.68895814178191017, -30.50265578621382190 ) ) ;
#138013 = CARTESIAN_POINT ( 'NONE',  ( 17.23472005113827876, 10.30788195451192379, -111.9534231399313597 ) ) ;
#138014 = DIRECTION ( 'NONE',  ( 0.000000000000000000, 1.000000000000000000, 6.352154140967427193E-15 ) ) ;
#138015 = DIRECTION ( 'NONE',  ( 1.000000000000000000, 0.000000000000000000, 0.000000000000000000 ) ) ;
#138016 = ADVANCED_FACE ( 'NONE', ( #38557 ), #47013, .T. ) ;
#138017 = CARTESIAN_POINT ( 'NONE',  ( 23.14999999999999858, 1.115600667400684642E-11, -200.9999999999999432 ) ) ;
#138018 = LINE ( 'NONE', #141882, #72350 ) ;
#138020 = DIRECTION ( 'NONE',  ( 0.000000000000000000, 6.982962677686267499E-15, -1.000000000000000000 ) ) ;
#138019 = DIRECTION ( 'NONE',  ( 6.938893903907030216E-14, 0.000000000000000000, -1.000000000000000000 ) ) ;
#138021 = ORIENTED_EDGE ( 'NONE', *, *, #188635, .T. ) ;
#138022 = ORIENTED_EDGE ( 'NONE', *, *, #52221, .F. ) ;
#138023 = EDGE_CURVE ( 'NONE', #178493, #143742, #63787, .T. ) ;
#138024 = FACE_OUTER_BOUND ( 'NONE', #134160, .T. ) ;
#138026 = ORIENTED_EDGE ( 'NONE', *, *, #143512, .T. ) ;
#138025 = CARTESIAN_POINT ( 'NONE',  ( 22.39999999999999503, 1.115600667400684642E-11, -159.7092204016265669 ) ) ;
#138027 = CARTESIAN_POINT ( 'NONE',  ( -17.71734398241072839, 59.45641310563337356, -223.1004793665990746 ) ) ;
#138028 = ORIENTED_EDGE ( 'NONE', *, *, #158333, .F. ) ;
#138030 = PLANE ( 'NONE',  #184983 ) ;
#138029 = TOROIDAL_SURFACE ( 'NONE', #21534, 0.2000000000000000111, 0.1000000000000000056 ) ;
#138031 = VERTEX_POINT ( 'NONE', #137631 ) ;
#138032 = ADVANCED_FACE ( 'NONE', ( #200202 ), #172827, .F. ) ;
#138033 = CARTESIAN_POINT ( 'NONE',  ( -16.87683809663752399, 22.97806745954242302, -230.9350634111226270 ) ) ;
#138034 = EDGE_CURVE ( 'NONE', #167339, #93005, #76376, .T. ) ;
#138035 = AXIS2_PLACEMENT_3D ( 'NONE', #237550, #58879, #19800 ) ;
#138036 = ORIENTED_EDGE ( 'NONE', *, *, #217492, .T. ) ;
#138038 = CIRCLE ( 'NONE', #175498, 0.09999999999999939493 ) ;
#138037 = DIRECTION ( 'NONE',  ( 0.000000000000000000, -6.608470384673536824E-15, 1.000000000000000000 ) ) ;
#138039 = CARTESIAN_POINT ( 'NONE',  ( 21.97500000000000497, 9.749999999999998224, -21.15000000000000213 ) ) ;
#138041 = ORIENTED_EDGE ( 'NONE', *, *, #140449, .F. ) ;
#138040 = ORIENTED_EDGE ( 'NONE', *, *, #111226, .T. ) ;
#138042 = ORIENTED_EDGE ( 'NONE', *, *, #180233, .T. ) ;
#138044 = DIRECTION ( 'NONE',  ( 1.000000000000000000, 0.000000000000000000, 0.000000000000000000 ) ) ;
#138043 = CIRCLE ( 'NONE', #100611, 2.000000000000001776 ) ;
#138045 = ORIENTED_EDGE ( 'NONE', *, *, #170737, .F. ) ;
#138046 = EDGE_LOOP ( 'NONE', ( #235342, #249305, #249013, #216995 ) ) ;
#138047 = CARTESIAN_POINT ( 'NONE',  ( -16.94445028196808778, 12.44605341304038859, -211.1922452800140775 ) ) ;
#138048 = CIRCLE ( 'NONE', #163041, 12.87499999999999822 ) ;
#138050 = ORIENTED_EDGE ( 'NONE', *, *, #126729, .F. ) ;
#138049 = DIRECTION ( 'NONE',  ( 0.000000000000000000, 0.9915357197604860451, -0.1298341882519964408 ) ) ;
#138051 = ADVANCED_FACE ( 'NONE', ( #180638, #39865 ), #158527, .F. ) ;
#138053 = CYLINDRICAL_SURFACE ( 'NONE', #90232, 0.09999999999998898659 ) ;
#138052 = DIRECTION ( 'NONE',  ( 1.186688945009009831E-16, -1.000000000000000000, 0.000000000000000000 ) ) ;
#138054 = CYLINDRICAL_SURFACE ( 'NONE', #24164, 11.75000000000000000 ) ;
#138055 = CARTESIAN_POINT ( 'NONE',  ( -23.25000000000000000, 64.25000000001269029, -203.5231074845244166 ) ) ;
#138056 = FACE_OUTER_BOUND ( 'NONE', #138615, .T. ) ;
#138057 = ORIENTED_EDGE ( 'NONE', *, *, #215127, .F. ) ;
#138058 = VECTOR ( 'NONE', #137429, 1000.000000000000000 ) ;
#138059 = EDGE_LOOP ( 'NONE', ( #232973, #209257, #64178, #138365 ) ) ;
#138060 = LINE ( 'NONE', #224960, #237215 ) ;
#138061 = DIRECTION ( 'NONE',  ( 1.000000000000000000, 0.000000000000000000, -0.000000000000000000 ) ) ;
#138062 = FACE_OUTER_BOUND ( 'NONE', #158105, .T. ) ;
#138064 = VERTEX_POINT ( 'NONE', #219746 ) ;
#138063 = TOROIDAL_SURFACE ( 'NONE', #25656, 0.2000000000000000111, 0.1000000000000000056 ) ;
#138065 = DIRECTION ( 'NONE',  ( -1.000000000000000000, -0.000000000000000000, -0.000000000000000000 ) ) ;
#138066 = CIRCLE ( 'NONE', #25659, 0.09999999999999939493 ) ;
#138067 = DIRECTION ( 'NONE',  ( 0.000000000000000000, -7.056502275159890043E-15, 1.000000000000000000 ) ) ;
#138068 = CARTESIAN_POINT ( 'NONE',  ( 16.27683809663749770, 41.27791846035906786, -237.2365415511148115 ) ) ;
#138069 = ORIENTED_EDGE ( 'NONE', *, *, #209218, .T. ) ;
#138070 = ORIENTED_EDGE ( 'NONE', *, *, #111451, .F. ) ;
#138071 =( GEOMETRIC_REPRESENTATION_CONTEXT ( 3 ) GLOBAL_UNCERTAINTY_ASSIGNED_CONTEXT ( ( #206886 ) ) GLOBAL_UNIT_ASSIGNED_CONTEXT ( ( #169016, #12489, #24680 ) ) REPRESENTATION_CONTEXT ( 'NONE', 'WORKASPACE' ) );
#138072 = DIRECTION ( 'NONE',  ( -1.000000000000000000, 0.000000000000000000, 0.000000000000000000 ) ) ;
#138073 = ADVANCED_FACE ( 'NONE', ( #239327 ), #58090, .T. ) ;
#138074 = PLANE ( 'NONE',  #140424 ) ;
#138075 = EDGE_LOOP ( 'NONE', ( #55368, #131106, #108367, #111399 ) ) ;
#138076 = CARTESIAN_POINT ( 'NONE',  ( -20.94999999999994600, 66.15000000001120384, -5.923107484524795296 ) ) ;
#138077 = ORIENTED_EDGE ( 'NONE', *, *, #145536, .F. ) ;
#138078 = DIRECTION ( 'NONE',  ( -0.7071067811865127117, -0.7071067811865821007, 0.000000000000000000 ) ) ;
#138080 = AXIS2_PLACEMENT_3D ( 'NONE', #62921, #146301, #104584 ) ;
#138079 = LINE ( 'NONE', #235899, #216394 ) ;
#138082 = CARTESIAN_POINT ( 'NONE',  ( -21.64999999999999858, 7.250000000011148416, -45.75000000000000000 ) ) ;
#138081 = DIRECTION ( 'NONE',  ( -0.000000000000000000, 0.1332476588733665090, 0.9910827722268039652 ) ) ;
#138083 = DIRECTION ( 'NONE',  ( 0.000000000000000000, 0.000000000000000000, -1.000000000000000000 ) ) ;
#138084 = CARTESIAN_POINT ( 'NONE',  ( 21.00000000000000000, 8.058024882095860875, 1.378482379536266178 ) ) ;
#138085 = EDGE_CURVE ( 'NONE', #21212, #123927, #126122, .T. ) ;
#138086 = VECTOR ( 'NONE', #67674, 1000.000000000000000 ) ;
#138087 = AXIS2_PLACEMENT_3D ( 'NONE', #38423, #117953, #84894 ) ;
#138088 =( BOUNDED_SURFACE ( )  B_SPLINE_SURFACE ( 3, 2, ( 
 ( #211778, #47529, #210490 ),
 ( #228773, #111386, #168833 ),
 ( #129660, #209190, #110089 ),
 ( #190945, #250877, #206625 ),
 ( #189643, #127090, #117798 ),
 ( #16164, #255972, #254694 ),
 ( #257257, #175253, #196063 ),
 ( #77372, #235186, #57808 ) ),
 .UNSPECIFIED., .F., .F., .T. ) 
 B_SPLINE_SURFACE_WITH_KNOTS ( ( 4, 2, 2, 4 ),
 ( 3, 3 ),
 ( 0.0001704874539069779586, 0.0003809798300636547323, 0.0004862260181419930920, 0.0005914722062203315060 ),
 ( 0.000000000000000000, 1.000000000000000000 ),
 .UNSPECIFIED. ) 
 GEOMETRIC_REPRESENTATION_ITEM ( )  RATIONAL_B_SPLINE_SURFACE ( (
 ( 1.000000000000000000, 0.7071067811865088260, 1.000000000000000000),
 ( 1.000000000000000000, 0.7670648383569527162, 1.000000000000000000),
 ( 1.000000000000000000, 0.8204820770261292973, 1.000000000000000000),
 ( 1.000000000000000000, 0.8877218296109479212, 1.000000000000000000),
 ( 1.000000000000000000, 0.9080815932664854095, 1.000000000000000000),
 ( 1.000000000000000000, 0.9395541505862110565, 1.000000000000000000),
 ( 1.000000000000000000, 0.9506520335378865205, 1.000000000000000000),
 ( 1.000000000000000000, 0.9504532311154486601, 1.000000000000000000) ) ) 
 REPRESENTATION_ITEM ( '' )  SURFACE ( )  );
#138089 = VECTOR ( 'NONE', #12528, 1000.000000000000000 ) ;
#138091 = VERTEX_POINT ( 'NONE', #119383 ) ;
#138090 = VERTEX_POINT ( 'NONE', #77656 ) ;
#138093 = ORIENTED_EDGE ( 'NONE', *, *, #26837, .T. ) ;
#138092 = AXIS2_PLACEMENT_3D ( 'NONE', #186567, #88707, #168320 ) ;
#138094 = CARTESIAN_POINT ( 'NONE',  ( -17.01473183483382456, 12.43531352672262180, -211.3405985074572584 ) ) ;
#138095 = CARTESIAN_POINT ( 'NONE',  ( -21.05000000000000071, 76.00000000001188027, -99.02310748452428868 ) ) ;
#138096 = DIRECTION ( 'NONE',  ( -1.000000000000000000, 0.000000000000000000, -0.000000000000000000 ) ) ;
#138098 = CARTESIAN_POINT ( 'NONE',  ( 20.85000000000000142, 76.00000000001142553, -36.02310748452432421 ) ) ;
#138097 = CARTESIAN_POINT ( 'NONE',  ( -23.15000000000000213, 4.150000000011156764, -155.7499999999999716 ) ) ;
#138099 = CARTESIAN_POINT ( 'NONE',  ( -16.77683809663752257, 66.05416425680736836, -48.68705650362859672 ) ) ;
#138100 = VERTEX_POINT ( 'NONE', #41148 ) ;
#138101 = CARTESIAN_POINT ( 'NONE',  ( -20.54999999999999716, 85.00000000001149658, -45.91707660717669626 ) ) ;
#138102 = ORIENTED_EDGE ( 'NONE', *, *, #160261, .T. ) ;
#138103 = ORIENTED_EDGE ( 'NONE', *, *, #18445, .F. ) ;
#138104 = FACE_OUTER_BOUND ( 'NONE', #162504, .T. ) ;
#138105 = CARTESIAN_POINT ( 'NONE',  ( -16.97683809663752186, 12.57413723904469904, -211.9780204941619104 ) ) ;
#138106 = DIRECTION ( 'NONE',  ( 0.000000000000000000, -0.9654727137038715545, 0.2605042016806676242 ) ) ;
#138107 = CARTESIAN_POINT ( 'NONE',  ( 12.47034474403012183, 9.375538102059158163, -82.86987588099087532 ) ) ;
#138108 = AXIS2_PLACEMENT_3D ( 'NONE', #127862, #66601, #28802 ) ;
#138109 = DIRECTION ( 'NONE',  ( -1.000000000000000000, -7.304098846218134667E-16, 0.000000000000000000 ) ) ;
#138110 = ORIENTED_EDGE ( 'NONE', *, *, #124571, .F. ) ;
#138111 = ORIENTED_EDGE ( 'NONE', *, *, #229565, .T. ) ;
#138112 = CARTESIAN_POINT ( 'NONE',  ( -21.12844524849339223, 11.75000000001115197, -40.40441347084259860 ) ) ;
#138113 = ORIENTED_EDGE ( 'NONE', *, *, #142003, .F. ) ;
#138114 = CARTESIAN_POINT ( 'NONE',  ( -17.11825945287482753, 23.06621698515930419, -230.9822826988504119 ) ) ;
#138115 = DIRECTION ( 'NONE',  ( 0.000000000000000000, -6.938893903907222067E-15, -1.000000000000000000 ) ) ;
#138116 = CARTESIAN_POINT ( 'NONE',  ( -22.39999999999999858, 65.09550114356427741, -243.3481044654562879 ) ) ;
#138117 = DIRECTION ( 'NONE',  ( 0.000000000000000000, 0.000000000000000000, 1.000000000000000000 ) ) ;
#138118 = CARTESIAN_POINT ( 'NONE',  ( -18.39999999999999858, 85.60000000001264198, -196.4910380878246201 ) ) ;
#138119 = AXIS2_PLACEMENT_3D ( 'NONE', #2020, #22915, #144100 ) ;
#138120 = LINE ( 'NONE', #20782, #29446 ) ;
#138122 = CYLINDRICAL_SURFACE ( 'NONE', #228947, 0.09999999999999939493 ) ;
#138121 = DIRECTION ( 'NONE',  ( 0.000000000000000000, 0.000000000000000000, -1.000000000000000000 ) ) ;
#138124 = ADVANCED_FACE ( 'NONE', ( #175523 ), #116809, .F. ) ;
#138123 = FACE_OUTER_BOUND ( 'NONE', #194583, .T. ) ;
#138125 = FACE_OUTER_BOUND ( 'NONE', #136706, .T. ) ;
#138126 = CARTESIAN_POINT ( 'NONE',  ( -22.57320508075686405, 11.75000000001115552, -134.0000000000000568 ) ) ;
#138127 = CARTESIAN_POINT ( 'NONE',  ( 21.14999999999999858, 69.45934304831143891, -203.5231074845243882 ) ) ;
#138129 = ORIENTED_EDGE ( 'NONE', *, *, #199194, .F. ) ;
#138128 = CARTESIAN_POINT ( 'NONE',  ( 18.59999999999999076, 65.79142135624984178, -182.1731074845244223 ) ) ;
#138130 = VECTOR ( 'NONE', #150072, 1000.000000000000000 ) ;
#138131 = EDGE_CURVE ( 'NONE', #175678, #164109, #18979, .T. ) ;
#138132 = DIRECTION ( 'NONE',  ( -2.812466655313720057E-14, -0.9594490217226113726, -0.2818822000686178608 ) ) ;
#138133 = ORIENTED_EDGE ( 'NONE', *, *, #34503, .T. ) ;
#138134 =( BOUNDED_SURFACE ( )  B_SPLINE_SURFACE ( 3, 2, ( 
 ( #220355, #161675, #242457 ),
 ( #123817, #65112, #2560 ),
 ( #102939, #100363, #182522 ),
 ( #122539, #40463, #5105 ) ),
 .UNSPECIFIED., .F., .F., .F. ) 
 B_SPLINE_SURFACE_WITH_KNOTS ( ( 4, 4 ),
 ( 3, 3 ),
 ( 0.04058434257139457990, 0.04256401539001584966 ),
 ( 0.000000000000000000, 1.000000000000000000 ),
 .UNSPECIFIED. ) 
 GEOMETRIC_REPRESENTATION_ITEM ( )  RATIONAL_B_SPLINE_SURFACE ( (
 ( 1.000000000000000000, 0.7103081912008383236, 1.000000000000000000),
 ( 1.000000000000000000, 0.7104998333555154755, 1.000000000000000000),
 ( 1.000000000000000000, 0.7107238315755263214, 1.000000000000000000),
 ( 1.000000000000000000, 0.7110073749539205235, 1.000000000000000000) ) ) 
 REPRESENTATION_ITEM ( '' )  SURFACE ( )  );
#138135 = DIRECTION ( 'NONE',  ( -3.265361837132813093E-16, -1.000000000000000000, -6.982962677686266711E-15 ) ) ;
#138136 = EDGE_CURVE ( 'NONE', #74229, #234918, #98475, .T. ) ;
#138137 = CARTESIAN_POINT ( 'NONE',  ( -18.38204789744325396, 54.09641185402763597, -229.1605894844069837 ) ) ;
#138138 = ORIENTED_EDGE ( 'NONE', *, *, #232337, .T. ) ;
#138139 = CYLINDRICAL_SURFACE ( 'NONE', #188239, 0.1000000000000064587 ) ;
#138140 = CARTESIAN_POINT ( 'NONE',  ( -21.14999999999999858, 11.75000000001115552, -107.2261306360592243 ) ) ;
#138141 = CYLINDRICAL_SURFACE ( 'NONE', #67149, 0.09999999999999939493 ) ;
#138142 = AXIS2_PLACEMENT_3D ( 'NONE', #200708, #59881, #22083 ) ;
#138143 = EDGE_CURVE ( 'NONE', #149556, #16833, #176235, .T. ) ;
#138144 = DIRECTION ( 'NONE',  ( 1.000000000000000000, 1.394253735153569469E-16, 2.602809386958778209E-16 ) ) ;
#138145 = DIRECTION ( 'NONE',  ( 0.000000000000000000, -0.4999999999999608646, 0.8660254037844612451 ) ) ;
#138147 = CARTESIAN_POINT ( 'NONE',  ( -21.05000000000000071, -1.360870587192041681, -8.072997927090961312 ) ) ;
#138146 = AXIS2_PLACEMENT_3D ( 'NONE', #171327, #70918, #91734 ) ;
#138148 = EDGE_CURVE ( 'NONE', #64314, #213025, #163643, .T. ) ;
#138149 = ORIENTED_EDGE ( 'NONE', *, *, #106749, .F. ) ;
#138150 = DIRECTION ( 'NONE',  ( -1.000000000000000000, -1.652117596168391700E-15, -1.153667551319263085E-29 ) ) ;
#138152 = VERTEX_POINT ( 'NONE', #243164 ) ;
#138151 = DIRECTION ( 'NONE',  ( 0.000000000000000000, 0.000000000000000000, 1.000000000000000000 ) ) ;
#138153 = CARTESIAN_POINT ( 'NONE',  ( -21.05000000000000071, 87.48912529308842068, -166.9231074845242802 ) ) ;
#138154 = CARTESIAN_POINT ( 'NONE',  ( -20.07928932188135107, 66.77928932189340117, -124.1731074845243654 ) ) ;
#138155 = ADVANCED_FACE ( 'NONE', ( #7113 ), #64531, .T. ) ;
#138156 = DIRECTION ( 'NONE',  ( 1.000000000000000000, 0.000000000000000000, 0.000000000000000000 ) ) ;
#138157 = VERTEX_POINT ( 'NONE', #102340 ) ;
#138158 = CARTESIAN_POINT ( 'NONE',  ( -22.43310005002225438, 75.99436305787135382, -148.1727696116587083 ) ) ;
#138159 = APPLICATION_PROTOCOL_DEFINITION ( 'draft international standard', 'automotive_design', 1998, #255667 ) ;
#138160 = B_SPLINE_CURVE_WITH_KNOTS ( 'NONE', 3,
 ( #23358, #102835, #98974, #186262 ),
 .UNSPECIFIED., .F., .F.,
 ( 4, 4 ),
 ( 0.000000000000000000, 7.713889350928753320E-05 ),
 .UNSPECIFIED. ) ;
#138162 = ADVANCED_FACE ( 'NONE', ( #22870 ), #123228, .T. ) ;
#138161 = CARTESIAN_POINT ( 'NONE',  ( 22.59999999999999432, -2.401771312552908544, -189.4980873520049727 ) ) ;
#138163 = AXIS2_PLACEMENT_3D ( 'NONE', #114470, #153658, #195321 ) ;
#138164 = EDGE_LOOP ( 'NONE', ( #189996, #159144, #60784, #256417 ) ) ;
#138165 = CARTESIAN_POINT ( 'NONE',  ( 20.94999999999999929, 68.97833521811203639, -132.6895420826271277 ) ) ;
#138166 = SPHERICAL_SURFACE ( 'NONE', #125840, 0.1000000000000000056 ) ;
#138167 = DIRECTION ( 'NONE',  ( 0.000000000000000000, 0.5907332058517377193, -0.8068669527896954463 ) ) ;
#138168 = EDGE_LOOP ( 'NONE', ( #87027, #142599, #253376, #1923 ) ) ;
#138169 = ORIENTED_EDGE ( 'NONE', *, *, #171466, .F. ) ;
#138170 = FACE_OUTER_BOUND ( 'NONE', #3178, .T. ) ;
#138171 = DIRECTION ( 'NONE',  ( 1.000000000000000000, 3.265361837132813093E-16, -0.000000000000000000 ) ) ;
#138172 = EDGE_CURVE ( 'NONE', #231379, #187553, #185767, .T. ) ;
#138173 = LINE ( 'NONE', #216440, #19576 ) ;
#138174 = CARTESIAN_POINT ( 'NONE',  ( -22.47071067811865319, 67.23127455305841238, -235.8551265064783991 ) ) ;
#138176 = CARTESIAN_POINT ( 'NONE',  ( 18.49999999999999289, 10.44006789215403330, -125.2671177488814607 ) ) ;
#138175 = VECTOR ( 'NONE', #230980, 1000.000000000000000 ) ;
#138177 = VECTOR ( 'NONE', #248122, 1000.000000000000000 ) ;
#138180 = FACE_OUTER_BOUND ( 'NONE', #29436, .T. ) ;
#138179 = TOROIDAL_SURFACE ( 'NONE', #79900, 11.65000000000000036, 0.1000000000000000056 ) ;
#138178 = SPHERICAL_SURFACE ( 'NONE', #3702, 0.1000000000000000056 ) ;
#138181 = CARTESIAN_POINT ( 'NONE',  ( -23.15000000000000213, 84.66355140188105111, -93.49900636645693908 ) ) ;
#138182 = CARTESIAN_POINT ( 'NONE',  ( -20.54999999999999716, 71.75000000001156764, -57.27310748452435263 ) ) ;
#138183 = DIRECTION ( 'NONE',  ( 0.000000000000000000, 0.2605042016806672911, -0.9654727137038716656 ) ) ;
#138184 = VERTEX_POINT ( 'NONE', #5822 ) ;
#138185 = ORIENTED_EDGE ( 'NONE', *, *, #86847, .T. ) ;
#138186 = DIRECTION ( 'NONE',  ( -1.000000000000000000, 0.000000000000000000, 0.000000000000000000 ) ) ;
#138188 = CYLINDRICAL_SURFACE ( 'NONE', #136915, 4.049999999999998046 ) ;
#138187 = CARTESIAN_POINT ( 'NONE',  ( 21.08078803292165659, 69.66698703557453598, -69.60229347168214531 ) ) ;
#138189 = EDGE_CURVE ( 'NONE', #43158, #133225, #197333, .T. ) ;
#138190 = LINE ( 'NONE', #157828, #110216 ) ;
#138191 = CARTESIAN_POINT ( 'NONE',  ( -21.14999999999999858, 12.92448621296781930, -205.1280733356431938 ) ) ;
#138192 = CARTESIAN_POINT ( 'NONE',  ( 20.94999999999999929, 1.115600667400684642E-11, -200.9999999999999432 ) ) ;
#138193 = ORIENTED_EDGE ( 'NONE', *, *, #214076, .T. ) ;
#138194 = EDGE_CURVE ( 'NONE', #169542, #66484, #68065, .T. ) ;
#138196 = ORIENTED_EDGE ( 'NONE', *, *, #117310, .T. ) ;
#138195 = AXIS2_PLACEMENT_3D ( 'NONE', #22783, #240520, #136251 ) ;
#138197 = DIRECTION ( 'NONE',  ( -0.000000000000000000, -0.000000000000000000, -1.000000000000000000 ) ) ;
#138198 = EDGE_LOOP ( 'NONE', ( #194697, #8519, #161351, #229351, #209754, #249075, #155481, #126532, #80083, #162417 ) ) ;
#138199 = EDGE_CURVE ( 'NONE', #32708, #74886, #47517, .T. ) ;
#138200 = CARTESIAN_POINT ( 'NONE',  ( -23.15000000000000213, 6.835897784820962109, -211.9460267437856373 ) ) ;
#138201 = EDGE_CURVE ( 'NONE', #204625, #206475, #175661, .T. ) ;
#138202 = LINE ( 'NONE', #82073, #200458 ) ;
#138203 = EDGE_LOOP ( 'NONE', ( #131247, #72690, #236954, #69191 ) ) ;
#138204 = LINE ( 'NONE', #178682, #180805 ) ;
#138205 = CIRCLE ( 'NONE', #826, 7.800000000000001599 ) ;
#138206 = EDGE_CURVE ( 'NONE', #153790, #23751, #8422, .T. ) ;
#138207 = EDGE_LOOP ( 'NONE', ( #92550, #89343, #67582, #204971 ) ) ;
#138208 = CYLINDRICAL_SURFACE ( 'NONE', #16533, 0.09999999999999939493 ) ;
#138209 = CARTESIAN_POINT ( 'NONE',  ( 18.39999999999999858, -9.682403433465241349, -140.6568433774128266 ) ) ;
#138211 = VECTOR ( 'NONE', #229245, 1000.000000000000000 ) ;
#138210 = PLANE ( 'NONE',  #144887 ) ;
#138212 = EDGE_CURVE ( 'NONE', #39296, #81779, #184469, .T. ) ;
#138213 = CARTESIAN_POINT ( 'NONE',  ( -18.44448725179913851, 77.16080881524374036, -241.8056823530271231 ) ) ;
#138214 = EDGE_CURVE ( 'NONE', #54594, #41070, #65814, .T. ) ;
#138215 = CARTESIAN_POINT ( 'NONE',  ( 21.05000000000000071, 65.56210617110382088, -241.8873743484695353 ) ) ;
#138217 = CARTESIAN_POINT ( 'NONE',  ( 18.59999999999999432, 74.36282728704222222, -191.9409541190523498 ) ) ;
#138216 = CARTESIAN_POINT ( 'NONE',  ( 21.05000000000000071, -11.64999999998883595, -63.89999999999999858 ) ) ;
#138218 = CIRCLE ( 'NONE', #55377, 0.1000000000000000056 ) ;
#138220 = CARTESIAN_POINT ( 'NONE',  ( 20.94999999999999929, 85.00000000001149658, -45.91707660717670336 ) ) ;
#138219 = AXIS2_PLACEMENT_3D ( 'NONE', #33159, #110079, #227455 ) ;
#138221 = AXIS2_PLACEMENT_3D ( 'NONE', #13301, #195809, #253178 ) ;
#138222 = ORIENTED_EDGE ( 'NONE', *, *, #25154, .F. ) ;
#138224 = FACE_OUTER_BOUND ( 'NONE', #46829, .T. ) ;
#138223 = DIRECTION ( 'NONE',  ( 1.000000000000000000, -0.000000000000000000, -0.000000000000000000 ) ) ;
#138225 = ORIENTED_EDGE ( 'NONE', *, *, #245151, .T. ) ;
#138227 = ORIENTED_EDGE ( 'NONE', *, *, #174167, .T. ) ;
#138226 = DIRECTION ( 'NONE',  ( 1.000000000000000000, 0.000000000000000000, 0.000000000000000000 ) ) ;
#138228 = ORIENTED_EDGE ( 'NONE', *, *, #138962, .T. ) ;
#138229 = PLANE ( 'NONE',  #49220 ) ;
#138230 = CARTESIAN_POINT ( 'NONE',  ( -21.46681500597819081, 1.115542391533913547E-11, -26.64248884057156630 ) ) ;
#138231 = DIRECTION ( 'NONE',  ( 0.000000000000000000, -0.2617529984167792922, -0.9651348961776409219 ) ) ;
#138232 = EDGE_CURVE ( 'NONE', #143246, #165624, #10770, .T. ) ;
#138233 = CARTESIAN_POINT ( 'NONE',  ( 23.25000000000000000, -11.64999999998884483, -167.4999999999999432 ) ) ;
#138234 = VECTOR ( 'NONE', #226678, 1000.000000000000000 ) ;
#138235 = ORIENTED_EDGE ( 'NONE', *, *, #199378, .T. ) ;
#138236 = DIRECTION ( 'NONE',  ( -0.000000000000000000, -1.000000000000000000, -6.982962677686266711E-15 ) ) ;
#138237 = CARTESIAN_POINT ( 'NONE',  ( 18.49999999999999289, 10.49142135624846439, -125.3500000000000512 ) ) ;
#138238 = CARTESIAN_POINT ( 'NONE',  ( -21.14999999999999503, 64.25000000001264766, -196.6039602385656337 ) ) ;
#138239 = VERTEX_POINT ( 'NONE', #247010 ) ;
#138240 = VECTOR ( 'NONE', #53126, 999.9999999999998863 ) ;
#138241 = FACE_OUTER_BOUND ( 'NONE', #92334, .T. ) ;
#138242 = AXIS2_PLACEMENT_3D ( 'NONE', #94508, #32004, #111520 ) ;
#138243 = AXIS2_PLACEMENT_3D ( 'NONE', #19282, #77955, #179656 ) ;
#138244 = ORIENTED_EDGE ( 'NONE', *, *, #49517, .F. ) ;
#138245 = ORIENTED_EDGE ( 'NONE', *, *, #162096, .F. ) ;
#138246 = DIRECTION ( 'NONE',  ( 1.000000000000000000, 0.000000000000000000, 0.000000000000000000 ) ) ;
#138247 = CIRCLE ( 'NONE', #213087, 4.000000000000003553 ) ;
#138248 = ORIENTED_EDGE ( 'NONE', *, *, #227989, .F. ) ;
#138249 = CARTESIAN_POINT ( 'NONE',  ( -17.73285935861547813, 10.85798180378979971, -10.24143819022076052 ) ) ;
#138250 = EDGE_LOOP ( 'NONE', ( #39260, #116997, #234728, #123230 ) ) ;
#138251 = CARTESIAN_POINT ( 'NONE',  ( 20.85882249326303040, 10.33248238083634796, -173.0948465439131496 ) ) ;
#138252 = TOROIDAL_SURFACE ( 'NONE', #25857, 2.100000000000002309, 0.1000000000000000056 ) ;
#138253 = EDGE_CURVE ( 'NONE', #203104, #94857, #63239, .T. ) ;
#138254 = CARTESIAN_POINT ( 'NONE',  ( -33.30000000000001137, 3.332938107839112263, -347.0000000000001137 ) ) ;
#138255 = DIRECTION ( 'NONE',  ( 0.000000000000000000, -6.982962677686266711E-15, 1.000000000000000000 ) ) ;
#138256 = EDGE_CURVE ( 'NONE', #23498, #147377, #243024, .T. ) ;
#138257 = DIRECTION ( 'NONE',  ( 0.000000000000000000, 0.2128009952263602289, -0.9770955615653316162 ) ) ;
#138258 = ADVANCED_FACE ( 'NONE', ( #153105 ), #72251, .F. ) ;
#138259 = DIRECTION ( 'NONE',  ( 0.000000000000000000, 1.000000000000000000, 0.000000000000000000 ) ) ;
#138260 = CARTESIAN_POINT ( 'NONE',  ( -21.09316766718153247, 0.03926340232583150347, -27.12984668752529060 ) ) ;
#138261 = DIRECTION ( 'NONE',  ( 0.000000000000000000, 0.000000000000000000, -1.000000000000000000 ) ) ;
#138262 = VERTEX_POINT ( 'NONE', #249605 ) ;
#138264 = CYLINDRICAL_SURFACE ( 'NONE', #31572, 0.09999999999999939493 ) ;
#138263 = FACE_OUTER_BOUND ( 'NONE', #9444, .T. ) ;
#138265 = ORIENTED_EDGE ( 'NONE', *, *, #107408, .F. ) ;
#138268 = ORIENTED_EDGE ( 'NONE', *, *, #128011, .F. ) ;
#138267 = CARTESIAN_POINT ( 'NONE',  ( -18.47653818581421348, 85.46528038777458391, -62.39714666838443691 ) ) ;
#138266 = LINE ( 'NONE', #20941, #177986 ) ;
#138269 = AXIS2_PLACEMENT_3D ( 'NONE', #217097, #175454, #157179 ) ;
#138270 = ORIENTED_EDGE ( 'NONE', *, *, #231237, .F. ) ;
#138271 = FACE_OUTER_BOUND ( 'NONE', #121103, .T. ) ;
#138272 = CONICAL_SURFACE ( 'NONE', #29988, 4.299999999999964295, 0.7853981633974466137 ) ;
#138273 = CARTESIAN_POINT ( 'NONE',  ( 12.25000000000000000, 66.65000000001228386, -153.5015881126993520 ) ) ;
#138274 = CARTESIAN_POINT ( 'NONE',  ( 21.14999999999999503, 87.75000000001173817, -81.27310748452423184 ) ) ;
#138275 = CARTESIAN_POINT ( 'NONE',  ( -16.78493832629887450, 9.945835743215301505, -113.1639490191042796 ) ) ;
#138276 = VERTEX_POINT ( 'NONE', #128370 ) ;
#138277 = FACE_BOUND ( 'NONE', #184181, .T. ) ;
#138278 = DIRECTION ( 'NONE',  ( 7.304098846218134667E-16, 1.000000000000000000, -0.000000000000000000 ) ) ;
#138280 = CARTESIAN_POINT ( 'NONE',  ( -20.85000000000000142, -1.149570369564537842, -74.81591248450196474 ) ) ;
#138279 = FACE_BOUND ( 'NONE', #53913, .T. ) ;
#138282 = EDGE_LOOP ( 'NONE', ( #128836, #168660, #229529, #253115 ) ) ;
#138281 = CARTESIAN_POINT ( 'NONE',  ( -16.94275863006528482, 9.989496048678669027, -54.39169738207657900 ) ) ;
#138283 = EDGE_CURVE ( 'NONE', #198318, #156630, #192206, .T. ) ;
#138284 = VERTEX_POINT ( 'NONE', #170103 ) ;
#138285 = EDGE_CURVE ( 'NONE', #14082, #59138, #88894, .T. ) ;
#138286 = CIRCLE ( 'NONE', #130108, 0.09999999999999864553 ) ;
#138287 = DIRECTION ( 'NONE',  ( 0.000000000000000000, -7.086529944415894657E-15, 1.000000000000000000 ) ) ;
#138288 = ORIENTED_EDGE ( 'NONE', *, *, #18008, .F. ) ;
#138289 = DIRECTION ( 'NONE',  ( -1.000000000000000000, -7.304098846218135653E-16, 4.607487905232624742E-31 ) ) ;
#138290 = ORIENTED_EDGE ( 'NONE', *, *, #128876, .T. ) ;
#138291 = CARTESIAN_POINT ( 'NONE',  ( -21.05000000000000071, 87.65000000001192859, -105.9231074845242091 ) ) ;
#138292 = ADVANCED_FACE ( 'NONE', ( #31858 ), #91804, .F. ) ;
#138293 = CARTESIAN_POINT ( 'NONE',  ( 22.39999999999999503, 29.54900078958455367, -252.7363208912387051 ) ) ;
#138294 = CARTESIAN_POINT ( 'NONE',  ( 20.94999999999999929, 5.850000000011160495, -157.3675027757221017 ) ) ;
#138295 = EDGE_LOOP ( 'NONE', ( #253454, #131316, #210945, #70542 ) ) ;
#138296 = CARTESIAN_POINT ( 'NONE',  ( 23.24999999999999289, 55.91711482281188950, -232.6830152854666949 ) ) ;
#138297 = ADVANCED_FACE ( 'NONE', ( #151801 ), #18182, .F. ) ;
#138298 = EDGE_CURVE ( 'NONE', #125903, #32954, #35734, .T. ) ;
#138299 = CARTESIAN_POINT ( 'NONE',  ( -16.80100914604134132, 9.943149094114719588, -54.31704412728765874 ) ) ;
#138300 = ADVANCED_FACE ( 'NONE', ( #193485 ), #117926, .F. ) ;
#138302 = ORIENTED_EDGE ( 'NONE', *, *, #245738, .F. ) ;
#138301 = AXIS2_PLACEMENT_3D ( 'NONE', #254263, #193039, #156508 ) ;
#138303 = ORIENTED_EDGE ( 'NONE', *, *, #90457, .T. ) ;
#138305 = ADVANCED_FACE ( 'NONE', ( #115214 ), #120391, .T. ) ;
#138304 = ADVANCED_FACE ( 'NONE', ( #74843 ), #228762, .T. ) ;
#138306 = ORIENTED_EDGE ( 'NONE', *, *, #55691, .T. ) ;
#138307 = CYLINDRICAL_SURFACE ( 'NONE', #162366, 12.87499999999999822 ) ;
#138308 = ORIENTED_EDGE ( 'NONE', *, *, #173834, .F. ) ;
#138310 = ORIENTED_EDGE ( 'NONE', *, *, #225997, .F. ) ;
#138309 = DIRECTION ( 'NONE',  ( 0.000000000000000000, -0.9893560106964500722, 0.1455152366551550613 ) ) ;
#138311 = EDGE_LOOP ( 'NONE', ( #63694, #72050, #2200, #162776 ) ) ;
#138314 = VERTEX_POINT ( 'NONE', #17402 ) ;
#138313 = VERTEX_POINT ( 'NONE', #55206 ) ;
#138312 = CARTESIAN_POINT ( 'NONE',  ( 19.75857864376268935, 11.75000000001115907, -192.3499999999999659 ) ) ;
#138315 = CIRCLE ( 'NONE', #96804, 12.97499999999998721 ) ;
#138316 = ORIENTED_EDGE ( 'NONE', *, *, #221842, .F. ) ;
#138317 = CARTESIAN_POINT ( 'NONE',  ( -21.05000000000000071, -1.162701749938009677, -8.099999999999999645 ) ) ;
#138318 = EDGE_CURVE ( 'NONE', #76854, #180750, #16146, .T. ) ;
#138319 = EDGE_CURVE ( 'NONE', #185475, #83116, #122239, .T. ) ;
#138320 = DIRECTION ( 'NONE',  ( 2.840903330521633255E-16, -0.8700118002898322711, 0.4930308989875231696 ) ) ;
#138321 = AXIS2_PLACEMENT_3D ( 'NONE', #234787, #40481, #56129 ) ;
#138322 = CARTESIAN_POINT ( 'NONE',  ( -16.79270642812277359, 14.15297681976097977, -219.2450585461133130 ) ) ;
#138323 = ORIENTED_EDGE ( 'NONE', *, *, #80351, .F. ) ;
#138324 = EDGE_CURVE ( 'NONE', #42728, #154893, #188119, .T. ) ;
#138325 = LINE ( 'NONE', #41847, #187148 ) ;
#138327 = ORIENTED_EDGE ( 'NONE', *, *, #133370, .T. ) ;
#138326 = DIRECTION ( 'NONE',  ( 0.000000000000000000, 0.000000000000000000, 1.000000000000000000 ) ) ;
#138328 = CARTESIAN_POINT ( 'NONE',  ( -18.59999999999999787, 38.29773864426885410, -236.0513742605307925 ) ) ;
#138330 = VERTEX_POINT ( 'NONE', #134755 ) ;
#138329 = CARTESIAN_POINT ( 'NONE',  ( -20.94999999999999929, 61.95000000001175522, -75.03680255528533394 ) ) ;
#138331 = VERTEX_POINT ( 'NONE', #136033 ) ;
#138333 = EDGE_CURVE ( 'NONE', #253941, #131341, #9793, .T. ) ;
#138332 = CARTESIAN_POINT ( 'NONE',  ( -20.85000000000000142, 14.86477715130881272, -235.7932433709592601 ) ) ;
#138334 =( NAMED_UNIT ( * ) PLANE_ANGLE_UNIT ( ) SI_UNIT ( $, .RADIAN. ) );
#138335 = CIRCLE ( 'NONE', #184148, 0.09999999999998898659 ) ;
#138336 = CIRCLE ( 'NONE', #5619, 12.87499999999999112 ) ;
#138337 = VERTEX_POINT ( 'NONE', #159494 ) ;
#138338 = EDGE_CURVE ( 'NONE', #211554, #31271, #19989, .T. ) ;
#138339 = ORIENTED_EDGE ( 'NONE', *, *, #42529, .F. ) ;
#138340 = CARTESIAN_POINT ( 'NONE',  ( 20.94999999999999929, -11.48912529306489994, -97.50000000000004263 ) ) ;
#138341 = DIRECTION ( 'NONE',  ( 9.044546369203337730E-15, 0.7397360091702647189, 0.6728971962616949742 ) ) ;
#138343 = ORIENTED_EDGE ( 'NONE', *, *, #252772, .F. ) ;
#138342 = ORIENTED_EDGE ( 'NONE', *, *, #207675, .F. ) ;
#138344 = ORIENTED_EDGE ( 'NONE', *, *, #216275, .T. ) ;
#138345 = CARTESIAN_POINT ( 'NONE',  ( 18.59999999999999432, 43.57568952063339651, -245.1784935019914826 ) ) ;
#138346 = ORIENTED_EDGE ( 'NONE', *, *, #68311, .T. ) ;
#138347 = ORIENTED_EDGE ( 'NONE', *, *, #52879, .F. ) ;
#138348 = CARTESIAN_POINT ( 'NONE',  ( 20.95083306685154056, 18.81202456654950339, -229.8754792376871023 ) ) ;
#138349 = ORIENTED_EDGE ( 'NONE', *, *, #136835, .T. ) ;
#138350 = EDGE_CURVE ( 'NONE', #212838, #61516, #109745, .T. ) ;
#138351 = FACE_OUTER_BOUND ( 'NONE', #240507, .T. ) ;
#138353 = CARTESIAN_POINT ( 'NONE',  ( 20.04999999999999716, 67.25000000001230660, -160.7731074845244166 ) ) ;
#138352 = CARTESIAN_POINT ( 'NONE',  ( 18.59999999999999076, 65.79142135624880439, -48.17310748452439384 ) ) ;
#138354 = VERTEX_POINT ( 'NONE', #236441 ) ;
#138355 = VECTOR ( 'NONE', #116158, 1000.000000000000114 ) ;
#138356 = TOROIDAL_SURFACE ( 'NONE', #196825, 0.2000000000000000111, 0.1000000000000000056 ) ;
#138358 = ORIENTED_EDGE ( 'NONE', *, *, #52296, .F. ) ;
#138357 = ORIENTED_EDGE ( 'NONE', *, *, #91740, .T. ) ;
#138359 = CIRCLE ( 'NONE', #242425, 12.97499999999998721 ) ;
#138360 = ADVANCED_FACE ( 'NONE', ( #57788 ), #156938, .T. ) ;
#138361 = CARTESIAN_POINT ( 'NONE',  ( 20.94999999999999574, -11.48912529307605901, -3.100000000000000533 ) ) ;
#138362 = CARTESIAN_POINT ( 'NONE',  ( -20.54999999999999716, 68.75000000001230660, -157.7731074845244166 ) ) ;
#138363 = VERTEX_POINT ( 'NONE', #214321 ) ;
#138364 = FACE_OUTER_BOUND ( 'NONE', #131658, .T. ) ;
#138365 = ORIENTED_EDGE ( 'NONE', *, *, #9650, .F. ) ;
#138366 = VERTEX_POINT ( 'NONE', #137328 ) ;
#138367 = CARTESIAN_POINT ( 'NONE',  ( -21.05000000000000071, 5.900000000011102586, -110.7190997646564483 ) ) ;
#138368 = ADVANCED_FACE ( 'NONE', ( #99476 ), #138755, .F. ) ;
#138369 = ORIENTED_EDGE ( 'NONE', *, *, #118732, .T. ) ;
#138370 = CARTESIAN_POINT ( 'NONE',  ( -20.85000000000000142, -1.835859311432481045, -145.5044391687985694 ) ) ;
#138371 = CARTESIAN_POINT ( 'NONE',  ( -17.80356949364322716, 32.72696218579464045, -235.1059619251321067 ) ) ;
#138372 = ORIENTED_EDGE ( 'NONE', *, *, #118889, .F. ) ;
#138373 = DIRECTION ( 'NONE',  ( 0.000000000000000000, -6.467318590049456648E-15, 1.000000000000000000 ) ) ;
#138374 = CARTESIAN_POINT ( 'NONE',  ( -17.80356949363890706, 10.87673139701253788, -43.78692697577277215 ) ) ;
#138375 = AXIS2_PLACEMENT_3D ( 'NONE', #138513, #218058, #118998 ) ;
#138377 = CARTESIAN_POINT ( 'NONE',  ( -16.97683809663752186, 9.950000000011137047, -120.5976359818037196 ) ) ;
#138376 = FACE_OUTER_BOUND ( 'NONE', #163649, .T. ) ;
#138378 = DIRECTION ( 'NONE',  ( 0.000000000000000000, -1.000000000000000000, 0.000000000000000000 ) ) ;
#138379 = DIRECTION ( 'NONE',  ( 2.940209281316622002E-16, 0.9651348961777150848, -0.2617529984165055112 ) ) ;
#138380 = DIRECTION ( 'NONE',  ( 1.000000000000000000, -0.000000000000000000, 0.000000000000000000 ) ) ;
#138381 = CARTESIAN_POINT ( 'NONE',  ( 18.58685178364169843, -9.406733083793096029, -74.12442046908778082 ) ) ;
#138382 = CYLINDRICAL_SURFACE ( 'NONE', #47380, 0.1000000000000028644 ) ;
#138383 = ORIENTED_EDGE ( 'NONE', *, *, #149767, .T. ) ;
#138384 = CIRCLE ( 'NONE', #71967, 0.1000000000000028644 ) ;
#138386 = ORIENTED_EDGE ( 'NONE', *, *, #78510, .F. ) ;
#138385 = ORIENTED_EDGE ( 'NONE', *, *, #227286, .T. ) ;
#138387 = ORIENTED_EDGE ( 'NONE', *, *, #49809, .T. ) ;
#138388 = ORIENTED_EDGE ( 'NONE', *, *, #28824, .T. ) ;
#138389 = CARTESIAN_POINT ( 'NONE',  ( 18.59999999999999432, -1.162701749926853712, -75.10000000000003695 ) ) ;
#138391 = DIRECTION ( 'NONE',  ( -2.952720810173289605E-16, -1.000000000000000000, -7.086529944415894657E-15 ) ) ;
#138390 = CARTESIAN_POINT ( 'NONE',  ( -21.05000000000000071, 76.00000000001190870, -103.0231074845243029 ) ) ;
#138392 = ORIENTED_EDGE ( 'NONE', *, *, #202058, .F. ) ;
#138393 = AXIS2_PLACEMENT_3D ( 'NONE', #46417, #25596, #185940 ) ;
#138394 = CARTESIAN_POINT ( 'NONE',  ( -20.87600722750343252, 10.33112638556969465, -106.0901228926975080 ) ) ;
#138395 = DIRECTION ( 'NONE',  ( 1.000000000000000000, -1.186688945009009831E-16, -8.286604613020806758E-31 ) ) ;
#138396 = AXIS2_PLACEMENT_3D ( 'NONE', #212417, #191585, #110728 ) ;
#138397 = CARTESIAN_POINT ( 'NONE',  ( 18.49999999999999645, 47.89822068137787170, -246.3100470504847692 ) ) ;
#138398 = CIRCLE ( 'NONE', #844, 0.5000000000000051070 ) ;
#138399 = VECTOR ( 'NONE', #131, 1000.000000000000000 ) ;
#138400 = CARTESIAN_POINT ( 'NONE',  ( 18.42636655943171320, -9.496944315759476396, -73.60908057115553049 ) ) ;
#138401 = ORIENTED_EDGE ( 'NONE', *, *, #28189, .T. ) ;
#138402 = AXIS2_PLACEMENT_3D ( 'NONE', #202968, #7338, #4743 ) ;
#138403 = FACE_OUTER_BOUND ( 'NONE', #213614, .T. ) ;
#138404 = AXIS2_PLACEMENT_3D ( 'NONE', #229379, #32488, #15472 ) ;
#138405 = DIRECTION ( 'NONE',  ( 1.000000000000000000, 0.000000000000000000, 0.000000000000000000 ) ) ;
#138406 = ORIENTED_EDGE ( 'NONE', *, *, #185636, .T. ) ;
#138407 = DIRECTION ( 'NONE',  ( 2.659396599871503240E-15, 0.7672646620070624479, -0.6413305999523086776 ) ) ;
#138408 = LINE ( 'NONE', #115026, #144495 ) ;
#138409 = LINE ( 'NONE', #100560, #1929 ) ;
#138410 = CARTESIAN_POINT ( 'NONE',  ( -21.05000000000000071, 69.60000000001261355, -193.5926828544628222 ) ) ;
#138412 = AXIS2_PLACEMENT_3D ( 'NONE', #19135, #256395, #16594 ) ;
#138411 = DIRECTION ( 'NONE',  ( -1.000000000000000000, 0.000000000000000000, -0.000000000000000000 ) ) ;
#138413 = ORIENTED_EDGE ( 'NONE', *, *, #63548, .F. ) ;
#138414 = CARTESIAN_POINT ( 'NONE',  ( 18.49505832270840244, 47.08691893723204913, -255.2213761142054125 ) ) ;
#138415 = CARTESIAN_POINT ( 'NONE',  ( 21.05000000000000071, 0.5450571430110628945, -208.9664790259058691 ) ) ;
#138416 = FACE_OUTER_BOUND ( 'NONE', #63335, .T. ) ;
#138417 = AXIS2_PLACEMENT_3D ( 'NONE', #4100, #103181, #185309 ) ;
#138419 = CARTESIAN_POINT ( 'NONE',  ( -21.64999999999999858, 7.350000000011155166, -155.1500000000000057 ) ) ;
#138418 = DIRECTION ( 'NONE',  ( 0.000000000000000000, 0.000000000000000000, 1.000000000000000000 ) ) ;
#138421 = EDGE_CURVE ( 'NONE', #152525, #229077, #179076, .T. ) ;
#138420 = DIRECTION ( 'NONE',  ( -2.915501640297154283E-16, 1.000000000000000000, 0.000000000000000000 ) ) ;
#138422 = CARTESIAN_POINT ( 'NONE',  ( -21.64999999999999858, 51.48671849539696410, -231.8960919591225718 ) ) ;
#138423 = CIRCLE ( 'NONE', #121898, 11.70000000000000817 ) ;
#138424 = DIRECTION ( 'NONE',  ( 1.000000000000000000, 0.000000000000000000, 0.000000000000000000 ) ) ;
#138425 = DIRECTION ( 'NONE',  ( 0.000000000000000000, 0.2617529984165031243, 0.9651348961777157509 ) ) ;
#138426 = AXIS2_PLACEMENT_3D ( 'NONE', #156454, #39054, #36496 ) ;
#138427 = ORIENTED_EDGE ( 'NONE', *, *, #117001, .T. ) ;
#138428 = AXIS2_PLACEMENT_3D ( 'NONE', #2967, #180341, #181634 ) ;
#138429 = AXIS2_PLACEMENT_3D ( 'NONE', #68591, #90703, #133689 ) ;
#138430 = VERTEX_POINT ( 'NONE', #98179 ) ;
#138431 = CARTESIAN_POINT ( 'NONE',  ( -18.39999999999999858, 64.25000000001190870, -93.77310748452438816 ) ) ;
#138432 = VERTEX_POINT ( 'NONE', #237732 ) ;
#138433 = ADVANCED_FACE ( 'NONE', ( #59057 ), #121658, .F. ) ;
#138434 = AXIS2_PLACEMENT_3D ( 'NONE', #149333, #170211, #153198 ) ;
#138435 = DIRECTION ( 'NONE',  ( 1.000000000000000000, 0.000000000000000000, 0.000000000000000000 ) ) ;
#138436 = ADVANCED_FACE ( 'NONE', ( #2957 ), #181625, .F. ) ;
#138437 = DIRECTION ( 'NONE',  ( 1.000000000000000000, 0.000000000000000000, 0.000000000000000000 ) ) ;
#138438 = ORIENTED_EDGE ( 'NONE', *, *, #238528, .T. ) ;
#138440 = FACE_OUTER_BOUND ( 'NONE', #115829, .T. ) ;
#138439 = AXIS2_PLACEMENT_3D ( 'NONE', #114085, #154545, #171538 ) ;
#138441 = DIRECTION ( 'NONE',  ( 0.000000000000000000, 1.000000000000000000, 0.000000000000000000 ) ) ;
#138442 = FACE_OUTER_BOUND ( 'NONE', #55703, .T. ) ;
#138443 = EDGE_CURVE ( 'NONE', #153892, #9803, #22551, .T. ) ;
#138444 = EDGE_CURVE ( 'NONE', #129669, #221938, #184165, .T. ) ;
#138445 = CARTESIAN_POINT ( 'NONE',  ( 20.94999999999999929, 64.11611521369653133, -222.3177418886732539 ) ) ;
#138447 = ORIENTED_EDGE ( 'NONE', *, *, #174886, .T. ) ;
#138446 = CARTESIAN_POINT ( 'NONE',  ( 21.05000000000000071, 11.75000000001116263, -160.4851942293460638 ) ) ;
#138449 = FACE_OUTER_BOUND ( 'NONE', #148231, .T. ) ;
#138448 = DIRECTION ( 'NONE',  ( 0.000000000000000000, -0.8814952561688444987, 0.4721928772777320149 ) ) ;
#138450 = DIRECTION ( 'NONE',  ( 1.875376730785737719E-16, -1.000000000000000000, 0.000000000000000000 ) ) ;
#138451 =( BOUNDED_CURVE ( )  B_SPLINE_CURVE ( 3, ( #218306, #59213, #18843, #177938 ),
 .UNSPECIFIED., .F., .F. ) 
 B_SPLINE_CURVE_WITH_KNOTS ( ( 4, 4 ),
 ( 0.000000000000000000, 1.570796326794908992 ),
 .UNSPECIFIED. ) 
 CURVE ( )  GEOMETRIC_REPRESENTATION_ITEM ( )  RATIONAL_B_SPLINE_CURVE ( ( 1.000000000000000000, 0.8047378541243619399, 0.8047378541243619399, 1.000000000000000000 ) ) 
 REPRESENTATION_ITEM ( '' )  );
#138452 = DIRECTION ( 'NONE',  ( -1.000000000000000000, 0.000000000000000000, 0.000000000000000000 ) ) ;
#138454 = EDGE_CURVE ( 'NONE', #23498, #4036, #10377, .T. ) ;
#138453 = CARTESIAN_POINT ( 'NONE',  ( -18.59999999999999787, 74.73821383144705521, -128.4366085209788366 ) ) ;
#138455 = FILL_AREA_STYLE ('',( #242707 ) ) ;
#138456 = ORIENTED_EDGE ( 'NONE', *, *, #204406, .F. ) ;
#138457 = DIRECTION ( 'NONE',  ( 0.000000000000000000, 0.000000000000000000, 1.000000000000000000 ) ) ;
#138458 = DIRECTION ( 'NONE',  ( 0.000000000000000000, -6.982962677686266711E-15, 1.000000000000000000 ) ) ;
#138459 = EDGE_CURVE ( 'NONE', #66990, #43171, #213817, .T. ) ;
#138460 = ORIENTED_EDGE ( 'NONE', *, *, #99131, .T. ) ;
#138461 = PLANE ( 'NONE',  #252708 ) ;
#138462 = AXIS2_PLACEMENT_3D ( 'NONE', #115649, #224986, #187194 ) ;
#138463 = ORIENTED_EDGE ( 'NONE', *, *, #139749, .T. ) ;
#138464 = CARTESIAN_POINT ( 'NONE',  ( 18.59999999999999076, 1.115600667400684642E-11, -100.5000000000000426 ) ) ;
#138465 = EDGE_CURVE ( 'NONE', #85964, #128522, #240309, .T. ) ;
#138466 = AXIS2_PLACEMENT_3D ( 'NONE', #28894, #150098, #247887 ) ;
#138467 = CARTESIAN_POINT ( 'NONE',  ( -13.40000000000000213, -11.75000000000000000, 15.00000000000000355 ) ) ;
#138468 = DIRECTION ( 'NONE',  ( 0.000000000000000000, 0.000000000000000000, -1.000000000000000000 ) ) ;
#138469 = ORIENTED_EDGE ( 'NONE', *, *, #134047, .T. ) ;
#138470 = EDGE_LOOP ( 'NONE', ( #246384, #60022, #165310, #140152 ) ) ;
#138471 = EDGE_CURVE ( 'NONE', #132077, #257696, #82474, .T. ) ;
#138472 = LINE ( 'NONE', #133373, #69467 ) ;
#138473 = CARTESIAN_POINT ( 'NONE',  ( 21.05000000000000071, -11.74999999999999112, -30.59999999999999432 ) ) ;
#138474 = CARTESIAN_POINT ( 'NONE',  ( -16.87333278164134853, 63.02430237963940840, -213.6115832883065195 ) ) ;
#138475 = DIRECTION ( 'NONE',  ( -1.000000000000000000, 0.000000000000000000, 0.000000000000000000 ) ) ;
#138477 = CARTESIAN_POINT ( 'NONE',  ( -22.39999999999999858, 7.790779598384560245, -133.9000000000000057 ) ) ;
#138476 = CARTESIAN_POINT ( 'NONE',  ( -22.47007471830798409, 76.00000000001219291, -144.2438181364507841 ) ) ;
#138478 = CARTESIAN_POINT ( 'NONE',  ( -18.34804628011471195, 58.57934086597928314, -223.9244941873114101 ) ) ;
#138479 = DIRECTION ( 'NONE',  ( -1.000000000000000000, -0.000000000000000000, -0.000000000000000000 ) ) ;
#138480 = CARTESIAN_POINT ( 'NONE',  ( 22.45380639572249137, 75.99999985734274333, -148.2735403756364008 ) ) ;
#138481 = ORIENTED_EDGE ( 'NONE', *, *, #220093, .F. ) ;
#138482 = LINE ( 'NONE', #197195, #185633 ) ;
#138483 = CIRCLE ( 'NONE', #217594, 0.09999999999999542588 ) ;
#138485 = ORIENTED_EDGE ( 'NONE', *, *, #98559, .F. ) ;
#138484 = CARTESIAN_POINT ( 'NONE',  ( -18.59999999999999787, 66.65000000001205649, -124.3731074845243683 ) ) ;
#138486 = CARTESIAN_POINT ( 'NONE',  ( 20.04142135623730070, 52.81534179157633702, -244.1198638051726277 ) ) ;
#138487 = CARTESIAN_POINT ( 'NONE',  ( 23.24999999999999645, 1.115600667400684642E-11, -134.0000000000000284 ) ) ;
#138489 = CARTESIAN_POINT ( 'NONE',  ( 21.05000000000000071, 1.115600667400684642E-11, -33.50000000000000000 ) ) ;
#138488 = DIRECTION ( 'NONE',  ( 0.000000000000000000, -6.982962677686266711E-15, 1.000000000000000000 ) ) ;
#138490 = ORIENTED_EDGE ( 'NONE', *, *, #198361, .T. ) ;
#138492 = DIRECTION ( 'NONE',  ( -1.000000000000000000, 0.000000000000000000, 0.000000000000000000 ) ) ;
#138491 = CARTESIAN_POINT ( 'NONE',  ( -16.80070461187911590, 66.05000000001234639, -56.87614365536322936 ) ) ;
#138493 = LINE ( 'NONE', #255855, #199556 ) ;
#138494 = CARTESIAN_POINT ( 'NONE',  ( -20.54999999999999716, -11.74999999998884448, -54.65000000000000568 ) ) ;
#138495 = DIRECTION ( 'NONE',  ( 1.000000000000000000, 0.000000000000000000, 0.000000000000000000 ) ) ;
#138496 = CARTESIAN_POINT ( 'NONE',  ( -18.50000000000000000, 77.83534155023646406, -124.9679561919613064 ) ) ;
#138497 = EDGE_LOOP ( 'NONE', ( #41203, #221214 ) ) ;
#138498 = LINE ( 'NONE', #141107, #142963 ) ;
#138499 = ORIENTED_EDGE ( 'NONE', *, *, #209354, .F. ) ;
#138501 = AXIS2_PLACEMENT_3D ( 'NONE', #13750, #112850, #194976 ) ;
#138500 = DIRECTION ( 'NONE',  ( 1.000000000000000000, 0.000000000000000000, 0.000000000000000000 ) ) ;
#138502 = VERTEX_POINT ( 'NONE', #23849 ) ;
#138503 = CARTESIAN_POINT ( 'NONE',  ( -20.94999999999999929, 46.33035574435032089, -243.0552603638194853 ) ) ;
#138504 = ORIENTED_EDGE ( 'NONE', *, *, #155348, .F. ) ;
#138505 = AXIS2_PLACEMENT_3D ( 'NONE', #45575, #125127, #63853 ) ;
#138506 = EDGE_CURVE ( 'NONE', #44045, #243775, #102045, .T. ) ;
#138507 = CARTESIAN_POINT ( 'NONE',  ( 20.94999999999999574, -1.835341550213255957, -179.0551512925629538 ) ) ;
#138508 = AXIS2_PLACEMENT_3D ( 'NONE', #251319, #229215, #89674 ) ;
#138509 = DIRECTION ( 'NONE',  ( -1.000000000000000000, -0.000000000000000000, -0.000000000000000000 ) ) ;
#138510 = EDGE_LOOP ( 'NONE', ( #64669, #128195, #179463, #5951 ) ) ;
#138511 = EDGE_CURVE ( 'NONE', #207660, #190676, #25125, .T. ) ;
#138512 = EDGE_CURVE ( 'NONE', #148974, #176630, #160796, .T. ) ;
#138513 = CARTESIAN_POINT ( 'NONE',  ( -18.59999999999999787, 43.57568952063339651, -245.1784935019914826 ) ) ;
#138514 = PLANE ( 'NONE',  #99006 ) ;
#138515 = ADVANCED_FACE ( 'NONE', ( #104601 ), #34776, .F. ) ;
#138516 = DIRECTION ( 'NONE',  ( 1.000000000000000000, 0.000000000000000000, -0.000000000000000000 ) ) ;
#138517 = AXIS2_PLACEMENT_3D ( 'NONE', #92446, #187732, #89879 ) ;
#138518 = ADVANCED_FACE ( 'NONE', ( #149893 ), #61662, .T. ) ;
#138519 = CARTESIAN_POINT ( 'NONE',  ( -23.25000000000000000, 86.52890073500824997, -209.5906233940697234 ) ) ;
#138520 = CARTESIAN_POINT ( 'NONE',  ( 23.24999999999999289, 71.85000000001268461, -203.5231074845243597 ) ) ;
#138521 = CARTESIAN_POINT ( 'NONE',  ( 23.14999999999999858, 53.86595165227826243, -236.3638196928718855 ) ) ;
#138522 = EDGE_CURVE ( 'NONE', #252227, #45216, #182910, .T. ) ;
#138523 = ORIENTED_EDGE ( 'NONE', *, *, #184480, .T. ) ;
#138525 = EDGE_CURVE ( 'NONE', #22291, #43175, #201168, .T. ) ;
#138524 = DIRECTION ( 'NONE',  ( 1.000000000000000000, 1.836970198721029934E-16, 0.000000000000000000 ) ) ;
#138526 = ORIENTED_EDGE ( 'NONE', *, *, #47410, .T. ) ;
#138528 = ORIENTED_EDGE ( 'NONE', *, *, #202750, .T. ) ;
#138527 = LINE ( 'NONE', #201097, #148184 ) ;
#138529 = VERTEX_POINT ( 'NONE', #221988 ) ;
#138530 = CARTESIAN_POINT ( 'NONE',  ( -20.90000000000000213, -1.300000000000000044, -7.900000000000000355 ) ) ;
#138531 = CARTESIAN_POINT ( 'NONE',  ( 13.88302573338719981, 66.54258905524520173, -188.5230235107344470 ) ) ;
#138532 = DIRECTION ( 'NONE',  ( 0.000000000000000000, -1.000000000000000000, -6.860497997771531562E-15 ) ) ;
#138533 = EDGE_CURVE ( 'NONE', #46490, #90293, #147170, .T. ) ;
#138534 = AXIS2_PLACEMENT_3D ( 'NONE', #89838, #91134, #254046 ) ;
#138535 = CARTESIAN_POINT ( 'NONE',  ( 20.12500000000000000, 9.750000000011153745, -75.11177128211431864 ) ) ;
#138536 = ORIENTED_EDGE ( 'NONE', *, *, #108446, .T. ) ;
#138537 = CARTESIAN_POINT ( 'NONE',  ( 22.50000000000000000, 64.35042919246716053, -103.1231074845243825 ) ) ;
#138538 = FACE_OUTER_BOUND ( 'NONE', #168657, .T. ) ;
#138539 = ORIENTED_EDGE ( 'NONE', *, *, #108273, .F. ) ;
#138540 = AXIS2_PLACEMENT_3D ( 'NONE', #7310, #125969, #205504 ) ;
#138542 = EDGE_LOOP ( 'NONE', ( #211414, #197506, #197219, #131937 ) ) ;
#138541 = CARTESIAN_POINT ( 'NONE',  ( 18.49999999999998934, 6.550000000011156231, -110.5170271704400591 ) ) ;
#138543 = VECTOR ( 'NONE', #141795, 1000.000000000000000 ) ;
#138544 = AXIS2_PLACEMENT_3D ( 'NONE', #71854, #211351, #230930 ) ;
#138545 = AXIS2_PLACEMENT_3D ( 'NONE', #248732, #90927, #147042 ) ;
#138546 = DIRECTION ( 'NONE',  ( 0.000000000000000000, -1.000000000000000000, 0.000000000000000000 ) ) ;
#138547 = ORIENTED_EDGE ( 'NONE', *, *, #65652, .F. ) ;
#138548 = EDGE_CURVE ( 'NONE', #173035, #102738, #4236, .T. ) ;
#138549 = CARTESIAN_POINT ( 'NONE',  ( 20.94560253601876809, 64.25000000001195133, -110.0130239720089094 ) ) ;
#138550 = VERTEX_POINT ( 'NONE', #168197 ) ;
#138551 = CARTESIAN_POINT ( 'NONE',  ( -21.65000000000000213, 68.75000000001226397, -149.1731074845244223 ) ) ;
#138552 = EDGE_CURVE ( 'NONE', #85197, #205292, #155596, .T. ) ;
#138553 = FACE_OUTER_BOUND ( 'NONE', #70316, .T. ) ;
#138554 = CARTESIAN_POINT ( 'NONE',  ( 15.74999999999999645, 66.65000000001155911, -52.77310748452439526 ) ) ;
#138555 = EDGE_CURVE ( 'NONE', #142940, #206366, #247106, .T. ) ;
#138556 = CARTESIAN_POINT ( 'NONE',  ( -21.59142135623730852, 7.850000000011158718, -188.7499999999999716 ) ) ;
#138557 = ORIENTED_EDGE ( 'NONE', *, *, #113268, .F. ) ;
#138558 = DIRECTION ( 'NONE',  ( -1.000000000000000000, 0.000000000000000000, 0.000000000000000000 ) ) ;
#138559 = ORIENTED_EDGE ( 'NONE', *, *, #112946, .T. ) ;
#138560 = CARTESIAN_POINT ( 'NONE',  ( -17.78043020864321377, 12.80471010483343619, -208.7905335770795716 ) ) ;
#138561 = CARTESIAN_POINT ( 'NONE',  ( 20.94999999999999929, 5.900000000011162093, -123.7809002353436654 ) ) ;
#138562 = AXIS2_PLACEMENT_3D ( 'NONE', #57854, #14919, #171448 ) ;
#138564 = EDGE_LOOP ( 'NONE', ( #8168, #12788, #173336, #250883 ) ) ;
#138563 = DIRECTION ( 'NONE',  ( -1.000000000000000000, -0.000000000000000000, -0.000000000000000000 ) ) ;
#138565 = CARTESIAN_POINT ( 'NONE',  ( -20.54999999999999716, 1.115600667400684642E-11, -167.4999999999999716 ) ) ;
#138566 = DIRECTION ( 'NONE',  ( 0.000000000000000000, 0.000000000000000000, -1.000000000000000000 ) ) ;
#138567 = CARTESIAN_POINT ( 'NONE',  ( -0.8999999999999437339, 64.35000000001120668, -12.62310748452478926 ) ) ;
#138568 = CARTESIAN_POINT ( 'NONE',  ( 23.15000000000000213, 85.60000000001220144, -146.4170766071767389 ) ) ;
#138569 = CARTESIAN_POINT ( 'NONE',  ( -16.87331047859651179, 9.950000000011142376, -180.1499999999999773 ) ) ;
#138570 = AXIS2_PLACEMENT_3D ( 'NONE', #177943, #224431, #257403 ) ;
#138571 = DIRECTION ( 'NONE',  ( 1.000000000000000000, 0.000000000000000000, 0.000000000000000000 ) ) ;
#138572 = DIRECTION ( 'NONE',  ( 1.000000000000000000, 0.000000000000000000, 0.000000000000000000 ) ) ;
#138574 = ORIENTED_EDGE ( 'NONE', *, *, #199990, .T. ) ;
#138573 = DIRECTION ( 'NONE',  ( 0.000000000000000000, 0.000000000000000000, 1.000000000000000000 ) ) ;
#138575 = AXIS2_PLACEMENT_3D ( 'NONE', #19329, #238365, #55855 ) ;
#138576 = AXIS2_PLACEMENT_3D ( 'NONE', #130325, #72968, #194186 ) ;
#138577 = VECTOR ( 'NONE', #78931, 999.9999999999998863 ) ;
#138578 = FACE_BOUND ( 'NONE', #106241, .T. ) ;
#138579 = ORIENTED_EDGE ( 'NONE', *, *, #125693, .F. ) ;
#138580 = ORIENTED_EDGE ( 'NONE', *, *, #9516, .F. ) ;
#138581 = CARTESIAN_POINT ( 'NONE',  ( -18.79999999999999716, 1.885425182446133885, -11.49641995933507843 ) ) ;
#138582 = CARTESIAN_POINT ( 'NONE',  ( -18.46093223321778609, 85.48068296828714097, -196.4385569705976025 ) ) ;
#138583 = AXIS2_PLACEMENT_3D ( 'NONE', #85180, #163477, #243001 ) ;
#138584 = VERTEX_POINT ( 'NONE', #172042 ) ;
#138585 = CARTESIAN_POINT ( 'NONE',  ( -20.64999999999999858, 2.000000000011154189, -187.7753780772378889 ) ) ;
#138586 = EDGE_CURVE ( 'NONE', #206051, #147657, #76742, .T. ) ;
#138587 = CARTESIAN_POINT ( 'NONE',  ( -18.59999999999999787, 64.35000000001161879, -62.50830171387040934 ) ) ;
#138588 = AXIS2_PLACEMENT_3D ( 'NONE', #106240, #206651, #127108 ) ;
#138589 = EDGE_CURVE ( 'NONE', #64043, #74308, #30672, .T. ) ;
#138590 = VERTEX_POINT ( 'NONE', #151167 ) ;
#138591 = CARTESIAN_POINT ( 'NONE',  ( -21.05000000000000071, 1.148907358139439339E-11, -201.0000000000015064 ) ) ;
#138592 = AXIS2_PLACEMENT_3D ( 'NONE', #195771, #138309, #101741 ) ;
#138593 = TOROIDAL_SURFACE ( 'NONE', #134342, 11.65000000000000036, 0.1000000000000000056 ) ;
#138595 = AXIS2_PLACEMENT_3D ( 'NONE', #13239, #212719, #133173 ) ;
#138594 = DIRECTION ( 'NONE',  ( 0.000000000000000000, -1.000000000000000000, -6.982962677686267499E-15 ) ) ;
#138596 = EDGE_CURVE ( 'NONE', #208096, #128297, #209721, .T. ) ;
#138597 = EDGE_LOOP ( 'NONE', ( #24798, #174207, #79744, #21369, #79818 ) ) ;
#138598 = AXIS2_PLACEMENT_3D ( 'NONE', #154255, #175106, #214185 ) ;
#138600 = EDGE_CURVE ( 'NONE', #167228, #130891, #14103, .T. ) ;
#138599 = DIRECTION ( 'NONE',  ( 1.000000000000000000, -0.000000000000000000, -0.000000000000000000 ) ) ;
#138601 = VERTEX_POINT ( 'NONE', #212428 ) ;
#138602 = DIRECTION ( 'NONE',  ( 1.000000000000000000, 0.000000000000000000, 0.000000000000000000 ) ) ;
#138604 = ORIENTED_EDGE ( 'NONE', *, *, #131669, .F. ) ;
#138603 = FACE_OUTER_BOUND ( 'NONE', #9537, .T. ) ;
#138605 = DIRECTION ( 'NONE',  ( 1.000000000000000000, 0.000000000000000000, 0.000000000000000000 ) ) ;
#138606 = ORIENTED_EDGE ( 'NONE', *, *, #111114, .T. ) ;
#138607 = CARTESIAN_POINT ( 'NONE',  ( 20.94999999999999929, -11.48912529307605546, -30.59999999999999432 ) ) ;
#138608 = ORIENTED_EDGE ( 'NONE', *, *, #238626, .T. ) ;
#138610 = ORIENTED_EDGE ( 'NONE', *, *, #250962, .T. ) ;
#138609 = VERTEX_POINT ( 'NONE', #192860 ) ;
#138611 = DIRECTION ( 'NONE',  ( -0.000000000000000000, -0.1350103645451718737, 0.9908441862701622416 ) ) ;
#138612 = ORIENTED_EDGE ( 'NONE', *, *, #43939, .F. ) ;
#138613 = CARTESIAN_POINT ( 'NONE',  ( 20.94999999999999574, 77.85102823015316176, -158.3691942151018566 ) ) ;
#138615 = EDGE_LOOP ( 'NONE', ( #144109, #133886, #163568, #209963, #209535, #226745, #163740, #178429, #131326, #215178, #207636, #132564 ) ) ;
#138614 = AXIS2_PLACEMENT_3D ( 'NONE', #226818, #70353, #109426 ) ;
#138616 = AXIS2_PLACEMENT_3D ( 'NONE', #26998, #143044, #43964 ) ;
#138617 = ADVANCED_FACE ( 'NONE', ( #194154 ), #143258, .T. ) ;
#138618 = CIRCLE ( 'NONE', #163602, 0.5999999999999998668 ) ;
#138619 = EDGE_CURVE ( 'NONE', #72909, #85365, #238955, .T. ) ;
#138620 = ORIENTED_EDGE ( 'NONE', *, *, #243569, .T. ) ;
#138621 = DIRECTION ( 'NONE',  ( -1.000000000000000000, -5.840638543281469327E-15, 6.917008051451466668E-14 ) ) ;
#138622 = CARTESIAN_POINT ( 'NONE',  ( -21.05000000000000071, 1.835341550235567887, -45.05515129256298223 ) ) ;
#138624 = ORIENTED_EDGE ( 'NONE', *, *, #112856, .T. ) ;
#138623 = LINE ( 'NONE', #124248, #24183 ) ;
#138625 = PLANE ( 'NONE',  #173020 ) ;
#138626 = EDGE_LOOP ( 'NONE', ( #180775, #181015, #70516, #18623 ) ) ;
#138627 = CYLINDRICAL_SURFACE ( 'NONE', #161905, 0.4999999999999944489 ) ;
#138628 = CARTESIAN_POINT ( 'NONE',  ( 23.25000000000000000, -11.64999999998883595, -130.9000000000000341 ) ) ;
#138629 = CARTESIAN_POINT ( 'NONE',  ( 21.05000000000000071, 64.25000000001249134, -177.0379132551784096 ) ) ;
#138630 = ORIENTED_EDGE ( 'NONE', *, *, #15503, .T. ) ;
#138631 = CARTESIAN_POINT ( 'NONE',  ( 20.94999999999999929, 10.29270135741298731, -72.45736188715193293 ) ) ;
#138632 = EDGE_CURVE ( 'NONE', #116862, #82909, #134848, .T. ) ;
#138633 = CARTESIAN_POINT ( 'NONE',  ( 20.94999999999999929, 6.650000000011155876, -146.1500000000000341 ) ) ;
#138634 = ORIENTED_EDGE ( 'NONE', *, *, #117263, .F. ) ;
#138635 = EDGE_CURVE ( 'NONE', #178504, #198869, #251529, .T. ) ;
#138637 = CARTESIAN_POINT ( 'NONE',  ( 23.14999999999999503, 64.35000000001156195, -57.37310748452439668 ) ) ;
#138636 = CIRCLE ( 'NONE', #125630, 0.1000000000000014766 ) ;
#138638 = ORIENTED_EDGE ( 'NONE', *, *, #140386, .T. ) ;
#138639 = ORIENTED_EDGE ( 'NONE', *, *, #88445, .F. ) ;
#138640 = DIRECTION ( 'NONE',  ( 0.000000000000000000, -0.9274965247785555977, 0.3738317757009190223 ) ) ;
#138641 = ORIENTED_EDGE ( 'NONE', *, *, #106157, .T. ) ;
#138642 = CIRCLE ( 'NONE', #122120, 0.1000000000000028644 ) ;
#138643 = ORIENTED_EDGE ( 'NONE', *, *, #124385, .F. ) ;
#138644 = CARTESIAN_POINT ( 'NONE',  ( -18.35663730107557257, 11.47390742652235573, -42.75000000000000000 ) ) ;
#138645 = DIRECTION ( 'NONE',  ( 0.000000000000000000, -6.608470384673536824E-15, 1.000000000000000000 ) ) ;
#138646 = ORIENTED_EDGE ( 'NONE', *, *, #108525, .T. ) ;
#138647 = ORIENTED_EDGE ( 'NONE', *, *, #152465, .T. ) ;
#138648 = EDGE_CURVE ( 'NONE', #205763, #46223, #26574, .T. ) ;
#138649 = CARTESIAN_POINT ( 'NONE',  ( -23.25000000000000000, 1.115600667400684642E-11, -167.4999999999999716 ) ) ;
#138650 = CARTESIAN_POINT ( 'NONE',  ( 21.14999999999999858, 0.02128009953412425548, -201.0977095561580370 ) ) ;
#138651 = ADVANCED_FACE ( 'NONE', ( #32531 ), #54610, .T. ) ;
#138652 = B_SPLINE_CURVE_WITH_KNOTS ( 'NONE', 3,
 ( #58270, #239504, #195262, #81663, #139071, #178268, #255148, #41323, #56977, #120864, #197790, #76563, #136521, #200373, #141669, #21745, #156139, #257712, #235631 ),
 .UNSPECIFIED., .F., .F.,
 ( 4, 3, 3, 3, 3, 3, 4 ),
 ( 0.0001624081864585767763, 0.0001685232196531791216, 0.0001764526673566963095, 0.0001916878551483256420, 0.0002009890782182563310, 0.0002238845907555157540, 0.0002283406619926372746 ),
 .UNSPECIFIED. ) ;
#138653 = VERTEX_POINT ( 'NONE', #16798 ) ;
#138654 = ORIENTED_EDGE ( 'NONE', *, *, #21294, .F. ) ;
#138655 = ADVANCED_FACE ( 'NONE', ( #255331 ), #15521, .F. ) ;
#138656 = ORIENTED_EDGE ( 'NONE', *, *, #74477, .T. ) ;
#138657 = AXIS2_PLACEMENT_3D ( 'NONE', #104511, #180243, #185363 ) ;
#138658 = DIRECTION ( 'NONE',  ( 0.000000000000000000, 1.000000000000000000, 6.352154140967427193E-15 ) ) ;
#138659 = EDGE_CURVE ( 'NONE', #129923, #211815, #72937, .T. ) ;
#138660 = LINE ( 'NONE', #43452, #76222 ) ;
#138661 = CARTESIAN_POINT ( 'NONE',  ( -20.54999999999999716, 66.36210077474692071, -222.8232602954134336 ) ) ;
#138662 = CARTESIAN_POINT ( 'NONE',  ( 20.95595012432474391, 65.39582078693598532, -162.4273381543061703 ) ) ;
#138663 = DIRECTION ( 'NONE',  ( 0.000000000000000000, -1.000000000000000000, 2.775557561562884094E-14 ) ) ;
#138664 = DIRECTION ( 'NONE',  ( -1.000000000000000000, 0.000000000000000000, 0.000000000000000000 ) ) ;
#138665 = EDGE_CURVE ( 'NONE', #109797, #90507, #51647, .T. ) ;
#138667 = CARTESIAN_POINT ( 'NONE',  ( -16.77683809663752257, 9.945835743215301505, -113.1639490191042512 ) ) ;
#138666 = DIRECTION ( 'NONE',  ( -1.000000000000000000, -0.000000000000000000, 0.000000000000000000 ) ) ;
#138668 = DIRECTION ( 'NONE',  ( 0.000000000000000000, 0.000000000000000000, -1.000000000000000000 ) ) ;
#138669 = FACE_OUTER_BOUND ( 'NONE', #157142, .T. ) ;
#138670 = TOROIDAL_SURFACE ( 'NONE', #126037, 4.149999999999999467, 0.1000000000000000056 ) ;
#138671 = DIRECTION ( 'NONE',  ( 2.342056488767302165E-15, 0.9594490217226113726, 0.2818822000686178608 ) ) ;
#138672 = CARTESIAN_POINT ( 'NONE',  ( 21.08832698747859169, 44.23125050195789498, -236.5431486773145480 ) ) ;
#138673 = VECTOR ( 'NONE', #93682, 1000.000000000000000 ) ;
#138674 = ORIENTED_EDGE ( 'NONE', *, *, #3451, .T. ) ;
#138675 = CIRCLE ( 'NONE', #255183, 0.1999999999999996503 ) ;
#138677 = ORIENTED_EDGE ( 'NONE', *, *, #175080, .T. ) ;
#138676 = DIRECTION ( 'NONE',  ( 0.000000000000000000, -0.1350103645451876944, 0.9908441862701601321 ) ) ;
#138678 = CARTESIAN_POINT ( 'NONE',  ( 18.69999999999999929, 11.75000000000000000, -15.00000000000000000 ) ) ;
#138679 = DIRECTION ( 'NONE',  ( 0.000000000000000000, 0.2128009952263604232, -0.9770955615653316162 ) ) ;
#138680 = SURFACE_SIDE_STYLE ('',( #20073 ) ) ;
#138681 = ORIENTED_EDGE ( 'NONE', *, *, #249290, .F. ) ;
#138682 = AXIS2_PLACEMENT_3D ( 'NONE', #14318, #54694, #55957 ) ;
#138684 = CIRCLE ( 'NONE', #26317, 7.899999999999990585 ) ;
#138683 = CARTESIAN_POINT ( 'NONE',  ( 21.05000000000000071, 7.916168987336737572, -211.9720049928963874 ) ) ;
#138685 = DIRECTION ( 'NONE',  ( -1.000000000000000000, 0.000000000000000000, 0.000000000000000000 ) ) ;
#138686 = ORIENTED_EDGE ( 'NONE', *, *, #107112, .F. ) ;
#138687 = CARTESIAN_POINT ( 'NONE',  ( -18.59117750673696889, 10.33248238083634796, -206.5948465439131496 ) ) ;
#138688 = DIRECTION ( 'NONE',  ( 1.000000000000000000, 0.000000000000000000, 0.000000000000000000 ) ) ;
#138689 = DIRECTION ( 'NONE',  ( -1.000000000000000000, -0.000000000000000000, -0.000000000000000000 ) ) ;
#138690 = AXIS2_PLACEMENT_3D ( 'NONE', #153547, #233055, #111812 ) ;
#138691 = DIRECTION ( 'NONE',  ( 1.000000000000000000, -7.667232114526941871E-17, 1.711482807214921537E-16 ) ) ;
#138693 = ORIENTED_EDGE ( 'NONE', *, *, #143849, .F. ) ;
#138692 = DIRECTION ( 'NONE',  ( 0.000000000000000000, 1.000000000000000000, 0.000000000000000000 ) ) ;
#138695 = ORIENTED_EDGE ( 'NONE', *, *, #117350, .F. ) ;
#138694 = CARTESIAN_POINT ( 'NONE',  ( -16.87683809663752399, 9.850000000011144508, -147.4023640181963515 ) ) ;
#138696 = VECTOR ( 'NONE', #13439, 1000.000000000000000 ) ;
#138697 = CARTESIAN_POINT ( 'NONE',  ( 20.94999999999999929, 23.49882452903949570, -253.1653563615082305 ) ) ;
#138699 = DIRECTION ( 'NONE',  ( 0.000000000000000000, 0.8814952561688476074, -0.4721928772777262417 ) ) ;
#138698 = CIRCLE ( 'NONE', #38800, 0.1999999999999945155 ) ;
#138700 = VECTOR ( 'NONE', #168105, 1000.000000000000000 ) ;
#138701 = CARTESIAN_POINT ( 'NONE',  ( -21.14999999999999858, 11.75000000001115552, -67.10000000000005116 ) ) ;
#138702 = CARTESIAN_POINT ( 'NONE',  ( -15.15766958671843589, 9.410538608540024441, -182.9326879971408175 ) ) ;
#138703 = CIRCLE ( 'NONE', #47149, 0.09999999999999939493 ) ;
#138705 = DIRECTION ( 'NONE',  ( -1.000000000000000000, -0.000000000000000000, 0.000000000000000000 ) ) ;
#138704 = CARTESIAN_POINT ( 'NONE',  ( -16.88705144915419964, 9.950000000011138823, -154.5690214052880265 ) ) ;
#138707 = EDGE_CURVE ( 'NONE', #45529, #134779, #105631, .T. ) ;
#138706 = CARTESIAN_POINT ( 'NONE',  ( -21.04999999999999716, 34.09556617704311776, -243.7880827679370270 ) ) ;
#138708 = DIRECTION ( 'NONE',  ( 1.000000000000000000, 0.000000000000000000, 0.000000000000000000 ) ) ;
#138709 = DIRECTION ( 'NONE',  ( -1.000000000000000000, -4.163336342344362270E-13, 0.000000000000000000 ) ) ;
#138710 = CARTESIAN_POINT ( 'NONE',  ( -18.43634282235122868, 85.67978719994030712, -163.3624555990703300 ) ) ;
#138711 = CARTESIAN_POINT ( 'NONE',  ( -21.14999999999999858, 11.65000000001115588, -67.00000000000004263 ) ) ;
#138712 = ORIENTED_EDGE ( 'NONE', *, *, #77356, .F. ) ;
#138713 = CARTESIAN_POINT ( 'NONE',  ( 21.05000000000000071, -0.02138556592644420135, -94.19503888731547647 ) ) ;
#138714 = VERTEX_POINT ( 'NONE', #230706 ) ;
#138715 = ORIENTED_EDGE ( 'NONE', *, *, #184007, .F. ) ;
#138716 = DIRECTION ( 'NONE',  ( 1.000000000000000000, 0.000000000000000000, -0.000000000000000000 ) ) ;
#138717 = EDGE_CURVE ( 'NONE', #235335, #99842, #132887, .T. ) ;
#138718 = CARTESIAN_POINT ( 'NONE',  ( 23.15000000000000213, 85.00000000001222134, -146.4170766071767389 ) ) ;
#138719 = ORIENTED_EDGE ( 'NONE', *, *, #255650, .F. ) ;
#138720 = B_SPLINE_CURVE_WITH_KNOTS ( 'NONE', 3,
 ( #125680, #224768, #108691, #8324, #203934, #227346, #27904, #83936, #188229, #183104, #147830, #24038, #46140, #226032, #68289, #167406, #248207, #69582, #48704 ),
 .UNSPECIFIED., .F., .F.,
 ( 4, 3, 3, 3, 3, 3, 4 ),
 ( 0.000000000000000000, 2.646747978908353324E-05, 5.271166642128929112E-05, 9.008788829885582504E-05, 0.0001426648776561122839, 0.0001897378458659801674, 0.0001917382627806533295 ),
 .UNSPECIFIED. ) ;
#138721 = EDGE_CURVE ( 'NONE', #257982, #223175, #147353, .T. ) ;
#138722 = ADVANCED_FACE ( 'NONE', ( #100131 ), #34971, .F. ) ;
#138723 = ORIENTED_EDGE ( 'NONE', *, *, #74709, .T. ) ;
#138724 = VECTOR ( 'NONE', #137252, 1000.000000000000000 ) ;
#138725 = TOROIDAL_SURFACE ( 'NONE', #213591, 11.65000000000000036, 0.1000000000000000056 ) ;
#138726 = VERTEX_POINT ( 'NONE', #119748 ) ;
#138727 = ORIENTED_EDGE ( 'NONE', *, *, #202565, .F. ) ;
#138728 = DIRECTION ( 'NONE',  ( 0.000000000000000000, -0.9908441862701596881, -0.1350103645451904977 ) ) ;
#138729 = CARTESIAN_POINT ( 'NONE',  ( -21.05000000000000071, -11.29603075033528015, -30.45210084033612929 ) ) ;
#138730 = DIRECTION ( 'NONE',  ( 1.000000000000000000, 0.000000000000000000, 0.000000000000000000 ) ) ;
#138731 = DIRECTION ( 'NONE',  ( 0.000000000000000000, 1.000000000000000000, 0.000000000000000000 ) ) ;
#138732 = CARTESIAN_POINT ( 'NONE',  ( -17.78043020864321022, 65.14640788800683424, -180.3600583188042208 ) ) ;
#138733 = AXIS2_PLACEMENT_3D ( 'NONE', #14899, #250905, #13603 ) ;
#138734 = ADVANCED_FACE ( 'NONE', ( #23222 ), #161441, .T. ) ;
#138735 = CARTESIAN_POINT ( 'NONE',  ( 21.12230431290518951, 65.53595890941556945, -242.0861857336640526 ) ) ;
#138736 = CARTESIAN_POINT ( 'NONE',  ( 21.07954640115206857, 75.93399229287231833, -142.8523951805472052 ) ) ;
#138738 = EDGE_LOOP ( 'NONE', ( #114372, #9533, #135335 ) ) ;
#138737 = CARTESIAN_POINT ( 'NONE',  ( 21.05000000000000071, 87.48912529308822172, -139.4231074845242802 ) ) ;
#138740 = LINE ( 'NONE', #43548, #162608 ) ;
#138739 = DIRECTION ( 'NONE',  ( 0.000000000000000000, 0.000000000000000000, -1.000000000000000000 ) ) ;
#138741 = CARTESIAN_POINT ( 'NONE',  ( -21.05000000000000071, 6.256349259666485807, -229.7266095100222572 ) ) ;
#138742 = VERTEX_POINT ( 'NONE', #20646 ) ;
#138743 = AXIS2_PLACEMENT_3D ( 'NONE', #255506, #155211, #13112 ) ;
#138744 = FACE_OUTER_BOUND ( 'NONE', #40621, .T. ) ;
#138745 = CARTESIAN_POINT ( 'NONE',  ( 21.87500000000000355, 66.25000000001253397, -182.3731074845244393 ) ) ;
#138746 = ORIENTED_EDGE ( 'NONE', *, *, #232307, .T. ) ;
#138747 = CIRCLE ( 'NONE', #192780, 0.1999999999999945155 ) ;
#138750 = DIRECTION ( 'NONE',  ( 0.000000000000000000, 0.000000000000000000, -1.000000000000000000 ) ) ;
#138749 = DIRECTION ( 'NONE',  ( 0.000000000000000000, -7.086529944415894657E-15, 1.000000000000000000 ) ) ;
#138748 = AXIS2_PLACEMENT_3D ( 'NONE', #18744, #93139, #253495 ) ;
#138751 = AXIS2_PLACEMENT_3D ( 'NONE', #222719, #100191, #198030 ) ;
#138752 = LINE ( 'NONE', #81353, #106974 ) ;
#138753 = DIRECTION ( 'NONE',  ( 0.000000000000000000, 0.2617529984165026247, 0.9651348961777158619 ) ) ;
#138754 = ORIENTED_EDGE ( 'NONE', *, *, #86774, .T. ) ;
#138755 = TOROIDAL_SURFACE ( 'NONE', #151295, 12.97499999999999787, 0.1000000000000000056 ) ;
#138756 = DIRECTION ( 'NONE',  ( -0.000000000000000000, -0.000000000000000000, 1.000000000000000000 ) ) ;
#138757 = EDGE_CURVE ( 'NONE', #116513, #48521, #180679, .T. ) ;
#138758 = CARTESIAN_POINT ( 'NONE',  ( -18.48408745364677586, -0.8919672813139534195, -242.3192850797796325 ) ) ;
#138759 = DIRECTION ( 'NONE',  ( -0.000000000000000000, 0.2617529984165031243, 0.9651348961777157509 ) ) ;
#138760 = CARTESIAN_POINT ( 'NONE',  ( 18.39999999999998082, 11.47316190337362585, -143.2500000000000284 ) ) ;
#138761 = ORIENTED_EDGE ( 'NONE', *, *, #104725, .T. ) ;
#138762 = CIRCLE ( 'NONE', #42951, 12.87499999999999822 ) ;
#138763 = FACE_OUTER_BOUND ( 'NONE', #225287, .T. ) ;
#138764 = ADVANCED_FACE ( 'NONE', ( #41494 ), #179714, .F. ) ;
#138765 = DIRECTION ( 'NONE',  ( 1.000000000000000000, 0.000000000000000000, 0.000000000000000000 ) ) ;
#138766 = DIRECTION ( 'NONE',  ( 1.000000000000000000, 0.000000000000000000, 0.000000000000000000 ) ) ;
#138767 = LINE ( 'NONE', #162251, #207511 ) ;
#138768 = DIRECTION ( 'NONE',  ( 0.000000000000000000, -7.056502275159890832E-15, 1.000000000000000000 ) ) ;
#138769 = VECTOR ( 'NONE', #45341, 1000.000000000000000 ) ;
#138770 = VECTOR ( 'NONE', #219335, 1000.000000000000000 ) ;
#138771 = VECTOR ( 'NONE', #204677, 1000.000000000000000 ) ;
#138773 = ORIENTED_EDGE ( 'NONE', *, *, #140460, .F. ) ;
#138772 = SPHERICAL_SURFACE ( 'NONE', #167131, 0.1000000000000000056 ) ;
#138774 = FACE_OUTER_BOUND ( 'NONE', #180268, .T. ) ;
#138775 = DIRECTION ( 'NONE',  ( 1.000000000000000000, 0.000000000000000000, 0.000000000000000000 ) ) ;
#138776 = DIRECTION ( 'NONE',  ( 0.000000000000000000, 0.2128009952263603677, -0.9770955615653313941 ) ) ;
#138777 = DIRECTION ( 'NONE',  ( 0.000000000000000000, -0.9651348961777164170, 0.2617529984165006263 ) ) ;
#138778 = FACE_OUTER_BOUND ( 'NONE', #251261, .T. ) ;
#138780 = VERTEX_POINT ( 'NONE', #101392 ) ;
#138779 = CARTESIAN_POINT ( 'NONE',  ( 18.49999999999999645, -1.835859311432484375, -145.5044391687985694 ) ) ;
#138781 = CARTESIAN_POINT ( 'NONE',  ( 23.14999999999999858, 70.50000000001199396, -115.4283735034374274 ) ) ;
#138782 = CARTESIAN_POINT ( 'NONE',  ( 21.14999999999999503, 1.115600667400684642E-11, -127.7500000000000284 ) ) ;
#138783 = ORIENTED_EDGE ( 'NONE', *, *, #49027, .F. ) ;
#138784 = CARTESIAN_POINT ( 'NONE',  ( 21.15000000000005542, 77.83551161375993388, -47.52760213295649550 ) ) ;
#138785 = CARTESIAN_POINT ( 'NONE',  ( 21.09107601085592520, 75.96069283529527638, -176.3869854598848974 ) ) ;
#138787 = ADVANCED_FACE ( 'NONE', ( #44042 ), #218810, .F. ) ;
#138786 = LINE ( 'NONE', #78833, #75578 ) ;
#138788 = DIRECTION ( 'NONE',  ( -1.000000000000000000, -0.000000000000000000, -0.000000000000000000 ) ) ;
#138789 = FACE_OUTER_BOUND ( 'NONE', #81795, .T. ) ;
#138790 = VECTOR ( 'NONE', #80547, 1000.000000000000114 ) ;
#138791 = FACE_OUTER_BOUND ( 'NONE', #11835, .T. ) ;
#138792 = AXIS2_PLACEMENT_3D ( 'NONE', #163970, #239656, #6152 ) ;
#138793 = AXIS2_PLACEMENT_3D ( 'NONE', #153485, #113024, #192564 ) ;
#138794 = ORIENTED_EDGE ( 'NONE', *, *, #71138, .T. ) ;
#138795 = VERTEX_POINT ( 'NONE', #240961 ) ;
#138796 = EDGE_CURVE ( 'NONE', #86021, #133057, #168248, .T. ) ;
#138797 = DIRECTION ( 'NONE',  ( -0.000000000000000000, 0.000000000000000000, 1.000000000000000000 ) ) ;
#138799 = EDGE_CURVE ( 'NONE', #141175, #128297, #79294, .T. ) ;
#138798 = CARTESIAN_POINT ( 'NONE',  ( -18.50000000000000000, 52.13794731297493712, -232.3713824252124880 ) ) ;
#138800 = LINE ( 'NONE', #7034, #62199 ) ;
#138801 = FACE_OUTER_BOUND ( 'NONE', #245647, .T. ) ;
#138802 = ORIENTED_EDGE ( 'NONE', *, *, #78791, .F. ) ;
#138803 = ADVANCED_FACE ( 'NONE', ( #242226 ), #197970, .F. ) ;
#138804 = ADVANCED_FACE ( 'NONE', ( #182279 ), #98840, .T. ) ;
#138805 = FACE_OUTER_BOUND ( 'NONE', #160973, .T. ) ;
#138806 = CARTESIAN_POINT ( 'NONE',  ( 20.41140022480414018, 11.79246562616856941, -206.2252339310995524 ) ) ;
#138807 = EDGE_CURVE ( 'NONE', #138653, #242609, #220116, .T. ) ;
#138808 = FACE_OUTER_BOUND ( 'NONE', #132806, .T. ) ;
#138809 = LINE ( 'NONE', #39789, #57678 ) ;
#138810 = DIRECTION ( 'NONE',  ( -0.000000000000000000, -6.982962677686266711E-15, 1.000000000000000000 ) ) ;
#138811 = ADVANCED_FACE ( 'NONE', ( #178447 ), #139262, .T. ) ;
#138813 = EDGE_CURVE ( 'NONE', #198298, #220754, #141845, .T. ) ;
#138812 = EDGE_CURVE ( 'NONE', #195790, #22117, #22488, .T. ) ;
#138814 = ORIENTED_EDGE ( 'NONE', *, *, #238732, .F. ) ;
#138815 = DIRECTION ( 'NONE',  ( 0.000000000000000000, -0.9553114395362733990, 0.2956011730205631016 ) ) ;
#138816 = EDGE_LOOP ( 'NONE', ( #21409, #163817, #32182, #143522 ) ) ;
#138817 = AXIS2_PLACEMENT_3D ( 'NONE', #45883, #125435, #204940 ) ;
#138818 = DIRECTION ( 'NONE',  ( -0.000000000000000000, 0.9126074666063770380, 0.4088369013363281068 ) ) ;
#138819 = ORIENTED_EDGE ( 'NONE', *, *, #7821, .T. ) ;
#138820 = DIRECTION ( 'NONE',  ( 0.000000000000000000, 0.000000000000000000, 1.000000000000000000 ) ) ;
#138821 = CARTESIAN_POINT ( 'NONE',  ( 21.87500000000000355, 66.25000000001151079, -48.27310748452438816 ) ) ;
#138822 = DIRECTION ( 'NONE',  ( 0.000000000000000000, -0.2128009952263601456, 0.9770955615653316162 ) ) ;
#138823 = EDGE_LOOP ( 'NONE', ( #104418, #50605, #103536, #105504 ) ) ;
#138824 = DIRECTION ( 'NONE',  ( 0.000000000000000000, 0.9893560106964510714, -0.1455152366551481502 ) ) ;
#138825 = EDGE_LOOP ( 'NONE', ( #9822, #211003, #221966, #178744 ) ) ;
#138826 = CARTESIAN_POINT ( 'NONE',  ( -12.48127053791145258, 9.376580978055098825, -151.6269462470119720 ) ) ;
#138827 = EDGE_CURVE ( 'NONE', #103521, #157381, #55735, .T. ) ;
#138829 = VERTEX_POINT ( 'NONE', #2326 ) ;
#138828 = FACE_OUTER_BOUND ( 'NONE', #247559, .T. ) ;
#138830 = DIRECTION ( 'NONE',  ( -1.000000000000000000, -0.000000000000000000, -0.000000000000000000 ) ) ;
#138831 = DIRECTION ( 'NONE',  ( 0.000000000000000000, 0.9770955615653316162, 0.2128009952263605342 ) ) ;
#138832 = EDGE_CURVE ( 'NONE', #133882, #187086, #201827, .T. ) ;
#138834 = EDGE_CURVE ( 'NONE', #112086, #126038, #243200, .T. ) ;
#138833 = VECTOR ( 'NONE', #201157, 1000.000000000000000 ) ;
#138835 = AXIS2_PLACEMENT_3D ( 'NONE', #93957, #99071, #114812 ) ;
#138836 = ORIENTED_EDGE ( 'NONE', *, *, #253820, .T. ) ;
#138837 = AXIS2_PLACEMENT_3D ( 'NONE', #19095, #786, #79046 ) ;
#138838 = CARTESIAN_POINT ( 'NONE',  ( -16.77779411503079032, 9.946101446935278645, -79.66305741761988202 ) ) ;
#138840 = EDGE_CURVE ( 'NONE', #4495, #51843, #169156, .T. ) ;
#138839 = CARTESIAN_POINT ( 'NONE',  ( 23.40000000000005187, 83.90000000001120384, -34.77310748452479316 ) ) ;
#138841 = DIRECTION ( 'NONE',  ( 1.000000000000000000, 0.000000000000000000, 0.000000000000000000 ) ) ;
#138842 = ORIENTED_EDGE ( 'NONE', *, *, #76682, .F. ) ;
#138843 = CARTESIAN_POINT ( 'NONE',  ( -22.50000000000000000, 64.35000000001197407, -103.0231074845244024 ) ) ;
#138844 = CARTESIAN_POINT ( 'NONE',  ( 15.74999999999999645, 48.12247445990688988, -234.1702647910923361 ) ) ;
#138845 = DIRECTION ( 'NONE',  ( 0.000000000000000000, 0.000000000000000000, 1.000000000000000000 ) ) ;
#138846 = EDGE_CURVE ( 'NONE', #154130, #199909, #226499, .T. ) ;
#138847 = ORIENTED_EDGE ( 'NONE', *, *, #251391, .F. ) ;
#138848 = AXIS2_PLACEMENT_3D ( 'NONE', #116751, #120632, #197566 ) ;
#138849 = ORIENTED_EDGE ( 'NONE', *, *, #236277, .T. ) ;
#138850 = AXIS2_PLACEMENT_3D ( 'NONE', #6789, #146293, #219727 ) ;
#138851 = CIRCLE ( 'NONE', #72273, 0.09999999999999484301 ) ;
#138852 = ORIENTED_EDGE ( 'NONE', *, *, #1025, .F. ) ;
#138853 = VECTOR ( 'NONE', #37652, 1000.000000000000000 ) ;
#138854 = ORIENTED_EDGE ( 'NONE', *, *, #149109, .T. ) ;
#138855 = DIRECTION ( 'NONE',  ( -0.000000000000000000, -6.982962677686266711E-15, 1.000000000000000000 ) ) ;
#138856 = FACE_OUTER_BOUND ( 'NONE', #234964, .T. ) ;
#138858 = VERTEX_POINT ( 'NONE', #68745 ) ;
#138857 = DIRECTION ( 'NONE',  ( -0.000000000000000000, 0.000000000000000000, 1.000000000000000000 ) ) ;
#138859 = DIRECTION ( 'NONE',  ( -0.000000000000000000, -1.000000000000000000, -6.982962677686266711E-15 ) ) ;
#138860 = CARTESIAN_POINT ( 'NONE',  ( -20.85000000000000142, 77.25000000001165290, -61.72262673010921930 ) ) ;
#138861 = DIRECTION ( 'NONE',  ( -0.000000000000000000, 0.000000000000000000, -1.000000000000000000 ) ) ;
#138862 = CARTESIAN_POINT ( 'NONE',  ( 20.94999999999999574, 0.4879293624014888198, -209.1697915983179428 ) ) ;
#138863 = CARTESIAN_POINT ( 'NONE',  ( -22.50000000000000000, 11.75000000001115552, -100.5000000000000284 ) ) ;
#138864 = TOROIDAL_SURFACE ( 'NONE', #63907, 11.70000000000000107, 0.1000000000000000056 ) ;
#138865 = DIRECTION ( 'NONE',  ( 0.000000000000000000, 6.982962677686266711E-15, -1.000000000000000000 ) ) ;
#138866 = AXIS2_PLACEMENT_3D ( 'NONE', #76125, #193527, #35749 ) ;
#138867 = ORIENTED_EDGE ( 'NONE', *, *, #176831, .F. ) ;
#138869 = ORIENTED_EDGE ( 'NONE', *, *, #48096, .F. ) ;
#138868 = CARTESIAN_POINT ( 'NONE',  ( 16.87683809663750267, 9.950000000011138823, -79.65000000000003411 ) ) ;
#138870 = AXIS2_PLACEMENT_3D ( 'NONE', #38199, #134690, #214256 ) ;
#138871 = VERTEX_POINT ( 'NONE', #148275 ) ;
#138872 = EDGE_LOOP ( 'NONE', ( #141805, #224968, #123756, #226868 ) ) ;
#138873 = CARTESIAN_POINT ( 'NONE',  ( -18.50000324121759121, 10.29307482169070553, -105.9586421466940749 ) ) ;
#138874 = DIRECTION ( 'NONE',  ( 0.000000000000000000, -6.769652589177784668E-15, 1.000000000000000000 ) ) ;
#138875 = DIRECTION ( 'NONE',  ( 0.000000000000000000, 0.000000000000000000, -1.000000000000000000 ) ) ;
#138876 = AXIS2_PLACEMENT_3D ( 'NONE', #12414, #111493, #214431 ) ;
#138877 = DIRECTION ( 'NONE',  ( 0.000000000000000000, 0.000000000000000000, -1.000000000000000000 ) ) ;
#138878 = LINE ( 'NONE', #119371, #201161 ) ;
#138879 = LINE ( 'NONE', #60649, #232315 ) ;
#138880 = CIRCLE ( 'NONE', #226380, 11.64999999999999325 ) ;
#138881 = CIRCLE ( 'NONE', #26515, 12.87500000000000000 ) ;
#138882 = AXIS2_PLACEMENT_3D ( 'NONE', #41399, #103891, #81749 ) ;
#138884 = AXIS2_PLACEMENT_3D ( 'NONE', #12180, #171283, #72146 ) ;
#138883 = CARTESIAN_POINT ( 'NONE',  ( 21.87500000000000355, 9.750000000011153745, -45.85000000000000142 ) ) ;
#138886 = EDGE_LOOP ( 'NONE', ( #39621, #157950, #26069, #204389 ) ) ;
#138885 = EDGE_CURVE ( 'NONE', #39159, #93529, #222332, .T. ) ;
#138887 = ORIENTED_EDGE ( 'NONE', *, *, #217231, .F. ) ;
#138888 = DIRECTION ( 'NONE',  ( 0.000000000000000000, 0.000000000000000000, -1.000000000000000000 ) ) ;
#138889 = EDGE_CURVE ( 'NONE', #145985, #98647, #248656, .T. ) ;
#138890 = ORIENTED_EDGE ( 'NONE', *, *, #54708, .T. ) ;
#138891 = DIRECTION ( 'NONE',  ( -1.000000000000000000, 0.000000000000000000, -0.000000000000000000 ) ) ;
#138892 = CARTESIAN_POINT ( 'NONE',  ( 21.05000000000000071, -8.999999999988842703, -57.10603087734755690 ) ) ;
#138893 = CARTESIAN_POINT ( 'NONE',  ( 23.24999999999999645, 4.775700934590591196, -122.1512318959540551 ) ) ;
#138894 = DIRECTION ( 'NONE',  ( 0.000000000000000000, -0.9651348961777155289, 0.2617529984165036794 ) ) ;
#138895 = EDGE_CURVE ( 'NONE', #198415, #129019, #159842, .T. ) ;
#138896 = VERTEX_POINT ( 'NONE', #163996 ) ;
#138898 = EDGE_CURVE ( 'NONE', #159529, #198941, #126509, .T. ) ;
#138897 = DIRECTION ( 'NONE',  ( -1.000000000000000000, -0.000000000000000000, 0.000000000000000000 ) ) ;
#138899 = VERTEX_POINT ( 'NONE', #243519 ) ;
#138900 = EDGE_LOOP ( 'NONE', ( #143791, #176627, #167452 ) ) ;
#138901 = DIRECTION ( 'NONE',  ( 0.000000000000000000, -0.4721928772776973204, -0.8814952561688629284 ) ) ;
#138902 = VECTOR ( 'NONE', #83029, 1000.000000000000000 ) ;
#138903 = CARTESIAN_POINT ( 'NONE',  ( 13.40000000000005898, 66.35000000001119247, -18.42310748452479530 ) ) ;
#138904 = ORIENTED_EDGE ( 'NONE', *, *, #12161, .T. ) ;
#138905 = VECTOR ( 'NONE', #1480, 1000.000000000000000 ) ;
#138906 = DIRECTION ( 'NONE',  ( 0.000000000000000000, 0.000000000000000000, 1.000000000000000000 ) ) ;
#138908 = ORIENTED_EDGE ( 'NONE', *, *, #87589, .T. ) ;
#138907 = DIRECTION ( 'NONE',  ( 1.000000000000000000, -0.000000000000000000, -0.000000000000000000 ) ) ;
#138909 = VECTOR ( 'NONE', #16715, 1000.000000000000227 ) ;
#138910 = DIRECTION ( 'NONE',  ( 1.713247197920696931E-14, -0.2606175937107791940, 0.9654421110809303652 ) ) ;
#138911 = VERTEX_POINT ( 'NONE', #208263 ) ;
#138912 = EDGE_CURVE ( 'NONE', #216037, #124124, #183557, .T. ) ;
#138913 = ADVANCED_FACE ( 'NONE', ( #149582 ), #64876, .T. ) ;
#138914 = AXIS2_PLACEMENT_3D ( 'NONE', #191822, #190535, #210084 ) ;
#138915 = AXIS2_PLACEMENT_3D ( 'NONE', #58830, #160554, #241365 ) ;
#138916 = CARTESIAN_POINT ( 'NONE',  ( 19.75857864376268935, 11.65000000001115943, -192.2499999999999716 ) ) ;
#138917 = ORIENTED_EDGE ( 'NONE', *, *, #106827, .T. ) ;
#138918 = CARTESIAN_POINT ( 'NONE',  ( 23.25000000000000000, 61.88149656937974896, -248.1136133839584090 ) ) ;
#138919 = CARTESIAN_POINT ( 'NONE',  ( -23.25000000000000355, 11.75000000001113953, -176.7499999999999716 ) ) ;
#138920 = DIRECTION ( 'NONE',  ( 0.000000000000000000, 6.982962677686266711E-15, -1.000000000000000000 ) ) ;
#138921 = CARTESIAN_POINT ( 'NONE',  ( -23.15000000000000213, 0.000000000000000000, -33.50000000000000000 ) ) ;
#138922 = CIRCLE ( 'NONE', #26564, 0.1000000000000028644 ) ;
#138923 = DIRECTION ( 'NONE',  ( 0.000000000000000000, 0.000000000000000000, -1.000000000000000000 ) ) ;
#138924 = CIRCLE ( 'NONE', #13893, 0.09999999999999939493 ) ;
#138925 = EDGE_LOOP ( 'NONE', ( #80136, #1535, #67190, #181841 ) ) ;
#138926 = AXIS2_PLACEMENT_3D ( 'NONE', #177200, #80603, #97593 ) ;
#138928 = EDGE_CURVE ( 'NONE', #254124, #183349, #184958, .T. ) ;
#138927 = CARTESIAN_POINT ( 'NONE',  ( -21.05000000000000071, 62.00000000001218581, -141.9502000149069261 ) ) ;
#138929 = DIRECTION ( 'NONE',  ( 0.5735764363510460484, -0.8191520442889919096, 0.000000000000000000 ) ) ;
#138931 = PLANE ( 'NONE',  #96890 ) ;
#138930 = TOROIDAL_SURFACE ( 'NONE', #184756, 4.150000000000000355, 0.1000000000000000056 ) ;
#138932 = ORIENTED_EDGE ( 'NONE', *, *, #57736, .F. ) ;
#138933 = EDGE_CURVE ( 'NONE', #9118, #233017, #80702, .T. ) ;
#138934 = CARTESIAN_POINT ( 'NONE',  ( 22.00411653962172664, 7.066231425286733092, -199.3596904452042793 ) ) ;
#138935 = ORIENTED_EDGE ( 'NONE', *, *, #67178, .T. ) ;
#138936 = FACE_OUTER_BOUND ( 'NONE', #183010, .T. ) ;
#138938 = ORIENTED_EDGE ( 'NONE', *, *, #254794, .T. ) ;
#138937 = AXIS2_PLACEMENT_3D ( 'NONE', #235814, #173339, #71635 ) ;
#138939 = CARTESIAN_POINT ( 'NONE',  ( -20.54999999999999716, 76.00000000001126921, -203.5231074845248997 ) ) ;
#138940 = CARTESIAN_POINT ( 'NONE',  ( 23.14999999999999503, 11.75000000000000711, 11.75000000000000000 ) ) ;
#138942 = EDGE_LOOP ( 'NONE', ( #49217, #45026, #128295, #242269 ) ) ;
#138941 = DIRECTION ( 'NONE',  ( -1.020425574104004196E-15, -1.210927747993693964E-31, -1.000000000000000000 ) ) ;
#138943 = DIRECTION ( 'NONE',  ( 1.000000000000000000, 0.000000000000000000, 0.000000000000000000 ) ) ;
#138944 = ORIENTED_EDGE ( 'NONE', *, *, #97017, .T. ) ;
#138945 = VECTOR ( 'NONE', #114756, 1000.000000000000227 ) ;
#138946 = EDGE_CURVE ( 'NONE', #146363, #236918, #128719, .T. ) ;
#138947 = DIRECTION ( 'NONE',  ( 1.000000000000000000, 0.000000000000000000, 0.000000000000000000 ) ) ;
#138948 = CARTESIAN_POINT ( 'NONE',  ( 20.94999999999999574, 35.88801296822693843, -234.5558624753690538 ) ) ;
#138949 = EDGE_CURVE ( 'NONE', #138726, #95676, #144391, .T. ) ;
#138950 = ORIENTED_EDGE ( 'NONE', *, *, #127295, .T. ) ;
#138951 = VERTEX_POINT ( 'NONE', #223945 ) ;
#138952 = AXIS2_PLACEMENT_3D ( 'NONE', #164027, #101426, #6216 ) ;
#138953 = DIRECTION ( 'NONE',  ( 1.000000000000000000, -3.265361837132813093E-16, -2.280189983783949500E-30 ) ) ;
#138954 = DIRECTION ( 'NONE',  ( 0.000000000000000000, 0.000000000000000000, -1.000000000000000000 ) ) ;
#138955 = ORIENTED_EDGE ( 'NONE', *, *, #242384, .F. ) ;
#138956 = PLANE ( 'NONE',  #153294 ) ;
#138957 = EDGE_CURVE ( 'NONE', #94515, #238290, #10044, .T. ) ;
#138959 = ORIENTED_EDGE ( 'NONE', *, *, #140332, .F. ) ;
#138958 = CIRCLE ( 'NONE', #26590, 11.65000000000000036 ) ;
#138960 = VERTEX_POINT ( 'NONE', #46583 ) ;
#138961 = AXIS2_PLACEMENT_3D ( 'NONE', #23865, #25141, #100754 ) ;
#138962 = EDGE_CURVE ( 'NONE', #97650, #167682, #168450, .T. ) ;
#138963 = CARTESIAN_POINT ( 'NONE',  ( -22.50000000000000000, 0.1000000000111554016, -167.4999999999999716 ) ) ;
#138964 = EDGE_CURVE ( 'NONE', #75696, #87867, #180294, .T. ) ;
#138966 = ORIENTED_EDGE ( 'NONE', *, *, #160448, .F. ) ;
#138965 = FACE_OUTER_BOUND ( 'NONE', #58892, .T. ) ;
#138967 = CARTESIAN_POINT ( 'NONE',  ( -20.64999999999999858, 7.250000000011155521, -79.35000000000005116 ) ) ;
#138968 = DIRECTION ( 'NONE',  ( 2.952720810173289112E-16, 1.000000000000000000, 6.938893903907222067E-15 ) ) ;
#138969 = DIRECTION ( 'NONE',  ( 0.000000000000000000, -7.189901751995769991E-15, 1.000000000000000000 ) ) ;
#138970 = EDGE_CURVE ( 'NONE', #86057, #130702, #67445, .T. ) ;
#138972 = CARTESIAN_POINT ( 'NONE',  ( -22.49510344025093644, 75.93287232181820912, -181.6730775896386376 ) ) ;
#138971 = CARTESIAN_POINT ( 'NONE',  ( -16.98495255085919098, 63.03613173686448334, -213.0982309764472689 ) ) ;
#138973 = CARTESIAN_POINT ( 'NONE',  ( -21.05000000000000071, 76.00000000001220712, -143.0637644362255401 ) ) ;
#138974 = AXIS2_PLACEMENT_3D ( 'NONE', #47222, #186770, #126779 ) ;
#138975 = FACE_OUTER_BOUND ( 'NONE', #227624, .T. ) ;
#138976 = CIRCLE ( 'NONE', #5718, 0.09999999999999939493 ) ;
#138977 = CARTESIAN_POINT ( 'NONE',  ( 0.9000000000000546452, 67.75000000001118394, -5.981686128287480919 ) ) ;
#138978 = CIRCLE ( 'NONE', #68107, 0.1000000000000090677 ) ;
#138979 = CIRCLE ( 'NONE', #214040, 0.09999999999999939493 ) ;
#138980 = VERTEX_POINT ( 'NONE', #28368 ) ;
#138982 = EDGE_LOOP ( 'NONE', ( #24585, #242604, #201301, #25115 ) ) ;
#138981 = DIRECTION ( 'NONE',  ( -0.000000000000000000, -0.2617529984165030132, -0.9651348961777157509 ) ) ;
#138983 = ORIENTED_EDGE ( 'NONE', *, *, #225875, .F. ) ;
#138984 = EDGE_CURVE ( 'NONE', #72339, #253511, #167867, .T. ) ;
#138985 = DIRECTION ( 'NONE',  ( -0.000000000000000000, 0.8660254037844411501, 0.4999999999999956701 ) ) ;
#138986 = EDGE_LOOP ( 'NONE', ( #198159, #29444, #95045, #111110 ) ) ;
#138987 = CARTESIAN_POINT ( 'NONE',  ( -22.59999999999999787, 0.000000000000000000, 0.000000000000000000 ) ) ;
#138988 = ORIENTED_EDGE ( 'NONE', *, *, #23555, .T. ) ;
#138989 = B_SPLINE_CURVE_WITH_KNOTS ( 'NONE', 3,
 ( #99689, #177992, #59262, #120591, #22779, #121866, #100948, #43605, #217077, #239233, #241798, #102248, #257448, #197526, #63145, #222210, #201384, #38464, #200110, #80112, #181831, #119294 ),
 .UNSPECIFIED., .F., .F.,
 ( 4, 3, 3, 3, 3, 3, 3, 4 ),
 ( 0.000000000000000000, 7.307836821080901168E-06, 4.161455748548336644E-05, 7.576591810647893463E-05, 0.0001098090429817568444, 0.0001438003617351259016, 0.0001777914035423789891, 0.0002117966137403338534 ),
 .UNSPECIFIED. ) ;
#138991 = ORIENTED_EDGE ( 'NONE', *, *, #222843, .F. ) ;
#138990 = ORIENTED_EDGE ( 'NONE', *, *, #55536, .T. ) ;
#138992 = EDGE_LOOP ( 'NONE', ( #207125, #245668, #203238, #244635 ) ) ;
#138993 = VERTEX_POINT ( 'NONE', #11333 ) ;
#138994 = CARTESIAN_POINT ( 'NONE',  ( -20.64999999999999858, -8.999999999988844479, -90.60603087734760663 ) ) ;
#138995 = AXIS2_PLACEMENT_3D ( 'NONE', #45579, #204632, #185087 ) ;
#138996 = CARTESIAN_POINT ( 'NONE',  ( -23.25000000000000000, 11.65000000001115588, -179.6499999999999773 ) ) ;
#138998 = ORIENTED_EDGE ( 'NONE', *, *, #4336, .F. ) ;
#138997 = CARTESIAN_POINT ( 'NONE',  ( 23.14999999999999503, 52.81534179157632991, -244.1198638051726277 ) ) ;
#138999 = CARTESIAN_POINT ( 'NONE',  ( 20.94999999999999574, 1.115600667400684642E-11, -33.50000000000000000 ) ) ;
#139001 = EDGE_LOOP ( 'NONE', ( #247883, #198618, #173805, #128464, #139475, #48505, #66566, #89482, #249256, #40003, #57531, #76788 ) ) ;
#139000 = DIRECTION ( 'NONE',  ( -0.000000000000000000, 0.8660254037844377084, 0.5000000000000016653 ) ) ;
#139002 = DIRECTION ( 'NONE',  ( -0.000000000000000000, 0.000000000000000000, 1.000000000000000000 ) ) ;
#139003 = ORIENTED_EDGE ( 'NONE', *, *, #162331, .F. ) ;
#139004 = CARTESIAN_POINT ( 'NONE',  ( 20.46382478191414833, 8.901379558713770734, -176.0457280948830885 ) ) ;
#139006 = VERTEX_POINT ( 'NONE', #251206 ) ;
#139005 = CARTESIAN_POINT ( 'NONE',  ( -21.14999999999999858, 6.540656951712397138, -167.4999999999999716 ) ) ;
#139007 = DIRECTION ( 'NONE',  ( -1.000000000000000000, 0.000000000000000000, 0.000000000000000000 ) ) ;
#139008 = CARTESIAN_POINT ( 'NONE',  ( 20.94999999999999929, 11.75000000001115730, -60.21613433702191287 ) ) ;
#139009 = ORIENTED_EDGE ( 'NONE', *, *, #169125, .T. ) ;
#139011 = CARTESIAN_POINT ( 'NONE',  ( -16.89060415895971090, 44.13125937934476184, -235.2994854922266370 ) ) ;
#139010 = DIRECTION ( 'NONE',  ( -0.000000000000000000, -0.9770955615653315052, -0.2128009952263603954 ) ) ;
#139012 = CARTESIAN_POINT ( 'NONE',  ( -12.25000000000000178, 66.65000000001185754, -86.27310748452437394 ) ) ;
#139013 = CIRCLE ( 'NONE', #30942, 0.1000000000000028644 ) ;
#139014 = DIRECTION ( 'NONE',  ( 0.000000000000000000, -1.000000000000000000, 0.000000000000000000 ) ) ;
#139015 = CIRCLE ( 'NONE', #88970, 0.8750000000000007772 ) ;
#139016 = DIRECTION ( 'NONE',  ( 0.000000000000000000, 0.000000000000000000, 1.000000000000000000 ) ) ;
#139017 = CARTESIAN_POINT ( 'NONE',  ( -21.05000000000000071, 36.02918351690955490, -236.0543695120161374 ) ) ;
#139018 = ORIENTED_EDGE ( 'NONE', *, *, #218031, .F. ) ;
#139020 = ORIENTED_EDGE ( 'NONE', *, *, #6841, .T. ) ;
#139019 = AXIS2_PLACEMENT_3D ( 'NONE', #23654, #122743, #22359 ) ;
#139021 = EDGE_LOOP ( 'NONE', ( #230989, #246361, #38376, #128380 ) ) ;
#139022 = CARTESIAN_POINT ( 'NONE',  ( 20.94999999999999929, 76.00000000001170974, -69.52310748452431710 ) ) ;
#139023 = VERTEX_POINT ( 'NONE', #34778 ) ;
#139024 = CARTESIAN_POINT ( 'NONE',  ( -20.85000000000000142, 67.85909929089923764, -227.8797997985275856 ) ) ;
#139025 = ORIENTED_EDGE ( 'NONE', *, *, #92649, .T. ) ;
#139026 = DIRECTION ( 'NONE',  ( 0.000000000000000000, 0.2128009952263603677, -0.9770955615653313941 ) ) ;
#139027 = ADVANCED_FACE ( 'NONE', ( #153460 ), #193828, .F. ) ;
#139028 = CARTESIAN_POINT ( 'NONE',  ( -18.40000000000000213, 11.47316190337362762, -79.65000000000004832 ) ) ;
#139029 = ADVANCED_FACE ( 'NONE', ( #72610 ), #156000, .T. ) ;
#139030 = EDGE_CURVE ( 'NONE', #202405, #19842, #55346, .T. ) ;
#139031 = ORIENTED_EDGE ( 'NONE', *, *, #96953, .F. ) ;
#139032 = AXIS2_PLACEMENT_3D ( 'NONE', #107464, #249563, #52622 ) ;
#139033 = CARTESIAN_POINT ( 'NONE',  ( -22.39999999999999858, 1.115600667400684642E-11, -21.85042919245520210 ) ) ;
#139034 =( NAMED_UNIT ( * ) SI_UNIT ( $, .STERADIAN. ) SOLID_ANGLE_UNIT ( ) );
#139035 = AXIS2_PLACEMENT_3D ( 'NONE', #126737, #206279, #204967 ) ;
#139036 = ORIENTED_EDGE ( 'NONE', *, *, #174273, .T. ) ;
#139037 = ORIENTED_EDGE ( 'NONE', *, *, #231964, .T. ) ;
#139038 = AXIS2_PLACEMENT_3D ( 'NONE', #123536, #25716, #124825 ) ;
#139039 = ORIENTED_EDGE ( 'NONE', *, *, #14773, .F. ) ;
#139040 = AXIS2_PLACEMENT_3D ( 'NONE', #121054, #101401, #179725 ) ;
#139041 = DIRECTION ( 'NONE',  ( 1.000000000000000000, -0.000000000000000000, -0.000000000000000000 ) ) ;
#139042 = CARTESIAN_POINT ( 'NONE',  ( 23.14999999999999503, 64.35000000001275566, -215.2731074845244450 ) ) ;
#139043 = DIRECTION ( 'NONE',  ( 0.000000000000000000, 0.000000000000000000, -1.000000000000000000 ) ) ;
#139044 = LINE ( 'NONE', #255125, #161290 ) ;
#139045 = CARTESIAN_POINT ( 'NONE',  ( 15.39170923737819763, 66.61047060254530550, -118.7059995716306986 ) ) ;
#139046 = EDGE_CURVE ( 'NONE', #60346, #224623, #131274, .T. ) ;
#139048 = LINE ( 'NONE', #218603, #7604 ) ;
#139047 = DIRECTION ( 'NONE',  ( -0.000000000000000000, 0.2617529984165031243, 0.9651348961777157509 ) ) ;
#139049 = CARTESIAN_POINT ( 'NONE',  ( -23.15000000000000213, 76.00000000001244871, -170.0231074845243597 ) ) ;
#139051 = ORIENTED_EDGE ( 'NONE', *, *, #193492, .T. ) ;
#139050 = PLANE ( 'NONE',  #56482 ) ;
#139052 = LINE ( 'NONE', #59520, #41641 ) ;
#139053 = ORIENTED_EDGE ( 'NONE', *, *, #240337, .F. ) ;
#139054 = CARTESIAN_POINT ( 'NONE',  ( -18.46093223321780030, -9.480682968263337784, -141.0845505139267004 ) ) ;
#139055 = ORIENTED_EDGE ( 'NONE', *, *, #42570, .T. ) ;
#139056 = ORIENTED_EDGE ( 'NONE', *, *, #176783, .T. ) ;
#139057 = DIRECTION ( 'NONE',  ( 0.000000000000000000, 0.9987946567507913764, -0.04908394489106009811 ) ) ;
#139059 = CIRCLE ( 'NONE', #14225, 4.149999999999987033 ) ;
#139058 = FACE_OUTER_BOUND ( 'NONE', #151764, .T. ) ;
#139060 = DIRECTION ( 'NONE',  ( -1.000000000000000000, -2.283407518332345398E-16, 1.048447799332034305E-15 ) ) ;
#139061 = CIRCLE ( 'NONE', #26693, 0.09999999999999939493 ) ;
#139062 = EDGE_LOOP ( 'NONE', ( #31457, #199597, #235123, #171539, #148953 ) ) ;
#139063 = AXIS2_PLACEMENT_3D ( 'NONE', #164607, #60350, #100729 ) ;
#139064 = DIRECTION ( 'NONE',  ( 1.000000000000000000, 0.000000000000000000, 0.000000000000000000 ) ) ;
#139065 = ORIENTED_EDGE ( 'NONE', *, *, #99677, .T. ) ;
#139066 = VERTEX_POINT ( 'NONE', #16486 ) ;
#139067 = AXIS2_PLACEMENT_3D ( 'NONE', #222978, #191263, #44370 ) ;
#139068 = CARTESIAN_POINT ( 'NONE',  ( -16.94878442675512531, 9.991729102990998257, -12.61178042436212010 ) ) ;
#139070 = EDGE_LOOP ( 'NONE', ( #43675, #204027, #79717, #113016 ) ) ;
#139069 = EDGE_CURVE ( 'NONE', #13982, #202471, #67861, .T. ) ;
#139071 = CARTESIAN_POINT ( 'NONE',  ( -16.93909480342659890, 60.88478451565230642, -221.0783736713412679 ) ) ;
#139072 = CARTESIAN_POINT ( 'NONE',  ( 20.94999999999999574, -11.48912529306490349, -137.1000000000000227 ) ) ;
#139073 = ORIENTED_EDGE ( 'NONE', *, *, #86418, .F. ) ;
#139074 = EDGE_CURVE ( 'NONE', #6293, #137417, #231680, .T. ) ;
#139075 = DIRECTION ( 'NONE',  ( 0.000000000000000000, 0.7397360091702755991, -0.6728971962616832059 ) ) ;
#139076 = CARTESIAN_POINT ( 'NONE',  ( -21.05000000000000071, -11.39257802170567224, -3.073949579831933843 ) ) ;
#139077 = CARTESIAN_POINT ( 'NONE',  ( -20.85000000000000142, -4.352039508298082282, -236.2331130063498676 ) ) ;
#139078 = ORIENTED_EDGE ( 'NONE', *, *, #112962, .T. ) ;
#139079 = AXIS2_PLACEMENT_3D ( 'NONE', #219111, #20957, #183850 ) ;
#139080 = VECTOR ( 'NONE', #73191, 1000.000000000000000 ) ;
#139081 = AXIS2_PLACEMENT_3D ( 'NONE', #195320, #38792, #16672 ) ;
#139082 = CARTESIAN_POINT ( 'NONE',  ( 21.05000000000000071, -1.162701749926853712, -175.5999999999999659 ) ) ;
#139083 = CARTESIAN_POINT ( 'NONE',  ( -20.64999999999999858, 7.250000000011155521, -188.6499999999999488 ) ) ;
#139084 = ADVANCED_FACE ( 'NONE', ( #212113 ), #172541, .T. ) ;
#139085 = DIRECTION ( 'NONE',  ( 1.000000000000000000, 0.000000000000000000, 0.000000000000000000 ) ) ;
#139086 = ORIENTED_EDGE ( 'NONE', *, *, #128318, .F. ) ;
#139087 = VERTEX_POINT ( 'NONE', #75181 ) ;
#139088 = ORIENTED_EDGE ( 'NONE', *, *, #107609, .F. ) ;
#139089 = DIRECTION ( 'NONE',  ( 1.000000000000000000, 0.000000000000000000, 0.000000000000000000 ) ) ;
#139090 = DIRECTION ( 'NONE',  ( 0.000000000000000000, 0.000000000000000000, -1.000000000000000000 ) ) ;
#139091 = DIRECTION ( 'NONE',  ( 0.000000000000000000, 6.982962677686266711E-15, -1.000000000000000000 ) ) ;
#139092 = DIRECTION ( 'NONE',  ( 0.000000000000000000, -0.8814952561688476074, 0.4721928772777262417 ) ) ;
#139093 = CARTESIAN_POINT ( 'NONE',  ( -16.88560720703333473, 66.04943515626236206, -123.8749955636606472 ) ) ;
#139094 = ORIENTED_EDGE ( 'NONE', *, *, #206547, .T. ) ;
#139095 = EDGE_CURVE ( 'NONE', #145909, #100153, #247499, .T. ) ;
#139096 = DIRECTION ( 'NONE',  ( -1.000000000000000000, -3.265361837132813093E-16, 0.000000000000000000 ) ) ;
#139097 = AXIS2_PLACEMENT_3D ( 'NONE', #32769, #228371, #112283 ) ;
#139098 = CARTESIAN_POINT ( 'NONE',  ( -21.00000000000000000, 8.000000000000000000, 1.212568896937007867 ) ) ;
#139099 = CARTESIAN_POINT ( 'NONE',  ( -18.50000000000000000, 77.35494420175976416, -241.6200040285045532 ) ) ;
#139101 = AXIS2_PLACEMENT_3D ( 'NONE', #55489, #120664, #77631 ) ;
#139100 = CARTESIAN_POINT ( 'NONE',  ( 22.00411653962158809, 7.253442868381323017, -133.9009618942314432 ) ) ;
#139102 = CARTESIAN_POINT ( 'NONE',  ( 20.21567752745066215, 65.80188589877963068, -61.64048713687273562 ) ) ;
#139103 = VERTEX_POINT ( 'NONE', #113002 ) ;
#139104 = VERTEX_POINT ( 'NONE', #174308 ) ;
#139105 = LINE ( 'NONE', #140418, #204276 ) ;
#139106 = AXIS2_PLACEMENT_3D ( 'NONE', #176152, #78294, #138261 ) ;
#139107 = DIRECTION ( 'NONE',  ( -0.000000000000000000, 0.8660254037844502539, 0.4999999999999799050 ) ) ;
#139109 = EDGE_CURVE ( 'NONE', #100439, #86243, #213595, .T. ) ;
#139108 = DIRECTION ( 'NONE',  ( 1.000000000000000000, 0.000000000000000000, 0.000000000000000000 ) ) ;
#139110 = CARTESIAN_POINT ( 'NONE',  ( 18.54999999999999716, 44.62608598762252399, -236.3940605665350745 ) ) ;
#139111 = CIRCLE ( 'NONE', #26738, 0.3999999999999994671 ) ;
#139112 = CARTESIAN_POINT ( 'NONE',  ( -16.94225986326250677, 23.23962418155415577, -231.0751721868350330 ) ) ;
#139113 = ORIENTED_EDGE ( 'NONE', *, *, #25256, .F. ) ;
#139114 = DIRECTION ( 'NONE',  ( 0.000000000000000000, 0.6728971962616697722, 0.7397360091702875895 ) ) ;
#139115 = TOROIDAL_SURFACE ( 'NONE', #197400, 0.2000000000000000111, 0.1000000000000000056 ) ;
#139116 = ADVANCED_FACE ( 'NONE', ( #192542 ), #173021, .T. ) ;
#139117 = EDGE_CURVE ( 'NONE', #92778, #230733, #134475, .T. ) ;
#139119 = CIRCLE ( 'NONE', #9972, 0.9000000000000014655 ) ;
#139118 = CARTESIAN_POINT ( 'NONE',  ( -17.04761207306819060, 10.02645087340892438, -113.1500000000000483 ) ) ;
#139120 = LINE ( 'NONE', #140427, #25615 ) ;
#139121 = AXIS2_PLACEMENT_3D ( 'NONE', #108066, #216133, #154919 ) ;
#139122 = VECTOR ( 'NONE', #99264, 1000.000000000000114 ) ;
#139123 = PRODUCT_DEFINITION_SHAPE ( 'NONE', 'NONE',  #258133 ) ;
#139124 = DIRECTION ( 'NONE',  ( -3.265361837132813093E-16, 1.000000000000000000, 0.000000000000000000 ) ) ;
#139125 = AXIS2_PLACEMENT_3D ( 'NONE', #152155, #30929, #15195 ) ;
#139126 = ADVANCED_FACE ( 'NONE', ( #133840 ), #205801, .T. ) ;
#139127 = EDGE_CURVE ( 'NONE', #120155, #201984, #113649, .T. ) ;
#139128 = VERTEX_POINT ( 'NONE', #209532 ) ;
#139129 = DIRECTION ( 'NONE',  ( 1.000000000000000000, 1.394253735153569469E-16, 2.602809386958778209E-16 ) ) ;
#139130 = VERTEX_POINT ( 'NONE', #249944 ) ;
#139131 = CARTESIAN_POINT ( 'NONE',  ( -20.54999999999999716, 74.00000000001259082, -190.7984855617622770 ) ) ;
#139132 = DIRECTION ( 'NONE',  ( -0.000000000000000000, 0.8814952561688430555, -0.4721928772777346239 ) ) ;
#139135 = EDGE_CURVE ( 'NONE', #160984, #254122, #22096, .T. ) ;
#139134 = CIRCLE ( 'NONE', #26772, 0.09999999999999939493 ) ;
#139133 = DIRECTION ( 'NONE',  ( 0.000000000000000000, 0.000000000000000000, -1.000000000000000000 ) ) ;
#139136 = DIRECTION ( 'NONE',  ( 0.000000000000000000, -0.9908441862701600211, -0.1350103645451876666 ) ) ;
#139137 = DIRECTION ( 'NONE',  ( -1.000000000000000000, 0.000000000000000000, -0.000000000000000000 ) ) ;
#139138 = DIRECTION ( 'NONE',  ( 0.000000000000000000, 0.000000000000000000, -1.000000000000000000 ) ) ;
#139139 = CARTESIAN_POINT ( 'NONE',  ( 23.24999999999999645, 53.62064951147646497, -235.8162552129080609 ) ) ;
#139140 = FACE_OUTER_BOUND ( 'NONE', #167283, .T. ) ;
#139141 = B_SPLINE_CURVE_WITH_KNOTS ( 'NONE', 3,
 ( #245257, #147431, #224386, #189126, #66615, #226967, #70499, #86137, #65317, #24939 ),
 .UNSPECIFIED., .F., .F.,
 ( 4, 3, 3, 4 ),
 ( 0.000000000000000000, 3.394313611811022212E-05, 6.779740500700426732E-05, 0.0001049857339142650257 ),
 .UNSPECIFIED. ) ;
#139142 = LINE ( 'NONE', #218690, #103843 ) ;
#139143 = AXIS2_PLACEMENT_3D ( 'NONE', #77735, #236819, #58167 ) ;
#139144 = EDGE_CURVE ( 'NONE', #205893, #126912, #191283, .T. ) ;
#139145 = CARTESIAN_POINT ( 'NONE',  ( -21.00000000000000000, -1.410778198689825347, -7.973296578895943121 ) ) ;
#139146 = DIRECTION ( 'NONE',  ( 1.000000000000000000, 0.000000000000000000, 0.000000000000000000 ) ) ;
#139147 = DIRECTION ( 'NONE',  ( -1.000000000000000000, -0.000000000000000000, -0.000000000000000000 ) ) ;
#139148 = EDGE_CURVE ( 'NONE', #235804, #130099, #55928, .T. ) ;
#139149 = EDGE_CURVE ( 'NONE', #122601, #175419, #76220, .T. ) ;
#139150 = VECTOR ( 'NONE', #146067, 1000.000000000000000 ) ;
#139151 = DIRECTION ( 'NONE',  ( -0.000000000000000000, 0.4721928772777346239, 0.8814952561688430555 ) ) ;
#139152 = CARTESIAN_POINT ( 'NONE',  ( 20.94999999999999929, 56.23643450586807546, -227.9054833905874204 ) ) ;
#139153 = CIRCLE ( 'NONE', #35177, 0.1000000000000043771 ) ;
#139154 = CIRCLE ( 'NONE', #6077, 0.1000000000000002554 ) ;
#139155 = VERTEX_POINT ( 'NONE', #81537 ) ;
#139156 = CARTESIAN_POINT ( 'NONE',  ( 21.13422380239043363, 6.493326514805634275, -9.351243737687475743E-16 ) ) ;
#139158 = EDGE_CURVE ( 'NONE', #114637, #183877, #22911, .T. ) ;
#139157 = CARTESIAN_POINT ( 'NONE',  ( 11.60000000000006004, 64.35000000001120668, -18.32310748452479388 ) ) ;
#139159 = CARTESIAN_POINT ( 'NONE',  ( 18.39999999999999858, 85.60000000001264198, -196.4910380878246201 ) ) ;
#139160 = APPLICATION_CONTEXT ( 'automotive_design' ) ;
#139161 = ORIENTED_EDGE ( 'NONE', *, *, #145100, .F. ) ;
#139162 = DIRECTION ( 'NONE',  ( 0.000000000000000000, -0.3738317757008748909, -0.9274965247785733613 ) ) ;
#139163 = EDGE_CURVE ( 'NONE', #220534, #12740, #119427, .T. ) ;
#139164 = ADVANCED_FACE ( 'NONE', ( #59399 ), #226638, .T. ) ;
#139165 = DIRECTION ( 'NONE',  ( 0.000000000000000000, 0.9788861828082167094, 0.2044060691544132835 ) ) ;
#139166 = ORIENTED_EDGE ( 'NONE', *, *, #14009, .F. ) ;
#139167 = DIRECTION ( 'NONE',  ( -1.000000000000000000, -0.000000000000000000, 0.000000000000000000 ) ) ;
#139168 = CARTESIAN_POINT ( 'NONE',  ( 22.59999985501178799, 31.79527822860963582, -238.8549629533907819 ) ) ;
#139169 = EDGE_CURVE ( 'NONE', #121414, #173153, #201699, .T. ) ;
#139170 = CIRCLE ( 'NONE', #26234, 0.1000000000000013933 ) ;
#139171 = ORIENTED_EDGE ( 'NONE', *, *, #91580, .T. ) ;
#139172 = VECTOR ( 'NONE', #30859, 1000.000000000000227 ) ;
#139173 = CIRCLE ( 'NONE', #185000, 0.09999999999999971412 ) ;
#139174 = ORIENTED_EDGE ( 'NONE', *, *, #11343, .F. ) ;
#139175 = DIRECTION ( 'NONE',  ( 0.000000000000000000, 0.000000000000000000, -1.000000000000000000 ) ) ;
#139176 =( BOUNDED_CURVE ( )  B_SPLINE_CURVE ( 3, ( #3615, #162718, #57157, #200542 ),
 .UNSPECIFIED., .F., .F. ) 
 B_SPLINE_CURVE_WITH_KNOTS ( ( 4, 4 ),
 ( 1.570796326794935860, 3.141592653589695416 ),
 .UNSPECIFIED. ) 
 CURVE ( )  GEOMETRIC_REPRESENTATION_ITEM ( )  RATIONAL_B_SPLINE_CURVE ( ( 1.000000000000000000, 0.8047378541243972450, 0.8047378541243972450, 1.000000000000000000 ) ) 
 REPRESENTATION_ITEM ( '' )  );
#139177 = ORIENTED_EDGE ( 'NONE', *, *, #101734, .F. ) ;
#139178 = EDGE_CURVE ( 'NONE', #95308, #141019, #180683, .T. ) ;
#139179 = FACE_OUTER_BOUND ( 'NONE', #159498, .T. ) ;
#139180 = ADVANCED_FACE ( 'NONE', ( #215927 ), #62023, .T. ) ;
#139181 = LINE ( 'NONE', #80475, #148918 ) ;
#139183 = LINE ( 'NONE', #77938, #224374 ) ;
#139182 = PRODUCT_DEFINITION_CONTEXT ( 'detailed design', #245812, 'design' ) ;
#139184 = CARTESIAN_POINT ( 'NONE',  ( -21.05000000000000071, 2.859758780633683273, -208.6670499591424459 ) ) ;
#139185 = DIRECTION ( 'NONE',  ( 0.000000000000000000, 0.4999999999999348299, -0.8660254037844762331 ) ) ;
#139186 = CARTESIAN_POINT ( 'NONE',  ( -12.47155713865592830, 47.30686838571506314, -234.5075185885025633 ) ) ;
#139187 = LINE ( 'NONE', #174550, #30336 ) ;
#139188 = CARTESIAN_POINT ( 'NONE',  ( -25.10847955711009760, 9.068702471349583405, -347.0000000000001137 ) ) ;
#139190 = ORIENTED_EDGE ( 'NONE', *, *, #206597, .T. ) ;
#139189 = CARTESIAN_POINT ( 'NONE',  ( -18.47079683080346513, -9.471664105233731590, -40.60886054099234599 ) ) ;
#139191 = ORIENTED_EDGE ( 'NONE', *, *, #111558, .T. ) ;
#139193 = DIRECTION ( 'NONE',  ( -1.000000000000000000, -0.000000000000000000, -0.000000000000000000 ) ) ;
#139192 = FACE_OUTER_BOUND ( 'NONE', #149820, .T. ) ;
#139196 = ORIENTED_EDGE ( 'NONE', *, *, #16754, .F. ) ;
#139195 = CARTESIAN_POINT ( 'NONE',  ( -16.97683809663752186, 61.13629130372252973, -220.3155949669961728 ) ) ;
#139194 = CARTESIAN_POINT ( 'NONE',  ( 20.95512820512820440, 65.37615131630072085, -191.3731074845244393 ) ) ;
#139197 = EDGE_LOOP ( 'NONE', ( #21877, #31587, #249319, #180767 ) ) ;
#139198 = LINE ( 'NONE', #41432, #33366 ) ;
#139199 = CARTESIAN_POINT ( 'NONE',  ( -23.25000000000000000, 33.22109292269086467, -247.7096104798602312 ) ) ;
#139200 = VECTOR ( 'NONE', #93686, 1000.000000000000000 ) ;
#139201 = CARTESIAN_POINT ( 'NONE',  ( 18.59999999999999787, -9.849999999999996092, 31.39999999999999858 ) ) ;
#139202 = CARTESIAN_POINT ( 'NONE',  ( 23.14999999999999858, 9.083024463225227052, -233.3070993219874083 ) ) ;
#139203 = CARTESIAN_POINT ( 'NONE',  ( -21.05000000000000071, -1.162701749926853712, -75.00000000000004263 ) ) ;
#139204 = FACE_OUTER_BOUND ( 'NONE', #53384, .T. ) ;
#139205 = DIRECTION ( 'NONE',  ( -0.7070776581708965169, 0.7071359030027827286, 4.937903618720407826E-15 ) ) ;
#139207 = ORIENTED_EDGE ( 'NONE', *, *, #97300, .T. ) ;
#139206 = EDGE_CURVE ( 'NONE', #87394, #170331, #56836, .T. ) ;
#139208 = VERTEX_POINT ( 'NONE', #37331 ) ;
#139209 = CARTESIAN_POINT ( 'NONE',  ( 18.59999999999999787, -1.835859311432481045, -212.5044391687984842 ) ) ;
#139210 = TOROIDAL_SURFACE ( 'NONE', #235118, 0.2000000000000000111, 0.1000000000000000056 ) ;
#139211 = EDGE_CURVE ( 'NONE', #120355, #217025, #201134, .T. ) ;
#139212 = CIRCLE ( 'NONE', #185035, 0.2000000000000042577 ) ;
#139213 = VERTEX_POINT ( 'NONE', #101077 ) ;
#139214 = FACE_OUTER_BOUND ( 'NONE', #181599, .T. ) ;
#139215 = ORIENTED_EDGE ( 'NONE', *, *, #237296, .T. ) ;
#139216 = CARTESIAN_POINT ( 'NONE',  ( -22.50000000000000000, 64.35042919246734527, -136.6231074845243825 ) ) ;
#139217 = AXIS2_PLACEMENT_3D ( 'NONE', #220246, #24630, #237231 ) ;
#139218 = CIRCLE ( 'NONE', #185041, 0.09999999999999438505 ) ;
#139219 = DIRECTION ( 'NONE',  ( -3.440080580676165868E-14, -0.1298341882520124002, -0.9915357197604841577 ) ) ;
#139220 = DIRECTION ( 'NONE',  ( -1.000000000000000000, -0.000000000000000000, -0.000000000000000000 ) ) ;
#139221 = DIRECTION ( 'NONE',  ( 1.000000000000000000, 0.000000000000000000, 0.000000000000000000 ) ) ;
#139222 = DIRECTION ( 'NONE',  ( 0.000000000000000000, 0.000000000000000000, -1.000000000000000000 ) ) ;
#139223 = EDGE_LOOP ( 'NONE', ( #125813, #3271, #208874, #93857 ) ) ;
#139224 = CARTESIAN_POINT ( 'NONE',  ( 20.94999999999999929, 77.07318729351892728, -199.5660544101962728 ) ) ;
#139225 = DIRECTION ( 'NONE',  ( 0.000000000000000000, 6.982962677686266711E-15, -1.000000000000000000 ) ) ;
#139226 = CYLINDRICAL_SURFACE ( 'NONE', #231468, 0.09999999999999939493 ) ;
#139228 = CIRCLE ( 'NONE', #89180, 0.5000000000000004441 ) ;
#139227 = DIRECTION ( 'NONE',  ( 1.000000000000000000, -0.000000000000000000, -0.000000000000000000 ) ) ;
#139229 = DIRECTION ( 'NONE',  ( 0.000000000000000000, 0.2617529984165031243, 0.9651348961777157509 ) ) ;
#139230 = EDGE_CURVE ( 'NONE', #151730, #237924, #122624, .T. ) ;
#139231 = ORIENTED_EDGE ( 'NONE', *, *, #96091, .F. ) ;
#139232 = DIRECTION ( 'NONE',  ( -1.000000000000000000, -0.000000000000000000, -0.000000000000000000 ) ) ;
#139234 = ORIENTED_EDGE ( 'NONE', *, *, #180682, .T. ) ;
#139233 = AXIS2_PLACEMENT_3D ( 'NONE', #55950, #132963, #251609 ) ;
#139236 = ORIENTED_EDGE ( 'NONE', *, *, #257903, .T. ) ;
#139235 = CARTESIAN_POINT ( 'NONE',  ( 21.05000000000000071, 28.08470566095357057, -239.2860081655328770 ) ) ;
#139237 = DIRECTION ( 'NONE',  ( 1.000000000000000000, -0.000000000000000000, 0.000000000000000000 ) ) ;
#139238 = CIRCLE ( 'NONE', #168540, 7.900000000000000355 ) ;
#139239 = AXIS2_PLACEMENT_3D ( 'NONE', #89580, #184832, #209543 ) ;
#139240 = DIRECTION ( 'NONE',  ( -3.035766082959430717E-14, 0.000000000000000000, -1.000000000000000000 ) ) ;
#139241 = ORIENTED_EDGE ( 'NONE', *, *, #91490, .T. ) ;
#139243 = CARTESIAN_POINT ( 'NONE',  ( 18.37172112093866971, 85.57096165225503626, -129.7063730310401297 ) ) ;
#139242 = AXIS2_PLACEMENT_3D ( 'NONE', #47100, #67970, #109651 ) ;
#139244 = LINE ( 'NONE', #140542, #207212 ) ;
#139245 = FACE_OUTER_BOUND ( 'NONE', #203682, .T. ) ;
#139247 = ORIENTED_EDGE ( 'NONE', *, *, #74093, .T. ) ;
#139246 = DIRECTION ( 'NONE',  ( 1.000000000000000000, 0.000000000000000000, 0.000000000000000000 ) ) ;
#139248 = AXIS2_PLACEMENT_3D ( 'NONE', #248124, #168648, #246833 ) ;
#139249 = CIRCLE ( 'NONE', #210032, 0.09999999999999609201 ) ;
#139250 = CARTESIAN_POINT ( 'NONE',  ( 23.14999999999999858, -3.999999999988843147, -200.9999999999999432 ) ) ;
#139251 = VECTOR ( 'NONE', #73817, 1000.000000000000000 ) ;
#139252 = ORIENTED_EDGE ( 'NONE', *, *, #6370, .T. ) ;
#139253 = DIRECTION ( 'NONE',  ( -0.000000000000000000, 1.000000000000000000, -0.000000000000000000 ) ) ;
#139254 = CYLINDRICAL_SURFACE ( 'NONE', #36927, 0.09999999999999892308 ) ;
#139255 = CIRCLE ( 'NONE', #97556, 0.09999999999998898659 ) ;
#139256 = DIRECTION ( 'NONE',  ( 0.000000000000000000, 0.000000000000000000, -1.000000000000000000 ) ) ;
#139257 = ORIENTED_EDGE ( 'NONE', *, *, #239062, .T. ) ;
#139258 = DIRECTION ( 'NONE',  ( -1.836970198721029934E-16, 1.000000000000000000, 0.000000000000000000 ) ) ;
#139259 = ORIENTED_EDGE ( 'NONE', *, *, #99096, .F. ) ;
#139260 = LINE ( 'NONE', #244791, #2234 ) ;
#139261 = VECTOR ( 'NONE', #28355, 1000.000000000000114 ) ;
#139262 = CYLINDRICAL_SURFACE ( 'NONE', #230761, 0.1000000000000028644 ) ;
#139263 = CARTESIAN_POINT ( 'NONE',  ( 22.39999999999999503, 11.75000000001115552, -133.9000000000000057 ) ) ;
#139264 = ORIENTED_EDGE ( 'NONE', *, *, #146673, .T. ) ;
#139265 = CARTESIAN_POINT ( 'NONE',  ( -18.59999999999999787, 66.75000000001199396, -115.3731074845243683 ) ) ;
#139266 = AXIS2_PLACEMENT_3D ( 'NONE', #85678, #244778, #148259 ) ;
#139267 = EDGE_CURVE ( 'NONE', #249181, #114887, #77699, .T. ) ;
#139269 = AXIS2_PLACEMENT_3D ( 'NONE', #192419, #33379, #249825 ) ;
#139268 = DIRECTION ( 'NONE',  ( -1.000000000000000000, -1.652117596168391700E-15, -1.153667551319263085E-29 ) ) ;
#139270 = CARTESIAN_POINT ( 'NONE',  ( -20.99780126800916591, 64.39461131213593603, -176.9357549128189362 ) ) ;
#139271 = EDGE_CURVE ( 'NONE', #158894, #46909, #114221, .T. ) ;
#139272 = ORIENTED_EDGE ( 'NONE', *, *, #90325, .T. ) ;
#139273 = CARTESIAN_POINT ( 'NONE',  ( 18.59999999999999076, 65.50857864377465489, -111.6731074845243796 ) ) ;
#139274 = CARTESIAN_POINT ( 'NONE',  ( 20.94999999999999929, 69.45000000001229523, -157.8731074845244109 ) ) ;
#139275 = ORIENTED_EDGE ( 'NONE', *, *, #169020, .F. ) ;
#139276 = CARTESIAN_POINT ( 'NONE',  ( 20.85000000000000142, -11.74999999998883560, -164.6000000000000227 ) ) ;
#139277 = ORIENTED_EDGE ( 'NONE', *, *, #150665, .T. ) ;
#139278 =( BOUNDED_CURVE ( )  B_SPLINE_CURVE ( 3, ( #179517, #154825, #119540, #59511 ),
 .UNSPECIFIED., .F., .T. ) 
 B_SPLINE_CURVE_WITH_KNOTS ( ( 4, 4 ),
 ( 3.192897208853993529, 4.712388980384689674 ),
 .UNSPECIFIED. ) 
 CURVE ( )  GEOMETRIC_REPRESENTATION_ITEM ( )  RATIONAL_B_SPLINE_CURVE ( ( 1.000000000000000000, 0.8166740347213228279, 0.8166740347213228279, 1.000000000000000000 ) ) 
 REPRESENTATION_ITEM ( '' )  );
#139279 = EDGE_CURVE ( 'NONE', #96257, #59994, #122024, .T. ) ;
#139280 = CYLINDRICAL_SURFACE ( 'NONE', #237557, 0.09999999999999939493 ) ;
#139281 = ORIENTED_EDGE ( 'NONE', *, *, #231383, .T. ) ;
#139283 = ORIENTED_EDGE ( 'NONE', *, *, #130601, .F. ) ;
#139282 = LINE ( 'NONE', #141867, #122070 ) ;
#139284 = EDGE_CURVE ( 'NONE', #208590, #246420, #78970, .T. ) ;
#139287 = ORIENTED_EDGE ( 'NONE', *, *, #10788, .F. ) ;
#139286 = EDGE_LOOP ( 'NONE', ( #39433, #96040, #168916, #110083 ) ) ;
#139285 = CARTESIAN_POINT ( 'NONE',  ( 20.05000000000002913, 11.52084357182977570, -219.8296352432475942 ) ) ;
#139288 = CIRCLE ( 'NONE', #47721, 0.09999999999999939493 ) ;
#139289 = FACE_OUTER_BOUND ( 'NONE', #250674, .T. ) ;
#139290 = CARTESIAN_POINT ( 'NONE',  ( -21.13498764882296044, 0.001656394742484908677, -161.0043818565260096 ) ) ;
#139291 = CIRCLE ( 'NONE', #185113, 0.1000000000000014488 ) ;
#139292 = DIRECTION ( 'NONE',  ( 0.000000000000000000, -1.000000000000000000, -6.982962677686266711E-15 ) ) ;
#139293 = EDGE_CURVE ( 'NONE', #25027, #193635, #188660, .T. ) ;
#139294 = DIRECTION ( 'NONE',  ( 0.000000000000000000, -1.000000000000000000, -6.982962677686266711E-15 ) ) ;
#139295 = DIRECTION ( 'NONE',  ( 0.000000000000000000, -0.4230464831072829335, 0.9061079809440810706 ) ) ;
#139296 = CIRCLE ( 'NONE', #89427, 7.900000000000013678 ) ;
#139297 = CARTESIAN_POINT ( 'NONE',  ( 20.95512820512820085, 65.37615131630074927, -195.8581939154368285 ) ) ;
#139298 = CARTESIAN_POINT ( 'NONE',  ( 21.05000000000000071, 5.500000000011153745, -188.5947339810868755 ) ) ;
#139300 = CARTESIAN_POINT ( 'NONE',  ( -21.05000000000000071, 18.18127959618848166, -237.5711165786817389 ) ) ;
#139299 = DIRECTION ( 'NONE',  ( 0.000000000000000000, -0.9770955615653551529, -0.2128009952262517601 ) ) ;
#139301 = ORIENTED_EDGE ( 'NONE', *, *, #187639, .T. ) ;
#139303 = VERTEX_POINT ( 'NONE', #717 ) ;
#139302 = CIRCLE ( 'NONE', #39406, 0.09999999999998712696 ) ;
#139304 = CARTESIAN_POINT ( 'NONE',  ( 23.14999999999999503, 11.65000000001116298, -93.58519422934611498 ) ) ;
#139305 = AXIS2_PLACEMENT_3D ( 'NONE', #23002, #64659, #145474 ) ;
#139307 = ORIENTED_EDGE ( 'NONE', *, *, #89458, .T. ) ;
#139306 = DIRECTION ( 'NONE',  ( 1.000000000000000000, 0.000000000000000000, 0.000000000000000000 ) ) ;
#139308 = CARTESIAN_POINT ( 'NONE',  ( 20.84999999999999787, 64.25000000001175238, -76.44225473048308572 ) ) ;
#139309 = VERTEX_POINT ( 'NONE', #257578 ) ;
#139310 = EDGE_CURVE ( 'NONE', #122787, #241009, #132969, .T. ) ;
#139311 = ORIENTED_EDGE ( 'NONE', *, *, #42913, .F. ) ;
#139312 = DIRECTION ( 'NONE',  ( 0.000000000000000000, 0.8814952561688444987, -0.4721928772777320149 ) ) ;
#139313 = VECTOR ( 'NONE', #29220, 999.9999999999998863 ) ;
#139314 = AXIS2_PLACEMENT_3D ( 'NONE', #88023, #167613, #247112 ) ;
#139315 = AXIS2_PLACEMENT_3D ( 'NONE', #248539, #228988, #86873 ) ;
#139316 = VERTEX_POINT ( 'NONE', #144093 ) ;
#139317 = CIRCLE ( 'NONE', #147723, 0.09999999999999939493 ) ;
#139318 = CARTESIAN_POINT ( 'NONE',  ( -16.94165728009537020, 66.01213024408802710, -82.13205247601418080 ) ) ;
#139319 = FACE_OUTER_BOUND ( 'NONE', #67777, .T. ) ;
#139321 = ORIENTED_EDGE ( 'NONE', *, *, #191581, .F. ) ;
#139320 = ORIENTED_EDGE ( 'NONE', *, *, #16719, .T. ) ;
#139322 = EDGE_LOOP ( 'NONE', ( #61497, #253391, #18141, #97844 ) ) ;
#139323 = DIRECTION ( 'NONE',  ( 0.000000000000000000, 0.2128009952263605342, -0.9770955615653315052 ) ) ;
#139324 = VERTEX_POINT ( 'NONE', #43731 ) ;
#139325 = ORIENTED_EDGE ( 'NONE', *, *, #192639, .F. ) ;
#139326 = FACE_OUTER_BOUND ( 'NONE', #18828, .T. ) ;
#139328 = EDGE_LOOP ( 'NONE', ( #77122, #165396, #180940, #116823 ) ) ;
#139327 = DIRECTION ( 'NONE',  ( 2.952720810173289112E-16, 1.000000000000000000, 6.982962677686266711E-15 ) ) ;
#139329 = AXIS2_PLACEMENT_3D ( 'NONE', #108384, #49685, #210061 ) ;
#139331 = CARTESIAN_POINT ( 'NONE',  ( -23.15000000000000213, 11.75000000001115552, -193.9851942293460070 ) ) ;
#139330 = CARTESIAN_POINT ( 'NONE',  ( -23.25000000000000000, 71.65000000001253966, -182.3731074845244109 ) ) ;
#139332 = FACE_OUTER_BOUND ( 'NONE', #25212, .T. ) ;
#139333 = DIRECTION ( 'NONE',  ( 1.000000000000000000, 0.000000000000000000, 0.000000000000000000 ) ) ;
#139334 = ORIENTED_EDGE ( 'NONE', *, *, #209252, .T. ) ;
#139335 = ORIENTED_EDGE ( 'NONE', *, *, #49242, .T. ) ;
#139336 = CARTESIAN_POINT ( 'NONE',  ( -20.54999999999999716, -9.499999999988846255, -191.1060308773475356 ) ) ;
#139337 = TOROIDAL_SURFACE ( 'NONE', #172731, 0.6000000000000009770, 0.1000000000000000056 ) ;
#139338 = LINE ( 'NONE', #199351, #139426 ) ;
#139339 = DIRECTION ( 'NONE',  ( -1.000000000000000000, 0.000000000000000000, 0.000000000000000000 ) ) ;
#139340 = VERTEX_POINT ( 'NONE', #146656 ) ;
#139341 = CARTESIAN_POINT ( 'NONE',  ( 20.94999999999999929, 77.83585931145526615, -58.01866831572577610 ) ) ;
#139342 = TOROIDAL_SURFACE ( 'NONE', #10210, 0.2000000000000000111, 0.1000000000000000056 ) ;
#139343 = AXIS2_PLACEMENT_3D ( 'NONE', #45366, #141893, #46627 ) ;
#139344 = EDGE_CURVE ( 'NONE', #203753, #186169, #109544, .T. ) ;
#139345 = LINE ( 'NONE', #141927, #247037 ) ;
#139346 = AXIS2_PLACEMENT_3D ( 'NONE', #247903, #189227, #230934 ) ;
#139347 = DIRECTION ( 'NONE',  ( 1.000000000000000000, 0.000000000000000000, 0.000000000000000000 ) ) ;
#139348 = EDGE_LOOP ( 'NONE', ( #94385, #160126, #9471, #115008 ) ) ;
#139349 = ORIENTED_EDGE ( 'NONE', *, *, #232288, .F. ) ;
#139350 = DIRECTION ( 'NONE',  ( 1.000000000000000000, 0.000000000000000000, 0.000000000000000000 ) ) ;
#139351 = DIRECTION ( 'NONE',  ( 1.000000000000000000, 0.000000000000000000, 0.000000000000000000 ) ) ;
#139352 = ORIENTED_EDGE ( 'NONE', *, *, #208019, .T. ) ;
#139353 = CARTESIAN_POINT ( 'NONE',  ( 21.87500000000000355, 9.749999999999998224, -21.25000000000000000 ) ) ;
#139354 = EDGE_LOOP ( 'NONE', ( #39628, #147320, #73914, #188258 ) ) ;
#139355 = DIRECTION ( 'NONE',  ( 0.7071067811865475727, -0.7071067811865475727, -5.142139384388981164E-15 ) ) ;
#139357 = ADVANCED_FACE ( 'NONE', ( #127117 ), #46282, .T. ) ;
#139356 = CARTESIAN_POINT ( 'NONE',  ( 19.90000000000000924, 4.513204987021263825, 22.00000000000000355 ) ) ;
#139358 = DIRECTION ( 'NONE',  ( 0.000000000000000000, -0.9915357197604971473, 0.1298341882519111479 ) ) ;
#139359 = CARTESIAN_POINT ( 'NONE',  ( 22.48508240969612615, 0.04627641452807085970, -55.34998926842647649 ) ) ;
#139360 = CARTESIAN_POINT ( 'NONE',  ( 23.15000000000000213, -8.596261682231833845, -109.9501275171503210 ) ) ;
#139361 = EDGE_CURVE ( 'NONE', #250224, #91092, #230349, .T. ) ;
#139362 = EDGE_CURVE ( 'NONE', #242093, #154034, #55528, .T. ) ;
#139363 = EDGE_LOOP ( 'NONE', ( #210877, #154066, #13563, #57074 ) ) ;
#139364 = DIRECTION ( 'NONE',  ( -0.000000000000000000, 1.000000000000000000, -0.000000000000000000 ) ) ;
#139365 = CIRCLE ( 'NONE', #218468, 0.1000000000000017680 ) ;
#139367 = ORIENTED_EDGE ( 'NONE', *, *, #10817, .T. ) ;
#139366 = EDGE_LOOP ( 'NONE', ( #66658, #255916, #174975, #169252 ) ) ;
#139368 = ORIENTED_EDGE ( 'NONE', *, *, #20650, .F. ) ;
#139369 = CARTESIAN_POINT ( 'NONE',  ( -16.94275863009466576, 66.01050395134991788, -157.4148048665655608 ) ) ;
#139370 = LINE ( 'NONE', #241085, #190685 ) ;
#139371 = VECTOR ( 'NONE', #45827, 1000.000000000000000 ) ;
#139372 = DIRECTION ( 'NONE',  ( 0.000000000000000000, 0.000000000000000000, -1.000000000000000000 ) ) ;
#139373 = DIRECTION ( 'NONE',  ( 1.000000000000000000, -0.000000000000000000, -0.000000000000000000 ) ) ;
#139374 = CARTESIAN_POINT ( 'NONE',  ( -18.42554971533678199, -9.497159669426592288, -107.5398269135486800 ) ) ;
#139375 = EDGE_CURVE ( 'NONE', #150422, #144467, #105426, .T. ) ;
#139377 = CARTESIAN_POINT ( 'NONE',  ( -14.23072895065542909, 66.54401276639910634, -88.01157631762657729 ) ) ;
#139376 = CARTESIAN_POINT ( 'NONE',  ( 20.72390388899083646, 10.58996311842368243, -7.511348295744856074 ) ) ;
#139378 = ORIENTED_EDGE ( 'NONE', *, *, #158264, .F. ) ;
#139379 = CARTESIAN_POINT ( 'NONE',  ( -18.59999999999999787, 7.021664781911246322, -137.6335654018973287 ) ) ;
#139380 = VERTEX_POINT ( 'NONE', #241919 ) ;
#139381 = EDGE_CURVE ( 'NONE', #10156, #4179, #97035, .T. ) ;
#139382 = DIRECTION ( 'NONE',  ( 0.000000000000000000, 0.000000000000000000, -1.000000000000000000 ) ) ;
#139383 = ORIENTED_EDGE ( 'NONE', *, *, #67992, .F. ) ;
#139384 = VERTEX_POINT ( 'NONE', #124564 ) ;
#139385 = CARTESIAN_POINT ( 'NONE',  ( 20.94999999999999929, -1.164121893230052995, -108.4148480855716485 ) ) ;
#139386 = DIRECTION ( 'NONE',  ( 1.000000000000000000, 0.000000000000000000, 0.000000000000000000 ) ) ;
#139387 = DIRECTION ( 'NONE',  ( -2.952720810173287633E-16, 0.9770955615653312831, 0.2128009952263610616 ) ) ;
#139388 = CARTESIAN_POINT ( 'NONE',  ( 13.12220780326571123, 9.430633469083950615, -82.23176579482412762 ) ) ;
#139389 = TOROIDAL_SURFACE ( 'NONE', #214407, 0.2000000000000000111, 0.1000000000000000056 ) ;
#139390 = CARTESIAN_POINT ( 'NONE',  ( 18.49999999999998934, 9.125777775466493935, -211.6520035670780544 ) ) ;
#139391 = ORIENTED_EDGE ( 'NONE', *, *, #15675, .F. ) ;
#139392 = ORIENTED_EDGE ( 'NONE', *, *, #155117, .T. ) ;
#139393 = ADVANCED_FACE ( 'NONE', ( #222334 ), #104948, .T. ) ;
#139394 = CARTESIAN_POINT ( 'NONE',  ( -21.14999999999999858, -0.09999999998884338825, -94.25000000000002842 ) ) ;
#139396 = ORIENTED_EDGE ( 'NONE', *, *, #201848, .F. ) ;
#139395 = ADVANCED_FACE ( 'NONE', ( #25467 ), #255241, .F. ) ;
#139397 = CYLINDRICAL_SURFACE ( 'NONE', #93903, 0.1000000000000028644 ) ;
#139398 = CARTESIAN_POINT ( 'NONE',  ( -16.94275863009466576, 9.989496048673542461, -46.10830261795888418 ) ) ;
#139399 = ADVANCED_FACE ( 'NONE', ( #166283 ), #45016, .F. ) ;
#139400 = DIRECTION ( 'NONE',  ( 1.000000000000000000, 0.000000000000000000, 0.000000000000000000 ) ) ;
#139401 = CARTESIAN_POINT ( 'NONE',  ( 13.40000000000000036, -9.650000000000002132, 17.60000000000000497 ) ) ;
#139402 = CARTESIAN_POINT ( 'NONE',  ( 21.17356465864818915, 0.09891124102502621418, -60.57719687375832507 ) ) ;
#139403 = CARTESIAN_POINT ( 'NONE',  ( -21.05000000000000071, 0.03363273533364569134, 6.258817194681472351 ) ) ;
#139405 = DIRECTION ( 'NONE',  ( 0.000000000000000000, -0.2128009952263604232, 0.9770955615653316162 ) ) ;
#139404 = CARTESIAN_POINT ( 'NONE',  ( 21.05000000000000071, 1.115600667400684642E-11, -200.9999999999999432 ) ) ;
#139406 = CARTESIAN_POINT ( 'NONE',  ( 18.39999999999999858, -7.785976468740638090, -209.8926132507865816 ) ) ;
#139407 = CARTESIAN_POINT ( 'NONE',  ( 18.56308993302918964, 65.61930884468881686, -178.7838848455861580 ) ) ;
#139408 = CYLINDRICAL_SURFACE ( 'NONE', #33119, 0.09999999999999939493 ) ;
#139409 = AXIS2_PLACEMENT_3D ( 'NONE', #107857, #8769, #49170 ) ;
#139410 = CARTESIAN_POINT ( 'NONE',  ( -20.85000000000000142, 68.97833521811131163, -32.28954208262708647 ) ) ;
#139411 = CIRCLE ( 'NONE', #10264, 0.09999999999999939493 ) ;
#139412 = AXIS2_PLACEMENT_3D ( 'NONE', #168979, #69854, #225028 ) ;
#139413 = CIRCLE ( 'NONE', #197677, 0.1999999999999987899 ) ;
#139414 = ORIENTED_EDGE ( 'NONE', *, *, #207935, .T. ) ;
#139415 = MECHANICAL_DESIGN_GEOMETRIC_PRESENTATION_REPRESENTATION (  '', ( #97888 ), #106444 ) ;
#139416 = CARTESIAN_POINT ( 'NONE',  ( 19.97071067811864609, 64.27928932189311695, -78.37310748452439668 ) ) ;
#139417 = ORIENTED_EDGE ( 'NONE', *, *, #252410, .T. ) ;
#139418 = CARTESIAN_POINT ( 'NONE',  ( 20.94999999999999929, 11.65000000001115943, -93.71613433702195550 ) ) ;
#139419 = CARTESIAN_POINT ( 'NONE',  ( -18.35663730107557257, 11.47390742652235573, -109.7500000000000426 ) ) ;
#139420 =( NAMED_UNIT ( * ) SI_UNIT ( $, .STERADIAN. ) SOLID_ANGLE_UNIT ( ) );
#139421 = ORIENTED_EDGE ( 'NONE', *, *, #73362, .F. ) ;
#139422 = EDGE_CURVE ( 'NONE', #95768, #197421, #109726, .T. ) ;
#139423 = DIRECTION ( 'NONE',  ( 0.000000000000000000, 0.1568667991644863147, -0.9876197685951252359 ) ) ;
#139424 = DIRECTION ( 'NONE',  ( 1.000000000000000000, -0.000000000000000000, -0.000000000000000000 ) ) ;
#139425 = CARTESIAN_POINT ( 'NONE',  ( 22.49999999999999645, 0.08880997639808872746, -21.85023708196807846 ) ) ;
#139426 = VECTOR ( 'NONE', #78090, 1000.000000000000227 ) ;
#139427 = DIRECTION ( 'NONE',  ( 1.000000000000000000, 0.000000000000000000, 0.000000000000000000 ) ) ;
#139428 = TOROIDAL_SURFACE ( 'NONE', #122726, 0.2000000000000000111, 0.1000000000000000056 ) ;
#139429 = CARTESIAN_POINT ( 'NONE',  ( -20.94999999999999929, -1.164121893230052995, -208.9148480855715775 ) ) ;
#139430 = CARTESIAN_POINT ( 'NONE',  ( 20.99999999999997868, 0.000000000000000000, 0.000000000000000000 ) ) ;
#139431 = AXIS2_PLACEMENT_3D ( 'NONE', #214052, #35454, #46946 ) ;
#139432 = AXIS2_PLACEMENT_3D ( 'NONE', #75398, #53238, #170671 ) ;
#139433 = ORIENTED_EDGE ( 'NONE', *, *, #57389, .F. ) ;
#139434 = CYLINDRICAL_SURFACE ( 'NONE', #212132, 0.09999999999998898659 ) ;
#139436 = ORIENTED_EDGE ( 'NONE', *, *, #168069, .T. ) ;
#139435 = DIRECTION ( 'NONE',  ( -1.000000000000000000, -0.000000000000000000, 0.000000000000000000 ) ) ;
#139437 = CARTESIAN_POINT ( 'NONE',  ( 23.14999999999999858, 7.128833340093095217, -233.7327013124392749 ) ) ;
#139438 = EDGE_CURVE ( 'NONE', #198825, #63545, #242825, .T. ) ;
#139439 = CARTESIAN_POINT ( 'NONE',  ( -22.24259225415828567, 68.50806212944695517, -170.1221733679772115 ) ) ;
#139440 = CARTESIAN_POINT ( 'NONE',  ( 21.14999999999999503, 11.65000000001116298, -167.5999999999999659 ) ) ;
#139441 = ORIENTED_EDGE ( 'NONE', *, *, #142453, .F. ) ;
#139442 = DIRECTION ( 'NONE',  ( 0.000000000000000000, 1.000000000000000000, 6.982962677686266711E-15 ) ) ;
#139443 = AXIS2_PLACEMENT_3D ( 'NONE', #195343, #11565, #114497 ) ;
#139444 = EDGE_CURVE ( 'NONE', #254691, #254440, #47175, .T. ) ;
#139445 = SHAPE_DEFINITION_REPRESENTATION ( #132765, #205135 ) ;
#139446 = AXIS2_PLACEMENT_3D ( 'NONE', #87225, #49405, #147216 ) ;
#139447 = AXIS2_PLACEMENT_3D ( 'NONE', #163308, #81170, #125466 ) ;
#139448 = DIRECTION ( 'NONE',  ( 1.000000000000000000, -7.304098846218134667E-16, 0.000000000000000000 ) ) ;
#139449 = ORIENTED_EDGE ( 'NONE', *, *, #138511, .T. ) ;
#139451 = EDGE_CURVE ( 'NONE', #89189, #140686, #30444, .T. ) ;
#139450 = DIRECTION ( 'NONE',  ( 2.952720810173289112E-16, -1.000000000000000000, -0.000000000000000000 ) ) ;
#139452 = DIRECTION ( 'NONE',  ( -0.000000000000000000, 0.8814952561688430555, -0.4721928772777346239 ) ) ;
#139453 = CIRCLE ( 'NONE', #26486, 2.100000000000002309 ) ;
#139454 = EDGE_CURVE ( 'NONE', #105012, #240054, #151274, .T. ) ;
#139455 = CIRCLE ( 'NONE', #206114, 11.80000000000000426 ) ;
#139456 = EDGE_CURVE ( 'NONE', #103887, #117101, #143028, .T. ) ;
#139457 = CYLINDRICAL_SURFACE ( 'NONE', #99405, 0.09999999999999986677 ) ;
#139459 = ORIENTED_EDGE ( 'NONE', *, *, #25811, .T. ) ;
#139458 =( GEOMETRIC_REPRESENTATION_CONTEXT ( 3 ) GLOBAL_UNCERTAINTY_ASSIGNED_CONTEXT ( ( #11258 ) ) GLOBAL_UNIT_ASSIGNED_CONTEXT ( ( #33384, #150728, #111602 ) ) REPRESENTATION_CONTEXT ( 'NONE', 'WORKASPACE' ) );
#139460 = ORIENTED_EDGE ( 'NONE', *, *, #141799, .T. ) ;
#139461 = CARTESIAN_POINT ( 'NONE',  ( -16.97683809663752186, 9.950000000011138823, -113.9023640181965220 ) ) ;
#139462 = VECTOR ( 'NONE', #214034, 1000.000000000000000 ) ;
#139463 = CARTESIAN_POINT ( 'NONE',  ( 23.14999999999998437, 71.95000000001267892, -203.5231074845243597 ) ) ;
#139464 = VECTOR ( 'NONE', #141788, 1000.000000000000000 ) ;
#139465 = CARTESIAN_POINT ( 'NONE',  ( -16.94445028196807002, 30.26380394232451465, -234.7901145182196956 ) ) ;
#139466 = SPHERICAL_SURFACE ( 'NONE', #44411, 0.1000000000000000056 ) ;
#139467 = CARTESIAN_POINT ( 'NONE',  ( -18.40000000000000213, 64.66825945288641719, -56.87310748452440379 ) ) ;
#139468 = CARTESIAN_POINT ( 'NONE',  ( 20.94999999999999929, 4.252251777740766236, -211.8999245327126744 ) ) ;
#139470 = DIRECTION ( 'NONE',  ( 0.000000000000000000, -0.2617529984165013479, -0.9651348961777163060 ) ) ;
#139469 = DIRECTION ( 'NONE',  ( 0.000000000000000000, -0.8660254037844247188, 0.5000000000000245359 ) ) ;
#139471 = CARTESIAN_POINT ( 'NONE',  ( -21.14999999999999858, 1.115600667400684642E-11, -60.45934304829880546 ) ) ;
#139472 = CARTESIAN_POINT ( 'NONE',  ( -20.54999999999999716, -8.999999999988846255, -76.89396912265249284 ) ) ;
#139473 = CARTESIAN_POINT ( 'NONE',  ( 18.59999999999996945, 65.66751761918619934, -30.42826094061123854 ) ) ;
#139474 = CARTESIAN_POINT ( 'NONE',  ( -23.15000000000000213, 64.35000000001245724, -181.7731074845244450 ) ) ;
#139475 = ORIENTED_EDGE ( 'NONE', *, *, #230813, .F. ) ;
#139476 = EDGE_CURVE ( 'NONE', #28264, #99799, #252189, .T. ) ;
#139477 = ORIENTED_EDGE ( 'NONE', *, *, #83834, .T. ) ;
#139478 = EDGE_CURVE ( 'NONE', #151389, #236311, #34474, .T. ) ;
#139479 = DIRECTION ( 'NONE',  ( 0.7071359030028202541, 0.6452843503173477657, 0.2890794387705640789 ) ) ;
#139481 = CARTESIAN_POINT ( 'NONE',  ( -23.25000000000000000, 7.128833340094563376, -233.7327013124401276 ) ) ;
#139480 = DIRECTION ( 'NONE',  ( 0.000000000000000000, 0.000000000000000000, -1.000000000000000000 ) ) ;
#139482 = CARTESIAN_POINT ( 'NONE',  ( -18.59999999999999787, 77.83534155023670564, -158.4679561919613491 ) ) ;
#139484 = ADVANCED_FACE ( 'NONE', ( #134798 ), #151849, .T. ) ;
#139483 = DIRECTION ( 'NONE',  ( 0.000000000000000000, 0.000000000000000000, 1.000000000000000000 ) ) ;
#139485 = CARTESIAN_POINT ( 'NONE',  ( 21.72449340488910252, 10.28395627750227703, -180.1499999999999773 ) ) ;
#139486 = VERTEX_POINT ( 'NONE', #192248 ) ;
#139487 = CARTESIAN_POINT ( 'NONE',  ( -23.15000000000000213, 23.68770167995059595, -252.8127582590406348 ) ) ;
#139488 = VERTEX_POINT ( 'NONE', #209219 ) ;
#139489 = CIRCLE ( 'NONE', #256138, 0.1000000000000028644 ) ;
#139490 = EDGE_CURVE ( 'NONE', #76616, #60113, #147153, .T. ) ;
#139491 = VECTOR ( 'NONE', #55847, 1000.000000000000000 ) ;
#139492 = CARTESIAN_POINT ( 'NONE',  ( -16.89318236219977010, 51.62291660267955962, -231.9429707449544082 ) ) ;
#139493 = ORIENTED_EDGE ( 'NONE', *, *, #133750, .F. ) ;
#139494 = DIRECTION ( 'NONE',  ( 1.000000000000000000, 0.000000000000000000, -0.000000000000000000 ) ) ;
#139495 = VECTOR ( 'NONE', #76702, 1000.000000000000000 ) ;
#139496 = EDGE_CURVE ( 'NONE', #78948, #124831, #30612, .T. ) ;
#139497 = DIRECTION ( 'NONE',  ( 0.000000000000000000, 0.9908441862701596881, -0.1350103645451904977 ) ) ;
#139498 = CIRCLE ( 'NONE', #206154, 0.5000000000000004441 ) ;
#139499 = EDGE_CURVE ( 'NONE', #127649, #141595, #205389, .T. ) ;
#139500 = CIRCLE ( 'NONE', #27120, 0.1000000000000028644 ) ;
#139501 = EDGE_LOOP ( 'NONE', ( #99322, #250029, #254268 ) ) ;
#139502 = DIRECTION ( 'NONE',  ( 0.000000000000000000, 0.000000000000000000, -1.000000000000000000 ) ) ;
#139503 = ORIENTED_EDGE ( 'NONE', *, *, #91118, .F. ) ;
#139504 = LINE ( 'NONE', #121284, #99518 ) ;
#139505 = ADVANCED_FACE ( 'NONE', ( #149276 ), #213070, .F. ) ;
#139507 = AXIS2_PLACEMENT_3D ( 'NONE', #46047, #106001, #168631 ) ;
#139506 = DIRECTION ( 'NONE',  ( 1.000000000000000000, 0.000000000000000000, 0.000000000000000000 ) ) ;
#139508 = DIRECTION ( 'NONE',  ( 0.000000000000000000, 0.9654727137038715545, 0.2605042016806676242 ) ) ;
#139509 = CARTESIAN_POINT ( 'NONE',  ( 21.72449340488909897, 10.28395627750227703, -54.34999999999999432 ) ) ;
#139510 = DIRECTION ( 'NONE',  ( 0.000000000000000000, 0.2128009952263403282, -0.9770955615653358350 ) ) ;
#139512 = DIRECTION ( 'NONE',  ( 0.000000000000000000, 0.000000000000000000, 1.000000000000000000 ) ) ;
#139511 = CARTESIAN_POINT ( 'NONE',  ( 22.39999999999999503, 64.35000000001164722, -69.42310748452440805 ) ) ;
#139513 = AXIS2_PLACEMENT_3D ( 'NONE', #189447, #245569, #70804 ) ;
#139514 = CARTESIAN_POINT ( 'NONE',  ( 18.59999999999999432, 1.736257131608553550, -112.0686523290175245 ) ) ;
#139516 = ORIENTED_EDGE ( 'NONE', *, *, #152237, .T. ) ;
#139515 = CARTESIAN_POINT ( 'NONE',  ( 21.05193202509564543, 65.27606398031542767, -191.3505728811986728 ) ) ;
#139518 = DIRECTION ( 'NONE',  ( 1.000000000000000000, 0.000000000000000000, 0.000000000000000000 ) ) ;
#139517 = LINE ( 'NONE', #40472, #170119 ) ;
#139519 = ORIENTED_EDGE ( 'NONE', *, *, #172720, .F. ) ;
#139521 = ORIENTED_EDGE ( 'NONE', *, *, #6804, .F. ) ;
#139520 = DIRECTION ( 'NONE',  ( 0.000000000000000000, 0.000000000000000000, 1.000000000000000000 ) ) ;
#139522 = AXIS2_PLACEMENT_3D ( 'NONE', #214916, #132830, #72880 ) ;
#139523 = ORIENTED_EDGE ( 'NONE', *, *, #238884, .T. ) ;
#139524 = CYLINDRICAL_SURFACE ( 'NONE', #107491, 0.09999999999999939493 ) ;
#139525 = DIRECTION ( 'NONE',  ( -1.000000000000000000, 0.000000000000000000, 0.000000000000000000 ) ) ;
#139526 = DIRECTION ( 'NONE',  ( -1.000000000000000000, 0.000000000000000000, 0.000000000000000000 ) ) ;
#139527 = ORIENTED_EDGE ( 'NONE', *, *, #34931, .T. ) ;
#139528 = CARTESIAN_POINT ( 'NONE',  ( 23.24999999999999645, 5.600000000011153389, -88.75000000000004263 ) ) ;
#139529 = DIRECTION ( 'NONE',  ( 0.000000000000000000, -0.9910827722268049644, 0.1332476588733589318 ) ) ;
#139531 = FACE_OUTER_BOUND ( 'NONE', #179898, .T. ) ;
#139530 = CIRCLE ( 'NONE', #102092, 11.64999999999999325 ) ;
#139532 = CARTESIAN_POINT ( 'NONE',  ( 20.94999999999999929, 1.115600667400684642E-11, -200.9999999999999432 ) ) ;
#139533 = CARTESIAN_POINT ( 'NONE',  ( -21.05000000000000071, -1.835341550213255957, -179.1551512925629197 ) ) ;
#139534 = EDGE_LOOP ( 'NONE', ( #189047, #41179, #176660, #61992 ) ) ;
#139535 = ORIENTED_EDGE ( 'NONE', *, *, #48190, .F. ) ;
#139536 = CARTESIAN_POINT ( 'NONE',  ( -16.89318236219977365, 9.951535257886286345, -188.3551296321058146 ) ) ;
#139537 = VECTOR ( 'NONE', #241969, 1000.000000000000000 ) ;
#139538 = ORIENTED_EDGE ( 'NONE', *, *, #243675, .T. ) ;
#139539 = CARTESIAN_POINT ( 'NONE',  ( 20.85000000000000142, -0.3238857010591806307, -66.95758958931398297 ) ) ;
#139540 = ORIENTED_EDGE ( 'NONE', *, *, #100669, .F. ) ;
#139541 = CARTESIAN_POINT ( 'NONE',  ( 18.54999999999999716, 23.65833333333332433, -16.75000000000000000 ) ) ;
#139542 = EDGE_CURVE ( 'NONE', #71101, #134996, #112699, .T. ) ;
#139543 = DIRECTION ( 'NONE',  ( 0.000000000000000000, 0.000000000000000000, -1.000000000000000000 ) ) ;
#139544 = FACE_OUTER_BOUND ( 'NONE', #234571, .T. ) ;
#139545 = DIRECTION ( 'NONE',  ( 1.000000000000000000, 0.000000000000000000, 0.000000000000000000 ) ) ;
#139546 = CARTESIAN_POINT ( 'NONE',  ( -16.97683809663752186, 11.69051004343035771, -207.9207640419785719 ) ) ;
#139548 = EDGE_CURVE ( 'NONE', #100199, #249188, #159631, .T. ) ;
#139547 = CARTESIAN_POINT ( 'NONE',  ( -20.00857864376270001, 66.85000000001150511, -48.37310748452438247 ) ) ;
#139549 = ORIENTED_EDGE ( 'NONE', *, *, #74610, .T. ) ;
#139550 = CIRCLE ( 'NONE', #60443, 0.1999999999999987899 ) ;
#139552 = CARTESIAN_POINT ( 'NONE',  ( -23.15000000000000213, 11.65000000001115588, -155.7499999999999716 ) ) ;
#139551 = CARTESIAN_POINT ( 'NONE',  ( 18.59999999999999787, -11.74999999998883737, -188.8499999999999659 ) ) ;
#139553 = VERTEX_POINT ( 'NONE', #73602 ) ;
#139556 = VERTEX_POINT ( 'NONE', #54002 ) ;
#139555 = CARTESIAN_POINT ( 'NONE',  ( -18.39999999999999858, 85.50000000001161027, -62.49103808782458458 ) ) ;
#139554 = CYLINDRICAL_SURFACE ( 'NONE', #65529, 11.79999999999999716 ) ;
#139557 = ORIENTED_EDGE ( 'NONE', *, *, #183465, .F. ) ;
#139558 = LINE ( 'NONE', #198260, #222501 ) ;
#139559 = LINE ( 'NONE', #17086, #243123 ) ;
#139560 = DIRECTION ( 'NONE',  ( 0.000000000000000000, -6.982962677686266711E-15, 1.000000000000000000 ) ) ;
#139561 = VECTOR ( 'NONE', #240853, 1000.000000000000000 ) ;
#139562 = VERTEX_POINT ( 'NONE', #110121 ) ;
#139563 = CARTESIAN_POINT ( 'NONE',  ( 21.14999999999999858, 60.12405517993034465, -221.1314479434109614 ) ) ;
#139564 = FACE_OUTER_BOUND ( 'NONE', #76098, .T. ) ;
#139566 = CARTESIAN_POINT ( 'NONE',  ( 21.05000000000000071, 0.5876173420563349792, -209.1618981382189588 ) ) ;
#139565 = CYLINDRICAL_SURFACE ( 'NONE', #113689, 0.09999999999999530098 ) ;
#139568 = ORIENTED_EDGE ( 'NONE', *, *, #179536, .F. ) ;
#139567 = DIRECTION ( 'NONE',  ( 0.000000000000000000, 0.000000000000000000, -1.000000000000000000 ) ) ;
#139569 = ORIENTED_EDGE ( 'NONE', *, *, #93935, .T. ) ;
#139570 = CIRCLE ( 'NONE', #143852, 0.09999999999999817368 ) ;
#139571 = CARTESIAN_POINT ( 'NONE',  ( -23.15000000000000213, 74.07476635515247665, -157.2928639513982318 ) ) ;
#139572 = ORIENTED_EDGE ( 'NONE', *, *, #2902, .F. ) ;
#139573 = DIRECTION ( 'NONE',  ( 0.000000000000000000, 0.8660254037844377084, 0.5000000000000016653 ) ) ;
#139574 = ORIENTED_EDGE ( 'NONE', *, *, #256036, .F. ) ;
#139575 = DIRECTION ( 'NONE',  ( 1.000000000000000000, 0.000000000000000000, 0.000000000000000000 ) ) ;
#139576 = DIRECTION ( 'NONE',  ( -1.000000000000000000, 0.000000000000000000, -0.000000000000000000 ) ) ;
#139577 = DIRECTION ( 'NONE',  ( 1.000000000000000000, 0.000000000000000000, 0.000000000000000000 ) ) ;
#139578 = VERTEX_POINT ( 'NONE', #174002 ) ;
#139579 = DIRECTION ( 'NONE',  ( 0.000000000000000000, 0.000000000000000000, 1.000000000000000000 ) ) ;
#139580 = ADVANCED_FACE ( 'NONE', ( #194828 ), #16188, .F. ) ;
#139581 = EDGE_CURVE ( 'NONE', #131063, #169539, #130399, .T. ) ;
#139582 = CARTESIAN_POINT ( 'NONE',  ( -16.80469485234340965, 9.942151663152193564, -54.30996684393117846 ) ) ;
#139583 = AXIS2_PLACEMENT_3D ( 'NONE', #145957, #142113, #225480 ) ;
#139584 = AXIS2_PLACEMENT_3D ( 'NONE', #117930, #136183, #215741 ) ;
#139585 = AXIS2_PLACEMENT_3D ( 'NONE', #6624, #245254, #9197 ) ;
#139586 = ORIENTED_EDGE ( 'NONE', *, *, #169591, .F. ) ;
#139587 = VERTEX_POINT ( 'NONE', #39616 ) ;
#139588 = ORIENTED_EDGE ( 'NONE', *, *, #253676, .T. ) ;
#139589 = COLOUR_RGB ( '', 0.66274510, 0.83137255, 0.94901961) ;
#139590 = EDGE_CURVE ( 'NONE', #115263, #166854, #9773, .T. ) ;
#139591 = CARTESIAN_POINT ( 'NONE',  ( 20.94999999999999929, 70.50000000001223555, -148.9283735034374843 ) ) ;
#139592 = EDGE_LOOP ( 'NONE', ( #166168, #241629, #60495, #14859 ) ) ;
#139594 = ORIENTED_EDGE ( 'NONE', *, *, #207474, .F. ) ;
#139593 = CARTESIAN_POINT ( 'NONE',  ( 15.69410316191959254, 66.64325398293429714, -186.3197477631601942 ) ) ;
#139595 = EDGE_CURVE ( 'NONE', #178236, #147021, #184551, .T. ) ;
#139596 = ORIENTED_EDGE ( 'NONE', *, *, #225858, .F. ) ;
#139599 = VERTEX_POINT ( 'NONE', #98222 ) ;
#139598 = ORIENTED_EDGE ( 'NONE', *, *, #158339, .T. ) ;
#139597 = FACE_OUTER_BOUND ( 'NONE', #239979, .T. ) ;
#139601 = ADVANCED_FACE ( 'NONE', ( #198647 ), #168051, .T. ) ;
#139600 = ORIENTED_EDGE ( 'NONE', *, *, #115012, .T. ) ;
#139602 = DIRECTION ( 'NONE',  ( 0.000000000000000000, -0.4721928772777346794, -0.8814952561688431665 ) ) ;
#139603 = CIRCLE ( 'NONE', #222825, 11.79999999999999361 ) ;
#139604 = AXIS2_PLACEMENT_3D ( 'NONE', #194206, #217569, #138037 ) ;
#139605 = CARTESIAN_POINT ( 'NONE',  ( -16.82542659449969591, 14.12371795089690352, -219.1659029699155781 ) ) ;
#139606 = VECTOR ( 'NONE', #77918, 1000.000000000000000 ) ;
#139607 = ORIENTED_EDGE ( 'NONE', *, *, #42577, .T. ) ;
#139608 = DIRECTION ( 'NONE',  ( 0.000000000000000000, -0.9994937237965558774, -0.03181660087586650476 ) ) ;
#139610 = ORIENTED_EDGE ( 'NONE', *, *, #5136, .F. ) ;
#139609 = CARTESIAN_POINT ( 'NONE',  ( 18.49999999999999645, 68.48451787451661232, -224.2224406095231757 ) ) ;
#139611 = DIRECTION ( 'NONE',  ( 1.000000000000000000, -2.952720810173289112E-16, -2.061873921506763405E-30 ) ) ;
#139613 = ORIENTED_EDGE ( 'NONE', *, *, #33811, .F. ) ;
#139612 = DIRECTION ( 'NONE',  ( 0.000000000000000000, -6.530723674265620862E-15, 1.000000000000000000 ) ) ;
#139614 = EDGE_CURVE ( 'NONE', #224437, #101747, #17960, .T. ) ;
#139615 = ORIENTED_EDGE ( 'NONE', *, *, #86803, .F. ) ;
#139616 = AXIS2_PLACEMENT_3D ( 'NONE', #164563, #1614, #163283 ) ;
#139617 = CIRCLE ( 'NONE', #118813, 12.97499999999999964 ) ;
#139618 = VECTOR ( 'NONE', #90557, 1000.000000000000000 ) ;
#139619 = CARTESIAN_POINT ( 'NONE',  ( -23.15000000000000213, 76.00000000001213607, -136.5231074845242745 ) ) ;
#139620 = CARTESIAN_POINT ( 'NONE',  ( 18.59117750673696179, 18.41524492703433324, -237.0006385043383546 ) ) ;
#139621 = VERTEX_POINT ( 'NONE', #431 ) ;
#139622 = ORIENTED_EDGE ( 'NONE', *, *, #8854, .T. ) ;
#139623 = CARTESIAN_POINT ( 'NONE',  ( -16.93226657140833069, 9.999543822735571297, -180.0787131109735810 ) ) ;
#139624 = DIRECTION ( 'NONE',  ( -0.000000000000000000, -0.9126074666063771490, -0.4088369013363281623 ) ) ;
#139627 = EDGE_LOOP ( 'NONE', ( #167518, #181389, #184486 ) ) ;
#139626 = VERTEX_POINT ( 'NONE', #40893 ) ;
#139625 = AXIS2_PLACEMENT_3D ( 'NONE', #26745, #121972, #183234 ) ;
#139628 = EDGE_LOOP ( 'NONE', ( #216317, #237379, #62907, #111838 ) ) ;
#139629 = DIRECTION ( 'NONE',  ( 1.000000000000000000, 0.000000000000000000, 0.000000000000000000 ) ) ;
#139630 = ORIENTED_EDGE ( 'NONE', *, *, #110613, .F. ) ;
#139631 = CIRCLE ( 'NONE', #214654, 0.1000000000000043771 ) ;
#139632 = ORIENTED_EDGE ( 'NONE', *, *, #167685, .T. ) ;
#139633 = DIRECTION ( 'NONE',  ( -1.000000000000000000, 0.000000000000000000, 0.000000000000000000 ) ) ;
#139634 = ORIENTED_EDGE ( 'NONE', *, *, #101478, .T. ) ;
#139635 = FACE_OUTER_BOUND ( 'NONE', #235304, .T. ) ;
#139636 = AXIS2_PLACEMENT_3D ( 'NONE', #135310, #194045, #214862 ) ;
#139637 = VECTOR ( 'NONE', #162362, 999.9999999999998863 ) ;
#139639 = CARTESIAN_POINT ( 'NONE',  ( -23.25000000000000000, 76.00000000001270450, -207.5731074845243427 ) ) ;
#139638 = CARTESIAN_POINT ( 'NONE',  ( 23.40000000000005187, 82.78482233730476025, -26.42994920107286916 ) ) ;
#139640 = EDGE_CURVE ( 'NONE', #236182, #27566, #234643, .T. ) ;
#139641 = ORIENTED_EDGE ( 'NONE', *, *, #14390, .F. ) ;
#139643 = ORIENTED_EDGE ( 'NONE', *, *, #166097, .T. ) ;
#139642 = ORIENTED_EDGE ( 'NONE', *, *, #168349, .T. ) ;
#139644 = DIRECTION ( 'NONE',  ( -1.000000000000000000, 0.000000000000000000, -0.000000000000000000 ) ) ;
#139645 = CARTESIAN_POINT ( 'NONE',  ( 23.40000000000005187, 76.00000000001119815, -36.02310748452479316 ) ) ;
#139646 = VERTEX_POINT ( 'NONE', #77398 ) ;
#139647 = ADVANCED_FACE ( 'NONE', ( #119123 ), #1387, .T. ) ;
#139648 = DIRECTION ( 'NONE',  ( 0.000000000000000000, 0.000000000000000000, 1.000000000000000000 ) ) ;
#139649 = ORIENTED_EDGE ( 'NONE', *, *, #141900, .F. ) ;
#139650 = VERTEX_POINT ( 'NONE', #175275 ) ;
#139651 = LINE ( 'NONE', #60125, #112667 ) ;
#139652 = VERTEX_POINT ( 'NONE', #37038 ) ;
#139653 = CARTESIAN_POINT ( 'NONE',  ( 21.14999999999999858, 11.65000000001116298, -146.1500000000000341 ) ) ;
#139654 = FACE_OUTER_BOUND ( 'NONE', #112860, .T. ) ;
#139655 = EDGE_LOOP ( 'NONE', ( #67028, #190094, #122576, #156697, #182588, #155790 ) ) ;
#139656 = DIRECTION ( 'NONE',  ( 1.000000000000000000, 0.000000000000000000, 0.000000000000000000 ) ) ;
#139658 = ADVANCED_FACE ( 'NONE', ( #180381 ), #255999, .T. ) ;
#139657 = CARTESIAN_POINT ( 'NONE',  ( -18.50000000000000000, 1.115600667400684642E-11, -167.4999999999999716 ) ) ;
#139660 = CARTESIAN_POINT ( 'NONE',  ( -16.80891096016338437, 9.950000000011137047, -121.3676628072671235 ) ) ;
#139659 = DIRECTION ( 'NONE',  ( 1.000000000000000000, 0.000000000000000000, 0.000000000000000000 ) ) ;
#139661 = DIRECTION ( 'NONE',  ( 0.000000000000000000, 0.000000000000000000, 1.000000000000000000 ) ) ;
#139662 = VECTOR ( 'NONE', #130572, 1000.000000000000000 ) ;
#139663 = LINE ( 'NONE', #184911, #66287 ) ;
#139664 = DIRECTION ( 'NONE',  ( 0.000000000000000000, 0.000000000000000000, 1.000000000000000000 ) ) ;
#139665 = DIRECTION ( 'NONE',  ( -1.073024830501117528E-15, 0.8814952561688430555, -0.4721928772777346239 ) ) ;
#139666 = CIRCLE ( 'NONE', #27299, 0.5000000000000007772 ) ;
#139667 = CARTESIAN_POINT ( 'NONE',  ( 18.59999999999999432, 74.83729825007388570, -95.02310748452431710 ) ) ;
#139668 = DIRECTION ( 'NONE',  ( 0.000000000000000000, 0.000000000000000000, -1.000000000000000000 ) ) ;
#139669 = ADVANCED_FACE ( 'NONE', ( #177832 ), #117823, .T. ) ;
#139670 = VECTOR ( 'NONE', #62285, 1000.000000000000114 ) ;
#139671 = VERTEX_POINT ( 'NONE', #59100 ) ;
#139672 = VECTOR ( 'NONE', #52041, 1000.000000000000000 ) ;
#139674 = EDGE_LOOP ( 'NONE', ( #87634, #37595, #33123, #162048 ) ) ;
#139673 = ORIENTED_EDGE ( 'NONE', *, *, #95501, .T. ) ;
#139675 = CIRCLE ( 'NONE', #247846, 0.1000000000000124678 ) ;
#139676 = ORIENTED_EDGE ( 'NONE', *, *, #195180, .T. ) ;
#139677 = ORIENTED_EDGE ( 'NONE', *, *, #194540, .T. ) ;
#139678 = DIRECTION ( 'NONE',  ( 0.000000000000000000, -0.07893460099012301889, 0.9968797965484754720 ) ) ;
#139679 = EDGE_CURVE ( 'NONE', #202894, #66864, #188852, .T. ) ;
#139680 = DIRECTION ( 'NONE',  ( 0.000000000000000000, 0.000000000000000000, 1.000000000000000000 ) ) ;
#139681 = VECTOR ( 'NONE', #218211, 1000.000000000000000 ) ;
#139683 = CARTESIAN_POINT ( 'NONE',  ( -20.54999999999999716, 8.772386841380839684, -220.8375963540301257 ) ) ;
#139682 = FACE_OUTER_BOUND ( 'NONE', #107524, .T. ) ;
#139684 = CARTESIAN_POINT ( 'NONE',  ( 18.52928932188133970, 33.71149860592453251, -236.3111109633099716 ) ) ;
#139686 = VERTEX_POINT ( 'NONE', #215631 ) ;
#139685 = VECTOR ( 'NONE', #32320, 1000.000000000000000 ) ;
#139687 = ADVANCED_FACE ( 'NONE', ( #236486 ), #158282, .F. ) ;
#139688 = FACE_OUTER_BOUND ( 'NONE', #121165, .T. ) ;
#139689 =( NAMED_UNIT ( * ) SI_UNIT ( $, .STERADIAN. ) SOLID_ANGLE_UNIT ( ) );
#139690 = EDGE_CURVE ( 'NONE', #41808, #208701, #222133, .T. ) ;
#139691 = DIRECTION ( 'NONE',  ( 0.000000000000000000, 0.9126074666063769270, 0.4088369013363280513 ) ) ;
#139692 = CIRCLE ( 'NONE', #148093, 0.09999999999998712696 ) ;
#139693 = CARTESIAN_POINT ( 'NONE',  ( 18.39999999999999503, 64.52683809664938508, -90.37310748452438247 ) ) ;
#139694 = DIRECTION ( 'NONE',  ( -0.000000000000000000, -0.2617529984165030132, -0.9651348961777157509 ) ) ;
#139695 = ORIENTED_EDGE ( 'NONE', *, *, #218853, .F. ) ;
#139696 = B_SPLINE_CURVE_WITH_KNOTS ( 'NONE', 3,
 ( #250809, #179953, #139515, #23468, #44293, #2569, #224189, #63845, #222904, #202077, #102948, #143373, #162964, #40470, #241213, #182529 ),
 .UNSPECIFIED., .F., .F.,
 ( 4, 3, 3, 3, 3, 4 ),
 ( 0.000000000000000000, 3.357088238235088736E-05, 6.714213034887092689E-05, 0.0001007408646120986739, 0.0001343627955914349754, 0.0001573956632896092792 ),
 .UNSPECIFIED. ) ;
#139697 = EDGE_CURVE ( 'NONE', #110167, #207747, #96511, .T. ) ;
#139698 = CARTESIAN_POINT ( 'NONE',  ( -21.05000000000000071, 0.09779029131994597390, -94.24218538952392521 ) ) ;
#139699 = EDGE_LOOP ( 'NONE', ( #246754, #59114, #1576, #223283, #60090, #177480, #200193, #180109, #189570, #207620, #35087, #60724 ) ) ;
#139700 = FACE_OUTER_BOUND ( 'NONE', #103217, .T. ) ;
#139701 = CIRCLE ( 'NONE', #27342, 0.1000000000000009492 ) ;
#139702 = DIRECTION ( 'NONE',  ( 0.000000000000000000, 1.000000000000000000, 6.982962677686266711E-15 ) ) ;
#139703 = EDGE_CURVE ( 'NONE', #36086, #88284, #211363, .T. ) ;
#139704 = DIRECTION ( 'NONE',  ( 1.000000000000000000, 0.000000000000000000, 0.000000000000000000 ) ) ;
#139705 = DIRECTION ( 'NONE',  ( 1.000000000000000000, 0.000000000000000000, 0.000000000000000000 ) ) ;
#139706 = EDGE_CURVE ( 'NONE', #204733, #80372, #234831, .T. ) ;
#139707 = DIRECTION ( 'NONE',  ( 0.000000000000000000, 0.000000000000000000, -1.000000000000000000 ) ) ;
#139708 = ORIENTED_EDGE ( 'NONE', *, *, #135925, .F. ) ;
#139709 = CARTESIAN_POINT ( 'NONE',  ( 18.50000000000000000, 47.16152503674118890, -255.1462838189583806 ) ) ;
#139710 = DIRECTION ( 'NONE',  ( 0.000000000000000000, 0.1568667991644355497, -0.9876197685951332295 ) ) ;
#139711 = DIRECTION ( 'NONE',  ( 1.000000000000000000, 0.000000000000000000, 0.000000000000000000 ) ) ;
#139713 = CARTESIAN_POINT ( 'NONE',  ( 20.94999999999999929, 1.835341550235569663, -112.0551512925630249 ) ) ;
#139712 = LINE ( 'NONE', #64047, #111664 ) ;
#139714 = DIRECTION ( 'NONE',  ( 0.000000000000000000, 0.000000000000000000, 1.000000000000000000 ) ) ;
#139715 = CARTESIAN_POINT ( 'NONE',  ( -18.59999999999999787, -1.835859311432484375, -78.50443916879852679 ) ) ;
#139716 = CARTESIAN_POINT ( 'NONE',  ( -20.64999999999999858, 1.115600667400684642E-11, -67.00000000000004263 ) ) ;
#139718 = CARTESIAN_POINT ( 'NONE',  ( -23.15000000000000213, 21.13195309841794867, -243.6318585593224100 ) ) ;
#139717 = B_SPLINE_CURVE_WITH_KNOTS ( 'NONE', 3,
 ( #27773, #12053, #51125, #111129, #126839, #246774, #168588 ),
 .UNSPECIFIED., .F., .F.,
 ( 4, 3, 4 ),
 ( 0.000000000000000000, 0.0009834301579440022593, 0.001767853679402679300 ),
 .UNSPECIFIED. ) ;
#139720 = VERTEX_POINT ( 'NONE', #31468 ) ;
#139719 = AXIS2_PLACEMENT_3D ( 'NONE', #99255, #19756, #79690 ) ;
#139721 = TOROIDAL_SURFACE ( 'NONE', #64718, 0.4000000000000017431, 0.1000000000000000056 ) ;
#139722 = EDGE_LOOP ( 'NONE', ( #224885, #49877, #70051, #51283 ) ) ;
#139723 = EDGE_CURVE ( 'NONE', #214500, #170250, #151401, .T. ) ;
#139724 = ORIENTED_EDGE ( 'NONE', *, *, #150799, .F. ) ;
#139725 = EDGE_CURVE ( 'NONE', #246982, #160597, #116116, .T. ) ;
#139726 = CARTESIAN_POINT ( 'NONE',  ( -18.40000000000000213, 11.75000000001113953, -180.1499999999999773 ) ) ;
#139727 = FACE_OUTER_BOUND ( 'NONE', #4628, .T. ) ;
#139728 = EDGE_CURVE ( 'NONE', #127870, #163992, #9958, .T. ) ;
#139729 = CARTESIAN_POINT ( 'NONE',  ( -18.49719636458551264, -9.446365359216978064, -174.5716138698830662 ) ) ;
#139730 = DIRECTION ( 'NONE',  ( -0.000000000000000000, 1.000000000000000000, -0.000000000000000000 ) ) ;
#139731 = VECTOR ( 'NONE', #10793, 1000.000000000000000 ) ;
#139732 = ORIENTED_EDGE ( 'NONE', *, *, #118918, .T. ) ;
#139733 = DIRECTION ( 'NONE',  ( 0.000000000000000000, 0.000000000000000000, 1.000000000000000000 ) ) ;
#139734 = CARTESIAN_POINT ( 'NONE',  ( -15.39126916658602973, 9.389571634557563939, -51.31764071236917601 ) ) ;
#139735 = CARTESIAN_POINT ( 'NONE',  ( -21.93340585899446182, 76.00000000001200817, -110.3472545066445178 ) ) ;
#139736 = AXIS2_PLACEMENT_3D ( 'NONE', #150734, #92035, #16378 ) ;
#139737 = DIRECTION ( 'NONE',  ( -1.000000000000000000, -3.265361837132813093E-16, 0.000000000000000000 ) ) ;
#139739 = VERTEX_POINT ( 'NONE', #91415 ) ;
#139738 = DIRECTION ( 'NONE',  ( 1.000000000000000000, 0.000000000000000000, 0.000000000000000000 ) ) ;
#139741 = CARTESIAN_POINT ( 'NONE',  ( -20.64999999999999858, -9.500000000000001776, -23.60603087734756045 ) ) ;
#139740 = CARTESIAN_POINT ( 'NONE',  ( 23.25000000000000000, -11.64999999998883595, -122.2500000000000284 ) ) ;
#139742 = CARTESIAN_POINT ( 'NONE',  ( -20.94999999999999929, 43.18640298906419162, -245.2812653309023574 ) ) ;
#139743 = ORIENTED_EDGE ( 'NONE', *, *, #53020, .F. ) ;
#139744 = ADVANCED_FACE ( 'NONE', ( #229637 ), #110970, .T. ) ;
#139745 = CARTESIAN_POINT ( 'NONE',  ( -23.15000000000000213, 76.00000000001237765, -170.0231074845243597 ) ) ;
#139746 = LINE ( 'NONE', #181484, #127376 ) ;
#139747 = VERTEX_POINT ( 'NONE', #54826 ) ;
#139749 = EDGE_CURVE ( 'NONE', #223792, #54460, #72340, .T. ) ;
#139748 = DIRECTION ( 'NONE',  ( 0.000000000000000000, 0.2617529984165152257, 0.9651348961777124202 ) ) ;
#139750 = FACE_OUTER_BOUND ( 'NONE', #46831, .T. ) ;
#139751 = ORIENTED_EDGE ( 'NONE', *, *, #216786, .F. ) ;
#139752 = CIRCLE ( 'NONE', #56537, 0.1000000000000009492 ) ;
#139754 = DIRECTION ( 'NONE',  ( -1.000000000000000000, 3.265361837132813093E-16, 2.280189983783949500E-30 ) ) ;
#139753 = VECTOR ( 'NONE', #78521, 1000.000000000000000 ) ;
#139755 = DIRECTION ( 'NONE',  ( 0.000000000000000000, 0.9126074666063844765, 0.4088369013363114535 ) ) ;
#139756 = EDGE_CURVE ( 'NONE', #148962, #215885, #159819, .T. ) ;
#139757 = DIRECTION ( 'NONE',  ( 0.000000000000000000, -0.9595780032479205301, 0.2814428106787130734 ) ) ;
#139758 = ORIENTED_EDGE ( 'NONE', *, *, #36684, .T. ) ;
#139759 = ORIENTED_EDGE ( 'NONE', *, *, #94616, .F. ) ;
#139760 = EDGE_CURVE ( 'NONE', #119332, #149548, #168228, .T. ) ;
#139761 = CARTESIAN_POINT ( 'NONE',  ( -20.64999999999999858, 23.45160524131172508, -253.2535058871250726 ) ) ;
#139762 = FACE_OUTER_BOUND ( 'NONE', #144407, .T. ) ;
#139763 = CARTESIAN_POINT ( 'NONE',  ( -16.96982749440682525, 62.96145768098447348, -213.5858467972242636 ) ) ;
#139764 = DIRECTION ( 'NONE',  ( 3.265361837132812600E-16, -0.4721928772777346239, -0.8814952561688430555 ) ) ;
#139765 = EDGE_CURVE ( 'NONE', #241028, #55613, #32758, .T. ) ;
#139768 = CARTESIAN_POINT ( 'NONE',  ( -22.39999999999999858, 68.20922040163927136, -203.6231074845244109 ) ) ;
#139767 = VECTOR ( 'NONE', #43116, 1000.000000000000000 ) ;
#139766 = CARTESIAN_POINT ( 'NONE',  ( -22.47071067811865319, 75.90090754530959316, -144.2431822290223806 ) ) ;
#139769 = CARTESIAN_POINT ( 'NONE',  ( -21.05000000000000071, -1.851028230129704522, -145.6539132694225032 ) ) ;
#139770 = VECTOR ( 'NONE', #93696, 1000.000000000000000 ) ;
#139771 = CARTESIAN_POINT ( 'NONE',  ( -22.57320508075687115, 12.67709964810647882, -223.3751320524553705 ) ) ;
#139772 = CARTESIAN_POINT ( 'NONE',  ( -22.59999999999999787, 64.25043287652275126, -136.6239658536231047 ) ) ;
#139774 = VERTEX_POINT ( 'NONE', #152697 ) ;
#139773 = AXIS2_PLACEMENT_3D ( 'NONE', #208433, #248832, #70212 ) ;
#139775 = CARTESIAN_POINT ( 'NONE',  ( 16.27683809663750125, 9.350000000011137402, -42.75000000000000000 ) ) ;
#139776 = CIRCLE ( 'NONE', #202157, 0.09999999999999939493 ) ;
#139777 = EDGE_CURVE ( 'NONE', #67059, #69468, #14085, .T. ) ;
#139779 = EDGE_LOOP ( 'NONE', ( #198881, #54843, #93779, #246124 ) ) ;
#139778 = DIRECTION ( 'NONE',  ( 1.000000000000000000, -1.836970198721029934E-16, -1.282749433769087582E-30 ) ) ;
#139780 = CARTESIAN_POINT ( 'NONE',  ( 20.95566103547454517, 65.38175234906556454, -195.8912672915438122 ) ) ;
#139782 = EDGE_CURVE ( 'NONE', #149025, #124845, #21259, .T. ) ;
#139781 = EDGE_CURVE ( 'NONE', #185034, #27505, #174847, .T. ) ;
#139783 = CARTESIAN_POINT ( 'NONE',  ( 21.14999999999999503, 76.10000000001222986, -148.1726782920690937 ) ) ;
#139785 = DIRECTION ( 'NONE',  ( 1.000000000000000000, 0.000000000000000000, 0.000000000000000000 ) ) ;
#139784 = DIRECTION ( 'NONE',  ( 0.000000000000000000, -0.2128009952263601456, 0.9770955615653316162 ) ) ;
#139786 = COLOUR_RGB ( '', 0.09019608, 0.27058824, 0.51372549) ;
#139787 = ORIENTED_EDGE ( 'NONE', *, *, #178344, .F. ) ;
#139789 = CARTESIAN_POINT ( 'NONE',  ( 23.14999999999999147, 1.115600667400684642E-11, -134.0000000000000000 ) ) ;
#139788 = CARTESIAN_POINT ( 'NONE',  ( -21.59142135623730852, 10.27701234982225920, -211.2989328166499092 ) ) ;
#139790 = CARTESIAN_POINT ( 'NONE',  ( 18.59999999999999787, -8.150000000000005684, 10.52591260281975138 ) ) ;
#139791 = CARTESIAN_POINT ( 'NONE',  ( 21.03670563405601968, 65.37517631068381263, -124.1975605983152491 ) ) ;
#139792 = CARTESIAN_POINT ( 'NONE',  ( -22.19999999999999929, -11.75000000000000000, 32.89999999999999858 ) ) ;
#139793 = LINE ( 'NONE', #122835, #103486 ) ;
#139794 = EDGE_LOOP ( 'NONE', ( #21328, #120917, #39912, #242268 ) ) ;
#139795 = DIRECTION ( 'NONE',  ( -0.000000000000000000, 0.2128009952263604232, -0.9770955615653316162 ) ) ;
#139796 = VERTEX_POINT ( 'NONE', #75706 ) ;
#139797 = CYLINDRICAL_SURFACE ( 'NONE', #105192, 0.09999999999999939493 ) ;
#139798 = ORIENTED_EDGE ( 'NONE', *, *, #227017, .F. ) ;
#139799 = DIRECTION ( 'NONE',  ( 0.000000000000000000, 0.2617529984165152257, 0.9651348961777124202 ) ) ;
#139800 = EDGE_CURVE ( 'NONE', #47766, #86497, #57768, .T. ) ;
#139801 = EDGE_CURVE ( 'NONE', #205753, #131400, #173565, .T. ) ;
#139802 = AXIS2_PLACEMENT_3D ( 'NONE', #21610, #221066, #137668 ) ;
#139803 = ORIENTED_EDGE ( 'NONE', *, *, #33527, .F. ) ;
#139804 = AXIS2_PLACEMENT_3D ( 'NONE', #229157, #186175, #50479 ) ;
#139805 = FACE_OUTER_BOUND ( 'NONE', #140031, .T. ) ;
#139806 = CIRCLE ( 'NONE', #223006, 0.1000000000000028644 ) ;
#139807 = EDGE_CURVE ( 'NONE', #39875, #72959, #18160, .T. ) ;
#139808 = FACE_OUTER_BOUND ( 'NONE', #153505, .T. ) ;
#139810 = ORIENTED_EDGE ( 'NONE', *, *, #68953, .T. ) ;
#139809 = CIRCLE ( 'NONE', #256264, 0.09999999999999939493 ) ;
#139811 = EDGE_CURVE ( 'NONE', #114284, #19733, #36604, .T. ) ;
#139812 = AXIS2_PLACEMENT_3D ( 'NONE', #237366, #59985, #181261 ) ;
#139814 = AXIS2_PLACEMENT_3D ( 'NONE', #138254, #121324, #20927 ) ;
#139813 = DIRECTION ( 'NONE',  ( 0.000000000000000000, 1.000000000000000000, 2.891205793294679805E-16 ) ) ;
#139816 = CARTESIAN_POINT ( 'NONE',  ( 21.05000000000000071, 30.90801580390627734, -252.0203440857197279 ) ) ;
#139815 = AXIS2_PLACEMENT_3D ( 'NONE', #142518, #85091, #43440 ) ;
#139817 = EDGE_CURVE ( 'NONE', #240363, #67785, #218053, .T. ) ;
#139818 = FACE_OUTER_BOUND ( 'NONE', #58795, .T. ) ;
#139819 = CARTESIAN_POINT ( 'NONE',  ( 23.14999999999999858, 1.115600667400684642E-11, -134.0000000000000284 ) ) ;
#139820 = LINE ( 'NONE', #236364, #162129 ) ;
#139821 = CARTESIAN_POINT ( 'NONE',  ( 12.93225390519046769, 62.16217865953740329, -218.5667261927901279 ) ) ;
#139822 = ORIENTED_EDGE ( 'NONE', *, *, #217354, .T. ) ;
#139823 = CYLINDRICAL_SURFACE ( 'NONE', #186662, 0.09999999999999939493 ) ;
#139824 = EDGE_LOOP ( 'NONE', ( #191833, #72295, #250455, #115808, #84825 ) ) ;
#139826 = ORIENTED_EDGE ( 'NONE', *, *, #148612, .T. ) ;
#139825 = PLANE ( 'NONE',  #114888 ) ;
#139827 = AXIS2_PLACEMENT_3D ( 'NONE', #15224, #192567, #210845 ) ;
#139828 = ORIENTED_EDGE ( 'NONE', *, *, #130824, .T. ) ;
#139829 = DIRECTION ( 'NONE',  ( -1.000000000000000000, -0.000000000000000000, -0.000000000000000000 ) ) ;
#139830 = CARTESIAN_POINT ( 'NONE',  ( -20.94999999999999929, 1.148907358139439339E-11, -201.0000000000015064 ) ) ;
#139831 = DIRECTION ( 'NONE',  ( 1.000000000000000000, -2.952720810173289112E-16, -2.061873921506763405E-30 ) ) ;
#139832 = AXIS2_PLACEMENT_3D ( 'NONE', #181511, #221872, #238905 ) ;
#139833 = CARTESIAN_POINT ( 'NONE',  ( 21.09793522318404158, 60.08423627381927901, -221.2353571599898032 ) ) ;
#139834 = PLANE ( 'NONE',  #229053 ) ;
#139835 = EDGE_LOOP ( 'NONE', ( #75662, #17693, #113399, #23394 ) ) ;
#139836 = EDGE_CURVE ( 'NONE', #15098, #43174, #247271, .T. ) ;
#139837 = EDGE_CURVE ( 'NONE', #19078, #182432, #151460, .T. ) ;
#139838 = DIRECTION ( 'NONE',  ( -1.000000000000000000, -2.952720810173289112E-16, 0.000000000000000000 ) ) ;
#139839 = DIRECTION ( 'NONE',  ( -0.000000000000000000, -6.982962677686266711E-15, 1.000000000000000000 ) ) ;
#139841 = ORIENTED_EDGE ( 'NONE', *, *, #206628, .T. ) ;
#139840 = CARTESIAN_POINT ( 'NONE',  ( -18.59999999999999787, 7.021664781900089913, -37.33356540189728889 ) ) ;
#139842 = CARTESIAN_POINT ( 'NONE',  ( -20.92356734117541706, 10.31973158070286622, -39.05053347133544150 ) ) ;
#139843 = EDGE_CURVE ( 'NONE', #127135, #232908, #245405, .T. ) ;
#139844 = CARTESIAN_POINT ( 'NONE',  ( 21.70464131381650219, 7.095358018979006864, -100.5000000000000284 ) ) ;
#139845 = ORIENTED_EDGE ( 'NONE', *, *, #201137, .T. ) ;
#139846 = B_SPLINE_CURVE_WITH_KNOTS ( 'NONE', 3,
 ( #94568, #117995, #78845, #194988, #95842, #237936, #59255 ),
 .UNSPECIFIED., .F., .F.,
 ( 4, 3, 4 ),
 ( 0.000000000000000000, 4.520325912680430423E-05, 5.794988040901246848E-05 ),
 .UNSPECIFIED. ) ;
#139847 = CARTESIAN_POINT ( 'NONE',  ( 21.02374657821584947, 64.39999999919209017, -109.9513107143265387 ) ) ;
#139848 = EDGE_LOOP ( 'NONE', ( #189660, #162100, #153024, #73784 ) ) ;
#139849 = CARTESIAN_POINT ( 'NONE',  ( -23.49999999999994316, 83.98667523412385094, -34.76145429838185663 ) ) ;
#139850 = EDGE_CURVE ( 'NONE', #249646, #143246, #93159, .T. ) ;
#139851 = CARTESIAN_POINT ( 'NONE',  ( -18.40000000000000213, 58.56629890316250453, -223.9209570932885356 ) ) ;
#139852 = CARTESIAN_POINT ( 'NONE',  ( 15.74999999999999289, 66.65000000001155911, -52.65736431725049016 ) ) ;
#139853 = DIRECTION ( 'NONE',  ( 0.000000000000000000, -6.417474130781252121E-15, 1.000000000000000000 ) ) ;
#139854 = CIRCLE ( 'NONE', #214875, 0.1000000000000013933 ) ;
#139855 = CIRCLE ( 'NONE', #218970, 0.09999999999999939493 ) ;
#139856 = AXIS2_PLACEMENT_3D ( 'NONE', #73025, #74305, #234623 ) ;
#139857 = AXIS2_PLACEMENT_3D ( 'NONE', #64539, #181928, #1984 ) ;
#139858 = ADVANCED_FACE ( 'NONE', ( #83708 ), #2915, .T. ) ;
#139859 = ORIENTED_EDGE ( 'NONE', *, *, #233784, .T. ) ;
#139860 = CARTESIAN_POINT ( 'NONE',  ( 17.23472005113827166, 10.30788195450076650, -22.04657686006867578 ) ) ;
#139861 = AXIS2_PLACEMENT_3D ( 'NONE', #85700, #165279, #201839 ) ;
#139862 = ORIENTED_EDGE ( 'NONE', *, *, #51529, .T. ) ;
#139863 = CARTESIAN_POINT ( 'NONE',  ( -17.04295772865475556, 10.02489942527111744, -188.3499999999999659 ) ) ;
#139864 = CARTESIAN_POINT ( 'NONE',  ( -22.59999999999999787, 0.1008583691098682150, -21.75043287651061164 ) ) ;
#139866 = ORIENTED_EDGE ( 'NONE', *, *, #87265, .F. ) ;
#139865 = DIRECTION ( 'NONE',  ( 1.000000000000000000, 0.000000000000000000, 0.000000000000000000 ) ) ;
#139867 = CARTESIAN_POINT ( 'NONE',  ( -17.11825945287481332, 10.05000000001113847, -54.35000000000000142 ) ) ;
#139868 = CARTESIAN_POINT ( 'NONE',  ( -15.75000000000000355, 9.350000000011140955, -50.25000000000000711 ) ) ;
#139870 = DIRECTION ( 'NONE',  ( 0.000000000000000000, -0.3738317757008748909, -0.9274965247785733613 ) ) ;
#139869 = AXIS2_PLACEMENT_3D ( 'NONE', #95424, #214090, #138378 ) ;
#139871 = CARTESIAN_POINT ( 'NONE',  ( 23.24999999999999289, 80.15000000001238334, -170.0231074845243313 ) ) ;
#139872 = AXIS2_PLACEMENT_3D ( 'NONE', #8572, #166392, #167663 ) ;
#139873 = LINE ( 'NONE', #19964, #180721 ) ;
#139874 = CARTESIAN_POINT ( 'NONE',  ( -23.15000000000000213, 15.92646454033039660, -219.3818586450342423 ) ) ;
#139876 = ORIENTED_EDGE ( 'NONE', *, *, #101079, .T. ) ;
#139875 = DIRECTION ( 'NONE',  ( 0.000000000000000000, 0.000000000000000000, 1.000000000000000000 ) ) ;
#139877 = AXIS2_PLACEMENT_3D ( 'NONE', #211633, #16015, #33036 ) ;
#139878 = PLANE ( 'NONE',  #60166 ) ;
#139879 = VERTEX_POINT ( 'NONE', #201129 ) ;
#139880 = ORIENTED_EDGE ( 'NONE', *, *, #89531, .T. ) ;
#139881 = CIRCLE ( 'NONE', #2514, 0.09999999999999939493 ) ;
#139882 = CARTESIAN_POINT ( 'NONE',  ( -18.43459694179559349, 85.49421012500970107, -62.90610228186317698 ) ) ;
#139883 = CARTESIAN_POINT ( 'NONE',  ( -18.54159361262947314, 85.46313213550581622, -196.4739852682315018 ) ) ;
#139884 = EDGE_LOOP ( 'NONE', ( #29696, #9138, #206718, #254802 ) ) ;
#139885 = CARTESIAN_POINT ( 'NONE',  ( 20.94999999999999929, 1.835341550235569663, -179.0551512925629538 ) ) ;
#139886 = EDGE_CURVE ( 'NONE', #166883, #195496, #176577, .T. ) ;
#139887 = ORIENTED_EDGE ( 'NONE', *, *, #78337, .F. ) ;
#139888 = AXIS2_PLACEMENT_3D ( 'NONE', #824, #159958, #101195 ) ;
#139889 = CIRCLE ( 'NONE', #164869, 0.1000000000000002831 ) ;
#139890 = CARTESIAN_POINT ( 'NONE',  ( 20.94999999999999929, 7.525330762710603416, -212.0571253909869256 ) ) ;
#139891 = TOROIDAL_SURFACE ( 'NONE', #219020, 4.149999999999999467, 0.1000000000000000056 ) ;
#139892 = AXIS2_PLACEMENT_3D ( 'NONE', #250718, #249462, #109919 ) ;
#139893 = CARTESIAN_POINT ( 'NONE',  ( -16.93909480342659890, 66.00692163521105726, -190.9227604678521004 ) ) ;
#139894 = ORIENTED_EDGE ( 'NONE', *, *, #101523, .F. ) ;
#139895 = VERTEX_POINT ( 'NONE', #184126 ) ;
#139896 = CARTESIAN_POINT ( 'NONE',  ( -23.25000000000000000, 10.33248238083634440, -72.59484654391314962 ) ) ;
#139897 = ORIENTED_EDGE ( 'NONE', *, *, #145341, .T. ) ;
#139898 = EDGE_CURVE ( 'NONE', #101747, #137667, #107159, .T. ) ;
#139899 = DIRECTION ( 'NONE',  ( -1.000000000000000000, 0.000000000000000000, 0.000000000000000000 ) ) ;
#139901 = EDGE_LOOP ( 'NONE', ( #176167, #226834, #135105, #122981 ) ) ;
#139900 = PLANE ( 'NONE',  #17630 ) ;
#139903 = EDGE_CURVE ( 'NONE', #24660, #134638, #213988, .T. ) ;
#139902 = CARTESIAN_POINT ( 'NONE',  ( 21.05000000000000071, 65.27628289530480288, -162.3581939154368285 ) ) ;
#139904 = ORIENTED_EDGE ( 'NONE', *, *, #113216, .T. ) ;
#139905 = DIRECTION ( 'NONE',  ( 0.000000000000000000, 0.000000000000000000, -1.000000000000000000 ) ) ;
#139906 = ORIENTED_EDGE ( 'NONE', *, *, #91803, .T. ) ;
#139908 = ORIENTED_EDGE ( 'NONE', *, *, #79868, .F. ) ;
#139907 = VERTEX_POINT ( 'NONE', #142437 ) ;
#139909 = CARTESIAN_POINT ( 'NONE',  ( -20.90000000000000213, -1.212568896937008089, -7.800000000000000711 ) ) ;
#139910 = AXIS2_PLACEMENT_3D ( 'NONE', #190445, #251675, #73084 ) ;
#139911 = ORIENTED_EDGE ( 'NONE', *, *, #1896, .T. ) ;
#139912 = DIRECTION ( 'NONE',  ( 0.000000000000000000, 0.000000000000000000, 1.000000000000000000 ) ) ;
#139913 = AXIS2_PLACEMENT_3D ( 'NONE', #203553, #6628, #5317 ) ;
#139915 = ADVANCED_FACE ( 'NONE', ( #5469 ), #85004, .F. ) ;
#139914 = ORIENTED_EDGE ( 'NONE', *, *, #79263, .F. ) ;
#139916 = EDGE_CURVE ( 'NONE', #156656, #161687, #27675, .T. ) ;
#139917 = CIRCLE ( 'NONE', #152449, 0.09999999999999681366 ) ;
#139918 = ADVANCED_FACE ( 'NONE', ( #124180 ), #162030, .T. ) ;
#139919 = EDGE_LOOP ( 'NONE', ( #148714, #189188, #135101, #218444 ) ) ;
#139920 = CARTESIAN_POINT ( 'NONE',  ( 21.05000000000000071, 5.850000000011105428, -77.13249722427802624 ) ) ;
#139921 = DIRECTION ( 'NONE',  ( -0.7071067811865456854, -0.7071067811865493491, -4.937700262164544098E-15 ) ) ;
#139923 = ORIENTED_EDGE ( 'NONE', *, *, #119723, .F. ) ;
#139922 = DIRECTION ( 'NONE',  ( 1.000000000000000000, -7.304098846218133681E-16, 4.607487905232622991E-31 ) ) ;
#139924 = DIRECTION ( 'NONE',  ( 0.000000000000000000, 6.982962677686266711E-15, -1.000000000000000000 ) ) ;
#139925 = ORIENTED_EDGE ( 'NONE', *, *, #256277, .F. ) ;
#139926 = ADVANCED_FACE ( 'NONE', ( #224539 ), #109548, .T. ) ;
#139927 = CARTESIAN_POINT ( 'NONE',  ( -18.55121869061588669, 65.67252876774553272, -130.9457041994994881 ) ) ;
#139928 = CARTESIAN_POINT ( 'NONE',  ( 20.94999999999999574, 10.47338541491290442, -7.578654464248542943 ) ) ;
#139929 = ORIENTED_EDGE ( 'NONE', *, *, #248474, .F. ) ;
#139930 = DIRECTION ( 'NONE',  ( 1.000000000000000000, 0.000000000000000000, 0.000000000000000000 ) ) ;
#139931 = DIRECTION ( 'NONE',  ( 0.000000000000000000, -0.8660254037844412611, -0.4999999999999956701 ) ) ;
#139932 = CARTESIAN_POINT ( 'NONE',  ( -18.59999999999999787, 7.804459559388684298, -245.4620200072988325 ) ) ;
#139933 = EDGE_CURVE ( 'NONE', #9735, #24478, #22469, .T. ) ;
#139934 = ORIENTED_EDGE ( 'NONE', *, *, #108531, .T. ) ;
#139935 = FACE_OUTER_BOUND ( 'NONE', #231263, .T. ) ;
#139936 = ORIENTED_EDGE ( 'NONE', *, *, #223611, .F. ) ;
#139937 = ORIENTED_EDGE ( 'NONE', *, *, #231932, .F. ) ;
#139938 = CIRCLE ( 'NONE', #127299, 0.09999999999998898659 ) ;
#139939 = DIRECTION ( 'NONE',  ( 1.000000000000000000, 0.000000000000000000, 0.000000000000000000 ) ) ;
#139940 = ORIENTED_EDGE ( 'NONE', *, *, #124426, .T. ) ;
#139941 = EDGE_LOOP ( 'NONE', ( #152081, #118706, #28681, #42106 ) ) ;
#139942 = DIRECTION ( 'NONE',  ( -1.000000000000000000, 0.000000000000000000, 0.000000000000000000 ) ) ;
#139943 = CARTESIAN_POINT ( 'NONE',  ( -21.14999999999999858, 57.66663670110953888, -226.2321832927624712 ) ) ;
#139944 = ORIENTED_EDGE ( 'NONE', *, *, #210765, .T. ) ;
#139945 = ORIENTED_EDGE ( 'NONE', *, *, #90460, .F. ) ;
#139946 = DIRECTION ( 'NONE',  ( -1.000000000000000000, 0.000000000000000000, 0.000000000000000000 ) ) ;
#139947 = DIRECTION ( 'NONE',  ( 1.000000000000000000, 0.000000000000000000, 0.000000000000000000 ) ) ;
#139948 = EDGE_CURVE ( 'NONE', #31603, #104861, #143230, .T. ) ;
#139949 = VERTEX_POINT ( 'NONE', #30212 ) ;
#139950 = ORIENTED_EDGE ( 'NONE', *, *, #13846, .F. ) ;
#139951 = AXIS2_PLACEMENT_3D ( 'NONE', #78520, #215470, #116390 ) ;
#139952 = EDGE_LOOP ( 'NONE', ( #131368, #125582, #121456, #187691 ) ) ;
#139953 = AXIS2_PLACEMENT_3D ( 'NONE', #40072, #180842, #158735 ) ;
#139954 = AXIS2_PLACEMENT_3D ( 'NONE', #63628, #143147, #184853 ) ;
#139955 = ADVANCED_FACE ( 'NONE', ( #53616 ), #10640, .F. ) ;
#139956 = CARTESIAN_POINT ( 'NONE',  ( -22.57848426163147693, -0.004264329271961049897, -155.7499416931096619 ) ) ;
#139957 = CARTESIAN_POINT ( 'NONE',  ( 18.59999994388910238, 85.36356618708362021, -196.3419902477231744 ) ) ;
#139958 = DIRECTION ( 'NONE',  ( 0.000000000000000000, -6.982962677686266711E-15, 1.000000000000000000 ) ) ;
#139959 = DIRECTION ( 'NONE',  ( 0.000000000000000000, 0.000000000000000000, -1.000000000000000000 ) ) ;
#139960 = DIRECTION ( 'NONE',  ( -0.000000000000000000, -0.9126074666063770380, -0.4088369013363281068 ) ) ;
#139961 = LINE ( 'NONE', #176564, #223383 ) ;
#139962 = DIRECTION ( 'NONE',  ( 0.000000000000000000, -6.982962677686266711E-15, 1.000000000000000000 ) ) ;
#139963 = CARTESIAN_POINT ( 'NONE',  ( -16.78270389226384651, 66.05262738339523310, -149.1819004476129464 ) ) ;
#139964 = PLANE ( 'NONE',  #157380 ) ;
#139965 = CARTESIAN_POINT ( 'NONE',  ( -16.85722902420145175, 23.07992200953330197, -230.9896241052242090 ) ) ;
#139966 = DIRECTION ( 'NONE',  ( 0.000000000000000000, -6.938893903907222067E-15, 1.000000000000000000 ) ) ;
#139967 = AXIS2_PLACEMENT_3D ( 'NONE', #169704, #190532, #95251 ) ;
#139968 = VERTEX_POINT ( 'NONE', #187994 ) ;
#139969 = EDGE_CURVE ( 'NONE', #81862, #139553, #74504, .T. ) ;
#139970 = CIRCLE ( 'NONE', #181700, 0.09999999999998898659 ) ;
#139972 = ORIENTED_EDGE ( 'NONE', *, *, #129478, .T. ) ;
#139971 = LINE ( 'NONE', #3036, #198968 ) ;
#139973 = TOROIDAL_SURFACE ( 'NONE', #52503, 0.2000000000000000111, 0.1000000000000000056 ) ;
#139974 = CARTESIAN_POINT ( 'NONE',  ( 21.05000000000000071, 71.00000000001151079, -48.42837350343745584 ) ) ;
#139976 = EDGE_CURVE ( 'NONE', #250411, #66273, #48470, .T. ) ;
#139975 =( BOUNDED_SURFACE ( )  B_SPLINE_SURFACE ( 3, 2, ( 
 ( #164595, #244109, #125468 ),
 ( #186736, #32496, #8092 ),
 ( #152433, #146297, #87593 ),
 ( #75463, #194118, #225813 ),
 ( #172011, #167190, #211094 ),
 ( #151130, #113276, #192825 ),
 ( #191558, #131553, #153742 ),
 ( #132854, #212392, #33784 ),
 ( #15479, #245417, #173303 ),
 ( #35063, #47180, #231962 ) ),
 .UNSPECIFIED., .F., .F., .F. ) 
 B_SPLINE_SURFACE_WITH_KNOTS ( ( 4, 2, 2, 2, 4 ),
 ( 3, 3 ),
 ( 0.0001836757140119304782, 0.0004000170051583700577, 0.0005081876507315898203, 0.0005622729735181997016, 0.0006163582963048095829 ),
 ( 0.000000000000000000, 1.000000000000000000 ),
 .UNSPECIFIED. ) 
 GEOMETRIC_REPRESENTATION_ITEM ( )  RATIONAL_B_SPLINE_SURFACE ( (
 ( 1.000000000000000000, 0.7071067811865425767, 1.000000000000000000),
 ( 1.000000000000000000, 0.6461995200056629418, 1.000000000000000000),
 ( 1.000000000000000000, 0.5776453529514137264, 1.000000000000000000),
 ( 1.000000000000000000, 0.4585233068370012655, 1.000000000000000000),
 ( 1.000000000000000000, 0.4154092989940034730, 1.000000000000000000),
 ( 1.000000000000000000, 0.3550093145838931763, 1.000000000000000000),
 ( 1.000000000000000000, 0.3354498651688588295, 1.000000000000000000),
 ( 1.000000000000000000, 0.3060347992252818172, 1.000000000000000000),
 ( 1.000000000000000000, 0.2963555829626350335, 1.000000000000000000),
 ( 1.000000000000000000, 0.2966190024563380434, 1.000000000000000000) ) ) 
 REPRESENTATION_ITEM ( '' )  SURFACE ( )  );
#139977 = CARTESIAN_POINT ( 'NONE',  ( -21.14999999999999858, 0.09779029131994770863, -161.2421853895238542 ) ) ;
#139978 = CIRCLE ( 'NONE', #56580, 11.64999999999998970 ) ;
#139979 = AXIS2_PLACEMENT_3D ( 'NONE', #5254, #185209, #86072 ) ;
#139980 = DIRECTION ( 'NONE',  ( -0.000000000000000000, 0.9126074666063770380, 0.4088369013363281068 ) ) ;
#139981 = ORIENTED_EDGE ( 'NONE', *, *, #163597, .F. ) ;
#139982 = EDGE_CURVE ( 'NONE', #88756, #7969, #148877, .T. ) ;
#139983 = ADVANCED_FACE ( 'NONE', ( #129302 ), #208837, .T. ) ;
#139984 = DIRECTION ( 'NONE',  ( 0.000000000000000000, 0.000000000000000000, 1.000000000000000000 ) ) ;
#139985 = DIRECTION ( 'NONE',  ( 0.000000000000000000, 0.000000000000000000, -1.000000000000000000 ) ) ;
#139986 = ADVANCED_FACE ( 'NONE', ( #150165 ), #108454, .F. ) ;
#139987 = EDGE_LOOP ( 'NONE', ( #54420, #243785, #224727, #59941 ) ) ;
#139989 = CARTESIAN_POINT ( 'NONE',  ( -21.00250684356850073, 11.75000000001115197, -141.0148057687580092 ) ) ;
#139988 = CIRCLE ( 'NONE', #227490, 0.4000000000000033529 ) ;
#139990 = CARTESIAN_POINT ( 'NONE',  ( 21.14999999999999858, -11.74999999998884448, -179.7499999999999716 ) ) ;
#139991 = AXIS2_PLACEMENT_3D ( 'NONE', #23005, #82911, #127213 ) ;
#139992 = DIRECTION ( 'NONE',  ( 1.000000000000000000, 0.000000000000000000, 0.000000000000000000 ) ) ;
#139994 =( BOUNDED_SURFACE ( )  B_SPLINE_SURFACE ( 3, 2, ( 
 ( #213869, #255509, #138161 ),
 ( #216429, #59905, #14417 ),
 ( #99025, #118646, #173518 ),
 ( #258080, #93918, #252987 ) ),
 .UNSPECIFIED., .F., .F., .F. ) 
 B_SPLINE_SURFACE_WITH_KNOTS ( ( 4, 4 ),
 ( 3, 3 ),
 ( -2.141299290658871257E-18, 0.0003124336600439480273 ),
 ( 0.000000000000000000, 1.000000000000000000 ),
 .UNSPECIFIED. ) 
 GEOMETRIC_REPRESENTATION_ITEM ( )  RATIONAL_B_SPLINE_SURFACE ( (
 ( 1.000000000000000000, 0.7071067811865472397, 1.000000000000000000),
 ( 1.000000000000000000, 0.7089187706049221438, 1.000000000000000000),
 ( 1.000000000000000000, 0.7039288185052831048, 1.000000000000000000),
 ( 1.000000000000000000, 0.7040654476016580121, 1.000000000000000000) ) ) 
 REPRESENTATION_ITEM ( '' )  SURFACE ( )  );
#139993 = VECTOR ( 'NONE', #160035, 1000.000000000000000 ) ;
#139995 = ADVANCED_FACE ( 'NONE', ( #128026 ), #147333, .T. ) ;
#139996 = CARTESIAN_POINT ( 'NONE',  ( 21.05000000000000071, 40.74071615341952679, -237.9411309446948053 ) ) ;
#139998 = VERTEX_POINT ( 'NONE', #228416 ) ;
#139997 = CARTESIAN_POINT ( 'NONE',  ( -20.05000000000000426, 66.75000000001158185, -57.17310748452438673 ) ) ;
#139999 = CIRCLE ( 'NONE', #156814, 9.500000000000001776 ) ;
#140001 = ORIENTED_EDGE ( 'NONE', *, *, #23417, .F. ) ;
#140000 = CARTESIAN_POINT ( 'NONE',  ( -18.47130263965443220, 85.47115558597577945, -96.33970271904722438 ) ) ;
#140002 = FACE_OUTER_BOUND ( 'NONE', #21546, .T. ) ;
#140003 = CARTESIAN_POINT ( 'NONE',  ( 20.94999999999999929, 20.42498087366621817, -235.1829032864613396 ) ) ;
#140004 = DIRECTION ( 'NONE',  ( 0.000000000000000000, 1.000000000000000000, 0.000000000000000000 ) ) ;
#140005 = CARTESIAN_POINT ( 'NONE',  ( -13.77178122865954002, 9.456028260519072859, -182.5111980350657177 ) ) ;
#140007 = DIRECTION ( 'NONE',  ( 0.000000000000000000, 0.000000000000000000, 1.000000000000000000 ) ) ;
#140006 = CARTESIAN_POINT ( 'NONE',  ( -17.80356949363276087, 65.12326860301656950, -79.81003446029008330 ) ) ;
#140008 = CARTESIAN_POINT ( 'NONE',  ( -21.05000000000000071, 34.06366114622594665, -243.8432908520872786 ) ) ;
#140009 = DIRECTION ( 'NONE',  ( -0.000000000000000000, -0.9126074666063771490, -0.4088369013363281623 ) ) ;
#140010 = DIRECTION ( 'NONE',  ( -1.020425574104003999E-15, 0.8814952561688429444, -0.4721928772777345684 ) ) ;
#140011 = DIRECTION ( 'NONE',  ( -0.000000000000000000, 1.000000000000000000, -0.000000000000000000 ) ) ;
#140012 = DIRECTION ( 'NONE',  ( 0.000000000000000000, 0.2617529984165031243, 0.9651348961777158619 ) ) ;
#140013 =( BOUNDED_SURFACE ( )  B_SPLINE_SURFACE ( 3, 2, ( 
 ( #5954, #185894, #24280 ),
 ( #165053, #3390, #242017 ),
 ( #25556, #63367, #47649 ),
 ( #206746, #187205, #142893 ) ),
 .UNSPECIFIED., .F., .F., .F. ) 
 B_SPLINE_SURFACE_WITH_KNOTS ( ( 4, 4 ),
 ( 3, 3 ),
 ( 0.3000847527772387280, 0.5552748953338751958 ),
 ( 0.000000000000000000, 1.000000000000000000 ),
 .UNSPECIFIED. ) 
 GEOMETRIC_REPRESENTATION_ITEM ( )  RATIONAL_B_SPLINE_SURFACE ( (
 ( 1.000000000000000000, 0.9152888060719439611, 1.000000000000000000),
 ( 1.000000000000000000, 0.9104333467450288486, 1.000000000000000000),
 ( 1.000000000000000000, 0.9035312726221058632, 1.000000000000000000),
 ( 1.000000000000000000, 0.8946697475932068322, 1.000000000000000000) ) ) 
 REPRESENTATION_ITEM ( '' )  SURFACE ( )  );
#140014 = ORIENTED_EDGE ( 'NONE', *, *, #65408, .T. ) ;
#140015 = EDGE_CURVE ( 'NONE', #157651, #218493, #168477, .T. ) ;
#140016 = CARTESIAN_POINT ( 'NONE',  ( 21.05000000000000071, 0.09779029132038109806, -94.24218538951851087 ) ) ;
#140017 = ORIENTED_EDGE ( 'NONE', *, *, #124729, .F. ) ;
#140018 = VERTEX_POINT ( 'NONE', #112318 ) ;
#140019 = CARTESIAN_POINT ( 'NONE',  ( 20.97107704358301916, 67.12452184799060717, -94.46413425513512152 ) ) ;
#140020 = CARTESIAN_POINT ( 'NONE',  ( -20.85000000000000142, 70.22659352830977753, -197.9852579278363578 ) ) ;
#140021 = EDGE_CURVE ( 'NONE', #247118, #163587, #92724, .T. ) ;
#140022 = ORIENTED_EDGE ( 'NONE', *, *, #240395, .F. ) ;
#140023 = EDGE_CURVE ( 'NONE', #104319, #102316, #163906, .T. ) ;
#140024 = CIRCLE ( 'NONE', #235902, 0.5000000000000004441 ) ;
#140025 = AXIS2_PLACEMENT_3D ( 'NONE', #82051, #161652, #241179 ) ;
#140026 = ORIENTED_EDGE ( 'NONE', *, *, #142987, .F. ) ;
#140027 = FILL_AREA_STYLE_COLOUR ( '', #114862 ) ;
#140028 = AXIS2_PLACEMENT_3D ( 'NONE', #246182, #127518, #247456 ) ;
#140029 = CIRCLE ( 'NONE', #48297, 0.09999999999999824307 ) ;
#140030 = EDGE_CURVE ( 'NONE', #94008, #9660, #251808, .T. ) ;
#140031 = EDGE_LOOP ( 'NONE', ( #136815, #13950, #222381, #33576 ) ) ;
#140032 = ORIENTED_EDGE ( 'NONE', *, *, #174697, .T. ) ;
#140033 = AXIS2_PLACEMENT_3D ( 'NONE', #68128, #54953, #90231 ) ;
#140034 = CARTESIAN_POINT ( 'NONE',  ( -23.25000000000000000, 64.25000000001151079, -48.17310748452440805 ) ) ;
#140035 = CARTESIAN_POINT ( 'NONE',  ( 18.39999999999999503, 23.82801463864234037, -229.3483719500187306 ) ) ;
#140036 = FACE_OUTER_BOUND ( 'NONE', #181620, .T. ) ;
#140037 = CARTESIAN_POINT ( 'NONE',  ( 23.24999999999999645, 1.115600667400684642E-11, -134.0000000000000000 ) ) ;
#140038 = DIRECTION ( 'NONE',  ( 0.000000000000000000, -0.000000000000000000, -1.000000000000000000 ) ) ;
#140039 = DIRECTION ( 'NONE',  ( 0.000000000000000000, 0.2617529984165036239, 0.9651348961777156399 ) ) ;
#140041 = ORIENTED_EDGE ( 'NONE', *, *, #211974, .F. ) ;
#140040 = DIRECTION ( 'NONE',  ( 0.000000000000000000, 0.000000000000000000, 1.000000000000000000 ) ) ;
#140043 = CARTESIAN_POINT ( 'NONE',  ( 20.85000000000000142, 77.36242903720467723, -28.13422623660311217 ) ) ;
#140042 = CARTESIAN_POINT ( 'NONE',  ( -17.22767730083624116, 63.03870491652143215, -211.7757501871273860 ) ) ;
#140044 = CARTESIAN_POINT ( 'NONE',  ( 18.59999999999999076, 69.55000000001159322, -59.50608031408435039 ) ) ;
#140045 = AXIS2_PLACEMENT_3D ( 'NONE', #148045, #105010, #28116 ) ;
#140046 = ORIENTED_EDGE ( 'NONE', *, *, #133360, .F. ) ;
#140047 = DIRECTION ( 'NONE',  ( 0.000000000000000000, -0.4088369013363280513, 0.9126074666063769270 ) ) ;
#140048 = CARTESIAN_POINT ( 'NONE',  ( -20.85000000000000142, -11.74999999998884448, -167.5000000000000000 ) ) ;
#140050 = VERTEX_POINT ( 'NONE', #31515 ) ;
#140049 = AXIS2_PLACEMENT_3D ( 'NONE', #256131, #93270, #116686 ) ;
#140051 = ADVANCED_FACE ( 'NONE', ( #14515 ), #212699, .F. ) ;
#140052 = AXIS2_PLACEMENT_3D ( 'NONE', #58930, #142344, #43260 ) ;
#140054 = CARTESIAN_POINT ( 'NONE',  ( -23.25000000000000000, -8.596261682231835621, -143.4501275171502925 ) ) ;
#140053 = CARTESIAN_POINT ( 'NONE',  ( -20.85000000000000142, 64.75617845954087670, -200.4736850529726269 ) ) ;
#140055 = CARTESIAN_POINT ( 'NONE',  ( -16.96982749440706328, 66.05000000001182059, -82.64788589333610958 ) ) ;
#140056 = CARTESIAN_POINT ( 'NONE',  ( 22.59066674512251183, 64.25000000001163869, -69.55361160815502330 ) ) ;
#140057 = ORIENTED_EDGE ( 'NONE', *, *, #1416, .T. ) ;
#140058 = CARTESIAN_POINT ( 'NONE',  ( 21.04999999999999361, 6.344359042054570352, -66.98514436510659209 ) ) ;
#140059 = DIRECTION ( 'NONE',  ( 0.000000000000000000, 0.000000000000000000, -1.000000000000000000 ) ) ;
#140060 = CARTESIAN_POINT ( 'NONE',  ( -20.65000000000000568, 7.249999999999983125, -9.250000000000001776 ) ) ;
#140061 = AXIS2_PLACEMENT_3D ( 'NONE', #151880, #133567, #11054 ) ;
#140062 = CARTESIAN_POINT ( 'NONE',  ( -21.05000000000000071, 68.59681812508419796, -224.1344059333694361 ) ) ;
#140063 = LINE ( 'NONE', #109619, #47003 ) ;
#140064 = ORIENTED_EDGE ( 'NONE', *, *, #137092, .F. ) ;
#140065 = DIRECTION ( 'NONE',  ( 0.000000000000000000, 0.000000000000000000, 1.000000000000000000 ) ) ;
#140066 = ADVANCED_FACE ( 'NONE', ( #253083 ), #130569, .T. ) ;
#140067 = DIRECTION ( 'NONE',  ( -1.000000000000000000, 0.000000000000000000, 0.000000000000000000 ) ) ;
#140068 = CARTESIAN_POINT ( 'NONE',  ( -21.14999999999994174, 76.00000000001119815, -36.02310748452479316 ) ) ;
#140069 = FACE_OUTER_BOUND ( 'NONE', #11429, .T. ) ;
#140070 = EDGE_CURVE ( 'NONE', #57915, #143626, #217686, .T. ) ;
#140071 = CIRCLE ( 'NONE', #210831, 0.09999999999999230338 ) ;
#140072 = AXIS2_PLACEMENT_3D ( 'NONE', #55332, #133621, #194906 ) ;
#140073 = FACE_OUTER_BOUND ( 'NONE', #65560, .T. ) ;
#140074 = AXIS2_PLACEMENT_3D ( 'NONE', #207237, #26029, #108126 ) ;
#140075 = VECTOR ( 'NONE', #203208, 1000.000000000000000 ) ;
#140076 = DIRECTION ( 'NONE',  ( 0.000000000000000000, 0.8814952561688476074, -0.4721928772777262417 ) ) ;
#140077 = EDGE_CURVE ( 'NONE', #196163, #77148, #230988, .T. ) ;
#140079 = ORIENTED_EDGE ( 'NONE', *, *, #72921, .T. ) ;
#140078 = CARTESIAN_POINT ( 'NONE',  ( 21.04999999999908411, 8.776282895301829257, -179.6579090026524739 ) ) ;
#140080 = DIRECTION ( 'NONE',  ( 1.000000000000000000, 2.952720810173289112E-16, -0.000000000000000000 ) ) ;
#140081 = ADVANCED_FACE ( 'NONE', ( #17074 ), #35134, .F. ) ;
#140082 = LINE ( 'NONE', #99660, #90689 ) ;
#140083 = CARTESIAN_POINT ( 'NONE',  ( 18.39999999999999503, 64.52683809664932824, -82.17310748452439384 ) ) ;
#140084 = DIRECTION ( 'NONE',  ( 0.000000000000000000, -7.993605777301079759E-15, 1.000000000000000000 ) ) ;
#140085 = CARTESIAN_POINT ( 'NONE',  ( 18.59999999999999076, 53.32357432685029153, -235.0179440783709879 ) ) ;
#140087 = ORIENTED_EDGE ( 'NONE', *, *, #193020, .F. ) ;
#140086 = CARTESIAN_POINT ( 'NONE',  ( -21.05000000000000071, 64.25000000001219291, -143.5379132551784096 ) ) ;
#140088 = LINE ( 'NONE', #60558, #54969 ) ;
#140089 = CARTESIAN_POINT ( 'NONE',  ( -17.11825945287481687, 63.05955705323258798, -213.2241350765465597 ) ) ;
#140090 = CARTESIAN_POINT ( 'NONE',  ( -33.72168855820452649, 52.34166666667822199, -52.77310748452448763 ) ) ;
#140091 = VERTEX_POINT ( 'NONE', #255611 ) ;
#140092 = CARTESIAN_POINT ( 'NONE',  ( -12.68215100488890634, 66.60336962369453317, -152.1160500917060858 ) ) ;
#140093 = CARTESIAN_POINT ( 'NONE',  ( 20.85000000000000142, 87.75000000001142553, -38.92310748452424463 ) ) ;
#140094 = DIRECTION ( 'NONE',  ( -0.000000000000000000, 0.1350103645451876666, 0.9908441862701600211 ) ) ;
#140095 = AXIS2_PLACEMENT_3D ( 'NONE', #56650, #34581, #134910 ) ;
#140096 = AXIS2_PLACEMENT_3D ( 'NONE', #255464, #174747, #54741 ) ;
#140098 = AXIS2_PLACEMENT_3D ( 'NONE', #212711, #116187, #195732 ) ;
#140097 = CARTESIAN_POINT ( 'NONE',  ( -22.50485643085239928, -0.07878633906603055292, -88.75020506082762495 ) ) ;
#140099 = DIRECTION ( 'NONE',  ( 0.000000000000000000, 0.000000000000000000, 1.000000000000000000 ) ) ;
#140100 = EDGE_CURVE ( 'NONE', #137139, #45034, #160020, .T. ) ;
#140101 = EDGE_CURVE ( 'NONE', #197300, #49158, #172521, .T. ) ;
#140102 = ORIENTED_EDGE ( 'NONE', *, *, #147397, .T. ) ;
#140103 = ORIENTED_EDGE ( 'NONE', *, *, #20762, .F. ) ;
#140105 = CARTESIAN_POINT ( 'NONE',  ( 23.40000000000005187, 64.25000000001119815, -51.02310748452479316 ) ) ;
#140104 = CIRCLE ( 'NONE', #256776, 0.1000000000000021844 ) ;
#140106 = LINE ( 'NONE', #21485, #224706 ) ;
#140107 = DIRECTION ( 'NONE',  ( 1.000000000000000000, 0.000000000000000000, 0.000000000000000000 ) ) ;
#140108 = DIRECTION ( 'NONE',  ( -2.940209281316621016E-16, -1.000000000000000000, -7.056502275159890832E-15 ) ) ;
#140109 = ORIENTED_EDGE ( 'NONE', *, *, #243323, .F. ) ;
#140110 = DIRECTION ( 'NONE',  ( 0.000000000000000000, 1.000000000000000000, -0.000000000000000000 ) ) ;
#140111 = CARTESIAN_POINT ( 'NONE',  ( 20.97565083910961192, 11.84729602164285112, -206.1753656360330069 ) ) ;
#140112 = EDGE_CURVE ( 'NONE', #250227, #199184, #184934, .T. ) ;
#140113 = CARTESIAN_POINT ( 'NONE',  ( 21.15000000000005542, 83.97335046823651794, -34.66234602115918051 ) ) ;
#140114 = ADVANCED_FACE ( 'NONE', ( #15803 ), #136997, .T. ) ;
#140115 = DIRECTION ( 'NONE',  ( 1.000000000000000000, 0.000000000000000000, 0.000000000000000000 ) ) ;
#140116 = CARTESIAN_POINT ( 'NONE',  ( -20.54999999999999716, 68.71679287596359131, -222.9654461259447658 ) ) ;
#140117 = AXIS2_PLACEMENT_3D ( 'NONE', #247750, #110802, #30017 ) ;
#140118 = ORIENTED_EDGE ( 'NONE', *, *, #167121, .F. ) ;
#140120 = ORIENTED_EDGE ( 'NONE', *, *, #78932, .T. ) ;
#140119 = CARTESIAN_POINT ( 'NONE',  ( -20.94999999999999929, 7.021664781911246322, -171.3335654018973173 ) ) ;
#140121 = ORIENTED_EDGE ( 'NONE', *, *, #217922, .F. ) ;
#140122 = DIRECTION ( 'NONE',  ( 0.000000000000000000, 0.1568667991644355497, 0.9876197685951332295 ) ) ;
#140123 = VERTEX_POINT ( 'NONE', #56159 ) ;
#140124 = CARTESIAN_POINT ( 'NONE',  ( -17.05016517655658603, 9.950000000011137047, -154.8273020040062420 ) ) ;
#140125 = DIRECTION ( 'NONE',  ( 1.000000000000000000, 1.875376730785737719E-16, 0.000000000000000000 ) ) ;
#140126 = DIRECTION ( 'NONE',  ( 1.000000000000000000, -1.875376730785737719E-16, -1.309568571767809260E-30 ) ) ;
#140127 = EDGE_LOOP ( 'NONE', ( #117143, #74151, #8177, #26922 ) ) ;
#140128 = EDGE_CURVE ( 'NONE', #70299, #173723, #36651, .T. ) ;
#140129 = DIRECTION ( 'NONE',  ( 0.000000000000000000, -0.2128009952263403282, 0.9770955615653358350 ) ) ;
#140130 = CYLINDRICAL_SURFACE ( 'NONE', #76298, 0.09999999999999939493 ) ;
#140131 = CONICAL_SURFACE ( 'NONE', #244748, 6.250000000000005329, 0.7853981633974431720 ) ;
#140132 = ORIENTED_EDGE ( 'NONE', *, *, #3215, .F. ) ;
#140133 = CARTESIAN_POINT ( 'NONE',  ( -15.75000000000000355, 9.350000000011140955, -150.7500000000000284 ) ) ;
#140135 = VERTEX_POINT ( 'NONE', #116171 ) ;
#140134 = CARTESIAN_POINT ( 'NONE',  ( 20.94999999999999929, 1.835341550235569663, -145.5551512925629822 ) ) ;
#140136 = CARTESIAN_POINT ( 'NONE',  ( -23.15000000000000213, 1.115600667400684642E-11, -67.00000000000000000 ) ) ;
#140137 = LINE ( 'NONE', #200139, #185526 ) ;
#140138 = CIRCLE ( 'NONE', #235821, 0.09999999999999939493 ) ;
#140139 = ADVANCED_FACE ( 'NONE', ( #216532 ), #117443, .F. ) ;
#140140 = CIRCLE ( 'NONE', #135866, 0.1000000000000024342 ) ;
#140141 = CIRCLE ( 'NONE', #56918, 0.09999999999999939493 ) ;
#140142 = ORIENTED_EDGE ( 'NONE', *, *, #256615, .F. ) ;
#140144 = FACE_OUTER_BOUND ( 'NONE', #146442, .T. ) ;
#140143 = MECHANICAL_DESIGN_GEOMETRIC_PRESENTATION_REPRESENTATION (  '', ( #169247 ), #85969 ) ;
#140145 = CARTESIAN_POINT ( 'NONE',  ( -18.38204789744325396, 11.47950103716508252, -24.25000000000000000 ) ) ;
#140146 = CYLINDRICAL_SURFACE ( 'NONE', #35088, 0.09999999999999939493 ) ;
#140147 = VERTEX_POINT ( 'NONE', #196959 ) ;
#140148 = LINE ( 'NONE', #80154, #217375 ) ;
#140149 = EDGE_CURVE ( 'NONE', #166958, #181320, #180851, .T. ) ;
#140150 = DIRECTION ( 'NONE',  ( 0.000000000000000000, -6.982962677686266711E-15, 1.000000000000000000 ) ) ;
#140151 = CARTESIAN_POINT ( 'NONE',  ( -18.50000000000000000, 1.115600667400684642E-11, -67.00000000000004263 ) ) ;
#140152 = ORIENTED_EDGE ( 'NONE', *, *, #186062, .F. ) ;
#140153 = VECTOR ( 'NONE', #206486, 1000.000000000000000 ) ;
#140154 = AXIS2_PLACEMENT_3D ( 'NONE', #184471, #70988, #67106 ) ;
#140155 = ORIENTED_EDGE ( 'NONE', *, *, #127819, .T. ) ;
#140156 = CIRCLE ( 'NONE', #173562, 0.1000000000000028644 ) ;
#140157 = ORIENTED_EDGE ( 'NONE', *, *, #124509, .F. ) ;
#140158 = AXIS2_PLACEMENT_3D ( 'NONE', #104859, #184436, #137919 ) ;
#140159 = DIRECTION ( 'NONE',  ( 0.000000000000000000, 0.2617529984165152257, 0.9651348961777124202 ) ) ;
#140160 = CARTESIAN_POINT ( 'NONE',  ( 21.14999999999999858, 8.786607556611267356, -45.75000000000000000 ) ) ;
#140162 = VERTEX_POINT ( 'NONE', #238669 ) ;
#140161 = DIRECTION ( 'NONE',  ( 0.000000000000000000, 0.000000000000000000, -1.000000000000000000 ) ) ;
#140163 = DIRECTION ( 'NONE',  ( 4.239556034732055511E-17, 0.8127272543710951647, -0.5826443254700257590 ) ) ;
#140165 = TOROIDAL_SURFACE ( 'NONE', #215205, 4.149999999999999467, 0.1000000000000000056 ) ;
#140164 = FACE_BOUND ( 'NONE', #100531, .T. ) ;
#140166 = DIRECTION ( 'NONE',  ( -1.000000000000000000, -2.952720810173289112E-16, 0.000000000000000000 ) ) ;
#140167 = FACE_OUTER_BOUND ( 'NONE', #6375, .T. ) ;
#140168 = CARTESIAN_POINT ( 'NONE',  ( -20.94999999999999574, 64.37928932189385023, -176.8915241368654279 ) ) ;
#140169 = LINE ( 'NONE', #102309, #9833 ) ;
#140171 = ORIENTED_EDGE ( 'NONE', *, *, #250444, .F. ) ;
#140170 = DIRECTION ( 'NONE',  ( 0.000000000000000000, -6.853228547068871147E-15, 1.000000000000000000 ) ) ;
#140173 = VERTEX_POINT ( 'NONE', #215256 ) ;
#140172 = DIRECTION ( 'NONE',  ( 1.000000000000000000, -0.000000000000000000, -0.000000000000000000 ) ) ;
#140174 = DIRECTION ( 'NONE',  ( 0.7071359030027419834, 0.000000000000000000, -0.7070776581709371511 ) ) ;
#140175 = ORIENTED_EDGE ( 'NONE', *, *, #119771, .F. ) ;
#140176 = VERTEX_POINT ( 'NONE', #217794 ) ;
#140177 = CARTESIAN_POINT ( 'NONE',  ( -21.05000000000000426, 6.477046381801004671, -167.5999999999999659 ) ) ;
#140178 = PLANE ( 'NONE',  #138850 ) ;
#140179 = AXIS2_PLACEMENT_3D ( 'NONE', #99543, #214385, #235232 ) ;
#140180 = AXIS2_PLACEMENT_3D ( 'NONE', #171218, #70814, #228586 ) ;
#140181 = CIRCLE ( 'NONE', #106880, 0.5999999999999968692 ) ;
#140182 = CARTESIAN_POINT ( 'NONE',  ( 23.25000000000000000, -11.64999999999999147, 11.75000000000000000 ) ) ;
#140183 = DIRECTION ( 'NONE',  ( 1.000000000000000000, 0.000000000000000000, 0.000000000000000000 ) ) ;
#140184 = CARTESIAN_POINT ( 'NONE',  ( -20.94999999999999929, 74.16465844978745281, -91.46795619196133487 ) ) ;
#140185 = CARTESIAN_POINT ( 'NONE',  ( 23.14999999999999858, 76.00000000001244871, -170.0231074845243597 ) ) ;
#140186 = ORIENTED_EDGE ( 'NONE', *, *, #39021, .F. ) ;
#140187 = EDGE_LOOP ( 'NONE', ( #71663, #32444, #156995, #13638 ) ) ;
#140188 = ADVANCED_FACE ( 'NONE', ( #39211, #198249, #156605 ), #177445, .F. ) ;
#140189 = DIRECTION ( 'NONE',  ( 0.000000000000000000, 0.000000000000000000, 1.000000000000000000 ) ) ;
#140190 = AXIS2_PLACEMENT_3D ( 'NONE', #116882, #157321, #158602 ) ;
#140191 = ORIENTED_EDGE ( 'NONE', *, *, #171175, .T. ) ;
#140192 = DIRECTION ( 'NONE',  ( 0.000000000000000000, 7.147358527629766941E-15, -1.000000000000000000 ) ) ;
#140193 = CARTESIAN_POINT ( 'NONE',  ( 18.52643265882457868, 68.07764576057049055, -224.1679995073710359 ) ) ;
#140194 = CARTESIAN_POINT ( 'NONE',  ( -12.93407622233968191, 66.58221053305935300, -54.16572294054751779 ) ) ;
#140195 = CARTESIAN_POINT ( 'NONE',  ( -21.46681500597999914, -1.459285199490397256, -194.2995562827408662 ) ) ;
#140196 = ORIENTED_EDGE ( 'NONE', *, *, #200054, .T. ) ;
#140197 = CARTESIAN_POINT ( 'NONE',  ( -16.93234230245722216, 66.00189262946514646, -149.1054172028581775 ) ) ;
#140198 = ORIENTED_EDGE ( 'NONE', *, *, #154312, .T. ) ;
#140199 = DIRECTION ( 'NONE',  ( 1.000000000000000000, 0.000000000000000000, 0.000000000000000000 ) ) ;
#140200 = ORIENTED_EDGE ( 'NONE', *, *, #245879, .T. ) ;
#140201 = AXIS2_PLACEMENT_3D ( 'NONE', #59072, #138611, #13576 ) ;
#140202 = EDGE_CURVE ( 'NONE', #5885, #126059, #136181, .T. ) ;
#140203 = CARTESIAN_POINT ( 'NONE',  ( 21.05000000000000071, 1.115653327213047955E-11, -138.3000000000000398 ) ) ;
#140204 = VECTOR ( 'NONE', #221060, 1000.000000000000000 ) ;
#140205 = DIRECTION ( 'NONE',  ( 0.000000000000000000, 0.9126074666063770380, 0.4088369013363281068 ) ) ;
#140206 = AXIS2_PLACEMENT_3D ( 'NONE', #229833, #129452, #169911 ) ;
#140207 = CIRCLE ( 'NONE', #119394, 0.1000000000000028644 ) ;
#140208 = ORIENTED_EDGE ( 'NONE', *, *, #149701, .T. ) ;
#140209 = DIRECTION ( 'NONE',  ( 1.000000000000000000, -0.000000000000000000, -0.000000000000000000 ) ) ;
#140211 = ORIENTED_EDGE ( 'NONE', *, *, #46754, .F. ) ;
#140210 = CARTESIAN_POINT ( 'NONE',  ( 23.04999999999999716, 8.822561741677553471, -113.1500000000000483 ) ) ;
#140212 = ORIENTED_EDGE ( 'NONE', *, *, #123348, .F. ) ;
#140213 = CIRCLE ( 'NONE', #215264, 0.1000000000000013933 ) ;
#140214 = EDGE_CURVE ( 'NONE', #50987, #53620, #1321, .T. ) ;
#140215 = DIRECTION ( 'NONE',  ( 0.000000000000000000, 0.000000000000000000, 1.000000000000000000 ) ) ;
#140216 = EDGE_CURVE ( 'NONE', #175804, #47883, #226613, .T. ) ;
#140217 = EDGE_LOOP ( 'NONE', ( #169200, #102098, #18760 ) ) ;
#140218 = DIRECTION ( 'NONE',  ( -1.000000000000000000, 0.000000000000000000, 0.000000000000000000 ) ) ;
#140219 = CARTESIAN_POINT ( 'NONE',  ( 19.99999999738052381, 64.25000000001250555, -178.8359355348915471 ) ) ;
#140220 = AXIS2_PLACEMENT_3D ( 'NONE', #141313, #157041, #198713 ) ;
#140221 = CARTESIAN_POINT ( 'NONE',  ( -21.05000000000000071, 87.48912529308822172, -139.6231074845242688 ) ) ;
#140222 = CARTESIAN_POINT ( 'NONE',  ( -16.94180778212363236, 66.00755694427942899, -56.91892391399115070 ) ) ;
#140223 = EDGE_CURVE ( 'NONE', #81229, #218397, #5842, .T. ) ;
#140224 = AXIS2_PLACEMENT_3D ( 'NONE', #61099, #38990, #217584 ) ;
#140225 = CARTESIAN_POINT ( 'NONE',  ( -20.64999999999999858, 68.85000000001228670, -157.6731074845243938 ) ) ;
#140226 = CIRCLE ( 'NONE', #211002, 11.74999999999999645 ) ;
#140227 = ORIENTED_EDGE ( 'NONE', *, *, #16982, .T. ) ;
#140228 = CARTESIAN_POINT ( 'NONE',  ( -23.25000000000000000, 87.75000000001165290, -69.52310748452424605 ) ) ;
#140229 = CYLINDRICAL_SURFACE ( 'NONE', #145200, 0.1000000000000000472 ) ;
#140230 = ADVANCED_FACE ( 'NONE', ( #174901 ), #23512, .T. ) ;
#140231 = FACE_OUTER_BOUND ( 'NONE', #239250, .T. ) ;
#140232 = ORIENTED_EDGE ( 'NONE', *, *, #213416, .T. ) ;
#140233 = DIRECTION ( 'NONE',  ( 1.000000000000000000, 2.952720810173289112E-16, -0.000000000000000000 ) ) ;
#140234 = ORIENTED_EDGE ( 'NONE', *, *, #245037, .F. ) ;
#140235 = DIRECTION ( 'NONE',  ( 0.000000000000000000, 0.000000000000000000, 1.000000000000000000 ) ) ;
#140236 = ORIENTED_EDGE ( 'NONE', *, *, #220196, .F. ) ;
#140237 = EDGE_CURVE ( 'NONE', #5240, #143749, #60025, .T. ) ;
#140238 = DIRECTION ( 'NONE',  ( 0.000000000000000000, 0.2128009952263485993, -0.9770955615653341697 ) ) ;
#140239 = CARTESIAN_POINT ( 'NONE',  ( -16.91256925476569606, 66.01426884188437327, -182.5554649955192019 ) ) ;
#140240 = ORIENTED_EDGE ( 'NONE', *, *, #40186, .T. ) ;
#140241 = VECTOR ( 'NONE', #5583, 1000.000000000000000 ) ;
#140243 = ORIENTED_EDGE ( 'NONE', *, *, #3809, .T. ) ;
#140242 = DIRECTION ( 'NONE',  ( -1.000000000000000000, 0.000000000000000000, -0.000000000000000000 ) ) ;
#140244 = CARTESIAN_POINT ( 'NONE',  ( -18.51991288638472000, 8.990547036368365497, -245.3850893028505595 ) ) ;
#140245 = ORIENTED_EDGE ( 'NONE', *, *, #66071, .F. ) ;
#140246 = LINE ( 'NONE', #19036, #219123 ) ;
#140247 = CARTESIAN_POINT ( 'NONE',  ( 20.94999999999999574, -11.48912529306490349, -103.5000000000000426 ) ) ;
#140249 = EDGE_CURVE ( 'NONE', #154503, #59716, #181287, .T. ) ;
#140248 = ORIENTED_EDGE ( 'NONE', *, *, #141265, .F. ) ;
#140250 = EDGE_LOOP ( 'NONE', ( #139417, #16870, #139866, #233070 ) ) ;
#140251 = CARTESIAN_POINT ( 'NONE',  ( 23.14999999999999858, 62.99095723518624368, -207.1734234082435080 ) ) ;
#140252 = CARTESIAN_POINT ( 'NONE',  ( -21.14999999999999858, 64.25000000001210765, -129.7969768484651922 ) ) ;
#140253 = EDGE_LOOP ( 'NONE', ( #220507, #36047, #131913, #121879 ) ) ;
#140254 = CARTESIAN_POINT ( 'NONE',  ( 22.39999999999999503, 64.35000000001164722, -69.62310748452439668 ) ) ;
#140255 = AXIS2_PLACEMENT_3D ( 'NONE', #161913, #201022, #22400 ) ;
#140256 = CIRCLE ( 'NONE', #219382, 4.149999999999999467 ) ;
#140257 = VECTOR ( 'NONE', #180611, 1000.000000000000114 ) ;
#140258 = CIRCLE ( 'NONE', #244321, 11.65000000000001457 ) ;
#140259 = ORIENTED_EDGE ( 'NONE', *, *, #209514, .F. ) ;
#140260 = VERTEX_POINT ( 'NONE', #65156 ) ;
#140261 = PLANE ( 'NONE',  #176444 ) ;
#140263 = ORIENTED_EDGE ( 'NONE', *, *, #131449, .T. ) ;
#140262 = FACE_BOUND ( 'NONE', #5797, .T. ) ;
#140264 = FACE_OUTER_BOUND ( 'NONE', #218026, .T. ) ;
#140265 = FACE_OUTER_BOUND ( 'NONE', #232235, .T. ) ;
#140266 = DIRECTION ( 'NONE',  ( 0.000000000000000000, 0.6728971962616783209, 0.7397360091702797069 ) ) ;
#140267 = AXIS2_PLACEMENT_3D ( 'NONE', #31724, #250726, #133366 ) ;
#140269 = DIRECTION ( 'NONE',  ( -1.000000000000000000, 0.000000000000000000, 0.000000000000000000 ) ) ;
#140268 = CARTESIAN_POINT ( 'NONE',  ( -16.94062896051973865, 66.00728089491119022, -90.42059094240558181 ) ) ;
#140270 = DIRECTION ( 'NONE',  ( 0.000000000000000000, 0.000000000000000000, 1.000000000000000000 ) ) ;
#140271 = TOROIDAL_SURFACE ( 'NONE', #27912, 4.099999999999999645, 0.1000000000000000056 ) ;
#140272 = AXIS2_PLACEMENT_3D ( 'NONE', #126432, #66465, #69052 ) ;
#140273 = CARTESIAN_POINT ( 'NONE',  ( 18.59999999999999076, -1.835859311443637010, -45.10443916879852821 ) ) ;
#140274 = CARTESIAN_POINT ( 'NONE',  ( 20.94999999999999574, 68.20313450767837082, -227.8297066677462794 ) ) ;
#140275 = ORIENTED_EDGE ( 'NONE', *, *, #178934, .F. ) ;
#140276 = ADVANCED_FACE ( 'NONE', ( #41780 ), #63885, .T. ) ;
#140277 = AXIS2_PLACEMENT_3D ( 'NONE', #172946, #235423, #35973 ) ;
#140278 = EDGE_CURVE ( 'NONE', #145487, #50212, #55909, .T. ) ;
#140279 = VERTEX_POINT ( 'NONE', #140861 ) ;
#140280 = VERTEX_POINT ( 'NONE', #44332 ) ;
#140281 = FACE_OUTER_BOUND ( 'NONE', #27403, .T. ) ;
#140282 = EDGE_LOOP ( 'NONE', ( #87806, #124769, #161390, #229338, #161771 ) ) ;
#140283 = DIRECTION ( 'NONE',  ( -3.265361837132813586E-16, -0.9651348961777156399, 0.2617529984165041235 ) ) ;
#140284 = ADVANCED_FACE ( 'NONE', ( #200833 ), #164281, .F. ) ;
#140285 = EDGE_CURVE ( 'NONE', #22276, #217558, #201684, .T. ) ;
#140286 = CARTESIAN_POINT ( 'NONE',  ( -16.87683809663752399, 66.15000000001153069, -49.42547150272069700 ) ) ;
#140287 = VERTEX_POINT ( 'NONE', #66452 ) ;
#140288 = EDGE_CURVE ( 'NONE', #28102, #85530, #202115, .T. ) ;
#140289 = CARTESIAN_POINT ( 'NONE',  ( 0.9000000000000546452, 67.65000000001118963, -14.06452884076210630 ) ) ;
#140290 = ADVANCED_FACE ( 'NONE', ( #123872 ), #51614, .F. ) ;
#140293 = EDGE_LOOP ( 'NONE', ( #111825, #202346, #152696, #164051 ) ) ;
#140292 = EDGE_LOOP ( 'NONE', ( #26655, #35499, #13247, #136517 ) ) ;
#140291 = AXIS2_PLACEMENT_3D ( 'NONE', #98908, #237180, #93801 ) ;
#140294 = ORIENTED_EDGE ( 'NONE', *, *, #25046, .T. ) ;
#140296 = EDGE_CURVE ( 'NONE', #53618, #76942, #151651, .T. ) ;
#140295 = ADVANCED_FACE ( 'NONE', ( #126420 ), #105538, .F. ) ;
#140297 = VERTEX_POINT ( 'NONE', #182568 ) ;
#140298 = FACE_OUTER_BOUND ( 'NONE', #58826, .T. ) ;
#140299 = DIRECTION ( 'NONE',  ( 1.000000000000000000, 0.000000000000000000, 0.000000000000000000 ) ) ;
#140301 = ORIENTED_EDGE ( 'NONE', *, *, #12656, .T. ) ;
#140300 = DIRECTION ( 'NONE',  ( 0.000000000000000000, 0.2617529984165031243, 0.9651348961777157509 ) ) ;
#140302 = ADVANCED_FACE ( 'NONE', ( #22209 ), #125153, .F. ) ;
#140303 = CARTESIAN_POINT ( 'NONE',  ( -23.15000000000000213, 24.12844930803501597, -253.0488546976795021 ) ) ;
#140304 = CARTESIAN_POINT ( 'NONE',  ( -21.44999999999999929, 7.150000000000000355, -12.34999999999999964 ) ) ;
#140306 = ORIENTED_EDGE ( 'NONE', *, *, #219565, .T. ) ;
#140305 = DIRECTION ( 'NONE',  ( 0.000000000000000000, 0.8700118002898321601, -0.4930308989875230585 ) ) ;
#140307 = DIRECTION ( 'NONE',  ( -1.000000000000000000, 0.000000000000000000, 0.000000000000000000 ) ) ;
#140308 = ORIENTED_EDGE ( 'NONE', *, *, #188559, .F. ) ;
#140310 = DIRECTION ( 'NONE',  ( -1.186688945009010077E-16, 1.000000000000000000, 0.000000000000000000 ) ) ;
#140309 = CIRCLE ( 'NONE', #115204, 0.09999999999999739653 ) ;
#140312 = ORIENTED_EDGE ( 'NONE', *, *, #8809, .F. ) ;
#140311 = CARTESIAN_POINT ( 'NONE',  ( 18.59999999999999076, 1.835341550235567887, -145.5551512925629822 ) ) ;
#140313 = CARTESIAN_POINT ( 'NONE',  ( 23.14999999999999503, 64.23880400315596262, -222.2474036988971307 ) ) ;
#140315 = EDGE_CURVE ( 'NONE', #139578, #98827, #251566, .T. ) ;
#140314 = DIRECTION ( 'NONE',  ( 0.000000000000000000, -0.05689261644169250898, 0.9983803033886528011 ) ) ;
#140316 = DIRECTION ( 'NONE',  ( 0.000000000000000000, -1.000000000000000000, -6.352154140967427193E-15 ) ) ;
#140317 = AXIS2_PLACEMENT_3D ( 'NONE', #59924, #199484, #20850 ) ;
#140318 = ORIENTED_EDGE ( 'NONE', *, *, #167430, .F. ) ;
#140320 = CARTESIAN_POINT ( 'NONE',  ( 21.97500000000000497, 9.750000000011153745, -146.2500000000000568 ) ) ;
#140319 = FACE_OUTER_BOUND ( 'NONE', #237799, .T. ) ;
#140321 = DIRECTION ( 'NONE',  ( 0.000000000000000000, 0.4999999999999949485, -0.8660254037844415942 ) ) ;
#140322 = EDGE_CURVE ( 'NONE', #198203, #133285, #230742, .T. ) ;
#140323 = EDGE_CURVE ( 'NONE', #60723, #82975, #163005, .T. ) ;
#140324 = LINE ( 'NONE', #239451, #35148 ) ;
#140325 = AXIS2_PLACEMENT_3D ( 'NONE', #2709, #178832, #242612 ) ;
#140326 = AXIS2_PLACEMENT_3D ( 'NONE', #175956, #59801, #98923 ) ;
#140327 = CARTESIAN_POINT ( 'NONE',  ( -18.50000000000000000, 9.150000000011157653, -88.15000000000004832 ) ) ;
#140328 = CARTESIAN_POINT ( 'NONE',  ( 16.87683809663749557, 14.15900158805613174, -219.2550725561364118 ) ) ;
#140329 = ORIENTED_EDGE ( 'NONE', *, *, #74520, .T. ) ;
#140330 = VERTEX_POINT ( 'NONE', #145976 ) ;
#140331 = ORIENTED_EDGE ( 'NONE', *, *, #109595, .T. ) ;
#140332 = EDGE_CURVE ( 'NONE', #249634, #58239, #46868, .T. ) ;
#140333 = DIRECTION ( 'NONE',  ( -0.000000000000000000, -0.1350103645451928291, -0.9908441862701594660 ) ) ;
#140334 = VECTOR ( 'NONE', #247739, 1000.000000000000000 ) ;
#140335 = ORIENTED_EDGE ( 'NONE', *, *, #231947, .F. ) ;
#140336 = DIRECTION ( 'NONE',  ( 1.000000000000000000, 0.000000000000000000, 0.000000000000000000 ) ) ;
#140337 = EDGE_LOOP ( 'NONE', ( #107133, #235559, #135313, #219241 ) ) ;
#140339 = CARTESIAN_POINT ( 'NONE',  ( -18.54118089899634114, -7.746836289017205779, -209.9009841126467109 ) ) ;
#140338 = CIRCLE ( 'NONE', #56441, 0.1999999999999987899 ) ;
#140340 = DIRECTION ( 'NONE',  ( 1.000000000000000000, 0.000000000000000000, 0.000000000000000000 ) ) ;
#140341 = ADVANCED_FACE ( 'NONE', ( #175521 ), #1755, .F. ) ;
#140342 = ADVANCED_FACE ( 'NONE', ( #116807 ), #170744, .F. ) ;
#140343 = VERTEX_POINT ( 'NONE', #169446 ) ;
#140344 = CARTESIAN_POINT ( 'NONE',  ( 21.72449340488910252, 65.71604372252073745, -90.37310748452436826 ) ) ;
#140345 = FILL_AREA_STYLE_COLOUR ( '', #177438 ) ;
#140346 = CIRCLE ( 'NONE', #102928, 7.720710678118678061 ) ;
#140347 = EDGE_LOOP ( 'NONE', ( #169897, #137963, #161253, #232043 ) ) ;
#140348 = ORIENTED_EDGE ( 'NONE', *, *, #204096, .F. ) ;
#140349 = VERTEX_POINT ( 'NONE', #190264 ) ;
#140351 = CARTESIAN_POINT ( 'NONE',  ( 20.04142135623730070, 64.35000000001147669, -44.87310748452440379 ) ) ;
#140350 = AXIS2_PLACEMENT_3D ( 'NONE', #234986, #96716, #216693 ) ;
#140352 = CARTESIAN_POINT ( 'NONE',  ( -21.44999999999999929, 7.350000000011155166, -88.15000000000004832 ) ) ;
#140353 = CARTESIAN_POINT ( 'NONE',  ( -16.92925196614875105, 66.02766820360145061, -56.90636263680760010 ) ) ;
#140354 = CARTESIAN_POINT ( 'NONE',  ( -23.15000000000000213, 1.115600667400684642E-11, -134.0000000000000284 ) ) ;
#140355 = DIRECTION ( 'NONE',  ( 0.000000000000000000, 0.000000000000000000, -1.000000000000000000 ) ) ;
#140356 = AXIS2_PLACEMENT_3D ( 'NONE', #166203, #171354, #187041 ) ;
#140357 = CARTESIAN_POINT ( 'NONE',  ( 23.24999999999999645, 67.17743825834546101, -90.37310748452436826 ) ) ;
#140359 = DIRECTION ( 'NONE',  ( -0.000000000000000000, 0.000000000000000000, 1.000000000000000000 ) ) ;
#140358 = DIRECTION ( 'NONE',  ( 1.000000000000000000, 0.000000000000000000, 0.000000000000000000 ) ) ;
#140360 = CYLINDRICAL_SURFACE ( 'NONE', #79010, 0.09999999999998898659 ) ;
#140362 = VERTEX_POINT ( 'NONE', #29918 ) ;
#140361 = CARTESIAN_POINT ( 'NONE',  ( 22.32929514600007792, 68.42135243463546601, -103.1221831626382794 ) ) ;
#140363 = CARTESIAN_POINT ( 'NONE',  ( 21.12757541349815682, 69.52661942876049750, -103.0282687003341096 ) ) ;
#140364 = AXIS2_PLACEMENT_3D ( 'NONE', #250845, #58734, #118758 ) ;
#140365 = CARTESIAN_POINT ( 'NONE',  ( -21.65000000000000213, 7.750000000011155521, -146.3500000000000227 ) ) ;
#140366 = CIRCLE ( 'NONE', #252792, 0.4000000000000114575 ) ;
#140367 = EDGE_LOOP ( 'NONE', ( #35423, #131910, #20172, #204952 ) ) ;
#140368 = ORIENTED_EDGE ( 'NONE', *, *, #44778, .T. ) ;
#140369 = CARTESIAN_POINT ( 'NONE',  ( -22.39999999999999858, 67.13476106344063510, -235.8289512066367024 ) ) ;
#140370 = CARTESIAN_POINT ( 'NONE',  ( -20.90000000000000213, 11.61130914238355771, -1.800000000000000044 ) ) ;
#140371 = PLANE ( 'NONE',  #87830 ) ;
#140372 = ORIENTED_EDGE ( 'NONE', *, *, #170397, .F. ) ;
#140373 = AXIS2_PLACEMENT_3D ( 'NONE', #122716, #83530, #62724 ) ;
#140374 = CARTESIAN_POINT ( 'NONE',  ( -20.94999999999999929, 4.252251777740766236, -211.8999245327126744 ) ) ;
#140375 = EDGE_LOOP ( 'NONE', ( #119990, #171974, #72355, #34682 ) ) ;
#140376 = ORIENTED_EDGE ( 'NONE', *, *, #118794, .T. ) ;
#140377 = CYLINDRICAL_SURFACE ( 'NONE', #57381, 0.09999999999999543976 ) ;
#140378 = ORIENTED_EDGE ( 'NONE', *, *, #89995, .T. ) ;
#140379 = CARTESIAN_POINT ( 'NONE',  ( -20.54999999999999716, -8.663551401858004652, -143.5241011180673070 ) ) ;
#140380 = DIRECTION ( 'NONE',  ( -1.000000000000000000, -0.000000000000000000, 0.000000000000000000 ) ) ;
#140381 = CYLINDRICAL_SURFACE ( 'NONE', #194840, 0.1000000000000075273 ) ;
#140382 = DIRECTION ( 'NONE',  ( 0.000000000000000000, 1.000000000000000000, 0.000000000000000000 ) ) ;
#140383 = CARTESIAN_POINT ( 'NONE',  ( -22.94999999999999929, 1.800000000000000044, -11.61130914238355771 ) ) ;
#140384 = ORIENTED_EDGE ( 'NONE', *, *, #990, .T. ) ;
#140385 = FACE_OUTER_BOUND ( 'NONE', #135901, .T. ) ;
#140386 = EDGE_CURVE ( 'NONE', #91302, #88568, #155914, .T. ) ;
#140387 = CARTESIAN_POINT ( 'NONE',  ( -20.94999999999999929, 64.40000000001190017, -96.09490425424884563 ) ) ;
#140388 = AXIS2_PLACEMENT_3D ( 'NONE', #120465, #23928, #86405 ) ;
#140389 = DIRECTION ( 'NONE',  ( 0.000000000000000000, 0.000000000000000000, -1.000000000000000000 ) ) ;
#140390 = ADVANCED_FACE ( 'NONE', ( #88559 ), #247656, .T. ) ;
#140391 = ORIENTED_EDGE ( 'NONE', *, *, #256074, .T. ) ;
#140392 = VECTOR ( 'NONE', #152187, 1000.000000000000000 ) ;
#140393 = EDGE_CURVE ( 'NONE', #39510, #197787, #189229, .T. ) ;
#140395 = ORIENTED_EDGE ( 'NONE', *, *, #134714, .T. ) ;
#140394 = DIRECTION ( 'NONE',  ( -0.000000000000000000, -0.9876197685951290106, 0.1568667991644625281 ) ) ;
#140396 = EDGE_CURVE ( 'NONE', #185172, #217355, #229390, .T. ) ;
#140397 = CARTESIAN_POINT ( 'NONE',  ( -17.11825945287481332, 10.05000000001113847, -87.75000000000005684 ) ) ;
#140398 = CARTESIAN_POINT ( 'NONE',  ( -20.64999999999999858, 4.350000000011156054, -88.15000000000004832 ) ) ;
#140399 = DIRECTION ( 'NONE',  ( 1.000000000000000000, 0.000000000000000000, 0.000000000000000000 ) ) ;
#140400 = DIRECTION ( 'NONE',  ( -1.000000000000000000, 0.000000000000000000, 0.000000000000000000 ) ) ;
#140401 = AXIS2_PLACEMENT_3D ( 'NONE', #133510, #116526, #17416 ) ;
#140402 = CARTESIAN_POINT ( 'NONE',  ( -16.85718274719427257, 9.976142314632859609, -46.06334633218259000 ) ) ;
#140403 = CARTESIAN_POINT ( 'NONE',  ( -18.50000000000000000, -1.866714910057309273, -11.75267524628200633 ) ) ;
#140405 = ORIENTED_EDGE ( 'NONE', *, *, #85734, .T. ) ;
#140404 = CIRCLE ( 'NONE', #185821, 4.100000000000008527 ) ;
#140406 = DIRECTION ( 'NONE',  ( 0.000000000000000000, 2.891205793294679805E-16, -1.000000000000000000 ) ) ;
#140407 = CARTESIAN_POINT ( 'NONE',  ( -16.78569801330232281, 9.947933733124651567, -146.6569129053475251 ) ) ;
#140408 = AXIS2_PLACEMENT_3D ( 'NONE', #159308, #139702, #60173 ) ;
#140409 = TOROIDAL_SURFACE ( 'NONE', #40509, 0.4000000000000005773, 0.1000000000000000056 ) ;
#140410 = CARTESIAN_POINT ( 'NONE',  ( -18.47130263965429720, 77.20275754622504394, -241.7661513169259422 ) ) ;
#140411 = FACE_OUTER_BOUND ( 'NONE', #243875, .T. ) ;
#140412 = CARTESIAN_POINT ( 'NONE',  ( 20.77526135991769607, 67.06799098339034515, -61.05453894179962049 ) ) ;
#140413 = CIRCLE ( 'NONE', #103000, 0.09999999999999939493 ) ;
#140414 = EDGE_CURVE ( 'NONE', #80413, #74293, #248954, .T. ) ;
#140415 = EDGE_CURVE ( 'NONE', #244854, #249043, #143426, .T. ) ;
#140416 = EDGE_LOOP ( 'NONE', ( #59953, #61222, #112976, #81467 ) ) ;
#140417 = VERTEX_POINT ( 'NONE', #89852 ) ;
#140418 = CARTESIAN_POINT ( 'NONE',  ( 20.94999999999999574, 18.89897916088800756, -232.6070900604709379 ) ) ;
#140419 = LINE ( 'NONE', #157467, #167680 ) ;
#140420 = DIRECTION ( 'NONE',  ( 1.000000000000000000, 0.000000000000000000, 0.000000000000000000 ) ) ;
#140421 = CARTESIAN_POINT ( 'NONE',  ( 21.05315837326108763, 17.15379753644537786, -224.5473496284387238 ) ) ;
#140422 = ORIENTED_EDGE ( 'NONE', *, *, #250407, .T. ) ;
#140423 = CARTESIAN_POINT ( 'NONE',  ( -18.40000000000000213, 34.05335961020092128, -234.8258093264404351 ) ) ;
#140424 = AXIS2_PLACEMENT_3D ( 'NONE', #157704, #152557, #217601 ) ;
#140425 = CARTESIAN_POINT ( 'NONE',  ( 21.05000000000000071, 0.09779029131994770863, -94.24218538952391100 ) ) ;
#140426 = AXIS2_PLACEMENT_3D ( 'NONE', #223821, #201708, #163877 ) ;
#140427 = CARTESIAN_POINT ( 'NONE',  ( 20.94999999999999929, 65.71172719659838890, -223.0701118083454446 ) ) ;
#140428 = EDGE_CURVE ( 'NONE', #123153, #208014, #64143, .T. ) ;
#140429 = CARTESIAN_POINT ( 'NONE',  ( -18.39999999999999858, -9.519327731092436906, -6.972976376559334888 ) ) ;
#140430 = ADVANCED_FACE ( 'NONE', ( #187703 ), #168165, .T. ) ;
#140431 = CIRCLE ( 'NONE', #48859, 0.09999999999999939493 ) ;
#140432 = ORIENTED_EDGE ( 'NONE', *, *, #170940, .T. ) ;
#140433 = CARTESIAN_POINT ( 'NONE',  ( -20.54999999999999716, 1.115600667400684642E-11, -68.90000000000000568 ) ) ;
#140434 = ORIENTED_EDGE ( 'NONE', *, *, #211974, .T. ) ;
#140435 = CARTESIAN_POINT ( 'NONE',  ( -21.05000000000000071, 75.90220970870291239, -75.78092209500044873 ) ) ;
#140436 = CARTESIAN_POINT ( 'NONE',  ( 21.05000000000000071, 69.69548367074834516, -170.0020041764652774 ) ) ;
#140437 = CARTESIAN_POINT ( 'NONE',  ( -21.09107601085565520, 10.09916211269090880, -228.1044125031166061 ) ) ;
#140438 = ADVANCED_FACE ( 'NONE', ( #52002 ), #211099, .F. ) ;
#140439 = CARTESIAN_POINT ( 'NONE',  ( 18.51024323315077069, 65.68895814178219439, -64.00265578621379348 ) ) ;
#140440 = CARTESIAN_POINT ( 'NONE',  ( 18.52928932188133970, 10.27928932189250411, -192.1499999999999488 ) ) ;
#140441 = CARTESIAN_POINT ( 'NONE',  ( 21.05000000000000071, 67.22371710471985295, -161.4644784893834810 ) ) ;
#140442 = CARTESIAN_POINT ( 'NONE',  ( -22.50000000000000000, 76.00000000001242029, -176.2731074845243597 ) ) ;
#140443 = CARTESIAN_POINT ( 'NONE',  ( 21.14999999999999858, 64.04577702392042227, -222.1950530992138226 ) ) ;
#140444 = ADVANCED_FACE ( 'NONE', ( #195085 ), #76964, .T. ) ;
#140445 = CARTESIAN_POINT ( 'NONE',  ( 5.999999999999995559, -11.34999999999999964, 10.10000000000000142 ) ) ;
#140446 = DIRECTION ( 'NONE',  ( 0.000000000000000000, -6.652207440891584540E-15, 1.000000000000000000 ) ) ;
#140447 = CARTESIAN_POINT ( 'NONE',  ( -20.54999999999999716, 29.07070048091676995, -242.7637123387158624 ) ) ;
#140448 = CYLINDRICAL_SURFACE ( 'NONE', #56445, 0.09999999999998898659 ) ;
#140449 = EDGE_CURVE ( 'NONE', #131787, #221121, #114386, .T. ) ;
#140450 = VECTOR ( 'NONE', #66343, 1000.000000000000000 ) ;
#140451 = AXIS2_PLACEMENT_3D ( 'NONE', #191420, #170595, #94842 ) ;
#140452 = CIRCLE ( 'NONE', #132094, 0.1000000000000023231 ) ;
#140453 = CIRCLE ( 'NONE', #252891, 7.900000000000010125 ) ;
#140454 = FACE_OUTER_BOUND ( 'NONE', #95657, .T. ) ;
#140455 = DIRECTION ( 'NONE',  ( -0.000000000000000000, -0.000000000000000000, 1.000000000000000000 ) ) ;
#140456 = VERTEX_POINT ( 'NONE', #67734 ) ;
#140457 = CARTESIAN_POINT ( 'NONE',  ( 21.14999999999999858, 6.540656951701244282, -9.351243737687475743E-16 ) ) ;
#140458 = DIRECTION ( 'NONE',  ( 0.000000000000000000, -6.982962677686266711E-15, 1.000000000000000000 ) ) ;
#140459 = CARTESIAN_POINT ( 'NONE',  ( 11.60000000000000142, -8.279289321881350361, 15.00000000000000355 ) ) ;
#140460 = EDGE_CURVE ( 'NONE', #194241, #177733, #47730, .T. ) ;
#140461 = ORIENTED_EDGE ( 'NONE', *, *, #250588, .F. ) ;
#140462 = CARTESIAN_POINT ( 'NONE',  ( -22.44366136229477249, 0.009341569497225223756, -55.35028144252613203 ) ) ;
#140463 = DIRECTION ( 'NONE',  ( -0.000000000000000000, -0.1350103645451928291, -0.9908441862701594660 ) ) ;
#140464 = EDGE_CURVE ( 'NONE', #183161, #198203, #139302, .T. ) ;
#140465 = ORIENTED_EDGE ( 'NONE', *, *, #194627, .F. ) ;
#140466 = VECTOR ( 'NONE', #199571, 1000.000000000000227 ) ;
#140467 = CARTESIAN_POINT ( 'NONE',  ( -16.86733706339143168, 9.965990529650822438, -188.4031153019986675 ) ) ;
#140468 = CARTESIAN_POINT ( 'NONE',  ( 20.94999999999999929, 87.65000000001244018, -170.0231074845242745 ) ) ;
#140469 = CIRCLE ( 'NONE', #215499, 0.1000000000000028644 ) ;
#140470 = ORIENTED_EDGE ( 'NONE', *, *, #173356, .T. ) ;
#140471 = CIRCLE ( 'NONE', #227980, 0.6000000000000033085 ) ;
#140472 = EDGE_LOOP ( 'NONE', ( #106622, #81516, #64700, #117037 ) ) ;
#140473 = DIRECTION ( 'NONE',  ( 1.000000000000000000, 0.000000000000000000, 0.000000000000000000 ) ) ;
#140474 = VERTEX_POINT ( 'NONE', #138893 ) ;
#140475 = DIRECTION ( 'NONE',  ( 0.000000000000000000, 0.000000000000000000, -1.000000000000000000 ) ) ;
#140476 = CARTESIAN_POINT ( 'NONE',  ( -18.59999999999999787, 76.00000000001267608, -203.5231074845243597 ) ) ;
#140477 = CARTESIAN_POINT ( 'NONE',  ( -20.94999999999999929, 14.09264586382695938, -237.4630250429333671 ) ) ;
#140478 = DIRECTION ( 'NONE',  ( -0.000000000000000000, -0.000000000000000000, -1.000000000000000000 ) ) ;
#140479 = CARTESIAN_POINT ( 'NONE',  ( -16.89935556175678855, 66.05000000001231797, -156.8834311216385515 ) ) ;
#140480 = DIRECTION ( 'NONE',  ( 0.000000000000000000, -0.8814952561688430555, 0.4721928772777346239 ) ) ;
#140481 = DIRECTION ( 'NONE',  ( 0.7071067811865462405, -0.3338907855510739875, -0.6233112732207629625 ) ) ;
#140482 = CARTESIAN_POINT ( 'NONE',  ( 21.46681500598086956, 1.083969783934416675, -230.4946333871058926 ) ) ;
#140484 = ORIENTED_EDGE ( 'NONE', *, *, #10190, .T. ) ;
#140483 = DIRECTION ( 'NONE',  ( 1.000000000000000000, 7.304098846218134667E-16, 0.000000000000000000 ) ) ;
#140485 = VERTEX_POINT ( 'NONE', #256240 ) ;
#140487 = DIRECTION ( 'NONE',  ( -0.000000000000000000, -0.8660254037844420383, 0.4999999999999943379 ) ) ;
#140486 = CARTESIAN_POINT ( 'NONE',  ( 22.40000000000020819, -0.1008583690996671112, 11.74956712348970100 ) ) ;
#140489 = ORIENTED_EDGE ( 'NONE', *, *, #188098, .T. ) ;
#140488 = DIRECTION ( 'NONE',  ( 0.000000000000000000, 0.2617529984165152257, 0.9651348961777124202 ) ) ;
#140490 = CIRCLE ( 'NONE', #165467, 4.049999999999998934 ) ;
#140491 = ORIENTED_EDGE ( 'NONE', *, *, #84, .T. ) ;
#140492 = CARTESIAN_POINT ( 'NONE',  ( -20.64999999999999858, 65.40605961984560679, -236.6728003091511425 ) ) ;
#140493 = DIRECTION ( 'NONE',  ( -1.000000000000000000, 0.000000000000000000, 0.000000000000000000 ) ) ;
#140494 = DIRECTION ( 'NONE',  ( -1.000000000000000000, -0.000000000000000000, -0.000000000000000000 ) ) ;
#140495 = CYLINDRICAL_SURFACE ( 'NONE', #235102, 0.09999999999999063804 ) ;
#140497 = CARTESIAN_POINT ( 'NONE',  ( -23.25000000000000000, 4.150000000011156764, -188.6499999999999488 ) ) ;
#140496 = AXIS2_PLACEMENT_3D ( 'NONE', #24343, #77861, #58291 ) ;
#140498 = DIRECTION ( 'NONE',  ( 0.000000000000000000, 0.4930308989875230585, 0.8700118002898322711 ) ) ;
#140500 = CIRCLE ( 'NONE', #173900, 0.09999999999999749367 ) ;
#140499 = CARTESIAN_POINT ( 'NONE',  ( -21.14999999999999858, 11.65000000000000036, -0.1000000000000028644 ) ) ;
#140501 = ORIENTED_EDGE ( 'NONE', *, *, #137522, .T. ) ;
#140502 = ORIENTED_EDGE ( 'NONE', *, *, #138421, .T. ) ;
#140503 = CARTESIAN_POINT ( 'NONE',  ( 23.24999999999999645, 20.83093076766827423, -227.7429161672744442 ) ) ;
#140504 = VECTOR ( 'NONE', #131216, 1000.000000000000227 ) ;
#140505 = AXIS2_PLACEMENT_3D ( 'NONE', #23298, #81917, #161518 ) ;
#140506 = ORIENTED_EDGE ( 'NONE', *, *, #209698, .T. ) ;
#140507 = FACE_OUTER_BOUND ( 'NONE', #176986, .T. ) ;
#140508 = ORIENTED_EDGE ( 'NONE', *, *, #145840, .F. ) ;
#140509 = CARTESIAN_POINT ( 'NONE',  ( -18.39999999999999858, 40.43017315096746955, -235.2838021754311058 ) ) ;
#140510 = PRODUCT_DEFINITION_FORMATION_WITH_SPECIFIED_SOURCE ( 'ANY', '', #205405, .NOT_KNOWN. ) ;
#140511 = AXIS2_PLACEMENT_3D ( 'NONE', #195499, #58502, #136767 ) ;
#140512 = PLANE ( 'NONE',  #92633 ) ;
#140513 = DIRECTION ( 'NONE',  ( 0.000000000000000000, 7.086529944415894657E-15, -1.000000000000000000 ) ) ;
#140514 = TOROIDAL_SURFACE ( 'NONE', #144620, 0.2000000000000000111, 0.1000000000000000056 ) ;
#140515 = ADVANCED_FACE ( 'NONE', ( #121945 ), #74577, .F. ) ;
#140516 = DIRECTION ( 'NONE',  ( -0.000000000000000000, 1.000000000000000000, -0.000000000000000000 ) ) ;
#140517 = CARTESIAN_POINT ( 'NONE',  ( 19.75857864376268935, 34.44688795055758135, -235.1500552906961730 ) ) ;
#140518 = ORIENTED_EDGE ( 'NONE', *, *, #71824, .F. ) ;
#140519 = FACE_OUTER_BOUND ( 'NONE', #225993, .T. ) ;
#140520 = VERTEX_POINT ( 'NONE', #218452 ) ;
#140521 = EDGE_CURVE ( 'NONE', #9696, #152504, #235191, .T. ) ;
#140522 = EDGE_CURVE ( 'NONE', #231766, #54998, #147708, .T. ) ;
#140523 = CARTESIAN_POINT ( 'NONE',  ( -21.14999999999999858, 55.89093952297024970, -232.7795287750844579 ) ) ;
#140524 = DIRECTION ( 'NONE',  ( 0.000000000000000000, 1.181088324069315448E-15, 1.000000000000000000 ) ) ;
#140525 = DIRECTION ( 'NONE',  ( 0.000000000000000000, 1.000000000000000000, 0.000000000000000000 ) ) ;
#140526 = ORIENTED_EDGE ( 'NONE', *, *, #96418, .F. ) ;
#140527 = CARTESIAN_POINT ( 'NONE',  ( -21.00448002041605733, 64.25000000001189449, -96.17476662221315564 ) ) ;
#140528 = TOROIDAL_SURFACE ( 'NONE', #198801, 11.65000000000000036, 0.1000000000000000056 ) ;
#140529 = ORIENTED_EDGE ( 'NONE', *, *, #257733, .T. ) ;
#140532 = ORIENTED_EDGE ( 'NONE', *, *, #40936, .F. ) ;
#140531 = CARTESIAN_POINT ( 'NONE',  ( 21.05000000000000071, 6.257814610487280937, -66.90220970869124528 ) ) ;
#140530 = FACE_OUTER_BOUND ( 'NONE', #254386, .T. ) ;
#140533 = CARTESIAN_POINT ( 'NONE',  ( -21.95218792049438861, 0.09902843981107177507, -160.2984924387532999 ) ) ;
#140534 = CIRCLE ( 'NONE', #40643, 0.09999999999999939493 ) ;
#140535 = CIRCLE ( 'NONE', #98818, 0.1000000000000001860 ) ;
#140536 = PLANE ( 'NONE',  #221004 ) ;
#140537 = ORIENTED_EDGE ( 'NONE', *, *, #64090, .F. ) ;
#140539 = CIRCLE ( 'NONE', #107796, 0.1000000000000028227 ) ;
#140538 = CARTESIAN_POINT ( 'NONE',  ( 18.50000000000000355, 85.40000000001209912, -129.6410656363516125 ) ) ;
#140540 = CIRCLE ( 'NONE', #115603, 0.1000000000000028783 ) ;
#140541 = EDGE_CURVE ( 'NONE', #207046, #22691, #189402, .T. ) ;
#140542 = CARTESIAN_POINT ( 'NONE',  ( -23.25000000000000000, 85.68240343348850274, -129.8662641071115047 ) ) ;
#140543 = CIRCLE ( 'NONE', #190477, 11.74999999999999645 ) ;
#140544 = DIRECTION ( 'NONE',  ( 1.000000000000000000, 0.000000000000000000, 0.000000000000000000 ) ) ;
#140545 = UNCERTAINTY_MEASURE_WITH_UNIT (LENGTH_MEASURE( 1.000000000000000082E-05 ), #164712, 'distance_accuracy_value', 'NONE');
#140547 = ORIENTED_EDGE ( 'NONE', *, *, #123670, .T. ) ;
#140546 = DIRECTION ( 'NONE',  ( -0.000000000000000000, -6.982962677686266711E-15, 1.000000000000000000 ) ) ;
#140548 = DIRECTION ( 'NONE',  ( -1.000000000000000000, 2.952720810173289112E-16, 2.061873921506763405E-30 ) ) ;
#140549 = EDGE_LOOP ( 'NONE', ( #125090, #238757, #161526 ) ) ;
#140550 = DIRECTION ( 'NONE',  ( 2.952720810173289112E-16, 0.4088369013363280513, -0.9126074666063769270 ) ) ;
#140551 = FACE_OUTER_BOUND ( 'NONE', #46793, .T. ) ;
#140552 = DIRECTION ( 'NONE',  ( 0.000000000000000000, -1.000000000000000000, -6.982962677686266711E-15 ) ) ;
#140553 = TOROIDAL_SURFACE ( 'NONE', #73957, 11.65000000000000036, 0.1000000000000000056 ) ;
#140554 = ORIENTED_EDGE ( 'NONE', *, *, #18745, .F. ) ;
#140555 = CARTESIAN_POINT ( 'NONE',  ( -21.64999999999999858, 10.05000000001113847, -87.85000000000003695 ) ) ;
#140557 = ORIENTED_EDGE ( 'NONE', *, *, #133849, .F. ) ;
#140556 = AXIS2_PLACEMENT_3D ( 'NONE', #168402, #91387, #52231 ) ;
#140558 = DIRECTION ( 'NONE',  ( -0.000000000000000000, 1.000000000000000000, -0.000000000000000000 ) ) ;
#140559 = ADVANCED_FACE ( 'NONE', ( #241879 ), #63234, .F. ) ;
#140560 = DIRECTION ( 'NONE',  ( 1.186688945009010077E-16, 1.000000000000000000, 6.982962677686266711E-15 ) ) ;
#140561 = FACE_OUTER_BOUND ( 'NONE', #31940, .T. ) ;
#140562 = ADVANCED_FACE ( 'NONE', ( #101033 ), #80206, .F. ) ;
#140563 = ORIENTED_EDGE ( 'NONE', *, *, #113471, .F. ) ;
#140564 = CARTESIAN_POINT ( 'NONE',  ( -20.54999999999999716, 66.65000000001150227, -48.37310748452438958 ) ) ;
#140565 = CARTESIAN_POINT ( 'NONE',  ( 21.05000000000000071, 71.00000000001230660, -157.6178414656113205 ) ) ;
#140566 = CIRCLE ( 'NONE', #61483, 0.09999999999998898659 ) ;
#140567 = CARTESIAN_POINT ( 'NONE',  ( 21.14999999999999858, 69.35000000001205933, -124.3731074845243540 ) ) ;
#140568 = CIRCLE ( 'NONE', #257061, 6.329289321881348407 ) ;
#140570 = EDGE_CURVE ( 'NONE', #230076, #163978, #113982, .T. ) ;
#140569 = VERTEX_POINT ( 'NONE', #159798 ) ;
#140571 = CARTESIAN_POINT ( 'NONE',  ( 13.40000000000000036, -8.250000000000005329, 15.00000000000000355 ) ) ;
#140572 = CARTESIAN_POINT ( 'NONE',  ( -18.40000000000000213, 54.05352898164365882, -229.1867466607862127 ) ) ;
#140573 = AXIS2_PLACEMENT_3D ( 'NONE', #212923, #72143, #133392 ) ;
#140574 = ORIENTED_EDGE ( 'NONE', *, *, #126665, .F. ) ;
#140575 = CARTESIAN_POINT ( 'NONE',  ( -23.15000000000000213, -11.65000000000000036, -30.50000000000000000 ) ) ;
#140576 = VERTEX_POINT ( 'NONE', #119382 ) ;
#140577 = EDGE_LOOP ( 'NONE', ( #9353, #169396, #9448, #59809 ) ) ;
#140578 = AXIS2_PLACEMENT_3D ( 'NONE', #233953, #55280, #134825 ) ;
#140579 = CARTESIAN_POINT ( 'NONE',  ( 21.87500000000000355, 12.15477401631902588, -210.9923204818763622 ) ) ;
#140580 = ORIENTED_EDGE ( 'NONE', *, *, #141465, .T. ) ;
#140581 = ORIENTED_EDGE ( 'NONE', *, *, #192727, .T. ) ;
#140585 = EDGE_CURVE ( 'NONE', #89464, #114288, #185765, .T. ) ;
#140584 = EDGE_LOOP ( 'NONE', ( #169890, #257862, #15851, #222762 ) ) ;
#140583 = ORIENTED_EDGE ( 'NONE', *, *, #21238, .F. ) ;
#140582 = CARTESIAN_POINT ( 'NONE',  ( 18.59999999999999076, 6.550000000000000711, -21.15000000000000213 ) ) ;
#140586 = CARTESIAN_POINT ( 'NONE',  ( -17.71734398241073905, 10.84235722847571814, -77.27486174699446053 ) ) ;
#140587 = FACE_OUTER_BOUND ( 'NONE', #7865, .T. ) ;
#140588 = AXIS2_PLACEMENT_3D ( 'NONE', #133639, #213170, #29450 ) ;
#140589 = DIRECTION ( 'NONE',  ( 0.000000000000000000, -6.547589603894048205E-15, 1.000000000000000000 ) ) ;
#140590 = VECTOR ( 'NONE', #52936, 1000.000000000000000 ) ;
#140591 = CARTESIAN_POINT ( 'NONE',  ( 20.94999999999999929, 1.115600667400684642E-11, -134.0000000000000284 ) ) ;
#140592 = LINE ( 'NONE', #23254, #253214 ) ;
#140593 = B_SPLINE_CURVE_WITH_KNOTS ( 'NONE', 3,
 ( #131017, #232709, #189715, #50182, #170203, #132298, #129736, #252240, #250949, #112746 ),
 .UNSPECIFIED., .F., .F.,
 ( 4, 3, 3, 4 ),
 ( 0.000000000000000000, 1.004626015992112955E-05, 1.831183478184268218E-05, 2.062343583996018031E-05 ),
 .UNSPECIFIED. ) ;
#140594 = CARTESIAN_POINT ( 'NONE',  ( 21.05000000000000071, 1.115600667400684642E-11, -100.5000000000000284 ) ) ;
#140595 = AXIS2_PLACEMENT_3D ( 'NONE', #227548, #48907, #187165 ) ;
#140596 = DIRECTION ( 'NONE',  ( 0.000000000000000000, 1.000000000000000000, 0.000000000000000000 ) ) ;
#140598 = DIRECTION ( 'NONE',  ( 6.938893903907030216E-14, 0.000000000000000000, -1.000000000000000000 ) ) ;
#140597 = CARTESIAN_POINT ( 'NONE',  ( 20.94999999999999574, 1.148907358139439339E-11, -201.0000000000015064 ) ) ;
#140599 = VERTEX_POINT ( 'NONE', #204036 ) ;
#140600 = ORIENTED_EDGE ( 'NONE', *, *, #221688, .F. ) ;
#140601 = EDGE_CURVE ( 'NONE', #128152, #62001, #239284, .T. ) ;
#140602 = CARTESIAN_POINT ( 'NONE',  ( -21.65000000000000213, 7.250000000011138646, -113.1500000000000341 ) ) ;
#140603 = EDGE_CURVE ( 'NONE', #253474, #256624, #207919, .T. ) ;
#140605 = VERTEX_POINT ( 'NONE', #188333 ) ;
#140604 = DIRECTION ( 'NONE',  ( -1.000000000000000000, 0.000000000000000000, -0.000000000000000000 ) ) ;
#140606 = ORIENTED_EDGE ( 'NONE', *, *, #3754, .T. ) ;
#140607 = CARTESIAN_POINT ( 'NONE',  ( -16.78569801330232281, 12.41348556013404192, -211.2500832240831130 ) ) ;
#140608 = ORIENTED_EDGE ( 'NONE', *, *, #191621, .T. ) ;
#140609 = DIRECTION ( 'NONE',  ( -1.000000000000000000, -8.673617379884087537E-15, 0.000000000000000000 ) ) ;
#140610 = ADVANCED_FACE ( 'NONE', ( #46242 ), #216164, .T. ) ;
#140611 = EDGE_CURVE ( 'NONE', #112449, #229099, #89223, .T. ) ;
#140612 = VECTOR ( 'NONE', #608, 1000.000000000000000 ) ;
#140613 = EDGE_LOOP ( 'NONE', ( #81921, #24400, #194695, #70669 ) ) ;
#140614 = FACE_OUTER_BOUND ( 'NONE', #134882, .T. ) ;
#140615 = CARTESIAN_POINT ( 'NONE',  ( -21.05000000000000071, -9.519327731081284938, -174.4729763765593020 ) ) ;
#140616 = CIRCLE ( 'NONE', #28234, 0.1999999999999987899 ) ;
#140617 = EDGE_CURVE ( 'NONE', #249928, #222594, #89432, .T. ) ;
#140619 = ORIENTED_EDGE ( 'NONE', *, *, #81253, .F. ) ;
#140618 = EDGE_LOOP ( 'NONE', ( #137035, #250300, #246428, #138869, #200228 ) ) ;
#140620 = ORIENTED_EDGE ( 'NONE', *, *, #99661, .T. ) ;
#140622 = ADVANCED_FACE ( 'NONE', ( #184467 ), #243163, .F. ) ;
#140621 = CARTESIAN_POINT ( 'NONE',  ( 18.54999999999999716, 26.68086916408615750, -212.3318337774905160 ) ) ;
#140623 = VERTEX_POINT ( 'NONE', #244443 ) ;
#140624 = EDGE_LOOP ( 'NONE', ( #147878, #255976, #206843, #57529 ) ) ;
#140625 = FACE_OUTER_BOUND ( 'NONE', #119276, .T. ) ;
#140627 = ORIENTED_EDGE ( 'NONE', *, *, #98136, .F. ) ;
#140626 = CARTESIAN_POINT ( 'NONE',  ( -22.94999999999999929, 1.885425182446134107, -11.49641995933507843 ) ) ;
#140628 = ADVANCED_FACE ( 'NONE', ( #106203 ), #93531, .T. ) ;
#140629 = DIRECTION ( 'NONE',  ( 0.000000000000000000, 0.9126074666063770380, 0.4088369013363281068 ) ) ;
#140630 = DIRECTION ( 'NONE',  ( 0.000000000000000000, -6.982962677686266711E-15, 1.000000000000000000 ) ) ;
#140631 = DIRECTION ( 'NONE',  ( -0.000000000000000000, 1.000000000000000000, 0.000000000000000000 ) ) ;
#140632 = CARTESIAN_POINT ( 'NONE',  ( -21.59780538579341425, 6.847090529954407145, -66.90102133040205956 ) ) ;
#140633 = ORIENTED_EDGE ( 'NONE', *, *, #220577, .T. ) ;
#140634 = ORIENTED_EDGE ( 'NONE', *, *, #13424, .F. ) ;
#140635 = DIRECTION ( 'NONE',  ( -1.000000000000000000, -0.000000000000000000, -0.000000000000000000 ) ) ;
#140636 = CARTESIAN_POINT ( 'NONE',  ( -16.86379686415369150, 66.02478224075908031, -149.0897175954341662 ) ) ;
#140638 = EDGE_CURVE ( 'NONE', #46071, #85130, #26932, .T. ) ;
#140637 = DIRECTION ( 'NONE',  ( 0.000000000000000000, -6.982962677686266711E-15, 1.000000000000000000 ) ) ;
#140639 = ORIENTED_EDGE ( 'NONE', *, *, #145628, .F. ) ;
#140640 = AXIS2_PLACEMENT_3D ( 'NONE', #217377, #40075, #195296 ) ;
#140641 = CIRCLE ( 'NONE', #232257, 2.000000000000002665 ) ;
#140642 = DIRECTION ( 'NONE',  ( 0.000000000000000000, 0.4088369013363287729, -0.9126074666063767049 ) ) ;
#140643 = EDGE_CURVE ( 'NONE', #6026, #64921, #18530, .T. ) ;
#140644 = ADVANCED_FACE ( 'NONE', ( #248307 ), #143606, .T. ) ;
#140645 = DIRECTION ( 'NONE',  ( 0.000000000000000000, -0.2617529984165152257, -0.9651348961777124202 ) ) ;
#140646 = PLANE ( 'NONE',  #26850 ) ;
#140647 = ORIENTED_EDGE ( 'NONE', *, *, #34925, .F. ) ;
#140648 = EDGE_LOOP ( 'NONE', ( #185109, #6836, #98564, #114291 ) ) ;
#140649 = EDGE_CURVE ( 'NONE', #212214, #130380, #183207, .T. ) ;
#140650 = CARTESIAN_POINT ( 'NONE',  ( 21.05000000000000071, 1.115600667400684642E-11, -146.9749999999999943 ) ) ;
#140651 = CARTESIAN_POINT ( 'NONE',  ( -23.25000000000000000, -9.599999999988845900, -191.1060308773475356 ) ) ;
#140652 = ORIENTED_EDGE ( 'NONE', *, *, #12566, .F. ) ;
#140653 = CARTESIAN_POINT ( 'NONE',  ( -21.05000000000000071, 1.115600667400684642E-11, -155.7000000000000455 ) ) ;
#140654 = VERTEX_POINT ( 'NONE', #167513 ) ;
#140655 = CARTESIAN_POINT ( 'NONE',  ( 20.94999999999999929, 67.63082410804655353, -211.8415745842588649 ) ) ;
#140656 = DIRECTION ( 'NONE',  ( 1.000000000000000000, 0.000000000000000000, 0.000000000000000000 ) ) ;
#140658 = CARTESIAN_POINT ( 'NONE',  ( -20.92356734117541706, 68.07764576057049055, -224.1679995073710359 ) ) ;
#140657 = DIRECTION ( 'NONE',  ( -1.000000000000000000, 0.000000000000000000, 0.000000000000000000 ) ) ;
#140659 = EDGE_CURVE ( 'NONE', #186279, #216286, #56098, .T. ) ;
#140661 = EDGE_CURVE ( 'NONE', #244782, #155996, #13558, .T. ) ;
#140660 = CARTESIAN_POINT ( 'NONE',  ( -21.05000000000000071, 76.00000000001244871, -170.0231074845243597 ) ) ;
#140662 = CARTESIAN_POINT ( 'NONE',  ( 23.14999999999999147, 1.115600667400684642E-11, -134.0000000000000000 ) ) ;
#140663 = TOROIDAL_SURFACE ( 'NONE', #161535, 11.70000000000000107, 0.1000000000000000056 ) ;
#140664 = EDGE_CURVE ( 'NONE', #35438, #252099, #231331, .T. ) ;
#140665 = ORIENTED_EDGE ( 'NONE', *, *, #191504, .T. ) ;
#140666 = TOROIDAL_SURFACE ( 'NONE', #69952, 12.97499999999999609, 0.1000000000000000056 ) ;
#140667 = DIRECTION ( 'NONE',  ( 0.000000000000000000, -1.000000000000000000, 0.000000000000000000 ) ) ;
#140669 = ORIENTED_EDGE ( 'NONE', *, *, #17254, .T. ) ;
#140668 = ORIENTED_EDGE ( 'NONE', *, *, #252765, .F. ) ;
#140670 = CIRCLE ( 'NONE', #178299, 0.09999999999999939493 ) ;
#140671 = ORIENTED_EDGE ( 'NONE', *, *, #202883, .F. ) ;
#140672 = ORIENTED_EDGE ( 'NONE', *, *, #167771, .F. ) ;
#140673 = CARTESIAN_POINT ( 'NONE',  ( 21.95218792049437795, 7.201507561257818324, -33.40097156020008384 ) ) ;
#140674 = DIRECTION ( 'NONE',  ( 0.000000000000000000, 0.000000000000000000, -1.000000000000000000 ) ) ;
#140675 = DIRECTION ( 'NONE',  ( -0.000000000000000000, -1.265107689135680095E-16, 1.000000000000000000 ) ) ;
#140676 = LINE ( 'NONE', #41607, #11246 ) ;
#140677 = DIRECTION ( 'NONE',  ( -1.000000000000000000, 0.000000000000000000, 0.000000000000000000 ) ) ;
#140678 = ADVANCED_FACE ( 'NONE', ( #172673 ), #126856, .T. ) ;
#140680 = CARTESIAN_POINT ( 'NONE',  ( -23.25000000000000000, 7.021664781911246322, -204.8335654018972605 ) ) ;
#140679 = CARTESIAN_POINT ( 'NONE',  ( -18.50000000000000000, 66.85000000001221565, -148.2731074845243597 ) ) ;
#140681 = ORIENTED_EDGE ( 'NONE', *, *, #203497, .T. ) ;
#140682 = CARTESIAN_POINT ( 'NONE',  ( 23.14999999999999858, 76.00000000001247713, -174.0231074845243882 ) ) ;
#140683 = VERTEX_POINT ( 'NONE', #250858 ) ;
#140684 = CARTESIAN_POINT ( 'NONE',  ( -22.48660254037843487, 11.75000000001115730, -66.95000000000007390 ) ) ;
#140685 = ORIENTED_EDGE ( 'NONE', *, *, #17983, .F. ) ;
#140686 = VERTEX_POINT ( 'NONE', #33152 ) ;
#140687 = DIRECTION ( 'NONE',  ( 0.000000000000000000, -7.487053152578127080E-15, 1.000000000000000000 ) ) ;
#140688 = CARTESIAN_POINT ( 'NONE',  ( -20.54999999999999716, 71.65000000001180069, -81.87310748452433984 ) ) ;
#140689 = LINE ( 'NONE', #220247, #196017 ) ;
#140690 = DIRECTION ( 'NONE',  ( 0.000000000000000000, 0.000000000000000000, -1.000000000000000000 ) ) ;
#140691 = AXIS2_PLACEMENT_3D ( 'NONE', #30060, #109550, #189109 ) ;
#140692 = CIRCLE ( 'NONE', #82400, 0.09999999999999062417 ) ;
#140693 = B_SPLINE_CURVE_WITH_KNOTS ( 'NONE', 3,
 ( #119914, #237268, #18216, #217668, #160321, #121202 ),
 .UNSPECIFIED., .F., .F.,
 ( 4, 2, 4 ),
 ( 0.000000000000000000, 0.0001569047307838622170, 0.0003138094615677244339 ),
 .UNSPECIFIED. ) ;
#140694 = DIRECTION ( 'NONE',  ( -1.000000000000000000, -2.952720810173289112E-16, 0.000000000000000000 ) ) ;
#140695 = VERTEX_POINT ( 'NONE', #173960 ) ;
#140696 = ORIENTED_EDGE ( 'NONE', *, *, #198474, .F. ) ;
#140697 = DIRECTION ( 'NONE',  ( -1.020425574104004196E-15, -1.210927747993693964E-31, 1.000000000000000000 ) ) ;
#140698 = EDGE_LOOP ( 'NONE', ( #34461, #214949, #242722, #79152 ) ) ;
#140699 = DIRECTION ( 'NONE',  ( 0.000000000000000000, 0.000000000000000000, -1.000000000000000000 ) ) ;
#140700 = DIRECTION ( 'NONE',  ( 0.000000000000000000, -7.026728003956683390E-15, 1.000000000000000000 ) ) ;
#140701 = TOROIDAL_SURFACE ( 'NONE', #203046, 4.099999999999999645, 0.1000000000000000056 ) ;
#140702 = DIRECTION ( 'NONE',  ( 0.000000000000000000, 0.000000000000000000, 1.000000000000000000 ) ) ;
#140703 = CARTESIAN_POINT ( 'NONE',  ( 20.94999999999999929, 10.72371710471868056, -45.65000000000000568 ) ) ;
#140704 = CARTESIAN_POINT ( 'NONE',  ( -21.65000000000000213, 66.05000000001157900, -56.87310748452438958 ) ) ;
#140705 = DIRECTION ( 'NONE',  ( 0.000000000000000000, 0.8814952561688449428, -0.4721928772777310157 ) ) ;
#140706 = LINE ( 'NONE', #198117, #149904 ) ;
#140707 = VECTOR ( 'NONE', #61276, 1000.000000000000000 ) ;
#140708 = CARTESIAN_POINT ( 'NONE',  ( 18.58143601961851843, 65.56427058491756554, -178.7731074845244166 ) ) ;
#140709 = ADVANCED_FACE ( 'NONE', ( #209174 ), #30566, .T. ) ;
#140710 = DIRECTION ( 'NONE',  ( 0.000000000000000000, 0.5283051335750404975, -0.8490545835446967615 ) ) ;
#140711 = CIRCLE ( 'NONE', #178146, 0.4000000000000010214 ) ;
#140712 = AXIS2_PLACEMENT_3D ( 'NONE', #176611, #13665, #256062 ) ;
#140713 = EDGE_CURVE ( 'NONE', #198087, #37506, #112653, .T. ) ;
#140714 = CIRCLE ( 'NONE', #115770, 0.09999999999999939493 ) ;
#140715 = EDGE_LOOP ( 'NONE', ( #24112, #77364, #23312 ) ) ;
#140716 = EDGE_CURVE ( 'NONE', #116058, #252068, #135210, .T. ) ;
#140717 = LINE ( 'NONE', #199434, #137041 ) ;
#140718 = AXIS2_PLACEMENT_3D ( 'NONE', #56641, #157083, #80053 ) ;
#140719 = ADVANCED_FACE ( 'NONE', ( #192203 ), #230024, .T. ) ;
#140720 = VERTEX_POINT ( 'NONE', #90501 ) ;
#140721 = APPLICATION_CONTEXT ( 'automotive_design' ) ;
#140722 = CARTESIAN_POINT ( 'NONE',  ( -18.50000000000000000, 1.115600667400684642E-11, -100.5000000000000426 ) ) ;
#140723 = DIRECTION ( 'NONE',  ( 0.000000000000000000, 0.9983803033886529121, 0.05689261644169053833 ) ) ;
#140724 = DIRECTION ( 'NONE',  ( 0.000000000000000000, -0.4721928772777402861, -0.8814952561688399468 ) ) ;
#140725 = ORIENTED_EDGE ( 'NONE', *, *, #5642, .F. ) ;
#140726 = DIRECTION ( 'NONE',  ( -2.978066053179067751E-16, 1.000000000000000000, 0.000000000000000000 ) ) ;
#140727 = LINE ( 'NONE', #102862, #27204 ) ;
#140728 = FACE_OUTER_BOUND ( 'NONE', #1994, .T. ) ;
#140729 = AXIS2_PLACEMENT_3D ( 'NONE', #33079, #50021, #190856 ) ;
#140730 = DIRECTION ( 'NONE',  ( 0.000000000000000000, -0.000000000000000000, -1.000000000000000000 ) ) ;
#140731 = AXIS2_PLACEMENT_3D ( 'NONE', #6868, #129386, #29047 ) ;
#140732 = CARTESIAN_POINT ( 'NONE',  ( -16.93415306273742260, 9.995622260023669270, -121.4100569423604412 ) ) ;
#140733 = DIRECTION ( 'NONE',  ( -1.000000000000000000, -0.000000000000000000, -0.000000000000000000 ) ) ;
#140734 = CIRCLE ( 'NONE', #28346, 1.749999999999998002 ) ;
#140735 = AXIS2_PLACEMENT_3D ( 'NONE', #12021, #91540, #189360 ) ;
#140736 = ORIENTED_EDGE ( 'NONE', *, *, #10489, .F. ) ;
#140737 = DIRECTION ( 'NONE',  ( 0.000000000000000000, -0.000000000000000000, 1.000000000000000000 ) ) ;
#140740 = ORIENTED_EDGE ( 'NONE', *, *, #149458, .T. ) ;
#140739 = CARTESIAN_POINT ( 'NONE',  ( -20.54999999999999716, 63.44052078637213299, -222.1345147897817185 ) ) ;
#140738 = CIRCLE ( 'NONE', #174101, 2.000000000000001776 ) ;
#140741 = CARTESIAN_POINT ( 'NONE',  ( 20.99999999999999645, 9.750000000011137757, -42.75000000000000000 ) ) ;
#140742 =( BOUNDED_SURFACE ( )  B_SPLINE_SURFACE ( 3, 2, ( 
 ( #39548, #220715, #196031 ),
 ( #79884, #77337, #1648 ),
 ( #40826, #160774, #255936 ),
 ( #141184, #215570, #218123 ),
 ( #17384, #177763, #119058 ),
 ( #96873, #236422, #57773 ),
 ( #137311, #216852, #38238 ),
 ( #117757, #197293, #18664 ) ),
 .UNSPECIFIED., .F., .F., .F. ) 
 B_SPLINE_SURFACE_WITH_KNOTS ( ( 4, 2, 2, 4 ),
 ( 3, 3 ),
 ( 0.0001723339234021429623, 0.0002782939632049932365, 0.0003842540030078435377, 0.0005961740826135441401 ),
 ( 0.000000000000000000, 1.000000000000000000 ),
 .UNSPECIFIED. ) 
 GEOMETRIC_REPRESENTATION_ITEM ( )  RATIONAL_B_SPLINE_SURFACE ( (
 ( 1.000000000000000000, 0.9504532311154486601, 1.000000000000000000),
 ( 1.000000000000000000, 0.9506023220705424048, 1.000000000000000000),
 ( 1.000000000000000000, 0.9395774818187647703, 1.000000000000000000),
 ( 1.000000000000000000, 0.9079328464641989171, 1.000000000000000000),
 ( 1.000000000000000000, 0.8875702416207198464, 1.000000000000000000),
 ( 1.000000000000000000, 0.8205919608037975932, 1.000000000000000000),
 ( 1.000000000000000000, 0.7666842783600120725, 1.000000000000000000),
 ( 1.000000000000000000, 0.7071067811865088260, 1.000000000000000000) ) ) 
 REPRESENTATION_ITEM ( '' )  SURFACE ( )  );
#140743 = DIRECTION ( 'NONE',  ( 1.000000000000000000, 0.000000000000000000, 0.000000000000000000 ) ) ;
#140744 = AXIS2_PLACEMENT_3D ( 'NONE', #161102, #141517, #239347 ) ;
#140745 = FILL_AREA_STYLE ('',( #181174 ) ) ;
#140746 = EDGE_LOOP ( 'NONE', ( #128389, #36023, #146514, #192490 ) ) ;
#140747 = CARTESIAN_POINT ( 'NONE',  ( -22.47886152344871036, 75.96249906115053818, -148.1730961275722223 ) ) ;
#140748 = APPLICATION_PROTOCOL_DEFINITION ( 'draft international standard', 'automotive_design', 1998, #69159 ) ;
#140749 = DIRECTION ( 'NONE',  ( 0.000000000000000000, -0.8700118002898357128, 0.4930308989875170633 ) ) ;
#140750 = ORIENTED_EDGE ( 'NONE', *, *, #206842, .F. ) ;
#140751 = CARTESIAN_POINT ( 'NONE',  ( 23.14999999999998437, 80.05000000001194849, -103.0231074845242887 ) ) ;
#140752 = CARTESIAN_POINT ( 'NONE',  ( 15.57250062127603130, 9.370689921613767126, -185.0264651266610372 ) ) ;
#140753 = AXIS2_PLACEMENT_3D ( 'NONE', #132317, #93190, #171488 ) ;
#140754 = EDGE_CURVE ( 'NONE', #183242, #28201, #97598, .T. ) ;
#140755 = CIRCLE ( 'NONE', #28363, 0.1000000000000028644 ) ;
#140756 = AXIS2_PLACEMENT_3D ( 'NONE', #94225, #209048, #173827 ) ;
#140757 = CLOSED_SHELL ( 'NONE', ( #235431, #232580, #73815, #216014, #26053, #2718, #34959, #188571, #114335, #85099, #211480, #225308, #194841, #3836, #150412, #17334, #54791, #249665, #192960, #116637, #155794, #53487, #181783, #127138, #60856, #36856, #1233, #153096, #12720, #119646, #56782, #154050, #204025, #247071, #153873, #60937, #56974, #149848, #174546, #155233, #211945, #60921, #46006, #126601, #77378, #159074, #227503, #201291, #108653, #199151, #60985, #9591, #98422 ) ) ;
#140758 = DIRECTION ( 'NONE',  ( 1.000000000000000000, 0.000000000000000000, 0.000000000000000000 ) ) ;
#140759 = VERTEX_POINT ( 'NONE', #252145 ) ;
#140760 = EDGE_LOOP ( 'NONE', ( #176576, #49855, #188903, #59968, #91731 ) ) ;
#140761 = CARTESIAN_POINT ( 'NONE',  ( -18.59999999999999787, 74.75000000001159606, -61.52310748452433131 ) ) ;
#140762 = DIRECTION ( 'NONE',  ( 0.000000000000000000, -6.454785026890489601E-15, 1.000000000000000000 ) ) ;
#140763 = ADVANCED_FACE ( 'NONE', ( #50096 ), #35322, .T. ) ;
#140764 = CARTESIAN_POINT ( 'NONE',  ( 21.05000000000000071, 69.06797323185276127, -247.4100621602722470 ) ) ;
#140766 = CIRCLE ( 'NONE', #249125, 0.1000000000000028644 ) ;
#140765 = DIRECTION ( 'NONE',  ( -0.000000000000000000, 6.982962677686266711E-15, -1.000000000000000000 ) ) ;
#140767 = CARTESIAN_POINT ( 'NONE',  ( -18.40000000000000213, 11.47316190337362762, -79.55000000000005400 ) ) ;
#140768 = DIRECTION ( 'NONE',  ( -0.000000000000000000, 0.1298341882520022694, 0.9915357197604853789 ) ) ;
#140769 = ADVANCED_FACE ( 'NONE', ( #133494 ), #43654, .F. ) ;
#140770 = VECTOR ( 'NONE', #244894, 1000.000000000000000 ) ;
#140772 = CARTESIAN_POINT ( 'NONE',  ( -20.64999999999999858, 68.85000000001156195, -57.27310748452436684 ) ) ;
#140771 = CARTESIAN_POINT ( 'NONE',  ( -20.64999999999999858, 74.05981308412370367, -56.69398827347101388 ) ) ;
#140773 = FACE_OUTER_BOUND ( 'NONE', #199560, .T. ) ;
#140774 = CIRCLE ( 'NONE', #32678, 0.09999999999998898659 ) ;
#140775 = DIRECTION ( 'NONE',  ( 0.000000000000000000, 4.336808689942043768E-15, -1.000000000000000000 ) ) ;
#140776 = CARTESIAN_POINT ( 'NONE',  ( 22.41477678272288188, 0.0008238657741001837072, -155.8504147154845612 ) ) ;
#140777 = DIRECTION ( 'NONE',  ( 1.000000000000000000, 0.000000000000000000, 0.000000000000000000 ) ) ;
#140778 = ORIENTED_EDGE ( 'NONE', *, *, #172806, .T. ) ;
#140779 = ORIENTED_EDGE ( 'NONE', *, *, #115565, .T. ) ;
#140780 = CARTESIAN_POINT ( 'NONE',  ( -18.50000000000000000, -1.164121893230052995, -141.9148480855716343 ) ) ;
#140782 = DIRECTION ( 'NONE',  ( 1.652117596168391700E-15, -1.000000000000000000, -6.982962677686266711E-15 ) ) ;
#140781 = CARTESIAN_POINT ( 'NONE',  ( -20.94999999999999929, 77.16412189325258453, -28.10825939895270764 ) ) ;
#140783 = AXIS2_PLACEMENT_3D ( 'NONE', #29075, #109837, #251929 ) ;
#140784 = EDGE_CURVE ( 'NONE', #8311, #92109, #31233, .T. ) ;
#140785 = DIRECTION ( 'NONE',  ( 0.000000000000000000, 0.2128009952263605342, -0.9770955615653315052 ) ) ;
#140786 = CARTESIAN_POINT ( 'NONE',  ( -23.15000000000000213, -11.74999999998884448, -100.5000000000000284 ) ) ;
#140787 = LINE ( 'NONE', #159090, #214848 ) ;
#140788 = EDGE_CURVE ( 'NONE', #168638, #162902, #64500, .T. ) ;
#140789 = ORIENTED_EDGE ( 'NONE', *, *, #52352, .F. ) ;
#140790 = AXIS2_PLACEMENT_3D ( 'NONE', #123593, #107872, #127441 ) ;
#140791 = ADVANCED_FACE ( 'NONE', ( #95638 ), #73556, .T. ) ;
#140792 = FACE_OUTER_BOUND ( 'NONE', #159281, .T. ) ;
#140793 = ORIENTED_EDGE ( 'NONE', *, *, #144395, .T. ) ;
#140794 = AXIS2_PLACEMENT_3D ( 'NONE', #28505, #107996, #8896 ) ;
#140795 = AXIS2_PLACEMENT_3D ( 'NONE', #23988, #66939, #4387 ) ;
#140796 = ADVANCED_FACE ( 'NONE', ( #51349 ), #31857, .F. ) ;
#140797 = AXIS2_PLACEMENT_3D ( 'NONE', #95181, #193008, #70518 ) ;
#140798 = ORIENTED_EDGE ( 'NONE', *, *, #243166, .F. ) ;
#140799 = CARTESIAN_POINT ( 'NONE',  ( -18.59999999999999787, 9.350000000011156942, -54.65000000000000568 ) ) ;
#140800 = CIRCLE ( 'NONE', #232588, 0.1000000000000028644 ) ;
#140801 = B_SPLINE_CURVE_WITH_KNOTS ( 'NONE', 3,
 ( #121839, #201359, #145226, #162257, #86518, #107390, #245630, #5701, #241763, #184354, #26600, #46132, #143945, #125674, #224762, #141379, #64426, #63118, #244329 ),
 .UNSPECIFIED., .F., .F.,
 ( 4, 3, 3, 3, 3, 3, 4 ),
 ( 0.000000000000000000, 1.655171619026205498E-05, 2.773500582849481967E-05, 5.941817267378896972E-05, 0.0001114174635873591685, 0.0001914169455916391949, 0.0002627181070750695150 ),
 .UNSPECIFIED. ) ;
#140802 = CARTESIAN_POINT ( 'NONE',  ( -20.54999999999999716, 27.82649702422227733, -239.8850763025288870 ) ) ;
#140803 = ORIENTED_EDGE ( 'NONE', *, *, #1400, .T. ) ;
#140804 = DIRECTION ( 'NONE',  ( 0.000000000000000000, -6.982962677686266711E-15, 1.000000000000000000 ) ) ;
#140805 = ADVANCED_FACE ( 'NONE', ( #160793 ), #218408, .F. ) ;
#140806 = EDGE_LOOP ( 'NONE', ( #230702, #44011, #121197, #248442 ) ) ;
#140807 = CARTESIAN_POINT ( 'NONE',  ( -21.14999999999999858, 76.10000000001241460, -176.2731074845243597 ) ) ;
#140808 = CARTESIAN_POINT ( 'NONE',  ( 18.59999999999999432, 1.162701749938009677, -8.000000000000000000 ) ) ;
#140810 = CARTESIAN_POINT ( 'NONE',  ( -23.25000000000000000, -1.249999999999999334, -41.30048075441507649 ) ) ;
#140809 = AXIS2_PLACEMENT_3D ( 'NONE', #14158, #230624, #214893 ) ;
#140811 = CARTESIAN_POINT ( 'NONE',  ( -18.59999999999999787, -1.851028230129704522, -78.65391326942254580 ) ) ;
#140812 = DIRECTION ( 'NONE',  ( -1.000000000000000000, 0.000000000000000000, 0.000000000000000000 ) ) ;
#140814 = CARTESIAN_POINT ( 'NONE',  ( 18.55121869061587958, 65.67252876774553272, -130.9457041994994881 ) ) ;
#140813 = DIRECTION ( 'NONE',  ( 1.000000000000000000, 0.000000000000000000, -0.000000000000000000 ) ) ;
#140815 = CARTESIAN_POINT ( 'NONE',  ( -1.820710678118658388, 24.16915171043284261, -254.1248771717017974 ) ) ;
#140816 = B_SPLINE_CURVE_WITH_KNOTS ( 'NONE', 3,
 ( #13782, #71206, #172904, #213252, #170337, #210695 ),
 .UNSPECIFIED., .F., .F.,
 ( 4, 2, 4 ),
 ( 0.000000000000000000, 0.0001568709654583473091, 0.0003137419309166946182 ),
 .UNSPECIFIED. ) ;
#140818 = ORIENTED_EDGE ( 'NONE', *, *, #160418, .F. ) ;
#140817 = CARTESIAN_POINT ( 'NONE',  ( 20.41140022480505323, 65.58956915761045536, -128.9081061808921334 ) ) ;
#140820 = DIRECTION ( 'NONE',  ( 1.000000000000000000, 0.000000000000000000, -0.000000000000000000 ) ) ;
#140819 = DIRECTION ( 'NONE',  ( -0.000000000000000000, -0.9770955615653316162, -0.2128009952263604232 ) ) ;
#140821 = ORIENTED_EDGE ( 'NONE', *, *, #52932, .F. ) ;
#140823 = ORIENTED_EDGE ( 'NONE', *, *, #161606, .F. ) ;
#140822 = LINE ( 'NONE', #160412, #10833 ) ;
#140824 = AXIS2_PLACEMENT_3D ( 'NONE', #82100, #117407, #61286 ) ;
#140825 = EDGE_LOOP ( 'NONE', ( #117526, #186194, #74839, #159856, #28341 ) ) ;
#140826 = DIRECTION ( 'NONE',  ( 1.000000000000000000, 0.000000000000000000, -2.168404344971008868E-16 ) ) ;
#140827 = CARTESIAN_POINT ( 'NONE',  ( -21.14999999999999858, 11.40444339177023814, -198.6185779617709670 ) ) ;
#140828 = CARTESIAN_POINT ( 'NONE',  ( -18.40000000000000213, 11.75000000001113953, -57.75000000000000000 ) ) ;
#140829 = ORIENTED_EDGE ( 'NONE', *, *, #36194, .F. ) ;
#140830 = CARTESIAN_POINT ( 'NONE',  ( 18.49999999999998934, 62.46583972339646351, -208.9186153945276487 ) ) ;
#140831 = FACE_OUTER_BOUND ( 'NONE', #130015, .T. ) ;
#140832 = DIRECTION ( 'NONE',  ( 1.000000000000000000, 1.394253735153569469E-16, 2.602809386958778209E-16 ) ) ;
#140833 = CARTESIAN_POINT ( 'NONE',  ( -16.91256925476569961, 9.985731158139330432, -154.9676424890052999 ) ) ;
#140834 = CARTESIAN_POINT ( 'NONE',  ( -18.50596464788227635, 46.37740828070796084, -243.0652246697500800 ) ) ;
#140835 = CARTESIAN_POINT ( 'NONE',  ( 20.94999999999999929, 47.95459712139159336, -246.5019368548292675 ) ) ;
#140836 = VECTOR ( 'NONE', #159383, 1000.000000000000000 ) ;
#140837 = ORIENTED_EDGE ( 'NONE', *, *, #39328, .F. ) ;
#140838 = VERTEX_POINT ( 'NONE', #385 ) ;
#140839 = TOROIDAL_SURFACE ( 'NONE', #182550, 0.2000000000000000111, 0.1000000000000000056 ) ;
#140840 = CARTESIAN_POINT ( 'NONE',  ( -20.07928932188135107, 66.77928932189333011, -115.3731074845243683 ) ) ;
#140841 = AXIS2_PLACEMENT_3D ( 'NONE', #66973, #146491, #126951 ) ;
#140842 = B_SPLINE_CURVE_WITH_KNOTS ( 'NONE', 3,
 ( #162444, #157317, #20369, #179437, #82843, #181994, #56864, #58160, #178160, #743, #217236, #2045, #80280, #239399 ),
 .UNSPECIFIED., .F., .F.,
 ( 4, 2, 2, 2, 2, 2, 4 ),
 ( 0.000000000000000000, 0.0003823333598417312821, 0.0005735000397626380687, 0.0006690833797230922751, 0.0007168750497033180230, 0.0007407708846934308970, 0.0007646667196835437710 ),
 .UNSPECIFIED. ) ;
#140843 = EDGE_CURVE ( 'NONE', #247087, #208402, #110462, .T. ) ;
#140844 = ORIENTED_EDGE ( 'NONE', *, *, #186929, .T. ) ;
#140845 = DIRECTION ( 'NONE',  ( 1.000000000000000000, 0.000000000000000000, 0.000000000000000000 ) ) ;
#140846 = VERTEX_POINT ( 'NONE', #218141 ) ;
#140847 = DIRECTION ( 'NONE',  ( -1.000000000000000000, 0.000000000000000000, 0.000000000000000000 ) ) ;
#140848 =( BOUNDED_CURVE ( )  B_SPLINE_CURVE ( 3, ( #215851, #257507, #137598, #18947 ),
 .UNSPECIFIED., .F., .F. ) 
 B_SPLINE_CURVE_WITH_KNOTS ( ( 4, 4 ),
 ( 5.733388419619902088, 5.983100554402347449 ),
 .UNSPECIFIED. ) 
 CURVE ( )  GEOMETRIC_REPRESENTATION_ITEM ( )  RATIONAL_B_SPLINE_CURVE ( ( 1.000000000000000000, 0.9948104011409417691, 0.9948104011409417691, 1.000000000000000000 ) ) 
 REPRESENTATION_ITEM ( '' )  );
#140849 = CARTESIAN_POINT ( 'NONE',  ( -21.65000000000000213, 7.250000000011138646, -42.75000000000000000 ) ) ;
#140850 = CARTESIAN_POINT ( 'NONE',  ( -21.14999999999999858, 11.65000000001115588, -167.5999999999999659 ) ) ;
#140851 = EDGE_CURVE ( 'NONE', #202597, #193142, #35498, .T. ) ;
#140852 = CARTESIAN_POINT ( 'NONE',  ( -21.64999999999999858, 10.04999999999998295, -20.75000000000000000 ) ) ;
#140853 = DIRECTION ( 'NONE',  ( -0.7071067811865487940, 0.7071067811865463515, 0.000000000000000000 ) ) ;
#140854 = ORIENTED_EDGE ( 'NONE', *, *, #153109, .F. ) ;
#140855 = EDGE_CURVE ( 'NONE', #230224, #73853, #139498, .T. ) ;
#140856 = VECTOR ( 'NONE', #83921, 1000.000000000000114 ) ;
#140857 = EDGE_CURVE ( 'NONE', #234336, #239412, #56497, .T. ) ;
#140859 = VECTOR ( 'NONE', #164549, 1000.000000000000000 ) ;
#140858 = CARTESIAN_POINT ( 'NONE',  ( -20.64999999999999858, 1.115623935689868526E-11, -65.10000000000000853 ) ) ;
#140860 = CARTESIAN_POINT ( 'NONE',  ( 21.14999999999999858, 67.21339244341248786, -191.1731074845244223 ) ) ;
#140861 = CARTESIAN_POINT ( 'NONE',  ( 18.59999999999997655, 1.115600667400684642E-11, -175.4000000000000341 ) ) ;
#140862 = VERTEX_POINT ( 'NONE', #137326 ) ;
#140864 = DIRECTION ( 'NONE',  ( 1.186688945009010077E-16, 0.4088369013363280513, -0.9126074666063769270 ) ) ;
#140863 = DIRECTION ( 'NONE',  ( 0.000000000000000000, 0.000000000000000000, 1.000000000000000000 ) ) ;
#140865 = ORIENTED_EDGE ( 'NONE', *, *, #18326, .F. ) ;
#140868 = ORIENTED_EDGE ( 'NONE', *, *, #254971, .T. ) ;
#140867 = CARTESIAN_POINT ( 'NONE',  ( 23.15000000000000213, 87.48912529308779540, -72.62310748452422615 ) ) ;
#140866 = FACE_OUTER_BOUND ( 'NONE', #139354, .T. ) ;
#140869 = ORIENTED_EDGE ( 'NONE', *, *, #252133, .T. ) ;
#140870 = AXIS2_PLACEMENT_3D ( 'NONE', #67205, #103731, #204133 ) ;
#140871 = CARTESIAN_POINT ( 'NONE',  ( 21.05000000000000071, 87.48912529308817909, -133.6231074845242119 ) ) ;
#140872 = DIRECTION ( 'NONE',  ( 1.836970198721029441E-16, -0.4721928772777346239, -0.8814952561688430555 ) ) ;
#140873 = CARTESIAN_POINT ( 'NONE',  ( -23.25000000000000000, 0.000000000000000000, 0.000000000000000000 ) ) ;
#140874 = EDGE_LOOP ( 'NONE', ( #184351, #217840, #208944, #40596 ) ) ;
#140875 = CARTESIAN_POINT ( 'NONE',  ( 19.99999999999999645, 16.72641738073392403, -222.5849938986771974 ) ) ;
#140876 = ADVANCED_FACE ( 'NONE', ( #239016 ), #1669, .F. ) ;
#140877 = FACE_OUTER_BOUND ( 'NONE', #22159, .T. ) ;
#140878 = EDGE_CURVE ( 'NONE', #4740, #72990, #40845, .T. ) ;
#140880 = CARTESIAN_POINT ( 'NONE',  ( -23.25000000000000000, -1.249999999988843369, -141.8004807544151333 ) ) ;
#140879 = DIRECTION ( 'NONE',  ( 0.000000000000000000, 0.9126074666063660468, 0.4088369013363524762 ) ) ;
#140882 = ORIENTED_EDGE ( 'NONE', *, *, #53510, .F. ) ;
#140881 = FACE_OUTER_BOUND ( 'NONE', #64783, .T. ) ;
#140883 = PRODUCT_RELATED_PRODUCT_CATEGORY ( 'part', '', ( #209720 ) ) ;
#140884 = VERTEX_POINT ( 'NONE', #216872 ) ;
#140885 = VECTOR ( 'NONE', #98955, 1000.000000000000000 ) ;
#140886 = AXIS2_PLACEMENT_3D ( 'NONE', #139609, #83479, #180057 ) ;
#140887 = AXIS2_PLACEMENT_3D ( 'NONE', #171919, #148473, #72811 ) ;
#140888 = CARTESIAN_POINT ( 'NONE',  ( -16.92778301347103920, 44.04299733248424076, -235.2845399950809906 ) ) ;
#140889 = VERTEX_POINT ( 'NONE', #199905 ) ;
#140890 = CARTESIAN_POINT ( 'NONE',  ( -21.14999999999999858, 64.25000000001263345, -196.7392418215462726 ) ) ;
#140891 = VERTEX_POINT ( 'NONE', #158232 ) ;
#140892 = ADVANCED_FACE ( 'NONE', ( #22548 ), #196045, .T. ) ;
#140893 = DIRECTION ( 'NONE',  ( 1.000000000000000000, 0.000000000000000000, 0.000000000000000000 ) ) ;
#140895 = EDGE_CURVE ( 'NONE', #176023, #89706, #236439, .T. ) ;
#140894 = DIRECTION ( 'NONE',  ( -2.915501640297153790E-16, 1.000000000000000000, 0.000000000000000000 ) ) ;
#140896 = CARTESIAN_POINT ( 'NONE',  ( 21.00023020733438273, 6.390869245278871347, -33.50000000000000711 ) ) ;
#140897 = ADVANCED_FACE ( 'NONE', ( #19985 ), #100739, .T. ) ;
#140898 = VECTOR ( 'NONE', #81102, 1000.000000000000000 ) ;
#140899 = VERTEX_POINT ( 'NONE', #179074 ) ;
#140900 = CARTESIAN_POINT ( 'NONE',  ( -21.37071067811865532, 64.97802595716100882, -213.3299907329700318 ) ) ;
#140901 = EDGE_CURVE ( 'NONE', #36199, #98560, #85311, .T. ) ;
#140902 = TOROIDAL_SURFACE ( 'NONE', #190815, 11.90000000000000213, 0.1000000000000000056 ) ;
#140903 = AXIS2_PLACEMENT_3D ( 'NONE', #49914, #167327, #111183 ) ;
#140904 = CARTESIAN_POINT ( 'NONE',  ( 18.79999999999999716, 7.800000000000000711, -15.00000000000000000 ) ) ;
#140905 = AXIS2_PLACEMENT_3D ( 'NONE', #235140, #136009, #254658 ) ;
#140906 = ORIENTED_EDGE ( 'NONE', *, *, #115343, .T. ) ;
#140907 = ORIENTED_EDGE ( 'NONE', *, *, #112456, .F. ) ;
#140908 = AXIS2_PLACEMENT_3D ( 'NONE', #130701, #26489, #105983 ) ;
#140909 = ORIENTED_EDGE ( 'NONE', *, *, #94076, .F. ) ;
#140910 = CARTESIAN_POINT ( 'NONE',  ( -18.39999999999999858, -9.399999999988850163, -155.7499999999999716 ) ) ;
#140911 = ORIENTED_EDGE ( 'NONE', *, *, #135742, .F. ) ;
#140913 = VERTEX_POINT ( 'NONE', #215585 ) ;
#140912 = CARTESIAN_POINT ( 'NONE',  ( 13.88638282980484284, 66.54257354752368769, -185.0230656161244553 ) ) ;
#140914 = ORIENTED_EDGE ( 'NONE', *, *, #119837, .T. ) ;
#140915 = CIRCLE ( 'NONE', #240868, 0.09999999999999939493 ) ;
#140919 = EDGE_CURVE ( 'NONE', #65120, #68194, #201165, .T. ) ;
#140918 = ORIENTED_EDGE ( 'NONE', *, *, #57762, .F. ) ;
#140917 = ORIENTED_EDGE ( 'NONE', *, *, #235090, .F. ) ;
#140916 = CARTESIAN_POINT ( 'NONE',  ( -16.77828822508139694, 9.946229374931901290, -113.1626282513739881 ) ) ;
#140921 = VERTEX_POINT ( 'NONE', #235167 ) ;
#140920 = AXIS2_PLACEMENT_3D ( 'NONE', #143364, #26001, #121285 ) ;
#140922 = DIRECTION ( 'NONE',  ( 1.000000000000000000, 0.000000000000000000, 0.000000000000000000 ) ) ;
#140923 = AXIS2_PLACEMENT_3D ( 'NONE', #137089, #190675, #12031 ) ;
#140924 = CARTESIAN_POINT ( 'NONE',  ( -20.94999999999999929, -10.86374996222471090, -206.3339888224507206 ) ) ;
#140925 = AXIS2_PLACEMENT_3D ( 'NONE', #132000, #210268, #231125 ) ;
#140926 = CYLINDRICAL_SURFACE ( 'NONE', #113299, 12.87500000000000178 ) ;
#140927 = AXIS2_PLACEMENT_3D ( 'NONE', #73549, #110069, #249598 ) ;
#140928 = CIRCLE ( 'NONE', #144999, 0.09999999999999939493 ) ;
#140929 = VERTEX_POINT ( 'NONE', #102044 ) ;
#140930 = CIRCLE ( 'NONE', #45234, 7.900000000000003908 ) ;
#140931 = EDGE_CURVE ( 'NONE', #126259, #178504, #38256, .T. ) ;
#140932 = CARTESIAN_POINT ( 'NONE',  ( 23.15000000000000213, 85.00000000001159606, -59.62913836187181715 ) ) ;
#140934 = ORIENTED_EDGE ( 'NONE', *, *, #1141, .F. ) ;
#140933 = CARTESIAN_POINT ( 'NONE',  ( 18.59999999999999076, 10.20857864377385127, -88.25000000000005684 ) ) ;
#140935 = FACE_OUTER_BOUND ( 'NONE', #148923, .T. ) ;
#140937 = VERTEX_POINT ( 'NONE', #96892 ) ;
#140936 = DIRECTION ( 'NONE',  ( 0.000000000000000000, -0.4088369013363281068, 0.9126074666063769270 ) ) ;
#140938 = VECTOR ( 'NONE', #101937, 1000.000000000000000 ) ;
#140939 = ORIENTED_EDGE ( 'NONE', *, *, #88801, .T. ) ;
#140940 = EDGE_CURVE ( 'NONE', #152727, #154309, #36992, .T. ) ;
#140941 = CARTESIAN_POINT ( 'NONE',  ( 21.30000000000002558, 1.115600667400684642E-11, -33.50000000000000000 ) ) ;
#140942 = LINE ( 'NONE', #215326, #28545 ) ;
#140943 = B_SPLINE_CURVE_WITH_KNOTS ( 'NONE', 3,
 ( #234170, #196333, #256237, #60660, #120682, #217166, #99777, #36000, #197612, #140193, #118088, #158523, #41145, #219744, #55505, #17687, #95940, #135058, #97190 ),
 .UNSPECIFIED., .F., .F.,
 ( 4, 3, 3, 3, 3, 3, 4 ),
 ( -2.000416914671369846E-06, 0.000000000000000000, 4.714008503745774695E-05, 9.979203887777935550E-05, 0.0001372215519229537709, 0.0001635031576221019581, 0.0001900083748504146253 ),
 .UNSPECIFIED. ) ;
#140944 = VERTEX_POINT ( 'NONE', #17401 ) ;
#140945 = ORIENTED_EDGE ( 'NONE', *, *, #98241, .T. ) ;
#140946 = B_SPLINE_CURVE_WITH_KNOTS ( 'NONE', 3,
 ( #159453, #158208, #56471, #96863, #237706, #139864 ),
 .UNSPECIFIED., .F., .F.,
 ( 4, 2, 4 ),
 ( 0.000000000000000000, 0.0001568709654583420778, 0.0003137419309166841557 ),
 .UNSPECIFIED. ) ;
#140947 = CARTESIAN_POINT ( 'NONE',  ( -16.96982749440708460, 9.950000000011137047, -180.6247784088108688 ) ) ;
#140948 = CARTESIAN_POINT ( 'NONE',  ( -21.05000000000000071, 0.01485563490490060361, -161.1556409579560523 ) ) ;
#140949 = MECHANICAL_DESIGN_GEOMETRIC_PRESENTATION_REPRESENTATION (  '', ( #253361 ), #91052 ) ;
#140950 = AXIS2_PLACEMENT_3D ( 'NONE', #52217, #49666, #7986 ) ;
#140951 = ADVANCED_FACE ( 'NONE', ( #176490 ), #93724, .T. ) ;
#140953 = ORIENTED_EDGE ( 'NONE', *, *, #40244, .T. ) ;
#140952 = ORIENTED_EDGE ( 'NONE', *, *, #158030, .F. ) ;
#140955 = VERTEX_POINT ( 'NONE', #48511 ) ;
#140954 = CLOSED_SHELL ( 'NONE', ( #125449, #195887, #224364, #179453, #217914, #3780, #82190, #214282, #147364, #164489, #55296, #80285, #192190, #11386, #109116, #112112, #55731, #34189, #129992, #172528, #158152, #2127, #57027, #130995, #23904, #26664, #205120, #23977, #203352, #216162, #44886, #66738, #92013, #246714, #213720, #15336, #14733, #108235, #216665, #33651, #2916, #43220, #46735, #159439, #59904, #255043, #84469, #80099, #131466, #115019, #21465, #167643, #64455, #198271, #216557, #13238, #135054, #203696, #210196, #130910, #146478, #48798, #105598, #173593, #241793, #92357, #96757, #86240, #173142, #88140, #140188, #110890, #78041, #220797, #157730, #26179, #65802, #127856, #55418, #251874, #77847, #252541, #80793, #129300, #15269, #71675, #182297, #84076, #250274, #226979, #74123, #109282, #485, #103519, #4215, #209993, #28841, #162540, #23910, #32361, #238068, #2601, #207828, #88212, #108216, #242232, #25850, #212695, #93656, #191602, #67016, #103295, #111767, #213608, #254236, #5204, #182743, #6677, #135380, #247742, #44997, #85571, #6816, #209083, #139180, #19696, #153637, #132381, #29627, #67541, #235192, #111173, #5039, #67667, #115700, #925, #187834, #125006, #95258, #238748, #134966, #257198, #124873, #6591, #116103, #88680, #109922, #17638, #77262, #12356, #69187, #218282, #195782, #36242, #206253, #220446, #169822, #18014, #52807, #100090, #210479, #102557, #233188, #55222, #219080, #245715, #6272, #128808, #177238, #75997, #44277, #75965, #219391, #143011, #86079, #39132, #221676, #89710, #168552, #138722, #54481, #103623, #13030, #184987, #146808, #9652, #146259, #4864, #232180, #8789, #51490, #61463, #55492, #135185, #618, #214780, #191950, #28173, #96165, #12677, #131056, #5203, #117181, #189214, #159718, #110823, #109162, #243922, #126361, #27337, #105620, #19345, #171879, #158191, #44427, #235770, #146479, #100872, #151215, #226386, #216484, #150525, #113378, #175097, #143702, #235647, #214855, #144146, #182397, #99930, #147426, #106537, #59966, #75881, #41287, #8613, #210840, #107563, #17546, #103742, #109518, #81140, #161281, #53232, #46649, #10974, #208317, #32904, #35382, #4957, #15457, #76145, #51380, #14161, #58103, #56211, #110368, #101286, #219732, #135211, #186476, #128944, #33121, #115332, #69793, #247384, #47361, #122455, #107615, #231095, #29535, #96789, #54451, #252012, #237488, #153316, #120176, #255351, #79973, #118156, #54335, #221164, #125267, #103272, #198837, #137984, #204793, #54303, #157202, #246871, #60915, #133743, #55600, #198194, #79327, #167738, #119367, #76120, #19130, #127140, #34031, #161903, #226025, #67273, #58470, #119890, #188843, #178520, #221389, #77704, #106751, #216356, #106447, #40655, #211784, #137722, #106050, #139744, #204738, #85847, #176520, #44785, #14813, #67893, #116500, #173103, #216789, #55816, #91730, #148586, #165483, #23873, #173719, #61358, #160116, #126966, #94113, #224567, #41861, #150467, #242719, #43411, #213621, #133822, #153230, #249595, #200831, #35712, #17095, #92139, #240367, #160884, #171505, #74410, #27622, #210003, #146026, #129252, #84677, #197331, #49113, #239892, #72739, #187373, #139580, #225041, #231518, #3788, #130318, #209848, #91959, #82894, #213970, #65325, #104269, #145327, #235975, #60555, #28420, #44874, #222208, #29186, #54596, #209868, #159490, #133305, #221236, #228454, #73071, #154794, #225050, #96983, #164941, #161836, #16978, #94612, #51708, #40929, #9690, #178437, #55162, #253686, #72328, #219083, #52870, #178316, #66323, #132853, #18519, #110419, #52080, #246129, #218036, #197030, #228631, #89551, #229350, #170417, #180378, #221228, #33957, #93883, #171078, #79442, #15784, #127103, #197111, #37317, #230179, #131994, #42624, #60363, #156580, #174902, #148574, #127034, #138300, #169436, #208006, #119857, #97612, #91416, #206640, #20868, #100412, #188012, #214280, #207494, #131868, #16567, #248637, #236217, #106657, #3904, #149966, #256254, #107520, #225129, #32626, #235346, #67354, #174270, #8176, #29663, #131525, #181555, #90129, #248136, #153018, #215638, #8466, #181920, #13427, #56369, #254616, #196596, #94263, #237900 ) ) ;
#140957 = ADVANCED_FACE ( 'NONE', ( #126767 ), #202460, .T. ) ;
#140956 = CARTESIAN_POINT ( 'NONE',  ( 21.05000000000000071, 68.48451787451661232, -224.2224406095231757 ) ) ;
#140958 = VERTEX_POINT ( 'NONE', #185464 ) ;
#140959 = ORIENTED_EDGE ( 'NONE', *, *, #39267, .F. ) ;
#140960 = DIRECTION ( 'NONE',  ( 1.301042606982683418E-14, -0.9525900758537759749, 0.3042567129660372904 ) ) ;
#140961 = VERTEX_POINT ( 'NONE', #184164 ) ;
#140962 = DIRECTION ( 'NONE',  ( 0.000000000000000000, -0.9595780032479205301, 0.2814428106787130734 ) ) ;
#140964 = CARTESIAN_POINT ( 'NONE',  ( 18.59999994388910238, -9.363566187059737089, -107.6811172368012848 ) ) ;
#140963 = CYLINDRICAL_SURFACE ( 'NONE', #7258, 0.09999999999998898659 ) ;
#140965 = ORIENTED_EDGE ( 'NONE', *, *, #97142, .F. ) ;
#140966 = CIRCLE ( 'NONE', #174315, 7.900000000000003908 ) ;
#140967 = CIRCLE ( 'NONE', #203315, 0.3999999999999926392 ) ;
#140969 = VERTEX_POINT ( 'NONE', #65502 ) ;
#140968 = ORIENTED_EDGE ( 'NONE', *, *, #157557, .F. ) ;
#140970 = DIRECTION ( 'NONE',  ( 1.000000000000000000, 0.000000000000000000, 0.000000000000000000 ) ) ;
#140971 = CARTESIAN_POINT ( 'NONE',  ( 23.14999999999999503, 11.65000000001116298, -155.7499999999999716 ) ) ;
#140972 = VECTOR ( 'NONE', #15730, 1000.000000000000000 ) ;
#140973 = ORIENTED_EDGE ( 'NONE', *, *, #12265, .F. ) ;
#140974 = ADVANCED_FACE ( 'NONE', ( #206313 ), #86324, .F. ) ;
#140975 = AXIS2_PLACEMENT_3D ( 'NONE', #206729, #243273, #103748 ) ;
#140976 = CARTESIAN_POINT ( 'NONE',  ( -22.59999999999999787, 1.115600667400684642E-11, -167.4999999999999716 ) ) ;
#140977 = ORIENTED_EDGE ( 'NONE', *, *, #8150, .F. ) ;
#140978 = ORIENTED_EDGE ( 'NONE', *, *, #240803, .F. ) ;
#140979 = EDGE_CURVE ( 'NONE', #5593, #44687, #27711, .T. ) ;
#140980 = VERTEX_POINT ( 'NONE', #242861 ) ;
#140981 = CARTESIAN_POINT ( 'NONE',  ( 22.39999999999999503, 59.71212129423884818, -233.8158665866020272 ) ) ;
#140982 = DIRECTION ( 'NONE',  ( 0.000000000000000000, -0.2128009952263602012, 0.9770955615653315052 ) ) ;
#140983 = ORIENTED_EDGE ( 'NONE', *, *, #40228, .F. ) ;
#140984 = AXIS2_PLACEMENT_3D ( 'NONE', #227509, #122857, #163270 ) ;
#140985 = CYLINDRICAL_SURFACE ( 'NONE', #2340, 0.09999999999999892308 ) ;
#140986 = FACE_OUTER_BOUND ( 'NONE', #153532, .T. ) ;
#140988 = CARTESIAN_POINT ( 'NONE',  ( 18.49999999999999645, 1.162701749949165642, -108.6000000000000227 ) ) ;
#140987 = CYLINDRICAL_SURFACE ( 'NONE', #194585, 0.1000000000000028644 ) ;
#140989 = DIRECTION ( 'NONE',  ( 0.000000000000000000, 0.4088369013363280513, -0.9126074666063769270 ) ) ;
#140991 = CIRCLE ( 'NONE', #149368, 0.2000000000000057288 ) ;
#140990 = DIRECTION ( 'NONE',  ( 0.000000000000000000, -0.4088369013363296611, 0.9126074666063762608 ) ) ;
#140993 = ADVANCED_FACE ( 'NONE', ( #143753 ), #227147, .T. ) ;
#140992 = DIRECTION ( 'NONE',  ( 0.000000000000000000, -0.4088369013363281623, 0.9126074666063771490 ) ) ;
#140994 = LINE ( 'NONE', #160568, #36915 ) ;
#140995 = AXIS2_PLACEMENT_3D ( 'NONE', #217667, #216405, #36525 ) ;
#140996 = EDGE_CURVE ( 'NONE', #167341, #214263, #185305, .T. ) ;
#140998 = ORIENTED_EDGE ( 'NONE', *, *, #38261, .T. ) ;
#140997 = AXIS2_PLACEMENT_3D ( 'NONE', #167588, #123308, #185837 ) ;
#141000 = EDGE_LOOP ( 'NONE', ( #61063, #171823, #32275, #232637 ) ) ;
#140999 = ORIENTED_EDGE ( 'NONE', *, *, #8237, .F. ) ;
#141001 = ORIENTED_EDGE ( 'NONE', *, *, #110454, .F. ) ;
#141002 = ORIENTED_EDGE ( 'NONE', *, *, #193789, .F. ) ;
#141003 = DIRECTION ( 'NONE',  ( 0.000000000000000000, 0.9887567792719341719, -0.1495327102803664099 ) ) ;
#141004 = FACE_OUTER_BOUND ( 'NONE', #249756, .T. ) ;
#141005 = EDGE_CURVE ( 'NONE', #56652, #232238, #163339, .T. ) ;
#141007 = DIRECTION ( 'NONE',  ( -2.952720810173289605E-16, -1.000000000000000000, -7.086529944415894657E-15 ) ) ;
#141006 = FACE_OUTER_BOUND ( 'NONE', #129476, .T. ) ;
#141008 = EDGE_CURVE ( 'NONE', #135166, #147029, #160390, .T. ) ;
#141009 = CARTESIAN_POINT ( 'NONE',  ( -18.40000000000000213, 11.74999999999998224, -24.25000000000000000 ) ) ;
#141010 = ORIENTED_EDGE ( 'NONE', *, *, #238713, .T. ) ;
#141011 = AXIS2_PLACEMENT_3D ( 'NONE', #171962, #131506, #32448 ) ;
#141012 = DIRECTION ( 'NONE',  ( 0.000000000000000000, 0.000000000000000000, -1.000000000000000000 ) ) ;
#141013 = CARTESIAN_POINT ( 'NONE',  ( 21.05000000000000071, 67.23127455305841238, -235.8551265064783991 ) ) ;
#141014 = DIRECTION ( 'NONE',  ( -0.000000000000000000, -0.9667078373770160438, -0.2558827019433959071 ) ) ;
#141015 = CARTESIAN_POINT ( 'NONE',  ( -20.64999999999999858, 6.353932154659650777, -220.7762181625030848 ) ) ;
#141016 = ORIENTED_EDGE ( 'NONE', *, *, #211342, .T. ) ;
#141017 = CARTESIAN_POINT ( 'NONE',  ( -21.05000000000000071, 64.35000000001268461, -203.4231074845244507 ) ) ;
#141018 = FACE_OUTER_BOUND ( 'NONE', #188379, .T. ) ;
#141019 = VERTEX_POINT ( 'NONE', #225835 ) ;
#141020 = SPHERICAL_SURFACE ( 'NONE', #87221, 0.1000000000000000056 ) ;
#141021 = DIRECTION ( 'NONE',  ( 0.000000000000000000, 6.982962677686266711E-15, -1.000000000000000000 ) ) ;
#141022 = DIRECTION ( 'NONE',  ( 1.000000000000000000, 0.000000000000000000, 0.000000000000000000 ) ) ;
#141023 = DIRECTION ( 'NONE',  ( 1.000000000000000000, 0.000000000000000000, 0.000000000000000000 ) ) ;
#141024 = ORIENTED_EDGE ( 'NONE', *, *, #135998, .T. ) ;
#141025 = DIRECTION ( 'NONE',  ( 1.000000000000000000, 0.000000000000000000, 0.000000000000000000 ) ) ;
#141026 = FACE_OUTER_BOUND ( 'NONE', #244764, .T. ) ;
#141027 = DIRECTION ( 'NONE',  ( -0.7071067811865456854, -0.7071067811865493491, -4.937700262164544098E-15 ) ) ;
#141029 = LINE ( 'NONE', #204826, #145353 ) ;
#141028 = CARTESIAN_POINT ( 'NONE',  ( -20.64999999999999858, 1.148907358139439339E-11, -201.0000000000015064 ) ) ;
#141030 = DIRECTION ( 'NONE',  ( 0.000000000000000000, 0.9126074666063844765, 0.4088369013363114535 ) ) ;
#141031 = CARTESIAN_POINT ( 'NONE',  ( 20.73486653747088582, 68.75000000001259082, -194.2731074845244166 ) ) ;
#141032 = CIRCLE ( 'NONE', #111988, 0.1000000000000028644 ) ;
#141033 = CIRCLE ( 'NONE', #53530, 12.87500000000000178 ) ;
#141034 = DIRECTION ( 'NONE',  ( 1.186688945009009831E-16, -1.000000000000000000, 0.000000000000000000 ) ) ;
#141035 = DIRECTION ( 'NONE',  ( 0.000000000000000000, 1.000000000000000000, 0.000000000000000000 ) ) ;
#141037 = ORIENTED_EDGE ( 'NONE', *, *, #230586, .F. ) ;
#141036 = CARTESIAN_POINT ( 'NONE',  ( 21.05000000000000071, 1.115600667400684642E-11, -134.1000000000000227 ) ) ;
#141038 = EDGE_CURVE ( 'NONE', #250639, #216812, #181229, .T. ) ;
#141039 = VERTEX_POINT ( 'NONE', #165924 ) ;
#141040 = AXIS2_PLACEMENT_3D ( 'NONE', #150349, #231184, #49943 ) ;
#141041 = FACE_OUTER_BOUND ( 'NONE', #26863, .T. ) ;
#141042 = DIRECTION ( 'NONE',  ( 1.000000000000000000, 0.000000000000000000, 0.000000000000000000 ) ) ;
#141043 = AXIS2_PLACEMENT_3D ( 'NONE', #137363, #216903, #257271 ) ;
#141045 = AXIS2_PLACEMENT_3D ( 'NONE', #49418, #5117, #9006 ) ;
#141044 = CARTESIAN_POINT ( 'NONE',  ( -20.64999999999999858, 76.00000000001149658, -48.89810748452431710 ) ) ;
#141046 = EDGE_CURVE ( 'NONE', #112394, #14611, #35944, .T. ) ;
#141047 = DIRECTION ( 'NONE',  ( -0.000000000000000000, -0.000000000000000000, 1.000000000000000000 ) ) ;
#141048 = ORIENTED_EDGE ( 'NONE', *, *, #180396, .T. ) ;
#141049 = AXIS2_PLACEMENT_3D ( 'NONE', #228854, #252247, #48916 ) ;
#141050 = DIRECTION ( 'NONE',  ( 0.000000000000000000, -6.982962677686266711E-15, 1.000000000000000000 ) ) ;
#141051 = FACE_OUTER_BOUND ( 'NONE', #240638, .T. ) ;
#141052 = CARTESIAN_POINT ( 'NONE',  ( -18.54148534481894472, 65.67467670974414773, -97.45317318268841689 ) ) ;
#141053 = CARTESIAN_POINT ( 'NONE',  ( -21.05000000000000071, 61.95000000001210338, -131.0094124137634140 ) ) ;
#141055 = EDGE_LOOP ( 'NONE', ( #117183, #28588, #138547, #53318 ) ) ;
#141054 = FACE_OUTER_BOUND ( 'NONE', #73964, .T. ) ;
#141057 = CARTESIAN_POINT ( 'NONE',  ( -18.59999999999999787, 13.96869538424787649, -210.3925794786331949 ) ) ;
#141056 = CARTESIAN_POINT ( 'NONE',  ( -23.25000000000000000, 2.000000000011154189, -120.7753780772379315 ) ) ;
#141058 = DIRECTION ( 'NONE',  ( 0.000000000000000000, -0.9126074666063771490, -0.4088369013363281623 ) ) ;
#141059 = FACE_OUTER_BOUND ( 'NONE', #157591, .T. ) ;
#141060 = ORIENTED_EDGE ( 'NONE', *, *, #233172, .F. ) ;
#141061 = CARTESIAN_POINT ( 'NONE',  ( 0.000000000000000000, 0.000000000000000000, 0.000000000000000000 ) ) ;
#141062 = CARTESIAN_POINT ( 'NONE',  ( 23.25000000000000000, 85.60000000001208775, -126.6291383618717816 ) ) ;
#141063 = FACE_OUTER_BOUND ( 'NONE', #107339, .T. ) ;
#141064 = ORIENTED_EDGE ( 'NONE', *, *, #208045, .F. ) ;
#141065 = CARTESIAN_POINT ( 'NONE',  ( -23.25000000000000000, 70.05000000001149374, -46.32880978955918039 ) ) ;
#141066 = AXIS2_PLACEMENT_3D ( 'NONE', #21719, #24300, #244597 ) ;
#141067 = CARTESIAN_POINT ( 'NONE',  ( 23.24999999999999645, 4.775700934590591196, -55.15123189595403375 ) ) ;
#141068 = ORIENTED_EDGE ( 'NONE', *, *, #181323, .F. ) ;
#141069 = CIRCLE ( 'NONE', #49484, 0.1000000000000106914 ) ;
#141070 = CARTESIAN_POINT ( 'NONE',  ( 18.56308993302884147, 54.99211411440564490, -229.9633593191885836 ) ) ;
#141071 = CARTESIAN_POINT ( 'NONE',  ( 20.94999999999999574, 18.27667581256378071, -237.6066273148655057 ) ) ;
#141072 = CARTESIAN_POINT ( 'NONE',  ( -22.46246831459151494, 0.02191216695058596786, -122.3501354387900619 ) ) ;
#141073 = ORIENTED_EDGE ( 'NONE', *, *, #185465, .F. ) ;
#141074 = VECTOR ( 'NONE', #192609, 1000.000000000000000 ) ;
#141075 = ORIENTED_EDGE ( 'NONE', *, *, #140, .T. ) ;
#141076 = LINE ( 'NONE', #142342, #23871 ) ;
#141077 = DIRECTION ( 'NONE',  ( -1.000000000000000000, 0.000000000000000000, 0.000000000000000000 ) ) ;
#141078 = CARTESIAN_POINT ( 'NONE',  ( 21.05000000000000071, 10.62950747927168216, -141.6279793999966898 ) ) ;
#141079 = LINE ( 'NONE', #41994, #207566 ) ;
#141080 = EDGE_CURVE ( 'NONE', #31271, #160183, #160180, .T. ) ;
#141082 = LINE ( 'NONE', #235050, #191011 ) ;
#141081 = CARTESIAN_POINT ( 'NONE',  ( -16.83199030136657370, 12.42117176568584824, -211.3666045650834633 ) ) ;
#141083 = AXIS2_PLACEMENT_3D ( 'NONE', #225527, #152134, #125184 ) ;
#141085 = DIRECTION ( 'NONE',  ( -1.000000000000000000, 0.000000000000000000, 0.000000000000000000 ) ) ;
#141084 = AXIS2_PLACEMENT_3D ( 'NONE', #7282, #177307, #166402 ) ;
#141086 = CARTESIAN_POINT ( 'NONE',  ( 21.14999999999999858, 64.25000000001193712, -102.9231074845243938 ) ) ;
#141087 = LINE ( 'NONE', #182792, #180626 ) ;
#141088 = CIRCLE ( 'NONE', #207741, 4.099999999999999645 ) ;
#141089 = EDGE_LOOP ( 'NONE', ( #13956, #81551, #174911, #230160 ) ) ;
#141090 = DIRECTION ( 'NONE',  ( 1.000000000000000000, 0.000000000000000000, 0.000000000000000000 ) ) ;
#141092 = ORIENTED_EDGE ( 'NONE', *, *, #160351, .F. ) ;
#141091 = CARTESIAN_POINT ( 'NONE',  ( 18.69999999999999929, -11.74999999999999289, 30.09999999999999787 ) ) ;
#141093 = CYLINDRICAL_SURFACE ( 'NONE', #235220, 0.1000000000000028644 ) ;
#141094 = VECTOR ( 'NONE', #131475, 1000.000000000000114 ) ;
#141095 = SPHERICAL_SURFACE ( 'NONE', #11815, 0.1000000000000000056 ) ;
#141097 = CARTESIAN_POINT ( 'NONE',  ( 21.00000000000000000, 66.25000000001253397, -182.2731074845244450 ) ) ;
#141096 = CARTESIAN_POINT ( 'NONE',  ( 22.00356870070003978, 76.00000000000741807, -110.2773498462693595 ) ) ;
#141098 = ADVANCED_FACE ( 'NONE', ( #169790 ), #249302, .T. ) ;
#141099 = ORIENTED_EDGE ( 'NONE', *, *, #71085, .T. ) ;
#141101 = CARTESIAN_POINT ( 'NONE',  ( -16.98495255085919098, 22.99074469765236728, -230.8788200404308952 ) ) ;
#141100 = CARTESIAN_POINT ( 'NONE',  ( -16.79270642812310399, 66.05375578307352669, -56.86204076308684563 ) ) ;
#141102 = DIRECTION ( 'NONE',  ( -1.000000000000000000, 2.952720810173289112E-16, 2.061873921506763405E-30 ) ) ;
#141103 = DIRECTION ( 'NONE',  ( 0.000000000000000000, 0.2617529984165033463, 0.9651348961777157509 ) ) ;
#141104 = DIRECTION ( 'NONE',  ( -7.304098846217948299E-16, -1.000000000000000000, 0.000000000000000000 ) ) ;
#141105 = EDGE_CURVE ( 'NONE', #74036, #34485, #194475, .T. ) ;
#141106 = ORIENTED_EDGE ( 'NONE', *, *, #29027, .F. ) ;
#141107 = CARTESIAN_POINT ( 'NONE',  ( -23.24999999999999645, -9.599999999988845900, -107.2001893912220964 ) ) ;
#141108 = VECTOR ( 'NONE', #20095, 1000.000000000000000 ) ;
#141109 = AXIS2_PLACEMENT_3D ( 'NONE', #94900, #72814, #134028 ) ;
#141110 = EDGE_LOOP ( 'NONE', ( #136264, #64258, #95922, #156631 ) ) ;
#141111 = CARTESIAN_POINT ( 'NONE',  ( 20.84999999999998721, -11.74999999998884448, -100.5000000000000426 ) ) ;
#141113 = EDGE_CURVE ( 'NONE', #15934, #56184, #151497, .T. ) ;
#141112 = VECTOR ( 'NONE', #111964, 1000.000000000000000 ) ;
#141114 = ORIENTED_EDGE ( 'NONE', *, *, #26092, .T. ) ;
#141115 = DIRECTION ( 'NONE',  ( 0.000000000000000000, -0.8814952561688476074, 0.4721928772777262417 ) ) ;
#141116 = ORIENTED_EDGE ( 'NONE', *, *, #48847, .T. ) ;
#141117 = TOROIDAL_SURFACE ( 'NONE', #236963, 0.2000000000000000111, 0.1000000000000000056 ) ;
#141118 = CARTESIAN_POINT ( 'NONE',  ( -20.94999999999999929, 64.40000000001147384, -42.95131071479990936 ) ) ;
#141119 = AXIS2_PLACEMENT_3D ( 'NONE', #59923, #37844, #139470 ) ;
#141120 = VECTOR ( 'NONE', #255428, 1000.000000000000000 ) ;
#141121 = TOROIDAL_SURFACE ( 'NONE', #41170, 11.65000000000000036, 0.1000000000000000056 ) ;
#141122 = DIRECTION ( 'NONE',  ( 1.040834085586049673E-13, 0.7899159663865300551, 0.6132151058540831201 ) ) ;
#141123 = ORIENTED_EDGE ( 'NONE', *, *, #85711, .T. ) ;
#141124 = CIRCLE ( 'NONE', #62003, 0.09999999999999939493 ) ;
#141125 = ADVANCED_FACE ( 'NONE', ( #129334 ), #253122, .F. ) ;
#141126 = CARTESIAN_POINT ( 'NONE',  ( -0.8999999999999425127, 67.72071067812984779, -13.99381816264344813 ) ) ;
#141127 = CARTESIAN_POINT ( 'NONE',  ( -21.14999999999999858, 0.000000000000000000, 11.64957080754479968 ) ) ;
#141128 = CARTESIAN_POINT ( 'NONE',  ( 20.94999999999999929, 11.75000000001115552, -160.7161343370219413 ) ) ;
#141129 = CARTESIAN_POINT ( 'NONE',  ( -16.81744102076749314, 44.13548170601895038, -235.2989316066074821 ) ) ;
#141130 = DIRECTION ( 'NONE',  ( 0.000000000000000000, -0.9126074666063769270, -0.4088369013363280513 ) ) ;
#141131 = CARTESIAN_POINT ( 'NONE',  ( 19.97071067695804203, 62.37829099644529407, -208.9712820482884581 ) ) ;
#141132 = VERTEX_POINT ( 'NONE', #34129 ) ;
#141133 = DIRECTION ( 'NONE',  ( -1.000000000000000000, -0.000000000000000000, -0.000000000000000000 ) ) ;
#141134 = VECTOR ( 'NONE', #222850, 1000.000000000000000 ) ;
#141135 = VERTEX_POINT ( 'NONE', #88908 ) ;
#141137 = EDGE_LOOP ( 'NONE', ( #160212, #5916, #179513, #47995 ) ) ;
#141136 = CARTESIAN_POINT ( 'NONE',  ( -21.05000000000000071, 76.00000000001244871, -170.0231074845243597 ) ) ;
#141138 = ORIENTED_EDGE ( 'NONE', *, *, #44073, .T. ) ;
#141139 = CARTESIAN_POINT ( 'NONE',  ( 20.94999999999999929, -11.48912529306489994, -64.00000000000000000 ) ) ;
#141140 = CIRCLE ( 'NONE', #245181, 0.09999999999999939493 ) ;
#141141 = CARTESIAN_POINT ( 'NONE',  ( 14.87567385445977308, 66.56923500459026855, -188.2925700897740455 ) ) ;
#141142 = CARTESIAN_POINT ( 'NONE',  ( 20.95512820512820440, 60.15812638745688901, -221.3479132702343009 ) ) ;
#141143 = CARTESIAN_POINT ( 'NONE',  ( -23.25000000000000000, 74.08971962618002749, -82.15447533972326255 ) ) ;
#141144 = ORIENTED_EDGE ( 'NONE', *, *, #168463, .T. ) ;
#141145 = DIRECTION ( 'NONE',  ( 0.000000000000000000, -6.853228547068871147E-15, 1.000000000000000000 ) ) ;
#141146 = LINE ( 'NONE', #65443, #27259 ) ;
#141147 = B_SPLINE_CURVE_WITH_KNOTS ( 'NONE', 3,
 ( #44752, #203810, #459, #99545, #139963, #179149, #124291, #159562, #25200, #78709 ),
 .UNSPECIFIED., .F., .F.,
 ( 4, 3, 3, 4 ),
 ( -2.000561356218653466E-06, 0.000000000000000000, 1.787822682428266431E-05, 4.206475347089715442E-05 ),
 .UNSPECIFIED. ) ;
#141148 = CIRCLE ( 'NONE', #195325, 0.1000000000000028644 ) ;
#141149 = VERTEX_POINT ( 'NONE', #231030 ) ;
#141150 = AXIS2_PLACEMENT_3D ( 'NONE', #69064, #148591, #237103 ) ;
#141151 = CARTESIAN_POINT ( 'NONE',  ( -20.91682497891422798, 10.32263460346243633, -39.06059579686719019 ) ) ;
#141152 = VECTOR ( 'NONE', #72827, 1000.000000000000000 ) ;
#141153 = DIRECTION ( 'NONE',  ( 0.000000000000000000, -0.2128009952263609783, 0.9770955615653315052 ) ) ;
#141154 = ORIENTED_EDGE ( 'NONE', *, *, #182802, .T. ) ;
#141155 = CARTESIAN_POINT ( 'NONE',  ( -18.59999999999999787, -1.736257131586239844, -45.06865232901750318 ) ) ;
#141156 = AXIS2_PLACEMENT_3D ( 'NONE', #87746, #206425, #167329 ) ;
#141157 = EDGE_CURVE ( 'NONE', #10689, #180521, #164465, .T. ) ;
#141158 = CARTESIAN_POINT ( 'NONE',  ( 20.85000000000000142, 64.25000000001195133, -109.8069731475024753 ) ) ;
#141159 = ORIENTED_EDGE ( 'NONE', *, *, #69423, .F. ) ;
#141160 = CARTESIAN_POINT ( 'NONE',  ( -20.54999999999999716, 2.000000000011154189, -154.6753780772379514 ) ) ;
#141161 = CARTESIAN_POINT ( 'NONE',  ( -21.98333005346336932, 1.115600667400684642E-11, -126.6259246709433626 ) ) ;
#141162 = DIRECTION ( 'NONE',  ( 1.000000000000000000, 2.952720810173289112E-16, -0.000000000000000000 ) ) ;
#141163 = EDGE_CURVE ( 'NONE', #185216, #40045, #251188, .T. ) ;
#141164 = CARTESIAN_POINT ( 'NONE',  ( -23.25000000000000000, 76.00000000001126921, -203.5231074845248997 ) ) ;
#141165 = AXIS2_PLACEMENT_3D ( 'NONE', #37821, #213864, #114765 ) ;
#141166 = CIRCLE ( 'NONE', #78604, 11.70000000000000639 ) ;
#141167 = CIRCLE ( 'NONE', #162027, 0.1000000000000028644 ) ;
#141168 = ADVANCED_FACE ( 'NONE', ( #90188 ), #52347, .T. ) ;
#141169 = ORIENTED_EDGE ( 'NONE', *, *, #129234, .T. ) ;
#141170 = FILL_AREA_STYLE ('',( #199875 ) ) ;
#141171 = ORIENTED_EDGE ( 'NONE', *, *, #117429, .T. ) ;
#141172 = DIRECTION ( 'NONE',  ( -1.000000000000000000, -0.000000000000000000, -0.000000000000000000 ) ) ;
#141173 = DIRECTION ( 'NONE',  ( -1.000000000000000000, 0.000000000000000000, -0.000000000000000000 ) ) ;
#141176 = ADVANCED_FACE ( 'NONE', ( #112359 ), #250560, .T. ) ;
#141175 = VERTEX_POINT ( 'NONE', #171081 ) ;
#141174 = DIRECTION ( 'NONE',  ( -1.000000000000000000, 0.000000000000000000, 0.000000000000000000 ) ) ;
#141177 = DIRECTION ( 'NONE',  ( 0.000000000000000000, -0.8814952561688429444, 0.4721928772777349570 ) ) ;
#141178 = DIRECTION ( 'NONE',  ( 1.000000000000000000, 0.000000000000000000, 0.000000000000000000 ) ) ;
#141179 = DIRECTION ( 'NONE',  ( 0.000000000000000000, 0.000000000000000000, 1.000000000000000000 ) ) ;
#141180 = CARTESIAN_POINT ( 'NONE',  ( 23.14999999999999147, 71.85000000001194564, -103.0231074845243455 ) ) ;
#141181 = EDGE_CURVE ( 'NONE', #61384, #168421, #210446, .T. ) ;
#141182 = CARTESIAN_POINT ( 'NONE',  ( -5.899999999999938183, 64.75000000001119815, -22.02310748452479316 ) ) ;
#141183 = EDGE_CURVE ( 'NONE', #73952, #126560, #77149, .T. ) ;
#141184 = CARTESIAN_POINT ( 'NONE',  ( -18.46093223321778609, 85.48068296828660095, -129.4385569705975456 ) ) ;
#141186 = VERTEX_POINT ( 'NONE', #150202 ) ;
#141185 = CARTESIAN_POINT ( 'NONE',  ( 20.97462148592287079, 67.12526242356170769, -157.7684631527933732 ) ) ;
#141188 = EDGE_CURVE ( 'NONE', #253373, #248043, #114577, .T. ) ;
#141187 = DIRECTION ( 'NONE',  ( -1.000000000000000000, 0.000000000000000000, 0.000000000000000000 ) ) ;
#141189 = EDGE_LOOP ( 'NONE', ( #226596, #9005, #199142, #3222 ) ) ;
#141190 = ORIENTED_EDGE ( 'NONE', *, *, #85453, .F. ) ;
#141192 = EDGE_CURVE ( 'NONE', #220454, #191282, #97974, .T. ) ;
#141191 = PLANE ( 'NONE',  #224091 ) ;
#141193 = LINE ( 'NONE', #143746, #217965 ) ;
#141194 = EDGE_CURVE ( 'NONE', #106770, #137660, #11985, .T. ) ;
#141195 = ORIENTED_EDGE ( 'NONE', *, *, #201969, .T. ) ;
#141196 = DIRECTION ( 'NONE',  ( 0.000000000000000000, 0.2128009952263403282, -0.9770955615653358350 ) ) ;
#141197 = CARTESIAN_POINT ( 'NONE',  ( 21.15000000000005187, 74.14873292176677921, -47.62635315998165453 ) ) ;
#141198 = AXIS2_PLACEMENT_3D ( 'NONE', #151060, #15409, #130187 ) ;
#141199 = CIRCLE ( 'NONE', #232798, 0.09999999999999609201 ) ;
#141200 = VERTEX_POINT ( 'NONE', #35414 ) ;
#141201 = AXIS2_PLACEMENT_3D ( 'NONE', #55734, #14101, #136574 ) ;
#141202 = TOROIDAL_SURFACE ( 'NONE', #53710, 11.65000000000000036, 0.1000000000000000056 ) ;
#141203 = DIRECTION ( 'NONE',  ( 0.000000000000000000, -0.9752329468386645717, -0.2211802418851520069 ) ) ;
#141204 = DIRECTION ( 'NONE',  ( -0.000000000000000000, -0.000000000000000000, -1.000000000000000000 ) ) ;
#141205 = EDGE_LOOP ( 'NONE', ( #149357, #249889, #226075, #215521 ) ) ;
#141206 = AXIS2_PLACEMENT_3D ( 'NONE', #141053, #101887, #125339 ) ;
#141207 = EDGE_LOOP ( 'NONE', ( #209085, #199925, #92823, #132228 ) ) ;
#141208 = DIRECTION ( 'NONE',  ( 0.000000000000000000, 0.8660254037844377084, 0.5000000000000015543 ) ) ;
#141209 = EDGE_CURVE ( 'NONE', #57195, #252337, #168512, .T. ) ;
#141210 = VERTEX_POINT ( 'NONE', #172368 ) ;
#141211 = EDGE_CURVE ( 'NONE', #208590, #253025, #147898, .T. ) ;
#141212 = ORIENTED_EDGE ( 'NONE', *, *, #101570, .F. ) ;
#141213 = ORIENTED_EDGE ( 'NONE', *, *, #238851, .T. ) ;
#141214 = CARTESIAN_POINT ( 'NONE',  ( 20.94999999999999929, 67.12338541492499644, -128.1380270056797031 ) ) ;
#141215 = ORIENTED_EDGE ( 'NONE', *, *, #60837, .T. ) ;
#141216 = CARTESIAN_POINT ( 'NONE',  ( -21.53752568622132557, 0.09897446127749523481, -93.71319212545147082 ) ) ;
#141217 = CIRCLE ( 'NONE', #28843, 0.1000000000000028644 ) ;
#141218 = VERTEX_POINT ( 'NONE', #87 ) ;
#141221 = EDGE_CURVE ( 'NONE', #118463, #177719, #47851, .T. ) ;
#141220 = ORIENTED_EDGE ( 'NONE', *, *, #17032, .F. ) ;
#141219 = EDGE_LOOP ( 'NONE', ( #78074, #99571, #240640, #228152 ) ) ;
#141223 = DIRECTION ( 'NONE',  ( 0.000000000000000000, 0.8814952561688476074, -0.4721928772777262417 ) ) ;
#141222 = TOROIDAL_SURFACE ( 'NONE', #33120, 14.20833333333334103, 0.1000000000000000056 ) ;
#141224 = DIRECTION ( 'NONE',  ( -1.000000000000000000, -0.000000000000000000, 0.000000000000000000 ) ) ;
#141225 = ORIENTED_EDGE ( 'NONE', *, *, #233730, .F. ) ;
#141226 = CIRCLE ( 'NONE', #57995, 0.2000000000000057288 ) ;
#141227 = EDGE_LOOP ( 'NONE', ( #170164, #72151, #55931, #34151 ) ) ;
#141228 = LINE ( 'NONE', #159520, #7910 ) ;
#141229 = CARTESIAN_POINT ( 'NONE',  ( -18.59999999999999787, 64.35000000001187459, -90.77310748452440237 ) ) ;
#141231 = ORIENTED_EDGE ( 'NONE', *, *, #7442, .F. ) ;
#141230 = DIRECTION ( 'NONE',  ( -1.000000000000000000, -0.000000000000000000, 0.000000000000000000 ) ) ;
#141232 = CARTESIAN_POINT ( 'NONE',  ( 22.39999999999999503, -3.187427350888460076, -228.3200064793908837 ) ) ;
#141233 = ORIENTED_EDGE ( 'NONE', *, *, #104966, .T. ) ;
#141234 = DIRECTION ( 'NONE',  ( 1.734723475976817507E-14, 1.000000000000000000, 6.982962677686266711E-15 ) ) ;
#141235 = CARTESIAN_POINT ( 'NONE',  ( 18.53691006697094679, 65.69784844286142800, -111.8209087672256885 ) ) ;
#141237 = EDGE_LOOP ( 'NONE', ( #175673, #145895 ) ) ;
#141236 = EDGE_CURVE ( 'NONE', #173788, #191945, #189596, .T. ) ;
#141238 = LINE ( 'NONE', #67792, #174161 ) ;
#141239 = CARTESIAN_POINT ( 'NONE',  ( -23.25000000000000355, 17.95055421627409231, -233.1200372299043693 ) ) ;
#141240 = LINE ( 'NONE', #57826, #61628 ) ;
#141241 = EDGE_CURVE ( 'NONE', #88024, #128131, #202060, .T. ) ;
#141242 = ORIENTED_EDGE ( 'NONE', *, *, #192842, .F. ) ;
#141243 = CARTESIAN_POINT ( 'NONE',  ( 15.74999999999999645, 13.18880795147152618, -215.2702608532411830 ) ) ;
#141244 = ORIENTED_EDGE ( 'NONE', *, *, #131884, .T. ) ;
#141245 = VERTEX_POINT ( 'NONE', #156646 ) ;
#141246 = AXIS2_PLACEMENT_3D ( 'NONE', #144944, #208796, #225761 ) ;
#141247 = EDGE_CURVE ( 'NONE', #120584, #203821, #239659, .T. ) ;
#141248 = EDGE_LOOP ( 'NONE', ( #134226, #36443, #19387, #40151 ) ) ;
#141249 = EDGE_LOOP ( 'NONE', ( #108383, #94142, #179922, #40567 ) ) ;
#141251 = EDGE_CURVE ( 'NONE', #175518, #217669, #238712, .T. ) ;
#141250 = CARTESIAN_POINT ( 'NONE',  ( -16.89020380669786547, 9.950000000011137047, -79.75741114811062005 ) ) ;
#141252 = VERTEX_POINT ( 'NONE', #219127 ) ;
#141253 = CARTESIAN_POINT ( 'NONE',  ( 22.45305468355009992, 25.97741635855175346, -254.4468634167663197 ) ) ;
#141254 = AXIS2_PLACEMENT_3D ( 'NONE', #72354, #253524, #50184 ) ;
#141255 = ORIENTED_EDGE ( 'NONE', *, *, #219033, .F. ) ;
#141256 = DIRECTION ( 'NONE',  ( -0.000000000000000000, 1.000000000000000000, -0.000000000000000000 ) ) ;
#141257 = EDGE_CURVE ( 'NONE', #221635, #58706, #10706, .T. ) ;
#141258 = DIRECTION ( 'NONE',  ( 0.000000000000000000, 0.000000000000000000, -1.000000000000000000 ) ) ;
#141259 = ORIENTED_EDGE ( 'NONE', *, *, #2188, .F. ) ;
#141260 = ORIENTED_EDGE ( 'NONE', *, *, #158800, .F. ) ;
#141261 = AXIS2_PLACEMENT_3D ( 'NONE', #140053, #85198, #160942 ) ;
#141262 = EDGE_LOOP ( 'NONE', ( #69650, #157334 ) ) ;
#141263 = EDGE_CURVE ( 'NONE', #123899, #97258, #129226, .T. ) ;
#141265 = EDGE_CURVE ( 'NONE', #30110, #187156, #160573, .T. ) ;
#141264 = AXIS2_PLACEMENT_3D ( 'NONE', #153668, #184390, #223507 ) ;
#141266 = DIRECTION ( 'NONE',  ( -1.000000000000000000, 0.000000000000000000, 0.000000000000000000 ) ) ;
#141267 = EDGE_CURVE ( 'NONE', #177752, #9341, #77322, .T. ) ;
#141268 = FACE_OUTER_BOUND ( 'NONE', #48635, .T. ) ;
#141270 = AXIS2_PLACEMENT_3D ( 'NONE', #240849, #219988, #98719 ) ;
#141269 = CARTESIAN_POINT ( 'NONE',  ( 21.05000000000000071, 65.27628289530478867, -162.3581939154368285 ) ) ;
#141271 = CARTESIAN_POINT ( 'NONE',  ( -33.72168855820452649, 11.47316190337362585, -109.7500000000000284 ) ) ;
#141272 = LINE ( 'NONE', #220803, #81404 ) ;
#141274 = CARTESIAN_POINT ( 'NONE',  ( 21.15000000000000213, 33.98486250090727623, -243.5821103306120108 ) ) ;
#141273 = CARTESIAN_POINT ( 'NONE',  ( -20.54999999999999716, 49.36776662947724503, -253.7196102226803021 ) ) ;
#141275 = DIRECTION ( 'NONE',  ( 0.000000000000000000, 0.000000000000000000, -1.000000000000000000 ) ) ;
#141276 = CARTESIAN_POINT ( 'NONE',  ( -18.59999999999999787, 68.97833521811159585, -65.78954208262706516 ) ) ;
#141277 = DIRECTION ( 'NONE',  ( -1.000000000000000000, 0.000000000000000000, 0.000000000000000000 ) ) ;
#141278 = CARTESIAN_POINT ( 'NONE',  ( 18.59999999999999076, 69.55000000001230376, -160.0060803140843859 ) ) ;
#141279 = EDGE_CURVE ( 'NONE', #255434, #138354, #57484, .T. ) ;
#141280 = ORIENTED_EDGE ( 'NONE', *, *, #91863, .F. ) ;
#141281 = AXIS2_PLACEMENT_3D ( 'NONE', #62438, #102813, #165388 ) ;
#141282 = AXIS2_PLACEMENT_3D ( 'NONE', #188885, #10257, #111934 ) ;
#141283 = AXIS2_PLACEMENT_3D ( 'NONE', #80022, #216984, #237850 ) ;
#141284 = VECTOR ( 'NONE', #42834, 1000.000000000000000 ) ;
#141285 = ADVANCED_FACE ( 'NONE', ( #160487 ), #61355, .T. ) ;
#141287 = ORIENTED_EDGE ( 'NONE', *, *, #22705, .F. ) ;
#141286 = CARTESIAN_POINT ( 'NONE',  ( 21.04999999999999716, 10.68430915749624610, -108.0266967903268807 ) ) ;
#141288 = ORIENTED_EDGE ( 'NONE', *, *, #256562, .F. ) ;
#141289 = AXIS2_PLACEMENT_3D ( 'NONE', #180115, #165354, #144476 ) ;
#141290 = CARTESIAN_POINT ( 'NONE',  ( 18.59999999999999432, 1.162701749949165642, -108.6000000000000227 ) ) ;
#141291 = ADVANCED_FACE ( 'NONE', ( #15844 ), #114759, .T. ) ;
#141292 = CYLINDRICAL_SURFACE ( 'NONE', #77823, 0.09999999999999939493 ) ;
#141293 = CARTESIAN_POINT ( 'NONE',  ( -22.44366136229477249, 64.17290991523515231, -247.0962312331226940 ) ) ;
#141294 = ADVANCED_FACE ( 'NONE', ( #135746 ), #197001, .T. ) ;
#141295 = VERTEX_POINT ( 'NONE', #182607 ) ;
#141296 = FILL_AREA_STYLE ('',( #61754 ) ) ;
#141297 = CARTESIAN_POINT ( 'NONE',  ( 20.94999999999999929, 75.50266930301991408, -205.3568637872625686 ) ) ;
#141298 = CARTESIAN_POINT ( 'NONE',  ( 21.05000000000000426, 65.52973064315669660, -241.8780481312162749 ) ) ;
#141299 = CIRCLE ( 'NONE', #95509, 0.9750000000000036415 ) ;
#141300 = ORIENTED_EDGE ( 'NONE', *, *, #167427, .T. ) ;
#141301 = CARTESIAN_POINT ( 'NONE',  ( 21.14999999999999858, 69.45934304831041572, -69.52310748452435973 ) ) ;
#141302 = CARTESIAN_POINT ( 'NONE',  ( 20.10000000000000497, 5.572697453181475247, 16.49970471148372297 ) ) ;
#141303 = ADVANCED_FACE ( 'NONE', ( #3948 ), #146021, .T. ) ;
#141304 = CARTESIAN_POINT ( 'NONE',  ( -18.59999999999999787, 70.65875701002036635, -112.8297576910123752 ) ) ;
#141306 = ORIENTED_EDGE ( 'NONE', *, *, #162734, .T. ) ;
#141305 = DIRECTION ( 'NONE',  ( 0.000000000000000000, 0.4930308989874980785, 0.8700118002898462599 ) ) ;
#141308 = ORIENTED_EDGE ( 'NONE', *, *, #157951, .F. ) ;
#141307 = DIRECTION ( 'NONE',  ( -1.000000000000000000, -2.952720810173289112E-16, 0.000000000000000000 ) ) ;
#141309 = FACE_OUTER_BOUND ( 'NONE', #188347, .T. ) ;
#141310 = LINE ( 'NONE', #198711, #166534 ) ;
#141311 = DIRECTION ( 'NONE',  ( 0.000000000000000000, -0.8660254037844468122, -0.4999999999999859557 ) ) ;
#141312 = CIRCLE ( 'NONE', #124576, 7.720710678118687831 ) ;
#141313 = CARTESIAN_POINT ( 'NONE',  ( 22.39999999999999503, 64.35000000001194564, -103.1231074845243825 ) ) ;
#141314 = ADVANCED_FACE ( 'NONE', ( #82170 ), #48205, .F. ) ;
#141316 = DIRECTION ( 'NONE',  ( 0.000000000000000000, 0.9916376685811618685, -0.1290532225514649800 ) ) ;
#141315 = CARTESIAN_POINT ( 'NONE',  ( -17.29838795459062695, 65.62845014205868210, -80.91836620191291729 ) ) ;
#141317 = CARTESIAN_POINT ( 'NONE',  ( 18.59999999999999076, 4.193200906077805712, -212.0298262072164164 ) ) ;
#141318 = AXIS2_PLACEMENT_3D ( 'NONE', #27811, #229826, #207714 ) ;
#141319 = CYLINDRICAL_SURFACE ( 'NONE', #16090, 11.79999999999999361 ) ;
#141320 = CARTESIAN_POINT ( 'NONE',  ( -21.05000000000000071, 75.90220970870339556, -142.7809220950004203 ) ) ;
#141321 = LINE ( 'NONE', #106018, #35334 ) ;
#141322 = B_SPLINE_CURVE_WITH_KNOTS ( 'NONE', 3,
 ( #107846, #24490, #103972, #63580, #184813, #47856, #225205, #201814, #163985, #4866 ),
 .UNSPECIFIED., .F., .F.,
 ( 4, 3, 3, 4 ),
 ( 1.956645815986047257E-15, 8.145022132834093008E-06, 1.905645951092512798E-05, 2.061107371225883743E-05 ),
 .UNSPECIFIED. ) ;
#141323 = DIRECTION ( 'NONE',  ( 1.000000000000000000, 0.000000000000000000, 0.000000000000000000 ) ) ;
#141325 = VERTEX_POINT ( 'NONE', #27406 ) ;
#141324 = CIRCLE ( 'NONE', #53845, 0.1000000000000028644 ) ;
#141326 = CARTESIAN_POINT ( 'NONE',  ( 21.05000000000000071, -0.09999999998884512298, -93.95934304829877703 ) ) ;
#141327 = ORIENTED_EDGE ( 'NONE', *, *, #36981, .F. ) ;
#141328 = ORIENTED_EDGE ( 'NONE', *, *, #136408, .F. ) ;
#141329 = EDGE_CURVE ( 'NONE', #118476, #257876, #210606, .T. ) ;
#141330 = CARTESIAN_POINT ( 'NONE',  ( -20.99749315643149217, 11.74999999999999645, -26.48519423124078642 ) ) ;
#141331 = FACE_OUTER_BOUND ( 'NONE', #226733, .T. ) ;
#141332 = ORIENTED_EDGE ( 'NONE', *, *, #136160, .F. ) ;
#141333 = AXIS2_PLACEMENT_3D ( 'NONE', #67310, #210675, #50301 ) ;
#141334 = ORIENTED_EDGE ( 'NONE', *, *, #207075, .F. ) ;
#141335 = SURFACE_SIDE_STYLE ('',( #119215 ) ) ;
#141336 = EDGE_CURVE ( 'NONE', #201923, #30729, #35677, .T. ) ;
#141337 = EDGE_LOOP ( 'NONE', ( #136383, #24344, #152485, #148621 ) ) ;
#141338 = DIRECTION ( 'NONE',  ( -0.7071067811865127117, -0.7071067811865821007, 0.000000000000000000 ) ) ;
#141339 = AXIS2_PLACEMENT_3D ( 'NONE', #163745, #146710, #84138 ) ;
#141340 = ORIENTED_EDGE ( 'NONE', *, *, #13954, .T. ) ;
#141341 = DIRECTION ( 'NONE',  ( 0.000000000000000000, 0.000000000000000000, 1.000000000000000000 ) ) ;
#141342 = CARTESIAN_POINT ( 'NONE',  ( -23.25000000000000000, -0.09999999998884338825, -155.8504291924551808 ) ) ;
#141343 = CARTESIAN_POINT ( 'NONE',  ( 23.14999999999999858, 5.000000000011153745, -188.5947339810868755 ) ) ;
#141344 = DIRECTION ( 'NONE',  ( 0.000000000000000000, 0.000000000000000000, 1.000000000000000000 ) ) ;
#141345 = CARTESIAN_POINT ( 'NONE',  ( -21.14999999999999858, 64.35000000001238618, -169.9231074845244507 ) ) ;
#141346 = CARTESIAN_POINT ( 'NONE',  ( -18.79999999999999716, 1.212568896937007645, -8.000000000000000000 ) ) ;
#141347 = DIRECTION ( 'NONE',  ( 1.000000000000000000, 0.000000000000000000, 0.000000000000000000 ) ) ;
#141349 = EDGE_LOOP ( 'NONE', ( #148233, #218941, #119300 ) ) ;
#141348 = CARTESIAN_POINT ( 'NONE',  ( -21.30740335185486245, 75.90106547423584971, -76.07976540655232611 ) ) ;
#141351 = DIRECTION ( 'NONE',  ( 0.000000000000000000, -1.000000000000000000, 0.000000000000000000 ) ) ;
#141350 = CARTESIAN_POINT ( 'NONE',  ( 20.95017935633852346, 65.52451072038628865, -61.94566768713390559 ) ) ;
#141352 = DIRECTION ( 'NONE',  ( -1.000000000000000000, 0.000000000000000000, 0.000000000000000000 ) ) ;
#141353 = ORIENTED_EDGE ( 'NONE', *, *, #48345, .F. ) ;
#141354 = CARTESIAN_POINT ( 'NONE',  ( -18.39999999999999858, 8.841736820195469804, -245.4273993276876240 ) ) ;
#141355 = CARTESIAN_POINT ( 'NONE',  ( 20.94999999999999929, 1.115600667400684642E-11, -100.5000000000000426 ) ) ;
#141356 = ORIENTED_EDGE ( 'NONE', *, *, #45632, .F. ) ;
#141358 = DIRECTION ( 'NONE',  ( 0.000000000000000000, -0.9910827722268049644, 0.1332476588733589040 ) ) ;
#141357 = PLANE ( 'NONE',  #174633 ) ;
#141359 = VECTOR ( 'NONE', #234454, 1000.000000000000000 ) ;
#141360 = CARTESIAN_POINT ( 'NONE',  ( -16.87333278164152972, 66.11739021543296246, -82.65627529067786838 ) ) ;
#141361 = VERTEX_POINT ( 'NONE', #83457 ) ;
#141362 = DIRECTION ( 'NONE',  ( 0.000000000000000000, 1.000000000000000000, 0.000000000000000000 ) ) ;
#141363 = CARTESIAN_POINT ( 'NONE',  ( -21.05000000000000071, 76.00000000001213607, -136.5231074845243313 ) ) ;
#141364 = DIRECTION ( 'NONE',  ( 1.000000000000000000, 0.000000000000000000, 0.000000000000000000 ) ) ;
#141365 = EDGE_LOOP ( 'NONE', ( #124613, #49280, #236146, #163504 ) ) ;
#141366 = EDGE_CURVE ( 'NONE', #20965, #124745, #248018, .T. ) ;
#141367 = CARTESIAN_POINT ( 'NONE',  ( -18.50000000000000000, 70.05000000001165006, -59.21740517948951066 ) ) ;
#141368 = AXIS2_PLACEMENT_3D ( 'NONE', #179302, #178009, #157170 ) ;
#141369 = CARTESIAN_POINT ( 'NONE',  ( -20.64999999999999858, 20.06933876993645782, -235.7297789824848451 ) ) ;
#141371 = DIRECTION ( 'NONE',  ( 1.000000000000000000, -0.000000000000000000, 0.000000000000000000 ) ) ;
#141370 = AXIS2_PLACEMENT_3D ( 'NONE', #147391, #65283, #48288 ) ;
#141372 = AXIS2_PLACEMENT_3D ( 'NONE', #157156, #220939, #97113 ) ;
#141373 = DIRECTION ( 'NONE',  ( 0.000000000000000000, 0.2128009952263485993, -0.9770955615653341697 ) ) ;
#141374 = DIRECTION ( 'NONE',  ( -4.408576920032448588E-17, 0.1350103645451876666, 0.9908441862701600211 ) ) ;
#141376 = EDGE_LOOP ( 'NONE', ( #42876, #72293, #6172, #255362 ) ) ;
#141375 = DIRECTION ( 'NONE',  ( 0.000000000000000000, 0.8814952561688437216, -0.4721928772777332362 ) ) ;
#141377 = DIRECTION ( 'NONE',  ( 2.952720810173289112E-16, 0.9651348961777146407, -0.2617529984165072321 ) ) ;
#141378 = LINE ( 'NONE', #180524, #228086 ) ;
#141379 = CARTESIAN_POINT ( 'NONE',  ( -21.12757541349819590, 75.99483878420197414, -75.99648805577588462 ) ) ;
#141380 = DIRECTION ( 'NONE',  ( 0.000000000000000000, 1.000000000000000000, 0.000000000000000000 ) ) ;
#141381 = EDGE_CURVE ( 'NONE', #3179, #203889, #23558, .T. ) ;
#141382 = DIRECTION ( 'NONE',  ( 0.000000000000000000, 0.000000000000000000, 1.000000000000000000 ) ) ;
#141384 = EDGE_LOOP ( 'NONE', ( #213992, #31494, #122512, #187499 ) ) ;
#141383 = DIRECTION ( 'NONE',  ( -0.7071067811865474617, 0.7071067811865474617, 0.000000000000000000 ) ) ;
#141385 = DIRECTION ( 'NONE',  ( -2.252264143451594314E-15, 0.9579639084728162057, 0.2868887416115976086 ) ) ;
#141386 = DIRECTION ( 'NONE',  ( 1.000000000000000000, 0.000000000000000000, 0.000000000000000000 ) ) ;
#141387 = DIRECTION ( 'NONE',  ( -1.000000000000000000, 0.000000000000000000, -0.000000000000000000 ) ) ;
#141388 = ADVANCED_FACE ( 'NONE', ( #6509 ), #243836, .F. ) ;
#141389 = ORIENTED_EDGE ( 'NONE', *, *, #169202, .T. ) ;
#141390 = CARTESIAN_POINT ( 'NONE',  ( -12.25000000000000000, 66.65000000001226965, -153.1573643172505115 ) ) ;
#141391 = DIRECTION ( 'NONE',  ( 1.000000000000000000, 0.000000000000000000, 0.000000000000000000 ) ) ;
#141392 = AXIS2_PLACEMENT_3D ( 'NONE', #27102, #186145, #7500 ) ;
#141393 = CIRCLE ( 'NONE', #174770, 4.099999999999992539 ) ;
#141394 = CARTESIAN_POINT ( 'NONE',  ( 21.14999999999999858, 67.21339244341145047, -57.27310748452438105 ) ) ;
#141395 = AXIS2_PLACEMENT_3D ( 'NONE', #248588, #32136, #191213 ) ;
#141396 = CARTESIAN_POINT ( 'NONE',  ( 18.49999999999999645, 77.16270174994990327, -94.92310748452430857 ) ) ;
#141397 = EDGE_CURVE ( 'NONE', #76393, #139587, #73382, .T. ) ;
#141398 = CARTESIAN_POINT ( 'NONE',  ( -16.83233564386403458, 9.930221796595763095, -87.72452066347565847 ) ) ;
#141399 = CIRCLE ( 'NONE', #116469, 0.1000000000000028644 ) ;
#141400 = ORIENTED_EDGE ( 'NONE', *, *, #87414, .F. ) ;
#141401 = EDGE_LOOP ( 'NONE', ( #85299, #229813, #183345, #13773, #20622 ) ) ;
#141402 = EDGE_CURVE ( 'NONE', #237327, #81995, #106891, .T. ) ;
#141403 = DIRECTION ( 'NONE',  ( 0.000000000000000000, -1.000000000000000000, 0.000000000000000000 ) ) ;
#141404 = DIRECTION ( 'NONE',  ( 1.000000000000000000, 0.000000000000000000, 0.000000000000000000 ) ) ;
#141405 = EDGE_CURVE ( 'NONE', #178434, #223761, #186451, .T. ) ;
#141406 = DIRECTION ( 'NONE',  ( 0.000000000000000000, 0.000000000000000000, -1.000000000000000000 ) ) ;
#141407 = LINE ( 'NONE', #98386, #180664 ) ;
#141408 = ORIENTED_EDGE ( 'NONE', *, *, #150159, .F. ) ;
#141409 = ADVANCED_FACE ( 'NONE', ( #204700 ), #206005, .T. ) ;
#141410 = DIRECTION ( 'NONE',  ( 0.000000000000000000, 0.2128009952263485993, -0.9770955615653341697 ) ) ;
#141411 = CARTESIAN_POINT ( 'NONE',  ( 20.87631937322879239, 11.84462878906222727, -206.1777914865159005 ) ) ;
#141412 = ADVANCED_FACE ( 'NONE', ( #163050 ), #87321, .F. ) ;
#141413 = DIRECTION ( 'NONE',  ( 0.000000000000000000, 0.9126074666063769270, 0.4088369013363280513 ) ) ;
#141414 = FACE_OUTER_BOUND ( 'NONE', #73320, .T. ) ;
#141416 = CARTESIAN_POINT ( 'NONE',  ( 21.30000000000002558, 0.8618440306782485516, -204.9572370243411115 ) ) ;
#141415 = AXIS2_PLACEMENT_3D ( 'NONE', #228047, #49407, #10295 ) ;
#141417 = FACE_OUTER_BOUND ( 'NONE', #248139, .T. ) ;
#141418 = VERTEX_POINT ( 'NONE', #66497 ) ;
#141420 = ORIENTED_EDGE ( 'NONE', *, *, #155134, .F. ) ;
#141419 = DIRECTION ( 'NONE',  ( 1.000000000000000000, 0.000000000000000000, 0.000000000000000000 ) ) ;
#141421 = ORIENTED_EDGE ( 'NONE', *, *, #34063, .F. ) ;
#141422 = PLANE ( 'NONE',  #227938 ) ;
#141423 = ORIENTED_EDGE ( 'NONE', *, *, #40686, .T. ) ;
#141424 = CARTESIAN_POINT ( 'NONE',  ( 21.12230431290518951, 75.99479014832341761, -176.4806741378173740 ) ) ;
#141425 = CARTESIAN_POINT ( 'NONE',  ( 20.27550659511089037, 22.63149853307782422, -231.5820423879664247 ) ) ;
#141426 = DIRECTION ( 'NONE',  ( 0.000000000000000000, 0.2617529984164915779, 0.9651348961777187485 ) ) ;
#141427 = VECTOR ( 'NONE', #254494, 1000.000000000000114 ) ;
#141428 = EDGE_LOOP ( 'NONE', ( #46521, #160175, #138783, #201399 ) ) ;
#141429 = CARTESIAN_POINT ( 'NONE',  ( -16.89318236219976654, 66.04846474213643148, -56.87823711663025250 ) ) ;
#141430 = CARTESIAN_POINT ( 'NONE',  ( 19.75857864376268935, 11.65000000001115943, -91.75000000000005684 ) ) ;
#141431 = ORIENTED_EDGE ( 'NONE', *, *, #136881, .F. ) ;
#141432 = EDGE_CURVE ( 'NONE', #176380, #120793, #202154, .T. ) ;
#141433 = CARTESIAN_POINT ( 'NONE',  ( -13.54036565897076194, 9.451541661396669625, -152.4538754988305982 ) ) ;
#141435 = EDGE_LOOP ( 'NONE', ( #202015, #20986, #91521, #40600 ) ) ;
#141434 = LINE ( 'NONE', #179309, #63259 ) ;
#141436 = DIRECTION ( 'NONE',  ( 1.000000000000000000, 0.000000000000000000, -0.000000000000000000 ) ) ;
#141437 = DIRECTION ( 'NONE',  ( 0.000000000000000000, -0.9126074666063622720, -0.4088369013363611360 ) ) ;
#141438 = AXIS2_PLACEMENT_3D ( 'NONE', #99372, #79807, #238915 ) ;
#141439 = AXIS2_PLACEMENT_3D ( 'NONE', #256847, #254315, #135656 ) ;
#141440 = ORIENTED_EDGE ( 'NONE', *, *, #49743, .F. ) ;
#141441 = DIRECTION ( 'NONE',  ( 2.840903330521631775E-16, 0.8700118002898354908, -0.4930308989875170078 ) ) ;
#141443 = EDGE_CURVE ( 'NONE', #77481, #235211, #235538, .T. ) ;
#141442 = DIRECTION ( 'NONE',  ( 0.000000000000000000, -6.982962677686266711E-15, 1.000000000000000000 ) ) ;
#141444 = CARTESIAN_POINT ( 'NONE',  ( 23.14999999999999858, 2.000000000011158630, -67.00000000000000000 ) ) ;
#141445 = ORIENTED_EDGE ( 'NONE', *, *, #89721, .T. ) ;
#141446 = CARTESIAN_POINT ( 'NONE',  ( -20.94999999999999929, 57.84918772656043728, -226.1321410194968280 ) ) ;
#141447 = CARTESIAN_POINT ( 'NONE',  ( 20.94999999999997442, 77.26327546522891510, -61.62124281777789037 ) ) ;
#141448 = CARTESIAN_POINT ( 'NONE',  ( -22.39999999999999858, 7.790779598384560245, -100.5000000000000284 ) ) ;
#141449 = CIRCLE ( 'NONE', #212393, 12.87499999999999822 ) ;
#141450 = ORIENTED_EDGE ( 'NONE', *, *, #203262, .T. ) ;
#141451 = EDGE_CURVE ( 'NONE', #12375, #118755, #181325, .T. ) ;
#141452 = ADVANCED_FACE ( 'NONE', ( #9088 ), #69079, .F. ) ;
#141453 = AXIS2_PLACEMENT_3D ( 'NONE', #172818, #209319, #72408 ) ;
#141454 = AXIS2_PLACEMENT_3D ( 'NONE', #202992, #239565, #85574 ) ;
#141455 = CIRCLE ( 'NONE', #187279, 0.09999999999999543976 ) ;
#141456 = ORIENTED_EDGE ( 'NONE', *, *, #109385, .F. ) ;
#141457 = CIRCLE ( 'NONE', #153997, 7.800000000000003375 ) ;
#141458 = AXIS2_PLACEMENT_3D ( 'NONE', #84326, #62257, #187355 ) ;
#141459 = ORIENTED_EDGE ( 'NONE', *, *, #170655, .F. ) ;
#141460 = DIRECTION ( 'NONE',  ( 0.000000000000000000, 0.8814952561688390587, -0.4721928772777420624 ) ) ;
#141461 = VECTOR ( 'NONE', #80019, 1000.000000000000000 ) ;
#141462 = CARTESIAN_POINT ( 'NONE',  ( -18.50000000000000000, -7.714568254029292582, -236.5586399380299270 ) ) ;
#141465 = EDGE_CURVE ( 'NONE', #155635, #198535, #156489, .T. ) ;
#141464 = ORIENTED_EDGE ( 'NONE', *, *, #218672, .F. ) ;
#141463 = DIRECTION ( 'NONE',  ( 0.000000000000000000, 0.9908441862701782288, -0.1350103645450542456 ) ) ;
#141466 = DIRECTION ( 'NONE',  ( 0.000000000000000000, -0.5283051335750404975, 0.8490545835446967615 ) ) ;
#141467 = LINE ( 'NONE', #24118, #15744 ) ;
#141468 = FACE_BOUND ( 'NONE', #197243, .T. ) ;
#141469 = CARTESIAN_POINT ( 'NONE',  ( -16.89146115310546037, 51.62267385565390043, -231.9431803160651384 ) ) ;
#141470 = CARTESIAN_POINT ( 'NONE',  ( -18.50000000000000000, 85.40000000001209912, -129.2258477248609552 ) ) ;
#141471 = EDGE_CURVE ( 'NONE', #22095, #144454, #53348, .T. ) ;
#141472 = DIRECTION ( 'NONE',  ( -1.000000000000000000, 0.000000000000000000, 0.000000000000000000 ) ) ;
#141473 = EDGE_CURVE ( 'NONE', #149811, #183814, #164648, .T. ) ;
#141475 = ORIENTED_EDGE ( 'NONE', *, *, #20926, .T. ) ;
#141474 = DIRECTION ( 'NONE',  ( 0.000000000000000000, 0.000000000000000000, 1.000000000000000000 ) ) ;
#141477 = ORIENTED_EDGE ( 'NONE', *, *, #115456, .T. ) ;
#141476 = LINE ( 'NONE', #7097, #11109 ) ;
#141478 = CARTESIAN_POINT ( 'NONE',  ( 22.60000000000000142, 0.1008583691098682150, -55.25043287651065782 ) ) ;
#141479 = ORIENTED_EDGE ( 'NONE', *, *, #60544, .F. ) ;
#141480 = ORIENTED_EDGE ( 'NONE', *, *, #229842, .T. ) ;
#141481 = CARTESIAN_POINT ( 'NONE',  ( -20.54999999999999716, 2.388061258337340615E-16, -31.59999999999999787 ) ) ;
#141482 = CARTESIAN_POINT ( 'NONE',  ( 21.05000000000000071, 8.876614585098254295, -175.8850804788446567 ) ) ;
#141484 = ADVANCED_FACE ( 'NONE', ( #247695 ), #70377, .F. ) ;
#141483 = DIRECTION ( 'NONE',  ( -1.000000000000000000, 2.849773892568378313E-16, -7.728835255496647986E-17 ) ) ;
#141485 = DIRECTION ( 'NONE',  ( -1.000000000000000000, -3.190570557967288949E-16, -6.948722487160392945E-17 ) ) ;
#141486 = FACE_OUTER_BOUND ( 'NONE', #239426, .T. ) ;
#141487 = DIRECTION ( 'NONE',  ( -1.000000000000000000, -0.000000000000000000, 0.000000000000000000 ) ) ;
#141488 = CIRCLE ( 'NONE', #249832, 0.1999999999999987899 ) ;
#141489 = DIRECTION ( 'NONE',  ( 1.000000000000000000, 0.000000000000000000, 0.000000000000000000 ) ) ;
#141490 = VERTEX_POINT ( 'NONE', #208593 ) ;
#141491 = EDGE_LOOP ( 'NONE', ( #231760, #35475, #6602, #63993 ) ) ;
#141492 = VECTOR ( 'NONE', #50757, 1000.000000000000000 ) ;
#141493 = ORIENTED_EDGE ( 'NONE', *, *, #204326, .T. ) ;
#141494 = DIRECTION ( 'NONE',  ( 0.000000000000000000, 1.000000000000000000, 0.000000000000000000 ) ) ;
#141495 = AXIS2_PLACEMENT_3D ( 'NONE', #88724, #13086, #73080 ) ;
#141496 = CARTESIAN_POINT ( 'NONE',  ( -14.23072895065542198, 66.54401276639880791, -54.51157631762654887 ) ) ;
#141497 = CARTESIAN_POINT ( 'NONE',  ( -22.47071067811865319, -1.546016791165058413, -193.4356622592196970 ) ) ;
#141498 = ORIENTED_EDGE ( 'NONE', *, *, #61700, .F. ) ;
#141499 = DIRECTION ( 'NONE',  ( 1.000000000000000000, 0.000000000000000000, 0.000000000000000000 ) ) ;
#141500 = EDGE_CURVE ( 'NONE', #218982, #50959, #256326, .T. ) ;
#141501 = ORIENTED_EDGE ( 'NONE', *, *, #60887, .T. ) ;
#141502 = EDGE_CURVE ( 'NONE', #180993, #147671, #31582, .T. ) ;
#141503 = FACE_OUTER_BOUND ( 'NONE', #79660, .T. ) ;
#141504 = ORIENTED_EDGE ( 'NONE', *, *, #69228, .F. ) ;
#141505 = CIRCLE ( 'NONE', #174897, 11.79999999999999716 ) ;
#141506 = DIRECTION ( 'NONE',  ( -1.000000000000000000, 7.801181613359275410E-16, 1.456333823655510085E-15 ) ) ;
#141507 = AXIS2_PLACEMENT_3D ( 'NONE', #52070, #135461, #74260 ) ;
#141508 = CARTESIAN_POINT ( 'NONE',  ( 15.15590539855245922, 9.410682294279107296, -182.9311434419481941 ) ) ;
#141509 = ORIENTED_EDGE ( 'NONE', *, *, #38315, .F. ) ;
#141510 = EDGE_CURVE ( 'NONE', #35933, #64409, #173057, .T. ) ;
#141511 = DIRECTION ( 'NONE',  ( 1.000000000000000000, 0.000000000000000000, 0.000000000000000000 ) ) ;
#141513 = ORIENTED_EDGE ( 'NONE', *, *, #125362, .T. ) ;
#141512 = FACE_OUTER_BOUND ( 'NONE', #29019, .T. ) ;
#141514 = CARTESIAN_POINT ( 'NONE',  ( 20.97462148592287079, 67.12526242356200612, -191.2684631527934016 ) ) ;
#141515 = AXIS2_PLACEMENT_3D ( 'NONE', #100202, #140635, #179788 ) ;
#141516 = VERTEX_POINT ( 'NONE', #11674 ) ;
#141517 = DIRECTION ( 'NONE',  ( 1.000000000000000000, 0.000000000000000000, -0.000000000000000000 ) ) ;
#141518 = ORIENTED_EDGE ( 'NONE', *, *, #110285, .T. ) ;
#141519 = FACE_OUTER_BOUND ( 'NONE', #86487, .T. ) ;
#141520 = CARTESIAN_POINT ( 'NONE',  ( 22.40736611211992368, 26.02743912001966464, -254.3139371321002216 ) ) ;
#141521 =( BOUNDED_SURFACE ( )  B_SPLINE_SURFACE ( 3, 2, ( 
 ( #230841, #229544, #190431 ),
 ( #71763, #191723, #189124 ),
 ( #32664, #112176, #212554 ),
 ( #10496, #53465, #13076 ) ),
 .UNSPECIFIED., .F., .F., .F. ) 
 B_SPLINE_SURFACE_WITH_KNOTS ( ( 4, 4 ),
 ( 3, 3 ),
 ( 0.0008258556059633754111, 0.0009616864997632785118 ),
 ( 0.000000000000000000, 1.000000000000000000 ),
 .UNSPECIFIED. ) 
 GEOMETRIC_REPRESENTATION_ITEM ( )  RATIONAL_B_SPLINE_SURFACE ( (
 ( 1.000000000000000000, 0.9152888060719349683, 1.000000000000000000),
 ( 1.000000000000000000, 0.9327727094138323904, 1.000000000000000000),
 ( 1.000000000000000000, 0.9369023509258284088, 1.000000000000000000),
 ( 1.000000000000000000, 0.9246339933864518024, 1.000000000000000000) ) ) 
 REPRESENTATION_ITEM ( '' )  SURFACE ( )  );
#141522 = CARTESIAN_POINT ( 'NONE',  ( -18.59999999999999787, 67.23127455305841238, -235.8551265064783991 ) ) ;
#141523 = DIRECTION ( 'NONE',  ( -4.448008912761042820E-16, 0.9770955615653312831, 0.2128009952263615334 ) ) ;
#141524 = DIRECTION ( 'NONE',  ( -1.000000000000000000, -7.304098846218164250E-16, 4.217023435051628197E-16 ) ) ;
#141525 = ORIENTED_EDGE ( 'NONE', *, *, #237074, .F. ) ;
#141526 = CARTESIAN_POINT ( 'NONE',  ( -23.15000000000000213, 64.35000000001146248, -43.03791325517834565 ) ) ;
#141527 = DIRECTION ( 'NONE',  ( 1.000000000000000000, 0.000000000000000000, 0.000000000000000000 ) ) ;
#141528 = AXIS2_PLACEMENT_3D ( 'NONE', #42681, #223865, #127356 ) ;
#141529 = DIRECTION ( 'NONE',  ( 0.000000000000000000, -0.2128009952263650861, 0.9770955615653305060 ) ) ;
#141530 = ADVANCED_FACE ( 'NONE', ( #148611 ), #19065, .T. ) ;
#141531 = ORIENTED_EDGE ( 'NONE', *, *, #137517, .T. ) ;
#141532 = DIRECTION ( 'NONE',  ( 1.073024830501117923E-15, -0.9126074666063771490, -0.4088369013363281623 ) ) ;
#141533 = ORIENTED_EDGE ( 'NONE', *, *, #210598, .T. ) ;
#141534 = DIRECTION ( 'NONE',  ( 0.000000000000000000, -7.034366652768095332E-15, 1.000000000000000000 ) ) ;
#141535 = ORIENTED_EDGE ( 'NONE', *, *, #74058, .F. ) ;
#141536 =( BOUNDED_CURVE ( )  B_SPLINE_CURVE ( 3, ( #163295, #204956, #122887, #165872 ),
 .UNSPECIFIED., .F., .F. ) 
 B_SPLINE_CURVE_WITH_KNOTS ( ( 4, 4 ),
 ( -1.092459456231154036E-13, 1.570796326794918985 ),
 .UNSPECIFIED. ) 
 CURVE ( )  GEOMETRIC_REPRESENTATION_ITEM ( )  RATIONAL_B_SPLINE_CURVE ( ( 1.000000000000000000, 0.8047378541243339622, 0.8047378541243339622, 1.000000000000000000 ) ) 
 REPRESENTATION_ITEM ( '' )  );
#141537 = CARTESIAN_POINT ( 'NONE',  ( -23.25000000000000000, -11.48087284838115885, -203.5004116939112464 ) ) ;
#141538 = DIRECTION ( 'NONE',  ( 0.000000000000000000, 0.000000000000000000, -1.000000000000000000 ) ) ;
#141539 = ORIENTED_EDGE ( 'NONE', *, *, #12047, .T. ) ;
#141542 = ORIENTED_EDGE ( 'NONE', *, *, #149989, .F. ) ;
#141541 = ADVANCED_FACE ( 'NONE', ( #91194 ), #132896, .T. ) ;
#141540 = CARTESIAN_POINT ( 'NONE',  ( -22.50000000000000000, 0.1000000000111554016, -67.00000000000004263 ) ) ;
#141543 = DIRECTION ( 'NONE',  ( 1.000000000000000000, -0.000000000000000000, 0.000000000000000000 ) ) ;
#141544 = ORIENTED_EDGE ( 'NONE', *, *, #179573, .T. ) ;
#141545 = CARTESIAN_POINT ( 'NONE',  ( -21.05000000000000071, 76.00000000001165290, -69.52310748452431710 ) ) ;
#141546 = EDGE_CURVE ( 'NONE', #103638, #256979, #92798, .T. ) ;
#141547 = CYLINDRICAL_SURFACE ( 'NONE', #114644, 0.1999999999999987899 ) ;
#141548 = ORIENTED_EDGE ( 'NONE', *, *, #142104, .F. ) ;
#141549 = ORIENTED_EDGE ( 'NONE', *, *, #232815, .T. ) ;
#141550 = AXIS2_PLACEMENT_3D ( 'NONE', #103263, #5443, #244074 ) ;
#141552 = VECTOR ( 'NONE', #215690, 1000.000000000000000 ) ;
#141551 = DIRECTION ( 'NONE',  ( -0.000000000000000000, 0.8814952561688430555, -0.4721928772777346239 ) ) ;
#141554 = EDGE_CURVE ( 'NONE', #26765, #171566, #172050, .T. ) ;
#141553 = CARTESIAN_POINT ( 'NONE',  ( 18.54999999999999716, 8.750000000011182166, -154.8500000000000227 ) ) ;
#141555 = AXIS2_PLACEMENT_3D ( 'NONE', #56427, #135965, #137256 ) ;
#141557 = CARTESIAN_POINT ( 'NONE',  ( -16.86422026484316916, 66.02955263915140449, -123.9408942588513725 ) ) ;
#141556 = AXIS2_PLACEMENT_3D ( 'NONE', #154833, #197776, #98637 ) ;
#141558 = ORIENTED_EDGE ( 'NONE', *, *, #30246, .T. ) ;
#141559 = ORIENTED_EDGE ( 'NONE', *, *, #54259, .F. ) ;
#141560 =( BOUNDED_SURFACE ( )  B_SPLINE_SURFACE ( 3, 2, ( 
 ( #76061, #51331, #155641 ),
 ( #33136, #136013, #56480 ),
 ( #252126, #154367, #36974 ),
 ( #95620, #133474, #172653 ),
 ( #74823, #73531, #253412 ),
 ( #153082, #193462, #150482 ) ),
 .UNSPECIFIED., .F., .F., .F. ) 
 B_SPLINE_SURFACE_WITH_KNOTS ( ( 4, 2, 4 ),
 ( 3, 3 ),
 ( 0.0001792624049599544510, 0.0003686986002124726996, 0.0005581347954649909212 ),
 ( 0.000000000000000000, 1.000000000000000000 ),
 .UNSPECIFIED. ) 
 GEOMETRIC_REPRESENTATION_ITEM ( )  RATIONAL_B_SPLINE_SURFACE ( (
 ( 1.000000000000000000, 0.9238795325112832968, 1.000000000000000000),
 ( 1.000000000000000000, 0.9229318695238958314, 1.000000000000000000),
 ( 1.000000000000000000, 0.8926288119230034734, 1.000000000000000000),
 ( 1.000000000000000000, 0.8123777807272225537, 1.000000000000000000),
 ( 1.000000000000000000, 0.7629087100930789234, 1.000000000000000000),
 ( 1.000000000000000000, 0.7071067811865475727, 1.000000000000000000) ) ) 
 REPRESENTATION_ITEM ( '' )  SURFACE ( )  );
#141561 = EDGE_CURVE ( 'NONE', #84465, #50748, #197946, .T. ) ;
#141562 = TOROIDAL_SURFACE ( 'NONE', #233184, 11.65000000000000036, 0.1000000000000000056 ) ;
#141565 = EDGE_CURVE ( 'NONE', #40828, #99793, #74234, .T. ) ;
#141564 = ADVANCED_FACE ( 'NONE', ( #32539 ), #112054, .F. ) ;
#141563 = FACE_OUTER_BOUND ( 'NONE', #32262, .T. ) ;
#141567 = ORIENTED_EDGE ( 'NONE', *, *, #59576, .F. ) ;
#141566 = CARTESIAN_POINT ( 'NONE',  ( 18.59999999999997655, 1.115600667400684642E-11, -200.9999999999999432 ) ) ;
#141568 = CARTESIAN_POINT ( 'NONE',  ( -18.40000000000000213, 64.66825945288744037, -190.8731074845244393 ) ) ;
#141569 = AXIS2_PLACEMENT_3D ( 'NONE', #65996, #185947, #67281 ) ;
#141570 = DIRECTION ( 'NONE',  ( 0.000000000000000000, 0.000000000000000000, -1.000000000000000000 ) ) ;
#141571 = DIRECTION ( 'NONE',  ( -0.000000000000000000, -0.4088369013363281623, 0.9126074666063771490 ) ) ;
#141572 = AXIS2_PLACEMENT_3D ( 'NONE', #82750, #103612, #5799 ) ;
#141574 = DIRECTION ( 'NONE',  ( 1.000000000000000000, 1.394253735153569469E-16, 2.602809386958778209E-16 ) ) ;
#141573 = CARTESIAN_POINT ( 'NONE',  ( -16.87036670365549540, 66.01058118071040326, -124.0026676018264311 ) ) ;
#141575 = CARTESIAN_POINT ( 'NONE',  ( -21.05000000000000071, 75.90220970870339556, -142.7809220950004203 ) ) ;
#141576 = DIRECTION ( 'NONE',  ( -8.673617379883787770E-15, -1.000000000000000000, 0.000000000000000000 ) ) ;
#141577 = CARTESIAN_POINT ( 'NONE',  ( -16.87036670365549895, 60.86740053880574663, -221.1564527318009254 ) ) ;
#141578 = DIRECTION ( 'NONE',  ( 0.000000000000000000, 0.2617529984165180013, 0.9651348961777117541 ) ) ;
#141579 = ADVANCED_FACE ( 'NONE', ( #108197 ), #29962, .T. ) ;
#141580 = EDGE_CURVE ( 'NONE', #181378, #214190, #38931, .T. ) ;
#141581 = ORIENTED_EDGE ( 'NONE', *, *, #93336, .F. ) ;
#141582 = ORIENTED_EDGE ( 'NONE', *, *, #53712, .F. ) ;
#141583 = ADVANCED_FACE ( 'NONE', ( #15531 ), #106344, .T. ) ;
#141584 = CARTESIAN_POINT ( 'NONE',  ( -20.64999999999999858, 2.400000000011155432, -46.72462192276210402 ) ) ;
#141585 = ORIENTED_EDGE ( 'NONE', *, *, #77965, .T. ) ;
#141586 = CARTESIAN_POINT ( 'NONE',  ( -21.05000000000000071, 64.40000000001177227, -76.45131071479988805 ) ) ;
#141587 = EDGE_CURVE ( 'NONE', #13339, #108178, #194065, .T. ) ;
#141588 = ORIENTED_EDGE ( 'NONE', *, *, #141587, .T. ) ;
#141589 = CARTESIAN_POINT ( 'NONE',  ( -23.15000000000000213, 85.00000000001222134, -146.4170766071767389 ) ) ;
#141590 = EDGE_CURVE ( 'NONE', #145938, #5729, #185677, .T. ) ;
#141591 = VECTOR ( 'NONE', #49081, 1000.000000000000114 ) ;
#141593 = ORIENTED_EDGE ( 'NONE', *, *, #100706, .T. ) ;
#141592 = ORIENTED_EDGE ( 'NONE', *, *, #132850, .F. ) ;
#141594 = VERTEX_POINT ( 'NONE', #156332 ) ;
#141595 = VERTEX_POINT ( 'NONE', #114605 ) ;
#141596 = CARTESIAN_POINT ( 'NONE',  ( -20.64999999999999858, 7.150000000000000355, -21.15000000000000213 ) ) ;
#141597 = DIRECTION ( 'NONE',  ( -2.342056488767301376E-15, -0.1350103645451904977, 0.9908441862701596881 ) ) ;
#141599 = EDGE_LOOP ( 'NONE', ( #28547, #135867, #13894, #8776 ) ) ;
#141598 = CARTESIAN_POINT ( 'NONE',  ( 22.60000000000000142, 76.00000000001267608, -203.5231074845243597 ) ) ;
#141600 = VECTOR ( 'NONE', #141970, 1000.000000000000000 ) ;
#141601 = CARTESIAN_POINT ( 'NONE',  ( 20.22483756094572271, 40.20239933964113277, -237.5519095886356240 ) ) ;
#141602 = EDGE_CURVE ( 'NONE', #176027, #27481, #218819, .T. ) ;
#141603 = CARTESIAN_POINT ( 'NONE',  ( 20.94403535211772294, 65.69367753730655579, -97.51892380663478832 ) ) ;
#141605 = VERTEX_POINT ( 'NONE', #237122 ) ;
#141604 = CARTESIAN_POINT ( 'NONE',  ( 20.95420533658165141, 10.54586447477073285, -141.5675060206932585 ) ) ;
#141606 = CARTESIAN_POINT ( 'NONE',  ( 19.81427058490545789, 11.66856398039208820, -125.2500000000000568 ) ) ;
#141607 = ORIENTED_EDGE ( 'NONE', *, *, #48184, .F. ) ;
#141608 = CARTESIAN_POINT ( 'NONE',  ( 20.94999999999999929, -11.64999999998883595, -64.00000000000000000 ) ) ;
#141610 = VERTEX_POINT ( 'NONE', #139274 ) ;
#141609 = DIRECTION ( 'NONE',  ( 0.000000000000000000, 7.086529944415894657E-15, -1.000000000000000000 ) ) ;
#141611 = DIRECTION ( 'NONE',  ( -0.000000000000000000, 1.000000000000000000, 6.982962677686266711E-15 ) ) ;
#141612 = CARTESIAN_POINT ( 'NONE',  ( -15.57281606413133979, 27.00251997126096271, -233.7480822475820332 ) ) ;
#141613 = DIRECTION ( 'NONE',  ( 0.000000000000000000, 1.000000000000000000, -3.469446951953635015E-14 ) ) ;
#141615 = EDGE_CURVE ( 'NONE', #71443, #181843, #57169, .T. ) ;
#141614 = ORIENTED_EDGE ( 'NONE', *, *, #52061, .F. ) ;
#141617 = DIRECTION ( 'NONE',  ( 1.000000000000000000, 0.000000000000000000, 0.000000000000000000 ) ) ;
#141616 = DIRECTION ( 'NONE',  ( 0.000000000000000000, -0.8700118002898321601, 0.4930308989875230030 ) ) ;
#141618 = CARTESIAN_POINT ( 'NONE',  ( -14.87770893841227071, 66.56936289831506315, -84.75484686646342425 ) ) ;
#141619 = AXIS2_PLACEMENT_3D ( 'NONE', #100346, #80784, #139483 ) ;
#141620 = DIRECTION ( 'NONE',  ( 1.000000000000000000, 0.000000000000000000, 0.000000000000000000 ) ) ;
#141621 = DIRECTION ( 'NONE',  ( 0.000000000000000000, 2.664535259100315349E-15, -1.000000000000000000 ) ) ;
#141622 = CARTESIAN_POINT ( 'NONE',  ( -17.04295772865321368, 44.10486005708381185, -235.2305778318707326 ) ) ;
#141623 = CIRCLE ( 'NONE', #145705, 0.1000000000000028644 ) ;
#141624 = VERTEX_POINT ( 'NONE', #213698 ) ;
#141625 = VERTEX_POINT ( 'NONE', #96303 ) ;
#141626 = EDGE_LOOP ( 'NONE', ( #56218, #116953, #200965, #219143, #114648 ) ) ;
#141627 = CARTESIAN_POINT ( 'NONE',  ( -23.25000000000000000, 74.00000000001254818, -182.6477294072865050 ) ) ;
#141628 = ORIENTED_EDGE ( 'NONE', *, *, #245758, .F. ) ;
#141630 = DIRECTION ( 'NONE',  ( 0.000000000000000000, -7.172728831056617961E-15, 1.000000000000000000 ) ) ;
#141629 = CIRCLE ( 'NONE', #62534, 11.80000000000000426 ) ;
#141631 = ORIENTED_EDGE ( 'NONE', *, *, #23501, .F. ) ;
#141632 = ADVANCED_FACE ( 'NONE', ( #174634 ), #16807, .F. ) ;
#141633 = CARTESIAN_POINT ( 'NONE',  ( 21.14999999999999858, -8.874060656858240748, -215.4698323230865640 ) ) ;
#141634 = CARTESIAN_POINT ( 'NONE',  ( 18.46921299892754575, -9.509378177812612520, -40.48657870937042702 ) ) ;
#141635 = CIRCLE ( 'NONE', #62541, 0.09999999999999939493 ) ;
#141636 = ORIENTED_EDGE ( 'NONE', *, *, #166526, .T. ) ;
#141637 = CARTESIAN_POINT ( 'NONE',  ( 12.33938619321248176, 9.360723793997193454, -151.3139271946067481 ) ) ;
#141639 = ORIENTED_EDGE ( 'NONE', *, *, #43945, .F. ) ;
#141638 = VECTOR ( 'NONE', #86477, 1000.000000000000000 ) ;
#141640 = VERTEX_POINT ( 'NONE', #20657 ) ;
#141641 = CIRCLE ( 'NONE', #195845, 4.049999999999998934 ) ;
#141642 = AXIS2_PLACEMENT_3D ( 'NONE', #91327, #71780, #151313 ) ;
#141643 = ORIENTED_EDGE ( 'NONE', *, *, #30688, .F. ) ;
#141644 = CIRCLE ( 'NONE', #75052, 0.1999999999999987899 ) ;
#141645 = AXIS2_PLACEMENT_3D ( 'NONE', #21098, #215409, #36815 ) ;
#141646 = DIRECTION ( 'NONE',  ( 0.000000000000000000, 0.000000000000000000, -1.000000000000000000 ) ) ;
#141647 = CARTESIAN_POINT ( 'NONE',  ( -20.54999999999999716, 76.00000000001142553, -36.02310748452432421 ) ) ;
#141648 = CARTESIAN_POINT ( 'NONE',  ( -22.59999999999999787, 11.74956712350054744, -167.3991416309012550 ) ) ;
#141649 = DIRECTION ( 'NONE',  ( 1.000000000000000000, 0.000000000000000000, 0.000000000000000000 ) ) ;
#141650 = LINE ( 'NONE', #200348, #67798 ) ;
#141651 = AXIS2_PLACEMENT_3D ( 'NONE', #150322, #130741, #207731 ) ;
#141653 = PLANE ( 'NONE',  #224254 ) ;
#141652 = CARTESIAN_POINT ( 'NONE',  ( 18.49999999999999289, 21.13195309841794867, -243.6318585593224100 ) ) ;
#141654 = FACE_OUTER_BOUND ( 'NONE', #233677, .T. ) ;
#141656 = EDGE_LOOP ( 'NONE', ( #160531, #170150, #220909, #204906 ) ) ;
#141655 = CARTESIAN_POINT ( 'NONE',  ( -18.59999999999999787, 9.350000000011156942, -121.7500000000000426 ) ) ;
#141657 = FACE_OUTER_BOUND ( 'NONE', #129915, .T. ) ;
#141658 = CARTESIAN_POINT ( 'NONE',  ( 20.95512820512820440, 67.12384868372420499, -161.4644784893834810 ) ) ;
#141659 = ORIENTED_EDGE ( 'NONE', *, *, #194260, .T. ) ;
#141660 = DIRECTION ( 'NONE',  ( -1.000000000000000000, 0.000000000000000000, 0.000000000000000000 ) ) ;
#141661 = FACE_OUTER_BOUND ( 'NONE', #247504, .T. ) ;
#141662 = CARTESIAN_POINT ( 'NONE',  ( 19.96984138294284250, 64.25000000001146816, -44.79853541332327893 ) ) ;
#141663 = EDGE_LOOP ( 'NONE', ( #127793, #123770, #103806, #113680, #179228, #136781, #20469, #89473, #93907, #223674, #241082 ) ) ;
#141664 = DIRECTION ( 'NONE',  ( 0.000000000000000000, 0.9126074666063770380, 0.4088369013363281068 ) ) ;
#141665 = VERTEX_POINT ( 'NONE', #37657 ) ;
#141666 = VERTEX_POINT ( 'NONE', #118473 ) ;
#141667 = CARTESIAN_POINT ( 'NONE',  ( -18.59999999999999787, -1.851617760457748618, -145.6031897196037050 ) ) ;
#141668 = ORIENTED_EDGE ( 'NONE', *, *, #247727, .F. ) ;
#141669 = CARTESIAN_POINT ( 'NONE',  ( -16.93583594267724379, 60.85906102366440962, -221.1138329385686063 ) ) ;
#141670 = LINE ( 'NONE', #185938, #74051 ) ;
#141671 = CARTESIAN_POINT ( 'NONE',  ( -16.81453563122428463, 9.939100205448109904, -121.2882586606453401 ) ) ;
#141672 = DIRECTION ( 'NONE',  ( 0.000000000000000000, 0.000000000000000000, -1.000000000000000000 ) ) ;
#141673 = ORIENTED_EDGE ( 'NONE', *, *, #121374, .T. ) ;
#141674 = AXIS2_PLACEMENT_3D ( 'NONE', #21275, #23841, #141196 ) ;
#141675 = CARTESIAN_POINT ( 'NONE',  ( -23.25000000000000000, 40.35498466150055918, -247.8953732508333587 ) ) ;
#141677 = EDGE_CURVE ( 'NONE', #92976, #13199, #198316, .T. ) ;
#141676 = DIRECTION ( 'NONE',  ( 0.000000000000000000, 0.000000000000000000, -1.000000000000000000 ) ) ;
#141678 = VECTOR ( 'NONE', #182614, 1000.000000000000000 ) ;
#141679 = CARTESIAN_POINT ( 'NONE',  ( 18.58143601961907976, 10.43572941510573315, -192.2499999999999716 ) ) ;
#141680 = FACE_OUTER_BOUND ( 'NONE', #196641, .T. ) ;
#141681 = VECTOR ( 'NONE', #243661, 1000.000000000000114 ) ;
#141682 = EDGE_LOOP ( 'NONE', ( #9512, #161453, #196808, #202417 ) ) ;
#141684 = ORIENTED_EDGE ( 'NONE', *, *, #258025, .F. ) ;
#141683 = CARTESIAN_POINT ( 'NONE',  ( -22.59999999999999787, 76.00000000001195133, -103.0231074845243171 ) ) ;
#141685 = FACE_OUTER_BOUND ( 'NONE', #166280, .T. ) ;
#141686 = DIRECTION ( 'NONE',  ( 1.875376730785738212E-16, -0.4721928772777346239, -0.8814952561688430555 ) ) ;
#141687 = CARTESIAN_POINT ( 'NONE',  ( -16.94878442675511465, 9.991729103002157331, -87.88821957563791898 ) ) ;
#141688 = CARTESIAN_POINT ( 'NONE',  ( -18.50000000000000000, -1.687074390091559906, 12.81457296654165212 ) ) ;
#141689 = CARTESIAN_POINT ( 'NONE',  ( -22.57320508075687115, 11.65000000001115588, -167.5000000000000000 ) ) ;
#141690 = CARTESIAN_POINT ( 'NONE',  ( 21.14999999999999858, -0.09999999998884338825, -21.85042919245520210 ) ) ;
#141691 = CIRCLE ( 'NONE', #120887, 0.09999999999999939493 ) ;
#141692 = ADVANCED_FACE ( 'NONE', ( #197981 ), #35840, .T. ) ;
#141693 = ORIENTED_EDGE ( 'NONE', *, *, #149757, .T. ) ;
#141694 = CARTESIAN_POINT ( 'NONE',  ( 22.84999999999999787, 4.776122516674678272E-16, 3.900000000000000355 ) ) ;
#141695 = TOROIDAL_SURFACE ( 'NONE', #54204, 11.90000000000000213, 0.1000000000000000056 ) ;
#141696 = DIRECTION ( 'NONE',  ( 0.000000000000000000, -1.000000000000000000, -0.000000000000000000 ) ) ;
#141697 = CARTESIAN_POINT ( 'NONE',  ( -18.31331870001099915, 77.39837993464469434, -241.7498918423547991 ) ) ;
#141698 = CARTESIAN_POINT ( 'NONE',  ( -21.14999999999999858, 76.00000000001242029, -176.5637644362255969 ) ) ;
#141700 = AXIS2_PLACEMENT_3D ( 'NONE', #210273, #87721, #167305 ) ;
#141699 = DIRECTION ( 'NONE',  ( -1.000000000000000000, -0.000000000000000000, -0.000000000000000000 ) ) ;
#141701 = CARTESIAN_POINT ( 'NONE',  ( 20.86036036209904054, 65.37895722344063643, -61.85675906601803575 ) ) ;
#141702 = AXIS2_PLACEMENT_3D ( 'NONE', #140567, #98847, #100138 ) ;
#141703 = ORIENTED_EDGE ( 'NONE', *, *, #230460, .T. ) ;
#141704 = EDGE_LOOP ( 'NONE', ( #197568, #174377, #155381, #165716 ) ) ;
#141705 = CARTESIAN_POINT ( 'NONE',  ( 20.94999999999999929, 85.50000000001149658, -45.91707660717669626 ) ) ;
#141706 = LINE ( 'NONE', #60883, #125946 ) ;
#141707 = EDGE_CURVE ( 'NONE', #213386, #177788, #1040, .T. ) ;
#141708 = DIRECTION ( 'NONE',  ( -0.000000000000000000, 0.9770955615653313941, 0.2128009952263603954 ) ) ;
#141709 = CARTESIAN_POINT ( 'NONE',  ( 21.02374657821566828, 16.98881331262128214, -224.4946931421776810 ) ) ;
#141710 = EDGE_CURVE ( 'NONE', #165270, #204719, #80577, .T. ) ;
#141711 = ORIENTED_EDGE ( 'NONE', *, *, #232215, .F. ) ;
#141712 = CARTESIAN_POINT ( 'NONE',  ( 21.14999999999999858, 60.09787988008869775, -221.2279614330287245 ) ) ;
#141713 = EDGE_CURVE ( 'NONE', #11251, #66400, #198139, .T. ) ;
#141714 = DIRECTION ( 'NONE',  ( 0.000000000000000000, 0.9999631594459055250, 0.008583690987131395445 ) ) ;
#141715 = CARTESIAN_POINT ( 'NONE',  ( 20.94999999999999929, 76.00000000001216449, -140.5231074845243597 ) ) ;
#141716 = AXIS2_PLACEMENT_3D ( 'NONE', #93487, #34836, #174367 ) ;
#141717 = ADVANCED_FACE ( 'NONE', ( #160177 ), #98851, .F. ) ;
#141718 = VECTOR ( 'NONE', #152448, 1000.000000000000000 ) ;
#141719 = LINE ( 'NONE', #896, #253606 ) ;
#141720 = EDGE_CURVE ( 'NONE', #188417, #254397, #65049, .T. ) ;
#141721 = ORIENTED_EDGE ( 'NONE', *, *, #8537, .F. ) ;
#141722 = FACE_OUTER_BOUND ( 'NONE', #235600, .T. ) ;
#141723 = EDGE_LOOP ( 'NONE', ( #98493, #115158, #170002, #228202 ) ) ;
#141724 = DIRECTION ( 'NONE',  ( 9.044546369203339308E-15, -0.7397360091702694929, -0.6728971962616898672 ) ) ;
#141725 = CARTESIAN_POINT ( 'NONE',  ( 18.79999999999999716, 1.350000000000000089, 21.90000000000000213 ) ) ;
#141726 = CARTESIAN_POINT ( 'NONE',  ( 20.94999999999999929, 68.97833521811131163, -32.18954208262707795 ) ) ;
#141727 = DIRECTION ( 'NONE',  ( 0.7071067811865475727, 0.6909108974501237954, 0.1504730267678056066 ) ) ;
#141728 = DIRECTION ( 'NONE',  ( 1.000000000000000000, 0.000000000000000000, 0.000000000000000000 ) ) ;
#141729 = CARTESIAN_POINT ( 'NONE',  ( 20.94999999999999929, 1.115600667400684642E-11, -175.3000000000000398 ) ) ;
#141730 = CARTESIAN_POINT ( 'NONE',  ( -20.94999999999999929, 76.00000000001244871, -170.0231074845243597 ) ) ;
#141731 = DIRECTION ( 'NONE',  ( 0.000000000000000000, 0.2617529984165152257, 0.9651348961777124202 ) ) ;
#141732 = EDGE_CURVE ( 'NONE', #250000, #151911, #177516, .T. ) ;
#141733 = CARTESIAN_POINT ( 'NONE',  ( -21.14999999999999858, 64.35000000001214460, -136.4231074845243938 ) ) ;
#141734 = AXIS2_PLACEMENT_3D ( 'NONE', #109693, #230965, #250491 ) ;
#141735 = DIRECTION ( 'NONE',  ( 0.000000000000000000, 0.000000000000000000, -1.000000000000000000 ) ) ;
#141736 = AXIS2_PLACEMENT_3D ( 'NONE', #147740, #26516, #167321 ) ;
#141737 = CARTESIAN_POINT ( 'NONE',  ( 20.94999999999999574, 1.115600667400684642E-11, -134.0000000000000000 ) ) ;
#141738 = CARTESIAN_POINT ( 'NONE',  ( 23.14999999999999858, 77.93026979236670115, -204.0466134813579231 ) ) ;
#141739 = AXIS2_PLACEMENT_3D ( 'NONE', #214456, #57941, #193629 ) ;
#141740 = FACE_OUTER_BOUND ( 'NONE', #254356, .T. ) ;
#141741 = CARTESIAN_POINT ( 'NONE',  ( 20.99551997958262106, 56.17759395754559648, -227.9318432312958294 ) ) ;
#141742 = AXIS2_PLACEMENT_3D ( 'NONE', #158742, #219965, #137843 ) ;
#141743 = ORIENTED_EDGE ( 'NONE', *, *, #87625, .T. ) ;
#141744 = CARTESIAN_POINT ( 'NONE',  ( 23.15000000000000213, -11.64999999998883595, -130.9000000000000341 ) ) ;
#141745 = CARTESIAN_POINT ( 'NONE',  ( 23.14999999999999858, 77.04701199367727327, -199.6625678998140359 ) ) ;
#141746 = ORIENTED_EDGE ( 'NONE', *, *, #141046, .T. ) ;
#141747 = CARTESIAN_POINT ( 'NONE',  ( -22.41119224318417125, 1.115600667400684642E-11, -55.35042919245524473 ) ) ;
#141748 = AXIS2_PLACEMENT_3D ( 'NONE', #48372, #109626, #28867 ) ;
#141749 = CARTESIAN_POINT ( 'NONE',  ( -17.73285935862007534, 10.85798180380174394, -190.7585618097804456 ) ) ;
#141750 = ORIENTED_EDGE ( 'NONE', *, *, #53591, .T. ) ;
#141751 = DIRECTION ( 'NONE',  ( 0.000000000000000000, 0.000000000000000000, -1.000000000000000000 ) ) ;
#141752 = LINE ( 'NONE', #221280, #47634 ) ;
#141753 = VERTEX_POINT ( 'NONE', #164007 ) ;
#141754 = EDGE_CURVE ( 'NONE', #14805, #213760, #70133, .T. ) ;
#141755 = ORIENTED_EDGE ( 'NONE', *, *, #209772, .T. ) ;
#141756 = ORIENTED_EDGE ( 'NONE', *, *, #231509, .F. ) ;
#141757 = ADVANCED_FACE ( 'NONE', ( #62335 ), #48299, .T. ) ;
#141759 = EDGE_CURVE ( 'NONE', #222651, #172976, #173249, .T. ) ;
#141758 = CARTESIAN_POINT ( 'NONE',  ( 20.94999999999999574, 79.28653038861995128, -235.9126307598797325 ) ) ;
#141760 = CARTESIAN_POINT ( 'NONE',  ( -18.59999999999999787, 64.35000000001141984, -36.02310748452440237 ) ) ;
#141762 = DIRECTION ( 'NONE',  ( 0.000000000000000000, 0.4721928772777346239, 0.8814952561688430555 ) ) ;
#141761 = UNCERTAINTY_MEASURE_WITH_UNIT (LENGTH_MEASURE( 1.000000000000000082E-05 ), #133337, 'distance_accuracy_value', 'NONE');
#141763 = CARTESIAN_POINT ( 'NONE',  ( 21.05000000000000071, 28.50120599808395028, -258.2149742250584268 ) ) ;
#141764 = CARTESIAN_POINT ( 'NONE',  ( 20.94999999999999574, 67.07338541492521244, -161.5514244653012952 ) ) ;
#141765 = CARTESIAN_POINT ( 'NONE',  ( -23.25000000000000000, 78.48087866980282001, -232.8271061603568910 ) ) ;
#141766 = EDGE_CURVE ( 'NONE', #192597, #18074, #181594, .T. ) ;
#141767 = DIRECTION ( 'NONE',  ( 0.000000000000000000, -0.9209589331071864615, 0.3896596508878908960 ) ) ;
#141768 = FACE_OUTER_BOUND ( 'NONE', #75954, .T. ) ;
#141770 = ORIENTED_EDGE ( 'NONE', *, *, #147124, .F. ) ;
#141769 = CARTESIAN_POINT ( 'NONE',  ( -18.54159361262942696, -9.463132135481966856, -40.54912221629287927 ) ) ;
#141771 = ORIENTED_EDGE ( 'NONE', *, *, #207671, .F. ) ;
#141773 = FACE_OUTER_BOUND ( 'NONE', #23935, .T. ) ;
#141772 = LINE ( 'NONE', #163924, #45351 ) ;
#141775 = ORIENTED_EDGE ( 'NONE', *, *, #255425, .T. ) ;
#141774 = CARTESIAN_POINT ( 'NONE',  ( -16.89155683852641232, 61.10357422879747702, -220.4362292707147333 ) ) ;
#141776 = AXIS2_PLACEMENT_3D ( 'NONE', #67073, #240570, #141463 ) ;
#141777 = EDGE_CURVE ( 'NONE', #234494, #36355, #222668, .T. ) ;
#141778 = ORIENTED_EDGE ( 'NONE', *, *, #236017, .F. ) ;
#141779 = DIRECTION ( 'NONE',  ( 1.000000000000000000, 0.000000000000000000, 0.000000000000000000 ) ) ;
#141780 = ADVANCED_FACE ( 'NONE', ( #7485 ), #182292, .T. ) ;
#141781 = CARTESIAN_POINT ( 'NONE',  ( -18.79999999999999716, 6.742993295648862961, 9.658650260582458458 ) ) ;
#141783 = EDGE_CURVE ( 'NONE', #121863, #138313, #98317, .T. ) ;
#141782 = CARTESIAN_POINT ( 'NONE',  ( 18.39999999999999503, 8.212522512469059066, -212.1579332307740344 ) ) ;
#141784 = VECTOR ( 'NONE', #202598, 1000.000000000000000 ) ;
#141785 = DIRECTION ( 'NONE',  ( -1.000000000000000000, -0.000000000000000000, -0.000000000000000000 ) ) ;
#141786 = DIRECTION ( 'NONE',  ( 1.000000000000000000, 0.000000000000000000, 0.000000000000000000 ) ) ;
#141787 = CARTESIAN_POINT ( 'NONE',  ( -18.40000000000000213, 11.47316190337364183, -87.89142135623735896 ) ) ;
#141788 = DIRECTION ( 'NONE',  ( -0.7071067811865463515, 0.7071067811865487940, -0.000000000000000000 ) ) ;
#141789 = ORIENTED_EDGE ( 'NONE', *, *, #234558, .F. ) ;
#141790 = EDGE_LOOP ( 'NONE', ( #71948, #71945, #8058, #133403 ) ) ;
#141791 = CARTESIAN_POINT ( 'NONE',  ( 20.94999999999999574, -10.47749788991998088, -206.4278944321438587 ) ) ;
#141792 = EDGE_CURVE ( 'NONE', #77947, #223496, #239850, .T. ) ;
#141793 = AXIS2_PLACEMENT_3D ( 'NONE', #38816, #15412, #115776 ) ;
#141794 = ORIENTED_EDGE ( 'NONE', *, *, #3716, .F. ) ;
#141795 = DIRECTION ( 'NONE',  ( 0.000000000000000000, 0.8814952561688430555, -0.4721928772777346239 ) ) ;
#141797 = ORIENTED_EDGE ( 'NONE', *, *, #182060, .F. ) ;
#141796 = AXIS2_PLACEMENT_3D ( 'NONE', #95910, #114205, #93350 ) ;
#141798 = CARTESIAN_POINT ( 'NONE',  ( -18.59999999999999787, 64.35000000001208775, -129.5083017138703667 ) ) ;
#141799 = EDGE_CURVE ( 'NONE', #210814, #38481, #69177, .T. ) ;
#141800 = AXIS2_PLACEMENT_3D ( 'NONE', #60216, #238870, #163194 ) ;
#141801 = LINE ( 'NONE', #235772, #176063 ) ;
#141802 = DIRECTION ( 'NONE',  ( 0.000000000000000000, -1.000000000000000000, 0.000000000000000000 ) ) ;
#141803 = EDGE_CURVE ( 'NONE', #230427, #223187, #114938, .T. ) ;
#141804 = DIRECTION ( 'NONE',  ( 1.836970198721029934E-16, -1.000000000000000000, -0.000000000000000000 ) ) ;
#141805 = ORIENTED_EDGE ( 'NONE', *, *, #222249, .T. ) ;
#141806 = ADVANCED_FACE ( 'NONE', ( #126137 ), #203120, .T. ) ;
#141807 = CIRCLE ( 'NONE', #183516, 0.09999999999998898659 ) ;
#141809 = TOROIDAL_SURFACE ( 'NONE', #29434, 0.2000000000000000111, 0.1000000000000000056 ) ;
#141808 = CARTESIAN_POINT ( 'NONE',  ( 21.05000000000000071, 1.349084418638171412, -108.4864989635455146 ) ) ;
#141810 = ORIENTED_EDGE ( 'NONE', *, *, #237917, .T. ) ;
#141811 = LINE ( 'NONE', #2287, #75750 ) ;
#141812 = CARTESIAN_POINT ( 'NONE',  ( 23.14999999999998437, 9.041214493067920799, -230.1626455249554795 ) ) ;
#141813 = CARTESIAN_POINT ( 'NONE',  ( 23.24999999999999289, 6.450000000011156587, -155.1500000000000057 ) ) ;
#141814 = LINE ( 'NONE', #21883, #15799 ) ;
#141815 = ORIENTED_EDGE ( 'NONE', *, *, #154989, .F. ) ;
#141816 = DIRECTION ( 'NONE',  ( 0.000000000000000000, -0.9126074666063771490, -0.4088369013363281623 ) ) ;
#141817 = ORIENTED_EDGE ( 'NONE', *, *, #7566, .T. ) ;
#141820 = VERTEX_POINT ( 'NONE', #63610 ) ;
#141819 = DIRECTION ( 'NONE',  ( 0.000000000000000000, 0.000000000000000000, -1.000000000000000000 ) ) ;
#141818 = CARTESIAN_POINT ( 'NONE',  ( 18.49713797159835948, 46.97446046665651664, -255.2810199801895408 ) ) ;
#141821 = AXIS2_PLACEMENT_3D ( 'NONE', #12794, #234369, #92295 ) ;
#141822 = DIRECTION ( 'NONE',  ( -1.000000000000000000, -0.000000000000000000, -0.000000000000000000 ) ) ;
#141823 = AXIS2_PLACEMENT_3D ( 'NONE', #92954, #13436, #228644 ) ;
#141825 = EDGE_LOOP ( 'NONE', ( #129689, #180942, #212632, #22255 ) ) ;
#141824 = AXIS2_PLACEMENT_3D ( 'NONE', #36189, #114425, #214798 ) ;
#141826 = VECTOR ( 'NONE', #190097, 1000.000000000000000 ) ;
#141827 = AXIS2_PLACEMENT_3D ( 'NONE', #125012, #184973, #141983 ) ;
#141828 = DIRECTION ( 'NONE',  ( 0.000000000000000000, 0.9915357197604882655, -0.1298341882519793711 ) ) ;
#141829 = VERTEX_POINT ( 'NONE', #24510 ) ;
#141830 = CARTESIAN_POINT ( 'NONE',  ( 18.44208962362720428, 85.55234049692090537, -129.6809344290617219 ) ) ;
#141831 = CARTESIAN_POINT ( 'NONE',  ( -16.93344882324368683, 9.996588767299030565, -54.41302569480492224 ) ) ;
#141832 = DIRECTION ( 'NONE',  ( 1.000000000000000000, -0.000000000000000000, -0.000000000000000000 ) ) ;
#141834 = ORIENTED_EDGE ( 'NONE', *, *, #180699, .T. ) ;
#141833 = CARTESIAN_POINT ( 'NONE',  ( -18.59999999999999787, 23.34004772283014972, -229.2004250369967338 ) ) ;
#141835 = DIRECTION ( 'NONE',  ( 0.000000000000000000, 0.2128009952264214300, -0.9770955615653181825 ) ) ;
#141836 = CIRCLE ( 'NONE', #50250, 0.2000000000000057288 ) ;
#141837 = VERTEX_POINT ( 'NONE', #183569 ) ;
#141838 = CARTESIAN_POINT ( 'NONE',  ( -21.05000000000000071, 36.65892442174472876, -249.5511627012454596 ) ) ;
#141839 = CARTESIAN_POINT ( 'NONE',  ( -16.94052228080551359, 9.986279733109993728, -188.3903755026694000 ) ) ;
#141840 = CARTESIAN_POINT ( 'NONE',  ( -18.48179518609124727, -9.518325300484486107, -140.8897055767626227 ) ) ;
#141841 = ORIENTED_EDGE ( 'NONE', *, *, #69333, .T. ) ;
#141842 = DIRECTION ( 'NONE',  ( 0.000000000000000000, -0.1350103645451807555, -0.9908441862701609093 ) ) ;
#141843 = ORIENTED_EDGE ( 'NONE', *, *, #164203, .T. ) ;
#141844 = DIRECTION ( 'NONE',  ( 0.000000000000000000, 3.552713678800509607E-15, -1.000000000000000000 ) ) ;
#141845 = LINE ( 'NONE', #200543, #255641 ) ;
#141846 = DIRECTION ( 'NONE',  ( 1.000000000000000000, 0.000000000000000000, 0.000000000000000000 ) ) ;
#141848 = ORIENTED_EDGE ( 'NONE', *, *, #109624, .F. ) ;
#141847 = DIRECTION ( 'NONE',  ( 0.5932847527679309119, 0.7769265190100943519, -0.2107092456252272483 ) ) ;
#141849 = CARTESIAN_POINT ( 'NONE',  ( -20.85000000000000142, 80.78317333349157536, -192.9003134612049166 ) ) ;
#141850 = AXIS2_PLACEMENT_3D ( 'NONE', #157935, #117484, #57480 ) ;
#141851 = DIRECTION ( 'NONE',  ( -1.000000000000000000, 0.000000000000000000, 0.000000000000000000 ) ) ;
#141852 = ADVANCED_FACE ( 'NONE', ( #66181 ), #14993, .F. ) ;
#141853 = DIRECTION ( 'NONE',  ( -1.000000000000000000, 0.000000000000000000, 0.000000000000000000 ) ) ;
#141854 = CIRCLE ( 'NONE', #158467, 0.1000000000000124678 ) ;
#141855 = VERTEX_POINT ( 'NONE', #223955 ) ;
#141856 = LINE ( 'NONE', #218818, #118235 ) ;
#141858 = EDGE_CURVE ( 'NONE', #84905, #78560, #85669, .T. ) ;
#141857 = CARTESIAN_POINT ( 'NONE',  ( -18.59999999999999787, 46.45388641681647357, -243.1520440498138385 ) ) ;
#141859 = VERTEX_POINT ( 'NONE', #42769 ) ;
#141860 = PLANE ( 'NONE',  #140790 ) ;
#141861 = CIRCLE ( 'NONE', #29483, 0.09999999999998898659 ) ;
#141862 = ORIENTED_EDGE ( 'NONE', *, *, #161303, .T. ) ;
#141863 = EDGE_CURVE ( 'NONE', #209494, #228778, #131691, .T. ) ;
#141865 = CARTESIAN_POINT ( 'NONE',  ( 21.00000000000000000, 61.05385884576949707, -221.3836188041226762 ) ) ;
#141864 = AXIS2_PLACEMENT_3D ( 'NONE', #128827, #50532, #11452 ) ;
#141866 = ORIENTED_EDGE ( 'NONE', *, *, #17181, .F. ) ;
#141869 = EDGE_CURVE ( 'NONE', #15594, #67110, #244806, .T. ) ;
#141868 = ORIENTED_EDGE ( 'NONE', *, *, #125511, .F. ) ;
#141867 = CARTESIAN_POINT ( 'NONE',  ( -18.40000000000000213, 11.74999999999998224, -12.65000000000000213 ) ) ;
#141872 = ORIENTED_EDGE ( 'NONE', *, *, #218090, .F. ) ;
#141871 = ORIENTED_EDGE ( 'NONE', *, *, #156808, .F. ) ;
#141870 = DIRECTION ( 'NONE',  ( 0.000000000000000000, 0.000000000000000000, -1.000000000000000000 ) ) ;
#141873 = VECTOR ( 'NONE', #74611, 1000.000000000000000 ) ;
#141874 = DIRECTION ( 'NONE',  ( 0.000000000000000000, 0.000000000000000000, -1.000000000000000000 ) ) ;
#141875 = CARTESIAN_POINT ( 'NONE',  ( -21.14999999999999858, 1.115600667400684642E-11, -160.9593430482987344 ) ) ;
#141876 = DIRECTION ( 'NONE',  ( 1.836970198721029934E-16, 1.000000000000000000, 6.982962677686266711E-15 ) ) ;
#141878 = FACE_OUTER_BOUND ( 'NONE', #234667, .T. ) ;
#141877 = PLANE ( 'NONE',  #81675 ) ;
#141879 = CIRCLE ( 'NONE', #121077, 0.6000000000000033085 ) ;
#141880 = CARTESIAN_POINT ( 'NONE',  ( -18.59999999999999787, 66.85000000001228670, -157.6731074845244223 ) ) ;
#141881 = AXIS2_PLACEMENT_3D ( 'NONE', #158667, #236883, #176945 ) ;
#141882 = CARTESIAN_POINT ( 'NONE',  ( -20.94999999999999929, 64.40000000001219860, -143.4513107147999449 ) ) ;
#141884 = DIRECTION ( 'NONE',  ( 1.186688945009009831E-16, 1.000000000000000000, 6.982962677686266711E-15 ) ) ;
#141883 = CARTESIAN_POINT ( 'NONE',  ( -16.77977881697927032, 22.98649307498303784, -230.9434316717720321 ) ) ;
#141885 = ADVANCED_FACE ( 'NONE', ( #23232 ), #2492, .T. ) ;
#141887 = EDGE_LOOP ( 'NONE', ( #146923, #166960, #124893, #100452 ) ) ;
#141886 = AXIS2_PLACEMENT_3D ( 'NONE', #66217, #153504, #94751 ) ;
#141888 = ORIENTED_EDGE ( 'NONE', *, *, #101843, .F. ) ;
#141889 = CARTESIAN_POINT ( 'NONE',  ( 23.14999999999999503, 11.65000000001116298, -112.6500000000000341 ) ) ;
#141891 = ORIENTED_EDGE ( 'NONE', *, *, #139095, .T. ) ;
#141890 = FACE_OUTER_BOUND ( 'NONE', #17307, .T. ) ;
#141892 = VERTEX_POINT ( 'NONE', #220127 ) ;
#141893 = DIRECTION ( 'NONE',  ( 1.000000000000000000, 0.000000000000000000, 0.000000000000000000 ) ) ;
#141894 = ORIENTED_EDGE ( 'NONE', *, *, #79105, .T. ) ;
#141895 = CARTESIAN_POINT ( 'NONE',  ( 18.59999999999999432, 77.13501884592258762, -162.3061306010920362 ) ) ;
#141896 = EDGE_CURVE ( 'NONE', #141135, #192810, #248669, .T. ) ;
#141897 = VERTEX_POINT ( 'NONE', #132581 ) ;
#141898 = AXIS2_PLACEMENT_3D ( 'NONE', #188984, #231978, #168180 ) ;
#141899 = CARTESIAN_POINT ( 'NONE',  ( -18.43707690579161351, -9.682403433465241349, -174.1568433774128266 ) ) ;
#141900 = EDGE_CURVE ( 'NONE', #196055, #140686, #90871, .T. ) ;
#141902 = VERTEX_POINT ( 'NONE', #249957 ) ;
#141901 = ORIENTED_EDGE ( 'NONE', *, *, #124275, .F. ) ;
#141903 = ORIENTED_EDGE ( 'NONE', *, *, #141221, .T. ) ;
#141904 = DIRECTION ( 'NONE',  ( -1.000000000000000000, 7.492892343619937423E-30, -1.073024830501117725E-15 ) ) ;
#141905 = ORIENTED_EDGE ( 'NONE', *, *, #245246, .T. ) ;
#141906 = EDGE_LOOP ( 'NONE', ( #122118, #133372, #115652, #76526 ) ) ;
#141907 = DIRECTION ( 'NONE',  ( 0.000000000000000000, 0.000000000000000000, 1.000000000000000000 ) ) ;
#141909 = ORIENTED_EDGE ( 'NONE', *, *, #75557, .F. ) ;
#141908 = CARTESIAN_POINT ( 'NONE',  ( 18.59999999999999076, 67.23127455305835554, -235.8551265064784559 ) ) ;
#141911 = CARTESIAN_POINT ( 'NONE',  ( 18.59999999999998721, 69.06610602788553877, -99.23746165015076315 ) ) ;
#141910 = PLANE ( 'NONE',  #194917 ) ;
#141912 = EDGE_CURVE ( 'NONE', #137027, #9728, #131287, .T. ) ;
#141913 = CARTESIAN_POINT ( 'NONE',  ( 21.13614978966381841, 1.115600836807273770E-11, -60.50089529816626310 ) ) ;
#141914 = DIRECTION ( 'NONE',  ( 0.000000000000000000, -0.9875055080513754913, 0.1575844902526733482 ) ) ;
#141915 = DIRECTION ( 'NONE',  ( -0.000000000000000000, -6.982962677686266711E-15, 1.000000000000000000 ) ) ;
#141916 = VERTEX_POINT ( 'NONE', #70059 ) ;
#141917 = EDGE_CURVE ( 'NONE', #31733, #146041, #230390, .T. ) ;
#141918 = ORIENTED_EDGE ( 'NONE', *, *, #49790, .T. ) ;
#141920 = CIRCLE ( 'NONE', #75326, 0.5000000000000004441 ) ;
#141919 = CARTESIAN_POINT ( 'NONE',  ( 18.49999999999999289, 65.67426406872414191, -145.1731074845244223 ) ) ;
#141921 = CARTESIAN_POINT ( 'NONE',  ( 23.14999999999999503, 64.35000000001201670, -114.7731074845243882 ) ) ;
#141922 = TOROIDAL_SURFACE ( 'NONE', #33656, 12.77500000000000036, 0.1000000000000000056 ) ;
#141923 = VECTOR ( 'NONE', #43238, 1000.000000000000000 ) ;
#141925 = EDGE_CURVE ( 'NONE', #11996, #45676, #229111, .T. ) ;
#141924 = EDGE_LOOP ( 'NONE', ( #182540, #16053, #234974, #140391 ) ) ;
#141926 = CARTESIAN_POINT ( 'NONE',  ( 21.12642695952774119, 0.09890328320052040045, -27.12434007796482760 ) ) ;
#141927 = CARTESIAN_POINT ( 'NONE',  ( -20.94999999999999929, 11.65000000001115232, -200.9999999999999432 ) ) ;
#141928 = AXIS2_PLACEMENT_3D ( 'NONE', #9575, #12178, #193380 ) ;
#141929 = DIRECTION ( 'NONE',  ( 0.000000000000000000, 0.000000000000000000, -1.000000000000000000 ) ) ;
#141930 = ORIENTED_EDGE ( 'NONE', *, *, #178101, .T. ) ;
#141931 = EDGE_LOOP ( 'NONE', ( #149912, #97536, #243798, #205169 ) ) ;
#141932 = LINE ( 'NONE', #238471, #184228 ) ;
#141933 = DIRECTION ( 'NONE',  ( -0.000000000000000000, 1.000000000000000000, 0.000000000000000000 ) ) ;
#141934 = ORIENTED_EDGE ( 'NONE', *, *, #200912, .T. ) ;
#141935 = DIRECTION ( 'NONE',  ( 0.000000000000000000, 0.2617529984165031243, 0.9651348961777157509 ) ) ;
#141936 = ORIENTED_EDGE ( 'NONE', *, *, #121474, .T. ) ;
#141937 = EDGE_CURVE ( 'NONE', #72705, #190923, #248222, .T. ) ;
#141938 = FACE_OUTER_BOUND ( 'NONE', #33276, .T. ) ;
#141940 = CARTESIAN_POINT ( 'NONE',  ( 21.05000000000000071, 1.115600667400684642E-11, -62.70000000000001705 ) ) ;
#141939 = SHAPE_REPRESENTATION ( 'Snap Open Cable Crossbars 9', ( #2425 ), #222606 ) ;
#141942 = CARTESIAN_POINT ( 'NONE',  ( -20.86777300164945004, 68.11153784908182729, -224.1393723182492579 ) ) ;
#141941 = LINE ( 'NONE', #98938, #157345 ) ;
#141943 = CARTESIAN_POINT ( 'NONE',  ( -23.25000000000000000, 64.25000000001253397, -182.1731074845244507 ) ) ;
#141945 = ADVANCED_FACE ( 'NONE', ( #89581 ), #8778, .F. ) ;
#141944 = CARTESIAN_POINT ( 'NONE',  ( -16.87435696428308063, 66.04999753707964771, -90.37311571935781274 ) ) ;
#141946 = ORIENTED_EDGE ( 'NONE', *, *, #254331, .F. ) ;
#141947 = CARTESIAN_POINT ( 'NONE',  ( 23.14999999999999503, 69.45000000001199680, -115.3731074845243398 ) ) ;
#141949 = ORIENTED_EDGE ( 'NONE', *, *, #52182, .F. ) ;
#141948 = EDGE_LOOP ( 'NONE', ( #256404, #177113, #236808, #41603 ) ) ;
#141950 = EDGE_LOOP ( 'NONE', ( #230966, #14290, #15010, #650 ) ) ;
#141951 = EDGE_LOOP ( 'NONE', ( #84980, #192694, #121025, #115228 ) ) ;
#141952 = CARTESIAN_POINT ( 'NONE',  ( -16.94333152886235183, 66.00965798856181266, -157.4151390155788590 ) ) ;
#141953 = DIRECTION ( 'NONE',  ( 1.000000000000000000, 0.000000000000000000, 0.000000000000000000 ) ) ;
#141954 = DIRECTION ( 'NONE',  ( 0.000000000000000000, 0.9875055080513743810, -0.1575844902526802316 ) ) ;
#141955 = FACE_OUTER_BOUND ( 'NONE', #51241, .T. ) ;
#141956 = CIRCLE ( 'NONE', #305, 4.900000000000001243 ) ;
#141958 = DIRECTION ( 'NONE',  ( 1.000000000000000000, -0.000000000000000000, 0.000000000000000000 ) ) ;
#141957 = CARTESIAN_POINT ( 'NONE',  ( 22.37643362114956247, 68.37421000605328913, -69.62218885820576020 ) ) ;
#141960 = ORIENTED_EDGE ( 'NONE', *, *, #146174, .F. ) ;
#141959 = CARTESIAN_POINT ( 'NONE',  ( 18.58725287972329454, 77.36873348216533941, -241.7964099312725637 ) ) ;
#141961 = CARTESIAN_POINT ( 'NONE',  ( -21.05000000000000071, 6.540656951712400691, -167.5999999999999659 ) ) ;
#141962 = ORIENTED_EDGE ( 'NONE', *, *, #122504, .T. ) ;
#141963 = CARTESIAN_POINT ( 'NONE',  ( -22.59999999999999787, 11.74956712350054566, -66.89914163090132604 ) ) ;
#141964 = ORIENTED_EDGE ( 'NONE', *, *, #38589, .T. ) ;
#141965 = ORIENTED_EDGE ( 'NONE', *, *, #60650, .T. ) ;
#141966 = DIRECTION ( 'NONE',  ( 1.000000000000000000, -0.000000000000000000, -0.000000000000000000 ) ) ;
#141967 = AXIS2_PLACEMENT_3D ( 'NONE', #149418, #50275, #129821 ) ;
#141968 = CARTESIAN_POINT ( 'NONE',  ( 18.39999999999999858, -9.499999999988842703, -107.4146583429697159 ) ) ;
#141969 = CARTESIAN_POINT ( 'NONE',  ( -16.85697194749128514, 66.09145628588790089, -48.95811175213842148 ) ) ;
#141970 = DIRECTION ( 'NONE',  ( 1.000000000000000000, -1.875376730785737719E-16, -1.309568571767809260E-30 ) ) ;
#141971 = VECTOR ( 'NONE', #6792, 1000.000000000000000 ) ;
#141972 = DIRECTION ( 'NONE',  ( 0.000000000000000000, 0.000000000000000000, 1.000000000000000000 ) ) ;
#141973 = VERTEX_POINT ( 'NONE', #210828 ) ;
#141974 = ORIENTED_EDGE ( 'NONE', *, *, #45591, .F. ) ;
#141975 = AXIS2_PLACEMENT_3D ( 'NONE', #158082, #237574, #99314 ) ;
#141976 = CARTESIAN_POINT ( 'NONE',  ( -23.25000000000000000, 73.40000000001157332, -56.29848556176223440 ) ) ;
#141977 = ORIENTED_EDGE ( 'NONE', *, *, #125835, .F. ) ;
#141978 = CARTESIAN_POINT ( 'NONE',  ( -16.92209698673482166, 23.03151742425346526, -230.9636950939940618 ) ) ;
#141979 = CYLINDRICAL_SURFACE ( 'NONE', #206751, 0.09999999999999939493 ) ;
#141980 = DIRECTION ( 'NONE',  ( 0.000000000000000000, 1.000000000000000000, 0.000000000000000000 ) ) ;
#141981 = CARTESIAN_POINT ( 'NONE',  ( -22.14074124539699540, 75.90094710416812518, -143.9131853355680732 ) ) ;
#141982 = DIRECTION ( 'NONE',  ( 0.000000000000000000, 0.000000000000000000, 1.000000000000000000 ) ) ;
#141983 = DIRECTION ( 'NONE',  ( 1.000000000000000000, 0.000000000000000000, 0.000000000000000000 ) ) ;
#141984 = DIRECTION ( 'NONE',  ( -0.000000000000000000, 1.000000000000000000, 6.982962677686266711E-15 ) ) ;
#141985 = CARTESIAN_POINT ( 'NONE',  ( -23.15000000000000213, -11.64999999998884483, -100.5000000000000284 ) ) ;
#141986 = CARTESIAN_POINT ( 'NONE',  ( 18.49999999999998224, 65.71984138295536582, -178.7985354133222131 ) ) ;
#141988 = EDGE_CURVE ( 'NONE', #138590, #109794, #194651, .T. ) ;
#141987 = CARTESIAN_POINT ( 'NONE',  ( -22.50000000000000000, 11.64987090377452361, -133.9174801091271263 ) ) ;
#141989 = VECTOR ( 'NONE', #163591, 1000.000000000000000 ) ;
#141990 = CARTESIAN_POINT ( 'NONE',  ( -21.05000000000000071, 35.97645343225767789, -235.9694016464868298 ) ) ;
#141991 = AXIS2_PLACEMENT_3D ( 'NONE', #160445, #139545, #118737 ) ;
#141993 = ORIENTED_EDGE ( 'NONE', *, *, #51435, .T. ) ;
#141992 = VECTOR ( 'NONE', #122883, 1000.000000000000000 ) ;
#141994 = CIRCLE ( 'NONE', #129540, 3.900000000000000799 ) ;
#141995 = DIRECTION ( 'NONE',  ( 1.284434275755705296E-16, -0.7071067811865471286, -0.7071067811865479058 ) ) ;
#141996 = ADVANCED_FACE ( 'NONE', ( #167879 ), #27503, .T. ) ;
#141997 = ORIENTED_EDGE ( 'NONE', *, *, #148049, .F. ) ;
#141998 = CIRCLE ( 'NONE', #125263, 0.1000000000000002554 ) ;
#141999 = AXIS2_PLACEMENT_3D ( 'NONE', #60339, #237712, #139870 ) ;
#142000 = DIRECTION ( 'NONE',  ( -1.000000000000000000, -0.000000000000000000, -0.000000000000000000 ) ) ;
#142002 = EDGE_CURVE ( 'NONE', #60954, #199798, #152378, .T. ) ;
#142001 = CARTESIAN_POINT ( 'NONE',  ( 21.05000000000000071, 61.94127660284455317, -221.8315191551248517 ) ) ;
#142003 = EDGE_CURVE ( 'NONE', #56502, #255841, #39944, .T. ) ;
#142004 = ORIENTED_EDGE ( 'NONE', *, *, #253693, .T. ) ;
#142005 = CYLINDRICAL_SURFACE ( 'NONE', #150808, 0.9000000000000014655 ) ;
#142006 = DIRECTION ( 'NONE',  ( 0.000000000000000000, -0.9999631594459053030, -0.008583690987162452199 ) ) ;
#142007 = DIRECTION ( 'NONE',  ( 1.000000000000000000, 2.986185139342070877E-16, -6.665775143889692774E-16 ) ) ;
#142008 = AXIS2_PLACEMENT_3D ( 'NONE', #32050, #91986, #213207 ) ;
#142009 = CARTESIAN_POINT ( 'NONE',  ( -20.64999999999999858, 63.56320957583155717, -222.0641766000055668 ) ) ;
#142010 = VECTOR ( 'NONE', #160455, 1000.000000000000000 ) ;
#142011 = CIRCLE ( 'NONE', #171301, 4.049999999999998046 ) ;
#142012 = CARTESIAN_POINT ( 'NONE',  ( -22.50000000000000000, 30.95512775545487472, -252.1063933345974988 ) ) ;
#142013 = DIRECTION ( 'NONE',  ( 1.000000000000000000, 0.000000000000000000, 0.000000000000000000 ) ) ;
#142014 = AXIS2_PLACEMENT_3D ( 'NONE', #228910, #206778, #112813 ) ;
#142015 = CIRCLE ( 'NONE', #129563, 0.1000000000000028644 ) ;
#142016 = VERTEX_POINT ( 'NONE', #152167 ) ;
#142017 = DIRECTION ( 'NONE',  ( -0.000000000000000000, 0.9876197685951279004, -0.1568667991644694115 ) ) ;
#142019 = ORIENTED_EDGE ( 'NONE', *, *, #237504, .F. ) ;
#142018 = FACE_OUTER_BOUND ( 'NONE', #15892, .T. ) ;
#142020 = DIRECTION ( 'NONE',  ( 1.000000000000000000, 0.000000000000000000, 0.000000000000000000 ) ) ;
#142021 = EDGE_CURVE ( 'NONE', #118445, #88637, #50441, .T. ) ;
#142022 = DIRECTION ( 'NONE',  ( 0.000000000000000000, 0.000000000000000000, -1.000000000000000000 ) ) ;
#142023 = DIRECTION ( 'NONE',  ( 1.000000000000000000, 0.000000000000000000, 0.000000000000000000 ) ) ;
#142024 = EDGE_LOOP ( 'NONE', ( #10696, #216583, #97090, #70912 ) ) ;
#142025 = CARTESIAN_POINT ( 'NONE',  ( 22.49999999999999645, 11.74956712350054744, -33.39914163090129051 ) ) ;
#142026 = CONTEXT_DEPENDENT_SHAPE_REPRESENTATION ( #157513, #43486 ) ;
#142027 = CIRCLE ( 'NONE', #29633, 0.5000000000000004441 ) ;
#142028 = DIRECTION ( 'NONE',  ( 1.000000000000000000, 0.000000000000000000, 0.000000000000000000 ) ) ;
#142029 = ORIENTED_EDGE ( 'NONE', *, *, #142347, .F. ) ;
#142030 = CARTESIAN_POINT ( 'NONE',  ( 20.99999999999999645, 66.25000000001264766, -194.2731074845244166 ) ) ;
#142031 = DIRECTION ( 'NONE',  ( 0.000000000000000000, 1.000000000000000000, 6.982962677686266711E-15 ) ) ;
#142032 = DIRECTION ( 'NONE',  ( 0.000000000000000000, -0.9126074666063772600, -0.4088369013363274407 ) ) ;
#142033 = ADVANCED_FACE ( 'NONE', ( #247371 ), #227813, .T. ) ;
#142034 = ORIENTED_EDGE ( 'NONE', *, *, #50910, .F. ) ;
#142035 = ORIENTED_EDGE ( 'NONE', *, *, #223667, .T. ) ;
#142036 = CARTESIAN_POINT ( 'NONE',  ( 20.95262331984766035, 10.50415726280100870, -74.56088832959336798 ) ) ;
#142037 = LINE ( 'NONE', #165475, #153394 ) ;
#142038 = CIRCLE ( 'NONE', #58813, 11.70000000000000284 ) ;
#142039 = DIRECTION ( 'NONE',  ( 0.000000000000000000, 0.000000000000000000, -1.000000000000000000 ) ) ;
#142040 = CARTESIAN_POINT ( 'NONE',  ( 20.94999999999999929, 7.128833340094563376, -233.7327013124401276 ) ) ;
#142041 = CARTESIAN_POINT ( 'NONE',  ( 18.49999999999999289, 10.20857864609425825, -125.2025068656296156 ) ) ;
#142042 = CARTESIAN_POINT ( 'NONE',  ( -21.05000000000000071, 87.48912529308852015, -173.1231074845242688 ) ) ;
#142043 = ADVANCED_FACE ( 'NONE', ( #150852 ), #91295, .T. ) ;
#142045 = SPHERICAL_SURFACE ( 'NONE', #228599, 0.1000000000000000056 ) ;
#142044 = PLANE ( 'NONE',  #136792 ) ;
#142046 = DIRECTION ( 'NONE',  ( 1.000000000000000000, 0.000000000000000000, 0.000000000000000000 ) ) ;
#142047 = DIRECTION ( 'NONE',  ( 1.713247197920696616E-14, 0.9876197685951252359, -0.1568667991644863424 ) ) ;
#142048 = DIRECTION ( 'NONE',  ( 0.000000000000000000, 0.000000000000000000, -1.000000000000000000 ) ) ;
#142049 = DIRECTION ( 'NONE',  ( 0.7071067811865473507, 0.3338907855510733769, 0.6233112732207618523 ) ) ;
#142050 = EDGE_LOOP ( 'NONE', ( #195038, #214556, #104398, #207866 ) ) ;
#142051 = ORIENTED_EDGE ( 'NONE', *, *, #216588, .F. ) ;
#142052 = CARTESIAN_POINT ( 'NONE',  ( -12.25000000000000178, 9.849999999999978328, -16.75000000000000355 ) ) ;
#142053 = DIRECTION ( 'NONE',  ( 1.836970198721029934E-16, 1.000000000000000000, 6.982962677686266711E-15 ) ) ;
#142055 = CARTESIAN_POINT ( 'NONE',  ( -21.70464131381649509, 7.095358018967854896, 0.000000000000000000 ) ) ;
#142054 = DIRECTION ( 'NONE',  ( 0.000000000000000000, 0.000000000000000000, 1.000000000000000000 ) ) ;
#142056 = VECTOR ( 'NONE', #180786, 1000.000000000000114 ) ;
#142057 = DIRECTION ( 'NONE',  ( 0.000000000000000000, 0.000000000000000000, -1.000000000000000000 ) ) ;
#142058 = DIRECTION ( 'NONE',  ( -0.7071067811865474617, -0.7071067811865474617, -0.000000000000000000 ) ) ;
#142059 = FACE_BOUND ( 'NONE', #242564, .T. ) ;
#142060 = VERTEX_POINT ( 'NONE', #198957 ) ;
#142061 = ORIENTED_EDGE ( 'NONE', *, *, #108751, .T. ) ;
#142062 = CARTESIAN_POINT ( 'NONE',  ( -12.92414019175886075, 9.417632963106292721, -18.14894846573227127 ) ) ;
#142063 = ORIENTED_EDGE ( 'NONE', *, *, #52596, .T. ) ;
#142064 = CARTESIAN_POINT ( 'NONE',  ( -21.65000000000000213, 7.708578643773852157, -88.25000000000005684 ) ) ;
#142065 = AXIS2_PLACEMENT_3D ( 'NONE', #105373, #8886, #209651 ) ;
#142066 = VECTOR ( 'NONE', #176907, 1000.000000000000000 ) ;
#142067 = DIRECTION ( 'NONE',  ( 0.000000000000000000, 0.000000000000000000, 1.000000000000000000 ) ) ;
#142068 = AXIS2_PLACEMENT_3D ( 'NONE', #8188, #147691, #128130 ) ;
#142069 = ADVANCED_FACE ( 'NONE', ( #76439 ), #244355, .T. ) ;
#142070 = EDGE_CURVE ( 'NONE', #23626, #145505, #81755, .T. ) ;
#142071 = EDGE_LOOP ( 'NONE', ( #141756, #212479, #98513, #230517 ) ) ;
#142072 = DIRECTION ( 'NONE',  ( 0.000000000000000000, 0.000000000000000000, 1.000000000000000000 ) ) ;
#142073 = ORIENTED_EDGE ( 'NONE', *, *, #152137, .F. ) ;
#142074 = EDGE_CURVE ( 'NONE', #253445, #103813, #136387, .T. ) ;
#142076 = ADVANCED_FACE ( 'NONE', ( #133853 ), #16497, .T. ) ;
#142075 = DIRECTION ( 'NONE',  ( -1.000000000000000000, -0.000000000000000000, -0.000000000000000000 ) ) ;
#142077 = DIRECTION ( 'NONE',  ( -0.7071067811865474617, -0.3338907855510734324, -0.6233112732207618523 ) ) ;
#142078 = DIRECTION ( 'NONE',  ( 0.000000000000000000, 0.9126074666063770380, 0.4088369013363278848 ) ) ;
#142079 = CARTESIAN_POINT ( 'NONE',  ( -20.54999999999999716, 23.68770167995059595, -252.8127582590406348 ) ) ;
#142080 = CARTESIAN_POINT ( 'NONE',  ( -18.59999999999999787, -1.835859311432481045, -145.6044391687985637 ) ) ;
#142082 = CARTESIAN_POINT ( 'NONE',  ( 21.14999999999999858, 69.45000000001229523, -157.6731074845243938 ) ) ;
#142081 = FACE_OUTER_BOUND ( 'NONE', #128471, .T. ) ;
#142083 = AXIS2_PLACEMENT_3D ( 'NONE', #13263, #204576, #25959 ) ;
#142084 = EDGE_CURVE ( 'NONE', #29706, #8700, #38616, .T. ) ;
#142085 = CARTESIAN_POINT ( 'NONE',  ( 21.15000000000005542, 77.16254490893143725, -43.92310748452479885 ) ) ;
#142087 = ORIENTED_EDGE ( 'NONE', *, *, #228610, .F. ) ;
#142086 = CARTESIAN_POINT ( 'NONE',  ( 20.77766267348356166, 65.55095760939339300, -128.9303985686466945 ) ) ;
#142089 = DIRECTION ( 'NONE',  ( -0.000000000000000000, 0.6132151058540549204, -0.7899159663865520375 ) ) ;
#142088 = CYLINDRICAL_SURFACE ( 'NONE', #190944, 0.09999999999999939493 ) ;
#142090 = ORIENTED_EDGE ( 'NONE', *, *, #95234, .T. ) ;
#142092 = ORIENTED_EDGE ( 'NONE', *, *, #111236, .T. ) ;
#142091 = DIRECTION ( 'NONE',  ( 0.000000000000000000, 1.000000000000000000, 0.000000000000000000 ) ) ;
#142093 = EDGE_CURVE ( 'NONE', #143626, #101654, #157231, .T. ) ;
#142094 = EDGE_LOOP ( 'NONE', ( #53451, #169804, #226807, #114072 ) ) ;
#142095 = DIRECTION ( 'NONE',  ( 0.000000000000000000, 0.2128009952263485993, -0.9770955615653341697 ) ) ;
#142097 = EDGE_CURVE ( 'NONE', #116117, #12050, #158582, .T. ) ;
#142096 = EDGE_CURVE ( 'NONE', #127734, #255180, #56816, .T. ) ;
#142098 = CARTESIAN_POINT ( 'NONE',  ( -22.42357213249529124, 29.61603862786154906, -252.5977130990568753 ) ) ;
#142099 = DIRECTION ( 'NONE',  ( -0.000000000000000000, 0.000000000000000000, 1.000000000000000000 ) ) ;
#142100 = EDGE_LOOP ( 'NONE', ( #71380, #251555, #229294, #17631 ) ) ;
#142101 = DIRECTION ( 'NONE',  ( -0.8660254037844500319, 0.000000000000000000, 0.4999999999999800715 ) ) ;
#142102 = DIRECTION ( 'NONE',  ( 0.000000000000000000, 0.000000000000000000, -1.000000000000000000 ) ) ;
#142104 = EDGE_CURVE ( 'NONE', #121663, #156856, #252503, .T. ) ;
#142103 = CARTESIAN_POINT ( 'NONE',  ( -18.59999999999999787, 1.736257131597397585, -11.56865232901749962 ) ) ;
#142105 = ORIENTED_EDGE ( 'NONE', *, *, #230502, .T. ) ;
#142106 = CARTESIAN_POINT ( 'NONE',  ( 23.24999999999999645, 1.115600667400684642E-11, -200.9999999999999432 ) ) ;
#142107 = EDGE_CURVE ( 'NONE', #215608, #103081, #213382, .T. ) ;
#142108 = CIRCLE ( 'NONE', #192197, 11.75000000000000000 ) ;
#142109 = AXIS2_PLACEMENT_3D ( 'NONE', #199171, #197877, #38826 ) ;
#142110 = CARTESIAN_POINT ( 'NONE',  ( 21.10320863425824811, 69.59972261355297007, -136.5481297357514734 ) ) ;
#142111 = VERTEX_POINT ( 'NONE', #201528 ) ;
#142112 = ORIENTED_EDGE ( 'NONE', *, *, #193185, .F. ) ;
#142113 = DIRECTION ( 'NONE',  ( 2.952720810173289112E-16, -1.000000000000000000, -0.000000000000000000 ) ) ;
#142114 = EDGE_CURVE ( 'NONE', #19112, #56619, #244278, .T. ) ;
#142115 = EDGE_CURVE ( 'NONE', #76792, #201406, #60719, .T. ) ;
#142116 = ORIENTED_EDGE ( 'NONE', *, *, #47162, .F. ) ;
#142117 = DIRECTION ( 'NONE',  ( 0.000000000000000000, -0.8814952561688430555, 0.4721928772777346239 ) ) ;
#142118 = ORIENTED_EDGE ( 'NONE', *, *, #71201, .F. ) ;
#142119 = CARTESIAN_POINT ( 'NONE',  ( 20.92356734117541706, 10.31973158071402175, -173.0505334713354841 ) ) ;
#142120 = ADVANCED_FACE ( 'NONE', ( #2028 ), #120744, .T. ) ;
#142121 = FACE_OUTER_BOUND ( 'NONE', #54673, .T. ) ;
#142122 = CYLINDRICAL_SURFACE ( 'NONE', #109641, 0.1000000000000028644 ) ;
#142123 = CARTESIAN_POINT ( 'NONE',  ( 20.85000000000000142, 64.35000000001146248, -42.80697314750249660 ) ) ;
#142124 = DIRECTION ( 'NONE',  ( 1.000000000000000000, 0.000000000000000000, 0.000000000000000000 ) ) ;
#142125 = EDGE_LOOP ( 'NONE', ( #89044, #115160, #29775, #231345, #6435, #227904, #119004, #4244, #152178 ) ) ;
#142126 = EDGE_CURVE ( 'NONE', #149588, #121114, #159860, .T. ) ;
#142127 = CIRCLE ( 'NONE', #34029, 11.70000000000000284 ) ;
#142128 = CARTESIAN_POINT ( 'NONE',  ( -22.57320508075687115, 12.62988036037873307, -223.4632815780722694 ) ) ;
#142129 = EDGE_CURVE ( 'NONE', #83659, #229015, #42211, .T. ) ;
#142130 = DIRECTION ( 'NONE',  ( 1.000000000000000000, 0.000000000000000000, 0.000000000000000000 ) ) ;
#142131 = CARTESIAN_POINT ( 'NONE',  ( -21.07928932188134041, 0.09889514566555068775, -27.17148334360670958 ) ) ;
#142132 = DIRECTION ( 'NONE',  ( -1.000000000000000000, 0.000000000000000000, 0.000000000000000000 ) ) ;
#142133 = ORIENTED_EDGE ( 'NONE', *, *, #32326, .T. ) ;
#142135 = DIRECTION ( 'NONE',  ( 2.659396599871503635E-15, 0.6132151058540549204, -0.7899159663865520375 ) ) ;
#142134 = DIRECTION ( 'NONE',  ( 1.000000000000000000, -0.000000000000000000, -0.000000000000000000 ) ) ;
#142136 = ORIENTED_EDGE ( 'NONE', *, *, #120818, .T. ) ;
#142139 = ORIENTED_EDGE ( 'NONE', *, *, #79730, .T. ) ;
#142138 = DIRECTION ( 'NONE',  ( 1.000000000000000000, 0.000000000000000000, 0.000000000000000000 ) ) ;
#142137 = DIRECTION ( 'NONE',  ( 0.000000000000000000, -0.6728971962617102953, -0.7397360091702507301 ) ) ;
#142140 = VERTEX_POINT ( 'NONE', #107245 ) ;
#142141 = DIRECTION ( 'NONE',  ( 0.000000000000000000, 0.000000000000000000, -1.000000000000000000 ) ) ;
#142142 = DIRECTION ( 'NONE',  ( 1.000000000000000000, -0.000000000000000000, -0.000000000000000000 ) ) ;
#142143 = CYLINDRICAL_SURFACE ( 'NONE', #195916, 4.049999999999998934 ) ;
#142144 = VERTEX_POINT ( 'NONE', #24200 ) ;
#142145 = CARTESIAN_POINT ( 'NONE',  ( 19.75857864376269291, 16.74769748025657279, -222.6827034548337849 ) ) ;
#142146 = ADVANCED_FACE ( 'NONE', ( #228498 ), #9427, .T. ) ;
#142147 = AXIS2_PLACEMENT_3D ( 'NONE', #152359, #228015, #110631 ) ;
#142148 = CARTESIAN_POINT ( 'NONE',  ( 21.05000000000000071, 47.92640890138473253, -246.4059919526569900 ) ) ;
#142150 = DIRECTION ( 'NONE',  ( 0.000000000000000000, 0.000000000000000000, 1.000000000000000000 ) ) ;
#142149 = CYLINDRICAL_SURFACE ( 'NONE', #51684, 1.749999999999998002 ) ;
#142152 = ORIENTED_EDGE ( 'NONE', *, *, #20603, .F. ) ;
#142151 = CARTESIAN_POINT ( 'NONE',  ( -20.54999999999999716, 54.18213181965657554, -236.9344197582443883 ) ) ;
#142153 = VECTOR ( 'NONE', #134637, 1000.000000000000000 ) ;
#142154 = ORIENTED_EDGE ( 'NONE', *, *, #251868, .T. ) ;
#142155 = VECTOR ( 'NONE', #73871, 1000.000000000000114 ) ;
#142156 = FACE_BOUND ( 'NONE', #248084, .T. ) ;
#142157 = CARTESIAN_POINT ( 'NONE',  ( -20.54999999999999716, 81.80425911359037627, -227.0113082700774783 ) ) ;
#142158 = CARTESIAN_POINT ( 'NONE',  ( -18.59999999999999787, 64.25000000001142553, -36.02310748452440237 ) ) ;
#142160 = ORIENTED_EDGE ( 'NONE', *, *, #111144, .T. ) ;
#142159 = AXIS2_PLACEMENT_3D ( 'NONE', #222140, #119233, #59201 ) ;
#142161 = FACE_OUTER_BOUND ( 'NONE', #72656, .T. ) ;
#142162 = EDGE_LOOP ( 'NONE', ( #78317, #35713 ) ) ;
#142163 = B_SPLINE_CURVE_WITH_KNOTS ( 'NONE', 3,
 ( #124173, #184117, #141161, #203698 ),
 .UNSPECIFIED., .F., .F.,
 ( 4, 4 ),
 ( 0.000000000000000000, 0.001767853679387123601 ),
 .UNSPECIFIED. ) ;
#142164 = DIRECTION ( 'NONE',  ( 0.000000000000000000, -6.982962677686266711E-15, 1.000000000000000000 ) ) ;
#142165 = AXIS2_PLACEMENT_3D ( 'NONE', #149747, #12805, #148452 ) ;
#142166 = CARTESIAN_POINT ( 'NONE',  ( -21.44999999999999929, 7.350000000011155166, -179.8499999999999943 ) ) ;
#142167 = LINE ( 'NONE', #200862, #97509 ) ;
#142168 = ORIENTED_EDGE ( 'NONE', *, *, #30027, .T. ) ;
#142169 = DIRECTION ( 'NONE',  ( -1.000000000000000000, 0.000000000000000000, 0.000000000000000000 ) ) ;
#142170 = AXIS2_PLACEMENT_3D ( 'NONE', #149028, #12092, #10785 ) ;
#142171 = EDGE_CURVE ( 'NONE', #131694, #173897, #49839, .T. ) ;
#142172 = VECTOR ( 'NONE', #160421, 1000.000000000000000 ) ;
#142174 = EDGE_CURVE ( 'NONE', #112086, #56194, #240659, .T. ) ;
#142173 = CARTESIAN_POINT ( 'NONE',  ( -22.39999999999999858, 10.71943444926882449, -226.8179467668883547 ) ) ;
#142175 = VECTOR ( 'NONE', #43043, 1000.000000000000000 ) ;
#142176 = EDGE_LOOP ( 'NONE', ( #242893, #10666, #63252, #226961, #112066, #36294, #225575 ) ) ;
#142177 = ORIENTED_EDGE ( 'NONE', *, *, #136614, .T. ) ;
#142178 = AXIS2_PLACEMENT_3D ( 'NONE', #229782, #51114, #152851 ) ;
#142179 = VERTEX_POINT ( 'NONE', #200252 ) ;
#142180 = ADVANCED_FACE ( 'NONE', ( #101096 ), #226054, .T. ) ;
#142181 = DIRECTION ( 'NONE',  ( 0.000000000000000000, 0.2617529984165174461, 0.9651348961777118651 ) ) ;
#142182 = VERTEX_POINT ( 'NONE', #222347 ) ;
#142185 = EDGE_CURVE ( 'NONE', #4326, #15539, #43746, .T. ) ;
#142184 = EDGE_LOOP ( 'NONE', ( #80820, #25111, #93793 ) ) ;
#142183 = CARTESIAN_POINT ( 'NONE',  ( 13.22461703343584816, 66.56333706821347107, -185.2000707522295215 ) ) ;
#142186 = AXIS2_PLACEMENT_3D ( 'NONE', #85322, #104872, #207899 ) ;
#142187 = ORIENTED_EDGE ( 'NONE', *, *, #82678, .F. ) ;
#142188 = ADVANCED_FACE ( 'NONE', ( #246748 ), #219152, .T. ) ;
#142191 = ORIENTED_EDGE ( 'NONE', *, *, #124960, .T. ) ;
#142190 = EDGE_LOOP ( 'NONE', ( #231586, #217775, #172765, #215308 ) ) ;
#142189 = CARTESIAN_POINT ( 'NONE',  ( -16.81744102076749314, 9.950000000011142376, -113.1500000000000341 ) ) ;
#142192 = ORIENTED_EDGE ( 'NONE', *, *, #128452, .T. ) ;
#142193 = DIRECTION ( 'NONE',  ( -1.000000000000000000, 0.000000000000000000, 0.000000000000000000 ) ) ;
#142194 = VECTOR ( 'NONE', #41713, 1000.000000000000000 ) ;
#142195 = CIRCLE ( 'NONE', #233801, 0.1000000000000124678 ) ;
#142196 = AXIS2_PLACEMENT_3D ( 'NONE', #2507, #22106, #44231 ) ;
#142197 = CIRCLE ( 'NONE', #183895, 0.09999999999998898659 ) ;
#142198 = ADVANCED_FACE ( 'NONE', ( #188077 ), #148965, .F. ) ;
#142199 = CARTESIAN_POINT ( 'NONE',  ( -16.87683809663752754, 13.99889777621145903, -218.5199410132753428 ) ) ;
#142200 = EDGE_LOOP ( 'NONE', ( #128406, #133799, #184136, #213477 ) ) ;
#142201 = DIRECTION ( 'NONE',  ( 2.952720810173289112E-16, 1.000000000000000000, 9.912705577010238578E-15 ) ) ;
#142203 = ORIENTED_EDGE ( 'NONE', *, *, #166224, .F. ) ;
#142202 = DIRECTION ( 'NONE',  ( 1.000000000000000000, 0.000000000000000000, 0.000000000000000000 ) ) ;
#142204 = DIRECTION ( 'NONE',  ( 0.000000000000000000, -6.982962677686266711E-15, 1.000000000000000000 ) ) ;
#142206 = ORIENTED_EDGE ( 'NONE', *, *, #54345, .T. ) ;
#142205 = LINE ( 'NONE', #183904, #131593 ) ;
#142207 = ORIENTED_EDGE ( 'NONE', *, *, #149482, .T. ) ;
#142208 = LINE ( 'NONE', #221720, #182449 ) ;
#142209 = ORIENTED_EDGE ( 'NONE', *, *, #11778, .T. ) ;
#142210 = ORIENTED_EDGE ( 'NONE', *, *, #173329, .T. ) ;
#142211 = CARTESIAN_POINT ( 'NONE',  ( -16.87683809663750978, 9.950000000011137047, -180.9023640181964652 ) ) ;
#142212 = CARTESIAN_POINT ( 'NONE',  ( -21.05000000000000071, -0.01465611850164896118, -161.0033134142318261 ) ) ;
#142213 = EDGE_CURVE ( 'NONE', #147420, #190547, #202600, .T. ) ;
#142215 = EDGE_LOOP ( 'NONE', ( #182517, #94773, #118318 ) ) ;
#142214 = ORIENTED_EDGE ( 'NONE', *, *, #220100, .T. ) ;
#142216 = VERTEX_POINT ( 'NONE', #134494 ) ;
#142217 = DIRECTION ( 'NONE',  ( -1.000000000000000000, -0.000000000000000000, -0.000000000000000000 ) ) ;
#142218 = ORIENTED_EDGE ( 'NONE', *, *, #171295, .F. ) ;
#142219 = ORIENTED_EDGE ( 'NONE', *, *, #45261, .T. ) ;
#142220 = LINE ( 'NONE', #159243, #96878 ) ;
#142222 = ORIENTED_EDGE ( 'NONE', *, *, #246706, .F. ) ;
#142221 = LINE ( 'NONE', #17458, #10004 ) ;
#142223 = CARTESIAN_POINT ( 'NONE',  ( 23.40000000000005542, 78.05591623545335267, -49.16694968567509250 ) ) ;
#142225 = CARTESIAN_POINT ( 'NONE',  ( 20.85000000000000142, -11.74999999999999112, -30.50000000000000000 ) ) ;
#142224 = FACE_OUTER_BOUND ( 'NONE', #144537, .T. ) ;
#142226 = ADVANCED_FACE ( 'NONE', ( #111101 ), #211490, .T. ) ;
#142227 = CIRCLE ( 'NONE', #8955, 0.09999999999999971412 ) ;
#142228 = VERTEX_POINT ( 'NONE', #171126 ) ;
#142229 = ADVANCED_FACE ( 'NONE', ( #232356 ), #14595, .T. ) ;
#142231 = ORIENTED_EDGE ( 'NONE', *, *, #145450, .F. ) ;
#142230 = ORIENTED_EDGE ( 'NONE', *, *, #191196, .T. ) ;
#142232 = DIRECTION ( 'NONE',  ( 0.000000000000000000, 0.000000000000000000, 1.000000000000000000 ) ) ;
#142233 = DIRECTION ( 'NONE',  ( 0.000000000000000000, -7.086529944415894657E-15, 1.000000000000000000 ) ) ;
#142234 = ORIENTED_EDGE ( 'NONE', *, *, #89081, .F. ) ;
#142235 = ADVANCED_FACE ( 'NONE', ( #190666 ), #252468, .T. ) ;
#142236 = AXIS2_PLACEMENT_3D ( 'NONE', #200039, #42252, #137469 ) ;
#142237 = CARTESIAN_POINT ( 'NONE',  ( -18.50000000000000000, 85.40000000001191438, -95.72584772486095517 ) ) ;
#142238 = EDGE_LOOP ( 'NONE', ( #163473, #165616, #208814, #19740 ) ) ;
#142239 = ORIENTED_EDGE ( 'NONE', *, *, #47224, .F. ) ;
#142240 = LINE ( 'NONE', #39321, #12924 ) ;
#142242 = EDGE_CURVE ( 'NONE', #82189, #18420, #92809, .T. ) ;
#142241 = VERTEX_POINT ( 'NONE', #208916 ) ;
#142243 = DIRECTION ( 'NONE',  ( 0.000000000000000000, 1.000000000000000000, 0.000000000000000000 ) ) ;
#142244 = CARTESIAN_POINT ( 'NONE',  ( 20.94999999999999929, 76.00000000001267608, -203.5231074845243597 ) ) ;
#142245 = ORIENTED_EDGE ( 'NONE', *, *, #205164, .F. ) ;
#142246 = EDGE_CURVE ( 'NONE', #208340, #205048, #169332, .T. ) ;
#142247 = DIRECTION ( 'NONE',  ( 0.000000000000000000, 1.734723475976997999E-14, 1.000000000000000000 ) ) ;
#142248 = DIRECTION ( 'NONE',  ( -1.000000000000000000, 0.000000000000000000, 0.000000000000000000 ) ) ;
#142250 = PLANE ( 'NONE',  #3938 ) ;
#142249 = LINE ( 'NONE', #144803, #11393 ) ;
#142251 = DIRECTION ( 'NONE',  ( -1.000000000000000000, -0.000000000000000000, -0.000000000000000000 ) ) ;
#142252 = DIRECTION ( 'NONE',  ( 0.000000000000000000, -8.673617379884087537E-15, -1.000000000000000000 ) ) ;
#142253 = CARTESIAN_POINT ( 'NONE',  ( -18.50000000000000000, 66.75000000001223555, -148.7731074845244166 ) ) ;
#142255 = EDGE_CURVE ( 'NONE', #105545, #51843, #144302, .T. ) ;
#142254 = CARTESIAN_POINT ( 'NONE',  ( -20.15000000000000568, 9.291421356237307805, -12.34999999999999964 ) ) ;
#142256 = DIRECTION ( 'NONE',  ( 0.000000000000000000, 0.000000000000000000, 1.000000000000000000 ) ) ;
#142257 = VECTOR ( 'NONE', #71135, 1000.000000000000000 ) ;
#142258 = ORIENTED_EDGE ( 'NONE', *, *, #221862, .F. ) ;
#142259 = AXIS2_PLACEMENT_3D ( 'NONE', #39028, #255437, #76845 ) ;
#142260 = VECTOR ( 'NONE', #174823, 1000.000000000000000 ) ;
#142262 = EDGE_LOOP ( 'NONE', ( #81383, #122230, #189936, #200922 ) ) ;
#142261 = VERTEX_POINT ( 'NONE', #251887 ) ;
#142263 = ORIENTED_EDGE ( 'NONE', *, *, #149257, .T. ) ;
#142265 = EDGE_CURVE ( 'NONE', #213669, #221570, #39542, .T. ) ;
#142264 = DIRECTION ( 'NONE',  ( 0.000000000000000000, 0.000000000000000000, -1.000000000000000000 ) ) ;
#142266 =( BOUNDED_SURFACE ( )  B_SPLINE_SURFACE ( 3, 2, ( 
 ( #185565, #139996, #219540 ),
 ( #100843, #104702, #224677 ),
 ( #4343, #180434, #202560 ),
 ( #203836, #241687, #21383 ) ),
 .UNSPECIFIED., .F., .F., .F. ) 
 B_SPLINE_SURFACE_WITH_KNOTS ( ( 4, 4 ),
 ( 3, 3 ),
 ( 0.0002700421466196669426, 0.0004789321604330889072 ),
 ( 0.000000000000000000, 1.000000000000000000 ),
 .UNSPECIFIED. ) 
 GEOMETRIC_REPRESENTATION_ITEM ( )  RATIONAL_B_SPLINE_SURFACE ( (
 ( 1.000000000000000000, 0.7071067811865475727, 1.000000000000000000),
 ( 1.000000000000000000, 0.7163411249511604240, 1.000000000000000000),
 ( 1.000000000000000000, 0.7221957104842396946, 1.000000000000000000),
 ( 1.000000000000000000, 0.7250110520819882387, 1.000000000000000000) ) ) 
 REPRESENTATION_ITEM ( '' )  SURFACE ( )  );
#142267 = DIRECTION ( 'NONE',  ( 0.000000000000000000, 0.000000000000000000, 1.000000000000000000 ) ) ;
#142269 = CARTESIAN_POINT ( 'NONE',  ( -12.25000000000000178, 9.349999999999983658, -16.75000000000000000 ) ) ;
#142268 = DIRECTION ( 'NONE',  ( 0.000000000000000000, 0.000000000000000000, -1.000000000000000000 ) ) ;
#142270 = DIRECTION ( 'NONE',  ( 2.952720810173288619E-16, -1.000000000000000000, 0.000000000000000000 ) ) ;
#142271 = VERTEX_POINT ( 'NONE', #70722 ) ;
#142272 = CARTESIAN_POINT ( 'NONE',  ( -20.94999999999999929, 10.29270135741298731, -105.9573618871519756 ) ) ;
#142273 = DIRECTION ( 'NONE',  ( 1.000000000000000000, 0.000000000000000000, 0.000000000000000000 ) ) ;
#142275 = VECTOR ( 'NONE', #244992, 1000.000000000000227 ) ;
#142274 = DIRECTION ( 'NONE',  ( -0.000000000000000000, 1.000000000000000000, 1.734723475976807292E-15 ) ) ;
#142276 = CARTESIAN_POINT ( 'NONE',  ( -21.05000000000000071, 77.83534155023627932, -91.46795619196132066 ) ) ;
#142278 = ORIENTED_EDGE ( 'NONE', *, *, #214573, .F. ) ;
#142277 = B_SPLINE_CURVE_WITH_KNOTS ( 'NONE', 3,
 ( #90721, #170323, #145563, #209394, #28228, #7345, #249815, #50304, #166458, #150712 ),
 .UNSPECIFIED., .F., .F.,
 ( 4, 3, 3, 4 ),
 ( 0.000000000000000000, 0.0002000000000002884074, 0.001000000000045112589, 0.001967863649472103085 ),
 .UNSPECIFIED. ) ;
#142279 = B_SPLINE_CURVE_WITH_KNOTS ( 'NONE', 3,
 ( #217481, #38884, #75457, #118416, #154990, #197926, #214934, #36321 ),
 .UNSPECIFIED., .F., .F.,
 ( 4, 2, 2, 4 ),
 ( 0.000000000000000000, 0.0002181133598169334407, 0.0003271700397253676351, 0.0004362267196338018836 ),
 .UNSPECIFIED. ) ;
#142280 = CARTESIAN_POINT ( 'NONE',  ( -21.05000000000000071, 64.35000000001161879, -62.73924182154625129 ) ) ;
#142281 = CARTESIAN_POINT ( 'NONE',  ( -21.05000000000000071, 87.65000000001215597, -139.4231074845242802 ) ) ;
#142282 = ORIENTED_EDGE ( 'NONE', *, *, #21343, .T. ) ;
#142283 = CARTESIAN_POINT ( 'NONE',  ( -16.88219499860498374, 66.04979357458398681, -56.87379779441709360 ) ) ;
#142284 = FACE_OUTER_BOUND ( 'NONE', #250394, .T. ) ;
#142285 = FACE_OUTER_BOUND ( 'NONE', #15190, .T. ) ;
#142286 = DIRECTION ( 'NONE',  ( 0.000000000000000000, 1.000000000000000000, 0.000000000000000000 ) ) ;
#142287 = FACE_OUTER_BOUND ( 'NONE', #220854, .T. ) ;
#142288 = ORIENTED_EDGE ( 'NONE', *, *, #154278, .F. ) ;
#142289 = CARTESIAN_POINT ( 'NONE',  ( 22.10000000000000497, -11.65000000000000036, 32.89999999999999858 ) ) ;
#142290 = FACE_OUTER_BOUND ( 'NONE', #239274, .T. ) ;
#142291 = CARTESIAN_POINT ( 'NONE',  ( 21.05000000000000071, 12.09419181799517062, -206.1384361755945918 ) ) ;
#142294 = FACE_OUTER_BOUND ( 'NONE', #118911, .T. ) ;
#142293 = AXIS2_PLACEMENT_3D ( 'NONE', #218096, #39519, #100698 ) ;
#142292 = DIRECTION ( 'NONE',  ( 0.000000000000000000, 0.000000000000000000, 1.000000000000000000 ) ) ;
#142296 = CYLINDRICAL_SURFACE ( 'NONE', #170609, 0.8750000000000007772 ) ;
#142295 = CIRCLE ( 'NONE', #63175, 0.1000000000000028644 ) ;
#142297 = CARTESIAN_POINT ( 'NONE',  ( 20.94999999999999929, 7.675662554762638479, -241.7139905447625381 ) ) ;
#142298 = CYLINDRICAL_SURFACE ( 'NONE', #19124, 0.09999999999999939493 ) ;
#142300 = ORIENTED_EDGE ( 'NONE', *, *, #255720, .F. ) ;
#142299 = CARTESIAN_POINT ( 'NONE',  ( 18.49999999999999289, 11.65000000001115943, -125.3500000000000512 ) ) ;
#142301 = ORIENTED_EDGE ( 'NONE', *, *, #58861, .F. ) ;
#142302 = ADVANCED_FACE ( 'NONE', ( #233629 ), #34170, .T. ) ;
#142303 = CIRCLE ( 'NONE', #184004, 4.049999999999998934 ) ;
#142304 = CARTESIAN_POINT ( 'NONE',  ( 22.32929514600007792, 7.578647565387638174, -100.4009243218861229 ) ) ;
#142305 = EDGE_CURVE ( 'NONE', #94754, #38206, #150249, .T. ) ;
#142306 = EDGE_CURVE ( 'NONE', #22873, #92979, #253168, .T. ) ;
#142307 = CARTESIAN_POINT ( 'NONE',  ( 18.59999999999999787, 84.16003609933891028, -218.3250942044780345 ) ) ;
#142308 = DIRECTION ( 'NONE',  ( 0.000000000000000000, 0.000000000000000000, 1.000000000000000000 ) ) ;
#142309 = ORIENTED_EDGE ( 'NONE', *, *, #226884, .F. ) ;
#142310 = DIRECTION ( 'NONE',  ( -1.000000000000000000, 0.000000000000000000, 0.000000000000000000 ) ) ;
#142311 = DIRECTION ( 'NONE',  ( 0.000000000000000000, 0.000000000000000000, 1.000000000000000000 ) ) ;
#142312 = CARTESIAN_POINT ( 'NONE',  ( -21.07094088545368749, 75.90110629745977633, -109.3432747064414343 ) ) ;
#142313 = VERTEX_POINT ( 'NONE', #214053 ) ;
#142314 = DIRECTION ( 'NONE',  ( 0.000000000000000000, 0.000000000000000000, 1.000000000000000000 ) ) ;
#142316 = ORIENTED_EDGE ( 'NONE', *, *, #205291, .T. ) ;
#142315 = CARTESIAN_POINT ( 'NONE',  ( -18.59999999999999787, 9.250000000000001776, -21.15000000000000213 ) ) ;
#142318 = CARTESIAN_POINT ( 'NONE',  ( 21.05000000000000071, 59.13236860818124541, -225.8959333647716505 ) ) ;
#142317 = CARTESIAN_POINT ( 'NONE',  ( -20.54999999999999716, 7.128833340093095217, -233.7327013124392749 ) ) ;
#142319 = EDGE_CURVE ( 'NONE', #38262, #75744, #40135, .T. ) ;
#142321 = CARTESIAN_POINT ( 'NONE',  ( 20.72390388899090041, 65.41003688158824048, -162.5117591887780577 ) ) ;
#142320 = AXIS2_PLACEMENT_3D ( 'NONE', #88474, #28101, #106298 ) ;
#142322 = DIRECTION ( 'NONE',  ( 1.000000000000000000, -0.000000000000000000, 0.000000000000000000 ) ) ;
#142323 = ORIENTED_EDGE ( 'NONE', *, *, #137904, .F. ) ;
#142324 = CIRCLE ( 'NONE', #208969, 6.329289321881370611 ) ;
#142325 = DIRECTION ( 'NONE',  ( 0.000000000000000000, 0.000000000000000000, 1.000000000000000000 ) ) ;
#142326 = FACE_OUTER_BOUND ( 'NONE', #186926, .T. ) ;
#142327 = CARTESIAN_POINT ( 'NONE',  ( 20.95263205890728386, 67.10425989211800868, -128.0335990775827781 ) ) ;
#142328 = ORIENTED_EDGE ( 'NONE', *, *, #72592, .T. ) ;
#142329 = VECTOR ( 'NONE', #232182, 1000.000000000000000 ) ;
#142330 = LINE ( 'NONE', #41979, #208430 ) ;
#142331 = DIRECTION ( 'NONE',  ( 0.000000000000000000, 0.000000000000000000, 1.000000000000000000 ) ) ;
#142332 = CIRCLE ( 'NONE', #175683, 4.099999999999996980 ) ;
#142334 = DIRECTION ( 'NONE',  ( -1.000000000000000000, 0.000000000000000000, 0.000000000000000000 ) ) ;
#142333 = VECTOR ( 'NONE', #3469, 1000.000000000000000 ) ;
#142335 = CARTESIAN_POINT ( 'NONE',  ( -23.25000000000000000, 76.00000000001213607, -136.5231074845243313 ) ) ;
#142336 = ADVANCED_FACE ( 'NONE', ( #114953 ), #173444, .T. ) ;
#142337 = ORIENTED_EDGE ( 'NONE', *, *, #243428, .T. ) ;
#142338 = EDGE_CURVE ( 'NONE', #30032, #231849, #206698, .T. ) ;
#142339 = ORIENTED_EDGE ( 'NONE', *, *, #56374, .F. ) ;
#142341 = CIRCLE ( 'NONE', #46657, 0.4999999999999995004 ) ;
#142340 = CARTESIAN_POINT ( 'NONE',  ( 22.40000000000010516, 76.00000000001267608, -81.17267829206943475 ) ) ;
#142343 = CIRCLE ( 'NONE', #29958, 0.09999999999999939493 ) ;
#142342 = CARTESIAN_POINT ( 'NONE',  ( -18.59999999999999787, 69.01799029515524353, -65.82695536626808064 ) ) ;
#142344 = DIRECTION ( 'NONE',  ( 0.000000000000000000, 0.000000000000000000, -1.000000000000000000 ) ) ;
#142345 = DIRECTION ( 'NONE',  ( -0.000000000000000000, 1.000000000000000000, 0.000000000000000000 ) ) ;
#142346 = CARTESIAN_POINT ( 'NONE',  ( -18.58671080940901277, -9.406932858815459042, -141.1241544649047910 ) ) ;
#142347 = EDGE_CURVE ( 'NONE', #241890, #183380, #11063, .T. ) ;
#142349 =( NAMED_UNIT ( * ) PLANE_ANGLE_UNIT ( ) SI_UNIT ( $, .RADIAN. ) );
#142348 = CARTESIAN_POINT ( 'NONE',  ( -16.87372386987899020, 12.45246834913251455, -211.7454916664752886 ) ) ;
#142350 = VECTOR ( 'NONE', #165209, 1000.000000000000227 ) ;
#142351 = FACE_OUTER_BOUND ( 'NONE', #25938, .T. ) ;
#142352 = DIRECTION ( 'NONE',  ( -1.000000000000000000, -0.000000000000000000, -0.000000000000000000 ) ) ;
#142354 = CARTESIAN_POINT ( 'NONE',  ( 18.42636655943171320, -9.496944315759472843, -107.1090805711555731 ) ) ;
#142353 = TOROIDAL_SURFACE ( 'NONE', #13381, 4.099999999999999645, 0.1000000000000000056 ) ;
#142355 = ORIENTED_EDGE ( 'NONE', *, *, #49651, .T. ) ;
#142356 = CARTESIAN_POINT ( 'NONE',  ( -18.59999999999999787, 74.16465844978765176, -124.8679561919613263 ) ) ;
#142358 = ORIENTED_EDGE ( 'NONE', *, *, #150001, .F. ) ;
#142357 = CARTESIAN_POINT ( 'NONE',  ( 13.22461703343583572, 62.91973165888628472, -215.7008495347501480 ) ) ;
#142359 = CARTESIAN_POINT ( 'NONE',  ( -21.05000000000000071, 64.36312671090797721, -129.7013482711997199 ) ) ;
#142360 = CARTESIAN_POINT ( 'NONE',  ( 20.94999999999999929, -9.499999999988848032, -43.39396912265245021 ) ) ;
#142362 = DIRECTION ( 'NONE',  ( 0.000000000000000000, 0.000000000000000000, -1.000000000000000000 ) ) ;
#142361 = CARTESIAN_POINT ( 'NONE',  ( 22.47071067811864964, 75.90090754530939421, -110.7431822290223522 ) ) ;
#142364 =( BOUNDED_SURFACE ( )  B_SPLINE_SURFACE ( 3, 2, ( 
 ( #143039, #83045, #66089 ),
 ( #68668, #88189, #188598 ),
 ( #45245, #247281, #126046 ),
 ( #166506, #167790, #204301 ) ),
 .UNSPECIFIED., .F., .F., .T. ) 
 B_SPLINE_SURFACE_WITH_KNOTS ( ( 4, 4 ),
 ( 3, 3 ),
 ( 0.04058434257139457990, 0.04256401539001584966 ),
 ( 0.000000000000000000, 1.000000000000000000 ),
 .UNSPECIFIED. ) 
 GEOMETRIC_REPRESENTATION_ITEM ( )  RATIONAL_B_SPLINE_SURFACE ( (
 ( 1.000000000000000000, 0.7103081912007894738, 1.000000000000000000),
 ( 1.000000000000000000, 0.7104998333556562518, 1.000000000000000000),
 ( 1.000000000000000000, 0.7107238315754180746, 1.000000000000000000),
 ( 1.000000000000000000, 0.7110073749539692622, 1.000000000000000000) ) ) 
 REPRESENTATION_ITEM ( '' )  SURFACE ( )  );
#142363 = AXIS2_PLACEMENT_3D ( 'NONE', #94112, #253188, #231092 ) ;
#142365 = ORIENTED_EDGE ( 'NONE', *, *, #25309, .F. ) ;
#142367 = CARTESIAN_POINT ( 'NONE',  ( -17.04761207306819770, 23.01416701742251902, -230.8676723288925245 ) ) ;
#142366 = CARTESIAN_POINT ( 'NONE',  ( -20.94999999999999929, 77.83534155023598089, -57.86795619196132634 ) ) ;
#142368 = DIRECTION ( 'NONE',  ( -1.000000000000000000, -0.000000000000000000, -0.000000000000000000 ) ) ;
#142369 = CARTESIAN_POINT ( 'NONE',  ( 20.95512820512820440, 65.37615131630018084, -124.3731074845243825 ) ) ;
#142370 = FACE_OUTER_BOUND ( 'NONE', #221718, .T. ) ;
#142372 = DIRECTION ( 'NONE',  ( -1.000000000000000000, -0.000000000000000000, -0.000000000000000000 ) ) ;
#142371 = CIRCLE ( 'NONE', #175715, 0.09999999999999489853 ) ;
#142373 = VERTEX_POINT ( 'NONE', #60097 ) ;
#142374 = ORIENTED_EDGE ( 'NONE', *, *, #125289, .T. ) ;
#142375 = EDGE_CURVE ( 'NONE', #187652, #5270, #123491, .T. ) ;
#142376 = DIRECTION ( 'NONE',  ( -0.000000000000000000, -0.000000000000000000, -1.000000000000000000 ) ) ;
#142377 = ORIENTED_EDGE ( 'NONE', *, *, #80584, .T. ) ;
#142379 = CARTESIAN_POINT ( 'NONE',  ( -23.15000000000000213, 11.65000000001115588, -122.2500000000000284 ) ) ;
#142378 = VECTOR ( 'NONE', #220975, 999.9999999999998863 ) ;
#142380 = VECTOR ( 'NONE', #20514, 1000.000000000000114 ) ;
#142381 = ORIENTED_EDGE ( 'NONE', *, *, #123869, .F. ) ;
#142382 = AXIS2_PLACEMENT_3D ( 'NONE', #123168, #203976, #202692 ) ;
#142383 = CARTESIAN_POINT ( 'NONE',  ( -23.25000000000000000, 1.115600667400684642E-11, -200.9999999999999432 ) ) ;
#142384 = AXIS2_PLACEMENT_3D ( 'NONE', #66302, #225346, #33639 ) ;
#142385 = EDGE_CURVE ( 'NONE', #230341, #56486, #66154, .T. ) ;
#142386 = DIRECTION ( 'NONE',  ( 0.000000000000000000, -0.9908441862701783398, 0.1350103645450536627 ) ) ;
#142387 = ORIENTED_EDGE ( 'NONE', *, *, #96767, .F. ) ;
#142388 = ADVANCED_FACE ( 'NONE', ( #195802 ), #238756, .T. ) ;
#142390 = EDGE_CURVE ( 'NONE', #225601, #58341, #94269, .T. ) ;
#142389 = DIRECTION ( 'NONE',  ( 0.000000000000000000, 2.891205793294679805E-16, -1.000000000000000000 ) ) ;
#142391 = CARTESIAN_POINT ( 'NONE',  ( -21.05000000000000071, 65.56235145718194701, -241.8874454306706525 ) ) ;
#142392 = DIRECTION ( 'NONE',  ( 1.000000000000000000, -0.000000000000000000, -0.000000000000000000 ) ) ;
#142393 = DIRECTION ( 'NONE',  ( 0.000000000000000000, -0.9994937237965558774, -0.03181660087586650476 ) ) ;
#142394 = DIRECTION ( 'NONE',  ( -1.000000000000000000, -0.000000000000000000, 0.000000000000000000 ) ) ;
#142395 = CARTESIAN_POINT ( 'NONE',  ( 18.59999999999999076, 8.882751598337870647, -187.0399955572217721 ) ) ;
#142396 = FACE_OUTER_BOUND ( 'NONE', #174307, .T. ) ;
#142397 = ORIENTED_EDGE ( 'NONE', *, *, #12022, .F. ) ;
#142398 = TOROIDAL_SURFACE ( 'NONE', #154907, 0.2000000000000000111, 0.1000000000000000056 ) ;
#142400 = CARTESIAN_POINT ( 'NONE',  ( 21.15000000000005542, 83.90000000001120384, -37.18565239344504647 ) ) ;
#142399 = DIRECTION ( 'NONE',  ( 1.000000000000000000, 0.000000000000000000, 0.000000000000000000 ) ) ;
#142401 = VERTEX_POINT ( 'NONE', #236178 ) ;
#142403 = ORIENTED_EDGE ( 'NONE', *, *, #111394, .F. ) ;
#142402 = CARTESIAN_POINT ( 'NONE',  ( -20.85000000000000142, 11.75000000001115197, -194.1583993101029080 ) ) ;
#142404 = EDGE_CURVE ( 'NONE', #13799, #208746, #40591, .T. ) ;
#142405 = ORIENTED_EDGE ( 'NONE', *, *, #227452, .F. ) ;
#142406 = DIRECTION ( 'NONE',  ( 0.000000000000000000, 0.000000000000000000, 1.000000000000000000 ) ) ;
#142407 = EDGE_CURVE ( 'NONE', #148706, #175005, #131873, .T. ) ;
#142408 = CARTESIAN_POINT ( 'NONE',  ( 23.14999999999999858, 1.115600667400684642E-11, -100.5000000000000426 ) ) ;
#142409 = DIRECTION ( 'NONE',  ( 0.000000000000000000, -6.530723674265620862E-15, 1.000000000000000000 ) ) ;
#142410 = CARTESIAN_POINT ( 'NONE',  ( 23.15000000000000213, -3.770473190032740174, -225.9805569534692324 ) ) ;
#142411 = VERTEX_POINT ( 'NONE', #240045 ) ;
#142412 = DIRECTION ( 'NONE',  ( 1.000000000000000000, 0.000000000000000000, 0.000000000000000000 ) ) ;
#142414 = ADVANCED_FACE ( 'NONE', ( #181370 ), #165184, .F. ) ;
#142413 = LINE ( 'NONE', #221925, #235310 ) ;
#142415 = ORIENTED_EDGE ( 'NONE', *, *, #37352, .F. ) ;
#142416 = B_SPLINE_CURVE_WITH_KNOTS ( 'NONE', 3,
 ( #89655, #210904, #152245, #153550 ),
 .UNSPECIFIED., .F., .F.,
 ( 4, 4 ),
 ( 0.000000000000000000, 0.0001048066582182593560 ),
 .UNSPECIFIED. ) ;
#142417 = CARTESIAN_POINT ( 'NONE',  ( 18.51565452909345311, -9.352859338824332625, -174.6949093212327284 ) ) ;
#142418 = EDGE_CURVE ( 'NONE', #120853, #154121, #231657, .T. ) ;
#142419 = DIRECTION ( 'NONE',  ( 0.000000000000000000, -1.000000000000000000, 0.000000000000000000 ) ) ;
#142420 = EDGE_LOOP ( 'NONE', ( #94590, #158974, #69709, #90714 ) ) ;
#142421 = CARTESIAN_POINT ( 'NONE',  ( -16.82542659449978117, 9.934499891438612451, -146.7446356000260437 ) ) ;
#142422 = ADVANCED_FACE ( 'NONE', ( #176234 ), #57525, .F. ) ;
#142423 = EDGE_CURVE ( 'NONE', #114614, #80656, #119222, .T. ) ;
#142424 = AXIS2_PLACEMENT_3D ( 'NONE', #233464, #134316, #157801 ) ;
#142425 = CARTESIAN_POINT ( 'NONE',  ( 20.94999999999999929, 4.813084112160680661, -112.4415177565238650 ) ) ;
#142426 = ORIENTED_EDGE ( 'NONE', *, *, #4342, .F. ) ;
#142427 = DIRECTION ( 'NONE',  ( 0.000000000000000000, -1.000000000000000000, 0.000000000000000000 ) ) ;
#142428 = EDGE_CURVE ( 'NONE', #141916, #135166, #161808, .T. ) ;
#142429 = CARTESIAN_POINT ( 'NONE',  ( -21.05000000000000071, 1.115650877919449575E-11, -138.1000000000000227 ) ) ;
#142430 = DIRECTION ( 'NONE',  ( -0.000000000000000000, -1.000000000000000000, -6.982962677686266711E-15 ) ) ;
#142431 = DIRECTION ( 'NONE',  ( -0.000000000000000000, 0.2128009952263603677, -0.9770955615653313941 ) ) ;
#142432 = EDGE_CURVE ( 'NONE', #127762, #68761, #216616, .T. ) ;
#142433 = EDGE_CURVE ( 'NONE', #129337, #157637, #32114, .T. ) ;
#142434 = ADVANCED_FACE ( 'NONE', ( #117521 ), #154538, .T. ) ;
#142435 = AXIS2_PLACEMENT_3D ( 'NONE', #44210, #65039, #102858 ) ;
#142436 = DIRECTION ( 'NONE',  ( 0.000000000000000000, -0.1350103645451904977, -0.9908441862701596881 ) ) ;
#142437 = CARTESIAN_POINT ( 'NONE',  ( -20.85000000000000142, 68.92903212821357783, -166.2765432626560766 ) ) ;
#142438 = CARTESIAN_POINT ( 'NONE',  ( 20.94403535211772294, 10.30632246271647467, -72.50418367788957141 ) ) ;
#142440 = EDGE_LOOP ( 'NONE', ( #176198, #22771, #48163, #59398 ) ) ;
#142439 = AXIS2_PLACEMENT_3D ( 'NONE', #104830, #123159, #202682 ) ;
#142442 = DIRECTION ( 'NONE',  ( 1.000000000000000000, -3.151514657663852580E-16, 8.547182517843351137E-17 ) ) ;
#142441 = DIRECTION ( 'NONE',  ( 0.000000000000000000, 0.9915357197604792727, -0.1298341882520475943 ) ) ;
#142443 = EDGE_LOOP ( 'NONE', ( #176968, #90509, #40588, #168954 ) ) ;
#142444 = CARTESIAN_POINT ( 'NONE',  ( -16.89318236219976654, 12.41444193003837881, -211.2375501061338525 ) ) ;
#142445 = SPHERICAL_SURFACE ( 'NONE', #258024, 0.1000000000000000056 ) ;
#142447 = ORIENTED_EDGE ( 'NONE', *, *, #235535, .T. ) ;
#142446 = CARTESIAN_POINT ( 'NONE',  ( -20.85000000000000142, 7.668827189579289438, -241.6142244293585009 ) ) ;
#142448 = VERTEX_POINT ( 'NONE', #223028 ) ;
#142449 = EDGE_CURVE ( 'NONE', #14807, #167594, #104348, .T. ) ;
#142450 = CARTESIAN_POINT ( 'NONE',  ( 20.94999999999999929, 43.51422117117169108, -240.0698702536254530 ) ) ;
#142451 = DIRECTION ( 'NONE',  ( -0.000000000000000000, 0.4721928772777346239, 0.8814952561688430555 ) ) ;
#142452 = DIRECTION ( 'NONE',  ( 3.616040088954490704E-32, 7.105427357601001859E-15, -1.000000000000000000 ) ) ;
#142453 = EDGE_CURVE ( 'NONE', #129734, #178561, #2860, .T. ) ;
#142454 = CARTESIAN_POINT ( 'NONE',  ( 18.50000000000000000, 46.88959166481302532, -255.2681066192500339 ) ) ;
#142455 = ORIENTED_EDGE ( 'NONE', *, *, #217599, .T. ) ;
#142456 = CIRCLE ( 'NONE', #234033, 0.09999999999999939493 ) ;
#142457 = DIRECTION ( 'NONE',  ( 0.000000000000000000, 0.000000000000000000, 1.000000000000000000 ) ) ;
#142458 = EDGE_LOOP ( 'NONE', ( #60800, #145656, #40316, #8510 ) ) ;
#142459 = EDGE_LOOP ( 'NONE', ( #155053, #209805, #20339, #215925 ) ) ;
#142460 = CARTESIAN_POINT ( 'NONE',  ( -18.39999999999999858, 85.50000000001138289, -29.42291809330221497 ) ) ;
#142461 = DIRECTION ( 'NONE',  ( 0.000000000000000000, 0.8814952561688430555, -0.4721928772777346239 ) ) ;
#142462 = ORIENTED_EDGE ( 'NONE', *, *, #193185, .T. ) ;
#142463 = CARTESIAN_POINT ( 'NONE',  ( -21.05000000000000071, 87.48912529308817909, -133.6231074845242119 ) ) ;
#142464 = AXIS2_PLACEMENT_3D ( 'NONE', #96552, #176140, #222930 ) ;
#142465 = CIRCLE ( 'NONE', #54967, 0.9750000000000036415 ) ;
#142466 = CARTESIAN_POINT ( 'NONE',  ( 18.59999999999999076, 7.668827189579289438, -241.6142244293585009 ) ) ;
#142467 = EDGE_CURVE ( 'NONE', #51672, #13968, #36218, .T. ) ;
#142468 = ORIENTED_EDGE ( 'NONE', *, *, #69726, .F. ) ;
#142470 = EDGE_CURVE ( 'NONE', #257957, #85029, #27851, .T. ) ;
#142469 = DIRECTION ( 'NONE',  ( -0.5932847527679310229, 0.8049926720990042694, -6.366092712777067056E-16 ) ) ;
#142471 = CARTESIAN_POINT ( 'NONE',  ( 23.40000000000005187, 83.90000000001120384, -34.77310748452479316 ) ) ;
#142472 = EDGE_LOOP ( 'NONE', ( #19299, #29140, #15236, #239124 ) ) ;
#142473 = ORIENTED_EDGE ( 'NONE', *, *, #178780, .T. ) ;
#142474 = DIRECTION ( 'NONE',  ( 1.000000000000000000, 0.000000000000000000, 0.000000000000000000 ) ) ;
#142475 = ORIENTED_EDGE ( 'NONE', *, *, #81431, .F. ) ;
#142476 = FACE_OUTER_BOUND ( 'NONE', #198729, .T. ) ;
#142477 = ORIENTED_EDGE ( 'NONE', *, *, #193060, .F. ) ;
#142479 = ORIENTED_EDGE ( 'NONE', *, *, #162870, .F. ) ;
#142478 = CARTESIAN_POINT ( 'NONE',  ( -23.25000000000000000, 79.08634564045905790, -228.8189404293001132 ) ) ;
#142480 = AXIS2_PLACEMENT_3D ( 'NONE', #133417, #58976, #17329 ) ;
#142481 = DIRECTION ( 'NONE',  ( 1.000000000000000000, 0.000000000000000000, 0.000000000000000000 ) ) ;
#142482 = EDGE_LOOP ( 'NONE', ( #159083, #140829, #227580, #154798 ) ) ;
#142483 = VERTEX_POINT ( 'NONE', #105630 ) ;
#142485 = ORIENTED_EDGE ( 'NONE', *, *, #17871, .F. ) ;
#142484 = VERTEX_POINT ( 'NONE', #243877 ) ;
#142486 = DIRECTION ( 'NONE',  ( 1.000000000000000000, 0.000000000000000000, 0.000000000000000000 ) ) ;
#142487 = EDGE_CURVE ( 'NONE', #94999, #109724, #9132, .T. ) ;
#142488 = CARTESIAN_POINT ( 'NONE',  ( -23.25000000000000000, 13.96869538424788360, -210.3925794786332233 ) ) ;
#142489 = VERTEX_POINT ( 'NONE', #3986 ) ;
#142490 = VECTOR ( 'NONE', #242616, 1000.000000000000000 ) ;
#142491 = EDGE_LOOP ( 'NONE', ( #137896, #15768, #251200, #96891 ) ) ;
#142492 = CARTESIAN_POINT ( 'NONE',  ( 17.74533788810830615, 41.64821155081010318, -235.4615294780919896 ) ) ;
#142494 = DIRECTION ( 'NONE',  ( 0.000000000000000000, 0.6728971962617388280, -0.7397360091702248619 ) ) ;
#142493 = VECTOR ( 'NONE', #239724, 1000.000000000000000 ) ;
#142496 = ORIENTED_EDGE ( 'NONE', *, *, #90933, .T. ) ;
#142495 = CARTESIAN_POINT ( 'NONE',  ( 18.49999999999999645, 1.736257131608553550, -179.0686523290174819 ) ) ;
#142497 = DIRECTION ( 'NONE',  ( 0.000000000000000000, 6.982962677686266711E-15, -1.000000000000000000 ) ) ;
#142498 = ORIENTED_EDGE ( 'NONE', *, *, #6008, .F. ) ;
#142499 = DIRECTION ( 'NONE',  ( 1.020425574104004196E-15, 1.210927747993693964E-31, 1.000000000000000000 ) ) ;
#142500 = CARTESIAN_POINT ( 'NONE',  ( 18.49999999999999289, 65.79142135624927334, -111.8731074845243683 ) ) ;
#142501 = AXIS2_PLACEMENT_3D ( 'NONE', #209670, #110563, #36186 ) ;
#142502 = ORIENTED_EDGE ( 'NONE', *, *, #91827, .F. ) ;
#142503 = CARTESIAN_POINT ( 'NONE',  ( -18.59999999999999787, 45.99141771592758943, -256.5205054824189119 ) ) ;
#142504 = AXIS2_PLACEMENT_3D ( 'NONE', #181303, #200851, #41800 ) ;
#142505 = VECTOR ( 'NONE', #176212, 1000.000000000000000 ) ;
#142507 = ORIENTED_EDGE ( 'NONE', *, *, #75035, .F. ) ;
#142506 = TOROIDAL_SURFACE ( 'NONE', #30125, 1.900000000000002576, 0.1000000000000000056 ) ;
#142508 = DIRECTION ( 'NONE',  ( 0.000000000000000000, -0.9126074666063770380, -0.4088369013363281068 ) ) ;
#142509 = ORIENTED_EDGE ( 'NONE', *, *, #18221, .T. ) ;
#142510 = VECTOR ( 'NONE', #25943, 1000.000000000000000 ) ;
#142512 = VERTEX_POINT ( 'NONE', #65243 ) ;
#142511 = ORIENTED_EDGE ( 'NONE', *, *, #41768, .T. ) ;
#142513 = ORIENTED_EDGE ( 'NONE', *, *, #112045, .T. ) ;
#142514 = CARTESIAN_POINT ( 'NONE',  ( -16.92989143108098204, 9.950000000011138823, -79.88248387475671564 ) ) ;
#142515 = ORIENTED_EDGE ( 'NONE', *, *, #115686, .F. ) ;
#142516 = CARTESIAN_POINT ( 'NONE',  ( 20.94999999999999929, 10.38178547073510316, -72.50784536388417223 ) ) ;
#142517 = EDGE_LOOP ( 'NONE', ( #38753, #209592, #99361, #214724 ) ) ;
#142518 = CARTESIAN_POINT ( 'NONE',  ( -20.64999999999999858, 82.48249193998721296, -215.5326005316167084 ) ) ;
#142519 = B_SPLINE_CURVE_WITH_KNOTS ( 'NONE', 3,
 ( #195058, #16421, #95918, #18953, #98454, #185424, #27676, #6783, #87583, #43356, #225803, #8083, #142438, #221947, #86292, #64198, #165880, #223250, #167181 ),
 .UNSPECIFIED., .F., .F.,
 ( 4, 3, 3, 3, 3, 3, 4 ),
 ( 1.387778780781445676E-17, 2.646747978908994698E-05, 5.271166642128863382E-05, 9.008788829885137981E-05, 0.0001426648776561022008, 0.0001897378458659801945, 0.0001917382627806380965 ),
 .UNSPECIFIED. ) ;
#142520 = AXIS2_PLACEMENT_3D ( 'NONE', #63380, #182070, #103778 ) ;
#142521 = DIRECTION ( 'NONE',  ( 0.000000000000000000, 0.000000000000000000, 1.000000000000000000 ) ) ;
#142522 = EDGE_CURVE ( 'NONE', #61821, #216196, #169511, .T. ) ;
#142523 = ORIENTED_EDGE ( 'NONE', *, *, #100494, .F. ) ;
#142524 = ADVANCED_FACE ( 'NONE', ( #83492 ), #88635, .T. ) ;
#142525 = VERTEX_POINT ( 'NONE', #87359 ) ;
#142526 = CIRCLE ( 'NONE', #105084, 0.09999999999999939493 ) ;
#142527 = VECTOR ( 'NONE', #139350, 1000.000000000000000 ) ;
#142528 = AXIS2_PLACEMENT_3D ( 'NONE', #176809, #34737, #193790 ) ;
#142529 = VERTEX_POINT ( 'NONE', #127801 ) ;
#142530 = AXIS2_PLACEMENT_3D ( 'NONE', #77538, #18871, #78828 ) ;
#142531 = EDGE_CURVE ( 'NONE', #3167, #28760, #108234, .T. ) ;
#142532 = CARTESIAN_POINT ( 'NONE',  ( 21.09096482362066993, 69.63645563460816845, -203.5625557632985476 ) ) ;
#142533 = ORIENTED_EDGE ( 'NONE', *, *, #97982, .F. ) ;
#142534 = FACE_OUTER_BOUND ( 'NONE', #126201, .T. ) ;
#142535 = CIRCLE ( 'NONE', #30156, 0.5000000000000004441 ) ;
#142536 = EDGE_CURVE ( 'NONE', #88642, #241392, #164360, .T. ) ;
#142537 = CARTESIAN_POINT ( 'NONE',  ( -21.65000000000000213, 44.76114064897694789, -237.4293191035423831 ) ) ;
#142538 = DIRECTION ( 'NONE',  ( 1.000000000000000000, 0.000000000000000000, 0.000000000000000000 ) ) ;
#142539 = CARTESIAN_POINT ( 'NONE',  ( -20.00857864376270001, 9.150000000011157653, -146.3500000000000227 ) ) ;
#142540 = CARTESIAN_POINT ( 'NONE',  ( 18.59999999999999076, 53.24180694658302571, -234.8354225850497130 ) ) ;
#142541 = DIRECTION ( 'NONE',  ( 0.000000000000000000, -1.000000000000000000, 0.000000000000000000 ) ) ;
#142543 = DIRECTION ( 'NONE',  ( -1.000000000000000000, 0.000000000000000000, 0.000000000000000000 ) ) ;
#142542 = FACE_OUTER_BOUND ( 'NONE', #212519, .T. ) ;
#142544 = CARTESIAN_POINT ( 'NONE',  ( -2.995603634470891112E-16, 87.75000000001250555, -178.7731074845242745 ) ) ;
#142545 = DIRECTION ( 'NONE',  ( -1.000000000000000000, 0.000000000000000000, 0.000000000000000000 ) ) ;
#142546 = EDGE_CURVE ( 'NONE', #162078, #68363, #67812, .T. ) ;
#142547 = DIRECTION ( 'NONE',  ( 0.000000000000000000, -0.8814952561688437216, 0.4721928772777334582 ) ) ;
#142548 = CARTESIAN_POINT ( 'NONE',  ( 18.59999999999999432, 74.83729825007462466, -195.4231074845243654 ) ) ;
#142549 = AXIS2_PLACEMENT_3D ( 'NONE', #72472, #32074, #111587 ) ;
#142551 = VERTEX_POINT ( 'NONE', #6552 ) ;
#142550 = VECTOR ( 'NONE', #137912, 1000.000000000000114 ) ;
#142552 = VECTOR ( 'NONE', #134911, 1000.000000000000000 ) ;
#142554 = EDGE_LOOP ( 'NONE', ( #224003, #93306, #195002, #193869 ) ) ;
#142553 = DIRECTION ( 'NONE',  ( 0.000000000000000000, -0.8814952561688476074, 0.4721928772777262417 ) ) ;
#142555 = ORIENTED_EDGE ( 'NONE', *, *, #165006, .F. ) ;
#142557 = EDGE_CURVE ( 'NONE', #4792, #93776, #245175, .T. ) ;
#142556 = LINE ( 'NONE', #61749, #3391 ) ;
#142558 = CARTESIAN_POINT ( 'NONE',  ( 20.54374330479337374, 10.50501031423420351, -141.7256836348881279 ) ) ;
#142559 = CARTESIAN_POINT ( 'NONE',  ( 18.79999999999999716, -1.885425182446133663, -11.49641995933507665 ) ) ;
#142560 = VERTEX_POINT ( 'NONE', #168247 ) ;
#142561 = CARTESIAN_POINT ( 'NONE',  ( -20.94999999999999929, 87.39257802171731271, -66.44915790469229933 ) ) ;
#142562 = CARTESIAN_POINT ( 'NONE',  ( -21.05000000000000071, 88.41227409416111982, -38.92310748452423752 ) ) ;
#142563 = CIRCLE ( 'NONE', #146651, 11.90000000000000213 ) ;
#142564 = VERTEX_POINT ( 'NONE', #226883 ) ;
#142565 = LINE ( 'NONE', #246808, #133875 ) ;
#142566 = CARTESIAN_POINT ( 'NONE',  ( 23.14999999999999503, 11.65000000001116298, -160.4851942293460922 ) ) ;
#142567 = CARTESIAN_POINT ( 'NONE',  ( -23.15000000000000213, -9.600000000000001421, 11.74999999999999645 ) ) ;
#142568 = DIRECTION ( 'NONE',  ( 0.000000000000000000, -6.982962677686266711E-15, 1.000000000000000000 ) ) ;
#142570 = EDGE_LOOP ( 'NONE', ( #33388, #154403, #46241, #65797, #3569, #170094, #53463, #65434, #243353, #241995, #30620, #23476 ) ) ;
#142569 = DIRECTION ( 'NONE',  ( -1.000000000000000000, 0.000000000000000000, 0.000000000000000000 ) ) ;
#142571 = DIRECTION ( 'NONE',  ( -1.000000000000000000, 0.000000000000000000, 0.000000000000000000 ) ) ;
#142573 = VERTEX_POINT ( 'NONE', #46947 ) ;
#142572 = CARTESIAN_POINT ( 'NONE',  ( -18.59999999999999787, 64.35000000001254250, -182.1731074845244507 ) ) ;
#142574 = DIRECTION ( 'NONE',  ( 1.000000000000000000, 0.000000000000000000, 0.000000000000000000 ) ) ;
#142575 = DIRECTION ( 'NONE',  ( -0.000000000000000000, 0.2128009952263603677, -0.9770955615653313941 ) ) ;
#142576 = CARTESIAN_POINT ( 'NONE',  ( -20.54999999999999716, 2.400000000011155432, -124.1060308773475924 ) ) ;
#142577 = DIRECTION ( 'NONE',  ( 0.000000000000000000, 0.000000000000000000, -1.000000000000000000 ) ) ;
#142579 = DIRECTION ( 'NONE',  ( 0.000000000000000000, 0.000000000000000000, -1.000000000000000000 ) ) ;
#142578 = CARTESIAN_POINT ( 'NONE',  ( -16.93211319090181632, 63.05646689806795990, -213.0445598095664081 ) ) ;
#142580 = CARTESIAN_POINT ( 'NONE',  ( -23.25000000000000000, 76.00000000001190870, -103.0231074845243029 ) ) ;
#142581 = CARTESIAN_POINT ( 'NONE',  ( -16.92507428761701505, 23.03395201945197357, -230.9649992399934320 ) ) ;
#142582 = CARTESIAN_POINT ( 'NONE',  ( -18.50000324121759121, 10.29307482167955001, -38.95864214669403225 ) ) ;
#142583 = CARTESIAN_POINT ( 'NONE',  ( -23.25000000000000000, 85.68240343348777799, -29.36626410711146562 ) ) ;
#142584 = CARTESIAN_POINT ( 'NONE',  ( -16.77828822459933633, 9.946229375067616729, -87.83737174908110035 ) ) ;
#142585 = ORIENTED_EDGE ( 'NONE', *, *, #197405, .T. ) ;
#142586 = ADVANCED_FACE ( 'NONE', ( #126508 ), #240224, .F. ) ;
#142588 = CIRCLE ( 'NONE', #113392, 0.1000000000000045158 ) ;
#142587 = DIRECTION ( 'NONE',  ( 0.000000000000000000, -0.1350103645451807555, -0.9908441862701610203 ) ) ;
#142589 = ORIENTED_EDGE ( 'NONE', *, *, #59346, .F. ) ;
#142590 = ORIENTED_EDGE ( 'NONE', *, *, #50746, .F. ) ;
#142591 = CARTESIAN_POINT ( 'NONE',  ( -20.94999999999999929, 11.64999999999999680, -26.71613433702190576 ) ) ;
#142592 = CARTESIAN_POINT ( 'NONE',  ( -18.59999999999999787, 14.85285025691667293, -236.4388300032497057 ) ) ;
#142593 = ORIENTED_EDGE ( 'NONE', *, *, #92837, .T. ) ;
#142594 = ADVANCED_FACE ( 'NONE', ( #106929 ), #43128, .F. ) ;
#142595 = ORIENTED_EDGE ( 'NONE', *, *, #206773, .F. ) ;
#142596 = EDGE_CURVE ( 'NONE', #138896, #44452, #151219, .T. ) ;
#142597 = EDGE_CURVE ( 'NONE', #175274, #54282, #161101, .T. ) ;
#142598 = TOROIDAL_SURFACE ( 'NONE', #59186, 1.900000000000002576, 0.1000000000000000056 ) ;
#142599 = ORIENTED_EDGE ( 'NONE', *, *, #98367, .F. ) ;
#142600 = DIRECTION ( 'NONE',  ( 0.000000000000000000, -1.000000000000000000, 0.000000000000000000 ) ) ;
#142601 = VERTEX_POINT ( 'NONE', #89934 ) ;
#142602 = CIRCLE ( 'NONE', #109293, 0.09999999999998898659 ) ;
#142603 = DIRECTION ( 'NONE',  ( 0.000000000000000000, 0.8267009638119717785, 0.5626415523513675909 ) ) ;
#142604 = CARTESIAN_POINT ( 'NONE',  ( 22.50000000000000000, 1.148907358139439339E-11, -201.0000000000015064 ) ) ;
#142605 = CARTESIAN_POINT ( 'NONE',  ( -21.05000000000000071, 87.65000000001235492, -167.0231074845242460 ) ) ;
#142606 = DIRECTION ( 'NONE',  ( -1.000000000000000000, 7.304098846218135653E-16, -4.607487905232624742E-31 ) ) ;
#142607 = DIRECTION ( 'NONE',  ( 0.000000000000000000, 0.9667078373770114919, 0.2558827019434133931 ) ) ;
#142608 = AXIS2_PLACEMENT_3D ( 'NONE', #248778, #29755, #87108 ) ;
#142609 = DIRECTION ( 'NONE',  ( -1.000000000000000000, 0.000000000000000000, 0.000000000000000000 ) ) ;
#142610 = CARTESIAN_POINT ( 'NONE',  ( -20.64999999999999858, 76.00000000001267608, -203.5231074845243597 ) ) ;
#142612 = VERTEX_POINT ( 'NONE', #173385 ) ;
#142611 = DIRECTION ( 'NONE',  ( 1.000000000000000000, -0.000000000000000000, 0.000000000000000000 ) ) ;
#142614 = CARTESIAN_POINT ( 'NONE',  ( -20.54999999999999716, 34.89593390941166007, -248.6067769466879156 ) ) ;
#142613 = CARTESIAN_POINT ( 'NONE',  ( 20.95132126680579887, 65.51005012986480835, -61.95278294608986869 ) ) ;
#142615 = EDGE_CURVE ( 'NONE', #183920, #224594, #65415, .T. ) ;
#142616 = CARTESIAN_POINT ( 'NONE',  ( -18.59999999999999787, -1.835859311432481045, -112.0044391687985694 ) ) ;
#142617 = EDGE_LOOP ( 'NONE', ( #34350, #152165, #223601, #6555 ) ) ;
#142618 = DIRECTION ( 'NONE',  ( 0.000000000000000000, 0.4999999999999689138, -0.8660254037844565822 ) ) ;
#142620 = EDGE_CURVE ( 'NONE', #66849, #18395, #247733, .T. ) ;
#142619 = DIRECTION ( 'NONE',  ( -1.020425574104004394E-15, 0.9126074666063769270, 0.4088369013363280513 ) ) ;
#142621 = ORIENTED_EDGE ( 'NONE', *, *, #132512, .T. ) ;
#142624 = DIRECTION ( 'NONE',  ( 0.000000000000000000, -0.1332476588733448597, -0.9910827722268067408 ) ) ;
#142623 = AXIS2_PLACEMENT_3D ( 'NONE', #243514, #62319, #124861 ) ;
#142622 = DIRECTION ( 'NONE',  ( -7.304098846218134667E-16, -1.000000000000000000, 0.000000000000000000 ) ) ;
#142625 = CARTESIAN_POINT ( 'NONE',  ( -20.65000000000000568, 63.54522198573874192, -221.7484608313106378 ) ) ;
#142626 = ORIENTED_EDGE ( 'NONE', *, *, #151633, .T. ) ;
#142627 = CARTESIAN_POINT ( 'NONE',  ( 21.14999999999999503, -8.777002227904191045, -238.5420042644097975 ) ) ;
#142628 = DIRECTION ( 'NONE',  ( 0.000000000000000000, 2.891205793294679805E-16, -1.000000000000000000 ) ) ;
#142629 = EDGE_CURVE ( 'NONE', #160519, #151240, #54660, .T. ) ;
#142630 = DIRECTION ( 'NONE',  ( -1.000000000000000000, -0.000000000000000000, -0.000000000000000000 ) ) ;
#142631 = CARTESIAN_POINT ( 'NONE',  ( 23.14999999999999858, 76.00000000001190870, -103.0231074845243029 ) ) ;
#142632 = ADVANCED_FACE ( 'NONE', ( #249038 ), #132939, .T. ) ;
#142633 = ORIENTED_EDGE ( 'NONE', *, *, #30021, .F. ) ;
#142634 = ADVANCED_FACE ( 'NONE', ( #32581 ), #73635, .T. ) ;
#142635 = VECTOR ( 'NONE', #192372, 1000.000000000000000 ) ;
#142636 = AXIS2_PLACEMENT_3D ( 'NONE', #71281, #127383, #189927 ) ;
#142637 = CIRCLE ( 'NONE', #126070, 0.09999999999999542588 ) ;
#142638 = AXIS2_PLACEMENT_3D ( 'NONE', #68821, #8836, #209603 ) ;
#142639 = CARTESIAN_POINT ( 'NONE',  ( 21.14999999999999858, 67.21339244341174890, -90.77310748452437394 ) ) ;
#142640 = DIRECTION ( 'NONE',  ( -0.7071067811865633379, 0.6824534298470439353, -0.1850873201761353837 ) ) ;
#142641 = DIRECTION ( 'NONE',  ( 0.000000000000000000, 0.8814952561688476074, -0.4721928772777262417 ) ) ;
#142642 = CARTESIAN_POINT ( 'NONE',  ( -16.87304349924914604, 30.24631159100806599, -234.8151387799927363 ) ) ;
#142643 = LINE ( 'NONE', #123113, #161723 ) ;
#142644 = SPHERICAL_SURFACE ( 'NONE', #168020, 0.1000000000000000056 ) ;
#142646 = ORIENTED_EDGE ( 'NONE', *, *, #210701, .F. ) ;
#142645 = CARTESIAN_POINT ( 'NONE',  ( -20.64999999999999858, 0.000000000000000000, -33.50000000000000000 ) ) ;
#142647 = DIRECTION ( 'NONE',  ( -1.000000000000000000, -0.000000000000000000, -0.000000000000000000 ) ) ;
#142649 = EDGE_CURVE ( 'NONE', #91045, #125402, #98689, .T. ) ;
#142648 = FACE_OUTER_BOUND ( 'NONE', #142759, .T. ) ;
#142650 = LINE ( 'NONE', #183098, #250268 ) ;
#142651 = DIRECTION ( 'NONE',  ( -1.000000000000000000, 2.849773892568378313E-16, -7.728835255496647986E-17 ) ) ;
#142652 = LINE ( 'NONE', #83931, #133810 ) ;
#142654 = ORIENTED_EDGE ( 'NONE', *, *, #85648, .T. ) ;
#142653 = DIRECTION ( 'NONE',  ( 0.000000000000000000, 0.000000000000000000, -1.000000000000000000 ) ) ;
#142655 = CARTESIAN_POINT ( 'NONE',  ( -20.85000000000000142, 64.25000000001142553, -36.02310748452440237 ) ) ;
#142656 = DIRECTION ( 'NONE',  ( 0.000000000000000000, 0.2128009952263621718, -0.9770955615653310611 ) ) ;
#142657 = CARTESIAN_POINT ( 'NONE',  ( -21.05000000000000071, 76.00000000001190870, -103.0231074845243029 ) ) ;
#142658 = ORIENTED_EDGE ( 'NONE', *, *, #48641, .F. ) ;
#142659 = CARTESIAN_POINT ( 'NONE',  ( -14.45422546970482891, 66.54939790392373311, -151.5792115214277374 ) ) ;
#142660 = CARTESIAN_POINT ( 'NONE',  ( -20.64999999999999858, 68.75000000001260503, -191.2731074845244166 ) ) ;
#142661 = CYLINDRICAL_SURFACE ( 'NONE', #108645, 0.09999999999999939493 ) ;
#142662 = EDGE_CURVE ( 'NONE', #114575, #168296, #157017, .T. ) ;
#142663 = TOROIDAL_SURFACE ( 'NONE', #30275, 7.800000000000000711, 0.1000000000000000056 ) ;
#142664 = CARTESIAN_POINT ( 'NONE',  ( 20.94999999999999574, 10.62357026049396680, -141.4919452032305855 ) ) ;
#142665 = EDGE_LOOP ( 'NONE', ( #195024, #6878, #46586, #12556 ) ) ;
#142666 = CIRCLE ( 'NONE', #246728, 0.09999999999999938105 ) ;
#142667 = CARTESIAN_POINT ( 'NONE',  ( 0.8999999999999993561, -11.75000000000000000, 26.00000000000000355 ) ) ;
#142668 = ORIENTED_EDGE ( 'NONE', *, *, #205273, .T. ) ;
#142669 = CARTESIAN_POINT ( 'NONE',  ( 21.53551880898956838, 60.65712384523044420, -234.1747044932786253 ) ) ;
#142670 = CARTESIAN_POINT ( 'NONE',  ( 20.94999999999999574, 1.261786168576181755, -75.08649896354552311 ) ) ;
#142671 = EDGE_CURVE ( 'NONE', #252923, #97941, #251586, .T. ) ;
#142672 = AXIS2_PLACEMENT_3D ( 'NONE', #163409, #180401, #60430 ) ;
#142673 = DIRECTION ( 'NONE',  ( -3.265361837132813093E-16, -1.000000000000000000, -7.086529944415894657E-15 ) ) ;
#142674 = ORIENTED_EDGE ( 'NONE', *, *, #146159, .F. ) ;
#142675 = B_SPLINE_CURVE_WITH_KNOTS ( 'NONE', 3,
 ( #44943, #120647, #101004, #180599, #12257, #107477, #68362, #9663, #33129, #151772, #187046, #127044, #129618, #128342, #168793, #150476, #108764, #70960, #229995, #51326, #149199, #8394, #73524, #50071, #188294, #30535 ),
 .UNSPECIFIED., .F., .F.,
 ( 4, 2, 2, 2, 2, 2, 2, 2, 2, 2, 2, 2, 4 ),
 ( 0.005476422646581333500, 0.006160811967703513220, 0.006845201288825692940, 0.007187395949386799279, 0.007529590609947904752, 0.007871785270509010224, 0.008213979931070116564, 0.008556174591631222903, 0.008898369252192329243, 0.009240563912753433848, 0.009582758573314538453, 0.01026714789443678583, 0.01095153721555903320 ),
 .UNSPECIFIED. ) ;
#142676 = CARTESIAN_POINT ( 'NONE',  ( -18.59999999999999787, 1.835341550235567887, -78.55515129256302487 ) ) ;
#142677 = AXIS2_PLACEMENT_3D ( 'NONE', #201651, #118276, #23046 ) ;
#142678 = EDGE_CURVE ( 'NONE', #146093, #221590, #129081, .T. ) ;
#142679 = DIRECTION ( 'NONE',  ( 1.000000000000000000, 0.000000000000000000, 0.000000000000000000 ) ) ;
#142680 = AXIS2_PLACEMENT_3D ( 'NONE', #48183, #11652, #151157 ) ;
#142681 = DIRECTION ( 'NONE',  ( 0.000000000000000000, -0.4999999999999088507, 0.8660254037844913322 ) ) ;
#142682 = AXIS2_PLACEMENT_3D ( 'NONE', #127783, #245158, #246439 ) ;
#142683 = EDGE_CURVE ( 'NONE', #71853, #102606, #114643, .T. ) ;
#142684 = CIRCLE ( 'NONE', #34409, 0.1000000000000028644 ) ;
#142685 = CARTESIAN_POINT ( 'NONE',  ( 22.59999999999999787, 0.04781839070480805448, 11.75002241904723022 ) ) ;
#142686 = DIRECTION ( 'NONE',  ( 0.000000000000000000, 0.000000000000000000, 1.000000000000000000 ) ) ;
#142688 = DIRECTION ( 'NONE',  ( 0.000000000000000000, -0.1350103645451876666, 0.9908441862701600211 ) ) ;
#142687 = CIRCLE ( 'NONE', #30297, 0.1000000000000024342 ) ;
#142689 = VERTEX_POINT ( 'NONE', #209912 ) ;
#142691 = ORIENTED_EDGE ( 'NONE', *, *, #17247, .T. ) ;
#142690 = CARTESIAN_POINT ( 'NONE',  ( -17.11825945287481332, 66.05000000001153637, -48.77310748452439526 ) ) ;
#142692 = TOROIDAL_SURFACE ( 'NONE', #242661, 0.9750000000000019762, 0.1000000000000000056 ) ;
#142693 = EDGE_CURVE ( 'NONE', #78383, #109454, #234789, .T. ) ;
#142694 = ORIENTED_EDGE ( 'NONE', *, *, #165653, .T. ) ;
#142695 = DIRECTION ( 'NONE',  ( 0.000000000000000000, -0.8700118002898321601, 0.4930308989875230030 ) ) ;
#142696 = EDGE_CURVE ( 'NONE', #31765, #163039, #230759, .T. ) ;
#142697 = ORIENTED_EDGE ( 'NONE', *, *, #216857, .T. ) ;
#142698 = CARTESIAN_POINT ( 'NONE',  ( 21.06490991615909536, 65.27510865242494731, -124.3193961309912510 ) ) ;
#142699 = CARTESIAN_POINT ( 'NONE',  ( -23.15000000000000213, 4.250000000011156409, -155.1500000000000057 ) ) ;
#142700 = CARTESIAN_POINT ( 'NONE',  ( -21.05000000000000071, 0.000000000000000000, -33.50000000000000000 ) ) ;
#142701 = ORIENTED_EDGE ( 'NONE', *, *, #28824, .F. ) ;
#142702 = DIRECTION ( 'NONE',  ( -1.000000000000000000, -2.952720810173289112E-16, 0.000000000000000000 ) ) ;
#142703 = CYLINDRICAL_SURFACE ( 'NONE', #113732, 0.1000000000000028644 ) ;
#142704 = CIRCLE ( 'NONE', #92820, 0.1000000000000028644 ) ;
#142705 = ORIENTED_EDGE ( 'NONE', *, *, #250941, .T. ) ;
#142706 = CARTESIAN_POINT ( 'NONE',  ( 23.14999999999999858, 76.00000000001142553, -36.02310748452432421 ) ) ;
#142707 = CIRCLE ( 'NONE', #192802, 0.1000000000000028644 ) ;
#142709 = ORIENTED_EDGE ( 'NONE', *, *, #69433, .F. ) ;
#142708 = CARTESIAN_POINT ( 'NONE',  ( 20.94999999999999929, 65.61821452928772658, -64.01526212064021593 ) ) ;
#142710 = LINE ( 'NONE', #243105, #52233 ) ;
#142711 = CIRCLE ( 'NONE', #30314, 0.1000000000000118433 ) ;
#142712 = ADVANCED_FACE ( 'NONE', ( #194207 ), #15573, .F. ) ;
#142713 = EDGE_CURVE ( 'NONE', #240913, #17892, #140213, .T. ) ;
#142714 = VECTOR ( 'NONE', #153795, 999.9999999999998863 ) ;
#142715 = VERTEX_POINT ( 'NONE', #191653 ) ;
#142716 = CIRCLE ( 'NONE', #88732, 2.000000000000001776 ) ;
#142717 = DIRECTION ( 'NONE',  ( 0.000000000000000000, 0.000000000000000000, -1.000000000000000000 ) ) ;
#142718 = FACE_OUTER_BOUND ( 'NONE', #22509, .T. ) ;
#142719 = DIRECTION ( 'NONE',  ( 5.421010862427555697E-16, 0.4088369013363311044, -0.9126074666063758167 ) ) ;
#142720 = ORIENTED_EDGE ( 'NONE', *, *, #46402, .T. ) ;
#142721 = DIRECTION ( 'NONE',  ( -1.000000000000000000, -0.000000000000000000, -0.000000000000000000 ) ) ;
#142722 = ADVANCED_FACE ( 'NONE', ( #13005 ), #135472, .T. ) ;
#142723 = DIRECTION ( 'NONE',  ( 1.000000000000000000, 0.000000000000000000, 0.000000000000000000 ) ) ;
#142724 = ORIENTED_EDGE ( 'NONE', *, *, #129281, .F. ) ;
#142725 = EDGE_CURVE ( 'NONE', #89054, #183644, #119603, .T. ) ;
#142726 = AXIS2_PLACEMENT_3D ( 'NONE', #81406, #61885, #141410 ) ;
#142727 = AXIS2_PLACEMENT_3D ( 'NONE', #68671, #148197, #210741 ) ;
#142728 = CIRCLE ( 'NONE', #188540, 0.1000000000000028644 ) ;
#142729 = ORIENTED_EDGE ( 'NONE', *, *, #134351, .F. ) ;
#142730 = ADVANCED_FACE ( 'NONE', ( #139319 ), #1083, .T. ) ;
#142731 = ORIENTED_EDGE ( 'NONE', *, *, #252195, .T. ) ;
#142732 = DIRECTION ( 'NONE',  ( 0.000000000000000000, -1.000000000000000000, 0.000000000000000000 ) ) ;
#142733 = CARTESIAN_POINT ( 'NONE',  ( -16.79270642812263503, 66.05375578307393880, -182.6841742059602041 ) ) ;
#142735 = ORIENTED_EDGE ( 'NONE', *, *, #223029, .T. ) ;
#142734 = CARTESIAN_POINT ( 'NONE',  ( -16.85939591225058720, 9.905226478399001167, -146.9600682464690635 ) ) ;
#142736 = DIRECTION ( 'NONE',  ( -1.073024830501117725E-15, -6.982962677686266711E-15, 1.000000000000000000 ) ) ;
#142737 = FACE_OUTER_BOUND ( 'NONE', #80034, .T. ) ;
#142738 = DIRECTION ( 'NONE',  ( 1.000000000000000000, 0.000000000000000000, 0.000000000000000000 ) ) ;
#142739 = DIRECTION ( 'NONE',  ( 1.000000000000000000, 0.000000000000000000, 0.000000000000000000 ) ) ;
#142740 = EDGE_CURVE ( 'NONE', #103735, #5222, #254138, .T. ) ;
#142741 = DIRECTION ( 'NONE',  ( 0.000000000000000000, 0.000000000000000000, -1.000000000000000000 ) ) ;
#142742 = DIRECTION ( 'NONE',  ( 0.000000000000000000, -1.000000000000000000, 0.000000000000000000 ) ) ;
#142744 = ORIENTED_EDGE ( 'NONE', *, *, #116453, .F. ) ;
#142743 = DIRECTION ( 'NONE',  ( -0.000000000000000000, 0.8660254037844377084, 0.5000000000000016653 ) ) ;
#142746 = EDGE_LOOP ( 'NONE', ( #214753, #248328, #204255, #201274 ) ) ;
#142745 = CARTESIAN_POINT ( 'NONE',  ( 23.14999999999999858, 1.115600667400684642E-11, -100.5000000000000426 ) ) ;
#142747 = EDGE_LOOP ( 'NONE', ( #15874, #255350, #181976, #32863, #116435 ) ) ;
#142748 = DIRECTION ( 'NONE',  ( -0.000000000000000000, -0.000000000000000000, -1.000000000000000000 ) ) ;
#142749 = VECTOR ( 'NONE', #137757, 1000.000000000000000 ) ;
#142750 = B_SPLINE_CURVE_WITH_KNOTS ( 'NONE', 3,
 ( #22681, #97012, #140008, #138706, #1788, #78755, #200014, #102153 ),
 .UNSPECIFIED., .F., .F.,
 ( 4, 2, 2, 4 ),
 ( 0.000000000000000000, 9.550056980121915124E-05, 0.0001910011396024383025, 0.0003820022792049600885 ),
 .UNSPECIFIED. ) ;
#142751 = FACE_OUTER_BOUND ( 'NONE', #133983, .T. ) ;
#142752 = CIRCLE ( 'NONE', #30363, 0.1000000000000000888 ) ;
#142753 = CARTESIAN_POINT ( 'NONE',  ( 18.39999999999999503, 67.23581240663841641, -214.2531594801197627 ) ) ;
#142754 = DIRECTION ( 'NONE',  ( 0.000000000000000000, 0.9126074666063765939, 0.4088369013363289950 ) ) ;
#142755 = CARTESIAN_POINT ( 'NONE',  ( -20.94999999999999929, 74.98773774893902555, -233.8732236541320333 ) ) ;
#142756 = ORIENTED_EDGE ( 'NONE', *, *, #206628, .F. ) ;
#142757 = FACE_OUTER_BOUND ( 'NONE', #22916, .T. ) ;
#142758 = ORIENTED_EDGE ( 'NONE', *, *, #128557, .T. ) ;
#142759 = EDGE_LOOP ( 'NONE', ( #130788, #82881, #206627, #42705 ) ) ;
#142760 = CARTESIAN_POINT ( 'NONE',  ( 20.73486653747090003, 52.72272256579930172, -234.4105091754867658 ) ) ;
#142761 = ORIENTED_EDGE ( 'NONE', *, *, #52697, .F. ) ;
#142762 = DIRECTION ( 'NONE',  ( 0.000000000000000000, 0.000000000000000000, -1.000000000000000000 ) ) ;
#142763 = AXIS2_PLACEMENT_3D ( 'NONE', #53869, #249512, #90413 ) ;
#142764 = CARTESIAN_POINT ( 'NONE',  ( 20.94999999999999929, -8.999999999988842703, -91.10603087734760663 ) ) ;
#142765 = ORIENTED_EDGE ( 'NONE', *, *, #182195, .T. ) ;
#142766 = EDGE_CURVE ( 'NONE', #60596, #202492, #198019, .T. ) ;
#142767 = CARTESIAN_POINT ( 'NONE',  ( -16.94132844910799918, 66.00756324483191406, -149.1269057285421411 ) ) ;
#142768 = ORIENTED_EDGE ( 'NONE', *, *, #232400, .T. ) ;
#142769 = CARTESIAN_POINT ( 'NONE',  ( -13.54795643572458452, 9.450668889178684751, -48.55554649020736235 ) ) ;
#142770 = ORIENTED_EDGE ( 'NONE', *, *, #139451, .T. ) ;
#142771 = CARTESIAN_POINT ( 'NONE',  ( 18.49999999999999645, 1.115600667400684642E-11, -100.5000000000000284 ) ) ;
#142772 = ORIENTED_EDGE ( 'NONE', *, *, #91717, .F. ) ;
#142774 = DIRECTION ( 'NONE',  ( 0.000000000000000000, 0.000000000000000000, 1.000000000000000000 ) ) ;
#142773 = AXIS2_PLACEMENT_3D ( 'NONE', #160979, #80097, #22763 ) ;
#142776 = ORIENTED_EDGE ( 'NONE', *, *, #4381, .F. ) ;
#142775 = DIRECTION ( 'NONE',  ( 0.000000000000000000, -1.000000000000000000, 0.000000000000000000 ) ) ;
#142777 = EDGE_CURVE ( 'NONE', #205, #249334, #40332, .T. ) ;
#142778 = DIRECTION ( 'NONE',  ( -0.5932847527679298016, 0.8049926720990051576, 0.000000000000000000 ) ) ;
#142779 = VERTEX_POINT ( 'NONE', #19402 ) ;
#142780 = AXIS2_PLACEMENT_3D ( 'NONE', #85628, #84328, #204319 ) ;
#142781 = AXIS2_PLACEMENT_3D ( 'NONE', #158684, #217315, #154827 ) ;
#142782 = DIRECTION ( 'NONE',  ( 0.000000000000000000, -0.9998779222360104635, -0.01562499999996343723 ) ) ;
#142783 = EDGE_LOOP ( 'NONE', ( #119809, #125778, #57798, #44967 ) ) ;
#142784 = DIRECTION ( 'NONE',  ( 0.000000000000000000, -1.000000000000000000, 0.000000000000000000 ) ) ;
#142785 = CARTESIAN_POINT ( 'NONE',  ( 19.75857864376268935, 64.25000000001250555, -178.7731074845244450 ) ) ;
#142786 = CARTESIAN_POINT ( 'NONE',  ( 22.39999999999999858, 75.90000000001242597, -177.8138870828977360 ) ) ;
#142787 = LINE ( 'NONE', #238054, #85283 ) ;
#142788 = CARTESIAN_POINT ( 'NONE',  ( -15.75000000000000355, 66.65000000001258229, -187.0015881126992952 ) ) ;
#142789 = CONICAL_SURFACE ( 'NONE', #30416, 4.000000000000000000, 0.7853981633974489451 ) ;
#142790 = ORIENTED_EDGE ( 'NONE', *, *, #127365, .T. ) ;
#142791 = VECTOR ( 'NONE', #201822, 1000.000000000000114 ) ;
#142792 = FACE_OUTER_BOUND ( 'NONE', #35715, .T. ) ;
#142793 = DIRECTION ( 'NONE',  ( 1.000000000000000000, 0.000000000000000000, 0.000000000000000000 ) ) ;
#142794 = CARTESIAN_POINT ( 'NONE',  ( 21.05000000000000071, 6.299230910098046365, -100.4015625000000398 ) ) ;
#142795 = EDGE_LOOP ( 'NONE', ( #200875, #138469, #191340, #142854, #10505, #225985, #201484 ) ) ;
#142796 = CARTESIAN_POINT ( 'NONE',  ( 20.94403535211772294, 68.04082873524789932, -224.1991862745062178 ) ) ;
#142797 = ORIENTED_EDGE ( 'NONE', *, *, #45184, .T. ) ;
#142798 = CARTESIAN_POINT ( 'NONE',  ( 14.22821877134046709, 9.456028260519074635, -115.5111980350658030 ) ) ;
#142799 = ORIENTED_EDGE ( 'NONE', *, *, #116562, .F. ) ;
#142800 = CARTESIAN_POINT ( 'NONE',  ( 23.40000000000005542, 77.83551161375991967, -47.52760213295649550 ) ) ;
#142801 = CARTESIAN_POINT ( 'NONE',  ( -18.44085059012132177, 64.48598750652871558, -179.2828021654028987 ) ) ;
#142803 = ORIENTED_EDGE ( 'NONE', *, *, #117147, .T. ) ;
#142802 = CIRCLE ( 'NONE', #42891, 0.1000000000000013933 ) ;
#142805 = EDGE_LOOP ( 'NONE', ( #224766, #139020, #211684, #159636 ) ) ;
#142804 = DIRECTION ( 'NONE',  ( -1.000000000000000000, -3.190570557967288949E-16, -6.948722487160392945E-17 ) ) ;
#142806 = PLANE ( 'NONE',  #250557 ) ;
#142807 = ORIENTED_EDGE ( 'NONE', *, *, #77049, .T. ) ;
#142808 = DIRECTION ( 'NONE',  ( 0.000000000000000000, 0.8814952561688437216, -0.4721928772777334582 ) ) ;
#142809 = AXIS2_PLACEMENT_3D ( 'NONE', #13246, #91488, #111044 ) ;
#142811 = EDGE_CURVE ( 'NONE', #64683, #178434, #190330, .T. ) ;
#142810 = CIRCLE ( 'NONE', #9558, 7.720710678118678061 ) ;
#142812 = DIRECTION ( 'NONE',  ( 1.000000000000000000, 0.000000000000000000, 0.000000000000000000 ) ) ;
#142813 = VERTEX_POINT ( 'NONE', #115935 ) ;
#142814 = CIRCLE ( 'NONE', #138545, 11.70000000000000284 ) ;
#142815 = ORIENTED_EDGE ( 'NONE', *, *, #157063, .F. ) ;
#142816 = CARTESIAN_POINT ( 'NONE',  ( -23.25000000000000355, 20.83093076766827423, -227.7429161672744442 ) ) ;
#142817 = CARTESIAN_POINT ( 'NONE',  ( -16.94878442675511820, 14.20790807310963899, -219.2835367392106889 ) ) ;
#142818 = CARTESIAN_POINT ( 'NONE',  ( -23.15000000000000213, 11.75000000001116263, -45.65000000000000568 ) ) ;
#142819 = EDGE_LOOP ( 'NONE', ( #123535, #134092, #252580, #2677 ) ) ;
#142820 = VERTEX_POINT ( 'NONE', #58497 ) ;
#142821 = DIRECTION ( 'NONE',  ( -1.000000000000000000, 0.000000000000000000, -0.000000000000000000 ) ) ;
#142822 = EDGE_CURVE ( 'NONE', #158502, #233103, #94443, .T. ) ;
#142823 = B_SPLINE_CURVE_WITH_KNOTS ( 'NONE', 3,
 ( #185893, #86775, #200330, #166372, #140339, #219886, #21701, #150626 ),
 .UNSPECIFIED., .F., .F.,
 ( 4, 2, 2, 4 ),
 ( 0.000000000000000000, 0.0001049670497869903125, 0.0002099340995739806251, 0.0004198681991480121534 ),
 .UNSPECIFIED. ) ;
#142824 = EDGE_CURVE ( 'NONE', #162495, #248548, #252658, .T. ) ;
#142826 = EDGE_LOOP ( 'NONE', ( #203645, #147400, #34188, #158960, #235680 ) ) ;
#142825 = CARTESIAN_POINT ( 'NONE',  ( -16.78493832629887450, 9.945835743215301505, -46.16394901910420856 ) ) ;
#142827 = CARTESIAN_POINT ( 'NONE',  ( -22.57320508075687115, 11.38316329224760892, -198.5208684056144364 ) ) ;
#142828 = DIRECTION ( 'NONE',  ( 0.000000000000000000, -0.9126074666063660468, -0.4088369013363524762 ) ) ;
#142830 = CARTESIAN_POINT ( 'NONE',  ( -23.25000000000000000, 76.00000000001170974, -69.52310748452431710 ) ) ;
#142829 = CARTESIAN_POINT ( 'NONE',  ( -20.15000000000000568, 66.70857864377528301, -191.1731074845244223 ) ) ;
#142831 = CARTESIAN_POINT ( 'NONE',  ( 21.05000000000000071, 10.56271494673975120, -107.9568021056449680 ) ) ;
#142832 = DIRECTION ( 'NONE',  ( 1.000000000000000000, -2.952720810173289112E-16, -2.061873921506763405E-30 ) ) ;
#142833 = VECTOR ( 'NONE', #133303, 1000.000000000000000 ) ;
#142834 = EDGE_CURVE ( 'NONE', #156131, #192659, #123879, .T. ) ;
#142835 = CARTESIAN_POINT ( 'NONE',  ( -23.15000000000000213, -8.729782940176420425, -238.4538547387928986 ) ) ;
#142836 = CARTESIAN_POINT ( 'NONE',  ( 18.59999999999999076, 11.65000000001115943, -58.35000000000000142 ) ) ;
#142837 = ORIENTED_EDGE ( 'NONE', *, *, #103107, .T. ) ;
#142838 = AXIS2_PLACEMENT_3D ( 'NONE', #33202, #214362, #189667 ) ;
#142839 = ORIENTED_EDGE ( 'NONE', *, *, #162498, .F. ) ;
#142841 = PLANE ( 'NONE',  #14688 ) ;
#142840 = CIRCLE ( 'NONE', #88687, 12.87500000000000000 ) ;
#142842 = VERTEX_POINT ( 'NONE', #234587 ) ;
#142843 = EDGE_CURVE ( 'NONE', #205018, #67554, #115471, .T. ) ;
#142844 = CARTESIAN_POINT ( 'NONE',  ( -23.25000000000000000, 23.68770167995059595, -252.8127582590406348 ) ) ;
#142845 = AXIS2_PLACEMENT_3D ( 'NONE', #37156, #98344, #80068 ) ;
#142846 = ORIENTED_EDGE ( 'NONE', *, *, #30230, .T. ) ;
#142848 = ADVANCED_FACE ( 'NONE', ( #174673 ), #111392, .T. ) ;
#142847 = VECTOR ( 'NONE', #210498, 1000.000000000000000 ) ;
#142849 = DIRECTION ( 'NONE',  ( 0.000000000000000000, 0.000000000000000000, -1.000000000000000000 ) ) ;
#142850 = AXIS2_PLACEMENT_3D ( 'NONE', #37389, #13969, #235556 ) ;
#142852 = ORIENTED_EDGE ( 'NONE', *, *, #230109, .F. ) ;
#142851 = EDGE_LOOP ( 'NONE', ( #199010, #104604 ) ) ;
#142853 = CARTESIAN_POINT ( 'NONE',  ( -21.44999999999999929, 9.788464569039593499, -211.4053333142630891 ) ) ;
#142854 = ORIENTED_EDGE ( 'NONE', *, *, #166826, .T. ) ;
#142855 = ORIENTED_EDGE ( 'NONE', *, *, #102890, .T. ) ;
#142856 = CARTESIAN_POINT ( 'NONE',  ( 20.94999999999999929, 71.18691588786276725, -158.0815897280005800 ) ) ;
#142857 = CARTESIAN_POINT ( 'NONE',  ( -21.08035267497491816, 75.91731137523596828, -109.3548143243073554 ) ) ;
#142859 = VERTEX_POINT ( 'NONE', #257953 ) ;
#142858 = DIRECTION ( 'NONE',  ( 1.000000000000000000, -0.000000000000000000, -0.000000000000000000 ) ) ;
#142860 = CARTESIAN_POINT ( 'NONE',  ( 20.88420186297724257, 65.66974365629666011, -97.43601455626048846 ) ) ;
#142862 = EDGE_LOOP ( 'NONE', ( #251531, #20906, #86964, #222434 ) ) ;
#142861 = DIRECTION ( 'NONE',  ( 0.7071067811865474617, 0.2890913453342131012, -0.6453109281988449464 ) ) ;
#142863 = CARTESIAN_POINT ( 'NONE',  ( -22.42357213249529124, 0.09908696401271366305, -59.32706761364011072 ) ) ;
#142864 = ORIENTED_EDGE ( 'NONE', *, *, #171881, .F. ) ;
#142865 = DIRECTION ( 'NONE',  ( 1.000000000000000000, 0.000000000000000000, -0.000000000000000000 ) ) ;
#142866 = AXIS2_PLACEMENT_3D ( 'NONE', #160634, #143603, #21120 ) ;
#142869 = EDGE_CURVE ( 'NONE', #153832, #45216, #140413, .T. ) ;
#142868 = ORIENTED_EDGE ( 'NONE', *, *, #6136, .F. ) ;
#142867 = DIRECTION ( 'NONE',  ( 1.000000000000000000, 0.000000000000000000, 0.000000000000000000 ) ) ;
#142870 = CIRCLE ( 'NONE', #188685, 0.09999999999999950595 ) ;
#142871 = CARTESIAN_POINT ( 'NONE',  ( 23.25000000000000000, 87.48912529308749697, -39.12310748452424747 ) ) ;
#142872 = CARTESIAN_POINT ( 'NONE',  ( -18.59999999999999787, 0.6770221356676882074, -212.8807256103264649 ) ) ;
#142873 = CARTESIAN_POINT ( 'NONE',  ( 18.59999999999999432, 74.36282728704118483, -57.94095411905231430 ) ) ;
#142874 = ORIENTED_EDGE ( 'NONE', *, *, #146384, .F. ) ;
#142875 = AXIS2_PLACEMENT_3D ( 'NONE', #101752, #138320, #178802 ) ;
#142877 = DIRECTION ( 'NONE',  ( 0.000000000000000000, -0.6855225566104692358, -0.7280513885559494192 ) ) ;
#142876 = DIRECTION ( 'NONE',  ( -1.000000000000000000, -0.000000000000000000, -0.000000000000000000 ) ) ;
#142878 = DIRECTION ( 'NONE',  ( -1.000000000000000000, -0.000000000000000000, -0.000000000000000000 ) ) ;
#142879 = DIRECTION ( 'NONE',  ( 0.000000000000000000, 0.000000000000000000, -1.000000000000000000 ) ) ;
#142880 = DIRECTION ( 'NONE',  ( -0.7071067811865475727, 0.7071067811865475727, 4.937700262164531476E-15 ) ) ;
#142882 = ORIENTED_EDGE ( 'NONE', *, *, #94653, .F. ) ;
#142881 = AXIS2_PLACEMENT_3D ( 'NONE', #212133, #11356, #153481 ) ;
#142883 = ORIENTED_EDGE ( 'NONE', *, *, #57563, .F. ) ;
#142885 = ORIENTED_EDGE ( 'NONE', *, *, #81664, .F. ) ;
#142884 = CIRCLE ( 'NONE', #97074, 0.09999999999999892308 ) ;
#142886 = EDGE_CURVE ( 'NONE', #207337, #211613, #65594, .T. ) ;
#142887 = LINE ( 'NONE', #46363, #180620 ) ;
#142888 = CIRCLE ( 'NONE', #59492, 4.000000000000006217 ) ;
#142889 = EDGE_LOOP ( 'NONE', ( #50263, #249934, #157659, #221672 ) ) ;
#142890 = CARTESIAN_POINT ( 'NONE',  ( 18.49999999999999289, 10.20857864377385127, -55.25000000000004974 ) ) ;
#142891 = EDGE_LOOP ( 'NONE', ( #46288, #150453, #8880, #45426 ) ) ;
#142892 = LINE ( 'NONE', #161212, #102646 ) ;
#142893 = CARTESIAN_POINT ( 'NONE',  ( -18.37013991200266005, 16.40593182862863131, -222.2894472230003942 ) ) ;
#142894 = ADVANCED_FACE ( 'NONE', ( #217570 ), #220168, .T. ) ;
#142895 = ORIENTED_EDGE ( 'NONE', *, *, #132512, .F. ) ;
#142896 = CARTESIAN_POINT ( 'NONE',  ( 12.26145404764309355, 9.351413679112544841, -150.9803435675490277 ) ) ;
#142897 = EDGE_CURVE ( 'NONE', #168999, #176585, #18108, .T. ) ;
#142898 = CIRCLE ( 'NONE', #97096, 3.999999999999989786 ) ;
#142899 = CIRCLE ( 'NONE', #205453, 0.1000000000000028644 ) ;
#142900 = EDGE_CURVE ( 'NONE', #131204, #207133, #235862, .T. ) ;
#142901 = ORIENTED_EDGE ( 'NONE', *, *, #248969, .T. ) ;
#142902 = AXIS2_PLACEMENT_3D ( 'NONE', #232946, #54267, #133808 ) ;
#142904 = VERTEX_POINT ( 'NONE', #46635 ) ;
#142903 = AXIS2_PLACEMENT_3D ( 'NONE', #89903, #32550, #72958 ) ;
#142905 = ORIENTED_EDGE ( 'NONE', *, *, #93427, .F. ) ;
#142906 = FACE_OUTER_BOUND ( 'NONE', #120198, .T. ) ;
#142907 = DIRECTION ( 'NONE',  ( 0.000000000000000000, 0.000000000000000000, -1.000000000000000000 ) ) ;
#142908 = CARTESIAN_POINT ( 'NONE',  ( 21.05000000000000071, 1.115600667400684642E-11, -202.9999999999999716 ) ) ;
#142909 = CARTESIAN_POINT ( 'NONE',  ( -18.37160782347004329, 20.70136879309603728, -227.9847839959967075 ) ) ;
#142910 = CARTESIAN_POINT ( 'NONE',  ( -2.995603634470891112E-16, 87.75000000001220712, -145.2731074845242745 ) ) ;
#142911 = CARTESIAN_POINT ( 'NONE',  ( -20.54999999999999716, 11.43341603104965110, -245.8667934851861787 ) ) ;
#142912 = ADVANCED_FACE ( 'NONE', ( #181056 ), #242279, .T. ) ;
#142913 = DIRECTION ( 'NONE',  ( 1.000000000000000000, 0.000000000000000000, 0.000000000000000000 ) ) ;
#142914 = DIRECTION ( 'NONE',  ( 1.186688945009009831E-16, -0.4721928772777346239, -0.8814952561688430555 ) ) ;
#142916 = ORIENTED_EDGE ( 'NONE', *, *, #109434, .F. ) ;
#142915 = DIRECTION ( 'NONE',  ( -0.000000000000000000, -1.000000000000000000, -6.982962677686266711E-15 ) ) ;
#142918 = DIRECTION ( 'NONE',  ( 0.000000000000000000, -0.2617529984165024026, -0.9651348961777158619 ) ) ;
#142917 = CARTESIAN_POINT ( 'NONE',  ( -21.05439746398122836, 11.75000000001115197, -40.48991648748479122 ) ) ;
#142919 = DIRECTION ( 'NONE',  ( 0.000000000000000000, 0.000000000000000000, 1.000000000000000000 ) ) ;
#142920 = ORIENTED_EDGE ( 'NONE', *, *, #10280, .F. ) ;
#142921 = DIRECTION ( 'NONE',  ( 0.000000000000000000, -0.2617529984163859957, -0.9651348961777475033 ) ) ;
#142922 = CARTESIAN_POINT ( 'NONE',  ( -21.07928932188134041, 69.67148334361836248, -69.62200263017875557 ) ) ;
#142924 = EDGE_CURVE ( 'NONE', #58200, #76073, #257082, .T. ) ;
#142923 = CARTESIAN_POINT ( 'NONE',  ( -20.05000000000000426, 30.14024212288317628, -235.5657495473015501 ) ) ;
#142926 = EDGE_CURVE ( 'NONE', #78551, #86393, #104036, .T. ) ;
#142925 = ORIENTED_EDGE ( 'NONE', *, *, #21284, .F. ) ;
#142927 = CARTESIAN_POINT ( 'NONE',  ( 23.04999999999999716, 8.822561741666397950, -20.84999999999999432 ) ) ;
#142928 = DIRECTION ( 'NONE',  ( -7.304098846218419643E-16, 0.9770955615653543758, 0.2128009952262553683 ) ) ;
#142929 = EDGE_LOOP ( 'NONE', ( #93135, #108735, #93546, #105337 ) ) ;
#142930 = ORIENTED_EDGE ( 'NONE', *, *, #181960, .F. ) ;
#142931 = EDGE_CURVE ( 'NONE', #21663, #23059, #48837, .T. ) ;
#142932 = CIRCLE ( 'NONE', #30553, 7.720710678118671844 ) ;
#142933 = DIRECTION ( 'NONE',  ( 0.000000000000000000, 0.000000000000000000, 1.000000000000000000 ) ) ;
#142934 = VERTEX_POINT ( 'NONE', #25814 ) ;
#142935 = DIRECTION ( 'NONE',  ( 0.000000000000000000, 0.9987946567507778317, -0.04908394489133698774 ) ) ;
#142936 = CARTESIAN_POINT ( 'NONE',  ( 21.05000000000000071, -1.849084418627015891, -11.65601052144712391 ) ) ;
#142937 = CARTESIAN_POINT ( 'NONE',  ( -23.25000000000000000, -11.74999999998884448, -155.7499999999999716 ) ) ;
#142939 = EDGE_CURVE ( 'NONE', #165343, #133931, #183608, .T. ) ;
#142938 = CARTESIAN_POINT ( 'NONE',  ( -21.05000000000000071, 69.45934304831071415, -102.9231074845243512 ) ) ;
#142940 = VERTEX_POINT ( 'NONE', #64927 ) ;
#142941 = EDGE_CURVE ( 'NONE', #106325, #143460, #62378, .T. ) ;
#142942 = CARTESIAN_POINT ( 'NONE',  ( -23.15000000000000213, 4.350000000011156054, -188.6499999999999488 ) ) ;
#142943 = DIRECTION ( 'NONE',  ( -1.000000000000000000, -0.000000000000000000, -0.000000000000000000 ) ) ;
#142944 = DIRECTION ( 'NONE',  ( -1.000000000000000000, -3.265361837132813093E-16, 0.000000000000000000 ) ) ;
#142945 = LINE ( 'NONE', #67285, #124100 ) ;
#142947 = ORIENTED_EDGE ( 'NONE', *, *, #102570, .T. ) ;
#142946 = TOROIDAL_SURFACE ( 'NONE', #92896, 7.800000000000000711, 0.1000000000000000056 ) ;
#142949 = ORIENTED_EDGE ( 'NONE', *, *, #125030, .T. ) ;
#142948 = CARTESIAN_POINT ( 'NONE',  ( 21.05000000000000071, -11.48912529306489994, -197.8999999999999773 ) ) ;
#142950 = EDGE_CURVE ( 'NONE', #44801, #229458, #244001, .T. ) ;
#142951 = CYLINDRICAL_SURFACE ( 'NONE', #30964, 0.1000000000000028644 ) ;
#142952 = CARTESIAN_POINT ( 'NONE',  ( 18.59999999999999787, 78.12133356376092763, -231.3112718935514920 ) ) ;
#142953 = EDGE_CURVE ( 'NONE', #135978, #155156, #23931, .T. ) ;
#142954 = DIRECTION ( 'NONE',  ( -0.000000000000000000, 0.9651348961777157509, -0.2617529984165031243 ) ) ;
#142955 = DIRECTION ( 'NONE',  ( -0.4999999999999799050, 0.1842910678166416460, -0.8461895782406104738 ) ) ;
#142956 = LINE ( 'NONE', #245946, #221639 ) ;
#142957 = CARTESIAN_POINT ( 'NONE',  ( 20.94999999999999929, 5.500000000011153745, -188.5947339810868755 ) ) ;
#142958 = ORIENTED_EDGE ( 'NONE', *, *, #14339, .T. ) ;
#142959 = CARTESIAN_POINT ( 'NONE',  ( -16.77779411503078322, 9.946101446935278645, -146.6630574176198536 ) ) ;
#142960 = CARTESIAN_POINT ( 'NONE',  ( 15.31784899511109543, 9.396630376328870327, -51.40705739281828812 ) ) ;
#142961 = CARTESIAN_POINT ( 'NONE',  ( 21.14999999999999503, 1.115600667400684642E-11, -67.00000000000004263 ) ) ;
#142962 = EDGE_CURVE ( 'NONE', #119379, #238460, #123638, .T. ) ;
#142963 = VECTOR ( 'NONE', #42017, 1000.000000000000000 ) ;
#142964 = DIRECTION ( 'NONE',  ( 1.000000000000000000, 0.000000000000000000, 0.000000000000000000 ) ) ;
#142966 = CYLINDRICAL_SURFACE ( 'NONE', #165610, 0.09999999999999939493 ) ;
#142965 = CIRCLE ( 'NONE', #30589, 0.1000000000000052097 ) ;
#142967 = EDGE_LOOP ( 'NONE', ( #170809, #181099, #137341, #69615 ) ) ;
#142968 = ORIENTED_EDGE ( 'NONE', *, *, #126028, .F. ) ;
#142969 = CARTESIAN_POINT ( 'NONE',  ( 18.59999999999999787, 77.83585931145498193, -24.51866831572578675 ) ) ;
#142971 = CARTESIAN_POINT ( 'NONE',  ( 20.94999999999999574, 18.18127959618848521, -237.5711165786817389 ) ) ;
#142970 = AXIS2_PLACEMENT_3D ( 'NONE', #176331, #177625, #39396 ) ;
#142972 = CARTESIAN_POINT ( 'NONE',  ( 23.15000000000000213, -9.499999999988848032, -110.3939691226524786 ) ) ;
#142973 = FACE_OUTER_BOUND ( 'NONE', #243828, .T. ) ;
#142974 = ORIENTED_EDGE ( 'NONE', *, *, #34753, .F. ) ;
#142975 = CARTESIAN_POINT ( 'NONE',  ( -20.94999999999999929, 14.05000000001115623, -173.0136950707609458 ) ) ;
#142976 = DIRECTION ( 'NONE',  ( 0.000000000000000000, 0.000000000000000000, 1.000000000000000000 ) ) ;
#142977 = TOROIDAL_SURFACE ( 'NONE', #147290, 3.899999999999999467, 0.1000000000000000056 ) ;
#142978 = EDGE_CURVE ( 'NONE', #133329, #76888, #201883, .T. ) ;
#142979 = AXIS2_PLACEMENT_3D ( 'NONE', #40889, #124261, #239063 ) ;
#142980 = DIRECTION ( 'NONE',  ( 1.000000000000000000, 0.000000000000000000, 0.000000000000000000 ) ) ;
#142981 = AXIS2_PLACEMENT_3D ( 'NONE', #212966, #55137, #95579 ) ;
#142982 = DIRECTION ( 'NONE',  ( 0.000000000000000000, 0.4088369013363062909, -0.9126074666063868079 ) ) ;
#142983 = EDGE_CURVE ( 'NONE', #143470, #199184, #11448, .T. ) ;
#142984 = VERTEX_POINT ( 'NONE', #145743 ) ;
#142985 = FACE_OUTER_BOUND ( 'NONE', #179797, .T. ) ;
#142986 = AXIS2_PLACEMENT_3D ( 'NONE', #146734, #105024, #125906 ) ;
#142987 = EDGE_CURVE ( 'NONE', #86372, #196267, #57191, .T. ) ;
#142988 = EDGE_LOOP ( 'NONE', ( #185003, #231605, #85124, #23978 ) ) ;
#142989 = FACE_OUTER_BOUND ( 'NONE', #65164, .T. ) ;
#142990 = CARTESIAN_POINT ( 'NONE',  ( 21.05000000000000071, 0.09779029130879170195, 6.257814610476124528 ) ) ;
#142991 = CARTESIAN_POINT ( 'NONE',  ( -21.05000000000000071, 9.997527148598553737, -228.1702915402926237 ) ) ;
#142992 = LINE ( 'NONE', #222535, #15863 ) ;
#142994 = VECTOR ( 'NONE', #41692, 1000.000000000000000 ) ;
#142993 = CARTESIAN_POINT ( 'NONE',  ( 23.14999999999999503, 6.650000000011155876, -121.7500000000000426 ) ) ;
#142996 = EDGE_CURVE ( 'NONE', #1074, #165183, #252841, .T. ) ;
#142995 = CARTESIAN_POINT ( 'NONE',  ( -20.93284271247462058, 11.75000000001115019, -193.9851942293460070 ) ) ;
#142998 = CARTESIAN_POINT ( 'NONE',  ( -21.05000000000000071, -1.249999999988843369, -175.4999999999999716 ) ) ;
#142997 = AXIS2_PLACEMENT_3D ( 'NONE', #165598, #245120, #225520 ) ;
#142999 = AXIS2_PLACEMENT_3D ( 'NONE', #227701, #126032, #205564 ) ;
#143000 = CYLINDRICAL_SURFACE ( 'NONE', #189046, 0.09999999999999810429 ) ;
#143002 = DIRECTION ( 'NONE',  ( -1.000000000000000000, 0.000000000000000000, 0.000000000000000000 ) ) ;
#143001 = TOROIDAL_SURFACE ( 'NONE', #247063, 0.2000000000000000111, 0.1000000000000000056 ) ;
#143003 = DIRECTION ( 'NONE',  ( -1.000000000000000000, 2.849773892568378313E-16, -7.728835255496647986E-17 ) ) ;
#143004 = EDGE_CURVE ( 'NONE', #118445, #190257, #148823, .T. ) ;
#143005 = CARTESIAN_POINT ( 'NONE',  ( -11.60000000000000320, -12.25000000000000178, 15.00000000000000355 ) ) ;
#143006 = FACE_BOUND ( 'NONE', #107692, .T. ) ;
#143007 = LINE ( 'NONE', #67348, #162013 ) ;
#143008 = CARTESIAN_POINT ( 'NONE',  ( -20.64999999999999858, 21.43869811404188752, -233.1734427395952025 ) ) ;
#143009 = EDGE_CURVE ( 'NONE', #90553, #178434, #3033, .T. ) ;
#143011 = ADVANCED_FACE ( 'NONE', ( #182335 ), #102752, .T. ) ;
#143010 = EDGE_CURVE ( 'NONE', #223315, #57574, #202964, .T. ) ;
#143012 = ORIENTED_EDGE ( 'NONE', *, *, #211314, .T. ) ;
#143013 = CARTESIAN_POINT ( 'NONE',  ( 18.59999999999999076, 64.35000000001245724, -170.0231074845244166 ) ) ;
#143014 = ORIENTED_EDGE ( 'NONE', *, *, #246573, .T. ) ;
#143015 = CARTESIAN_POINT ( 'NONE',  ( -21.14999999999999858, 11.75000000001115552, -167.4999999999999716 ) ) ;
#143016 = CARTESIAN_POINT ( 'NONE',  ( 21.05281448260627641, 67.22398984147466194, -157.8495495727129878 ) ) ;
#143017 = CARTESIAN_POINT ( 'NONE',  ( -17.78241384947038028, 10.85557575281234044, -190.7509623274730188 ) ) ;
#143018 = AXIS2_PLACEMENT_3D ( 'NONE', #98094, #22471, #78559 ) ;
#143019 = VERTEX_POINT ( 'NONE', #51768 ) ;
#143020 = DIRECTION ( 'NONE',  ( 0.000000000000000000, -7.147358527629766941E-15, 1.000000000000000000 ) ) ;
#143021 = FACE_OUTER_BOUND ( 'NONE', #156393, .T. ) ;
#143022 = CIRCLE ( 'NONE', #97205, 0.09999999999998898659 ) ;
#143024 = ORIENTED_EDGE ( 'NONE', *, *, #68088, .T. ) ;
#143023 = AXIS2_PLACEMENT_3D ( 'NONE', #224185, #6424, #203354 ) ;
#143025 = ADVANCED_FACE ( 'NONE', ( #8821 ), #73956, .T. ) ;
#143026 = EDGE_CURVE ( 'NONE', #143764, #45390, #190530, .T. ) ;
#143027 = EDGE_LOOP ( 'NONE', ( #113771, #245434, #75508, #244546, #136376, #246645, #22489, #189036, #240110, #154946 ) ) ;
#143029 = CARTESIAN_POINT ( 'NONE',  ( 18.59999999999999076, 1.115600667400684642E-11, -100.5000000000000426 ) ) ;
#143028 = CIRCLE ( 'NONE', #238736, 0.1999999999999996503 ) ;
#143030 = EDGE_CURVE ( 'NONE', #22210, #6281, #78054, .T. ) ;
#143031 = AXIS2_PLACEMENT_3D ( 'NONE', #43159, #1442, #219206 ) ;
#143032 = VERTEX_POINT ( 'NONE', #212163 ) ;
#143033 = CARTESIAN_POINT ( 'NONE',  ( -22.39999999999999858, -0.1008583690875579364, -21.75043287651061164 ) ) ;
#143035 =( BOUNDED_SURFACE ( )  B_SPLINE_SURFACE ( 3, 2, ( 
 ( #227451, #168823, #245749 ),
 ( #50100, #26718, #129646 ),
 ( #48820, #146618, #244448 ),
 ( #104906, #30571, #46246 ),
 ( #185771, #226139, #205310 ),
 ( #128373, #209178, #127079 ) ),
 .UNSPECIFIED., .F., .F., .F. ) 
 B_SPLINE_SURFACE_WITH_KNOTS ( ( 4, 2, 4 ),
 ( 3, 3 ),
 ( 0.0001300404313046710908, 0.0003183318589266794407, 0.0005066232865486877636 ),
 ( 0.000000000000000000, 1.000000000000000000 ),
 .UNSPECIFIED. ) 
 GEOMETRIC_REPRESENTATION_ITEM ( )  RATIONAL_B_SPLINE_SURFACE ( (
 ( 1.000000000000000000, 0.7071067811865475727, 1.000000000000000000),
 ( 1.000000000000000000, 0.7625113560541593172, 1.000000000000000000),
 ( 1.000000000000000000, 0.8126073484686597848, 1.000000000000000000),
 ( 1.000000000000000000, 0.8923049332734360739, 1.000000000000000000),
 ( 1.000000000000000000, 0.9231914937768189722, 1.000000000000000000),
 ( 1.000000000000000000, 0.9238795325112911794, 1.000000000000000000) ) ) 
 REPRESENTATION_ITEM ( '' )  SURFACE ( )  );
#143034 = CARTESIAN_POINT ( 'NONE',  ( 21.05000000000000071, 4.813084112160684214, -155.5584822434762202 ) ) ;
#143036 = EDGE_CURVE ( 'NONE', #103428, #7914, #132236, .T. ) ;
#143037 = CARTESIAN_POINT ( 'NONE',  ( -21.05000000000000071, 69.74218538953626023, -170.1208977758331855 ) ) ;
#143038 = CARTESIAN_POINT ( 'NONE',  ( -20.64999999999999858, 76.00000000001267608, -203.5231074845243597 ) ) ;
#143039 = CARTESIAN_POINT ( 'NONE',  ( -22.39999999999999503, 68.20922040163927136, -203.5231074845244166 ) ) ;
#143040 = DIRECTION ( 'NONE',  ( -0.000000000000000000, 0.9770955615653313941, 0.2128009952263603954 ) ) ;
#143041 = ADVANCED_FACE ( 'NONE', ( #188729 ), #107910, .F. ) ;
#143042 = CARTESIAN_POINT ( 'NONE',  ( 15.74999999999999645, 47.91805600923871822, -233.7139610577891631 ) ) ;
#143043 = VECTOR ( 'NONE', #240341, 1000.000000000000000 ) ;
#143044 = DIRECTION ( 'NONE',  ( 1.000000000000000000, 0.000000000000000000, 0.000000000000000000 ) ) ;
#143046 = CARTESIAN_POINT ( 'NONE',  ( -20.64999999999999858, 74.00000000001151079, -49.24772940728643533 ) ) ;
#143045 = VECTOR ( 'NONE', #257002, 1000.000000000000000 ) ;
#143047 = AXIS2_PLACEMENT_3D ( 'NONE', #161477, #20680, #98877 ) ;
#143049 = ORIENTED_EDGE ( 'NONE', *, *, #14349, .T. ) ;
#143048 = CYLINDRICAL_SURFACE ( 'NONE', #131748, 0.09999999999999939493 ) ;
#143050 = EDGE_LOOP ( 'NONE', ( #74759, #146627, #102215 ) ) ;
#143052 = FACE_OUTER_BOUND ( 'NONE', #52244, .T. ) ;
#143051 = CARTESIAN_POINT ( 'NONE',  ( 23.14999999999999858, 71.18691588786300883, -181.9646252410481964 ) ) ;
#143053 = VECTOR ( 'NONE', #188112, 1000.000000000000227 ) ;
#143055 = ORIENTED_EDGE ( 'NONE', *, *, #113454, .F. ) ;
#143054 = CARTESIAN_POINT ( 'NONE',  ( -16.83558968593871796, 60.94257868581368598, -221.0298515696131005 ) ) ;
#143056 = ORIENTED_EDGE ( 'NONE', *, *, #120309, .T. ) ;
#143057 = CARTESIAN_POINT ( 'NONE',  ( -22.50000000000000000, 0.1000000000111554016, -155.8504291924551808 ) ) ;
#143058 = CARTESIAN_POINT ( 'NONE',  ( 20.59588692710267921, 10.36872342118052259, -175.1390810945102601 ) ) ;
#143059 = AXIS2_PLACEMENT_3D ( 'NONE', #145345, #68393, #201466 ) ;
#143060 = CARTESIAN_POINT ( 'NONE',  ( 18.49999999999999645, -1.362429037182155023, -108.3888812479212476 ) ) ;
#143061 = CARTESIAN_POINT ( 'NONE',  ( 20.85000000000000142, 64.25000000001244871, -170.0231074845244166 ) ) ;
#143062 = EDGE_CURVE ( 'NONE', #189304, #40848, #111773, .T. ) ;
#143063 = CARTESIAN_POINT ( 'NONE',  ( 13.99999999999999822, 26.54497872210689735, -232.9592037335782209 ) ) ;
#143064 = LINE ( 'NONE', #238327, #227817 ) ;
#143065 = EDGE_CURVE ( 'NONE', #61601, #65298, #244654, .T. ) ;
#143066 = VECTOR ( 'NONE', #97592, 1000.000000000000000 ) ;
#143067 = VERTEX_POINT ( 'NONE', #231727 ) ;
#143068 = ORIENTED_EDGE ( 'NONE', *, *, #2542, .T. ) ;
#143069 = DIRECTION ( 'NONE',  ( 0.7071067811865463515, 0.7071067811865487940, 4.937700262164540154E-15 ) ) ;
#143070 = VERTEX_POINT ( 'NONE', #248713 ) ;
#143071 = DIRECTION ( 'NONE',  ( 0.000000000000000000, -6.467318590049456648E-15, 1.000000000000000000 ) ) ;
#143072 = ORIENTED_EDGE ( 'NONE', *, *, #58873, .T. ) ;
#143074 = AXIS2_PLACEMENT_3D ( 'NONE', #102402, #180706, #236804 ) ;
#143073 = FACE_OUTER_BOUND ( 'NONE', #109931, .T. ) ;
#143075 =( BOUNDED_SURFACE ( )  B_SPLINE_SURFACE ( 3, 2, ( 
 ( #94325, #173926, #74816 ),
 ( #89191, #248277, #69656 ),
 ( #19954, #99446, #21254 ),
 ( #100715, #362, #76052 ) ),
 .UNSPECIFIED., .F., .F., .F. ) 
 B_SPLINE_SURFACE_WITH_KNOTS ( ( 4, 4 ),
 ( 3, 3 ),
 ( 0.0008258556059633901563, 0.0009616864997632837159 ),
 ( 0.000000000000000000, 1.000000000000000000 ),
 .UNSPECIFIED. ) 
 GEOMETRIC_REPRESENTATION_ITEM ( )  RATIONAL_B_SPLINE_SURFACE ( (
 ( 1.000000000000000000, 0.9152888060719349683, 1.000000000000000000),
 ( 1.000000000000000000, 0.9327727094138192898, 1.000000000000000000),
 ( 1.000000000000000000, 0.9369023509258407323, 1.000000000000000000),
 ( 1.000000000000000000, 0.9246339933864529126, 1.000000000000000000) ) ) 
 REPRESENTATION_ITEM ( '' )  SURFACE ( )  );
#143076 = AXIS2_PLACEMENT_3D ( 'NONE', #53965, #233891, #158249 ) ;
#143077 = VECTOR ( 'NONE', #198463, 1000.000000000000000 ) ;
#143078 = LINE ( 'NONE', #247322, #226068 ) ;
#143079 = ADVANCED_FACE ( 'NONE', ( #92192 ), #130023, .F. ) ;
#143080 = CARTESIAN_POINT ( 'NONE',  ( 18.49999999999999289, 65.76093837589000657, -44.76871004992742087 ) ) ;
#143081 = DIRECTION ( 'NONE',  ( 0.000000000000000000, -1.000000000000000000, 0.000000000000000000 ) ) ;
#143082 = ORIENTED_EDGE ( 'NONE', *, *, #16731, .T. ) ;
#143083 = DIRECTION ( 'NONE',  ( -1.000000000000000000, -7.304098846218134667E-16, -5.311601492717084346E-30 ) ) ;
#143084 = ORIENTED_EDGE ( 'NONE', *, *, #53905, .F. ) ;
#143085 = CARTESIAN_POINT ( 'NONE',  ( 22.49436431346199683, 0.06690352973341695542, -122.3500490523465629 ) ) ;
#143086 = CARTESIAN_POINT ( 'NONE',  ( -20.85000000000000142, 18.41524492703433680, -237.0006385043383830 ) ) ;
#143087 = DIRECTION ( 'NONE',  ( -1.000000000000000000, 0.000000000000000000, -0.000000000000000000 ) ) ;
#143088 = FACE_OUTER_BOUND ( 'NONE', #248167, .T. ) ;
#143089 = ORIENTED_EDGE ( 'NONE', *, *, #141241, .F. ) ;
#143090 = CARTESIAN_POINT ( 'NONE',  ( -21.12844524849339223, 64.25000000001189449, -96.11869401368159060 ) ) ;
#143091 = CIRCLE ( 'NONE', #97272, 0.09999999999999993616 ) ;
#143092 = ORIENTED_EDGE ( 'NONE', *, *, #97645, .T. ) ;
#143095 = ORIENTED_EDGE ( 'NONE', *, *, #7214, .T. ) ;
#143094 = CARTESIAN_POINT ( 'NONE',  ( 23.24999999999999645, 76.00000000001213607, -136.5231074845242745 ) ) ;
#143093 = CARTESIAN_POINT ( 'NONE',  ( 23.15000000000000213, 84.59626168225447884, -45.47323500167454569 ) ) ;
#143096 = CIRCLE ( 'NONE', #84623, 11.65000000000000391 ) ;
#143097 = EDGE_CURVE ( 'NONE', #215553, #254300, #53120, .T. ) ;
#143098 = AXIS2_PLACEMENT_3D ( 'NONE', #145360, #30585, #204052 ) ;
#143099 = DIRECTION ( 'NONE',  ( 0.000000000000000000, 1.000000000000000000, -0.000000000000000000 ) ) ;
#143100 = AXIS2_PLACEMENT_3D ( 'NONE', #221391, #166610, #244816 ) ;
#143101 = ORIENTED_EDGE ( 'NONE', *, *, #131986, .T. ) ;
#143102 = FACE_OUTER_BOUND ( 'NONE', #241533, .T. ) ;
#143103 = ORIENTED_EDGE ( 'NONE', *, *, #197515, .T. ) ;
#143104 = CARTESIAN_POINT ( 'NONE',  ( 21.07016717457012689, 76.00000000001219291, -142.8440483226252127 ) ) ;
#143105 = CARTESIAN_POINT ( 'NONE',  ( -16.94132844910802405, 9.992436755191501874, -54.39620175598232521 ) ) ;
#143106 = DIRECTION ( 'NONE',  ( -1.000000000000000000, -0.000000000000000000, 0.000000000000000000 ) ) ;
#143107 = LINE ( 'NONE', #201808, #185089 ) ;
#143108 = CARTESIAN_POINT ( 'NONE',  ( -20.00857864376270001, 66.85000000001150511, -48.37310748452438247 ) ) ;
#143109 = VERTEX_POINT ( 'NONE', #149632 ) ;
#143110 = CARTESIAN_POINT ( 'NONE',  ( 18.39999999999999503, 11.47316190337363828, -180.1499999999999773 ) ) ;
#143111 = CARTESIAN_POINT ( 'NONE',  ( 21.46681500593416914, 60.61285123220954318, -234.0601523988351857 ) ) ;
#143112 = CARTESIAN_POINT ( 'NONE',  ( -14.56556274378147897, 66.55344247693973614, -154.9331655301785133 ) ) ;
#143113 = ORIENTED_EDGE ( 'NONE', *, *, #15947, .T. ) ;
#143114 = DIRECTION ( 'NONE',  ( 0.000000000000000000, -0.9651348961777157509, 0.2617529984165031243 ) ) ;
#143115 = VERTEX_POINT ( 'NONE', #152209 ) ;
#143116 = CARTESIAN_POINT ( 'NONE',  ( 20.94999999999999929, 5.500000000011153745, -79.40526601891313874 ) ) ;
#143117 = AXIS2_PLACEMENT_3D ( 'NONE', #30195, #169727, #92703 ) ;
#143118 = CARTESIAN_POINT ( 'NONE',  ( -21.05000000000000071, -11.74999999998884448, -64.00000000000000000 ) ) ;
#143119 = CARTESIAN_POINT ( 'NONE',  ( -23.15000000000000213, 4.250000000011156409, -54.75000000000000000 ) ) ;
#143121 = ORIENTED_EDGE ( 'NONE', *, *, #53452, .F. ) ;
#143120 = FACE_OUTER_BOUND ( 'NONE', #112621, .T. ) ;
#143122 = CARTESIAN_POINT ( 'NONE',  ( 18.59999999999999432, 77.73625713160926409, -91.45445515550680682 ) ) ;
#143123 = CARTESIAN_POINT ( 'NONE',  ( 18.49999999999999289, 11.75000000001115907, -55.25000000000004974 ) ) ;
#143124 = ADVANCED_FACE ( 'NONE', ( #150892 ), #148326, .T. ) ;
#143125 = CARTESIAN_POINT ( 'NONE',  ( 23.15000000000000213, 28.15345123516638637, -259.0759448016705733 ) ) ;
#143126 = VERTEX_POINT ( 'NONE', #209588 ) ;
#143127 = DIRECTION ( 'NONE',  ( 0.000000000000000000, -0.4088369013363280513, 0.9126074666063769270 ) ) ;
#143128 = DIRECTION ( 'NONE',  ( 0.000000000000000000, -0.2617529984165033463, -0.9651348961777156399 ) ) ;
#143129 = VERTEX_POINT ( 'NONE', #249996 ) ;
#143131 = CARTESIAN_POINT ( 'NONE',  ( -21.46681500597755488, 65.43630044540329038, -242.4735498273712153 ) ) ;
#143130 = CIRCLE ( 'NONE', #197305, 11.75000000000000000 ) ;
#143132 = AXIS2_PLACEMENT_3D ( 'NONE', #40450, #44273, #45548 ) ;
#143133 = EDGE_LOOP ( 'NONE', ( #170456, #177542, #77007, #145467 ) ) ;
#143134 = CIRCLE ( 'NONE', #93074, 0.1000000000000024342 ) ;
#143135 = CARTESIAN_POINT ( 'NONE',  ( -20.54999999999999716, 74.00000000001186606, -89.79848556176222019 ) ) ;
#143137 = ORIENTED_EDGE ( 'NONE', *, *, #193925, .T. ) ;
#143136 = CYLINDRICAL_SURFACE ( 'NONE', #163768, 0.09999999999999939493 ) ;
#143138 = EDGE_CURVE ( 'NONE', #80064, #3980, #161296, .T. ) ;
#143139 = ADVANCED_FACE ( 'NONE', ( #190022 ), #40520, .T. ) ;
#143142 = ORIENTED_EDGE ( 'NONE', *, *, #93923, .F. ) ;
#143141 = ORIENTED_EDGE ( 'NONE', *, *, #251446, .T. ) ;
#143140 = LINE ( 'NONE', #146993, #155454 ) ;
#143143 = DIRECTION ( 'NONE',  ( 1.000000000000000000, -0.000000000000000000, -0.000000000000000000 ) ) ;
#143144 = CARTESIAN_POINT ( 'NONE',  ( -21.05000000000000071, -1.835341550213255957, -112.0551512925630107 ) ) ;
#143145 = DIRECTION ( 'NONE',  ( 3.265361837132813093E-16, 1.000000000000000000, 6.982962677686266711E-15 ) ) ;
#143146 = AXIS2_PLACEMENT_3D ( 'NONE', #34382, #132170, #112609 ) ;
#143148 = DIRECTION ( 'NONE',  ( 0.000000000000000000, 0.9770955615653548199, 0.2128009952262535920 ) ) ;
#143147 = DIRECTION ( 'NONE',  ( 1.000000000000000000, -1.186688945009010077E-16, -8.286604613020808509E-31 ) ) ;
#143149 = DIRECTION ( 'NONE',  ( 1.000000000000000000, 0.000000000000000000, 0.000000000000000000 ) ) ;
#143150 = EDGE_CURVE ( 'NONE', #115296, #51379, #73814, .T. ) ;
#143151 = DIRECTION ( 'NONE',  ( -0.000000000000000000, 1.000000000000000000, 6.352154140967427193E-15 ) ) ;
#143152 = AXIS2_PLACEMENT_3D ( 'NONE', #225809, #207580, #8088 ) ;
#143153 = DIRECTION ( 'NONE',  ( -1.000000000000000000, -2.952720810173289112E-16, 0.000000000000000000 ) ) ;
#143154 = CARTESIAN_POINT ( 'NONE',  ( -23.25000000000000000, 28.50120599808395028, -258.2149742250584268 ) ) ;
#143155 = TOROIDAL_SURFACE ( 'NONE', #59950, 0.2000000000000000111, 0.1000000000000000056 ) ;
#143156 = VERTEX_POINT ( 'NONE', #191335 ) ;
#143157 = ORIENTED_EDGE ( 'NONE', *, *, #230940, .F. ) ;
#143158 = AXIS2_PLACEMENT_3D ( 'NONE', #27405, #106890, #136718 ) ;
#143159 = EDGE_CURVE ( 'NONE', #215983, #5545, #111577, .T. ) ;
#143160 = DIRECTION ( 'NONE',  ( 0.000000000000000000, -6.467318590049456648E-15, 1.000000000000000000 ) ) ;
#143163 = VERTEX_POINT ( 'NONE', #97294 ) ;
#143162 = EDGE_CURVE ( 'NONE', #56398, #192073, #215611, .T. ) ;
#143161 = LINE ( 'NONE', #164036, #236915 ) ;
#143164 = ORIENTED_EDGE ( 'NONE', *, *, #137287, .F. ) ;
#143165 = CARTESIAN_POINT ( 'NONE',  ( -22.00411653962169467, 7.253442868370059138, 0.09903810578604851922 ) ) ;
#143166 = EDGE_LOOP ( 'NONE', ( #76981, #95213, #155703, #220007, #28613 ) ) ;
#143167 = LINE ( 'NONE', #226545, #162910 ) ;
#143168 = EDGE_CURVE ( 'NONE', #234077, #14935, #78243, .T. ) ;
#143169 = CIRCLE ( 'NONE', #55858, 0.09999999999999939493 ) ;
#143170 = CIRCLE ( 'NONE', #43243, 0.09999999999998898659 ) ;
#143171 = EDGE_LOOP ( 'NONE', ( #129577, #30946, #5943, #231679, #203237, #236104, #78319 ) ) ;
#143172 = AXIS2_PLACEMENT_3D ( 'NONE', #231588, #249859, #15106 ) ;
#143173 = EDGE_CURVE ( 'NONE', #14440, #205787, #115669, .T. ) ;
#143174 = B_SPLINE_CURVE_WITH_KNOTS ( 'NONE', 3,
 ( #110460, #96021, #190009, #255040, #76462, #156036, #235536 ),
 .UNSPECIFIED., .F., .F.,
 ( 4, 3, 4 ),
 ( 0.000000000000000000, 0.0009834301579440022593, 0.001767853679402679300 ),
 .UNSPECIFIED. ) ;
#143175 = CARTESIAN_POINT ( 'NONE',  ( -21.05000000000000071, 87.48912529308749697, -39.02310748452423894 ) ) ;
#143176 = DIRECTION ( 'NONE',  ( 1.000000000000000000, 0.000000000000000000, 0.000000000000000000 ) ) ;
#143178 = EDGE_LOOP ( 'NONE', ( #189054, #141974, #31726, #138610 ) ) ;
#143177 = ORIENTED_EDGE ( 'NONE', *, *, #72211, .T. ) ;
#143179 = VERTEX_POINT ( 'NONE', #98571 ) ;
#143180 = DIRECTION ( 'NONE',  ( 0.000000000000000000, -7.116814260417668513E-15, 1.000000000000000000 ) ) ;
#143181 = ORIENTED_EDGE ( 'NONE', *, *, #227790, .T. ) ;
#143182 = ORIENTED_EDGE ( 'NONE', *, *, #175711, .F. ) ;
#143184 = DIRECTION ( 'NONE',  ( 0.000000000000000000, 0.000000000000000000, 1.000000000000000000 ) ) ;
#143183 = AXIS2_PLACEMENT_3D ( 'NONE', #104726, #166055, #106024 ) ;
#143185 = CARTESIAN_POINT ( 'NONE',  ( 21.05000000000000071, 1.349084418638171412, -141.9864989635455004 ) ) ;
#143187 = ORIENTED_EDGE ( 'NONE', *, *, #245827, .F. ) ;
#143186 = CARTESIAN_POINT ( 'NONE',  ( 23.25000000000000000, 87.75000000001276135, -215.2731074845242745 ) ) ;
#143188 = EDGE_CURVE ( 'NONE', #102370, #38899, #256340, .T. ) ;
#143190 = CARTESIAN_POINT ( 'NONE',  ( -16.88219499860498019, 60.93897784699102260, -221.0423399452780870 ) ) ;
#143189 = CARTESIAN_POINT ( 'NONE',  ( 21.05000000000000071, 85.50000000001197975, -112.9170766071766820 ) ) ;
#143191 = CARTESIAN_POINT ( 'NONE',  ( 20.85000000000000142, 79.11538813396778380, -196.3722783875038544 ) ) ;
#143193 = ORIENTED_EDGE ( 'NONE', *, *, #221796, .F. ) ;
#143192 = DIRECTION ( 'NONE',  ( 0.000000000000000000, -1.000000000000000000, -6.982962677686265922E-15 ) ) ;
#143194 = CARTESIAN_POINT ( 'NONE',  ( -22.47071067811865319, 7.720074744509219933, -66.90090754529744288 ) ) ;
#143195 = EDGE_LOOP ( 'NONE', ( #200031, #99305, #187012, #218253 ) ) ;
#143196 = CIRCLE ( 'NONE', #176550, 0.09999999999999939493 ) ;
#143197 = LINE ( 'NONE', #44115, #32781 ) ;
#143198 = AXIS2_PLACEMENT_3D ( 'NONE', #96545, #118723, #29 ) ;
#143200 = EDGE_CURVE ( 'NONE', #46601, #45320, #36095, .T. ) ;
#143199 = ORIENTED_EDGE ( 'NONE', *, *, #235590, .T. ) ;
#143201 = CARTESIAN_POINT ( 'NONE',  ( 22.14074124539698829, 68.60992214896863572, -170.1221603803684843 ) ) ;
#143202 = CARTESIAN_POINT ( 'NONE',  ( -11.59999999999994458, 67.65000000001118963, -25.06452884076210452 ) ) ;
#143203 = EDGE_LOOP ( 'NONE', ( #42451, #111042, #254134, #137718, #63917, #207534, #19500, #240393, #26418 ) ) ;
#143204 = CARTESIAN_POINT ( 'NONE',  ( 21.06280952165568721, 10.62713230061198111, -45.70405388677878022 ) ) ;
#143205 = CARTESIAN_POINT ( 'NONE',  ( 18.49999999999999289, 11.65000000001115588, -200.9999999999999432 ) ) ;
#143206 = ORIENTED_EDGE ( 'NONE', *, *, #197530, .T. ) ;
#143207 = EDGE_LOOP ( 'NONE', ( #99393, #88304, #81244, #239472 ) ) ;
#143208 = ADVANCED_FACE ( 'NONE', ( #255060 ), #58182, .F. ) ;
#143209 = CARTESIAN_POINT ( 'NONE',  ( 20.94999999999999929, -11.64999999998883595, -67.00000000000000000 ) ) ;
#143210 = CARTESIAN_POINT ( 'NONE',  ( 20.27550659511088682, 66.78395627750272467, -56.87310748452438247 ) ) ;
#143211 = ORIENTED_EDGE ( 'NONE', *, *, #22075, .F. ) ;
#143212 = CYLINDRICAL_SURFACE ( 'NONE', #164101, 0.09999999999999939493 ) ;
#143213 = ORIENTED_EDGE ( 'NONE', *, *, #210720, .F. ) ;
#143214 = LINE ( 'NONE', #106643, #231508 ) ;
#143215 = DIRECTION ( 'NONE',  ( 0.000000000000000000, -1.000000000000000000, 0.000000000000000000 ) ) ;
#143217 = LINE ( 'NONE', #207062, #204416 ) ;
#143216 = LINE ( 'NONE', #203200, #36560 ) ;
#143218 = DIRECTION ( 'NONE',  ( -1.000000000000000000, 0.000000000000000000, 0.000000000000000000 ) ) ;
#143219 = LINE ( 'NONE', #20741, #45425 ) ;
#143220 = AXIS2_PLACEMENT_3D ( 'NONE', #100990, #102288, #18928 ) ;
#143221 = CIRCLE ( 'NONE', #109898, 0.09999999999999939493 ) ;
#143222 = ORIENTED_EDGE ( 'NONE', *, *, #227461, .T. ) ;
#143223 = CARTESIAN_POINT ( 'NONE',  ( 18.49362639424903776, -9.442604367876930027, -207.7644409335117359 ) ) ;
#143224 = AXIS2_PLACEMENT_3D ( 'NONE', #11586, #211056, #91102 ) ;
#143225 = ADVANCED_FACE ( 'NONE', ( #195185 ), #15248, .T. ) ;
#143227 = ORIENTED_EDGE ( 'NONE', *, *, #179597, .T. ) ;
#143226 = ORIENTED_EDGE ( 'NONE', *, *, #241033, .F. ) ;
#143228 = ORIENTED_EDGE ( 'NONE', *, *, #58044, .T. ) ;
#143229 = EDGE_LOOP ( 'NONE', ( #62407, #13781, #233520, #118591 ) ) ;
#143230 = CIRCLE ( 'NONE', #30832, 0.1000000000000028644 ) ;
#143231 = DIRECTION ( 'NONE',  ( -1.836970198721029934E-16, -1.000000000000000000, -6.982962677686266711E-15 ) ) ;
#143232 = CARTESIAN_POINT ( 'NONE',  ( 18.49999999999999645, 77.13501884592184865, -61.80613060109197932 ) ) ;
#143233 = TOROIDAL_SURFACE ( 'NONE', #9960, 3.899999999999999467, 0.1000000000000000056 ) ;
#143234 = DIRECTION ( 'NONE',  ( 1.000000000000000000, 0.000000000000000000, 0.000000000000000000 ) ) ;
#143235 = DIRECTION ( 'NONE',  ( -3.265361837132812600E-16, -0.4088369013363246096, 0.9126074666063785923 ) ) ;
#143236 = FACE_OUTER_BOUND ( 'NONE', #78861, .T. ) ;
#143237 = EDGE_CURVE ( 'NONE', #162306, #222722, #79023, .T. ) ;
#143239 = CARTESIAN_POINT ( 'NONE',  ( -22.47007471830799119, 1.115783626517291571E-11, -159.7792893480734904 ) ) ;
#143238 = CARTESIAN_POINT ( 'NONE',  ( 21.30740335185486245, 69.44334207798367231, -69.62204201030021977 ) ) ;
#143241 = EDGE_LOOP ( 'NONE', ( #147675, #190534, #155843, #247991 ) ) ;
#143240 = CARTESIAN_POINT ( 'NONE',  ( 20.94999999999999929, 7.128833340094563376, -233.7327013124401276 ) ) ;
#143242 = CARTESIAN_POINT ( 'NONE',  ( -21.05000000000000071, 6.540656951712399803, -167.4999999999999716 ) ) ;
#143243 = ORIENTED_EDGE ( 'NONE', *, *, #142824, .T. ) ;
#143244 = TOROIDAL_SURFACE ( 'NONE', #184947, 7.800000000000000711, 0.1000000000000000056 ) ;
#143245 = CARTESIAN_POINT ( 'NONE',  ( -22.50014994444013539, 11.74971973190329955, -66.91691984328113563 ) ) ;
#143246 = VERTEX_POINT ( 'NONE', #94761 ) ;
#143247 = ORIENTED_EDGE ( 'NONE', *, *, #107012, .F. ) ;
#143248 = DIRECTION ( 'NONE',  ( 0.000000000000000000, -0.9651348961777157509, 0.2617529984165031243 ) ) ;
#143249 = CIRCLE ( 'NONE', #80696, 0.1000000000000106914 ) ;
#143250 = DIRECTION ( 'NONE',  ( 0.000000000000000000, 0.000000000000000000, 1.000000000000000000 ) ) ;
#143252 = EDGE_CURVE ( 'NONE', #244818, #140958, #82315, .T. ) ;
#143251 = DIRECTION ( 'NONE',  ( 0.000000000000000000, 0.000000000000000000, -1.000000000000000000 ) ) ;
#143253 = EDGE_CURVE ( 'NONE', #157944, #202583, #182318, .T. ) ;
#143254 = CIRCLE ( 'NONE', #226426, 0.1000000000000055844 ) ;
#143255 = CARTESIAN_POINT ( 'NONE',  ( -20.64999999999999858, -9.000000000000003553, -9.893969122652444881 ) ) ;
#143256 = AXIS2_PLACEMENT_3D ( 'NONE', #80984, #121450, #241378 ) ;
#143257 = EDGE_CURVE ( 'NONE', #204155, #147319, #169885, .T. ) ;
#143258 = TOROIDAL_SURFACE ( 'NONE', #218073, 11.65000000000000036, 0.1000000000000000056 ) ;
#143259 = CARTESIAN_POINT ( 'NONE',  ( -21.14999999999994174, 77.83551161375991967, -47.52760213295649550 ) ) ;
#143260 = ORIENTED_EDGE ( 'NONE', *, *, #53468, .F. ) ;
#143261 = ORIENTED_EDGE ( 'NONE', *, *, #233532, .F. ) ;
#143262 = EDGE_CURVE ( 'NONE', #237217, #59718, #11643, .T. ) ;
#143263 = DIRECTION ( 'NONE',  ( 1.000000000000000000, 0.000000000000000000, 0.000000000000000000 ) ) ;
#143264 = ORIENTED_EDGE ( 'NONE', *, *, #199555, .T. ) ;
#143265 = LINE ( 'NONE', #46723, #189597 ) ;
#143266 = DIRECTION ( 'NONE',  ( -2.940209281316620030E-16, 0.9770955615653310611, 0.2128009952263628379 ) ) ;
#143267 = CARTESIAN_POINT ( 'NONE',  ( -20.94999999999999929, 7.476371755685461196, -241.7308184205399471 ) ) ;
#143269 = CIRCLE ( 'NONE', #230773, 0.09999999999998898659 ) ;
#143268 = CARTESIAN_POINT ( 'NONE',  ( -16.81744102076748959, 66.05000000001255955, -182.6731074845244223 ) ) ;
#143270 = DIRECTION ( 'NONE',  ( 2.940209281316622495E-16, -1.000000000000000000, -1.764125568789973497E-15 ) ) ;
#143271 = CARTESIAN_POINT ( 'NONE',  ( -18.40000000000000213, 59.20211495293902004, -220.5705723384363921 ) ) ;
#143272 = DIRECTION ( 'NONE',  ( 1.000000000000000000, 0.000000000000000000, 0.000000000000000000 ) ) ;
#143273 = CARTESIAN_POINT ( 'NONE',  ( 18.59999999999999076, 10.20857864377385127, -58.25000000000000000 ) ) ;
#143274 = CARTESIAN_POINT ( 'NONE',  ( -21.05000000000094218, 6.196269102992084221, -199.6354557928876829 ) ) ;
#143275 = CIRCLE ( 'NONE', #84982, 0.09999999999999939493 ) ;
#143276 = DIRECTION ( 'NONE',  ( 0.000000000000000000, -0.9553114395362780620, -0.2956011730205483912 ) ) ;
#143277 = DIRECTION ( 'NONE',  ( 1.000000000000000000, -0.000000000000000000, -0.000000000000000000 ) ) ;
#143278 = VECTOR ( 'NONE', #3995, 1000.000000000000000 ) ;
#143279 = CIRCLE ( 'NONE', #76637, 0.09999999999998898659 ) ;
#143280 = ADVANCED_FACE ( 'NONE', ( #38651 ), #207275, .T. ) ;
#143281 = EDGE_LOOP ( 'NONE', ( #97496, #118209, #191808, #163427 ) ) ;
#143282 = CIRCLE ( 'NONE', #184985, 1.749999999999998002 ) ;
#143283 = CARTESIAN_POINT ( 'NONE',  ( 23.14999999999999858, 6.649999999999999467, -12.35000000000000320 ) ) ;
#143284 = ORIENTED_EDGE ( 'NONE', *, *, #11936, .F. ) ;
#143285 = ADVANCED_FACE ( 'NONE', ( #197711 ), #19077, .T. ) ;
#143286 = EDGE_CURVE ( 'NONE', #173371, #139652, #39960, .T. ) ;
#143287 = CYLINDRICAL_SURFACE ( 'NONE', #71113, 0.09999999999999939493 ) ;
#143288 = CYLINDRICAL_SURFACE ( 'NONE', #114774, 0.1000000000000028644 ) ;
#143289 = DIRECTION ( 'NONE',  ( -0.000000000000000000, -0.1335171055202901413, 0.9910465087640860649 ) ) ;
#143290 = ORIENTED_EDGE ( 'NONE', *, *, #35736, .T. ) ;
#143291 = DIRECTION ( 'NONE',  ( 0.000000000000000000, -0.9876197685951252359, -0.1568667991644863424 ) ) ;
#143292 = SPHERICAL_SURFACE ( 'NONE', #89717, 0.1000000000000000056 ) ;
#143293 = CARTESIAN_POINT ( 'NONE',  ( -23.15000000000000213, 76.00000000001270450, -207.5731074845243427 ) ) ;
#143294 = DIRECTION ( 'NONE',  ( -0.000000000000000000, 0.9579639084728162057, 0.2868887416115976086 ) ) ;
#143295 = AXIS2_PLACEMENT_3D ( 'NONE', #22533, #370, #82454 ) ;
#143296 = COLOUR_RGB ( '', 0.40784314, 0.44705882, 0.49803922) ;
#143298 = CARTESIAN_POINT ( 'NONE',  ( 21.14999999999999858, 75.90220970870291239, -75.78092209500044873 ) ) ;
#143297 = AXIS2_PLACEMENT_3D ( 'NONE', #207985, #170173, #50159 ) ;
#143299 = DIRECTION ( 'NONE',  ( 1.000000000000000000, 0.000000000000000000, 0.000000000000000000 ) ) ;
#143300 = ORIENTED_EDGE ( 'NONE', *, *, #238083, .T. ) ;
#143301 = DIRECTION ( 'NONE',  ( 0.000000000000000000, 0.000000000000000000, -1.000000000000000000 ) ) ;
#143303 = EDGE_LOOP ( 'NONE', ( #189889, #82747, #151631, #233621 ) ) ;
#143302 = DIRECTION ( 'NONE',  ( 0.000000000000000000, -0.8660254037844387076, 0.4999999999999998335 ) ) ;
#143304 = FACE_OUTER_BOUND ( 'NONE', #754, .T. ) ;
#143305 = CARTESIAN_POINT ( 'NONE',  ( -21.65000000000000213, 44.77807522791015060, -237.4671205425215135 ) ) ;
#143306 = CARTESIAN_POINT ( 'NONE',  ( -21.45000000000000284, 29.41239393758413811, -236.9245051605820720 ) ) ;
#143307 = ORIENTED_EDGE ( 'NONE', *, *, #125868, .F. ) ;
#143308 = CARTESIAN_POINT ( 'NONE',  ( -22.49917693094574389, 75.91477003579055349, -148.1729032690549559 ) ) ;
#143309 = EDGE_CURVE ( 'NONE', #179202, #10328, #171309, .T. ) ;
#143310 = PLANE ( 'NONE',  #83886 ) ;
#143311 = ORIENTED_EDGE ( 'NONE', *, *, #146118, .T. ) ;
#143312 = CARTESIAN_POINT ( 'NONE',  ( 21.00000000000000000, 66.25000000001223555, -148.7731074845244450 ) ) ;
#143313 = CARTESIAN_POINT ( 'NONE',  ( 17.74533788810830615, 21.32866134633797017, -229.0662642334345378 ) ) ;
#143314 = AXIS2_PLACEMENT_3D ( 'NONE', #46838, #147238, #70307 ) ;
#143315 = DIRECTION ( 'NONE',  ( -1.000000000000000000, 0.000000000000000000, 0.000000000000000000 ) ) ;
#143316 = VERTEX_POINT ( 'NONE', #215979 ) ;
#143317 = B_SPLINE_CURVE_WITH_KNOTS ( 'NONE', 3,
 ( #187919, #53528, #208767, #169675, #113502, #9265, #110934, #151367, #69259, #50932, #148791, #13133, #193053, #210054, #31437, #93934 ),
 .UNSPECIFIED., .F., .F.,
 ( 4, 3, 3, 3, 3, 4 ),
 ( 0.000000000000000000, 2.209833635978128636E-05, 5.595056164119354553E-05, 8.979992002655480337E-05, 0.0001236482757198921142, 0.0001574984039363022149 ),
 .UNSPECIFIED. ) ;
#143318 = VERTEX_POINT ( 'NONE', #80302 ) ;
#143319 = CARTESIAN_POINT ( 'NONE',  ( -22.50000000000000000, 11.65000000001113278, -167.4999999999999716 ) ) ;
#143320 = DIRECTION ( 'NONE',  ( -1.000000000000000000, -0.000000000000000000, -0.000000000000000000 ) ) ;
#143321 = LINE ( 'NONE', #225412, #3487 ) ;
#143322 = DIRECTION ( 'NONE',  ( 1.000000000000000000, 0.000000000000000000, 0.000000000000000000 ) ) ;
#143323 = DIRECTION ( 'NONE',  ( -0.7071067811865475727, -0.6909108974501237954, -0.1504730267678056066 ) ) ;
#143324 = EDGE_CURVE ( 'NONE', #178566, #194138, #239422, .T. ) ;
#143325 = CARTESIAN_POINT ( 'NONE',  ( 18.49999999999999289, 10.25000000001115730, -125.1500000000000483 ) ) ;
#143326 = DIRECTION ( 'NONE',  ( 1.000000000000000000, 0.000000000000000000, 0.000000000000000000 ) ) ;
#143328 = CARTESIAN_POINT ( 'NONE',  ( -21.45000000000000284, 7.708578643773852157, -121.7500000000000426 ) ) ;
#143327 = CARTESIAN_POINT ( 'NONE',  ( 21.53699400380599371, 6.787711793191639309, -6.911788849595090767E-16 ) ) ;
#143329 = DIRECTION ( 'NONE',  ( 0.000000000000000000, -6.982962677686266711E-15, 1.000000000000000000 ) ) ;
#143330 = EDGE_CURVE ( 'NONE', #172048, #167228, #114336, .T. ) ;
#143331 = DIRECTION ( 'NONE',  ( -1.000000000000000000, 0.000000000000000000, 0.000000000000000000 ) ) ;
#143332 = DIRECTION ( 'NONE',  ( -1.000000000000000000, -0.000000000000000000, -0.000000000000000000 ) ) ;
#143334 = CARTESIAN_POINT ( 'NONE',  ( -21.05000000000000071, -1.835341550213255957, -145.6551512925629766 ) ) ;
#143333 = AXIS2_PLACEMENT_3D ( 'NONE', #163043, #123905, #183867 ) ;
#143335 = ORIENTED_EDGE ( 'NONE', *, *, #55718, .F. ) ;
#143336 = VERTEX_POINT ( 'NONE', #123326 ) ;
#143337 = CARTESIAN_POINT ( 'NONE',  ( -20.85000000000000142, 10.33248238083635151, -139.5948465439131780 ) ) ;
#143338 = DIRECTION ( 'NONE',  ( 0.000000000000000000, 0.000000000000000000, -1.000000000000000000 ) ) ;
#143341 = DIRECTION ( 'NONE',  ( 1.000000000000000000, 0.000000000000000000, 0.000000000000000000 ) ) ;
#143340 = CARTESIAN_POINT ( 'NONE',  ( 20.94999999999999929, 86.10439672154322466, -209.4215112426525138 ) ) ;
#143339 = CIRCLE ( 'NONE', #64229, 1.749999999999998002 ) ;
#143342 = AXIS2_PLACEMENT_3D ( 'NONE', #60793, #156092, #97329 ) ;
#143343 = EDGE_CURVE ( 'NONE', #94754, #183270, #252742, .T. ) ;
#143344 = ADVANCED_FACE ( 'NONE', ( #25514 ), #104989, .F. ) ;
#143345 = DIRECTION ( 'NONE',  ( 0.000000000000000000, 0.9126074666063545004, 0.4088369013363783999 ) ) ;
#143346 = CARTESIAN_POINT ( 'NONE',  ( -21.05000000000000071, -11.64999999998884306, -64.00000000000000000 ) ) ;
#143347 = CARTESIAN_POINT ( 'NONE',  ( -16.94107738177414291, 10.01423928514777373, -87.95000000000004547 ) ) ;
#143348 = DIRECTION ( 'NONE',  ( 0.000000000000000000, -0.4088369013363283289, 0.9126074666063768159 ) ) ;
#143349 = ORIENTED_EDGE ( 'NONE', *, *, #145789, .T. ) ;
#143351 = VECTOR ( 'NONE', #42075, 1000.000000000000000 ) ;
#143350 = CARTESIAN_POINT ( 'NONE',  ( -16.87036670365548474, 51.72098459467785858, -231.8575261499355520 ) ) ;
#143352 = ORIENTED_EDGE ( 'NONE', *, *, #107713, .T. ) ;
#143353 = DIRECTION ( 'NONE',  ( 0.000000000000000000, 0.000000000000000000, 1.000000000000000000 ) ) ;
#143354 = VECTOR ( 'NONE', #153847, 1000.000000000000000 ) ;
#143355 = EDGE_CURVE ( 'NONE', #245692, #87416, #228116, .T. ) ;
#143356 = EDGE_CURVE ( 'NONE', #102386, #5593, #257263, .T. ) ;
#143358 = CARTESIAN_POINT ( 'NONE',  ( 18.48197441911692707, 85.51795479471786621, -29.13289584231640461 ) ) ;
#143357 = AXIS2_PLACEMENT_3D ( 'NONE', #75783, #57473, #94042 ) ;
#143359 = CIRCLE ( 'NONE', #201621, 0.09999999999999577283 ) ;
#143360 = ORIENTED_EDGE ( 'NONE', *, *, #38217, .T. ) ;
#143361 = DIRECTION ( 'NONE',  ( 1.000000000000000000, 0.000000000000000000, -0.000000000000000000 ) ) ;
#143362 = VERTEX_POINT ( 'NONE', #241976 ) ;
#143363 = CARTESIAN_POINT ( 'NONE',  ( -20.85000000000000142, 64.25000000001250555, -176.8069731475025321 ) ) ;
#143364 = CARTESIAN_POINT ( 'NONE',  ( -21.07928932188134041, 76.00000000001213607, -136.5231074845242745 ) ) ;
#143365 = DIRECTION ( 'NONE',  ( 0.000000000000000000, -0.1568667991644693838, -0.9876197685951279004 ) ) ;
#143366 = AXIS2_PLACEMENT_3D ( 'NONE', #5633, #43514, #68211 ) ;
#143367 = CYLINDRICAL_SURFACE ( 'NONE', #25137, 2.000000000000001776 ) ;
#143368 = DIRECTION ( 'NONE',  ( 1.000000000000000000, 0.000000000000000000, 0.000000000000000000 ) ) ;
#143369 = EDGE_CURVE ( 'NONE', #101028, #135761, #28221, .T. ) ;
#143371 = CIRCLE ( 'NONE', #185067, 0.1000000000000028644 ) ;
#143370 = CARTESIAN_POINT ( 'NONE',  ( 21.00000000000000000, 9.750000000011153745, -155.1500000000000057 ) ) ;
#143372 = CARTESIAN_POINT ( 'NONE',  ( -20.64999999999999858, 1.115600667400684642E-11, -87.62500000000005684 ) ) ;
#143375 = ORIENTED_EDGE ( 'NONE', *, *, #148111, .T. ) ;
#143374 = ADVANCED_FACE ( 'NONE', ( #165010 ), #44935, .T. ) ;
#143373 = CARTESIAN_POINT ( 'NONE',  ( 21.11701782572532693, 65.27839088400513390, -191.2780700550132167 ) ) ;
#143377 = LINE ( 'NONE', #2572, #76955 ) ;
#143376 = DIRECTION ( 'NONE',  ( 0.000000000000000000, 0.000000000000000000, 1.000000000000000000 ) ) ;
#143378 = AXIS2_PLACEMENT_3D ( 'NONE', #9675, #150489, #211747 ) ;
#143379 = ORIENTED_EDGE ( 'NONE', *, *, #154310, .T. ) ;
#143381 = VERTEX_POINT ( 'NONE', #223681 ) ;
#143380 = CARTESIAN_POINT ( 'NONE',  ( 21.05000000000000071, 67.18454772081508963, -195.1027149319101568 ) ) ;
#143382 = ORIENTED_EDGE ( 'NONE', *, *, #129131, .T. ) ;
#143383 = DIRECTION ( 'NONE',  ( 1.000000000000000000, 0.000000000000000000, 0.000000000000000000 ) ) ;
#143384 = CARTESIAN_POINT ( 'NONE',  ( -21.76363531954647357, 30.21839054580515693, -252.3279600990519498 ) ) ;
#143385 = DIRECTION ( 'NONE',  ( -1.000000000000000000, -1.875376730785737719E-16, -0.000000000000000000 ) ) ;
#143386 = CIRCLE ( 'NONE', #72674, 0.09999999999999939493 ) ;
#143387 = ORIENTED_EDGE ( 'NONE', *, *, #162173, .T. ) ;
#143388 = CYLINDRICAL_SURFACE ( 'NONE', #42228, 0.09999999999998898659 ) ;
#143389 = DIRECTION ( 'NONE',  ( 1.000000000000000000, 1.186688945009009831E-16, 0.000000000000000000 ) ) ;
#143390 = CARTESIAN_POINT ( 'NONE',  ( 23.14999999999999503, 28.91254064196106910, -237.8576372133405528 ) ) ;
#143391 = EDGE_CURVE ( 'NONE', #89902, #100947, #126308, .T. ) ;
#143392 = CIRCLE ( 'NONE', #226775, 2.000000000000002665 ) ;
#143393 = DIRECTION ( 'NONE',  ( 1.000000000000000000, 0.000000000000000000, 0.000000000000000000 ) ) ;
#143394 = AXIS2_PLACEMENT_3D ( 'NONE', #10326, #29899, #92398 ) ;
#143395 = CARTESIAN_POINT ( 'NONE',  ( -18.53317502108577131, 46.43483777265582546, -243.0774829958280918 ) ) ;
#143396 = AXIS2_PLACEMENT_3D ( 'NONE', #255204, #216124, #120918 ) ;
#143397 = LINE ( 'NONE', #22189, #26903 ) ;
#143398 = EDGE_CURVE ( 'NONE', #223063, #98112, #203145, .T. ) ;
#143399 = ORIENTED_EDGE ( 'NONE', *, *, #240139, .F. ) ;
#143400 = ORIENTED_EDGE ( 'NONE', *, *, #174180, .F. ) ;
#143401 = CARTESIAN_POINT ( 'NONE',  ( 20.94999999999999929, 2.761092913073515120, -213.6778149113116854 ) ) ;
#143402 = ORIENTED_EDGE ( 'NONE', *, *, #251362, .T. ) ;
#143403 = DIRECTION ( 'NONE',  ( -0.000000000000000000, 0.9770955615653313941, 0.2128009952263603954 ) ) ;
#143404 = ORIENTED_EDGE ( 'NONE', *, *, #195922, .T. ) ;
#143405 = CARTESIAN_POINT ( 'NONE',  ( -18.40000000000000213, 5.650000000011139001, -113.1500000000000341 ) ) ;
#143406 = DIRECTION ( 'NONE',  ( -1.000000000000000000, -0.000000000000000000, -0.000000000000000000 ) ) ;
#143407 = FACE_OUTER_BOUND ( 'NONE', #51155, .T. ) ;
#143408 = EDGE_CURVE ( 'NONE', #240571, #145384, #165973, .T. ) ;
#143409 = CARTESIAN_POINT ( 'NONE',  ( -21.09813707148783379, 30.81905141938414516, -252.1330000948349834 ) ) ;
#143410 = CARTESIAN_POINT ( 'NONE',  ( 21.13461538461538325, 10.61458296203669427, -179.8499999999999943 ) ) ;
#143411 = VERTEX_POINT ( 'NONE', #86731 ) ;
#143412 = CARTESIAN_POINT ( 'NONE',  ( 21.30000000000002558, 76.00000000001165290, -69.52310748452431710 ) ) ;
#143413 = CIRCLE ( 'NONE', #139097, 0.1000000000000028644 ) ;
#143414 = AXIS2_PLACEMENT_3D ( 'NONE', #10356, #89862, #66461 ) ;
#143415 = CARTESIAN_POINT ( 'NONE',  ( -16.87304349924914604, 66.03825492205537273, -182.6340408094791883 ) ) ;
#143416 = DIRECTION ( 'NONE',  ( 0.000000000000000000, -0.8777080977375132376, 0.4791956752371582251 ) ) ;
#143417 = DIRECTION ( 'NONE',  ( 1.000000000000000000, -0.000000000000000000, -0.000000000000000000 ) ) ;
#143418 = EDGE_LOOP ( 'NONE', ( #201939, #193801, #146340 ) ) ;
#143420 = FACE_OUTER_BOUND ( 'NONE', #30588, .T. ) ;
#143419 = CARTESIAN_POINT ( 'NONE',  ( -22.32929514600008503, 75.90092432189851479, -177.6017550499008735 ) ) ;
#143421 = ORIENTED_EDGE ( 'NONE', *, *, #244079, .F. ) ;
#143423 = VERTEX_POINT ( 'NONE', #166332 ) ;
#143422 = DIRECTION ( 'NONE',  ( 0.000000000000000000, -0.2617529984165152257, -0.9651348961777124202 ) ) ;
#143424 = ORIENTED_EDGE ( 'NONE', *, *, #63523, .F. ) ;
#143425 = DIRECTION ( 'NONE',  ( -0.000000000000000000, 0.9876197685951241256, 0.1568667991644932258 ) ) ;
#143426 = CIRCLE ( 'NONE', #31034, 11.65000000000000924 ) ;
#143427 = CARTESIAN_POINT ( 'NONE',  ( 22.39999999999999858, 10.71943444926881561, -226.8179467668883547 ) ) ;
#143428 = FACE_OUTER_BOUND ( 'NONE', #31154, .T. ) ;
#143429 = TOROIDAL_SURFACE ( 'NONE', #214164, 0.2000000000000000111, 0.1000000000000000056 ) ;
#143430 = ORIENTED_EDGE ( 'NONE', *, *, #29737, .F. ) ;
#143431 = DIRECTION ( 'NONE',  ( -1.073024830501117725E-15, -0.000000000000000000, -1.000000000000000000 ) ) ;
#143432 = DIRECTION ( 'NONE',  ( -3.265361837132813093E-16, -1.000000000000000000, -6.982962677686266711E-15 ) ) ;
#143434 = CARTESIAN_POINT ( 'NONE',  ( -16.92507428761701505, 44.19333870103346129, -235.2730123856632076 ) ) ;
#143433 = DIRECTION ( 'NONE',  ( 1.186688945009010077E-16, 1.000000000000000000, 6.982962677686266711E-15 ) ) ;
#143436 = ORIENTED_EDGE ( 'NONE', *, *, #199609, .F. ) ;
#143435 = LINE ( 'NONE', #222965, #9927 ) ;
#143437 = CIRCLE ( 'NONE', #114206, 0.1000000000000004496 ) ;
#143438 = AXIS2_PLACEMENT_3D ( 'NONE', #153214, #91911, #188449 ) ;
#143439 = PRODUCT_DEFINITION_SHAPE ( 'NONE', 'NONE',  #258126 ) ;
#143440 = ORIENTED_EDGE ( 'NONE', *, *, #151879, .T. ) ;
#143441 = CARTESIAN_POINT ( 'NONE',  ( -16.87331047859651179, 9.950000000011142376, -79.65000000000004832 ) ) ;
#143442 = CARTESIAN_POINT ( 'NONE',  ( 20.94999999999999929, 71.00000000001186606, -90.61784146561124942 ) ) ;
#143443 = DIRECTION ( 'NONE',  ( -0.000000000000000000, 7.109473446599835262E-15, -1.000000000000000000 ) ) ;
#143444 = ORIENTED_EDGE ( 'NONE', *, *, #214522, .F. ) ;
#143445 = CARTESIAN_POINT ( 'NONE',  ( 22.39999999999999503, 33.47376623175147614, -242.4412390690852988 ) ) ;
#143446 = ORIENTED_EDGE ( 'NONE', *, *, #52908, .F. ) ;
#143447 = CYLINDRICAL_SURFACE ( 'NONE', #214126, 11.79999999999999361 ) ;
#143448 = DIRECTION ( 'NONE',  ( 0.000000000000000000, -0.000000000000000000, -1.000000000000000000 ) ) ;
#143449 = DIRECTION ( 'NONE',  ( -1.186688945009010077E-16, 0.9770955615653317272, 0.2128009952263595073 ) ) ;
#143450 = VECTOR ( 'NONE', #47094, 1000.000000000000114 ) ;
#143451 = ORIENTED_EDGE ( 'NONE', *, *, #4055, .T. ) ;
#143452 = DIRECTION ( 'NONE',  ( 0.000000000000000000, 1.000000000000000000, 0.000000000000000000 ) ) ;
#143453 = CIRCLE ( 'NONE', #206001, 0.1000000000000022676 ) ;
#143454 = EDGE_CURVE ( 'NONE', #128093, #59419, #245834, .T. ) ;
#143455 = DIRECTION ( 'NONE',  ( -1.000000000000000000, 2.952720810173289112E-16, 2.061873921506763405E-30 ) ) ;
#143456 = AXIS2_PLACEMENT_3D ( 'NONE', #141908, #221427, #122363 ) ;
#143457 = AXIS2_PLACEMENT_3D ( 'NONE', #104031, #164039, #4921 ) ;
#143458 = ORIENTED_EDGE ( 'NONE', *, *, #246576, .F. ) ;
#143459 = AXIS2_PLACEMENT_3D ( 'NONE', #246918, #109979, #91712 ) ;
#143460 = VERTEX_POINT ( 'NONE', #188419 ) ;
#143461 = VERTEX_POINT ( 'NONE', #150592 ) ;
#143462 = CARTESIAN_POINT ( 'NONE',  ( 20.94999999999999929, 76.00000000001141132, -34.12310748452431852 ) ) ;
#143464 = ADVANCED_FACE ( 'NONE', ( #146702 ), #206706, .T. ) ;
#143463 = ORIENTED_EDGE ( 'NONE', *, *, #193503, .T. ) ;
#143466 = ORIENTED_EDGE ( 'NONE', *, *, #58815, .F. ) ;
#143465 = DIRECTION ( 'NONE',  ( 1.000000000000000000, 0.000000000000000000, 0.000000000000000000 ) ) ;
#143467 = ORIENTED_EDGE ( 'NONE', *, *, #12205, .T. ) ;
#143468 = EDGE_CURVE ( 'NONE', #155936, #71652, #86596, .T. ) ;
#143471 = ORIENTED_EDGE ( 'NONE', *, *, #125252, .F. ) ;
#143470 = VERTEX_POINT ( 'NONE', #111456 ) ;
#143469 = DIRECTION ( 'NONE',  ( -1.000000000000000000, 0.000000000000000000, 0.000000000000000000 ) ) ;
#143472 = CARTESIAN_POINT ( 'NONE',  ( 15.74999999999999645, 9.350000000011139178, -150.7500000000000284 ) ) ;
#143473 = ORIENTED_EDGE ( 'NONE', *, *, #144102, .T. ) ;
#143474 = DIRECTION ( 'NONE',  ( -1.073024830501117725E-15, -6.982962677686266711E-15, 1.000000000000000000 ) ) ;
#143475 = AXIS2_PLACEMENT_3D ( 'NONE', #75856, #116284, #197073 ) ;
#143476 = DIRECTION ( 'NONE',  ( 0.000000000000000000, -0.1495327102803078179, -0.9887567792719429427 ) ) ;
#143477 = CARTESIAN_POINT ( 'NONE',  ( 18.79999999999999716, -11.65000000000000036, 5.900000000000001243 ) ) ;
#143478 = ORIENTED_EDGE ( 'NONE', *, *, #176486, .T. ) ;
#143479 = EDGE_CURVE ( 'NONE', #102599, #137205, #68487, .T. ) ;
#143480 = CARTESIAN_POINT ( 'NONE',  ( -21.05000000000000071, 69.34766280046808617, -247.6726305063181144 ) ) ;
#143481 = CIRCLE ( 'NONE', #47779, 0.09999999999998898659 ) ;
#143484 = ORIENTED_EDGE ( 'NONE', *, *, #177340, .F. ) ;
#143483 = EDGE_CURVE ( 'NONE', #117242, #108268, #223982, .T. ) ;
#143482 = FACE_OUTER_BOUND ( 'NONE', #237642, .T. ) ;
#143485 = CARTESIAN_POINT ( 'NONE',  ( -16.77779411503078322, 9.946101446935278645, -180.1630574176197968 ) ) ;
#143487 = ORIENTED_EDGE ( 'NONE', *, *, #144390, .F. ) ;
#143486 = CYLINDRICAL_SURFACE ( 'NONE', #114668, 0.09999999999999939493 ) ;
#143488 = ORIENTED_EDGE ( 'NONE', *, *, #220571, .T. ) ;
#143489 = EDGE_CURVE ( 'NONE', #226256, #91428, #108884, .T. ) ;
#143490 = VERTEX_POINT ( 'NONE', #230118 ) ;
#143491 = ORIENTED_EDGE ( 'NONE', *, *, #145528, .F. ) ;
#143492 = DIRECTION ( 'NONE',  ( 0.000000000000000000, 1.000000000000000000, 0.000000000000000000 ) ) ;
#143493 = CARTESIAN_POINT ( 'NONE',  ( -20.64999999999999858, 71.65000000001187175, -90.67310748452433700 ) ) ;
#143496 = ORIENTED_EDGE ( 'NONE', *, *, #120119, .F. ) ;
#143495 = ORIENTED_EDGE ( 'NONE', *, *, #45938, .F. ) ;
#143494 = AXIS2_PLACEMENT_3D ( 'NONE', #198898, #44969, #219739 ) ;
#143497 = CIRCLE ( 'NONE', #31119, 0.1000000000000028644 ) ;
#143498 = ORIENTED_EDGE ( 'NONE', *, *, #194839, .T. ) ;
#143499 = CARTESIAN_POINT ( 'NONE',  ( -18.59999999999999787, 7.021664781911246322, -104.3335654018973315 ) ) ;
#143501 = ORIENTED_EDGE ( 'NONE', *, *, #197330, .T. ) ;
#143500 = EDGE_CURVE ( 'NONE', #43099, #168869, #170202, .T. ) ;
#143502 = EDGE_LOOP ( 'NONE', ( #40910, #85256, #140461, #116723 ) ) ;
#143503 = DIRECTION ( 'NONE',  ( 1.000000000000000000, -0.000000000000000000, -0.000000000000000000 ) ) ;
#143505 = ORIENTED_EDGE ( 'NONE', *, *, #156021, .F. ) ;
#143504 = CYLINDRICAL_SURFACE ( 'NONE', #201530, 12.87499999999999822 ) ;
#143506 = DIRECTION ( 'NONE',  ( 0.000000000000000000, 1.897661533703519897E-16, -1.000000000000000000 ) ) ;
#143508 = CARTESIAN_POINT ( 'NONE',  ( 18.49713797159848383, -9.446482327567720105, -107.5714581216104193 ) ) ;
#143507 = CARTESIAN_POINT ( 'NONE',  ( 18.59999999999999076, 10.49142135624846439, -91.85000000000003695 ) ) ;
#143509 = ORIENTED_EDGE ( 'NONE', *, *, #238350, .T. ) ;
#143512 = EDGE_CURVE ( 'NONE', #96622, #208385, #232401, .T. ) ;
#143511 = VERTEX_POINT ( 'NONE', #28097 ) ;
#143510 = ORIENTED_EDGE ( 'NONE', *, *, #51400, .F. ) ;
#143513 = FACE_OUTER_BOUND ( 'NONE', #248357, .T. ) ;
#143514 = FACE_OUTER_BOUND ( 'NONE', #237977, .T. ) ;
#143515 = AXIS2_PLACEMENT_3D ( 'NONE', #9078, #209858, #53338 ) ;
#143516 = VERTEX_POINT ( 'NONE', #9785 ) ;
#143517 = CIRCLE ( 'NONE', #6127, 0.1000000000000008937 ) ;
#143518 = CIRCLE ( 'NONE', #31145, 0.2000000000000057288 ) ;
#143519 = VECTOR ( 'NONE', #67054, 1000.000000000000000 ) ;
#143520 = LINE ( 'NONE', #223055, #167649 ) ;
#143521 = EDGE_LOOP ( 'NONE', ( #199313, #179182, #166401, #105421 ) ) ;
#143522 = ORIENTED_EDGE ( 'NONE', *, *, #100875, .F. ) ;
#143523 = CARTESIAN_POINT ( 'NONE',  ( 13.99999999999999822, 9.850000000011137402, -184.2499999999999716 ) ) ;
#143524 = ORIENTED_EDGE ( 'NONE', *, *, #195901, .F. ) ;
#143525 = FACE_OUTER_BOUND ( 'NONE', #36700, .T. ) ;
#143526 = DIRECTION ( 'NONE',  ( 0.000000000000000000, 0.000000000000000000, 1.000000000000000000 ) ) ;
#143527 = ORIENTED_EDGE ( 'NONE', *, *, #36825, .F. ) ;
#143528 = CARTESIAN_POINT ( 'NONE',  ( 19.96984138294286026, 64.25000000001220712, -145.2985354133239753 ) ) ;
#143529 = CYLINDRICAL_SURFACE ( 'NONE', #112190, 0.09999999999998898659 ) ;
#143531 = DIRECTION ( 'NONE',  ( 2.710505431213777355E-16, -1.000000000000000000, 0.000000000000000000 ) ) ;
#143530 = CARTESIAN_POINT ( 'NONE',  ( 18.39999999999999503, 59.46930106059529209, -220.6430355403071530 ) ) ;
#143532 = CARTESIAN_POINT ( 'NONE',  ( 23.25000000000000000, 87.65000000001215597, -139.6231074845242688 ) ) ;
#143533 = CARTESIAN_POINT ( 'NONE',  ( -20.94999999999999929, 1.115649653272650466E-11, -171.5000000000000284 ) ) ;
#143534 = CARTESIAN_POINT ( 'NONE',  ( 18.59999999999999432, 74.26374286841418382, -57.95445515550683524 ) ) ;
#143535 = CARTESIAN_POINT ( 'NONE',  ( 21.05000000000000071, 75.90220970870339556, -142.7809220950004203 ) ) ;
#143536 = CARTESIAN_POINT ( 'NONE',  ( 20.85000000000000142, 87.65000000001246860, -172.9231074845242802 ) ) ;
#143537 = TOROIDAL_SURFACE ( 'NONE', #101818, 11.70000000000000639, 0.1000000000000000056 ) ;
#143538 = ORIENTED_EDGE ( 'NONE', *, *, #2562, .F. ) ;
#143539 = CIRCLE ( 'NONE', #218524, 0.1000000000000043771 ) ;
#143540 = VECTOR ( 'NONE', #6551, 1000.000000000000000 ) ;
#143541 = EDGE_CURVE ( 'NONE', #3257, #199490, #49026, .T. ) ;
#143543 = ORIENTED_EDGE ( 'NONE', *, *, #165420, .F. ) ;
#143542 = EDGE_LOOP ( 'NONE', ( #102100, #82608, #180680, #35732 ) ) ;
#143544 = VERTEX_POINT ( 'NONE', #110164 ) ;
#143546 = EDGE_CURVE ( 'NONE', #136780, #188768, #11078, .T. ) ;
#143545 = AXIS2_PLACEMENT_3D ( 'NONE', #2540, #80783, #19564 ) ;
#143547 = DIRECTION ( 'NONE',  ( 0.000000000000000000, -1.000000000000000000, -0.000000000000000000 ) ) ;
#143548 = CARTESIAN_POINT ( 'NONE',  ( -16.86420534634261514, 66.02938455442009058, -82.10477093528699299 ) ) ;
#143549 = EDGE_CURVE ( 'NONE', #49099, #108030, #12383, .T. ) ;
#143550 = ADVANCED_FACE ( 'NONE', ( #149324 ), #228846, .T. ) ;
#143552 = CARTESIAN_POINT ( 'NONE',  ( 20.95000000000000284, 11.60000000001116227, -93.57179676972454274 ) ) ;
#143551 = CARTESIAN_POINT ( 'NONE',  ( -18.50000000000000000, 1.835341550224411922, -11.55515129256298046 ) ) ;
#143553 = CARTESIAN_POINT ( 'NONE',  ( 21.05000000000000071, 67.12791932463460398, -161.5020600656926035 ) ) ;
#143554 = ORIENTED_EDGE ( 'NONE', *, *, #51129, .F. ) ;
#143555 = AXIS2_PLACEMENT_3D ( 'NONE', #16695, #32429, #194054 ) ;
#143556 = CARTESIAN_POINT ( 'NONE',  ( -20.00857864376270001, 66.85000000001254250, -182.2731074845244166 ) ) ;
#143557 = TOROIDAL_SURFACE ( 'NONE', #151964, 0.6000000000000013101, 0.1000000000000000056 ) ;
#143559 = AXIS2_PLACEMENT_3D ( 'NONE', #196021, #74815, #154360 ) ;
#143558 = DIRECTION ( 'NONE',  ( -1.020425574104004196E-15, 0.000000000000000000, -1.000000000000000000 ) ) ;
#143560 = CARTESIAN_POINT ( 'NONE',  ( -18.59999999999999787, 76.00000000001213607, -136.5231074845242745 ) ) ;
#143561 = EDGE_CURVE ( 'NONE', #123203, #248473, #253032, .T. ) ;
#143562 = CARTESIAN_POINT ( 'NONE',  ( -16.94165728009537375, 9.987869755934930538, -87.89105500851024999 ) ) ;
#143564 = ORIENTED_EDGE ( 'NONE', *, *, #149184, .F. ) ;
#143563 = VECTOR ( 'NONE', #4223, 1000.000000000000000 ) ;
#143565 = ADVANCED_FACE ( 'NONE', ( #249690 ), #94811, .T. ) ;
#143567 = ADVANCED_FACE ( 'NONE', ( #201206 ), #106911, .T. ) ;
#143566 = ADVANCED_FACE ( 'NONE', ( #171471 ), #67195, .F. ) ;
#143568 = CARTESIAN_POINT ( 'NONE',  ( 20.05000000000002913, 7.250000000000015099, -9.250000000000001776 ) ) ;
#143569 = AXIS2_PLACEMENT_3D ( 'NONE', #102688, #145680, #223929 ) ;
#143570 = CARTESIAN_POINT ( 'NONE',  ( -21.04999999999931504, 0.05132743235277388572, -94.19981666373327300 ) ) ;
#143571 = ORIENTED_EDGE ( 'NONE', *, *, #180622, .F. ) ;
#143572 = LINE ( 'NONE', #160601, #137135 ) ;
#143573 = CARTESIAN_POINT ( 'NONE',  ( 13.40000000000000036, -8.250000000000005329, 10.95857864376269575 ) ) ;
#143574 = DIRECTION ( 'NONE',  ( 1.000000000000000000, 0.000000000000000000, 0.000000000000000000 ) ) ;
#143575 = DIRECTION ( 'NONE',  ( 2.827886303505249259E-16, 0.8660254037844377084, 0.5000000000000016653 ) ) ;
#143576 = CARTESIAN_POINT ( 'NONE',  ( 20.05000000000002913, 7.250000000011171508, -180.1499999999999773 ) ) ;
#143577 = B_SPLINE_CURVE_WITH_KNOTS ( 'NONE', 3,
 ( #255185, #94879, #213540, #238242, #234387, #174485, #253944, #194009 ),
 .UNSPECIFIED., .F., .F.,
 ( 4, 2, 2, 4 ),
 ( 0.000000000000000000, 0.0002181133598168980686, 0.0003271700397253479026, 0.0004362267196337977094 ),
 .UNSPECIFIED. ) ;
#143578 = VECTOR ( 'NONE', #56215, 1000.000000000000114 ) ;
#143579 = DIRECTION ( 'NONE',  ( 0.000000000000000000, -0.9651348961777157509, 0.2617529984165031243 ) ) ;
#143581 = VERTEX_POINT ( 'NONE', #69096 ) ;
#143580 = AXIS2_PLACEMENT_3D ( 'NONE', #107807, #188625, #90798 ) ;
#143582 = DIRECTION ( 'NONE',  ( 0.000000000000000000, -1.000000000000000000, 0.000000000000000000 ) ) ;
#143583 = DIRECTION ( 'NONE',  ( -0.000000000000000000, -6.982962677686266711E-15, 1.000000000000000000 ) ) ;
#143584 = CARTESIAN_POINT ( 'NONE',  ( -21.07928932188134397, 0.09889514566555071551, -60.67148334360674511 ) ) ;
#143585 = ADVANCED_FACE ( 'NONE', ( #46925 ), #61702, .F. ) ;
#143586 = CYLINDRICAL_SURFACE ( 'NONE', #78703, 0.09999999999999939493 ) ;
#143587 = CARTESIAN_POINT ( 'NONE',  ( -18.59999999999999787, -9.321008403350132809, -107.7359382490779183 ) ) ;
#143588 = CARTESIAN_POINT ( 'NONE',  ( -21.64999999999999858, 63.44052078637213299, -222.1345147897817185 ) ) ;
#143589 = DIRECTION ( 'NONE',  ( 1.000000000000000000, 0.000000000000000000, 0.000000000000000000 ) ) ;
#143590 = ADVANCED_FACE ( 'NONE', ( #160826 ), #178424, .T. ) ;
#143591 = EDGE_CURVE ( 'NONE', #176555, #17833, #81839, .T. ) ;
#143593 = VERTEX_POINT ( 'NONE', #49521 ) ;
#143592 = CARTESIAN_POINT ( 'NONE',  ( 18.49999999999999645, 16.44800918141279311, -240.8068063186265135 ) ) ;
#143594 = EDGE_CURVE ( 'NONE', #68170, #111962, #95003, .T. ) ;
#143595 = EDGE_CURVE ( 'NONE', #258015, #55258, #20187, .T. ) ;
#143596 = DIRECTION ( 'NONE',  ( 0.000000000000000000, -0.000000000000000000, -1.000000000000000000 ) ) ;
#143597 = VECTOR ( 'NONE', #131518, 1000.000000000000000 ) ;
#143598 = AXIS2_PLACEMENT_3D ( 'NONE', #79269, #237089, #158857 ) ;
#143599 = CARTESIAN_POINT ( 'NONE',  ( -18.50211644919735576, 65.69792220476271893, -30.53355541284615171 ) ) ;
#143600 = AXIS2_PLACEMENT_3D ( 'NONE', #29284, #90482, #69666 ) ;
#143601 = CARTESIAN_POINT ( 'NONE',  ( 21.05000000000000071, 10.42338541492406279, -74.49205192387015018 ) ) ;
#143602 = ORIENTED_EDGE ( 'NONE', *, *, #242816, .T. ) ;
#143603 = DIRECTION ( 'NONE',  ( 1.000000000000000000, -0.000000000000000000, -0.000000000000000000 ) ) ;
#143604 = DIRECTION ( 'NONE',  ( 0.000000000000000000, 0.000000000000000000, 1.000000000000000000 ) ) ;
#143605 = LINE ( 'NONE', #44520, #44617 ) ;
#143606 = TOROIDAL_SURFACE ( 'NONE', #6038, 0.6000000000000013101, 0.1000000000000000056 ) ;
#143607 = ORIENTED_EDGE ( 'NONE', *, *, #154248, .T. ) ;
#143608 = DIRECTION ( 'NONE',  ( -1.000000000000000000, 0.000000000000000000, 0.000000000000000000 ) ) ;
#143610 = ORIENTED_EDGE ( 'NONE', *, *, #172745, .T. ) ;
#143609 = FACE_OUTER_BOUND ( 'NONE', #173712, .T. ) ;
#143612 = CARTESIAN_POINT ( 'NONE',  ( 21.07946286933444568, 0.07668384325640636989, 6.329037319007706053 ) ) ;
#143611 = DIRECTION ( 'NONE',  ( 0.000000000000000000, 0.000000000000000000, -1.000000000000000000 ) ) ;
#143613 = EDGE_LOOP ( 'NONE', ( #205967, #152839, #194146 ) ) ;
#143614 = AXIS2_PLACEMENT_3D ( 'NONE', #200002, #57893, #38360 ) ;
#143615 = DIRECTION ( 'NONE',  ( -0.000000000000000000, -0.000000000000000000, -1.000000000000000000 ) ) ;
#143616 = CARTESIAN_POINT ( 'NONE',  ( 20.73486653747088582, 68.75000000001222134, -149.1731074845244223 ) ) ;
#143617 = CIRCLE ( 'NONE', #118701, 2.000000000000001776 ) ;
#143618 = EDGE_LOOP ( 'NONE', ( #237751, #46774, #228445, #111674 ) ) ;
#143619 = LINE ( 'NONE', #83611, #158534 ) ;
#143620 = VECTOR ( 'NONE', #113252, 1000.000000000000000 ) ;
#143621 = CARTESIAN_POINT ( 'NONE',  ( 18.49999999999822720, 54.99329599893192722, -229.8977671155099358 ) ) ;
#143622 = DIRECTION ( 'NONE',  ( -0.000000000000000000, 0.000000000000000000, 1.000000000000000000 ) ) ;
#143623 = DIRECTION ( 'NONE',  ( 0.000000000000000000, 1.000000000000000000, 7.272083257015735086E-15 ) ) ;
#143624 = ORIENTED_EDGE ( 'NONE', *, *, #237277, .F. ) ;
#143625 = CIRCLE ( 'NONE', #64521, 14.30833333333333890 ) ;
#143626 = VERTEX_POINT ( 'NONE', #50769 ) ;
#143627 = DIRECTION ( 'NONE',  ( 0.000000000000000000, 0.000000000000000000, -1.000000000000000000 ) ) ;
#143628 = DIRECTION ( 'NONE',  ( 0.000000000000000000, -1.000000000000000000, 0.000000000000000000 ) ) ;
#143629 = CARTESIAN_POINT ( 'NONE',  ( -18.59999999999999787, 7.021664781911246322, -137.8335654018973457 ) ) ;
#143630 = ADVANCED_FACE ( 'NONE', ( #7834 ), #99265, .T. ) ;
#143631 = CARTESIAN_POINT ( 'NONE',  ( 21.05000000000000071, 10.60832956796513216, -141.5916850132954039 ) ) ;
#143632 = CYLINDRICAL_SURFACE ( 'NONE', #103466, 0.09999999999999939493 ) ;
#143634 = CARTESIAN_POINT ( 'NONE',  ( -20.54999999999999716, 1.115600667400684642E-11, -200.9999999999999432 ) ) ;
#143633 = DIRECTION ( 'NONE',  ( -1.000000000000000000, 0.000000000000000000, 0.000000000000000000 ) ) ;
#143635 = DIRECTION ( 'NONE',  ( -0.000000000000000000, 1.000000000000000000, 6.982962677686266711E-15 ) ) ;
#143636 = EDGE_CURVE ( 'NONE', #14172, #210631, #141238, .T. ) ;
#143637 = DIRECTION ( 'NONE',  ( 0.000000000000000000, 0.4721928772777346239, 0.8814952561688430555 ) ) ;
#143638 = CARTESIAN_POINT ( 'NONE',  ( -18.54159361262917827, 46.96088360856536070, -255.3053464615296377 ) ) ;
#143639 = DIRECTION ( 'NONE',  ( 1.000000000000000000, -0.000000000000000000, 0.000000000000000000 ) ) ;
#143640 = AXIS2_PLACEMENT_3D ( 'NONE', #201554, #161162, #3339 ) ;
#143642 = EDGE_LOOP ( 'NONE', ( #91245, #82077, #198755 ) ) ;
#143641 = DIRECTION ( 'NONE',  ( 1.000000000000000000, 0.000000000000000000, 0.000000000000000000 ) ) ;
#143643 = CIRCLE ( 'NONE', #131166, 0.09999999999999939493 ) ;
#143644 = CARTESIAN_POINT ( 'NONE',  ( 20.95462737510932882, 65.44321804836889100, -195.9531574279621680 ) ) ;
#143645 = FACE_OUTER_BOUND ( 'NONE', #98902, .T. ) ;
#143647 = CARTESIAN_POINT ( 'NONE',  ( -23.25000000000000000, 76.00000000001126921, -203.5231074845248997 ) ) ;
#143646 = CARTESIAN_POINT ( 'NONE',  ( -21.05000000000000071, 63.48958393997221350, -237.5313578019574265 ) ) ;
#143648 = EDGE_CURVE ( 'NONE', #218497, #118710, #211730, .T. ) ;
#143649 = EDGE_CURVE ( 'NONE', #178423, #50215, #9109, .T. ) ;
#143650 = ORIENTED_EDGE ( 'NONE', *, *, #200475, .T. ) ;
#143652 = DIRECTION ( 'NONE',  ( -1.000000000000000000, -0.000000000000000000, -0.000000000000000000 ) ) ;
#143651 = LINE ( 'NONE', #178976, #76718 ) ;
#143653 = CARTESIAN_POINT ( 'NONE',  ( -23.25000000000000000, 6.835897784820962109, -211.9460267437856373 ) ) ;
#143654 = CARTESIAN_POINT ( 'NONE',  ( 18.50000000000000000, -9.499999999988842703, -107.1001893912220879 ) ) ;
#143655 = CARTESIAN_POINT ( 'NONE',  ( -14.11361717019514472, 66.54257354752367348, -185.0230656161243701 ) ) ;
#143656 = ORIENTED_EDGE ( 'NONE', *, *, #247152, .F. ) ;
#143657 = ORIENTED_EDGE ( 'NONE', *, *, #68339, .F. ) ;
#143658 = DIRECTION ( 'NONE',  ( 1.000000000000000000, -0.000000000000000000, -0.000000000000000000 ) ) ;
#143659 = VERTEX_POINT ( 'NONE', #189029 ) ;
#143660 = FACE_OUTER_BOUND ( 'NONE', #71804, .T. ) ;
#143661 = TOROIDAL_SURFACE ( 'NONE', #239342, 0.2000000000000000111, 0.1000000000000000056 ) ;
#143662 = EDGE_LOOP ( 'NONE', ( #49296, #38190, #16547, #157855, #220530, #26078, #33518, #118749, #60122, #80199, #91223, #47417, #183837, #199025 ) ) ;
#143663 = ADVANCED_FACE ( 'NONE', ( #249021 ), #70399, .F. ) ;
#143664 = CARTESIAN_POINT ( 'NONE',  ( 21.05000000000000071, 42.92370456684775348, -239.4578053278609104 ) ) ;
#143665 = EDGE_CURVE ( 'NONE', #113007, #113044, #194984, .T. ) ;
#143666 = CARTESIAN_POINT ( 'NONE',  ( 21.14999999999999858, 59.16775194334852728, -221.0793150863668473 ) ) ;
#143667 = AXIS2_PLACEMENT_3D ( 'NONE', #72820, #195333, #251426 ) ;
#143668 = CARTESIAN_POINT ( 'NONE',  ( -20.99780126800941815, 62.98982820228309265, -207.1569994557045788 ) ) ;
#143669 = ORIENTED_EDGE ( 'NONE', *, *, #54750, .F. ) ;
#143670 = B_SPLINE_CURVE_WITH_KNOTS ( 'NONE', 3,
 ( #206169, #147476, #169655, #249162, #70540, #2179, #194336 ),
 .UNSPECIFIED., .F., .F.,
 ( 4, 3, 4 ),
 ( 0.000000000000000000, 0.0009834301579440022593, 0.001767853679402679300 ),
 .UNSPECIFIED. ) ;
#143671 = CARTESIAN_POINT ( 'NONE',  ( -23.25000000000000000, 76.00000000001267608, -203.5231074845243597 ) ) ;
#143672 = CARTESIAN_POINT ( 'NONE',  ( -21.13422380238980125, 65.53162686811064930, -242.1220625181933030 ) ) ;
#143673 = LINE ( 'NONE', #180251, #28541 ) ;
#143674 = CARTESIAN_POINT ( 'NONE',  ( 21.05000000000000071, -9.399999999988846611, -43.39396912265245021 ) ) ;
#143675 = CYLINDRICAL_SURFACE ( 'NONE', #163904, 0.1000000000000028644 ) ;
#143676 = EDGE_CURVE ( 'NONE', #100043, #256383, #140800, .T. ) ;
#143677 = DIRECTION ( 'NONE',  ( -1.000000000000000000, -0.000000000000000000, 0.000000000000000000 ) ) ;
#143678 = CARTESIAN_POINT ( 'NONE',  ( 15.74999999999999645, 62.59162599727320497, -217.2417264603073477 ) ) ;
#143680 = ORIENTED_EDGE ( 'NONE', *, *, #144790, .F. ) ;
#143679 = ADVANCED_FACE ( 'NONE', ( #6529 ), #182514, .F. ) ;
#143682 = DIRECTION ( 'NONE',  ( 1.000000000000000000, 0.000000000000000000, -0.000000000000000000 ) ) ;
#143681 = CARTESIAN_POINT ( 'NONE',  ( -20.64999999999999858, 7.150000000000000355, -12.25000000000000000 ) ) ;
#143683 = ORIENTED_EDGE ( 'NONE', *, *, #44961, .T. ) ;
#143685 = EDGE_LOOP ( 'NONE', ( #57173, #220851, #227199 ) ) ;
#143684 = DIRECTION ( 'NONE',  ( 0.000000000000000000, 7.056502275159890832E-15, -1.000000000000000000 ) ) ;
#143686 = AXIS2_PLACEMENT_3D ( 'NONE', #133489, #91796, #136025 ) ;
#143687 = VERTEX_POINT ( 'NONE', #146037 ) ;
#143688 = VECTOR ( 'NONE', #180302, 1000.000000000000000 ) ;
#143689 = DIRECTION ( 'NONE',  ( -1.000000000000000000, -0.000000000000000000, -0.000000000000000000 ) ) ;
#143690 = CYLINDRICAL_SURFACE ( 'NONE', #92549, 0.1000000000000028644 ) ;
#143691 = DIRECTION ( 'NONE',  ( 0.000000000000000000, 6.982962677686266711E-15, -1.000000000000000000 ) ) ;
#143692 = DIRECTION ( 'NONE',  ( 1.000000000000000000, -0.000000000000000000, -0.000000000000000000 ) ) ;
#143693 = ORIENTED_EDGE ( 'NONE', *, *, #2902, .T. ) ;
#143694 = FACE_OUTER_BOUND ( 'NONE', #201191, .T. ) ;
#143695 = FACE_OUTER_BOUND ( 'NONE', #216062, .T. ) ;
#143696 = ADVANCED_FACE ( 'NONE', ( #16824 ), #240757, .T. ) ;
#143697 = ORIENTED_EDGE ( 'NONE', *, *, #157635, .F. ) ;
#143698 = EDGE_CURVE ( 'NONE', #234543, #5211, #235841, .T. ) ;
#143699 = CARTESIAN_POINT ( 'NONE',  ( 18.69999999999999929, -1.885425182446134107, -11.49641995933507843 ) ) ;
#143701 = CIRCLE ( 'NONE', #147810, 0.1000000000000003386 ) ;
#143700 = DIRECTION ( 'NONE',  ( 1.000000000000000000, 0.000000000000000000, 0.000000000000000000 ) ) ;
#143702 = ADVANCED_FACE ( 'NONE', ( #213717 ), #112072, .T. ) ;
#143703 = VERTEX_POINT ( 'NONE', #96321 ) ;
#143704 = CARTESIAN_POINT ( 'NONE',  ( -16.80891096016330266, 9.950000000011137047, -146.6323371927319101 ) ) ;
#143705 = AXIS2_PLACEMENT_3D ( 'NONE', #179531, #38726, #118255 ) ;
#143706 = CIRCLE ( 'NONE', #89526, 1.500000000000001332 ) ;
#143707 = VERTEX_POINT ( 'NONE', #251557 ) ;
#143708 = CARTESIAN_POINT ( 'NONE',  ( -23.25000000000000000, 6.268811756569107274, -220.3853799378769622 ) ) ;
#143709 = VERTEX_POINT ( 'NONE', #255357 ) ;
#143710 = DIRECTION ( 'NONE',  ( 1.000000000000000000, -0.000000000000000000, -0.000000000000000000 ) ) ;
#143711 = STYLED_ITEM ( 'NONE', ( #177593 ), #179045 ) ;
#143712 = DIRECTION ( 'NONE',  ( 0.000000000000000000, 0.9126074666063545004, 0.4088369013363783999 ) ) ;
#143713 = FACE_OUTER_BOUND ( 'NONE', #245182, .T. ) ;
#143714 = ADVANCED_FACE ( 'NONE', ( #35127 ), #191631, .F. ) ;
#143715 = DIRECTION ( 'NONE',  ( 0.000000000000000000, -1.000000000000000000, 0.000000000000000000 ) ) ;
#143716 = EDGE_CURVE ( 'NONE', #14542, #196907, #53498, .T. ) ;
#143717 = CARTESIAN_POINT ( 'NONE',  ( 18.49999999999999289, 6.846123162363745074, -104.2377262668499043 ) ) ;
#143718 = CARTESIAN_POINT ( 'NONE',  ( -21.14999999999999858, 9.997527148596390134, -228.1702915402975691 ) ) ;
#143719 = CARTESIAN_POINT ( 'NONE',  ( 21.00000000000000000, 0.3305886640091971196, 0.04453801223857078301 ) ) ;
#143720 = CIRCLE ( 'NONE', #210550, 2.000000000000001776 ) ;
#143721 = VERTEX_POINT ( 'NONE', #36397 ) ;
#143723 = CARTESIAN_POINT ( 'NONE',  ( -20.94999999999999929, -1.849153571964891274, -112.1059666197971012 ) ) ;
#143722 = CARTESIAN_POINT ( 'NONE',  ( -21.13435531349785634, 69.50627893642028710, -170.0231074845243882 ) ) ;
#143724 = CIRCLE ( 'NONE', #160509, 11.75000000000000355 ) ;
#143725 = VECTOR ( 'NONE', #59615, 1000.000000000000227 ) ;
#143726 = ORIENTED_EDGE ( 'NONE', *, *, #141707, .F. ) ;
#143727 = CARTESIAN_POINT ( 'NONE',  ( -18.47690164073607377, 85.46484453802463577, -163.3217265446882323 ) ) ;
#143728 = CARTESIAN_POINT ( 'NONE',  ( -20.85000000000000142, 1.115600667400684642E-11, -74.90000000000000568 ) ) ;
#143730 = ORIENTED_EDGE ( 'NONE', *, *, #225924, .F. ) ;
#143729 = CARTESIAN_POINT ( 'NONE',  ( 21.14999999999999858, 10.71339244341104013, -146.2500000000000568 ) ) ;
#143732 = ORIENTED_EDGE ( 'NONE', *, *, #207675, .T. ) ;
#143731 = DIRECTION ( 'NONE',  ( -1.000000000000000000, 0.000000000000000000, -0.000000000000000000 ) ) ;
#143733 = SURFACE_STYLE_USAGE ( .BOTH. , #42098 ) ;
#143734 = DIRECTION ( 'NONE',  ( 0.000000000000000000, -0.9274965247785555977, 0.3738317757009190223 ) ) ;
#143735 = CARTESIAN_POINT ( 'NONE',  ( 21.30000000000002558, 1.148907358139439339E-11, -201.0000000000015064 ) ) ;
#143736 = DIRECTION ( 'NONE',  ( 1.000000000000000000, 0.000000000000000000, 0.000000000000000000 ) ) ;
#143737 = AXIS2_PLACEMENT_3D ( 'NONE', #1625, #83700, #44627 ) ;
#143738 = CIRCLE ( 'NONE', #110999, 11.79999999999999716 ) ;
#143740 = ORIENTED_EDGE ( 'NONE', *, *, #116386, .F. ) ;
#143739 = DIRECTION ( 'NONE',  ( 1.000000000000000000, -0.000000000000000000, -0.000000000000000000 ) ) ;
#143741 = CARTESIAN_POINT ( 'NONE',  ( -20.85000000000000142, 87.75000000001215028, -136.5231074845242745 ) ) ;
#143742 = VERTEX_POINT ( 'NONE', #75521 ) ;
#143743 = ORIENTED_EDGE ( 'NONE', *, *, #151533, .F. ) ;
#143744 = AXIS2_PLACEMENT_3D ( 'NONE', #252371, #214542, #97125 ) ;
#143745 = FACE_OUTER_BOUND ( 'NONE', #230632, .T. ) ;
#143746 = CARTESIAN_POINT ( 'NONE',  ( -21.05000000000000071, 4.272272088314018390, -245.4186996786394843 ) ) ;
#143747 = CIRCLE ( 'NONE', #127190, 0.5000000000000004441 ) ;
#143749 = VERTEX_POINT ( 'NONE', #194181 ) ;
#143748 = CIRCLE ( 'NONE', #127192, 0.09999999999999568956 ) ;
#143750 = LINE ( 'NONE', #9373, #250012 ) ;
#143751 = CARTESIAN_POINT ( 'NONE',  ( -16.86757978335471364, 9.965650379045438712, -180.0980046531674930 ) ) ;
#143752 = ORIENTED_EDGE ( 'NONE', *, *, #142522, .F. ) ;
#143753 = FACE_OUTER_BOUND ( 'NONE', #162051, .T. ) ;
#143754 = CARTESIAN_POINT ( 'NONE',  ( -23.15000000000000213, 51.38014393322265505, -230.1906178717505611 ) ) ;
#143755 = ORIENTED_EDGE ( 'NONE', *, *, #125053, .T. ) ;
#143756 = VERTEX_POINT ( 'NONE', #211158 ) ;
#143757 = CARTESIAN_POINT ( 'NONE',  ( -18.46154800491015990, -9.480206274230827290, -73.65745083838122298 ) ) ;
#143758 = EDGE_LOOP ( 'NONE', ( #175149, #81472, #164065, #161805 ) ) ;
#143760 = EDGE_CURVE ( 'NONE', #252923, #106008, #38479, .T. ) ;
#143759 = ORIENTED_EDGE ( 'NONE', *, *, #70424, .T. ) ;
#143762 = ORIENTED_EDGE ( 'NONE', *, *, #158632, .T. ) ;
#143761 = DIRECTION ( 'NONE',  ( 0.000000000000000000, 0.000000000000000000, 1.000000000000000000 ) ) ;
#143763 = CARTESIAN_POINT ( 'NONE',  ( 20.94999999999999929, 64.35000000001218723, -143.3647081744214802 ) ) ;
#143764 = VERTEX_POINT ( 'NONE', #72965 ) ;
#143765 = CIRCLE ( 'NONE', #35671, 14.30833333333335133 ) ;
#143766 = EDGE_CURVE ( 'NONE', #81187, #245289, #12984, .T. ) ;
#143767 = CARTESIAN_POINT ( 'NONE',  ( -22.47007471830798409, 1.116756697967097312E-11, -92.77928934807356143 ) ) ;
#143768 = EDGE_CURVE ( 'NONE', #245837, #222623, #113338, .T. ) ;
#143769 = ORIENTED_EDGE ( 'NONE', *, *, #142021, .T. ) ;
#143770 = AXIS2_PLACEMENT_3D ( 'NONE', #115532, #195103, #98494 ) ;
#143772 = ORIENTED_EDGE ( 'NONE', *, *, #137167, .F. ) ;
#143771 = VERTEX_POINT ( 'NONE', #14262 ) ;
#143773 = CARTESIAN_POINT ( 'NONE',  ( -18.39999999999999858, 85.68240343348806221, -62.86626410711144786 ) ) ;
#143774 = AXIS2_PLACEMENT_3D ( 'NONE', #93710, #175839, #57125 ) ;
#143775 = CARTESIAN_POINT ( 'NONE',  ( -21.05000000000000071, 56.02567683926420727, -227.9999002286039058 ) ) ;
#143776 = ORIENTED_EDGE ( 'NONE', *, *, #209246, .F. ) ;
#143777 = AXIS2_PLACEMENT_3D ( 'NONE', #21281, #82472, #39567 ) ;
#143778 = AXIS2_PLACEMENT_3D ( 'NONE', #112178, #212557, #173475 ) ;
#143779 = ORIENTED_EDGE ( 'NONE', *, *, #192235, .T. ) ;
#143780 = ADVANCED_FACE ( 'NONE', ( #52060 ), #216277, .F. ) ;
#143781 = DIRECTION ( 'NONE',  ( -1.073024830501117528E-15, -0.8814952561688430555, 0.4721928772777346239 ) ) ;
#143782 = DIRECTION ( 'NONE',  ( 0.000000000000000000, 0.9126074666063660468, 0.4088369013363524762 ) ) ;
#143783 =( BOUNDED_SURFACE ( )  B_SPLINE_SURFACE ( 3, 2, ( 
 ( #114441, #247534, #197814 ),
 ( #16636, #175720, #140402 ),
 ( #98676, #239525, #255168 ),
 ( #238225, #38758, #118297 ) ),
 .UNSPECIFIED., .F., .F., .F. ) 
 B_SPLINE_SURFACE_WITH_KNOTS ( ( 4, 4 ),
 ( 3, 3 ),
 ( 0.0008258556059633777964, 0.0009616864997632780781 ),
 ( 0.000000000000000000, 1.000000000000000000 ),
 .UNSPECIFIED. ) 
 GEOMETRIC_REPRESENTATION_ITEM ( )  RATIONAL_B_SPLINE_SURFACE ( (
 ( 1.000000000000000000, 0.9152888060719349683, 1.000000000000000000),
 ( 1.000000000000000000, 0.9327727094138136277, 1.000000000000000000),
 ( 1.000000000000000000, 0.9369023509258470606, 1.000000000000000000),
 ( 1.000000000000000000, 0.9246339933864458072, 1.000000000000000000) ) ) 
 REPRESENTATION_ITEM ( '' )  SURFACE ( )  );
#143785 = ORIENTED_EDGE ( 'NONE', *, *, #73739, .T. ) ;
#143784 = DIRECTION ( 'NONE',  ( 1.000000000000000000, 0.000000000000000000, 0.000000000000000000 ) ) ;
#143786 = FACE_OUTER_BOUND ( 'NONE', #66234, .T. ) ;
#143787 = VERTEX_POINT ( 'NONE', #91217 ) ;
#143788 = DIRECTION ( 'NONE',  ( 0.000000000000000000, 0.7035695228903320331, 0.7106264324241468033 ) ) ;
#143789 = DIRECTION ( 'NONE',  ( 0.000000000000000000, -0.4088369013363281623, 0.9126074666063771490 ) ) ;
#143790 = AXIS2_PLACEMENT_3D ( 'NONE', #12095, #92877, #31664 ) ;
#143791 = ORIENTED_EDGE ( 'NONE', *, *, #208992, .T. ) ;
#143792 = CARTESIAN_POINT ( 'NONE',  ( -22.50000000000000000, 64.35042919246734527, -136.6231074845243825 ) ) ;
#143793 = DIRECTION ( 'NONE',  ( 0.000000000000000000, -0.2617529984164506107, -0.9651348961777299618 ) ) ;
#143794 = VECTOR ( 'NONE', #230543, 1000.000000000000000 ) ;
#143795 = VERTEX_POINT ( 'NONE', #170801 ) ;
#143796 = CARTESIAN_POINT ( 'NONE',  ( 20.99999999999999645, 9.750000000011137757, -76.25000000000004263 ) ) ;
#143797 = ORIENTED_EDGE ( 'NONE', *, *, #125298, .T. ) ;
#143799 = EDGE_LOOP ( 'NONE', ( #29860, #50498, #145794, #147253 ) ) ;
#143798 = EDGE_LOOP ( 'NONE', ( #244570, #184418, #97320, #66605 ) ) ;
#143800 = ORIENTED_EDGE ( 'NONE', *, *, #82726, .T. ) ;
#143801 = CARTESIAN_POINT ( 'NONE',  ( -18.38639463286148867, 11.48019957384713230, -42.75000000000000000 ) ) ;
#143802 = EDGE_CURVE ( 'NONE', #251152, #171702, #250284, .T. ) ;
#143803 = VERTEX_POINT ( 'NONE', #172068 ) ;
#143804 = ADVANCED_FACE ( 'NONE', ( #237140 ), #49205, .F. ) ;
#143805 = FACE_OUTER_BOUND ( 'NONE', #137821, .T. ) ;
#143806 = AXIS2_PLACEMENT_3D ( 'NONE', #173991, #33189, #213056 ) ;
#143807 = ORIENTED_EDGE ( 'NONE', *, *, #152507, .F. ) ;
#143808 = CARTESIAN_POINT ( 'NONE',  ( 23.15000000000000213, -11.64999999998883595, -164.4000000000000057 ) ) ;
#143809 = FACE_OUTER_BOUND ( 'NONE', #78344, .T. ) ;
#143810 = ORIENTED_EDGE ( 'NONE', *, *, #142897, .F. ) ;
#143812 = ADVANCED_FACE ( 'NONE', ( #200575 ), #228292, .T. ) ;
#143811 = ORIENTED_EDGE ( 'NONE', *, *, #65672, .T. ) ;
#143813 = ORIENTED_EDGE ( 'NONE', *, *, #116960, .F. ) ;
#143814 = AXIS2_PLACEMENT_3D ( 'NONE', #220210, #254174, #155130 ) ;
#143815 = VERTEX_POINT ( 'NONE', #1062 ) ;
#143816 = DIRECTION ( 'NONE',  ( 1.000000000000000000, -3.151514657663852580E-16, 8.547182517843351137E-17 ) ) ;
#143817 = CARTESIAN_POINT ( 'NONE',  ( -18.59999999999999787, 42.98415524044399660, -233.9519173640447889 ) ) ;
#143818 = DIRECTION ( 'NONE',  ( 0.000000000000000000, 3.122502256758250246E-14, -1.000000000000000000 ) ) ;
#143819 = DIRECTION ( 'NONE',  ( 0.000000000000000000, -0.9654727137038715545, 0.2605042016806676242 ) ) ;
#143820 = CARTESIAN_POINT ( 'NONE',  ( 21.05000000000000071, 65.31570632562512913, -162.4964335458869016 ) ) ;
#143821 = CARTESIAN_POINT ( 'NONE',  ( 20.94999999999999929, 76.00000000001205080, -123.5481074845242802 ) ) ;
#143822 = B_SPLINE_CURVE_WITH_KNOTS ( 'NONE', 3,
 ( #87547, #27632, #227065, #246630, #184094, #108420, #229650, #65430, #185382, #228370 ),
 .UNSPECIFIED., .F., .F.,
 ( 4, 2, 2, 2, 4 ),
 ( 0.000000000000000000, 0.0003916577441626822214, 0.0005874866162440240368, 0.0006854010522846949987, 0.0007833154883253658522 ),
 .UNSPECIFIED. ) ;
#143824 = ADVANCED_FACE ( 'NONE', ( #19379, #101425 ), #98874, .T. ) ;
#143823 = DIRECTION ( 'NONE',  ( 0.000000000000000000, -6.982962677686266711E-15, 1.000000000000000000 ) ) ;
#143826 = CARTESIAN_POINT ( 'NONE',  ( 21.12757541349815682, 6.473380571262609351, -100.4948387841902786 ) ) ;
#143825 = LINE ( 'NONE', #79983, #48760 ) ;
#143827 = DIRECTION ( 'NONE',  ( 1.000000000000000000, 0.000000000000000000, 0.000000000000000000 ) ) ;
#143828 = CARTESIAN_POINT ( 'NONE',  ( -21.05000000000000426, 64.40000000001208491, -129.5949042542488314 ) ) ;
#143829 = DIRECTION ( 'NONE',  ( 0.000000000000000000, 0.000000000000000000, 1.000000000000000000 ) ) ;
#143830 = PLANE ( 'NONE',  #147094 ) ;
#143831 = AXIS2_PLACEMENT_3D ( 'NONE', #249703, #256056, #115316 ) ;
#143832 = ORIENTED_EDGE ( 'NONE', *, *, #70547, .F. ) ;
#143833 = B_SPLINE_CURVE_WITH_KNOTS ( 'NONE', 3,
 ( #241466, #6693, #84915, #25005, #83626, #201046, #82347, #141081, #245318, #161942, #41996, #142348, #163217, #221865 ),
 .UNSPECIFIED., .F., .F.,
 ( 4, 2, 2, 2, 2, 2, 4 ),
 ( 0.000000000000000000, 2.389617747644273823E-05, 4.779235495288547647E-05, 9.558470990577095294E-05, 0.0001911694198115423396, 0.0003823388396230035808, 0.0007646776792460092216 ),
 .UNSPECIFIED. ) ;
#143834 = EDGE_CURVE ( 'NONE', #171717, #214033, #186788, .T. ) ;
#143835 = CIRCLE ( 'NONE', #31465, 0.09999999999999939493 ) ;
#143837 = ORIENTED_EDGE ( 'NONE', *, *, #32906, .F. ) ;
#143836 = LINE ( 'NONE', #44760, #182234 ) ;
#143838 = EDGE_LOOP ( 'NONE', ( #59107, #45651, #26446, #121660 ) ) ;
#143839 = LINE ( 'NONE', #99562, #99253 ) ;
#143840 = CARTESIAN_POINT ( 'NONE',  ( -20.64999999999999858, 7.150000000011155876, -54.65000000000000568 ) ) ;
#143841 = EDGE_CURVE ( 'NONE', #197693, #29779, #107648, .T. ) ;
#143842 = EDGE_CURVE ( 'NONE', #125974, #231927, #221398, .T. ) ;
#143843 = FACE_OUTER_BOUND ( 'NONE', #118013, .T. ) ;
#143844 = VERTEX_POINT ( 'NONE', #119784 ) ;
#143845 =( NAMED_UNIT ( * ) PLANE_ANGLE_UNIT ( ) SI_UNIT ( $, .RADIAN. ) );
#143846 = CARTESIAN_POINT ( 'NONE',  ( -20.12071067811865888, 9.320710678129810134, -45.85000000000000142 ) ) ;
#143847 = CARTESIAN_POINT ( 'NONE',  ( 18.39999999999999503, 11.47316190337363828, -121.3500000000000369 ) ) ;
#143848 = VERTEX_POINT ( 'NONE', #240996 ) ;
#143849 = EDGE_CURVE ( 'NONE', #81803, #116247, #80600, .T. ) ;
#143851 = DIRECTION ( 'NONE',  ( 0.000000000000000000, -0.4088369013363280513, 0.9126074666063769270 ) ) ;
#143850 = CIRCLE ( 'NONE', #189665, 7.900000000000000355 ) ;
#143852 = AXIS2_PLACEMENT_3D ( 'NONE', #181158, #2487, #99004 ) ;
#143853 = DIRECTION ( 'NONE',  ( 0.000000000000000000, 0.000000000000000000, -1.000000000000000000 ) ) ;
#143854 = ADVANCED_FACE ( 'NONE', ( #21952 ), #102729, .T. ) ;
#143855 = LINE ( 'NONE', #172475, #13872 ) ;
#143856 = DIRECTION ( 'NONE',  ( 0.000000000000000000, 1.000000000000000000, 0.000000000000000000 ) ) ;
#143858 = ORIENTED_EDGE ( 'NONE', *, *, #137025, .F. ) ;
#143857 = CARTESIAN_POINT ( 'NONE',  ( -15.55912972643740488, 67.50912972644923116, -82.17310748452437963 ) ) ;
#143859 = EDGE_CURVE ( 'NONE', #119221, #224911, #253400, .T. ) ;
#143860 = DIRECTION ( 'NONE',  ( 1.000000000000000000, -2.986185139342071370E-16, 6.665775143889693760E-16 ) ) ;
#143862 = EDGE_LOOP ( 'NONE', ( #243281, #71643, #25901 ) ) ;
#143861 = CARTESIAN_POINT ( 'NONE',  ( 23.14999999999999503, 6.650000000011155876, -45.75000000000000711 ) ) ;
#143863 = CARTESIAN_POINT ( 'NONE',  ( -20.54999999999999716, 2.000000000011154189, -80.22462192276213955 ) ) ;
#143864 = LINE ( 'NONE', #219547, #4185 ) ;
#143865 = ORIENTED_EDGE ( 'NONE', *, *, #140661, .F. ) ;
#143866 = CARTESIAN_POINT ( 'NONE',  ( -17.29158576265544056, 10.36474766602906783, -78.41724175520788265 ) ) ;
#143867 = DIRECTION ( 'NONE',  ( 1.000000000000000000, -0.000000000000000000, -0.000000000000000000 ) ) ;
#143868 = EDGE_CURVE ( 'NONE', #186535, #187411, #123614, .T. ) ;
#143870 = FACE_OUTER_BOUND ( 'NONE', #128505, .T. ) ;
#143869 = CARTESIAN_POINT ( 'NONE',  ( -16.93521499325732549, 63.05745603785386777, -213.0607812399036050 ) ) ;
#143871 = LINE ( 'NONE', #145150, #99595 ) ;
#143872 = DIRECTION ( 'NONE',  ( 1.000000000000000000, 0.000000000000000000, -0.000000000000000000 ) ) ;
#143873 = CIRCLE ( 'NONE', #48026, 14.20833333333334281 ) ;
#143874 = CARTESIAN_POINT ( 'NONE',  ( -18.58222699835055280, 10.33200063079656417, -39.09316749566429650 ) ) ;
#143875 = CARTESIAN_POINT ( 'NONE',  ( 20.90000000000000213, -1.899104650876408451, -11.59795743183152972 ) ) ;
#143876 = CIRCLE ( 'NONE', #35589, 0.09999999999999939493 ) ;
#143877 = DIRECTION ( 'NONE',  ( 0.000000000000000000, 0.000000000000000000, -1.000000000000000000 ) ) ;
#143878 = ADVANCED_FACE ( 'NONE', ( #122328 ), #238419, .F. ) ;
#143879 = ADVANCED_FACE ( 'NONE', ( #199306 ), #11831, .F. ) ;
#143880 = AXIS2_PLACEMENT_3D ( 'NONE', #183064, #166093, #205161 ) ;
#143881 = ORIENTED_EDGE ( 'NONE', *, *, #119206, .F. ) ;
#143882 = AXIS2_PLACEMENT_3D ( 'NONE', #132915, #189028, #28717 ) ;
#143883 = DIRECTION ( 'NONE',  ( 0.000000000000000000, -0.9908441862701610203, 0.1350103645451807555 ) ) ;
#143884 = ORIENTED_EDGE ( 'NONE', *, *, #92641, .F. ) ;
#143885 =( BOUNDED_CURVE ( )  B_SPLINE_CURVE ( 3, ( #155885, #16366, #256170, #197541 ),
 .UNSPECIFIED., .F., .T. ) 
 B_SPLINE_CURVE_WITH_KNOTS ( ( 4, 4 ),
 ( 4.712388980384690562, 5.672655318024762749 ),
 .UNSPECIFIED. ) 
 CURVE ( )  GEOMETRIC_REPRESENTATION_ITEM ( )  RATIONAL_B_SPLINE_CURVE ( ( 1.000000000000000000, 0.9246222802177245237, 0.9246222802177245237, 1.000000000000000000 ) ) 
 REPRESENTATION_ITEM ( '' )  );
#143886 = ORIENTED_EDGE ( 'NONE', *, *, #210509, .F. ) ;
#143887 = EDGE_CURVE ( 'NONE', #165812, #246837, #140592, .T. ) ;
#143888 = CARTESIAN_POINT ( 'NONE',  ( -20.90000000000000213, -1.901609089591594470, -11.59510167572422112 ) ) ;
#143889 = DIRECTION ( 'NONE',  ( 1.000000000000000000, 0.000000000000000000, 0.000000000000000000 ) ) ;
#143890 = ORIENTED_EDGE ( 'NONE', *, *, #137976, .T. ) ;
#143891 = ADVANCED_FACE ( 'NONE', ( #63630 ), #111754, .T. ) ;
#143892 = ADVANCED_FACE ( 'NONE', ( #83154 ), #78052, .F. ) ;
#143893 = ORIENTED_EDGE ( 'NONE', *, *, #766, .F. ) ;
#143894 = EDGE_CURVE ( 'NONE', #155635, #245692, #177197, .T. ) ;
#143895 = ORIENTED_EDGE ( 'NONE', *, *, #218081, .T. ) ;
#143896 = LINE ( 'NONE', #241723, #162655 ) ;
#143897 = VECTOR ( 'NONE', #153457, 1000.000000000000000 ) ;
#143898 = ORIENTED_EDGE ( 'NONE', *, *, #233944, .T. ) ;
#143899 = CIRCLE ( 'NONE', #85602, 0.09999999999998898659 ) ;
#143900 = FACE_OUTER_BOUND ( 'NONE', #5290, .T. ) ;
#143901 = FACE_OUTER_BOUND ( 'NONE', #155122, .T. ) ;
#143902 = AXIS2_PLACEMENT_3D ( 'NONE', #234491, #96256, #54572 ) ;
#143903 = DIRECTION ( 'NONE',  ( -0.000000000000000000, 0.8874830700839094755, -0.4608403197577646826 ) ) ;
#143904 = CARTESIAN_POINT ( 'NONE',  ( -18.50000000000000000, 11.65000000001115588, -167.5000000000000284 ) ) ;
#143905 = DIRECTION ( 'NONE',  ( -0.000000000000000000, -6.982962677686266711E-15, 1.000000000000000000 ) ) ;
#143908 = EDGE_LOOP ( 'NONE', ( #239155, #56212, #18408, #227732 ) ) ;
#143907 = CARTESIAN_POINT ( 'NONE',  ( -23.15000000000000213, 70.05000000001197691, -113.3288097895591591 ) ) ;
#143906 = CIRCLE ( 'NONE', #43952, 0.09999999999999939493 ) ;
#143910 = DIRECTION ( 'NONE',  ( 1.000000000000000000, 3.265361837132813093E-16, -0.000000000000000000 ) ) ;
#143909 = CARTESIAN_POINT ( 'NONE',  ( 23.15000000000000213, 62.12679871018153932, -248.6611778639222337 ) ) ;
#143911 = EDGE_CURVE ( 'NONE', #13111, #159544, #167901, .T. ) ;
#143912 = VERTEX_POINT ( 'NONE', #247392 ) ;
#143913 = AXIS2_PLACEMENT_3D ( 'NONE', #152726, #56134, #255586 ) ;
#143914 = CARTESIAN_POINT ( 'NONE',  ( -20.54999999999999716, 1.940186915899009490, -79.82911921105336717 ) ) ;
#143915 = DIRECTION ( 'NONE',  ( 1.000000000000000000, 9.312479980434134033E-16, 4.171876297610248080E-16 ) ) ;
#143916 = AXIS2_PLACEMENT_3D ( 'NONE', #202107, #143406, #1313 ) ;
#143918 = ORIENTED_EDGE ( 'NONE', *, *, #762, .F. ) ;
#143917 = TOROIDAL_SURFACE ( 'NONE', #227310, 0.2000000000000000111, 0.1000000000000000056 ) ;
#143920 = DIRECTION ( 'NONE',  ( 0.000000000000000000, 0.1575844902526835067, 0.9875055080513738259 ) ) ;
#143919 = DIRECTION ( 'NONE',  ( -1.000000000000000000, 0.000000000000000000, 0.000000000000000000 ) ) ;
#143921 = CARTESIAN_POINT ( 'NONE',  ( -18.79999999999999716, 11.50977166988710820, 1.786320531569725478 ) ) ;
#143922 = ORIENTED_EDGE ( 'NONE', *, *, #217386, .F. ) ;
#143923 = CIRCLE ( 'NONE', #10850, 0.09999999999999939493 ) ;
#143924 = CARTESIAN_POINT ( 'NONE',  ( 21.05000000000000426, 6.496686585778579826, -67.01465611851199355 ) ) ;
#143925 = CARTESIAN_POINT ( 'NONE',  ( 20.94999999999999929, -8.999999999988842703, -57.60603087734755690 ) ) ;
#143926 = VECTOR ( 'NONE', #198628, 1000.000000000000114 ) ;
#143927 = FACE_OUTER_BOUND ( 'NONE', #148324, .T. ) ;
#143928 = CARTESIAN_POINT ( 'NONE',  ( 20.90000000000000213, 1.311673547813416718, -7.986648289447971116 ) ) ;
#143929 = ORIENTED_EDGE ( 'NONE', *, *, #79424, .F. ) ;
#143930 = AXIS2_PLACEMENT_3D ( 'NONE', #27605, #105786, #47104 ) ;
#143931 = AXIS2_PLACEMENT_3D ( 'NONE', #212600, #200404, #120894 ) ;
#143932 = VERTEX_POINT ( 'NONE', #127459 ) ;
#143933 = FACE_OUTER_BOUND ( 'NONE', #111319, .T. ) ;
#143934 = DIRECTION ( 'NONE',  ( 0.000000000000000000, 0.9910827722268055195, -0.1332476588733540468 ) ) ;
#143935 = EDGE_CURVE ( 'NONE', #151091, #158360, #128754, .T. ) ;
#143936 = LINE ( 'NONE', #203912, #12044 ) ;
#143937 = DIRECTION ( 'NONE',  ( -3.469446951953772592E-14, -0.9651348961777379554, 0.2617529984164210233 ) ) ;
#143938 = DIRECTION ( 'NONE',  ( 0.000000000000000000, -0.1332476588733448597, -0.9910827722268067408 ) ) ;
#143939 = ADVANCED_FACE ( 'NONE', ( #164026 ), #198664, .F. ) ;
#143940 = CARTESIAN_POINT ( 'NONE',  ( 18.49999999999999645, 1.728086936805617757, -154.3844350051677452 ) ) ;
#143942 = ORIENTED_EDGE ( 'NONE', *, *, #153960, .T. ) ;
#143941 = CYLINDRICAL_SURFACE ( 'NONE', #171247, 0.09999999999999939493 ) ;
#143943 = FACE_OUTER_BOUND ( 'NONE', #141435, .T. ) ;
#143944 = CARTESIAN_POINT ( 'NONE',  ( 20.94999999999999574, 74.26374286841490857, -158.4544551555068779 ) ) ;
#143945 = CARTESIAN_POINT ( 'NONE',  ( -21.10320863425827298, 75.97497774878459609, -75.92338487098355415 ) ) ;
#143946 = LINE ( 'NONE', #223478, #113800 ) ;
#143947 = EDGE_CURVE ( 'NONE', #83073, #105461, #206999, .T. ) ;
#143948 = LINE ( 'NONE', #241767, #38169 ) ;
#143950 = VERTEX_POINT ( 'NONE', #28400 ) ;
#143949 = LINE ( 'NONE', #223480, #6800 ) ;
#143951 = DIRECTION ( 'NONE',  ( 0.000000000000000000, 1.000000000000000000, 0.000000000000000000 ) ) ;
#143952 = CARTESIAN_POINT ( 'NONE',  ( 21.14999999999999858, 76.10000000001276987, -215.1726782920691505 ) ) ;
#143953 = DIRECTION ( 'NONE',  ( -1.000000000000000000, -0.000000000000000000, -0.000000000000000000 ) ) ;
#143954 = DIRECTION ( 'NONE',  ( 0.000000000000000000, -7.147358527629762208E-15, 1.000000000000000000 ) ) ;
#143955 = ORIENTED_EDGE ( 'NONE', *, *, #161545, .F. ) ;
#143956 = DIRECTION ( 'NONE',  ( 1.000000000000000000, -0.000000000000000000, -0.000000000000000000 ) ) ;
#143957 = CYLINDRICAL_SURFACE ( 'NONE', #206608, 0.1000000000000013933 ) ;
#143959 = VECTOR ( 'NONE', #71965, 1000.000000000000000 ) ;
#143958 = CARTESIAN_POINT ( 'NONE',  ( -23.25000000000000355, 11.74999999999998224, -9.250000000000001776 ) ) ;
#143960 = ADVANCED_FACE ( 'NONE', ( #49202 ), #148310, .T. ) ;
#143961 = CARTESIAN_POINT ( 'NONE',  ( 22.59080734064468743, 11.75000000001115552, -167.4692502919029096 ) ) ;
#143962 = VERTEX_POINT ( 'NONE', #204413 ) ;
#143963 = LINE ( 'NONE', #184374, #246835 ) ;
#143964 = ORIENTED_EDGE ( 'NONE', *, *, #83520, .F. ) ;
#143965 = AXIS2_PLACEMENT_3D ( 'NONE', #89889, #190306, #191609 ) ;
#143966 = CARTESIAN_POINT ( 'NONE',  ( 22.47071067811865319, 59.75442326890421896, -233.9300113800879046 ) ) ;
#143967 = SPHERICAL_SURFACE ( 'NONE', #233133, 0.1000000000000000056 ) ;
#143968 = DIRECTION ( 'NONE',  ( 0.000000000000000000, -6.982962677686266711E-15, 1.000000000000000000 ) ) ;
#143969 = FACE_OUTER_BOUND ( 'NONE', #61304, .T. ) ;
#143970 = ORIENTED_EDGE ( 'NONE', *, *, #192964, .F. ) ;
#143971 = AXIS2_PLACEMENT_3D ( 'NONE', #10460, #108278, #195206 ) ;
#143972 = CARTESIAN_POINT ( 'NONE',  ( -20.85000000000000142, 64.35000000001251408, -176.8069731475025321 ) ) ;
#143973 = CIRCLE ( 'NONE', #31597, 0.1000000000000028644 ) ;
#143974 = DIRECTION ( 'NONE',  ( 0.000000000000000000, 0.01562499999998609446, -0.9998779222360101304 ) ) ;
#143975 = CARTESIAN_POINT ( 'NONE',  ( 23.30000000000000426, -11.79999999999999538, -347.0000000000001137 ) ) ;
#143976 = CARTESIAN_POINT ( 'NONE',  ( -16.92280123533710068, 9.949999999999983302, -20.64936768591492466 ) ) ;
#143977 = CARTESIAN_POINT ( 'NONE',  ( -20.94999999999999929, 1.162701749949165642, -108.5000000000000426 ) ) ;
#143978 = VERTEX_POINT ( 'NONE', #184855 ) ;
#143980 = ORIENTED_EDGE ( 'NONE', *, *, #342, .T. ) ;
#143979 = DIRECTION ( 'NONE',  ( 1.000000000000000000, -0.000000000000000000, 0.000000000000000000 ) ) ;
#143981 = ORIENTED_EDGE ( 'NONE', *, *, #100764, .T. ) ;
#143982 = LINE ( 'NONE', #120604, #136128 ) ;
#143983 = ORIENTED_EDGE ( 'NONE', *, *, #142869, .F. ) ;
#143984 = CARTESIAN_POINT ( 'NONE',  ( -23.15000000000000213, -8.596261682231835621, -42.95012751715027832 ) ) ;
#143985 = FACE_OUTER_BOUND ( 'NONE', #70352, .T. ) ;
#143986 = LINE ( 'NONE', #244372, #20788 ) ;
#143988 = ORIENTED_EDGE ( 'NONE', *, *, #69646, .T. ) ;
#143987 = CIRCLE ( 'NONE', #85517, 0.09999999999999939493 ) ;
#143989 = DIRECTION ( 'NONE',  ( 0.000000000000000000, 0.000000000000000000, 1.000000000000000000 ) ) ;
#143990 = DIRECTION ( 'NONE',  ( 0.000000000000000000, 0.2128009952263605897, -0.9770955615653315052 ) ) ;
#143991 = EDGE_CURVE ( 'NONE', #215393, #47690, #173789, .T. ) ;
#143992 = ORIENTED_EDGE ( 'NONE', *, *, #37285, .T. ) ;
#143993 = DIRECTION ( 'NONE',  ( 4.408576920032447355E-17, 0.1350103645451807555, 0.9908441862701610203 ) ) ;
#143995 = ORIENTED_EDGE ( 'NONE', *, *, #198337, .F. ) ;
#143994 = CARTESIAN_POINT ( 'NONE',  ( -21.14999999999999858, 64.35000000001214460, -136.5231074845243597 ) ) ;
#143997 = EDGE_CURVE ( 'NONE', #145161, #9837, #236270, .T. ) ;
#143996 = CYLINDRICAL_SURFACE ( 'NONE', #27557, 0.09999999999999724387 ) ;
#143998 = CARTESIAN_POINT ( 'NONE',  ( 20.85000000000000142, 64.35000000001176090, -76.30697314750248950 ) ) ;
#143999 = AXIS2_PLACEMENT_3D ( 'NONE', #185911, #7264, #110218 ) ;
#144000 = CIRCLE ( 'NONE', #177370, 0.1000000000000024342 ) ;
#144001 = AXIS2_PLACEMENT_3D ( 'NONE', #50044, #129595, #90445 ) ;
#144002 = AXIS2_PLACEMENT_3D ( 'NONE', #195908, #115070, #99327 ) ;
#144003 = ORIENTED_EDGE ( 'NONE', *, *, #100388, .T. ) ;
#144004 = LINE ( 'NONE', #164874, #235121 ) ;
#144006 = EDGE_CURVE ( 'NONE', #46490, #230635, #28608, .T. ) ;
#144005 = DIRECTION ( 'NONE',  ( 0.000000000000000000, -0.9274965247785504907, -0.3738317757009320674 ) ) ;
#144007 = CARTESIAN_POINT ( 'NONE',  ( 22.10000000000000142, -1.467286812112899463, 33.00000000000000000 ) ) ;
#144008 = EDGE_LOOP ( 'NONE', ( #207600, #54522, #187463, #51375, #226411, #25755, #95026, #29052, #70592, #174561, #218109, #153888, #93722, #141631 ) ) ;
#144009 = CARTESIAN_POINT ( 'NONE',  ( 22.60000000000000142, 75.95218160930768647, -181.7731299035715438 ) ) ;
#144010 = ADVANCED_FACE ( 'NONE', ( #243549 ), #123857, .T. ) ;
#144011 = DIRECTION ( 'NONE',  ( 0.000000000000000000, 1.000000000000000000, 0.000000000000000000 ) ) ;
#144012 = EDGE_CURVE ( 'NONE', #112606, #168680, #64905, .T. ) ;
#144013 = ORIENTED_EDGE ( 'NONE', *, *, #185994, .T. ) ;
#144014 = EDGE_CURVE ( 'NONE', #94420, #206437, #145721, .T. ) ;
#144015 = AXIS2_PLACEMENT_3D ( 'NONE', #91609, #210286, #169912 ) ;
#144016 = VERTEX_POINT ( 'NONE', #169186 ) ;
#144017 = CARTESIAN_POINT ( 'NONE',  ( 21.06280952165520404, 65.37286769941093212, -191.3190535977457785 ) ) ;
#144018 = VECTOR ( 'NONE', #24387, 1000.000000000000000 ) ;
#144019 = ORIENTED_EDGE ( 'NONE', *, *, #255441, .T. ) ;
#144020 = CARTESIAN_POINT ( 'NONE',  ( -21.05000000000000071, 87.39257802171759693, -99.94915790469229933 ) ) ;
#144022 = EDGE_CURVE ( 'NONE', #106738, #14516, #115453, .T. ) ;
#144021 = DIRECTION ( 'NONE',  ( 0.000000000000000000, 0.000000000000000000, 1.000000000000000000 ) ) ;
#144024 = ORIENTED_EDGE ( 'NONE', *, *, #190569, .F. ) ;
#144023 = LINE ( 'NONE', #245710, #166772 ) ;
#144025 = CARTESIAN_POINT ( 'NONE',  ( -20.94999999999999929, 87.75000000001163869, -66.42310748452423752 ) ) ;
#144026 = CARTESIAN_POINT ( 'NONE',  ( 18.39999999999999503, 11.47316190337363828, -146.6500000000000341 ) ) ;
#144027 = CARTESIAN_POINT ( 'NONE',  ( -20.54999999999999716, 1.940186915899004161, -154.6708807889467039 ) ) ;
#144028 = CARTESIAN_POINT ( 'NONE',  ( 18.59999999999999787, 20.40049075128452216, -254.1715885023028250 ) ) ;
#144029 = DIRECTION ( 'NONE',  ( -1.836970198721029934E-16, 1.000000000000000000, 0.000000000000000000 ) ) ;
#144030 = CARTESIAN_POINT ( 'NONE',  ( 18.49999999999999289, 62.92706838342916598, -212.5665282393149766 ) ) ;
#144031 = CARTESIAN_POINT ( 'NONE',  ( 23.24999999999999289, 64.35000000001267040, -203.4231074845244507 ) ) ;
#144033 = ORIENTED_EDGE ( 'NONE', *, *, #88974, .F. ) ;
#144032 = FACE_OUTER_BOUND ( 'NONE', #14907, .T. ) ;
#144034 = DIRECTION ( 'NONE',  ( 0.000000000000000000, 0.000000000000000000, 1.000000000000000000 ) ) ;
#144035 = ORIENTED_EDGE ( 'NONE', *, *, #112913, .T. ) ;
#144036 = DIRECTION ( 'NONE',  ( -0.000000000000000000, -6.982962677686266711E-15, 1.000000000000000000 ) ) ;
#144037 = AXIS2_PLACEMENT_3D ( 'NONE', #85093, #42167, #241637 ) ;
#144038 = DIRECTION ( 'NONE',  ( 0.000000000000000000, 6.608470384673547079E-15, -1.000000000000000000 ) ) ;
#144039 = CYLINDRICAL_SURFACE ( 'NONE', #2988, 0.1000000000000002554 ) ;
#144040 = CARTESIAN_POINT ( 'NONE',  ( -20.90000000000000213, -1.786320531569725478, -11.50977166988710820 ) ) ;
#144041 = CARTESIAN_POINT ( 'NONE',  ( -23.25000000000000355, 5.650000000011139001, -46.15000000000000568 ) ) ;
#144042 = VERTEX_POINT ( 'NONE', #248693 ) ;
#144043 = CARTESIAN_POINT ( 'NONE',  ( 21.04999999999782645, 10.49705515483494267, -207.3998863419698182 ) ) ;
#144044 = CYLINDRICAL_SURFACE ( 'NONE', #143494, 0.09999999999999939493 ) ;
#144045 = AXIS2_PLACEMENT_3D ( 'NONE', #118084, #12590, #197608 ) ;
#144046 = EDGE_LOOP ( 'NONE', ( #176103, #62800, #141334, #213646 ) ) ;
#144047 = AXIS2_PLACEMENT_3D ( 'NONE', #127591, #48044, #165442 ) ;
#144048 = AXIS2_PLACEMENT_3D ( 'NONE', #195470, #139294, #16823 ) ;
#144050 = EDGE_CURVE ( 'NONE', #18900, #221237, #225248, .T. ) ;
#144049 = CARTESIAN_POINT ( 'NONE',  ( 23.15000000000000213, 85.50000000001197975, -112.9170766071766820 ) ) ;
#144051 = CARTESIAN_POINT ( 'NONE',  ( -16.81744102076749314, 60.93935776605891164, -221.0417277355860790 ) ) ;
#144052 = EDGE_LOOP ( 'NONE', ( #22580, #105408, #191009, #106483 ) ) ;
#144053 = DIRECTION ( 'NONE',  ( -0.000000000000000000, 1.000000000000000000, 6.982962677686266711E-15 ) ) ;
#144054 = ORIENTED_EDGE ( 'NONE', *, *, #63315, .F. ) ;
#144056 = EDGE_CURVE ( 'NONE', #215838, #229311, #7112, .T. ) ;
#144055 = CARTESIAN_POINT ( 'NONE',  ( 23.14999999999999858, 1.115600667400684642E-11, -200.9999999999999432 ) ) ;
#144057 = ORIENTED_EDGE ( 'NONE', *, *, #212022, .T. ) ;
#144058 = FACE_OUTER_BOUND ( 'NONE', #146029, .T. ) ;
#144059 = EDGE_CURVE ( 'NONE', #125534, #10380, #166619, .T. ) ;
#144060 = CARTESIAN_POINT ( 'NONE',  ( 15.74999999999999645, 9.350000000011139178, -184.2499999999999716 ) ) ;
#144061 = EDGE_CURVE ( 'NONE', #147029, #90926, #7508, .T. ) ;
#144062 = VERTEX_POINT ( 'NONE', #55582 ) ;
#144063 = LINE ( 'NONE', #41162, #56996 ) ;
#144065 = ORIENTED_EDGE ( 'NONE', *, *, #208106, .T. ) ;
#144064 = CARTESIAN_POINT ( 'NONE',  ( 21.05000000000000071, 1.115600667400684642E-11, -179.6499999999999773 ) ) ;
#144066 = CARTESIAN_POINT ( 'NONE',  ( -22.60000000000094289, 75.89914163091425792, -215.2726746080137730 ) ) ;
#144068 = ORIENTED_EDGE ( 'NONE', *, *, #214901, .F. ) ;
#144067 = AXIS2_PLACEMENT_3D ( 'NONE', #183245, #147969, #64565 ) ;
#144069 = CIRCLE ( 'NONE', #215003, 0.09999999999999939493 ) ;
#144070 = ORIENTED_EDGE ( 'NONE', *, *, #133684, .F. ) ;
#144071 = AXIS2_PLACEMENT_3D ( 'NONE', #233519, #134375, #213935 ) ;
#144072 = EDGE_CURVE ( 'NONE', #197421, #8169, #86218, .T. ) ;
#144073 = DIRECTION ( 'NONE',  ( 0.000000000000000000, 0.000000000000000000, -1.000000000000000000 ) ) ;
#144074 = CARTESIAN_POINT ( 'NONE',  ( 19.81427058490531934, 64.33143601963072911, -178.7731074845244450 ) ) ;
#144075 = DIRECTION ( 'NONE',  ( 0.000000000000000000, -0.8660254037844411501, -0.4999999999999956146 ) ) ;
#144076 = AXIS2_PLACEMENT_3D ( 'NONE', #60967, #80501, #62261 ) ;
#144077 = ADVANCED_FACE ( 'NONE', ( #110457 ), #190005, .T. ) ;
#144078 = CYLINDRICAL_SURFACE ( 'NONE', #173019, 0.5000000000000007772 ) ;
#144079 = CARTESIAN_POINT ( 'NONE',  ( 18.59999999999998721, 69.06610602788607878, -166.2374616501508342 ) ) ;
#144080 = ORIENTED_EDGE ( 'NONE', *, *, #131049, .T. ) ;
#144081 = CARTESIAN_POINT ( 'NONE',  ( 20.94999999999999929, 6.846123162352588665, -37.23772626684986164 ) ) ;
#144082 = CARTESIAN_POINT ( 'NONE',  ( -20.64999999999999858, 71.65000000001207070, -124.1731074845243228 ) ) ;
#144084 = CYLINDRICAL_SURFACE ( 'NONE', #53641, 0.09999999999999939493 ) ;
#144083 = PRODUCT_DEFINITION ( 'UNKNOWN', '', #65503, #123499 ) ;
#144085 = CARTESIAN_POINT ( 'NONE',  ( 21.17356465864818915, 1.513868036494046887, -230.6127096343352889 ) ) ;
#144086 = VERTEX_POINT ( 'NONE', #170493 ) ;
#144087 = CARTESIAN_POINT ( 'NONE',  ( -18.50000000000000000, 66.65000000001222702, -148.8731074845244393 ) ) ;
#144088 = ORIENTED_EDGE ( 'NONE', *, *, #133341, .T. ) ;
#144089 = CARTESIAN_POINT ( 'NONE',  ( 12.47034474403012183, 9.375538102059159939, -116.3698758809908611 ) ) ;
#144090 = ORIENTED_EDGE ( 'NONE', *, *, #59876, .F. ) ;
#144091 = VECTOR ( 'NONE', #101104, 1000.000000000000000 ) ;
#144092 = AXIS2_PLACEMENT_3D ( 'NONE', #217397, #236988, #34973 ) ;
#144093 = CARTESIAN_POINT ( 'NONE',  ( 18.59999999999999076, 66.44571689960341132, -213.7280413126916017 ) ) ;
#144094 = DIRECTION ( 'NONE',  ( -1.000000000000000000, -0.000000000000000000, -0.000000000000000000 ) ) ;
#144095 = ADVANCED_FACE ( 'NONE', ( #72643 ), #33542, .T. ) ;
#144096 = ORIENTED_EDGE ( 'NONE', *, *, #58578, .F. ) ;
#144098 = ORIENTED_EDGE ( 'NONE', *, *, #3202, .T. ) ;
#144097 = CARTESIAN_POINT ( 'NONE',  ( 20.94999999999999929, 36.18002604163306302, -236.0784499204090991 ) ) ;
#144099 = ADVANCED_FACE ( 'NONE', ( #113031 ), #75213, .T. ) ;
#144100 = DIRECTION ( 'NONE',  ( 0.000000000000000000, -7.429790795770647916E-15, 1.000000000000000000 ) ) ;
#144101 = ORIENTED_EDGE ( 'NONE', *, *, #61860, .T. ) ;
#144102 = EDGE_CURVE ( 'NONE', #238448, #77760, #23912, .T. ) ;
#144103 = VECTOR ( 'NONE', #218494, 1000.000000000000000 ) ;
#144104 = CARTESIAN_POINT ( 'NONE',  ( -22.49072729836729678, 0.05648193274477467801, -21.84999175084506007 ) ) ;
#144105 = DIRECTION ( 'NONE',  ( 1.000000000000000000, 0.000000000000000000, 0.000000000000000000 ) ) ;
#144106 = ORIENTED_EDGE ( 'NONE', *, *, #70701, .F. ) ;
#144107 = DIRECTION ( 'NONE',  ( 0.000000000000000000, 0.000000000000000000, -1.000000000000000000 ) ) ;
#144108 = CIRCLE ( 'NONE', #98863, 4.049999999999998046 ) ;
#144109 = ORIENTED_EDGE ( 'NONE', *, *, #8659, .T. ) ;
#144110 = ORIENTED_EDGE ( 'NONE', *, *, #91274, .T. ) ;
#144111 = DIRECTION ( 'NONE',  ( 1.000000000000000000, 1.734723475976817507E-14, 0.000000000000000000 ) ) ;
#144112 =( REPRESENTATION_RELATIONSHIP ('NONE','NONE', #36900, #133560 ) REPRESENTATION_RELATIONSHIP_WITH_TRANSFORMATION ( #244980 )SHAPE_REPRESENTATION_RELATIONSHIP( ) );
#144114 = ORIENTED_EDGE ( 'NONE', *, *, #165875, .F. ) ;
#144113 = CARTESIAN_POINT ( 'NONE',  ( -23.15000000000000213, 64.35000000001156195, -57.37310748452440379 ) ) ;
#144115 = CIRCLE ( 'NONE', #102407, 0.09999999999999635569 ) ;
#144116 = FACE_OUTER_BOUND ( 'NONE', #139987, .T. ) ;
#144117 = DIRECTION ( 'NONE',  ( 0.000000000000000000, -0.2617529984169731372, -0.9651348961775882973 ) ) ;
#144118 = AXIS2_PLACEMENT_3D ( 'NONE', #7464, #84383, #2317 ) ;
#144120 = EDGE_CURVE ( 'NONE', #233466, #221470, #71356, .T. ) ;
#144119 = CARTESIAN_POINT ( 'NONE',  ( -16.92973740335348509, 9.992503814478576274, -121.4060590352024462 ) ) ;
#144122 = CARTESIAN_POINT ( 'NONE',  ( -17.11825945287481332, 9.950000000011138823, -188.2499999999999716 ) ) ;
#144121 = CARTESIAN_POINT ( 'NONE',  ( -16.93339986808596365, 65.99489607144595027, -90.45711381271152618 ) ) ;
#144124 = VECTOR ( 'NONE', #186211, 1000.000000000000000 ) ;
#144123 = CARTESIAN_POINT ( 'NONE',  ( 21.04999999999999716, 39.25007626008504502, -236.7661609525534629 ) ) ;
#144125 = AXIS2_PLACEMENT_3D ( 'NONE', #60671, #218460, #39873 ) ;
#144126 = DIRECTION ( 'NONE',  ( 0.000000000000000000, -6.982962677686266711E-15, 1.000000000000000000 ) ) ;
#144127 = CARTESIAN_POINT ( 'NONE',  ( 23.14999999999999147, 38.35559756229049100, -253.3384836876619204 ) ) ;
#144128 = FACE_OUTER_BOUND ( 'NONE', #54957, .T. ) ;
#144129 = VERTEX_POINT ( 'NONE', #252524 ) ;
#144130 = VERTEX_POINT ( 'NONE', #156032 ) ;
#144131 = EDGE_CURVE ( 'NONE', #248947, #48019, #195166, .T. ) ;
#144132 = CARTESIAN_POINT ( 'NONE',  ( -23.39999999999994529, 83.90000000001120384, -34.77310748452479316 ) ) ;
#144133 = ORIENTED_EDGE ( 'NONE', *, *, #58461, .T. ) ;
#144134 = AXIS2_PLACEMENT_3D ( 'NONE', #74948, #154494, #213141 ) ;
#144135 = CARTESIAN_POINT ( 'NONE',  ( -21.05000000000000071, -1.835341550213257733, -179.0551512925629538 ) ) ;
#144136 = EDGE_CURVE ( 'NONE', #175330, #127414, #230410, .T. ) ;
#144137 = CIRCLE ( 'NONE', #2686, 7.900000000000000355 ) ;
#144138 = VERTEX_POINT ( 'NONE', #94741 ) ;
#144139 = VECTOR ( 'NONE', #15715, 1000.000000000000000 ) ;
#144141 = EDGE_CURVE ( 'NONE', #29243, #172615, #209566, .T. ) ;
#144140 = DIRECTION ( 'NONE',  ( 0.000000000000000000, 0.000000000000000000, -1.000000000000000000 ) ) ;
#144142 = VERTEX_POINT ( 'NONE', #53049 ) ;
#144143 = LINE ( 'NONE', #47610, #179757 ) ;
#144144 = VERTEX_POINT ( 'NONE', #213398 ) ;
#144145 = EDGE_LOOP ( 'NONE', ( #227360, #222003, #230268, #206209 ) ) ;
#144146 = ADVANCED_FACE ( 'NONE', ( #234246 ), #111751, .T. ) ;
#144147 = CARTESIAN_POINT ( 'NONE',  ( -18.50000000000000000, 42.90983634497242605, -254.2202269430244996 ) ) ;
#144148 = CARTESIAN_POINT ( 'NONE',  ( -20.64999999999999858, 70.60814576644823148, -215.7631455941064189 ) ) ;
#144151 = EDGE_CURVE ( 'NONE', #116380, #218203, #144676, .T. ) ;
#144150 = ORIENTED_EDGE ( 'NONE', *, *, #119340, .T. ) ;
#144149 = DIRECTION ( 'NONE',  ( -1.000000000000000000, 0.000000000000000000, 0.000000000000000000 ) ) ;
#144152 = CIRCLE ( 'NONE', #31798, 0.09999999999999939493 ) ;
#144153 = DIRECTION ( 'NONE',  ( 0.000000000000000000, 0.000000000000000000, -1.000000000000000000 ) ) ;
#144155 = EDGE_LOOP ( 'NONE', ( #243515, #109184, #84824, #160815 ) ) ;
#144154 = CYLINDRICAL_SURFACE ( 'NONE', #85131, 0.09999999999999939493 ) ;
#144156 = CARTESIAN_POINT ( 'NONE',  ( 19.75857864376268935, 11.75000000001116440, -125.2500000000000426 ) ) ;
#144157 = EDGE_LOOP ( 'NONE', ( #24284, #142770 ) ) ;
#144158 = DIRECTION ( 'NONE',  ( -0.000000000000000000, 1.000000000000000000, 0.000000000000000000 ) ) ;
#144160 = EDGE_LOOP ( 'NONE', ( #209191, #134430 ) ) ;
#144159 = FACE_OUTER_BOUND ( 'NONE', #12193, .T. ) ;
#144161 = DIRECTION ( 'NONE',  ( -0.000000000000000000, 1.000000000000000000, 1.734723475976807292E-15 ) ) ;
#144162 = DIRECTION ( 'NONE',  ( 0.000000000000000000, 0.000000000000000000, -1.000000000000000000 ) ) ;
#144163 = DIRECTION ( 'NONE',  ( 0.000000000000000000, -1.000000000000000000, 0.000000000000000000 ) ) ;
#144164 = VERTEX_POINT ( 'NONE', #73935 ) ;
#144166 = DIRECTION ( 'NONE',  ( -0.000000000000000000, 0.000000000000000000, -1.000000000000000000 ) ) ;
#144165 = CARTESIAN_POINT ( 'NONE',  ( -22.39999999999999858, 7.128833340093095217, -233.7327013124392749 ) ) ;
#144167 = CARTESIAN_POINT ( 'NONE',  ( 18.50000000000000355, 85.48068669529135377, -163.0819923157664562 ) ) ;
#144168 = AXIS2_PLACEMENT_3D ( 'NONE', #192338, #172817, #155803 ) ;
#144169 = EDGE_CURVE ( 'NONE', #32720, #172675, #15535, .T. ) ;
#144170 = DIRECTION ( 'NONE',  ( 1.000000000000000000, -2.952720810173289112E-16, -2.061873921506763405E-30 ) ) ;
#144171 = VECTOR ( 'NONE', #237369, 1000.000000000000000 ) ;
#144173 = CARTESIAN_POINT ( 'NONE',  ( -16.97092634996807448, 44.09655455895979514, -235.2606083258442311 ) ) ;
#144172 = AXIS2_PLACEMENT_3D ( 'NONE', #115988, #195540, #13051 ) ;
#144174 = ADVANCED_FACE ( 'NONE', ( #115591 ), #34808, .T. ) ;
#144175 = VERTEX_POINT ( 'NONE', #12671 ) ;
#144176 = ORIENTED_EDGE ( 'NONE', *, *, #247522, .T. ) ;
#144177 = VERTEX_POINT ( 'NONE', #153496 ) ;
#144178 = CARTESIAN_POINT ( 'NONE',  ( -18.50000000000000000, 7.675662554762638479, -241.7139905447625381 ) ) ;
#144179 = ORIENTED_EDGE ( 'NONE', *, *, #187175, .F. ) ;
#144180 = DIRECTION ( 'NONE',  ( 1.000000000000000000, 0.000000000000000000, -0.000000000000000000 ) ) ;
#144181 = ORIENTED_EDGE ( 'NONE', *, *, #171755, .F. ) ;
#144182 = EDGE_CURVE ( 'NONE', #134179, #136679, #43975, .T. ) ;
#144183 = CARTESIAN_POINT ( 'NONE',  ( -23.15000000000000213, 0.000000000000000000, -33.50000000000000000 ) ) ;
#144184 = PRESENTATION_STYLE_ASSIGNMENT (( #64663 ) ) ;
#144185 = EDGE_CURVE ( 'NONE', #21932, #121672, #161273, .T. ) ;
#144186 = EDGE_LOOP ( 'NONE', ( #125536, #109374, #138654, #219227 ) ) ;
#144187 = CIRCLE ( 'NONE', #252347, 0.09999999999998898659 ) ;
#144188 = DIRECTION ( 'NONE',  ( -0.000000000000000000, 0.8814952561688430555, -0.4721928772777346239 ) ) ;
#144189 =( NAMED_UNIT ( * ) SI_UNIT ( $, .STERADIAN. ) SOLID_ANGLE_UNIT ( ) );
#144190 = ADVANCED_FACE ( 'NONE', ( #219823 ), #98552, .F. ) ;
#144191 = VECTOR ( 'NONE', #225651, 1000.000000000000000 ) ;
#144192 = ORIENTED_EDGE ( 'NONE', *, *, #134884, .T. ) ;
#144193 = EDGE_LOOP ( 'NONE', ( #79557, #118309, #209948, #17012 ) ) ;
#144194 = EDGE_LOOP ( 'NONE', ( #21694, #48821, #45706 ) ) ;
#144195 = DIRECTION ( 'NONE',  ( -0.000000000000000000, -1.265107689135680095E-16, 1.000000000000000000 ) ) ;
#144196 = DIRECTION ( 'NONE',  ( 1.000000000000000000, 0.000000000000000000, 0.000000000000000000 ) ) ;
#144197 = VECTOR ( 'NONE', #241822, 1000.000000000000000 ) ;
#144198 = FACE_OUTER_BOUND ( 'NONE', #143799, .T. ) ;
#144199 = CARTESIAN_POINT ( 'NONE',  ( -18.38639463286148867, 20.70353292814713342, -227.9807439630503154 ) ) ;
#144200 = DIRECTION ( 'NONE',  ( 1.000000000000000000, 0.000000000000000000, 0.000000000000000000 ) ) ;
#144202 = DIRECTION ( 'NONE',  ( 0.7071067811865475727, -0.7071067811865475727, 0.000000000000000000 ) ) ;
#144201 = DIRECTION ( 'NONE',  ( 0.000000000000000000, 0.2617529984165152257, 0.9651348961777124202 ) ) ;
#144203 = DIRECTION ( 'NONE',  ( 0.2834754621636439431, -0.2834754621636535465, -0.9161240771326838450 ) ) ;
#144205 = ORIENTED_EDGE ( 'NONE', *, *, #214990, .T. ) ;
#144204 = CARTESIAN_POINT ( 'NONE',  ( -20.94999027547553894, 10.29326151435327219, -139.4592822510415147 ) ) ;
#144207 = CARTESIAN_POINT ( 'NONE',  ( -16.94333152886235538, 12.44450707589361826, -211.1932353086754972 ) ) ;
#144206 = CARTESIAN_POINT ( 'NONE',  ( 18.49999999999999289, 65.70729864261056719, -164.5657455973725121 ) ) ;
#144208 = EDGE_CURVE ( 'NONE', #77369, #89853, #127950, .T. ) ;
#144209 = DIRECTION ( 'NONE',  ( 0.000000000000000000, 0.9915357197604804940, -0.1298341882520397950 ) ) ;
#144210 = EDGE_CURVE ( 'NONE', #64183, #78597, #3328, .T. ) ;
#144211 = ORIENTED_EDGE ( 'NONE', *, *, #97216, .T. ) ;
#144212 = CARTESIAN_POINT ( 'NONE',  ( -20.94999999999999929, 57.72708596674831938, -226.0092949359174952 ) ) ;
#144213 = CARTESIAN_POINT ( 'NONE',  ( 22.49533356619862801, 64.34999999370783996, -103.0882300648471528 ) ) ;
#144214 = CARTESIAN_POINT ( 'NONE',  ( 20.01093837587850288, 64.25000000001148237, -44.76871004992742797 ) ) ;
#144215 = ORIENTED_EDGE ( 'NONE', *, *, #33252, .F. ) ;
#144216 = CARTESIAN_POINT ( 'NONE',  ( -16.89268316805466341, 66.04827818677011919, -157.3788599630699707 ) ) ;
#144217 = CIRCLE ( 'NONE', #94157, 0.1000000000000052097 ) ;
#144218 = FACE_OUTER_BOUND ( 'NONE', #49691, .T. ) ;
#144219 = FACE_OUTER_BOUND ( 'NONE', #243481, .T. ) ;
#144220 = ORIENTED_EDGE ( 'NONE', *, *, #83225, .F. ) ;
#144221 = ORIENTED_EDGE ( 'NONE', *, *, #196291, .T. ) ;
#144222 = CARTESIAN_POINT ( 'NONE',  ( -21.14999999999999858, -1.391858308744747807, -194.6091531227727955 ) ) ;
#144223 = ORIENTED_EDGE ( 'NONE', *, *, #21938, .T. ) ;
#144224 = CARTESIAN_POINT ( 'NONE',  ( 22.47071067811865319, 7.720074744509197728, -66.90090754529744288 ) ) ;
#144225 = FACE_OUTER_BOUND ( 'NONE', #238683, .T. ) ;
#144226 = LINE ( 'NONE', #103811, #86556 ) ;
#144227 = CARTESIAN_POINT ( 'NONE',  ( 23.14999999999998437, 76.00000000001237765, -170.0231074845243597 ) ) ;
#144228 = EDGE_LOOP ( 'NONE', ( #94273, #214063, #79160, #211168 ) ) ;
#144229 = CARTESIAN_POINT ( 'NONE',  ( -12.33960340485503338, 9.360749169926259938, -117.8145701406072874 ) ) ;
#144230 = DIRECTION ( 'NONE',  ( 1.000000000000000000, 7.304098846218133681E-16, 5.311601492717083645E-30 ) ) ;
#144231 = AXIS2_PLACEMENT_3D ( 'NONE', #1238, #198172, #255526 ) ;
#144232 = CARTESIAN_POINT ( 'NONE',  ( 18.53691006697058796, 10.30215155716188669, -192.2021987172990407 ) ) ;
#144233 = DIRECTION ( 'NONE',  ( 0.000000000000000000, 0.000000000000000000, -1.000000000000000000 ) ) ;
#144234 = CIRCLE ( 'NONE', #81674, 0.09999999999998898659 ) ;
#144235 = EDGE_CURVE ( 'NONE', #193505, #34155, #28007, .T. ) ;
#144236 = ORIENTED_EDGE ( 'NONE', *, *, #129287, .F. ) ;
#144237 = MECHANICAL_DESIGN_GEOMETRIC_PRESENTATION_REPRESENTATION (  '', ( #256625 ), #107020 ) ;
#144239 = ORIENTED_EDGE ( 'NONE', *, *, #124691, .F. ) ;
#144238 = DIRECTION ( 'NONE',  ( 0.000000000000000000, -0.2128009952263403282, 0.9770955615653358350 ) ) ;
#144240 = DIRECTION ( 'NONE',  ( 1.000000000000000000, 0.000000000000000000, 0.000000000000000000 ) ) ;
#144241 = CARTESIAN_POINT ( 'NONE',  ( 18.58703555225035586, 78.17463401018991931, -231.4407306458928701 ) ) ;
#144242 = DIRECTION ( 'NONE',  ( 0.000000000000000000, 0.000000000000000000, -1.000000000000000000 ) ) ;
#144243 = CARTESIAN_POINT ( 'NONE',  ( -20.65000000000000568, 70.35000000001264198, -194.2731074845243882 ) ) ;
#144244 = CARTESIAN_POINT ( 'NONE',  ( -18.59999999999999787, 70.05000000001236060, -159.7174051794895320 ) ) ;
#144245 = CYLINDRICAL_SURFACE ( 'NONE', #32208, 0.1000000000000001305 ) ;
#144246 = ORIENTED_EDGE ( 'NONE', *, *, #215643, .T. ) ;
#144247 = CARTESIAN_POINT ( 'NONE',  ( 21.30000000000002558, 1.115600667400684642E-11, -134.0000000000000000 ) ) ;
#144248 = LINE ( 'NONE', #89423, #6879 ) ;
#144249 = ADVANCED_FACE ( 'NONE', ( #82847 ), #153014, .T. ) ;
#144250 = DIRECTION ( 'NONE',  ( 0.000000000000000000, 0.000000000000000000, 1.000000000000000000 ) ) ;
#144251 = CIRCLE ( 'NONE', #98432, 0.1000000000000051820 ) ;
#144252 = VERTEX_POINT ( 'NONE', #236817 ) ;
#144253 = ORIENTED_EDGE ( 'NONE', *, *, #232078, .T. ) ;
#144254 = CARTESIAN_POINT ( 'NONE',  ( 21.05315837717736827, 11.75000001535411798, -194.1583560219148978 ) ) ;
#144255 = CARTESIAN_POINT ( 'NONE',  ( -20.54999999999999716, -8.999999999988844479, -158.0060308773475981 ) ) ;
#144256 = CARTESIAN_POINT ( 'NONE',  ( 22.48660254037844197, 11.65000000000000746, 0.04999999999999796274 ) ) ;
#144257 = CARTESIAN_POINT ( 'NONE',  ( -16.84421487269768747, 22.99525848796287519, -230.9442721744328821 ) ) ;
#144258 = AXIS2_PLACEMENT_3D ( 'NONE', #173272, #194087, #231926 ) ;
#144259 = DIRECTION ( 'NONE',  ( 0.000000000000000000, 0.000000000000000000, 1.000000000000000000 ) ) ;
#144260 = DIRECTION ( 'NONE',  ( 1.000000000000000000, 0.000000000000000000, 0.000000000000000000 ) ) ;
#144261 = DIRECTION ( 'NONE',  ( 0.000000000000000000, 0.000000000000000000, -1.000000000000000000 ) ) ;
#144262 = CARTESIAN_POINT ( 'NONE',  ( 20.94999999999999574, 1.261786168576181755, -142.0864989635454947 ) ) ;
#144263 = AXIS2_PLACEMENT_3D ( 'NONE', #8196, #108568, #72022 ) ;
#144264 = AXIS2_PLACEMENT_3D ( 'NONE', #226282, #163780, #26857 ) ;
#144265 = ORIENTED_EDGE ( 'NONE', *, *, #89732, .T. ) ;
#144267 = CARTESIAN_POINT ( 'NONE',  ( 20.04999999999999716, 8.750000000000014211, -20.85000000000000142 ) ) ;
#144266 = AXIS2_PLACEMENT_3D ( 'NONE', #21797, #240839, #62201 ) ;
#144268 = EDGE_LOOP ( 'NONE', ( #13189, #9331, #213734 ) ) ;
#144269 = CARTESIAN_POINT ( 'NONE',  ( -21.11833042828127915, 75.99289949095243912, -75.96875217837973082 ) ) ;
#144270 = DIRECTION ( 'NONE',  ( -1.000000000000000000, -0.000000000000000000, 0.000000000000000000 ) ) ;
#144271 = DIRECTION ( 'NONE',  ( 0.000000000000000000, 0.000000000000000000, -1.000000000000000000 ) ) ;
#144272 = CARTESIAN_POINT ( 'NONE',  ( -13.40000000000000213, -8.250000000000007105, 17.60000000000000497 ) ) ;
#144273 = CARTESIAN_POINT ( 'NONE',  ( -21.64999999999999858, 11.82777609026078025, -211.3705695484364924 ) ) ;
#144274 = LINE ( 'NONE', #163879, #18672 ) ;
#144275 = CARTESIAN_POINT ( 'NONE',  ( -18.47079683080347579, -9.471664105244876453, -7.108860540992417043 ) ) ;
#144276 = CARTESIAN_POINT ( 'NONE',  ( 18.39999999999999858, -11.68510997261236106, -191.5194565067366455 ) ) ;
#144277 = CARTESIAN_POINT ( 'NONE',  ( -22.47071067811865674, 7.720074744509219045, -66.90090754529744288 ) ) ;
#144278 = DIRECTION ( 'NONE',  ( 0.000000000000000000, 0.1022405907414165593, 0.9947597004326453884 ) ) ;
#144280 = EDGE_CURVE ( 'NONE', #210220, #5518, #36382, .T. ) ;
#144279 = DIRECTION ( 'NONE',  ( 0.7071067811865474617, -0.7071067811865474617, -5.142139384388980375E-15 ) ) ;
#144281 = CIRCLE ( 'NONE', #215051, 0.5000000000000004441 ) ;
#144282 = DIRECTION ( 'NONE',  ( -1.000000000000000000, 0.000000000000000000, 0.000000000000000000 ) ) ;
#144283 = FACE_OUTER_BOUND ( 'NONE', #36142, .T. ) ;
#144284 = DIRECTION ( 'NONE',  ( 0.000000000000000000, 1.000000000000000000, 0.000000000000000000 ) ) ;
#144285 = ORIENTED_EDGE ( 'NONE', *, *, #188299, .T. ) ;
#144286 = CARTESIAN_POINT ( 'NONE',  ( 23.24999999999999645, 64.25000000001256240, -182.6731074845244507 ) ) ;
#144288 = EDGE_CURVE ( 'NONE', #226768, #111434, #244445, .T. ) ;
#144287 = CARTESIAN_POINT ( 'NONE',  ( 23.14999999999999503, 56.06656052939784729, -228.0911609752645290 ) ) ;
#144289 = VERTEX_POINT ( 'NONE', #198981 ) ;
#144291 = EDGE_CURVE ( 'NONE', #140147, #216955, #217239, .T. ) ;
#144290 = DIRECTION ( 'NONE',  ( 1.000000000000000000, -0.000000000000000000, -0.000000000000000000 ) ) ;
#144292 = LINE ( 'NONE', #126031, #127319 ) ;
#144293 = AXIS2_PLACEMENT_3D ( 'NONE', #166556, #27047, #240936 ) ;
#144294 = AXIS2_PLACEMENT_3D ( 'NONE', #193818, #95972, #56829 ) ;
#144295 = CARTESIAN_POINT ( 'NONE',  ( -16.87036670365547764, 9.989418819312797737, -188.4795601173019861 ) ) ;
#144296 = ORIENTED_EDGE ( 'NONE', *, *, #112736, .T. ) ;
#144297 = AXIS2_PLACEMENT_3D ( 'NONE', #189434, #167318, #70790 ) ;
#144298 = CARTESIAN_POINT ( 'NONE',  ( 21.05000000000000071, 87.65000000001172964, -72.62310748452422615 ) ) ;
#144299 = CIRCLE ( 'NONE', #81752, 0.4000000000000114575 ) ;
#144300 = EDGE_CURVE ( 'NONE', #94122, #101205, #176878, .T. ) ;
#144301 = ORIENTED_EDGE ( 'NONE', *, *, #81030, .T. ) ;
#144302 = CIRCLE ( 'NONE', #48476, 0.09999999999999939493 ) ;
#144303 = CARTESIAN_POINT ( 'NONE',  ( -23.15000000000000213, 2.449293598294710359E-16, -35.50000000000000711 ) ) ;
#144304 = EDGE_LOOP ( 'NONE', ( #212606, #254401, #105610, #158562 ) ) ;
#144306 = ADVANCED_FACE ( 'NONE', ( #215962 ), #19060, .T. ) ;
#144305 = CARTESIAN_POINT ( 'NONE',  ( 18.59999999999999076, 6.550000000011156231, -155.1500000000000057 ) ) ;
#144308 = VECTOR ( 'NONE', #158344, 1000.000000000000000 ) ;
#144307 = CARTESIAN_POINT ( 'NONE',  ( -21.05000000000000071, 1.261786168576181755, -41.58649896354548048 ) ) ;
#144309 = CARTESIAN_POINT ( 'NONE',  ( -18.59999999999999787, 11.64999999999999680, -21.35000000000000142 ) ) ;
#144311 = CARTESIAN_POINT ( 'NONE',  ( -23.25000000000000000, 54.34471204062663219, -239.4366250215122420 ) ) ;
#144310 = UNCERTAINTY_MEASURE_WITH_UNIT (LENGTH_MEASURE( 1.000000000000000082E-05 ), #6955, 'distance_accuracy_value', 'NONE');
#144312 = CARTESIAN_POINT ( 'NONE',  ( 21.05000000000000071, 87.29603075034673054, -39.07100664418810965 ) ) ;
#144313 = VECTOR ( 'NONE', #86523, 1000.000000000000000 ) ;
#144314 = DIRECTION ( 'NONE',  ( -0.000000000000000000, 0.000000000000000000, -1.000000000000000000 ) ) ;
#144315 = DIRECTION ( 'NONE',  ( 1.000000000000000000, 0.000000000000000000, 0.000000000000000000 ) ) ;
#144316 = VECTOR ( 'NONE', #53525, 1000.000000000000000 ) ;
#144317 = CARTESIAN_POINT ( 'NONE',  ( -18.50000000000000000, 11.65000000001115232, -155.7499999999999716 ) ) ;
#144318 = FACE_OUTER_BOUND ( 'NONE', #161286, .T. ) ;
#144320 = VERTEX_POINT ( 'NONE', #99850 ) ;
#144319 = DIRECTION ( 'NONE',  ( 0.000000000000000000, 0.000000000000000000, -1.000000000000000000 ) ) ;
#144321 = ORIENTED_EDGE ( 'NONE', *, *, #29759, .F. ) ;
#144323 = CARTESIAN_POINT ( 'NONE',  ( -21.05000000000000071, 43.51422117117169108, -240.0698702536254530 ) ) ;
#144322 = CARTESIAN_POINT ( 'NONE',  ( -23.25000000000000000, -8.596261682231832069, -191.5498724828496790 ) ) ;
#144325 = ORIENTED_EDGE ( 'NONE', *, *, #67579, .F. ) ;
#144324 = CARTESIAN_POINT ( 'NONE',  ( 21.14999999999999503, 64.27847795353595473, -247.1247091181747066 ) ) ;
#144326 = ORIENTED_EDGE ( 'NONE', *, *, #234756, .F. ) ;
#144327 = CARTESIAN_POINT ( 'NONE',  ( -18.50000000000000000, 1.115600667400684642E-11, -167.5000000000000284 ) ) ;
#144328 = DIRECTION ( 'NONE',  ( 0.000000000000000000, -6.982962677686266711E-15, 1.000000000000000000 ) ) ;
#144329 = DIRECTION ( 'NONE',  ( 1.000000000000000000, 0.000000000000000000, 0.000000000000000000 ) ) ;
#144331 = FACE_OUTER_BOUND ( 'NONE', #96099, .T. ) ;
#144330 = AXIS2_PLACEMENT_3D ( 'NONE', #161148, #141571, #221099 ) ;
#144332 = DIRECTION ( 'NONE',  ( -1.000000000000000000, -0.000000000000000000, -0.000000000000000000 ) ) ;
#144333 = DIRECTION ( 'NONE',  ( 0.000000000000000000, 6.982962677686266711E-15, -1.000000000000000000 ) ) ;
#144334 = ADVANCED_FACE ( 'NONE', ( #240675 ), #747, .F. ) ;
#144335 = CARTESIAN_POINT ( 'NONE',  ( -20.94999999999999929, 11.75000000001115552, -74.01480577065404987 ) ) ;
#144336 = VERTEX_POINT ( 'NONE', #226210 ) ;
#144337 = ORIENTED_EDGE ( 'NONE', *, *, #100716, .F. ) ;
#144338 = FACE_OUTER_BOUND ( 'NONE', #119695, .T. ) ;
#144339 = VECTOR ( 'NONE', #35553, 999.9999999999998863 ) ;
#144340 = AXIS2_PLACEMENT_3D ( 'NONE', #168014, #6316, #104123 ) ;
#144341 = ORIENTED_EDGE ( 'NONE', *, *, #97186, .F. ) ;
#144342 = CIRCLE ( 'NONE', #248434, 4.049999999999998046 ) ;
#144343 = CARTESIAN_POINT ( 'NONE',  ( 22.39999999999999503, 0.2972451047845541261, -230.0732065135368316 ) ) ;
#144344 = ORIENTED_EDGE ( 'NONE', *, *, #26939, .F. ) ;
#144345 = DIRECTION ( 'NONE',  ( 1.000000000000000000, 1.541880601228652843E-16, 2.878400969107353907E-16 ) ) ;
#144346 = EDGE_CURVE ( 'NONE', #43445, #13339, #109565, .T. ) ;
#144347 = DIRECTION ( 'NONE',  ( -1.000000000000000000, -0.000000000000000000, -0.000000000000000000 ) ) ;
#144348 = FACE_OUTER_BOUND ( 'NONE', #250874, .T. ) ;
#144349 = CARTESIAN_POINT ( 'NONE',  ( -21.00000000000000000, -11.75000000000000000, 12.09999999999999609 ) ) ;
#144350 = ORIENTED_EDGE ( 'NONE', *, *, #227821, .T. ) ;
#144352 = EDGE_CURVE ( 'NONE', #128029, #146076, #8499, .T. ) ;
#144351 = DIRECTION ( 'NONE',  ( 0.000000000000000000, 0.000000000000000000, -1.000000000000000000 ) ) ;
#144353 = ORIENTED_EDGE ( 'NONE', *, *, #234532, .T. ) ;
#144354 = CARTESIAN_POINT ( 'NONE',  ( 23.14999999999999858, 73.90000000001214175, -136.5231074845243597 ) ) ;
#144355 = DIRECTION ( 'NONE',  ( -1.000000000000000000, -2.808674667590276147E-16, -1.035613708381807261E-15 ) ) ;
#144356 = CARTESIAN_POINT ( 'NONE',  ( -23.25000000000000355, 11.75000000001113953, -109.7500000000000426 ) ) ;
#144357 = AXIS2_PLACEMENT_3D ( 'NONE', #204202, #9858, #149401 ) ;
#144358 = FACE_OUTER_BOUND ( 'NONE', #182933, .T. ) ;
#144359 = ADVANCED_FACE ( 'NONE', ( #163717 ), #232956, .F. ) ;
#144360 = VERTEX_POINT ( 'NONE', #164991 ) ;
#144361 = AXIS2_PLACEMENT_3D ( 'NONE', #153906, #172181, #75623 ) ;
#144363 = CARTESIAN_POINT ( 'NONE',  ( -21.00250684356851849, 64.25000000001189449, -96.00830171576455996 ) ) ;
#144362 = VECTOR ( 'NONE', #253095, 1000.000000000000000 ) ;
#144364 = VERTEX_POINT ( 'NONE', #9766 ) ;
#144367 = ORIENTED_EDGE ( 'NONE', *, *, #227229, .F. ) ;
#144366 = CARTESIAN_POINT ( 'NONE',  ( 20.94999999999999929, 77.83585931145546510, -91.51866831572576189 ) ) ;
#144365 = CARTESIAN_POINT ( 'NONE',  ( 18.42595409746855495, 46.93054525149890566, -255.3593358477256743 ) ) ;
#144368 = CARTESIAN_POINT ( 'NONE',  ( -22.50000000000000000, 75.90000000001276703, -215.1726782920691505 ) ) ;
#144369 = EDGE_LOOP ( 'NONE', ( #31952, #64164, #118354, #149236, #113281, #6280 ) ) ;
#144370 = CARTESIAN_POINT ( 'NONE',  ( 21.05000000000000071, 76.00000000001244871, -170.0231074845243597 ) ) ;
#144371 = AXIS2_PLACEMENT_3D ( 'NONE', #53903, #133440, #171336 ) ;
#144372 = ORIENTED_EDGE ( 'NONE', *, *, #149064, .T. ) ;
#144373 = PLANE ( 'NONE',  #72216 ) ;
#144375 = EDGE_CURVE ( 'NONE', #112246, #210246, #223779, .T. ) ;
#144374 = CARTESIAN_POINT ( 'NONE',  ( -16.93294127766158752, 10.00328010296601811, -54.42990726582922889 ) ) ;
#144376 = DIRECTION ( 'NONE',  ( 0.000000000000000000, -0.8814952561688438326, 0.4721928772777332917 ) ) ;
#144377 = FACE_OUTER_BOUND ( 'NONE', #101140, .T. ) ;
#144378 = ADVANCED_FACE ( 'NONE', ( #89296 ), #102685, .F. ) ;
#144379 = EDGE_CURVE ( 'NONE', #244468, #128093, #232691, .T. ) ;
#144380 = DIRECTION ( 'NONE',  ( 0.000000000000000000, -1.000000000000000000, 0.000000000000000000 ) ) ;
#144381 = ORIENTED_EDGE ( 'NONE', *, *, #52069, .T. ) ;
#144382 = CARTESIAN_POINT ( 'NONE',  ( -23.15000000000000213, 64.35000000001176090, -76.53791325517833855 ) ) ;
#144383 = CARTESIAN_POINT ( 'NONE',  ( -16.79140778683509083, 14.14974710992871643, -219.2363503299867489 ) ) ;
#144384 = CARTESIAN_POINT ( 'NONE',  ( -18.59999994787167310, -9.523637689750636071, -140.8824495347722632 ) ) ;
#144385 = AXIS2_PLACEMENT_3D ( 'NONE', #13641, #134839, #12380 ) ;
#144386 = ORIENTED_EDGE ( 'NONE', *, *, #44638, .F. ) ;
#144387 = FACE_OUTER_BOUND ( 'NONE', #26651, .T. ) ;
#144388 = VERTEX_POINT ( 'NONE', #111441 ) ;
#144389 = DIRECTION ( 'NONE',  ( -1.000000000000000000, 0.000000000000000000, -0.000000000000000000 ) ) ;
#144390 = EDGE_CURVE ( 'NONE', #48459, #12130, #113996, .T. ) ;
#144391 = LINE ( 'NONE', #70046, #126700 ) ;
#144392 = FACE_OUTER_BOUND ( 'NONE', #175379, .T. ) ;
#144394 = ORIENTED_EDGE ( 'NONE', *, *, #133629, .T. ) ;
#144393 = DIRECTION ( 'NONE',  ( -0.000000000000000000, 1.000000000000000000, -0.000000000000000000 ) ) ;
#144395 = EDGE_CURVE ( 'NONE', #193967, #98958, #236440, .T. ) ;
#144396 = DIRECTION ( 'NONE',  ( 0.000000000000000000, 0.9126074666063770380, 0.4088369013363278848 ) ) ;
#144397 = EDGE_CURVE ( 'NONE', #218982, #160449, #207252, .T. ) ;
#144398 = AXIS2_PLACEMENT_3D ( 'NONE', #196533, #97403, #111886 ) ;
#144399 = DIRECTION ( 'NONE',  ( 0.000000000000000000, -1.000000000000000000, -0.000000000000000000 ) ) ;
#144400 = DIRECTION ( 'NONE',  ( 1.073024830501117528E-15, -0.8814952561688430555, 0.4721928772777346239 ) ) ;
#144401 = ORIENTED_EDGE ( 'NONE', *, *, #235307, .F. ) ;
#144402 = FACE_OUTER_BOUND ( 'NONE', #13237, .T. ) ;
#144403 = DIRECTION ( 'NONE',  ( 0.000000000000000000, -1.000000000000000000, 0.000000000000000000 ) ) ;
#144404 = ORIENTED_EDGE ( 'NONE', *, *, #200419, .T. ) ;
#144405 = DIRECTION ( 'NONE',  ( -0.000000000000000000, 0.4721928772777345684, 0.8814952561688429444 ) ) ;
#144406 = AXIS2_PLACEMENT_3D ( 'NONE', #104674, #35175, #68156 ) ;
#144407 = EDGE_LOOP ( 'NONE', ( #79928, #4298, #153119, #154726, #248978 ) ) ;
#144408 = AXIS2_PLACEMENT_3D ( 'NONE', #199769, #159352, #238873 ) ;
#144409 = DIRECTION ( 'NONE',  ( -1.000000000000000000, -2.952720810173289112E-16, 0.000000000000000000 ) ) ;
#144411 = ORIENTED_EDGE ( 'NONE', *, *, #221774, .T. ) ;
#144410 = CARTESIAN_POINT ( 'NONE',  ( 23.24999999999999289, 64.35000000001186038, -90.87310748452438247 ) ) ;
#144412 = EDGE_CURVE ( 'NONE', #212130, #155495, #210546, .T. ) ;
#144413 = EDGE_CURVE ( 'NONE', #175353, #103723, #151883, .T. ) ;
#144414 = VECTOR ( 'NONE', #93562, 1000.000000000000000 ) ;
#144417 = ORIENTED_EDGE ( 'NONE', *, *, #93490, .F. ) ;
#144416 = EDGE_LOOP ( 'NONE', ( #245096, #106644, #211848 ) ) ;
#144415 = CARTESIAN_POINT ( 'NONE',  ( -18.40000000000000213, 11.47316190337362762, -46.04999999999999716 ) ) ;
#144418 = DIRECTION ( 'NONE',  ( 0.000000000000000000, -0.9126074666063769270, -0.4088369013363280513 ) ) ;
#144419 = LINE ( 'NONE', #167896, #177291 ) ;
#144421 = EDGE_CURVE ( 'NONE', #136972, #11015, #253506, .T. ) ;
#144420 = LINE ( 'NONE', #205695, #48323 ) ;
#144423 = DIRECTION ( 'NONE',  ( 0.000000000000000000, -0.9908441862701596881, -0.1350103645451904977 ) ) ;
#144422 = CARTESIAN_POINT ( 'NONE',  ( 20.92356734117541706, 46.42459709376391430, -243.0752906381742662 ) ) ;
#144424 = DIRECTION ( 'NONE',  ( 0.000000000000000000, -6.982962677686266711E-15, 1.000000000000000000 ) ) ;
#144425 = VECTOR ( 'NONE', #220612, 1000.000000000000000 ) ;
#144426 = CARTESIAN_POINT ( 'NONE',  ( -17.73285935861365203, 65.14201819622128653, -59.28166929430445009 ) ) ;
#144427 = DIRECTION ( 'NONE',  ( 0.000000000000000000, 0.000000000000000000, -1.000000000000000000 ) ) ;
#144428 = CARTESIAN_POINT ( 'NONE',  ( 21.14999999999999503, 76.00000000001165290, -69.52310748452431710 ) ) ;
#144429 = AXIS2_PLACEMENT_3D ( 'NONE', #53015, #92149, #171724 ) ;
#144430 = ORIENTED_EDGE ( 'NONE', *, *, #42362, .T. ) ;
#144431 = EDGE_LOOP ( 'NONE', ( #145489, #118027, #45894, #9852 ) ) ;
#144433 = CARTESIAN_POINT ( 'NONE',  ( -23.15000000000000213, 11.65000000001115588, -112.6500000000000341 ) ) ;
#144432 = AXIS2_PLACEMENT_3D ( 'NONE', #198416, #135855, #206 ) ;
#144435 = VERTEX_POINT ( 'NONE', #132283 ) ;
#144434 = FACE_OUTER_BOUND ( 'NONE', #225006, .T. ) ;
#144436 = CIRCLE ( 'NONE', #69654, 0.2000000000000057288 ) ;
#144437 = VERTEX_POINT ( 'NONE', #249676 ) ;
#144438 = CARTESIAN_POINT ( 'NONE',  ( -21.07016717456946253, 6.320940838100246317, -6.871554784600512487E-16 ) ) ;
#144439 = ORIENTED_EDGE ( 'NONE', *, *, #185094, .T. ) ;
#144440 = DIRECTION ( 'NONE',  ( 0.000000000000000000, -0.5273008465188072647, 0.8496786552930167824 ) ) ;
#144441 = CIRCLE ( 'NONE', #90284, 0.09999999999998715472 ) ;
#144442 = VECTOR ( 'NONE', #14645, 1000.000000000000000 ) ;
#144443 = ADVANCED_FACE ( 'NONE', ( #231402 ), #171455, .F. ) ;
#144444 = VERTEX_POINT ( 'NONE', #131002 ) ;
#144445 = DIRECTION ( 'NONE',  ( -1.000000000000000000, 2.952720810173289112E-16, 2.061873921506763405E-30 ) ) ;
#144447 = EDGE_CURVE ( 'NONE', #12552, #136660, #250931, .T. ) ;
#144446 = CARTESIAN_POINT ( 'NONE',  ( 20.94999999999999929, 7.021664781911246322, -70.83356540189728889 ) ) ;
#144450 = VERTEX_POINT ( 'NONE', #33231 ) ;
#144449 = ORIENTED_EDGE ( 'NONE', *, *, #91180, .F. ) ;
#144448 = VECTOR ( 'NONE', #257015, 1000.000000000000000 ) ;
#144451 = ORIENTED_EDGE ( 'NONE', *, *, #77324, .T. ) ;
#144452 = CARTESIAN_POINT ( 'NONE',  ( 21.13507111622890022, 10.71768338700954537, -45.74916858636079553 ) ) ;
#144453 = AXIS2_PLACEMENT_3D ( 'NONE', #121786, #146444, #125614 ) ;
#144454 = VERTEX_POINT ( 'NONE', #112729 ) ;
#144455 = CIRCLE ( 'NONE', #44542, 0.09999999999998898659 ) ;
#144456 = ORIENTED_EDGE ( 'NONE', *, *, #199125, .T. ) ;
#144457 = EDGE_CURVE ( 'NONE', #47866, #8189, #19814, .T. ) ;
#144458 = FACE_OUTER_BOUND ( 'NONE', #159011, .T. ) ;
#144461 = EDGE_CURVE ( 'NONE', #172105, #1731, #15733, .T. ) ;
#144460 = ORIENTED_EDGE ( 'NONE', *, *, #128349, .F. ) ;
#144459 = DIRECTION ( 'NONE',  ( 1.000000000000000000, 0.000000000000000000, 0.000000000000000000 ) ) ;
#144462 = CARTESIAN_POINT ( 'NONE',  ( -21.05000000000000071, 76.00000000001165290, -69.52310748452431710 ) ) ;
#144463 = CARTESIAN_POINT ( 'NONE',  ( -21.05000000000000071, 43.57568952063339651, -245.1784935019914826 ) ) ;
#144465 = VERTEX_POINT ( 'NONE', #174029 ) ;
#144464 = DIRECTION ( 'NONE',  ( 1.000000000000000000, 0.000000000000000000, 0.000000000000000000 ) ) ;
#144466 = CARTESIAN_POINT ( 'NONE',  ( -23.25000000000000000, -11.64999999998884483, -67.00000000000004263 ) ) ;
#144467 = VERTEX_POINT ( 'NONE', #193557 ) ;
#144468 = EDGE_CURVE ( 'NONE', #154309, #55514, #153180, .T. ) ;
#144469 = DIRECTION ( 'NONE',  ( 1.734723475976817507E-14, 0.2617529984165031243, 0.9651348961777157509 ) ) ;
#144470 = ORIENTED_EDGE ( 'NONE', *, *, #79743, .T. ) ;
#144471 = CARTESIAN_POINT ( 'NONE',  ( -20.94999999999999929, 18.86061765788380740, -226.6874733728449485 ) ) ;
#144472 = CARTESIAN_POINT ( 'NONE',  ( 23.14999999999999858, 72.13946041530040532, -202.4760954908588815 ) ) ;
#144473 = AXIS2_PLACEMENT_3D ( 'NONE', #44756, #184249, #205080 ) ;
#144474 = VERTEX_POINT ( 'NONE', #12368 ) ;
#144476 = DIRECTION ( 'NONE',  ( 0.000000000000000000, 1.000000000000000000, 0.000000000000000000 ) ) ;
#144475 = CARTESIAN_POINT ( 'NONE',  ( 21.06089410995825872, 10.72529553213474429, -45.70238073104311383 ) ) ;
#144477 = EDGE_CURVE ( 'NONE', #7471, #233607, #73993, .T. ) ;
#144478 = DIRECTION ( 'NONE',  ( 1.000000000000000000, 7.304098846218133681E-16, 4.639676173203992654E-30 ) ) ;
#144479 = CARTESIAN_POINT ( 'NONE',  ( 20.05000000000002913, 42.13647595316533767, -239.1530172309881550 ) ) ;
#144480 = ADVANCED_FACE ( 'NONE', ( #154458 ), #228833, .F. ) ;
#144481 = ORIENTED_EDGE ( 'NONE', *, *, #131904, .F. ) ;
#144482 = ORIENTED_EDGE ( 'NONE', *, *, #20997, .T. ) ;
#144483 = FACE_OUTER_BOUND ( 'NONE', #206956, .T. ) ;
#144484 = CYLINDRICAL_SURFACE ( 'NONE', #60932, 7.900000000000003908 ) ;
#144485 = ORIENTED_EDGE ( 'NONE', *, *, #14869, .T. ) ;
#144486 = LINE ( 'NONE', #224034, #168231 ) ;
#144487 = ORIENTED_EDGE ( 'NONE', *, *, #36143, .T. ) ;
#144488 = EDGE_CURVE ( 'NONE', #169929, #80509, #148988, .T. ) ;
#144489 = DIRECTION ( 'NONE',  ( 0.000000000000000000, -1.000000000000000000, 0.000000000000000000 ) ) ;
#144490 = CARTESIAN_POINT ( 'NONE',  ( 21.15000000000005187, 64.25000000001119815, -30.12310748452479103 ) ) ;
#144491 = CIRCLE ( 'NONE', #140201, 0.1000000000000052097 ) ;
#144492 = DIRECTION ( 'NONE',  ( -0.000000000000000000, -1.000000000000000000, 0.000000000000000000 ) ) ;
#144493 = AXIS2_PLACEMENT_3D ( 'NONE', #89256, #9720, #249641 ) ;
#144494 = FACE_OUTER_BOUND ( 'NONE', #256220, .T. ) ;
#144495 = VECTOR ( 'NONE', #55025, 1000.000000000000000 ) ;
#144496 = TOROIDAL_SURFACE ( 'NONE', #94438, 0.2000000000000000111, 0.1000000000000000056 ) ;
#144497 = VERTEX_POINT ( 'NONE', #168890 ) ;
#144498 = CARTESIAN_POINT ( 'NONE',  ( 18.36493879433156451, -9.500000806182013591, -207.9221486603419748 ) ) ;
#144499 = EDGE_CURVE ( 'NONE', #39976, #249989, #94796, .T. ) ;
#144500 = EDGE_CURVE ( 'NONE', #44319, #130475, #136105, .T. ) ;
#144501 = VECTOR ( 'NONE', #80940, 1000.000000000000000 ) ;
#144503 = ORIENTED_EDGE ( 'NONE', *, *, #184232, .F. ) ;
#144502 = ORIENTED_EDGE ( 'NONE', *, *, #21489, .T. ) ;
#144504 = VERTEX_POINT ( 'NONE', #237811 ) ;
#144505 = ORIENTED_EDGE ( 'NONE', *, *, #200678, .F. ) ;
#144506 = ADVANCED_FACE ( 'NONE', ( #119153 ), #160858, .F. ) ;
#144507 = DIRECTION ( 'NONE',  ( 0.000000000000000000, 0.9910465087640861759, 0.1335171055202901691 ) ) ;
#144508 = LINE ( 'NONE', #66284, #3189 ) ;
#144510 = CARTESIAN_POINT ( 'NONE',  ( -23.25000000000000000, -8.999999999988846255, -76.89396912265249284 ) ) ;
#144509 =( BOUNDED_SURFACE ( )  B_SPLINE_SURFACE ( 3, 2, ( 
 ( #26258, #243995, #40713 ),
 ( #23711, #62803, #142327 ),
 ( #223146, #202313, #184026 ),
 ( #24986, #224434, #65367 ) ),
 .UNSPECIFIED., .F., .F., .F. ) 
 B_SPLINE_SURFACE_WITH_KNOTS ( ( 4, 4 ),
 ( 3, 3 ),
 ( 0.0002700421466196767546, 0.0004789321604330748668 ),
 ( 0.000000000000000000, 1.000000000000000000 ),
 .UNSPECIFIED. ) 
 GEOMETRIC_REPRESENTATION_ITEM ( )  RATIONAL_B_SPLINE_SURFACE ( (
 ( 1.000000000000000000, 0.7071067811865475727, 1.000000000000000000),
 ( 1.000000000000000000, 0.7163411249511738577, 1.000000000000000000),
 ( 1.000000000000000000, 0.7221957104842052777, 1.000000000000000000),
 ( 1.000000000000000000, 0.7250110520819876836, 1.000000000000000000) ) ) 
 REPRESENTATION_ITEM ( '' )  SURFACE ( )  );
#144511 = CARTESIAN_POINT ( 'NONE',  ( 20.94999999999999574, -1.851028230129704522, -112.1539132694225316 ) ) ;
#144512 = DIRECTION ( 'NONE',  ( -1.000000000000000000, -0.000000000000000000, -0.000000000000000000 ) ) ;
#144514 = DIRECTION ( 'NONE',  ( -0.000000000000000000, 0.9910465087640869530, 0.1335171055202841461 ) ) ;
#144513 = DIRECTION ( 'NONE',  ( -0.000000000000000000, -0.2617529984165028467, -0.9651348961777159730 ) ) ;
#144515 = EDGE_CURVE ( 'NONE', #28934, #156274, #24098, .T. ) ;
#144517 = ORIENTED_EDGE ( 'NONE', *, *, #162393, .F. ) ;
#144516 = CARTESIAN_POINT ( 'NONE',  ( 18.59999996954842771, 77.40622708283223119, -241.7320322634360252 ) ) ;
#144518 = FACE_OUTER_BOUND ( 'NONE', #26660, .T. ) ;
#144519 = ORIENTED_EDGE ( 'NONE', *, *, #17558, .F. ) ;
#144520 = LINE ( 'NONE', #68873, #5009 ) ;
#144521 = AXIS2_PLACEMENT_3D ( 'NONE', #195528, #54700, #172129 ) ;
#144522 = EDGE_CURVE ( 'NONE', #248210, #223063, #98855, .T. ) ;
#144523 = VERTEX_POINT ( 'NONE', #236514 ) ;
#144524 = ORIENTED_EDGE ( 'NONE', *, *, #225080, .F. ) ;
#144525 = CARTESIAN_POINT ( 'NONE',  ( 22.50000000000000000, 1.148907358139439339E-11, -201.0000000000015064 ) ) ;
#144526 = CIRCLE ( 'NONE', #227934, 6.258578643762714222 ) ;
#144527 = DIRECTION ( 'NONE',  ( 0.000000000000000000, -0.9126074666063763718, -0.4088369013363293836 ) ) ;
#144528 = CARTESIAN_POINT ( 'NONE',  ( -16.77308656112215246, 66.05000000001153637, -48.67330067622668821 ) ) ;
#144529 = CARTESIAN_POINT ( 'NONE',  ( 18.39999999999999858, 85.60000000001240039, -163.3229180933022633 ) ) ;
#144530 = B_SPLINE_CURVE_WITH_KNOTS ( 'NONE', 3,
 ( #82180, #123922, #60072, #139593, #199620, #20989, #180041, #80911, #63937, #44383, #240012, #61364, #202164, #140912, #161776, #241305, #62662, #142183, #43093, #144733, #169495, #224285, #225544, #45658, #189018, #108204, #187750, #126471, #67781, #110755 ),
 .UNSPECIFIED., .F., .F.,
 ( 4, 2, 2, 2, 2, 2, 2, 2, 2, 2, 2, 2, 2, 2, 4 ),
 ( 0.000000000000000000, 0.0003422764154113056966, 0.0006845528308226113932, 0.001026829246233917090, 0.001369105661645222786, 0.002053658492467898798, 0.002738211323290575677, 0.003080487738701916719, 0.003422764154113257327, 0.003765040569524598368, 0.004107316984935938976, 0.004449593400347280452, 0.004791869815758621060, 0.005134146231169961667, 0.005476422646581303143 ),
 .UNSPECIFIED. ) ;
#144531 = ADVANCED_BREP_SHAPE_REPRESENTATION ( '', ( #105841, #2425 ), #247943 ) ;
#144532 = AXIS2_PLACEMENT_3D ( 'NONE', #104828, #70915, #89150 ) ;
#144533 = DIRECTION ( 'NONE',  ( 0.000000000000000000, 0.000000000000000000, -1.000000000000000000 ) ) ;
#144534 = ORIENTED_EDGE ( 'NONE', *, *, #25035, .T. ) ;
#144535 = ORIENTED_EDGE ( 'NONE', *, *, #154330, .F. ) ;
#144536 = PLANE ( 'NONE',  #178037 ) ;
#144538 = ADVANCED_FACE ( 'NONE', ( #461 ), #220807, .T. ) ;
#144537 = EDGE_LOOP ( 'NONE', ( #148867, #160909, #130600, #4253 ) ) ;
#144539 = CARTESIAN_POINT ( 'NONE',  ( -20.94999999999999929, 0.5876173420563349792, -209.1618981382189588 ) ) ;
#144540 = CARTESIAN_POINT ( 'NONE',  ( 20.84999999999999432, -1.164121893230052995, -175.4148480855716059 ) ) ;
#144541 = PLANE ( 'NONE',  #57237 ) ;
#144542 = CARTESIAN_POINT ( 'NONE',  ( 21.22070241538126467, -1.280157660226128646, -194.6571941450697807 ) ) ;
#144543 = PLANE ( 'NONE',  #248720 ) ;
#144544 = LINE ( 'NONE', #85834, #196671 ) ;
#144545 = EDGE_LOOP ( 'NONE', ( #30391, #206871, #25506, #62970, #109529, #132930, #87549, #207346, #175547, #58493, #200904, #67635, #154600, #179786, #143858, #230043, #217884, #247312, #72209, #234887, #139925, #30769, #235936, #48555, #182958, #196785, #126936 ) ) ;
#144546 = CARTESIAN_POINT ( 'NONE',  ( -23.15000000000000213, 85.60000000001231513, -160.1291383618718385 ) ) ;
#144547 = DIRECTION ( 'NONE',  ( 0.000000000000000000, -1.000000000000000000, -6.982962677686265922E-15 ) ) ;
#144548 = CARTESIAN_POINT ( 'NONE',  ( 21.30000000000002558, 76.00000000001234923, -165.9731074845243768 ) ) ;
#144550 = EDGE_CURVE ( 'NONE', #21983, #137338, #77424, .T. ) ;
#144549 = CARTESIAN_POINT ( 'NONE',  ( 18.49999999999998934, 65.74999999739348766, -178.8359355348929114 ) ) ;
#144551 = DIRECTION ( 'NONE',  ( -1.000000000000000000, 0.000000000000000000, 0.000000000000000000 ) ) ;
#144552 = VECTOR ( 'NONE', #24673, 1000.000000000000000 ) ;
#144554 = AXIS2_PLACEMENT_3D ( 'NONE', #194613, #255794, #14693 ) ;
#144553 = CARTESIAN_POINT ( 'NONE',  ( 18.44444291854882323, 77.16076536701955035, -241.8057231467951738 ) ) ;
#144555 = TOROIDAL_SURFACE ( 'NONE', #11289, 0.6000000000000006439, 0.1000000000000000056 ) ;
#144556 = VECTOR ( 'NONE', #185291, 1000.000000000000114 ) ;
#144557 = ORIENTED_EDGE ( 'NONE', *, *, #54275, .T. ) ;
#144559 = ADVANCED_FACE ( 'NONE', ( #78711 ), #116581, .T. ) ;
#144558 = CARTESIAN_POINT ( 'NONE',  ( 23.14999999999999858, 71.00000000001158185, -57.11784146561126363 ) ) ;
#144560 = ORIENTED_EDGE ( 'NONE', *, *, #30688, .T. ) ;
#144561 = DIRECTION ( 'NONE',  ( 0.000000000000000000, 0.000000000000000000, 1.000000000000000000 ) ) ;
#144562 = FACE_OUTER_BOUND ( 'NONE', #22646, .T. ) ;
#144563 = CARTESIAN_POINT ( 'NONE',  ( -20.07928932188135107, 9.220710678129810489, -155.1500000000000057 ) ) ;
#144564 = VERTEX_POINT ( 'NONE', #17471 ) ;
#144565 = DIRECTION ( 'NONE',  ( 1.000000000000000000, 0.000000000000000000, 0.000000000000000000 ) ) ;
#144566 = VECTOR ( 'NONE', #19632, 1000.000000000000000 ) ;
#144567 = CARTESIAN_POINT ( 'NONE',  ( -23.25000000000000000, 74.44087353924872730, -232.6253149859214773 ) ) ;
#144568 = LINE ( 'NONE', #125035, #75552 ) ;
#144569 = AXIS2_PLACEMENT_3D ( 'NONE', #98656, #140380, #87779 ) ;
#144570 = EDGE_CURVE ( 'NONE', #190789, #245573, #182296, .T. ) ;
#144571 = DIRECTION ( 'NONE',  ( 1.000000000000000000, -3.265361837132813093E-16, -2.280189983783949500E-30 ) ) ;
#144572 = CARTESIAN_POINT ( 'NONE',  ( 22.49999999999999645, 75.91119002362552237, -181.6728704025562706 ) ) ;
#144573 = VERTEX_POINT ( 'NONE', #81272 ) ;
#144574 = CARTESIAN_POINT ( 'NONE',  ( 20.73486653747088937, 68.25000000001257661, -190.8731074845244109 ) ) ;
#144576 = ORIENTED_EDGE ( 'NONE', *, *, #97566, .T. ) ;
#144575 = DIRECTION ( 'NONE',  ( 0.000000000000000000, 0.9651348961777148627, -0.2617529984165062329 ) ) ;
#144577 = CARTESIAN_POINT ( 'NONE',  ( -23.15000000000000213, 70.05000000001221849, -146.8288097895591875 ) ) ;
#144578 = DIRECTION ( 'NONE',  ( 0.000000000000000000, 0.000000000000000000, -1.000000000000000000 ) ) ;
#144579 =( BOUNDED_CURVE ( )  B_SPLINE_CURVE ( 3, ( #252102, #249558, #194731, #16096 ),
 .UNSPECIFIED., .F., .F. ) 
 B_SPLINE_CURVE_WITH_KNOTS ( ( 4, 4 ),
 ( -9.769962616701377556E-15, 1.570796326794891673 ),
 .UNSPECIFIED. ) 
 CURVE ( )  GEOMETRIC_REPRESENTATION_ITEM ( )  RATIONAL_B_SPLINE_CURVE ( ( 1.000000000000000000, 0.8047378541243637162, 0.8047378541243637162, 1.000000000000000000 ) ) 
 REPRESENTATION_ITEM ( '' )  );
#144580 = ORIENTED_EDGE ( 'NONE', *, *, #248641, .T. ) ;
#144581 = LINE ( 'NONE', #85876, #226226 ) ;
#144582 = SHAPE_DEFINITION_REPRESENTATION ( #201697, #63487 ) ;
#144583 = CARTESIAN_POINT ( 'NONE',  ( 22.39999999999999503, -0.1008583690987139431, 11.74956712348939192 ) ) ;
#144584 = ORIENTED_EDGE ( 'NONE', *, *, #26683, .T. ) ;
#144585 = LINE ( 'NONE', #224128, #13151 ) ;
#144586 = CARTESIAN_POINT ( 'NONE',  ( 12.68104795156994946, 9.396533993965075382, -185.4059397791732806 ) ) ;
#144587 = AXIS2_PLACEMENT_3D ( 'NONE', #79999, #157024, #236525 ) ;
#144588 = CARTESIAN_POINT ( 'NONE',  ( 21.05000000000000071, 70.10000000001251408, -180.2422072491807796 ) ) ;
#144589 = ORIENTED_EDGE ( 'NONE', *, *, #215664, .F. ) ;
#144590 = ORIENTED_EDGE ( 'NONE', *, *, #182569, .T. ) ;
#144591 = CARTESIAN_POINT ( 'NONE',  ( 20.94999999999999929, 76.00000000001169553, -67.62310748452431142 ) ) ;
#144592 = CARTESIAN_POINT ( 'NONE',  ( 20.94999999999999929, 7.525330762710603416, -212.0571253909869256 ) ) ;
#144593 = AXIS2_PLACEMENT_3D ( 'NONE', #187268, #4733, #125982 ) ;
#144594 = CARTESIAN_POINT ( 'NONE',  ( -20.94999999999999929, 77.83585931145570669, -125.0186683157258045 ) ) ;
#144595 = CARTESIAN_POINT ( 'NONE',  ( 22.50000000000000000, 11.64957080755595520, -33.40000000000000568 ) ) ;
#144596 = FACE_OUTER_BOUND ( 'NONE', #247038, .T. ) ;
#144597 = DIRECTION ( 'NONE',  ( 0.000000000000000000, 1.000000000000000000, 0.000000000000000000 ) ) ;
#144598 = ADVANCED_FACE ( 'NONE', ( #219513 ), #117849, .T. ) ;
#144599 = FACE_OUTER_BOUND ( 'NONE', #117772, .T. ) ;
#144601 = CARTESIAN_POINT ( 'NONE',  ( -23.15000000000000213, 4.590145742703442444, -213.0289728181953706 ) ) ;
#144600 = CARTESIAN_POINT ( 'NONE',  ( 21.07016717456946608, 6.320940838100256975, -6.911788849595090767E-16 ) ) ;
#144602 = DIRECTION ( 'NONE',  ( 0.000000000000000000, 0.4721928772777351790, 0.8814952561688427224 ) ) ;
#144603 = CARTESIAN_POINT ( 'NONE',  ( -16.87851181299898684, 9.950042924018893231, -113.1498564846331192 ) ) ;
#144604 = CARTESIAN_POINT ( 'NONE',  ( 18.59999999999999076, 53.28269063671665151, -234.9266833317103647 ) ) ;
#144605 = CARTESIAN_POINT ( 'NONE',  ( -23.15000000000000213, -11.48912529306489994, -97.50000000000004263 ) ) ;
#144606 = VECTOR ( 'NONE', #148217, 1000.000000000000000 ) ;
#144607 = ORIENTED_EDGE ( 'NONE', *, *, #247522, .F. ) ;
#144608 = AXIS2_PLACEMENT_3D ( 'NONE', #216006, #139010, #99891 ) ;
#144609 = ORIENTED_EDGE ( 'NONE', *, *, #63141, .T. ) ;
#144610 = DIRECTION ( 'NONE',  ( 0.000000000000000000, 0.4930308989875230585, 0.8700118002898322711 ) ) ;
#144611 = FACE_OUTER_BOUND ( 'NONE', #257873, .T. ) ;
#144613 = DIRECTION ( 'NONE',  ( 1.000000000000000000, 0.000000000000000000, 0.000000000000000000 ) ) ;
#144612 = CARTESIAN_POINT ( 'NONE',  ( -15.75000000000000355, 66.15000000001155911, -52.77310748452439526 ) ) ;
#144614 =( BOUNDED_CURVE ( )  B_SPLINE_CURVE ( 3, ( #14511, #52300, #34085, #32801 ),
 .UNSPECIFIED., .F., .F. ) 
 B_SPLINE_CURVE_WITH_KNOTS ( ( 4, 4 ),
 ( 1.570796326794896558, 3.141592653589793116 ),
 .UNSPECIFIED. ) 
 CURVE ( )  GEOMETRIC_REPRESENTATION_ITEM ( )  RATIONAL_B_SPLINE_CURVE ( ( 1.000000000000000000, 0.8047378541243649375, 0.8047378541243649375, 1.000000000000000000 ) ) 
 REPRESENTATION_ITEM ( '' )  );
#144615 = EDGE_LOOP ( 'NONE', ( #256444, #196033, #84781, #119128 ) ) ;
#144616 = AXIS2_PLACEMENT_3D ( 'NONE', #186181, #49224, #208325 ) ;
#144617 = DIRECTION ( 'NONE',  ( 0.000000000000000000, 0.8700118002898321601, -0.4930308989875230585 ) ) ;
#144619 = EDGE_CURVE ( 'NONE', #55134, #228509, #203126, .T. ) ;
#144618 = CYLINDRICAL_SURFACE ( 'NONE', #224983, 11.80000000000000426 ) ;
#144620 = AXIS2_PLACEMENT_3D ( 'NONE', #94826, #192663, #190091 ) ;
#144621 = FACE_OUTER_BOUND ( 'NONE', #31551, .T. ) ;
#144622 = DIRECTION ( 'NONE',  ( 0.000000000000000000, 0.000000000000000000, -1.000000000000000000 ) ) ;
#144623 = VERTEX_POINT ( 'NONE', #239098 ) ;
#144624 = EDGE_CURVE ( 'NONE', #221991, #239783, #124045, .T. ) ;
#144625 = DIRECTION ( 'NONE',  ( 1.000000000000000000, 0.000000000000000000, 0.000000000000000000 ) ) ;
#144626 = ORIENTED_EDGE ( 'NONE', *, *, #188022, .F. ) ;
#144627 = DIRECTION ( 'NONE',  ( 0.000000000000000000, 0.000000000000000000, -1.000000000000000000 ) ) ;
#144629 = EDGE_CURVE ( 'NONE', #33900, #125917, #179151, .T. ) ;
#144628 = AXIS2_PLACEMENT_3D ( 'NONE', #11856, #27583, #56067 ) ;
#144630 = AXIS2_PLACEMENT_3D ( 'NONE', #119432, #41192, #101082 ) ;
#144631 = CARTESIAN_POINT ( 'NONE',  ( 23.15000000000000213, -11.39257802169451139, -130.9260504201681101 ) ) ;
#144632 = EDGE_CURVE ( 'NONE', #1729, #73021, #132212, .T. ) ;
#144633 = TOROIDAL_SURFACE ( 'NONE', #211292, 0.2000000000000000111, 0.1000000000000000056 ) ;
#144634 = EDGE_CURVE ( 'NONE', #195387, #221355, #11618, .T. ) ;
#144636 = VERTEX_POINT ( 'NONE', #39642 ) ;
#144635 = TOROIDAL_SURFACE ( 'NONE', #32245, 0.4000000000000005773, 0.1000000000000000056 ) ;
#144637 = CARTESIAN_POINT ( 'NONE',  ( -18.50000324121759121, 18.34775554461856473, -236.8759397601555179 ) ) ;
#144638 = ORIENTED_EDGE ( 'NONE', *, *, #247899, .F. ) ;
#144639 = ADVANCED_FACE ( 'NONE', ( #198677 ), #139964, .F. ) ;
#144640 = CARTESIAN_POINT ( 'NONE',  ( -23.25000000000000000, 76.00000000001205080, -123.7481074845242972 ) ) ;
#144641 = DIRECTION ( 'NONE',  ( -0.000000000000000000, -6.982962677686266711E-15, 1.000000000000000000 ) ) ;
#144642 = DIRECTION ( 'NONE',  ( 1.000000000000000000, 0.000000000000000000, -0.000000000000000000 ) ) ;
#144643 = LINE ( 'NONE', #49411, #116692 ) ;
#144644 = DIRECTION ( 'NONE',  ( 0.000000000000000000, 1.000000000000000000, 0.000000000000000000 ) ) ;
#144645 = CARTESIAN_POINT ( 'NONE',  ( -21.93642651522410247, 7.327166239336959208, -134.0000000000000000 ) ) ;
#144646 = ADVANCED_FACE ( 'NONE', ( #86403 ), #66876, .T. ) ;
#144647 = CARTESIAN_POINT ( 'NONE',  ( 22.50000000000000000, 11.36146383068193444, -198.4232501820394816 ) ) ;
#144649 = ORIENTED_EDGE ( 'NONE', *, *, #37175, .F. ) ;
#144648 = CARTESIAN_POINT ( 'NONE',  ( 20.21494484322215968, 66.69682926214323970, -128.1828422927511610 ) ) ;
#144651 = CARTESIAN_POINT ( 'NONE',  ( 21.98333005346336222, 76.00000000001243450, -177.3971828135810256 ) ) ;
#144650 = CARTESIAN_POINT ( 'NONE',  ( -23.15000000000000213, 87.75000000001222134, -148.2731074845242176 ) ) ;
#144652 = VERTEX_POINT ( 'NONE', #166009 ) ;
#144654 = ORIENTED_EDGE ( 'NONE', *, *, #199548, .F. ) ;
#144653 = SPHERICAL_SURFACE ( 'NONE', #240154, 0.1000000000000000056 ) ;
#144655 = CIRCLE ( 'NONE', #190667, 0.09999999999999530098 ) ;
#144656 = ORIENTED_EDGE ( 'NONE', *, *, #36589, .T. ) ;
#144657 = CARTESIAN_POINT ( 'NONE',  ( 18.59999999999999076, 7.070967871809997973, -104.2465642218683541 ) ) ;
#144658 = CIRCLE ( 'NONE', #215396, 0.1000000000000028644 ) ;
#144659 = CIRCLE ( 'NONE', #215399, 11.79999999999999893 ) ;
#144660 = LINE ( 'NONE', #65128, #21829 ) ;
#144661 = CARTESIAN_POINT ( 'NONE',  ( 21.09107601085585415, 0.03930716472822039925, -127.6361220246393913 ) ) ;
#144662 = DIRECTION ( 'NONE',  ( 0.000000000000000000, 0.000000000000000000, -1.000000000000000000 ) ) ;
#144663 = LINE ( 'NONE', #224205, #74537 ) ;
#144665 = EDGE_CURVE ( 'NONE', #143795, #56745, #44924, .T. ) ;
#144664 = LINE ( 'NONE', #246352, #189988 ) ;
#144666 = CIRCLE ( 'NONE', #124412, 0.09999999999999158173 ) ;
#144667 = AXIS2_PLACEMENT_3D ( 'NONE', #64008, #125272, #182690 ) ;
#144668 = DIRECTION ( 'NONE',  ( 1.000000000000000000, 0.000000000000000000, -0.000000000000000000 ) ) ;
#144669 = ORIENTED_EDGE ( 'NONE', *, *, #224617, .T. ) ;
#144670 = VERTEX_POINT ( 'NONE', #126849 ) ;
#144671 = CARTESIAN_POINT ( 'NONE',  ( 18.39999999999999503, 11.74999999999998224, -24.25000000000001066 ) ) ;
#144672 = ORIENTED_EDGE ( 'NONE', *, *, #183522, .F. ) ;
#144673 = DIRECTION ( 'NONE',  ( -0.000000000000000000, -0.000000000000000000, 1.000000000000000000 ) ) ;
#144674 = EDGE_LOOP ( 'NONE', ( #42980, #82751, #142776, #38592 ) ) ;
#144675 = DIRECTION ( 'NONE',  ( 1.000000000000000000, 0.000000000000000000, -1.020425574104004196E-15 ) ) ;
#144676 = CIRCLE ( 'NONE', #3013, 0.1000000000000046824 ) ;
#144677 = EDGE_CURVE ( 'NONE', #62507, #178487, #223961, .T. ) ;
#144678 = CARTESIAN_POINT ( 'NONE',  ( 19.94784844284954772, 11.71308993302901946, -24.70219871729859662 ) ) ;
#144679 = CARTESIAN_POINT ( 'NONE',  ( -22.00356870143215460, 68.74575763754053526, -103.0231074845243455 ) ) ;
#144680 = DIRECTION ( 'NONE',  ( 0.000000000000000000, 0.000000000000000000, -1.000000000000000000 ) ) ;
#144681 = FACE_OUTER_BOUND ( 'NONE', #33084, .T. ) ;
#144682 = VERTEX_POINT ( 'NONE', #202532 ) ;
#144683 = AXIS2_PLACEMENT_3D ( 'NONE', #100759, #203762, #141223 ) ;
#144684 = AXIS2_PLACEMENT_3D ( 'NONE', #48551, #129376, #30289 ) ;
#144685 = DIRECTION ( 'NONE',  ( 0.000000000000000000, 6.982962677686266711E-15, -1.000000000000000000 ) ) ;
#144686 = AXIS2_PLACEMENT_3D ( 'NONE', #65967, #122098, #5972 ) ;
#144687 = DIRECTION ( 'NONE',  ( -1.000000000000000000, 0.000000000000000000, 0.000000000000000000 ) ) ;
#144688 = AXIS2_PLACEMENT_3D ( 'NONE', #17655, #97156, #176762 ) ;
#144689 = CARTESIAN_POINT ( 'NONE',  ( 18.50000000000000000, 85.40000000001158753, -62.22584772486099070 ) ) ;
#144690 = DIRECTION ( 'NONE',  ( 0.000000000000000000, 0.000000000000000000, -1.000000000000000000 ) ) ;
#144691 = EDGE_LOOP ( 'NONE', ( #79408, #3639, #256824, #91964 ) ) ;
#144692 = ORIENTED_EDGE ( 'NONE', *, *, #36194, .T. ) ;
#144695 = ORIENTED_EDGE ( 'NONE', *, *, #149212, .T. ) ;
#144694 = CARTESIAN_POINT ( 'NONE',  ( 20.94999999999999929, 87.29603075034775372, -173.0710066441881452 ) ) ;
#144693 = CARTESIAN_POINT ( 'NONE',  ( 21.51976009735019346, 69.08954155835274946, -103.0231074845243739 ) ) ;
#144696 = AXIS2_PLACEMENT_3D ( 'NONE', #126180, #7531, #4929 ) ;
#144697 = ADVANCED_FACE ( 'NONE', ( #102115 ), #245524, .T. ) ;
#144698 = ORIENTED_EDGE ( 'NONE', *, *, #176818, .F. ) ;
#144699 = CARTESIAN_POINT ( 'NONE',  ( -21.05000000000000071, 74.83729825007431202, -162.1231074845243540 ) ) ;
#144700 = FACE_OUTER_BOUND ( 'NONE', #208939, .T. ) ;
#144701 = DIRECTION ( 'NONE',  ( 1.000000000000000000, 0.000000000000000000, 0.000000000000000000 ) ) ;
#144702 = ORIENTED_EDGE ( 'NONE', *, *, #142021, .F. ) ;
#144703 = LINE ( 'NONE', #147283, #13755 ) ;
#144705 = EDGE_CURVE ( 'NONE', #96904, #216036, #186403, .T. ) ;
#144704 = CARTESIAN_POINT ( 'NONE',  ( -23.15000000000000213, 11.65000000001115588, -188.7499999999999716 ) ) ;
#144706 = DIRECTION ( 'NONE',  ( -4.408576920032448588E-17, 0.1350103645451876944, 0.9908441862701601321 ) ) ;
#144708 = VERTEX_POINT ( 'NONE', #181694 ) ;
#144707 = CARTESIAN_POINT ( 'NONE',  ( -18.59999999999999787, 76.00000000001170974, -69.52310748452431710 ) ) ;
#144709 = VECTOR ( 'NONE', #181851, 1000.000000000000227 ) ;
#144710 = EDGE_CURVE ( 'NONE', #47017, #102497, #219688, .T. ) ;
#144711 = EDGE_CURVE ( 'NONE', #188649, #207918, #144865, .T. ) ;
#144712 = ORIENTED_EDGE ( 'NONE', *, *, #188114, .F. ) ;
#144713 = DIRECTION ( 'NONE',  ( 0.000000000000000000, -0.9770955615653316162, -0.2128009952263604232 ) ) ;
#144714 = CARTESIAN_POINT ( 'NONE',  ( -18.37160782347004329, 11.47561641481354044, -176.7499999999999716 ) ) ;
#144715 = VECTOR ( 'NONE', #17341, 1000.000000000000114 ) ;
#144716 = DIRECTION ( 'NONE',  ( 0.000000000000000000, 0.9126074666063660468, 0.4088369013363524762 ) ) ;
#144717 = VERTEX_POINT ( 'NONE', #5586 ) ;
#144718 = CARTESIAN_POINT ( 'NONE',  ( -20.64999999999999858, 74.00000000001254818, -182.7477294072864709 ) ) ;
#144719 = ORIENTED_EDGE ( 'NONE', *, *, #200445, .T. ) ;
#144720 = EDGE_CURVE ( 'NONE', #160483, #82047, #244633, .T. ) ;
#144721 = FACE_OUTER_BOUND ( 'NONE', #180639, .T. ) ;
#144722 = CARTESIAN_POINT ( 'NONE',  ( 23.24999999999999289, 64.35000000001194564, -103.0231074845244024 ) ) ;
#144723 = ORIENTED_EDGE ( 'NONE', *, *, #65238, .F. ) ;
#144724 = DIRECTION ( 'NONE',  ( 1.000000000000000000, 0.000000000000000000, 0.000000000000000000 ) ) ;
#144725 = AXIS2_PLACEMENT_3D ( 'NONE', #221227, #42610, #23075 ) ;
#144726 = CARTESIAN_POINT ( 'NONE',  ( -18.35668295345803713, 64.52683809664931402, -78.77310748452438816 ) ) ;
#144727 = AXIS2_PLACEMENT_3D ( 'NONE', #61177, #217660, #102845 ) ;
#144728 = VERTEX_POINT ( 'NONE', #206391 ) ;
#144729 = ORIENTED_EDGE ( 'NONE', *, *, #26437, .T. ) ;
#144730 = ORIENTED_EDGE ( 'NONE', *, *, #11828, .T. ) ;
#144731 = CARTESIAN_POINT ( 'NONE',  ( -20.54999999999999716, 85.50000000001197975, -112.9170766071766820 ) ) ;
#144732 = ORIENTED_EDGE ( 'NONE', *, *, #155352, .F. ) ;
#144734 = ORIENTED_EDGE ( 'NONE', *, *, #49109, .T. ) ;
#144733 = CARTESIAN_POINT ( 'NONE',  ( 12.93279065517213766, 66.58230930894947619, -185.3815067877598040 ) ) ;
#144735 = EDGE_CURVE ( 'NONE', #128659, #248708, #215766, .T. ) ;
#144736 = EDGE_CURVE ( 'NONE', #168134, #108295, #253191, .T. ) ;
#144737 = ORIENTED_EDGE ( 'NONE', *, *, #227232, .T. ) ;
#144740 = EDGE_LOOP ( 'NONE', ( #151617, #30836, #160798, #188276 ) ) ;
#144739 = EDGE_LOOP ( 'NONE', ( #116529, #8824, #172921, #201682 ) ) ;
#144738 = CARTESIAN_POINT ( 'NONE',  ( -16.80438519320023616, 9.949779096479501206, -113.1507382809213027 ) ) ;
#144742 = ADVANCED_FACE ( 'NONE', ( #184248 ), #242934, .T. ) ;
#144741 = CARTESIAN_POINT ( 'NONE',  ( -18.41817142474039670, -9.498703066590936217, -107.1039654876371969 ) ) ;
#144743 = AXIS2_PLACEMENT_3D ( 'NONE', #213577, #49383, #230594 ) ;
#144744 = ORIENTED_EDGE ( 'NONE', *, *, #175926, .T. ) ;
#144745 = CARTESIAN_POINT ( 'NONE',  ( 20.94999999999999574, 1.115600667400684642E-11, -33.50000000000000000 ) ) ;
#144746 = CARTESIAN_POINT ( 'NONE',  ( 21.05000000000000071, 69.74218538953583391, -103.1208977758331571 ) ) ;
#144747 = AXIS2_PLACEMENT_3D ( 'NONE', #35692, #170084, #233863 ) ;
#144748 = ORIENTED_EDGE ( 'NONE', *, *, #92632, .T. ) ;
#144749 = FACE_OUTER_BOUND ( 'NONE', #88166, .T. ) ;
#144751 = ORIENTED_EDGE ( 'NONE', *, *, #141192, .F. ) ;
#144750 = CARTESIAN_POINT ( 'NONE',  ( -20.85000000000000142, -1.164121893230052995, -208.9148480855715775 ) ) ;
#144752 = CARTESIAN_POINT ( 'NONE',  ( -16.86337532320261090, 14.20933363574807728, -219.3453541648266309 ) ) ;
#144754 = ORIENTED_EDGE ( 'NONE', *, *, #43392, .T. ) ;
#144753 = DIRECTION ( 'NONE',  ( -1.000000000000000000, -2.952720810173289112E-16, 0.000000000000000000 ) ) ;
#144755 = ORIENTED_EDGE ( 'NONE', *, *, #241631, .T. ) ;
#144756 = CARTESIAN_POINT ( 'NONE',  ( 20.94999999999999574, -11.64999999998883595, -69.90000000000004832 ) ) ;
#144757 = ORIENTED_EDGE ( 'NONE', *, *, #54945, .F. ) ;
#144758 = ORIENTED_EDGE ( 'NONE', *, *, #147647, .T. ) ;
#144759 = DIRECTION ( 'NONE',  ( 0.000000000000000000, 0.000000000000000000, 1.000000000000000000 ) ) ;
#144761 = EDGE_CURVE ( 'NONE', #25415, #162117, #64308, .T. ) ;
#144760 = CARTESIAN_POINT ( 'NONE',  ( 23.14999999999999503, 64.25000000001151079, -48.27310748452440237 ) ) ;
#144762 = CIRCLE ( 'NONE', #236935, 0.09999999999999939493 ) ;
#144764 = EDGE_LOOP ( 'NONE', ( #50318, #191590, #190677, #70837, #25078, #147445 ) ) ;
#144763 = EDGE_LOOP ( 'NONE', ( #12304, #177138, #237107, #217513 ) ) ;
#144765 = ORIENTED_EDGE ( 'NONE', *, *, #125347, .F. ) ;
#144766 = DIRECTION ( 'NONE',  ( -0.000000000000000000, -6.982962677686266711E-15, 1.000000000000000000 ) ) ;
#144767 = ORIENTED_EDGE ( 'NONE', *, *, #188599, .T. ) ;
#144768 = ORIENTED_EDGE ( 'NONE', *, *, #94630, .F. ) ;
#144769 = CARTESIAN_POINT ( 'NONE',  ( 18.44444291854884099, 85.49010118095564792, -163.3942035196333507 ) ) ;
#144772 = EDGE_CURVE ( 'NONE', #256108, #172693, #174136, .T. ) ;
#144771 = ORIENTED_EDGE ( 'NONE', *, *, #229422, .F. ) ;
#144770 = DIRECTION ( 'NONE',  ( 0.000000000000000000, 0.000000000000000000, 1.000000000000000000 ) ) ;
#144773 = CARTESIAN_POINT ( 'NONE',  ( -22.39999999999999858, 64.25000000001215028, -136.4231074845243938 ) ) ;
#144774 = AXIS2_PLACEMENT_3D ( 'NONE', #102226, #219637, #1859 ) ;
#144775 = B_SPLINE_CURVE_WITH_KNOTS ( 'NONE', 3,
 ( #131421, #210969, #174458, #32364, #231827, #135259, #111878, #114433 ),
 .UNSPECIFIED., .F., .F.,
 ( 4, 2, 2, 4 ),
 ( 0.000000000000000000, 0.0001881495939909273306, 0.0002822243909863910230, 0.0003762991879818546612 ),
 .UNSPECIFIED. ) ;
#144777 = CARTESIAN_POINT ( 'NONE',  ( 18.49351773456750792, -9.443025695134291908, -107.6853255260268440 ) ) ;
#144776 = CARTESIAN_POINT ( 'NONE',  ( -16.77683809663752257, 66.05416425680765258, -82.18705650362858250 ) ) ;
#144778 = CARTESIAN_POINT ( 'NONE',  ( 18.46082813848004278, 85.48074965092008881, -196.4387373818086360 ) ) ;
#144779 = ORIENTED_EDGE ( 'NONE', *, *, #106194, .T. ) ;
#144780 = EDGE_CURVE ( 'NONE', #150591, #248567, #27783, .T. ) ;
#144781 = EDGE_LOOP ( 'NONE', ( #81145, #123190, #202186 ) ) ;
#144782 = VECTOR ( 'NONE', #211372, 1000.000000000000227 ) ;
#144783 = DIRECTION ( 'NONE',  ( 0.000000000000000000, -7.056502275159894776E-15, 1.000000000000000000 ) ) ;
#144784 = EDGE_CURVE ( 'NONE', #221637, #6683, #11820, .T. ) ;
#144785 = ORIENTED_EDGE ( 'NONE', *, *, #174916, .T. ) ;
#144786 = AXIS2_PLACEMENT_3D ( 'NONE', #121938, #39851, #119372 ) ;
#144787 = AXIS2_PLACEMENT_3D ( 'NONE', #93193, #172784, #213143 ) ;
#144788 = CIRCLE ( 'NONE', #40795, 4.049999999999998046 ) ;
#144789 = AXIS2_PLACEMENT_3D ( 'NONE', #86248, #165836, #249211 ) ;
#144790 = EDGE_CURVE ( 'NONE', #202540, #139774, #149178, .T. ) ;
#144791 = CARTESIAN_POINT ( 'NONE',  ( -23.25000000000000000, 45.99141771592758943, -256.5205054824189119 ) ) ;
#144793 = EDGE_CURVE ( 'NONE', #111920, #251883, #86580, .T. ) ;
#144792 = EDGE_CURVE ( 'NONE', #245368, #93742, #7490, .T. ) ;
#144794 = VERTEX_POINT ( 'NONE', #74624 ) ;
#144795 = ORIENTED_EDGE ( 'NONE', *, *, #82963, .F. ) ;
#144796 = FACE_OUTER_BOUND ( 'NONE', #136227, .T. ) ;
#144797 = VERTEX_POINT ( 'NONE', #232394 ) ;
#144798 = DIRECTION ( 'NONE',  ( 0.000000000000000000, 0.008583690987128059571, -0.9999631594459056361 ) ) ;
#144799 = CARTESIAN_POINT ( 'NONE',  ( 18.39999999999999503, 5.650000000011139001, -79.65000000000004832 ) ) ;
#144800 = ORIENTED_EDGE ( 'NONE', *, *, #81555, .F. ) ;
#144801 = DIRECTION ( 'NONE',  ( 0.000000000000000000, 1.000000000000000000, 6.982962677686266711E-15 ) ) ;
#144802 = DIRECTION ( 'NONE',  ( 0.000000000000000000, 0.000000000000000000, 1.000000000000000000 ) ) ;
#144804 = DIRECTION ( 'NONE',  ( 0.000000000000000000, 0.000000000000000000, -1.000000000000000000 ) ) ;
#144803 = CARTESIAN_POINT ( 'NONE',  ( -18.50000000000000000, -26.43935341558978891, -51.64150860750746119 ) ) ;
#144805 = CARTESIAN_POINT ( 'NONE',  ( 21.05000000000000071, -4.756823075239758225, -233.1486023682345490 ) ) ;
#144806 = CARTESIAN_POINT ( 'NONE',  ( 21.14999999999999858, 65.28660755661240955, -157.7731074845244450 ) ) ;
#144807 = DIRECTION ( 'NONE',  ( 0.000000000000000000, 0.8814952561688430555, -0.4721928772777346239 ) ) ;
#144808 = CARTESIAN_POINT ( 'NONE',  ( 17.23472005113828232, 65.69211804551129319, -125.0696843445930568 ) ) ;
#144809 = AXIS2_PLACEMENT_3D ( 'NONE', #214852, #36246, #152351 ) ;
#144810 = ORIENTED_EDGE ( 'NONE', *, *, #68840, .T. ) ;
#144811 = ADVANCED_FACE ( 'NONE', ( #92848 ), #49186, .T. ) ;
#144813 = EDGE_CURVE ( 'NONE', #139998, #45529, #130691, .T. ) ;
#144812 = AXIS2_PLACEMENT_3D ( 'NONE', #136083, #197362, #38308 ) ;
#144814 = ADVANCED_BREP_SHAPE_REPRESENTATION ( '', ( #108017, #2425 ), #231390 ) ;
#144817 = ORIENTED_EDGE ( 'NONE', *, *, #245717, .F. ) ;
#144816 = ORIENTED_EDGE ( 'NONE', *, *, #167239, .T. ) ;
#144815 = VECTOR ( 'NONE', #107925, 1000.000000000000114 ) ;
#144818 = VERTEX_POINT ( 'NONE', #52429 ) ;
#144819 = TOROIDAL_SURFACE ( 'NONE', #211471, 0.2000000000000000111, 0.1000000000000000056 ) ;
#144820 = AXIS2_PLACEMENT_3D ( 'NONE', #93720, #172020, #173314 ) ;
#144821 = EDGE_CURVE ( 'NONE', #257964, #175390, #119968, .T. ) ;
#144822 = DIRECTION ( 'NONE',  ( 0.000000000000000000, -0.000000000000000000, -1.000000000000000000 ) ) ;
#144823 = CARTESIAN_POINT ( 'NONE',  ( -16.88460203013675454, 66.04524099677610138, -82.15721567498616196 ) ) ;
#144824 = AXIS2_PLACEMENT_3D ( 'NONE', #138496, #116409, #216773 ) ;
#144826 = CARTESIAN_POINT ( 'NONE',  ( -16.87242674293850797, 9.950000000011138823, -146.6489097536276631 ) ) ;
#144825 = DIRECTION ( 'NONE',  ( 0.000000000000000000, 0.000000000000000000, 1.000000000000000000 ) ) ;
#144827 = CARTESIAN_POINT ( 'NONE',  ( -21.08884785362073089, 75.95021690494546363, -142.8803008519499258 ) ) ;
#144828 = VERTEX_POINT ( 'NONE', #210254 ) ;
#144829 = DIRECTION ( 'NONE',  ( 0.000000000000000000, 6.982962677686266711E-15, -1.000000000000000000 ) ) ;
#144830 = EDGE_CURVE ( 'NONE', #81533, #236784, #193643, .T. ) ;
#144831 = SPHERICAL_SURFACE ( 'NONE', #50116, 0.1000000000000000056 ) ;
#144832 = DIRECTION ( 'NONE',  ( 0.000000000000000000, 1.810617628050740656E-13, 1.000000000000000000 ) ) ;
#144833 = EDGE_CURVE ( 'NONE', #57112, #140955, #111735, .T. ) ;
#144834 = DIRECTION ( 'NONE',  ( -0.000000000000000000, 6.982962677686266711E-15, -1.000000000000000000 ) ) ;
#144835 = ORIENTED_EDGE ( 'NONE', *, *, #29131, .F. ) ;
#144836 = CIRCLE ( 'NONE', #153087, 0.09999999999999609201 ) ;
#144837 = CIRCLE ( 'NONE', #103319, 0.2000000000000057288 ) ;
#144838 = AXIS2_PLACEMENT_3D ( 'NONE', #129809, #89395, #170277 ) ;
#144839 = CARTESIAN_POINT ( 'NONE',  ( 18.50000000000000000, -9.399999999999998579, -7.297259759663296208 ) ) ;
#144840 = DIRECTION ( 'NONE',  ( 0.000000000000000000, 0.000000000000000000, 1.000000000000000000 ) ) ;
#144841 = ORIENTED_EDGE ( 'NONE', *, *, #224707, .F. ) ;
#144842 = EDGE_LOOP ( 'NONE', ( #131498, #228137, #195681, #1423 ) ) ;
#144843 = CARTESIAN_POINT ( 'NONE',  ( -16.87036670365549895, 66.01058118071095748, -191.0026676018264880 ) ) ;
#144844 = DIRECTION ( 'NONE',  ( 1.000000000000000000, -0.000000000000000000, 0.000000000000000000 ) ) ;
#144845 = CARTESIAN_POINT ( 'NONE',  ( 18.59999999999999787, -9.849999999999990763, 31.39999999999999858 ) ) ;
#144846 = EDGE_CURVE ( 'NONE', #88021, #46518, #153283, .T. ) ;
#144847 = DIRECTION ( 'NONE',  ( 0.000000000000000000, 1.000000000000000000, 0.000000000000000000 ) ) ;
#144848 = DIRECTION ( 'NONE',  ( 0.000000000000000000, -1.000000000000000000, 0.000000000000000000 ) ) ;
#144849 = CARTESIAN_POINT ( 'NONE',  ( -21.05000000000000071, 6.540656951701244282, 4.079310673976710433E-15 ) ) ;
#144850 = ORIENTED_EDGE ( 'NONE', *, *, #169316, .F. ) ;
#144851 = CARTESIAN_POINT ( 'NONE',  ( 18.39999999999997371, 11.75000000001113953, -42.75000000000000000 ) ) ;
#144852 = DIRECTION ( 'NONE',  ( 2.715809747126116015E-16, -0.9770955615653313941, -0.2128009952263606730 ) ) ;
#144853 = CYLINDRICAL_SURFACE ( 'NONE', #162519, 11.80000000000000426 ) ;
#144854 = AXIS2_PLACEMENT_3D ( 'NONE', #230820, #53444, #235916 ) ;
#144856 = DIRECTION ( 'NONE',  ( 0.000000000000000000, 0.9126074666063771490, 0.4088369013363281623 ) ) ;
#144855 = CARTESIAN_POINT ( 'NONE',  ( -16.93211319090181632, 9.999986781168624717, -87.92250549927310033 ) ) ;
#144857 = DIRECTION ( 'NONE',  ( -1.000000000000000000, 3.265361837132813093E-16, 2.280189983783949500E-30 ) ) ;
#144858 = AXIS2_PLACEMENT_3D ( 'NONE', #155135, #96385, #15621 ) ;
#144860 = EDGE_CURVE ( 'NONE', #203964, #209282, #31635, .T. ) ;
#144859 = SURFACE_STYLE_USAGE ( .BOTH. , #84856 ) ;
#144861 = CARTESIAN_POINT ( 'NONE',  ( -23.25000000000000355, 65.95000000001186891, -90.27310748452438816 ) ) ;
#144862 = DIRECTION ( 'NONE',  ( -1.000000000000000000, -0.000000000000000000, 0.000000000000000000 ) ) ;
#144864 = ORIENTED_EDGE ( 'NONE', *, *, #168287, .F. ) ;
#144863 = FACE_OUTER_BOUND ( 'NONE', #70583, .T. ) ;
#144865 = CIRCLE ( 'NONE', #178024, 0.09999999999999982514 ) ;
#144866 = EDGE_CURVE ( 'NONE', #153155, #218074, #72025, .T. ) ;
#144867 = CIRCLE ( 'NONE', #40858, 0.1000000000000021289 ) ;
#144868 = DIRECTION ( 'NONE',  ( 2.952720810173289112E-16, -1.000000000000000000, 0.000000000000000000 ) ) ;
#144869 = VECTOR ( 'NONE', #45141, 1000.000000000000000 ) ;
#144870 = AXIS2_PLACEMENT_3D ( 'NONE', #124359, #5653, #205147 ) ;
#144871 = CARTESIAN_POINT ( 'NONE',  ( 21.17356465864818915, 65.45462388619900196, -242.0281076209811033 ) ) ;
#144872 = AXIS2_PLACEMENT_3D ( 'NONE', #55175, #36972, #18656 ) ;
#144873 = DIRECTION ( 'NONE',  ( 0.000000000000000000, 1.000000000000000000, 6.982962677686266711E-15 ) ) ;
#144874 = ORIENTED_EDGE ( 'NONE', *, *, #94958, .T. ) ;
#144875 = CARTESIAN_POINT ( 'NONE',  ( -23.15000000000000213, 4.250000000000000000, -21.14999999999999858 ) ) ;
#144876 = CARTESIAN_POINT ( 'NONE',  ( -20.85000000000000142, 68.97833521811179480, -99.38954208262707368 ) ) ;
#144877 = DIRECTION ( 'NONE',  ( -0.000000000000000000, -6.982962677686266711E-15, 1.000000000000000000 ) ) ;
#144878 = ORIENTED_EDGE ( 'NONE', *, *, #172376, .T. ) ;
#144879 = DIRECTION ( 'NONE',  ( 1.000000000000000000, 0.000000000000000000, 0.000000000000000000 ) ) ;
#144881 = ORIENTED_EDGE ( 'NONE', *, *, #15520, .T. ) ;
#144880 = CARTESIAN_POINT ( 'NONE',  ( 20.85000000000000142, 36.48445852813179613, -249.2750065094666923 ) ) ;
#144883 = CARTESIAN_POINT ( 'NONE',  ( -21.05000000000000071, 76.10000000001203091, -114.6731074845243086 ) ) ;
#144882 = CARTESIAN_POINT ( 'NONE',  ( 18.54999999999999716, 67.25000000001197975, -115.6731074845243654 ) ) ;
#144884 = DIRECTION ( 'NONE',  ( -0.000000000000000000, -0.9887567792719339499, -0.1495327102803676589 ) ) ;
#144885 = ORIENTED_EDGE ( 'NONE', *, *, #231093, .F. ) ;
#144886 = FACE_OUTER_BOUND ( 'NONE', #48484, .T. ) ;
#144887 = AXIS2_PLACEMENT_3D ( 'NONE', #140810, #236051, #2958 ) ;
#144888 = DIRECTION ( 'NONE',  ( 1.000000000000000000, 0.000000000000000000, 0.000000000000000000 ) ) ;
#144889 = CARTESIAN_POINT ( 'NONE',  ( -22.50000000000000000, 76.00000000001267608, -203.5231074845243597 ) ) ;
#144890 = LINE ( 'NONE', #125350, #77302 ) ;
#144891 = DIRECTION ( 'NONE',  ( 1.000000000000000000, -0.000000000000000000, -0.000000000000000000 ) ) ;
#144892 = ORIENTED_EDGE ( 'NONE', *, *, #112252, .F. ) ;
#144893 = FACE_OUTER_BOUND ( 'NONE', #159262, .T. ) ;
#144894 = CIRCLE ( 'NONE', #82518, 0.09999999999999820144 ) ;
#144895 = LINE ( 'NONE', #219307, #234488 ) ;
#144896 = CARTESIAN_POINT ( 'NONE',  ( -23.25000000000000000, -8.999999999988844479, -57.10603087734755690 ) ) ;
#144897 = ORIENTED_EDGE ( 'NONE', *, *, #96928, .F. ) ;
#144898 = EDGE_LOOP ( 'NONE', ( #186052, #25771, #82024, #137098, #52586 ) ) ;
#144899 = LINE ( 'NONE', #207479, #192242 ) ;
#144900 = DIRECTION ( 'NONE',  ( 0.000000000000000000, 0.000000000000000000, -1.000000000000000000 ) ) ;
#144901 = DIRECTION ( 'NONE',  ( 0.000000000000000000, 0.000000000000000000, 1.000000000000000000 ) ) ;
#144902 = CARTESIAN_POINT ( 'NONE',  ( 21.05000000000000071, 13.06600978423091242, -210.6006273873371129 ) ) ;
#144903 = DIRECTION ( 'NONE',  ( 1.000000000000000000, 1.394253735153569469E-16, 2.602809386958778209E-16 ) ) ;
#144904 = ADVANCED_FACE ( 'NONE', ( #212818 ), #151581, .T. ) ;
#144906 = SURFACE_SIDE_STYLE ('',( #125372 ) ) ;
#144905 = CARTESIAN_POINT ( 'NONE',  ( 20.94999999999999929, -8.999999999988842703, -124.6060308773475924 ) ) ;
#144907 = AXIS2_PLACEMENT_3D ( 'NONE', #166444, #162579, #226355 ) ;
#144908 = AXIS2_PLACEMENT_3D ( 'NONE', #107680, #2151, #42574 ) ;
#144909 = DIRECTION ( 'NONE',  ( 1.000000000000000000, -0.000000000000000000, -0.000000000000000000 ) ) ;
#144910 = DIRECTION ( 'NONE',  ( -0.000000000000000000, 0.8660254037844377084, 0.5000000000000016653 ) ) ;
#144911 = AXIS2_PLACEMENT_3D ( 'NONE', #256429, #40054, #118284 ) ;
#144912 = CARTESIAN_POINT ( 'NONE',  ( -18.43599941264851338, 46.91436743304934254, -255.3877617659306338 ) ) ;
#144913 = CARTESIAN_POINT ( 'NONE',  ( 23.14999999999999858, 76.00000000001244871, -170.0231074845243597 ) ) ;
#144915 = ORIENTED_EDGE ( 'NONE', *, *, #154200, .F. ) ;
#144914 = CARTESIAN_POINT ( 'NONE',  ( 14.22916352759892433, 62.94600569631032982, -215.5247064183336363 ) ) ;
#144916 = DIRECTION ( 'NONE',  ( 0.000000000000000000, 0.9126074666063622720, 0.4088369013363611360 ) ) ;
#144917 = CARTESIAN_POINT ( 'NONE',  ( -20.85000000000000142, -1.164121893230052995, -175.2148480855716173 ) ) ;
#144919 = LINE ( 'NONE', #187928, #128364 ) ;
#144918 = DIRECTION ( 'NONE',  ( 6.938893903907030216E-14, 0.000000000000000000, 1.000000000000000000 ) ) ;
#144920 = EDGE_LOOP ( 'NONE', ( #169004, #226643, #195126, #206040 ) ) ;
#144921 = CARTESIAN_POINT ( 'NONE',  ( -23.15000000000000213, 11.75000000001115552, -167.4999999999999716 ) ) ;
#144922 = DIRECTION ( 'NONE',  ( 0.000000000000000000, 0.000000000000000000, -1.000000000000000000 ) ) ;
#144923 = DIRECTION ( 'NONE',  ( 0.000000000000000000, 0.1290532225515392817, 0.9916376685811522096 ) ) ;
#144924 = DIRECTION ( 'NONE',  ( 0.000000000000000000, 0.000000000000000000, -1.000000000000000000 ) ) ;
#144925 = CYLINDRICAL_SURFACE ( 'NONE', #41001, 4.049999999999998046 ) ;
#144926 = ORIENTED_EDGE ( 'NONE', *, *, #170366, .T. ) ;
#144928 = ADVANCED_FACE ( 'NONE', ( #188110 ), #113705, .F. ) ;
#144927 = EDGE_LOOP ( 'NONE', ( #149999, #203446, #161183, #48233 ) ) ;
#144929 = EDGE_CURVE ( 'NONE', #250188, #94806, #37511, .T. ) ;
#144930 = AXIS2_PLACEMENT_3D ( 'NONE', #155542, #111247, #10867 ) ;
#144932 = VECTOR ( 'NONE', #244363, 1000.000000000000000 ) ;
#144931 = CARTESIAN_POINT ( 'NONE',  ( 23.15000000000000213, 87.65000000001245439, -181.7731074845242745 ) ) ;
#144933 = EDGE_LOOP ( 'NONE', ( #72260, #118287, #7035, #256612 ) ) ;
#144934 = ORIENTED_EDGE ( 'NONE', *, *, #28388, .T. ) ;
#144935 =( BOUNDED_SURFACE ( )  B_SPLINE_SURFACE ( 3, 2, ( 
 ( #52325, #108471, #212720 ),
 ( #231009, #88884, #148894 ),
 ( #28982, #49776, #188017 ),
 ( #48489, #34111, #73230 ),
 ( #32830, #9356, #128042 ),
 ( #113606, #92744, #131886 ) ),
 .UNSPECIFIED., .F., .F., .T. ) 
 B_SPLINE_SURFACE_WITH_KNOTS ( ( 4, 2, 4 ),
 ( 3, 3 ),
 ( 3.141592653589852180, 3.926990816987266264, 4.712388980384680792 ),
 ( 0.000000000000000000, 1.000000000000000000 ),
 .UNSPECIFIED. ) 
 GEOMETRIC_REPRESENTATION_ITEM ( )  RATIONAL_B_SPLINE_SURFACE ( (
 ( 1.000000000000000000, 0.9238795325112717505, 1.000000000000000000),
 ( 1.000000000000000000, 0.9240297172246723090, 1.000000000000000000),
 ( 1.000000000000000000, 0.9038128468035413476, 1.000000000000000000),
 ( 1.000000000000000000, 0.8282379607653282960, 1.000000000000000000),
 ( 1.000000000000000000, 0.7727932973488256252, 1.000000000000000000),
 ( 1.000000000000000000, 0.7071067811865475727, 1.000000000000000000) ) ) 
 REPRESENTATION_ITEM ( '' )  SURFACE ( )  );
#144937 = DIRECTION ( 'NONE',  ( -0.000000000000000000, -0.2128009952263603677, 0.9770955615653313941 ) ) ;
#144936 = AXIS2_PLACEMENT_3D ( 'NONE', #21346, #1737, #243894 ) ;
#144938 = LINE ( 'NONE', #124128, #31698 ) ;
#144939 = EDGE_CURVE ( 'NONE', #217025, #40550, #99814, .T. ) ;
#144941 = EDGE_CURVE ( 'NONE', #113374, #119750, #155444, .T. ) ;
#144940 = DIRECTION ( 'NONE',  ( 1.000000000000000000, 0.000000000000000000, 0.000000000000000000 ) ) ;
#144942 = EDGE_LOOP ( 'NONE', ( #93316, #163701, #203052, #18127 ) ) ;
#144943 = EDGE_CURVE ( 'NONE', #170938, #81245, #240083, .T. ) ;
#144944 = CARTESIAN_POINT ( 'NONE',  ( -21.64999999999999858, 10.05000000001113847, -146.7500000000000284 ) ) ;
#144945 = CARTESIAN_POINT ( 'NONE',  ( 22.42357213249528769, 68.32706761365223258, -136.6221944485259030 ) ) ;
#144946 = CARTESIAN_POINT ( 'NONE',  ( 20.99780126800918723, 11.60538868788781031, -160.5873525717055372 ) ) ;
#144947 = CARTESIAN_POINT ( 'NONE',  ( -16.77732147262506146, 30.19251626946681810, -234.8042213958585478 ) ) ;
#144948 = DIRECTION ( 'NONE',  ( 1.000000000000000000, 0.000000000000000000, 0.000000000000000000 ) ) ;
#144949 = CARTESIAN_POINT ( 'NONE',  ( 22.59999999999999787, 64.35042919246734527, -136.6231074845243825 ) ) ;
#144950 = ADVANCED_FACE ( 'NONE', ( #35490 ), #117557, .F. ) ;
#144951 = CARTESIAN_POINT ( 'NONE',  ( 15.06592377766033053, 62.16167874586911779, -218.5680441376359227 ) ) ;
#144952 = CIRCLE ( 'NONE', #24177, 0.1999999999999987899 ) ;
#144953 = VERTEX_POINT ( 'NONE', #180116 ) ;
#144955 = FACE_OUTER_BOUND ( 'NONE', #167443, .T. ) ;
#144954 = CARTESIAN_POINT ( 'NONE',  ( -20.94999999999999929, 30.43677443282724937, -239.5249545687858870 ) ) ;
#144957 = ORIENTED_EDGE ( 'NONE', *, *, #237406, .F. ) ;
#144956 = AXIS2_PLACEMENT_3D ( 'NONE', #42146, #160820, #179109 ) ;
#144959 = ORIENTED_EDGE ( 'NONE', *, *, #154609, .T. ) ;
#144958 = DIRECTION ( 'NONE',  ( 0.000000000000000000, 0.000000000000000000, -1.000000000000000000 ) ) ;
#144960 = AXIS2_PLACEMENT_3D ( 'NONE', #50626, #153659, #151042 ) ;
#144961 = EDGE_LOOP ( 'NONE', ( #96315, #48596, #76092, #132233, #93772 ) ) ;
#144962 = DIRECTION ( 'NONE',  ( 0.000000000000000000, 0.000000000000000000, -1.000000000000000000 ) ) ;
#144963 = ADVANCED_FACE ( 'NONE', ( #198377 ), #165750, .T. ) ;
#144964 = DIRECTION ( 'NONE',  ( 0.000000000000000000, 0.1575844902526560010, 0.9875055080513781558 ) ) ;
#144965 = CARTESIAN_POINT ( 'NONE',  ( 21.05000000000000071, 60.06173988932783203, -221.3217724115915814 ) ) ;
#144966 = ORIENTED_EDGE ( 'NONE', *, *, #200865, .T. ) ;
#144967 = FACE_OUTER_BOUND ( 'NONE', #135227, .T. ) ;
#144968 = CIRCLE ( 'NONE', #199145, 1.500000000000001332 ) ;
#144969 = DIRECTION ( 'NONE',  ( 0.000000000000000000, -0.000000000000000000, -1.000000000000000000 ) ) ;
#144970 = ORIENTED_EDGE ( 'NONE', *, *, #54037, .F. ) ;
#144972 = EDGE_CURVE ( 'NONE', #24103, #3690, #57549, .T. ) ;
#144971 = FACE_OUTER_BOUND ( 'NONE', #205163, .T. ) ;
#144973 = CYLINDRICAL_SURFACE ( 'NONE', #230711, 0.1000000000000010741 ) ;
#144974 = CIRCLE ( 'NONE', #7629, 0.1000000000000124678 ) ;
#144975 = VERTEX_POINT ( 'NONE', #19762 ) ;
#144976 = AXIS2_PLACEMENT_3D ( 'NONE', #78459, #175060, #52467 ) ;
#144977 = CARTESIAN_POINT ( 'NONE',  ( -16.80621392010912984, 9.942202577518864715, -146.6895919654172076 ) ) ;
#144978 = CIRCLE ( 'NONE', #211823, 11.65000000000000036 ) ;
#144979 = ORIENTED_EDGE ( 'NONE', *, *, #51170, .T. ) ;
#144980 = DIRECTION ( 'NONE',  ( 1.000000000000000000, -0.000000000000000000, -0.000000000000000000 ) ) ;
#144982 = ORIENTED_EDGE ( 'NONE', *, *, #70985, .F. ) ;
#144981 = AXIS2_PLACEMENT_3D ( 'NONE', #73128, #246584, #90068 ) ;
#144983 = DIRECTION ( 'NONE',  ( 1.000000000000000000, 0.000000000000000000, 0.000000000000000000 ) ) ;
#144984 = DIRECTION ( 'NONE',  ( 0.000000000000000000, 0.000000000000000000, -1.000000000000000000 ) ) ;
#144985 =( BOUNDED_CURVE ( )  B_SPLINE_CURVE ( 3, ( #240658, #120742, #63296, #162425 ),
 .UNSPECIFIED., .F., .F. ) 
 B_SPLINE_CURVE_WITH_KNOTS ( ( 4, 4 ),
 ( 1.570796326794895448, 3.141592653589791784 ),
 .UNSPECIFIED. ) 
 CURVE ( )  GEOMETRIC_REPRESENTATION_ITEM ( )  RATIONAL_B_SPLINE_CURVE ( ( 1.000000000000000000, 0.8047378541243650485, 0.8047378541243650485, 1.000000000000000000 ) ) 
 REPRESENTATION_ITEM ( '' )  );
#144986 = CARTESIAN_POINT ( 'NONE',  ( 23.15000000000000213, 61.88149656937974896, -248.1136133839584090 ) ) ;
#144987 = AXIS2_PLACEMENT_3D ( 'NONE', #197851, #202988, #118338 ) ;
#144988 = CARTESIAN_POINT ( 'NONE',  ( 20.73486653747088937, 68.25000000001222134, -149.1731074845244223 ) ) ;
#144989 = DIRECTION ( 'NONE',  ( 0.000000000000000000, -1.387778780781454006E-13, 1.000000000000000000 ) ) ;
#144991 = DIRECTION ( 'NONE',  ( 0.000000000000000000, -0.2617529984164955192, -0.9651348961777178603 ) ) ;
#144990 = AXIS2_PLACEMENT_3D ( 'NONE', #250606, #212787, #71993 ) ;
#144992 = ORIENTED_EDGE ( 'NONE', *, *, #189485, .T. ) ;
#144994 = DIRECTION ( 'NONE',  ( -1.000000000000000000, -2.885090398161910739E-16, -6.283419270304611573E-17 ) ) ;
#144993 = CARTESIAN_POINT ( 'NONE',  ( 23.14999999999999147, 1.115600667400684642E-11, -167.4999999999999716 ) ) ;
#144995 = ADVANCED_FACE ( 'NONE', ( #219215 ), #107458, .T. ) ;
#144996 = AXIS2_PLACEMENT_3D ( 'NONE', #34216, #195854, #75877 ) ;
#144998 = ADVANCED_FACE ( 'NONE', ( #234946 ), #99058, .T. ) ;
#144997 = TOROIDAL_SURFACE ( 'NONE', #149137, 0.2000000000000000111, 0.1000000000000000056 ) ;
#144999 = AXIS2_PLACEMENT_3D ( 'NONE', #5284, #163127, #104390 ) ;
#145000 = CIRCLE ( 'NONE', #211681, 0.1999999999999987899 ) ;
#145001 = CARTESIAN_POINT ( 'NONE',  ( -18.50000000000000000, 85.40000000001241176, -163.1410656363516125 ) ) ;
#145002 = FACE_OUTER_BOUND ( 'NONE', #100262, .T. ) ;
#145004 = ORIENTED_EDGE ( 'NONE', *, *, #86065, .F. ) ;
#145003 = DIRECTION ( 'NONE',  ( 0.000000000000000000, 7.162729191130010591E-15, -1.000000000000000000 ) ) ;
#145006 = ORIENTED_EDGE ( 'NONE', *, *, #33971, .F. ) ;
#145005 = DIRECTION ( 'NONE',  ( -1.000000000000000000, -0.000000000000000000, -0.000000000000000000 ) ) ;
#145007 = AXIS2_PLACEMENT_3D ( 'NONE', #120762, #211836, #166318 ) ;
#145008 = EDGE_CURVE ( 'NONE', #172263, #75669, #227315, .T. ) ;
#145010 = EDGE_CURVE ( 'NONE', #22426, #208600, #249135, .T. ) ;
#145009 = CARTESIAN_POINT ( 'NONE',  ( -19.89999999999999858, 5.586869315528661062, 16.41686199900910736 ) ) ;
#145011 = DIRECTION ( 'NONE',  ( 0.000000000000000000, -6.467318590049456648E-15, 1.000000000000000000 ) ) ;
#145012 = CARTESIAN_POINT ( 'NONE',  ( -23.15000000000000213, 11.65000000001115588, -126.9851942293460922 ) ) ;
#145014 = ORIENTED_EDGE ( 'NONE', *, *, #187203, .T. ) ;
#145013 = CARTESIAN_POINT ( 'NONE',  ( 21.11345278033211414, 67.11787792664067354, -157.7770853137656104 ) ) ;
#145015 = ADVANCED_FACE ( 'NONE', ( #17194 ), #197082, .T. ) ;
#145016 = PRODUCT_DEFINITION_SHAPE ( 'NONE', 'NONE',  #75539 ) ;
#145017 = EDGE_CURVE ( 'NONE', #30910, #38939, #53298, .T. ) ;
#145019 = EDGE_CURVE ( 'NONE', #60353, #76100, #177472, .T. ) ;
#145018 = AXIS2_PLACEMENT_3D ( 'NONE', #2318, #24493, #197963 ) ;
#145020 = AXIS2_PLACEMENT_3D ( 'NONE', #186945, #24013, #125654 ) ;
#145021 = CARTESIAN_POINT ( 'NONE',  ( -18.40000000000000213, 64.58541674041228475, -123.8731074845243683 ) ) ;
#145022 = CARTESIAN_POINT ( 'NONE',  ( -21.55000000000000071, 7.250000000011155521, -112.8500000000000369 ) ) ;
#145023 = ORIENTED_EDGE ( 'NONE', *, *, #249936, .F. ) ;
#145024 = ORIENTED_EDGE ( 'NONE', *, *, #76129, .T. ) ;
#145025 = EDGE_CURVE ( 'NONE', #132976, #154226, #199042, .T. ) ;
#145026 = CARTESIAN_POINT ( 'NONE',  ( -20.54999999999999716, 76.00000000001170974, -69.52310748452431710 ) ) ;
#145027 = CARTESIAN_POINT ( 'NONE',  ( -23.25000000000000000, 76.00000000001237765, -170.0231074845243597 ) ) ;
#145028 = ORIENTED_EDGE ( 'NONE', *, *, #5033, .T. ) ;
#145029 = FACE_OUTER_BOUND ( 'NONE', #45375, .T. ) ;
#145030 = CIRCLE ( 'NONE', #90866, 4.049999999999998046 ) ;
#145031 = EDGE_CURVE ( 'NONE', #205417, #107215, #204782, .T. ) ;
#145032 = CIRCLE ( 'NONE', #49375, 11.65000000000000036 ) ;
#145033 = CARTESIAN_POINT ( 'NONE',  ( -21.05000000000000071, 79.07891399537199106, -236.0635483022085452 ) ) ;
#145035 = EDGE_LOOP ( 'NONE', ( #69856, #215442, #81323, #44151, #26108 ) ) ;
#145034 = CIRCLE ( 'NONE', #65941, 0.09999999999999982514 ) ;
#145036 = EDGE_CURVE ( 'NONE', #81393, #116965, #236617, .T. ) ;
#145037 = ADVANCED_FACE ( 'NONE', ( #43166 ), #211719, .F. ) ;
#145038 = DIRECTION ( 'NONE',  ( 0.000000000000000000, 0.4999999999999478195, -0.8660254037844686836 ) ) ;
#145039 = VECTOR ( 'NONE', #24906, 1000.000000000000000 ) ;
#145040 = EDGE_CURVE ( 'NONE', #219396, #144623, #45097, .T. ) ;
#145041 = ORIENTED_EDGE ( 'NONE', *, *, #182328, .F. ) ;
#145042 = ORIENTED_EDGE ( 'NONE', *, *, #18076, .F. ) ;
#145043 = CARTESIAN_POINT ( 'NONE',  ( -21.05000000000009663, 60.96458334440597326, -234.1404740665545319 ) ) ;
#145044 = VERTEX_POINT ( 'NONE', #23633 ) ;
#145045 = CARTESIAN_POINT ( 'NONE',  ( -16.85312841634288006, 23.17876450014587419, -231.0838577861638896 ) ) ;
#145046 = ORIENTED_EDGE ( 'NONE', *, *, #178012, .T. ) ;
#145048 = ORIENTED_EDGE ( 'NONE', *, *, #152912, .F. ) ;
#145047 = CARTESIAN_POINT ( 'NONE',  ( -18.39999999999999858, -9.399999999988850163, -55.25000000000004974 ) ) ;
#145049 = EDGE_CURVE ( 'NONE', #178909, #166239, #78403, .T. ) ;
#145050 = ADVANCED_FACE ( 'NONE', ( #245223 ), #44458, .F. ) ;
#145051 = CIRCLE ( 'NONE', #32687, 0.9000000000000014655 ) ;
#145052 = LINE ( 'NONE', #108500, #77667 ) ;
#145053 = ORIENTED_EDGE ( 'NONE', *, *, #74787, .F. ) ;
#145054 = DIRECTION ( 'NONE',  ( -1.000000000000000000, 0.000000000000000000, 0.000000000000000000 ) ) ;
#145055 = AXIS2_PLACEMENT_3D ( 'NONE', #176663, #234040, #253594 ) ;
#145056 = AXIS2_PLACEMENT_3D ( 'NONE', #180185, #122783, #161912 ) ;
#145057 = EDGE_LOOP ( 'NONE', ( #206551, #173687, #252590, #119214 ) ) ;
#145059 = EDGE_LOOP ( 'NONE', ( #178420, #180248, #151165, #111023 ) ) ;
#145058 = ORIENTED_EDGE ( 'NONE', *, *, #113141, .F. ) ;
#145060 = DIRECTION ( 'NONE',  ( 1.000000000000000000, 0.000000000000000000, 0.000000000000000000 ) ) ;
#145061 = AXIS2_PLACEMENT_3D ( 'NONE', #22080, #40386, #235963 ) ;
#145062 = DIRECTION ( 'NONE',  ( -0.000000000000000000, 1.000000000000000000, -0.000000000000000000 ) ) ;
#145063 = ORIENTED_EDGE ( 'NONE', *, *, #245442, .T. ) ;
#145064 = ORIENTED_EDGE ( 'NONE', *, *, #112888, .F. ) ;
#145065 = LINE ( 'NONE', #68112, #132803 ) ;
#145066 = CARTESIAN_POINT ( 'NONE',  ( 23.50000000000005684, 64.25000000001119815, -3.123107484524795474 ) ) ;
#145068 = ORIENTED_EDGE ( 'NONE', *, *, #43296, .F. ) ;
#145067 = DIRECTION ( 'NONE',  ( 0.000000000000000000, -6.938893903907222067E-15, 1.000000000000000000 ) ) ;
#145069 = DIRECTION ( 'NONE',  ( 0.000000000000000000, -0.9126074666063660468, -0.4088369013363524762 ) ) ;
#145070 = ORIENTED_EDGE ( 'NONE', *, *, #97835, .F. ) ;
#145071 = DIRECTION ( 'NONE',  ( -0.000000000000000000, -0.8660254037844459241, -0.4999999999999873990 ) ) ;
#145072 = DIRECTION ( 'NONE',  ( -1.000000000000000000, 0.000000000000000000, 0.000000000000000000 ) ) ;
#145073 = AXIS2_PLACEMENT_3D ( 'NONE', #156555, #178686, #199518 ) ;
#145074 = ORIENTED_EDGE ( 'NONE', *, *, #200150, .F. ) ;
#145075 = DIRECTION ( 'NONE',  ( 1.000000000000000000, 0.000000000000000000, 0.000000000000000000 ) ) ;
#145076 = DIRECTION ( 'NONE',  ( 0.000000000000000000, 0.000000000000000000, -1.000000000000000000 ) ) ;
#145077 = ORIENTED_EDGE ( 'NONE', *, *, #118208, .T. ) ;
#145078 = CARTESIAN_POINT ( 'NONE',  ( -18.59999999999999787, 11.75000000000000000, -21.25000000000000000 ) ) ;
#145079 = VERTEX_POINT ( 'NONE', #122719 ) ;
#145081 = ORIENTED_EDGE ( 'NONE', *, *, #185242, .F. ) ;
#145080 = VERTEX_POINT ( 'NONE', #161848 ) ;
#145082 = ORIENTED_EDGE ( 'NONE', *, *, #141677, .F. ) ;
#145083 = DIRECTION ( 'NONE',  ( 1.000000000000000000, 0.000000000000000000, -0.000000000000000000 ) ) ;
#145084 = ORIENTED_EDGE ( 'NONE', *, *, #624, .T. ) ;
#145085 = DIRECTION ( 'NONE',  ( 0.000000000000000000, -0.1350103645451807555, -0.9908441862701610203 ) ) ;
#145086 = ORIENTED_EDGE ( 'NONE', *, *, #251161, .T. ) ;
#145087 = DIRECTION ( 'NONE',  ( 0.000000000000000000, 1.000000000000000000, 2.891205793294679805E-16 ) ) ;
#145088 = LINE ( 'NONE', #201222, #231546 ) ;
#145089 = VERTEX_POINT ( 'NONE', #146103 ) ;
#145090 = EDGE_CURVE ( 'NONE', #1620, #2705, #4026, .T. ) ;
#145091 = EDGE_LOOP ( 'NONE', ( #75934, #91612, #251084, #125823, #166286, #171642 ) ) ;
#145092 = CIRCLE ( 'NONE', #228325, 0.1000000000000028644 ) ;
#145093 = CIRCLE ( 'NONE', #220126, 0.1000000000000028644 ) ;
#145094 = EDGE_CURVE ( 'NONE', #10423, #130825, #99242, .T. ) ;
#145095 = AXIS2_PLACEMENT_3D ( 'NONE', #100916, #98348, #60542 ) ;
#145096 = ORIENTED_EDGE ( 'NONE', *, *, #249532, .T. ) ;
#145097 = EDGE_CURVE ( 'NONE', #89128, #246033, #185239, .T. ) ;
#145098 = VECTOR ( 'NONE', #30405, 1000.000000000000000 ) ;
#145099 = CARTESIAN_POINT ( 'NONE',  ( -18.46902351632711614, 85.50947011869294556, -129.5366535502669478 ) ) ;
#145100 = EDGE_CURVE ( 'NONE', #73566, #152520, #236801, .T. ) ;
#145101 = ORIENTED_EDGE ( 'NONE', *, *, #10589, .T. ) ;
#145102 = CARTESIAN_POINT ( 'NONE',  ( 22.60000000000000142, 0.1008583691098682150, -122.2504328765106294 ) ) ;
#145104 = ORIENTED_EDGE ( 'NONE', *, *, #163052, .T. ) ;
#145103 = DIRECTION ( 'NONE',  ( -1.000000000000000000, 6.938893903907270030E-14, -2.775557561562908012E-13 ) ) ;
#145105 = CARTESIAN_POINT ( 'NONE',  ( 18.59999999999999076, 19.05165861791954285, -232.6888762659126826 ) ) ;
#145106 = DIRECTION ( 'NONE',  ( 0.000000000000000000, -1.000000000000000000, 0.000000000000000000 ) ) ;
#145109 = CARTESIAN_POINT ( 'NONE',  ( 21.07928932188134397, 33.98134083355422774, -243.8161431329846494 ) ) ;
#145108 = CIRCLE ( 'NONE', #144930, 0.5000000000000007772 ) ;
#145107 = DIRECTION ( 'NONE',  ( -0.000000000000000000, 1.000000000000000000, -0.000000000000000000 ) ) ;
#145110 = DIRECTION ( 'NONE',  ( 0.000000000000000000, 0.8814952561688428334, -0.4721928772777350125 ) ) ;
#145111 = FACE_OUTER_BOUND ( 'NONE', #27695, .T. ) ;
#145112 = AXIS2_PLACEMENT_3D ( 'NONE', #8043, #189244, #105818 ) ;
#145113 = DIRECTION ( 'NONE',  ( 0.000000000000000000, -6.982962677686266711E-15, 1.000000000000000000 ) ) ;
#145114 = DIRECTION ( 'NONE',  ( 0.000000000000000000, 0.4930308989875313852, 0.8700118002898274971 ) ) ;
#145115 = ORIENTED_EDGE ( 'NONE', *, *, #249926, .F. ) ;
#145116 = AXIS2_PLACEMENT_3D ( 'NONE', #156073, #116912, #75247 ) ;
#145117 = EDGE_CURVE ( 'NONE', #52116, #127854, #104387, .T. ) ;
#145119 = ORIENTED_EDGE ( 'NONE', *, *, #190146, .T. ) ;
#145118 = DIRECTION ( 'NONE',  ( 0.000000000000000000, -0.4999999999999608646, 0.8660254037844612451 ) ) ;
#145120 = ORIENTED_EDGE ( 'NONE', *, *, #164728, .F. ) ;
#145121 = LINE ( 'NONE', #240394, #199239 ) ;
#145122 = CARTESIAN_POINT ( 'NONE',  ( 20.97217846901851956, 8.875441724720829484, -142.5012276839372305 ) ) ;
#145123 = DIRECTION ( 'NONE',  ( 1.000000000000000000, 0.000000000000000000, 1.073024830501117725E-15 ) ) ;
#145124 = ORIENTED_EDGE ( 'NONE', *, *, #195117, .F. ) ;
#145125 = ADVANCED_FACE ( 'NONE', ( #163125 ), #84814, .T. ) ;
#145126 = FACE_OUTER_BOUND ( 'NONE', #226503, .T. ) ;
#145127 = AXIS2_PLACEMENT_3D ( 'NONE', #209320, #32002, #167661 ) ;
#145128 = EDGE_CURVE ( 'NONE', #47140, #223175, #46986, .T. ) ;
#145129 = DIRECTION ( 'NONE',  ( -1.000000000000000000, -0.000000000000000000, -0.000000000000000000 ) ) ;
#145130 = EDGE_LOOP ( 'NONE', ( #46171, #132330, #137006, #215539 ) ) ;
#145131 = VECTOR ( 'NONE', #147337, 1000.000000000000000 ) ;
#145132 = VECTOR ( 'NONE', #4761, 1000.000000000000000 ) ;
#145133 = CARTESIAN_POINT ( 'NONE',  ( 21.05000000000000071, 4.850467289730772791, -179.5342674090016430 ) ) ;
#145134 = SPHERICAL_SURFACE ( 'NONE', #83858, 0.1000000000000000056 ) ;
#145135 = B_SPLINE_CURVE_WITH_KNOTS ( 'NONE', 3,
 ( #91784, #112636, #13539, #254663, #218125, #96874, #34404, #116487, #137312, #94335 ),
 .UNSPECIFIED., .F., .F.,
 ( 4, 3, 3, 4 ),
 ( 0.000000000000000000, 0.0002000000000008537104, 0.001000000000082977483, 0.001967863649483339323 ),
 .UNSPECIFIED. ) ;
#145136 = FACE_OUTER_BOUND ( 'NONE', #125873, .T. ) ;
#145138 = VERTEX_POINT ( 'NONE', #183952 ) ;
#145137 = CARTESIAN_POINT ( 'NONE',  ( -18.59999999999999787, 35.94660524813657076, -234.4748257877825495 ) ) ;
#145139 = VECTOR ( 'NONE', #230923, 1000.000000000000000 ) ;
#145140 = CARTESIAN_POINT ( 'NONE',  ( 23.25000000000000000, -11.64999999998883595, -97.40000000000004832 ) ) ;
#145141 = ADVANCED_FACE ( 'NONE', ( #45725 ), #106970, .F. ) ;
#145142 = DIRECTION ( 'NONE',  ( 0.000000000000000000, 0.1084263158146956119, 0.9941044884914522761 ) ) ;
#145143 = LINE ( 'NONE', #43503, #162426 ) ;
#145144 = ORIENTED_EDGE ( 'NONE', *, *, #160036, .T. ) ;
#145145 = CARTESIAN_POINT ( 'NONE',  ( -16.94309007106720699, 66.00777380744230527, -157.4173162019689016 ) ) ;
#145146 = EDGE_CURVE ( 'NONE', #169815, #171633, #99430, .T. ) ;
#145147 = CARTESIAN_POINT ( 'NONE',  ( -18.40000000000000213, 13.89349365668996228, -210.8782859590407668 ) ) ;
#145149 = FACE_OUTER_BOUND ( 'NONE', #234873, .T. ) ;
#145148 = FACE_OUTER_BOUND ( 'NONE', #155154, .T. ) ;
#145150 = CARTESIAN_POINT ( 'NONE',  ( -20.64999999999999858, 4.250000000011156409, -146.2500000000000284 ) ) ;
#145151 = CARTESIAN_POINT ( 'NONE',  ( -16.87683809663752399, 9.850000000011139178, -53.59763598180368405 ) ) ;
#145153 = ADVANCED_FACE ( 'NONE', ( #207386 ), #151263, .F. ) ;
#145152 = CARTESIAN_POINT ( 'NONE',  ( -18.54148534481894472, 10.32532329026770590, -39.06993430183596416 ) ) ;
#145154 = CARTESIAN_POINT ( 'NONE',  ( -21.44999999999999929, 7.250000000011155521, -79.35000000000005116 ) ) ;
#145155 = LINE ( 'NONE', #224696, #4888 ) ;
#145156 = CARTESIAN_POINT ( 'NONE',  ( -16.77779411440718604, 9.946101447118758543, -87.83694258299551905 ) ) ;
#145157 = AXIS2_PLACEMENT_3D ( 'NONE', #142128, #202112, #243799 ) ;
#145158 = EDGE_LOOP ( 'NONE', ( #37127, #62844, #114052 ) ) ;
#145159 = LINE ( 'NONE', #164748, #168196 ) ;
#145160 = VECTOR ( 'NONE', #35294, 1000.000000000000000 ) ;
#145161 = VERTEX_POINT ( 'NONE', #149991 ) ;
#145162 = VERTEX_POINT ( 'NONE', #131682 ) ;
#145163 = DIRECTION ( 'NONE',  ( 0.000000000000000000, 0.000000000000000000, -1.000000000000000000 ) ) ;
#145164 = CARTESIAN_POINT ( 'NONE',  ( -23.15000000000000213, 70.12557831835937350, -215.6322690948981915 ) ) ;
#145165 = ORIENTED_EDGE ( 'NONE', *, *, #214462, .F. ) ;
#145166 = ADVANCED_FACE ( 'NONE', ( #168291 ), #13047, .F. ) ;
#145167 = AXIS2_PLACEMENT_3D ( 'NONE', #216442, #153964, #36571 ) ;
#145168 = ORIENTED_EDGE ( 'NONE', *, *, #220097, .T. ) ;
#145169 = EDGE_CURVE ( 'NONE', #8100, #49507, #257597, .T. ) ;
#145170 = SURFACE_STYLE_USAGE ( .BOTH. , #245583 ) ;
#145171 = VECTOR ( 'NONE', #124134, 1000.000000000000000 ) ;
#145172 = EDGE_LOOP ( 'NONE', ( #197374, #208576, #1831, #111643, #5753 ) ) ;
#145173 = LINE ( 'NONE', #6959, #12639 ) ;
#145174 = VERTEX_POINT ( 'NONE', #28783 ) ;
#145176 = DIRECTION ( 'NONE',  ( -1.000000000000000000, 0.000000000000000000, 0.000000000000000000 ) ) ;
#145175 = AXIS2_PLACEMENT_3D ( 'NONE', #182703, #67866, #144825 ) ;
#145177 = CARTESIAN_POINT ( 'NONE',  ( -22.50000000000000000, 1.115600667400684642E-11, -127.7500000000000284 ) ) ;
#145178 = LINE ( 'NONE', #46083, #242670 ) ;
#145179 = VECTOR ( 'NONE', #18567, 1000.000000000000000 ) ;
#145180 = CIRCLE ( 'NONE', #145366, 4.050000000000000711 ) ;
#145181 = CARTESIAN_POINT ( 'NONE',  ( -20.94999999999999929, 77.83534155023700407, -191.9679561919613491 ) ) ;
#145182 = DIRECTION ( 'NONE',  ( 1.000000000000000000, 0.000000000000000000, 0.000000000000000000 ) ) ;
#145183 = AXIS2_PLACEMENT_3D ( 'NONE', #44012, #103959, #166558 ) ;
#145184 = CYLINDRICAL_SURFACE ( 'NONE', #62548, 0.1000000000000013933 ) ;
#145185 = DIRECTION ( 'NONE',  ( 1.000000000000000000, 0.000000000000000000, 0.000000000000000000 ) ) ;
#145187 = ORIENTED_EDGE ( 'NONE', *, *, #176456, .F. ) ;
#145186 = CARTESIAN_POINT ( 'NONE',  ( 21.13461538461538680, 44.20567951878638269, -236.4340127271084384 ) ) ;
#145189 = DIRECTION ( 'NONE',  ( 0.000000000000000000, 0.000000000000000000, -1.000000000000000000 ) ) ;
#145188 = DIRECTION ( 'NONE',  ( 0.000000000000000000, -0.2617529984165031243, -0.9651348961777157509 ) ) ;
#145190 = VECTOR ( 'NONE', #214388, 1000.000000000000000 ) ;
#145191 = CARTESIAN_POINT ( 'NONE',  ( -18.50000000000000000, 9.250000000011157297, -54.65000000000000568 ) ) ;
#145192 = VERTEX_POINT ( 'NONE', #9170 ) ;
#145193 = CARTESIAN_POINT ( 'NONE',  ( 16.87683809663749557, 9.950000000011131718, -87.85000000000005116 ) ) ;
#145194 = DIRECTION ( 'NONE',  ( -1.000000000000000000, -3.265361837132813093E-16, 0.000000000000000000 ) ) ;
#145195 = LINE ( 'NONE', #3107, #75028 ) ;
#145196 = ORIENTED_EDGE ( 'NONE', *, *, #150887, .F. ) ;
#145198 = DIRECTION ( 'NONE',  ( -0.000000000000000000, 1.000000000000000000, 2.891205793294679805E-16 ) ) ;
#145197 = CARTESIAN_POINT ( 'NONE',  ( -20.64999999999999858, 26.13474583767463244, -241.1910018098189141 ) ) ;
#145199 = CARTESIAN_POINT ( 'NONE',  ( -16.79270642812295833, 66.05375578307362616, -82.18417420596148304 ) ) ;
#145200 = AXIS2_PLACEMENT_3D ( 'NONE', #39900, #64560, #84074 ) ;
#145202 = ORIENTED_EDGE ( 'NONE', *, *, #4267, .T. ) ;
#145201 = VECTOR ( 'NONE', #208757, 1000.000000000000227 ) ;
#145203 = CARTESIAN_POINT ( 'NONE',  ( 21.05000000000000071, 6.441084688482579423, -67.01771943330844294 ) ) ;
#145204 = AXIS2_PLACEMENT_3D ( 'NONE', #50681, #71584, #46839 ) ;
#145205 = DIRECTION ( 'NONE',  ( -0.000000000000000000, 0.000000000000000000, -1.000000000000000000 ) ) ;
#145206 = CYLINDRICAL_SURFACE ( 'NONE', #224023, 3.999999999999996447 ) ;
#145207 = DIRECTION ( 'NONE',  ( 0.000000000000000000, 1.000000000000000000, 6.938893903907222067E-15 ) ) ;
#145208 = ORIENTED_EDGE ( 'NONE', *, *, #65276, .F. ) ;
#145209 = ORIENTED_EDGE ( 'NONE', *, *, #228380, .T. ) ;
#145210 = VECTOR ( 'NONE', #119224, 1000.000000000000000 ) ;
#145211 = VECTOR ( 'NONE', #175865, 1000.000000000000000 ) ;
#145212 = FACE_OUTER_BOUND ( 'NONE', #112994, .T. ) ;
#145213 = FACE_OUTER_BOUND ( 'NONE', #12712, .T. ) ;
#145214 = FACE_OUTER_BOUND ( 'NONE', #8260, .T. ) ;
#145215 = DIRECTION ( 'NONE',  ( 0.000000000000000000, 0.000000000000000000, -1.000000000000000000 ) ) ;
#145216 = EDGE_CURVE ( 'NONE', #40198, #105588, #157771, .T. ) ;
#145217 = AXIS2_PLACEMENT_3D ( 'NONE', #241180, #179924, #63814 ) ;
#145218 = CARTESIAN_POINT ( 'NONE',  ( -20.54999999999999716, 7.250000000011155521, -54.75000000000000000 ) ) ;
#145219 = CARTESIAN_POINT ( 'NONE',  ( -20.54999999999999716, 7.128833340093095217, -233.7327013124392749 ) ) ;
#145220 = EDGE_LOOP ( 'NONE', ( #186425, #95587, #13145, #29564 ) ) ;
#145221 = DIRECTION ( 'NONE',  ( 0.000000000000000000, -0.8814952561688425003, 0.4721928772777354011 ) ) ;
#145222 = VECTOR ( 'NONE', #250347, 1000.000000000000000 ) ;
#145223 = ORIENTED_EDGE ( 'NONE', *, *, #190396, .F. ) ;
#145224 = FACE_OUTER_BOUND ( 'NONE', #120423, .T. ) ;
#145225 = CARTESIAN_POINT ( 'NONE',  ( -21.05000000000000071, 5.850000000011105428, -77.13249722427802624 ) ) ;
#145226 = CARTESIAN_POINT ( 'NONE',  ( -21.07971444708686093, 75.91217656369386191, -75.85289956615088158 ) ) ;
#145227 = EDGE_CURVE ( 'NONE', #107953, #55352, #130388, .T. ) ;
#145228 = CARTESIAN_POINT ( 'NONE',  ( -23.25000000000000000, 76.10085836911093793, -148.2726746080136877 ) ) ;
#145230 = VERTEX_POINT ( 'NONE', #109535 ) ;
#145229 = LINE ( 'NONE', #206501, #231668 ) ;
#145231 = CARTESIAN_POINT ( 'NONE',  ( 21.05000000000000071, 1.627786319807486892, -244.0021210468063089 ) ) ;
#145232 = CARTESIAN_POINT ( 'NONE',  ( 21.13507111622890022, 10.71768338700954537, -179.7491685863607529 ) ) ;
#145233 = CARTESIAN_POINT ( 'NONE',  ( -17.11825945287481332, 62.98921886345647181, -213.1014462870871284 ) ) ;
#145234 = DIRECTION ( 'NONE',  ( -0.000000000000000000, 0.9651348961777159730, -0.2617529984165026247 ) ) ;
#145235 = EDGE_LOOP ( 'NONE', ( #161649, #190606, #89866, #198592 ) ) ;
#145236 = CYLINDRICAL_SURFACE ( 'NONE', #231756, 0.1000000000000028644 ) ;
#145237 = EDGE_CURVE ( 'NONE', #172386, #131148, #148696, .T. ) ;
#145239 = EDGE_CURVE ( 'NONE', #205311, #23903, #228227, .T. ) ;
#145238 = VECTOR ( 'NONE', #224738, 1000.000000000000227 ) ;
#145240 = VECTOR ( 'NONE', #174140, 1000.000000000000000 ) ;
#145241 = CYLINDRICAL_SURFACE ( 'NONE', #187773, 0.1000000000000028644 ) ;
#145242 = CIRCLE ( 'NONE', #137061, 0.5000000000000007772 ) ;
#145243 = DIRECTION ( 'NONE',  ( -7.304098846218134667E-16, 1.000000000000000000, -0.000000000000000000 ) ) ;
#145244 = ORIENTED_EDGE ( 'NONE', *, *, #136896, .T. ) ;
#145245 = CARTESIAN_POINT ( 'NONE',  ( -16.80891096016337727, 9.950000000011137047, -87.86766280726713774 ) ) ;
#145246 = ORIENTED_EDGE ( 'NONE', *, *, #42462, .F. ) ;
#145247 = CARTESIAN_POINT ( 'NONE',  ( 21.07928932188134397, 61.09751618602743406, -234.2940654522722639 ) ) ;
#145248 = DIRECTION ( 'NONE',  ( -0.000000000000000000, 0.4721928772777345684, 0.8814952561688429444 ) ) ;
#145249 = ADVANCED_FACE ( 'NONE', ( #92542 ), #229510, .F. ) ;
#145250 = FACE_OUTER_BOUND ( 'NONE', #15810, .T. ) ;
#145251 = CARTESIAN_POINT ( 'NONE',  ( -23.15000000000000213, -9.499999999988848032, -177.3939691226524360 ) ) ;
#145252 = EDGE_LOOP ( 'NONE', ( #133623, #44842, #5525, #149884 ) ) ;
#145253 = AXIS2_PLACEMENT_3D ( 'NONE', #7389, #25686, #124790 ) ;
#145254 = DIRECTION ( 'NONE',  ( 0.000000000000000000, 1.000000000000000000, 0.000000000000000000 ) ) ;
#145255 = LINE ( 'NONE', #27926, #99832 ) ;
#145256 = CARTESIAN_POINT ( 'NONE',  ( 22.60000000000000142, 0.1008583690987122083, 11.74956712348939192 ) ) ;
#145257 = DIRECTION ( 'NONE',  ( 1.000000000000000000, 0.000000000000000000, 0.000000000000000000 ) ) ;
#145258 = DIRECTION ( 'NONE',  ( 0.000000000000000000, 1.000000000000000000, 0.000000000000000000 ) ) ;
#145259 = ORIENTED_EDGE ( 'NONE', *, *, #81788, .T. ) ;
#145261 = VERTEX_POINT ( 'NONE', #108280 ) ;
#145260 = CARTESIAN_POINT ( 'NONE',  ( -21.53752568617683849, 6.786807874514948935, -167.4010255387155439 ) ) ;
#145262 = ORIENTED_EDGE ( 'NONE', *, *, #100240, .F. ) ;
#145263 = DIRECTION ( 'NONE',  ( 0.000000000000000000, -1.000000000000000000, -7.813886390323680189E-15 ) ) ;
#145264 = EDGE_LOOP ( 'NONE', ( #19792, #194609, #4922, #145566, #50800, #229080, #168181, #98476, #172952 ) ) ;
#145265 = EDGE_CURVE ( 'NONE', #91601, #96601, #211891, .T. ) ;
#145266 = CARTESIAN_POINT ( 'NONE',  ( 21.05000000000001492, 61.01939706577768163, -234.1520516327897496 ) ) ;
#145267 = DIRECTION ( 'NONE',  ( 0.000000000000000000, -0.8814952561688430555, 0.4721928772777346239 ) ) ;
#145268 = EDGE_CURVE ( 'NONE', #36755, #172698, #129371, .T. ) ;
#145269 = CARTESIAN_POINT ( 'NONE',  ( 20.94999999999999929, 84.73084112150711178, -79.12118220350858167 ) ) ;
#145270 = ORIENTED_EDGE ( 'NONE', *, *, #195148, .T. ) ;
#145271 = DIRECTION ( 'NONE',  ( 1.000000000000000000, -0.000000000000000000, -0.000000000000000000 ) ) ;
#145272 = CARTESIAN_POINT ( 'NONE',  ( 20.99999999999997868, 1.115600667400684642E-11, -134.0000000000000000 ) ) ;
#145273 = FACE_OUTER_BOUND ( 'NONE', #40358, .T. ) ;
#145274 = ORIENTED_EDGE ( 'NONE', *, *, #242915, .F. ) ;
#145275 = CARTESIAN_POINT ( 'NONE',  ( -16.86379686415369150, 9.975217759264314310, -54.43338988909027876 ) ) ;
#145277 = VERTEX_POINT ( 'NONE', #49581 ) ;
#145276 = DIRECTION ( 'NONE',  ( 0.000000000000000000, 0.000000000000000000, -1.000000000000000000 ) ) ;
#145278 = DIRECTION ( 'NONE',  ( -0.000000000000000000, -1.000000000000000000, -0.000000000000000000 ) ) ;
#145280 = EDGE_CURVE ( 'NONE', #39117, #153564, #232575, .T. ) ;
#145279 = DIRECTION ( 'NONE',  ( 1.000000000000000000, 0.000000000000000000, 0.000000000000000000 ) ) ;
#145281 = VECTOR ( 'NONE', #48092, 1000.000000000000000 ) ;
#145282 = CIRCLE ( 'NONE', #199483, 0.09999999999998898659 ) ;
#145283 = VECTOR ( 'NONE', #209055, 1000.000000000000000 ) ;
#145284 = AXIS2_PLACEMENT_3D ( 'NONE', #36111, #94778, #58201 ) ;
#145285 = ORIENTED_EDGE ( 'NONE', *, *, #96218, .F. ) ;
#145286 = DIRECTION ( 'NONE',  ( -1.000000000000000000, 0.000000000000000000, 0.000000000000000000 ) ) ;
#145287 = CARTESIAN_POINT ( 'NONE',  ( -18.38817693311004575, 11.48149151589976924, -24.25000000000000000 ) ) ;
#145288 = TOROIDAL_SURFACE ( 'NONE', #12048, 0.2000000000000000111, 0.1000000000000000056 ) ;
#145289 = LINE ( 'NONE', #167467, #251709 ) ;
#145290 = ORIENTED_EDGE ( 'NONE', *, *, #214153, .F. ) ;
#145291 = FACE_OUTER_BOUND ( 'NONE', #135158, .T. ) ;
#145292 = DIRECTION ( 'NONE',  ( 0.000000000000000000, -1.000000000000000000, 0.000000000000000000 ) ) ;
#145293 = EDGE_LOOP ( 'NONE', ( #149916, #55867, #226041, #180967 ) ) ;
#145294 = CIRCLE ( 'NONE', #236884, 6.329289321881370611 ) ;
#145295 = VECTOR ( 'NONE', #195853, 1000.000000000000000 ) ;
#145296 = VECTOR ( 'NONE', #149821, 1000.000000000000000 ) ;
#145297 = AXIS2_PLACEMENT_3D ( 'NONE', #214409, #80008, #16248 ) ;
#145298 = ORIENTED_EDGE ( 'NONE', *, *, #223987, .T. ) ;
#145299 = CARTESIAN_POINT ( 'NONE',  ( 21.09551895715278391, 65.37856267284456635, -191.2859828186247171 ) ) ;
#145300 = EDGE_CURVE ( 'NONE', #32779, #250321, #226930, .T. ) ;
#145301 = EDGE_CURVE ( 'NONE', #216206, #19709, #169575, .T. ) ;
#145302 = ORIENTED_EDGE ( 'NONE', *, *, #134336, .T. ) ;
#145303 = DIRECTION ( 'NONE',  ( -1.000000000000000000, -0.000000000000000000, -0.000000000000000000 ) ) ;
#145304 = CARTESIAN_POINT ( 'NONE',  ( -16.88705144915432044, 66.05000000001257376, -182.9540860792355375 ) ) ;
#145307 = EDGE_LOOP ( 'NONE', ( #103374, #64622, #57997, #63299 ) ) ;
#145306 = LINE ( 'NONE', #103599, #91889 ) ;
#145305 =( BOUNDED_SURFACE ( )  B_SPLINE_SURFACE ( 3, 2, ( 
 ( #237232, #58568, #59845 ),
 ( #39047, #118584, #165401 ),
 ( #45445, #124992, #244924 ),
 ( #141969, #84519, #204505 ),
 ( #65000, #83256, #2451 ),
 ( #123709, #201960, #67573 ),
 ( #164120, #6303, #246218 ),
 ( #222779, #3749, #44176 ),
 ( #241101, #24631, #226634 ),
 ( #23348, #144528, #104109 ) ),
 .UNSPECIFIED., .F., .F., .F. ) 
 B_SPLINE_SURFACE_WITH_KNOTS ( ( 4, 2, 2, 2, 4 ),
 ( 3, 3 ),
 ( 0.002161241639767248670, 0.002579950749615824400, 0.002789305304540112482, 0.002893982582002256523, 0.002998659859464400564 ),
 ( 0.000000000000000000, 1.000000000000000000 ),
 .UNSPECIFIED. ) 
 GEOMETRIC_REPRESENTATION_ITEM ( )  RATIONAL_B_SPLINE_SURFACE ( (
 ( 1.000000000000000000, 0.7071067811865475727, 1.000000000000000000),
 ( 1.000000000000000000, 0.7632447400665651749, 1.000000000000000000),
 ( 1.000000000000000000, 0.8158073005108548159, 1.000000000000000000),
 ( 1.000000000000000000, 0.8906973462396701180, 1.000000000000000000),
 ( 1.000000000000000000, 0.9149408947804169578, 1.000000000000000000),
 ( 1.000000000000000000, 0.9493368785273816890, 1.000000000000000000),
 ( 1.000000000000000000, 0.9605194247156174647, 1.000000000000000000),
 ( 1.000000000000000000, 0.9803630264781744152, 1.000000000000000000),
 ( 1.000000000000000000, 0.9900844824270682576, 1.000000000000000000),
 ( 1.000000000000000000, 0.9894588281429290699, 1.000000000000000000) ) ) 
 REPRESENTATION_ITEM ( '' )  SURFACE ( )  );
#145308 = CARTESIAN_POINT ( 'NONE',  ( 20.94999999999999929, 11.65000000001115943, -127.2161343370219413 ) ) ;
#145309 = CARTESIAN_POINT ( 'NONE',  ( 23.14999999999999858, 68.86662215840367196, -239.5055563729039534 ) ) ;
#145311 = EDGE_CURVE ( 'NONE', #182294, #240102, #132586, .T. ) ;
#145310 = DIRECTION ( 'NONE',  ( 0.000000000000000000, -0.8490545835447254053, -0.5283051335749948674 ) ) ;
#145313 = EDGE_CURVE ( 'NONE', #195865, #24375, #91078, .T. ) ;
#145312 = CARTESIAN_POINT ( 'NONE',  ( 23.15000000000000213, 87.65000000001144542, -39.12310748452424747 ) ) ;
#145314 = DIRECTION ( 'NONE',  ( 0.000000000000000000, -1.000000000000000000, -6.982962677686265922E-15 ) ) ;
#145315 = DIRECTION ( 'NONE',  ( -1.000000000000000000, -0.000000000000000000, -0.000000000000000000 ) ) ;
#145316 = CYLINDRICAL_SURFACE ( 'NONE', #105482, 1.749999999999998002 ) ;
#145317 = CARTESIAN_POINT ( 'NONE',  ( -18.50000000000001066, -9.421308209727826011, -107.7423632140509397 ) ) ;
#145319 = ORIENTED_EDGE ( 'NONE', *, *, #127914, .F. ) ;
#145318 = LINE ( 'NONE', #103610, #36060 ) ;
#145320 = CARTESIAN_POINT ( 'NONE',  ( -20.54999999999999716, 1.115600667400684642E-11, -100.5000000000000284 ) ) ;
#145322 = ORIENTED_EDGE ( 'NONE', *, *, #220077, .F. ) ;
#145321 = ADVANCED_FACE ( 'NONE', ( #98600 ), #81608, .F. ) ;
#145323 = CARTESIAN_POINT ( 'NONE',  ( 20.85000000000000142, 69.06610602788505560, -32.23746165015079868 ) ) ;
#145324 = AXIS2_PLACEMENT_3D ( 'NONE', #58484, #221406, #218849 ) ;
#145325 = AXIS2_PLACEMENT_3D ( 'NONE', #20888, #99080, #11559 ) ;
#145326 = ADVANCED_FACE ( 'NONE', ( #59480 ), #240917, .F. ) ;
#145328 = EDGE_CURVE ( 'NONE', #21828, #211757, #153478, .T. ) ;
#145327 = ADVANCED_FACE ( 'NONE', ( #197741 ), #7705, .T. ) ;
#145329 = LINE ( 'NONE', #140182, #250854 ) ;
#145330 = CARTESIAN_POINT ( 'NONE',  ( -22.50000000000000000, 76.00000000001237765, -170.0231074845243597 ) ) ;
#145331 = AXIS2_PLACEMENT_3D ( 'NONE', #11082, #213124, #191025 ) ;
#145332 = EDGE_CURVE ( 'NONE', #26497, #92572, #72, .T. ) ;
#145333 = CARTESIAN_POINT ( 'NONE',  ( 20.96937028524355284, 65.37553062838595963, -196.0316813833548508 ) ) ;
#145334 = ORIENTED_EDGE ( 'NONE', *, *, #103832, .T. ) ;
#145335 = DIRECTION ( 'NONE',  ( -0.000000000000000000, 6.982962677686266711E-15, -1.000000000000000000 ) ) ;
#145336 = EDGE_CURVE ( 'NONE', #207643, #25751, #11986, .T. ) ;
#145337 = CARTESIAN_POINT ( 'NONE',  ( -21.05000000000000071, 77.16270174995010223, -128.4231074845242802 ) ) ;
#145338 = VECTOR ( 'NONE', #175384, 1000.000000000000000 ) ;
#145339 = ORIENTED_EDGE ( 'NONE', *, *, #34064, .T. ) ;
#145340 = EDGE_CURVE ( 'NONE', #154967, #49762, #66125, .T. ) ;
#145341 = EDGE_CURVE ( 'NONE', #132362, #234056, #128487, .T. ) ;
#145342 = CIRCLE ( 'NONE', #3894, 0.09999999999999939493 ) ;
#145343 = DIRECTION ( 'NONE',  ( -1.000000000000000000, 0.000000000000000000, 0.000000000000000000 ) ) ;
#145344 = AXIS2_PLACEMENT_3D ( 'NONE', #162286, #113196, #14118 ) ;
#145345 = CARTESIAN_POINT ( 'NONE',  ( -21.14999999999994174, 78.11805852053666399, -49.62915779269638961 ) ) ;
#145346 = ADVANCED_FACE ( 'NONE', ( #2095 ), #77779, .F. ) ;
#145347 = VERTEX_POINT ( 'NONE', #222407 ) ;
#145348 = DIRECTION ( 'NONE',  ( 1.000000000000000000, 0.000000000000000000, 0.000000000000000000 ) ) ;
#145349 = EDGE_LOOP ( 'NONE', ( #156637, #3963, #71264, #73086 ) ) ;
#145350 = DIRECTION ( 'NONE',  ( 0.000000000000000000, -0.9915357197604982575, 0.1298341882519033486 ) ) ;
#145351 = EDGE_LOOP ( 'NONE', ( #103896, #255103, #53553, #256673 ) ) ;
#145352 = EDGE_CURVE ( 'NONE', #17436, #43703, #136864, .T. ) ;
#145353 = VECTOR ( 'NONE', #79733, 1000.000000000000000 ) ;
#145354 = AXIS2_PLACEMENT_3D ( 'NONE', #231881, #53220, #234410 ) ;
#145355 = CARTESIAN_POINT ( 'NONE',  ( 21.05000000000000071, 85.00000000001188027, -93.12913836187181005 ) ) ;
#145356 = FACE_OUTER_BOUND ( 'NONE', #212553, .T. ) ;
#145358 = VERTEX_POINT ( 'NONE', #183322 ) ;
#145357 = EDGE_CURVE ( 'NONE', #126709, #110634, #245014, .T. ) ;
#145359 = CARTESIAN_POINT ( 'NONE',  ( 21.14999999999999858, 0.09779029131994770863, -161.2421853895238542 ) ) ;
#145361 = VERTEX_POINT ( 'NONE', #224982 ) ;
#145360 = CARTESIAN_POINT ( 'NONE',  ( 22.39999999999999858, 68.20922040163827660, -69.62310748452438247 ) ) ;
#145362 = CARTESIAN_POINT ( 'NONE',  ( 18.49999999999999289, 51.96945017402672562, -231.5060697639786440 ) ) ;
#145363 = ORIENTED_EDGE ( 'NONE', *, *, #69637, .T. ) ;
#145364 = VECTOR ( 'NONE', #214768, 999.9999999999998863 ) ;
#145365 = CIRCLE ( 'NONE', #70404, 0.09999999999999516220 ) ;
#145366 = AXIS2_PLACEMENT_3D ( 'NONE', #194257, #57255, #212529 ) ;
#145367 = VECTOR ( 'NONE', #113387, 1000.000000000000000 ) ;
#145368 = ORIENTED_EDGE ( 'NONE', *, *, #219105, .F. ) ;
#145369 = ADVANCED_FACE ( 'NONE', ( #29416 ), #170235, .F. ) ;
#145371 = CIRCLE ( 'NONE', #187099, 6.329289321881355512 ) ;
#145370 = DIRECTION ( 'NONE',  ( 0.000000000000000000, 0.9446535261619708468, -0.3280696808755038663 ) ) ;
#145372 = CARTESIAN_POINT ( 'NONE',  ( -18.40000000000000213, 5.650000000011139001, -113.1500000000000341 ) ) ;
#145373 = DIRECTION ( 'NONE',  ( 0.000000000000000000, -6.530723674265620862E-15, 1.000000000000000000 ) ) ;
#145374 = DIRECTION ( 'NONE',  ( 1.734723475976817507E-14, 0.000000000000000000, -1.000000000000000000 ) ) ;
#145375 = CARTESIAN_POINT ( 'NONE',  ( -14.45443560709638042, 66.54940788787891393, -188.4669191657160923 ) ) ;
#145376 = SPHERICAL_SURFACE ( 'NONE', #29623, 0.1000000000000000056 ) ;
#145377 = VERTEX_POINT ( 'NONE', #45090 ) ;
#145378 = CARTESIAN_POINT ( 'NONE',  ( 21.05000000000000071, 8.776282895303632259, -33.50000000000000000 ) ) ;
#145379 = SPHERICAL_SURFACE ( 'NONE', #44389, 0.1000000000000000056 ) ;
#145380 = CARTESIAN_POINT ( 'NONE',  ( 20.95443524775735611, 67.12144573613926468, -127.9893852089242188 ) ) ;
#145381 = CARTESIAN_POINT ( 'NONE',  ( -20.54999999999999716, 2.000000000011154189, -87.27537807723794572 ) ) ;
#145382 = VERTEX_POINT ( 'NONE', #209293 ) ;
#145383 = CARTESIAN_POINT ( 'NONE',  ( 20.99999999999999645, 44.21724908628621620, -235.4814530999287285 ) ) ;
#145384 = VERTEX_POINT ( 'NONE', #65940 ) ;
#145386 = COLOUR_RGB ( '', 0.08235294, 0.09019608, 0.10196078) ;
#145385 = DIRECTION ( 'NONE',  ( 0.000000000000000000, 0.000000000000000000, -1.000000000000000000 ) ) ;
#145387 = ORIENTED_EDGE ( 'NONE', *, *, #128845, .T. ) ;
#145388 = DIRECTION ( 'NONE',  ( 0.000000000000000000, 0.000000000000000000, 1.000000000000000000 ) ) ;
#145389 = CYLINDRICAL_SURFACE ( 'NONE', #2029, 0.09999999999999939493 ) ;
#145390 = ORIENTED_EDGE ( 'NONE', *, *, #19918, .F. ) ;
#145391 = ORIENTED_EDGE ( 'NONE', *, *, #113583, .T. ) ;
#145393 = ORIENTED_EDGE ( 'NONE', *, *, #93236, .F. ) ;
#145392 = LINE ( 'NONE', #85387, #7256 ) ;
#145394 = CARTESIAN_POINT ( 'NONE',  ( -18.40000000000000213, 64.51332499825421962, -93.77310748452438816 ) ) ;
#145395 = ORIENTED_EDGE ( 'NONE', *, *, #22910, .T. ) ;
#145396 = DIRECTION ( 'NONE',  ( -1.000000000000000000, 1.207181226542539700E-16, -2.694675058168174199E-16 ) ) ;
#145397 = CIRCLE ( 'NONE', #207795, 0.1000000000000008799 ) ;
#145398 = DIRECTION ( 'NONE',  ( 1.000000000000000000, 0.000000000000000000, 0.000000000000000000 ) ) ;
#145399 = ORIENTED_EDGE ( 'NONE', *, *, #39818, .F. ) ;
#145400 = ADVANCED_FACE ( 'NONE', ( #208036 ), #182671, .T. ) ;
#145401 = FACE_OUTER_BOUND ( 'NONE', #209894, .T. ) ;
#145402 = VECTOR ( 'NONE', #170668, 1000.000000000000000 ) ;
#145403 = CARTESIAN_POINT ( 'NONE',  ( 21.14999999999999858, -1.391858308744748696, -194.6091531227727955 ) ) ;
#145404 = EDGE_CURVE ( 'NONE', #160723, #194844, #32852, .T. ) ;
#145405 = ORIENTED_EDGE ( 'NONE', *, *, #194513, .F. ) ;
#145406 = CIRCLE ( 'NONE', #216143, 0.09999999999999939493 ) ;
#145407 = CARTESIAN_POINT ( 'NONE',  ( 20.94999999999999929, 5.850000000011105428, -77.13249722427802624 ) ) ;
#145408 =( BOUNDED_SURFACE ( )  B_SPLINE_SURFACE ( 3, 2, ( 
 ( #87519, #30157, #227043 ),
 ( #28902, #31456, #6715 ),
 ( #187934, #204904, #165818 ),
 ( #206205, #9286, #50954 ) ),
 .UNSPECIFIED., .F., .F., .T. ) 
 B_SPLINE_SURFACE_WITH_KNOTS ( ( 4, 4 ),
 ( 3, 3 ),
 ( 0.0006461284895273867708, 0.0007503702773985852087 ),
 ( 0.000000000000000000, 1.000000000000000000 ),
 .UNSPECIFIED. ) 
 GEOMETRIC_REPRESENTATION_ITEM ( )  RATIONAL_B_SPLINE_SURFACE ( (
 ( 1.000000000000000000, 0.7071067811865532349, 1.000000000000000000),
 ( 1.000000000000000000, 0.7076476444648546194, 1.000000000000000000),
 ( 1.000000000000000000, 0.7075727925190693490, 1.000000000000000000),
 ( 1.000000000000000000, 0.7071067811865725528, 1.000000000000000000) ) ) 
 REPRESENTATION_ITEM ( '' )  SURFACE ( )  );
#145409 = ADVANCED_FACE ( 'NONE', ( #105015 ), #84157, .T. ) ;
#145410 = EDGE_CURVE ( 'NONE', #225759, #139066, #89333, .T. ) ;
#145411 = DIRECTION ( 'NONE',  ( 1.000000000000000000, 0.000000000000000000, -0.000000000000000000 ) ) ;
#145413 = VERTEX_POINT ( 'NONE', #4657 ) ;
#145412 = LINE ( 'NONE', #223655, #76464 ) ;
#145414 = CARTESIAN_POINT ( 'NONE',  ( 23.14999999999998437, 0.000000000000000000, 0.000000000000000000 ) ) ;
#145415 = CARTESIAN_POINT ( 'NONE',  ( -22.39999999999999858, 76.00000000001173817, -81.17267829206912211 ) ) ;
#145416 = LINE ( 'NONE', #132279, #194287 ) ;
#145417 = VECTOR ( 'NONE', #197024, 1000.000000000000114 ) ;
#145419 = CYLINDRICAL_SURFACE ( 'NONE', #24421, 0.09999999999999939493 ) ;
#145418 = CARTESIAN_POINT ( 'NONE',  ( 11.60000000000000142, -8.279289321881348584, 18.97071067811865674 ) ) ;
#145420 = CARTESIAN_POINT ( 'NONE',  ( 21.05000000000000071, 39.14563005184295719, -236.8629343064758075 ) ) ;
#145421 = CARTESIAN_POINT ( 'NONE',  ( -22.39999999999999858, -2.576749817950531707, -189.6385361693310756 ) ) ;
#145422 = DIRECTION ( 'NONE',  ( 0.000000000000000000, 0.9126074666063770380, 0.4088369013363281068 ) ) ;
#145423 = LINE ( 'NONE', #245825, #113609 ) ;
#145424 = AXIS2_PLACEMENT_3D ( 'NONE', #189297, #208852, #186738 ) ;
#145425 = ORIENTED_EDGE ( 'NONE', *, *, #53676, .F. ) ;
#145426 = EDGE_CURVE ( 'NONE', #188436, #51707, #245205, .T. ) ;
#145427 = ORIENTED_EDGE ( 'NONE', *, *, #224428, .T. ) ;
#145428 = DIRECTION ( 'NONE',  ( 0.000000000000000000, 3.469446951953515108E-14, 1.000000000000000000 ) ) ;
#145429 = ORIENTED_EDGE ( 'NONE', *, *, #202996, .F. ) ;
#145430 = CARTESIAN_POINT ( 'NONE',  ( -20.99551997958407412, 64.25000000001219291, -143.3714483468355922 ) ) ;
#145431 = EDGE_LOOP ( 'NONE', ( #151230, #176707, #33681, #150078 ) ) ;
#145432 = SURFACE_STYLE_USAGE ( .BOTH. , #65912 ) ;
#145433 = CARTESIAN_POINT ( 'NONE',  ( 20.94999675878240808, 65.70692517833255408, -131.0644653378303985 ) ) ;
#145435 = DIRECTION ( 'NONE',  ( 2.952720810173289112E-16, 1.000000000000000000, 9.912705577010238578E-15 ) ) ;
#145434 = AXIS2_PLACEMENT_3D ( 'NONE', #89807, #229348, #50669 ) ;
#145436 = ORIENTED_EDGE ( 'NONE', *, *, #109712, .F. ) ;
#145437 = EDGE_CURVE ( 'NONE', #224935, #61278, #28594, .T. ) ;
#145438 = CARTESIAN_POINT ( 'NONE',  ( -21.14999999999999858, 6.390846877240202950, -199.6081416912452653 ) ) ;
#145439 = ORIENTED_EDGE ( 'NONE', *, *, #62854, .F. ) ;
#145440 = ORIENTED_EDGE ( 'NONE', *, *, #216926, .F. ) ;
#145441 = LINE ( 'NONE', #8517, #79701 ) ;
#145442 = CARTESIAN_POINT ( 'NONE',  ( -21.08134388332232589, 75.92418108250502939, -109.3577880650422856 ) ) ;
#145444 = ORIENTED_EDGE ( 'NONE', *, *, #54497, .F. ) ;
#145443 = CARTESIAN_POINT ( 'NONE',  ( 21.05000000000005400, 77.16254490893143725, -44.02310748452479316 ) ) ;
#145445 = FACE_OUTER_BOUND ( 'NONE', #206083, .T. ) ;
#145447 = VERTEX_POINT ( 'NONE', #69809 ) ;
#145446 = DIRECTION ( 'NONE',  ( -1.000000000000000000, 1.207181226542539700E-16, -2.694675058168174199E-16 ) ) ;
#145448 = CARTESIAN_POINT ( 'NONE',  ( -23.25000000000000355, 5.650000000011139001, -180.1499999999999773 ) ) ;
#145449 = FACE_OUTER_BOUND ( 'NONE', #44378, .T. ) ;
#145450 = EDGE_CURVE ( 'NONE', #206237, #88666, #95351, .T. ) ;
#145452 = ORIENTED_EDGE ( 'NONE', *, *, #246360, .T. ) ;
#145451 = CARTESIAN_POINT ( 'NONE',  ( 22.39999999999999503, 76.00000000001222134, -148.1726782920690937 ) ) ;
#145453 = DIRECTION ( 'NONE',  ( 0.000000000000000000, -7.304098846218139203E-15, 1.000000000000000000 ) ) ;
#145454 = CARTESIAN_POINT ( 'NONE',  ( 23.24999999999999645, 67.17743825834560312, -115.6731074845243654 ) ) ;
#145455 = ADVANCED_FACE ( 'NONE', ( #148048 ), #156052, .T. ) ;
#145456 = DIRECTION ( 'NONE',  ( 0.000000000000000000, -6.982962677686267499E-15, 1.000000000000000000 ) ) ;
#145457 = VECTOR ( 'NONE', #245977, 1000.000000000000000 ) ;
#145460 = FACE_OUTER_BOUND ( 'NONE', #58170, .T. ) ;
#145459 = AXIS2_PLACEMENT_3D ( 'NONE', #157709, #255422, #18147 ) ;
#145458 = FACE_OUTER_BOUND ( 'NONE', #140416, .T. ) ;
#145461 = DIRECTION ( 'NONE',  ( 0.000000000000000000, -0.9908441862701596881, -0.1350103645451904977 ) ) ;
#145462 = AXIS2_PLACEMENT_3D ( 'NONE', #117034, #59588, #139124 ) ;
#145463 = AXIS2_PLACEMENT_3D ( 'NONE', #22354, #204798, #47001 ) ;
#145464 = DIRECTION ( 'NONE',  ( 0.000000000000000000, 0.9126074666063805907, 0.4088369013363201132 ) ) ;
#145465 = DIRECTION ( 'NONE',  ( -1.646408749285562691E-14, -1.000000000000000000, -6.982962677686266711E-15 ) ) ;
#145466 = DIRECTION ( 'NONE',  ( 0.000000000000000000, -0.008583690987162452199, -0.9999631594459053030 ) ) ;
#145467 = ORIENTED_EDGE ( 'NONE', *, *, #89683, .F. ) ;
#145468 = ORIENTED_EDGE ( 'NONE', *, *, #172759, .F. ) ;
#145469 = ORIENTED_EDGE ( 'NONE', *, *, #241866, .T. ) ;
#145470 = EDGE_CURVE ( 'NONE', #160216, #135320, #3777, .T. ) ;
#145471 = CARTESIAN_POINT ( 'NONE',  ( 21.14999999999999858, 75.90220970870393558, -209.7809220950004772 ) ) ;
#145472 = VECTOR ( 'NONE', #26248, 1000.000000000000000 ) ;
#145473 = ORIENTED_EDGE ( 'NONE', *, *, #153415, .F. ) ;
#145474 = DIRECTION ( 'NONE',  ( 0.000000000000000000, -0.2128009952263485993, 0.9770955615653341697 ) ) ;
#145475 = ORIENTED_EDGE ( 'NONE', *, *, #99864, .T. ) ;
#145476 = DIRECTION ( 'NONE',  ( -0.000000000000000000, -0.2128009952263603677, 0.9770955615653313941 ) ) ;
#145477 = CARTESIAN_POINT ( 'NONE',  ( 20.85000000000000142, 62.46832465249013921, -225.2232495205141731 ) ) ;
#145478 = EDGE_CURVE ( 'NONE', #206061, #157661, #233987, .T. ) ;
#145479 = EDGE_CURVE ( 'NONE', #42394, #192176, #175337, .T. ) ;
#145480 = AXIS2_PLACEMENT_3D ( 'NONE', #72636, #188705, #71351 ) ;
#145481 = CIRCLE ( 'NONE', #212139, 7.900000000000003908 ) ;
#145482 = ORIENTED_EDGE ( 'NONE', *, *, #31088, .T. ) ;
#145483 = AXIS2_PLACEMENT_3D ( 'NONE', #240583, #243148, #25407 ) ;
#145484 = EDGE_CURVE ( 'NONE', #185809, #183191, #33268, .T. ) ;
#145485 = CARTESIAN_POINT ( 'NONE',  ( 15.66039659514495774, 9.360749169926261715, -151.3145701406073158 ) ) ;
#145486 = SURFACE_STYLE_USAGE ( .BOTH. , #110206 ) ;
#145487 = VERTEX_POINT ( 'NONE', #14967 ) ;
#145488 = CIRCLE ( 'NONE', #3856, 11.64999999999998970 ) ;
#145489 = ORIENTED_EDGE ( 'NONE', *, *, #43189, .T. ) ;
#145490 = ORIENTED_EDGE ( 'NONE', *, *, #58696, .F. ) ;
#145491 = CARTESIAN_POINT ( 'NONE',  ( 20.94999999999999574, 74.75000000001159606, -61.52310748452433131 ) ) ;
#145492 = DIRECTION ( 'NONE',  ( -1.000000000000000000, 0.000000000000000000, 0.000000000000000000 ) ) ;
#145493 = CARTESIAN_POINT ( 'NONE',  ( 15.74999999999999645, 26.30888228346803714, -233.3999513616626587 ) ) ;
#145494 = DIRECTION ( 'NONE',  ( -0.000000000000000000, 0.9126074666063770380, 0.4088369013363281068 ) ) ;
#145495 = CARTESIAN_POINT ( 'NONE',  ( -23.25000000000000000, 76.00000000001190870, -103.0231074845243029 ) ) ;
#145496 = EDGE_CURVE ( 'NONE', #239517, #52893, #115325, .T. ) ;
#145498 = DIRECTION ( 'NONE',  ( -0.000000000000000000, 1.000000000000000000, -0.000000000000000000 ) ) ;
#145497 = DIRECTION ( 'NONE',  ( 1.000000000000000000, 0.000000000000000000, 0.000000000000000000 ) ) ;
#145499 = CARTESIAN_POINT ( 'NONE',  ( -18.34374000495059676, 11.47316190337362940, -57.75000000000000711 ) ) ;
#145501 = ORIENTED_EDGE ( 'NONE', *, *, #242512, .F. ) ;
#145500 = LINE ( 'NONE', #26875, #77334 ) ;
#145503 = CARTESIAN_POINT ( 'NONE',  ( 19.99999999999998934, 64.25000000001196554, -111.6731074845243796 ) ) ;
#145502 = LINE ( 'NONE', #202914, #96728 ) ;
#145504 = DIRECTION ( 'NONE',  ( 0.000000000000000000, 0.000000000000000000, 1.000000000000000000 ) ) ;
#145505 = VERTEX_POINT ( 'NONE', #55323 ) ;
#145506 = CARTESIAN_POINT ( 'NONE',  ( 20.95576188350343116, 10.60898054497455512, -74.61123372275433496 ) ) ;
#145507 = CARTESIAN_POINT ( 'NONE',  ( 18.52928932188133970, 14.58714922055045626, -219.6735472415052755 ) ) ;
#145508 = ORIENTED_EDGE ( 'NONE', *, *, #191934, .F. ) ;
#145509 = CARTESIAN_POINT ( 'NONE',  ( -16.94165728009537375, 30.26040018438209955, -234.7930488771960427 ) ) ;
#145510 = AXIS2_PLACEMENT_3D ( 'NONE', #207213, #84633, #102937 ) ;
#145511 = FACE_OUTER_BOUND ( 'NONE', #254721, .T. ) ;
#145512 = DIRECTION ( 'NONE',  ( -1.000000000000000000, -0.000000000000000000, -0.000000000000000000 ) ) ;
#145513 = ORIENTED_EDGE ( 'NONE', *, *, #222209, .T. ) ;
#145514 = ORIENTED_EDGE ( 'NONE', *, *, #17060, .T. ) ;
#145515 = DIRECTION ( 'NONE',  ( -1.000000000000000000, 0.000000000000000000, 0.000000000000000000 ) ) ;
#145516 = ORIENTED_EDGE ( 'NONE', *, *, #148122, .F. ) ;
#145517 = CARTESIAN_POINT ( 'NONE',  ( 22.39999999999999858, 7.790779598384538041, -67.00000000000004263 ) ) ;
#145519 = DIRECTION ( 'NONE',  ( -1.000000000000000000, 0.000000000000000000, 0.000000000000000000 ) ) ;
#145518 = TOROIDAL_SURFACE ( 'NONE', #245497, 0.9750000000000019762, 0.1000000000000000056 ) ;
#145520 = FACE_OUTER_BOUND ( 'NONE', #32669, .T. ) ;
#145521 = DIRECTION ( 'NONE',  ( 0.000000000000000000, 0.8814952561688432775, -0.4721928772777344019 ) ) ;
#145522 = ORIENTED_EDGE ( 'NONE', *, *, #203848, .T. ) ;
#145523 = CARTESIAN_POINT ( 'NONE',  ( -12.26136940704871670, 9.351403174152810749, -117.4795304368385018 ) ) ;
#145524 = CARTESIAN_POINT ( 'NONE',  ( 18.59999999999999432, 1.637172712981537659, -45.08215336547201701 ) ) ;
#145525 = DIRECTION ( 'NONE',  ( 0.000000000000000000, 6.982962677686266711E-15, -1.000000000000000000 ) ) ;
#145526 = CARTESIAN_POINT ( 'NONE',  ( -20.94999999999999929, 11.70000000001115126, -93.74500185048142953 ) ) ;
#145527 = AXIS2_PLACEMENT_3D ( 'NONE', #195649, #178665, #119970 ) ;
#145528 = EDGE_CURVE ( 'NONE', #40125, #120362, #116218, .T. ) ;
#145529 = ORIENTED_EDGE ( 'NONE', *, *, #112389, .F. ) ;
#145531 = CARTESIAN_POINT ( 'NONE',  ( -23.25000000000000000, 1.115600667400684642E-11, -33.50000000000000000 ) ) ;
#145530 = CIRCLE ( 'NONE', #74842, 0.1000000000000043771 ) ;
#145533 = EDGE_LOOP ( 'NONE', ( #80912, #55606, #10856, #95838 ) ) ;
#145532 = CARTESIAN_POINT ( 'NONE',  ( -18.59999999999999787, 76.00000000001142553, -36.02310748452432421 ) ) ;
#145534 = DIRECTION ( 'NONE',  ( -1.000000000000000000, -0.000000000000000000, -0.000000000000000000 ) ) ;
#145535 = CARTESIAN_POINT ( 'NONE',  ( -21.05000000000000071, 33.99373157816623348, -243.8426824212930342 ) ) ;
#145536 = EDGE_CURVE ( 'NONE', #256823, #45859, #253552, .T. ) ;
#145537 = CARTESIAN_POINT ( 'NONE',  ( -16.85718274719420506, 9.976142314632891583, -87.93665366781755210 ) ) ;
#145538 = CARTESIAN_POINT ( 'NONE',  ( 18.59999999999999432, 1.736257131597397585, -11.56865232901749962 ) ) ;
#145539 = AXIS2_PLACEMENT_3D ( 'NONE', #22066, #79434, #83272 ) ;
#145540 = DIRECTION ( 'NONE',  ( 0.000000000000000000, -0.4999999999999088507, 0.8660254037844913322 ) ) ;
#145541 = DIRECTION ( 'NONE',  ( -0.000000000000000000, 1.000000000000000000, -0.000000000000000000 ) ) ;
#145542 = CIRCLE ( 'NONE', #33163, 0.09999999999999939493 ) ;
#145543 = ORIENTED_EDGE ( 'NONE', *, *, #135028, .T. ) ;
#145544 = PLANE ( 'NONE',  #115043 ) ;
#145545 = EDGE_CURVE ( 'NONE', #100848, #112967, #52773, .T. ) ;
#145546 = EDGE_CURVE ( 'NONE', #12767, #180952, #53656, .T. ) ;
#145547 = DIRECTION ( 'NONE',  ( 0.000000000000000000, 0.9651348961777379554, -0.2617529984164210233 ) ) ;
#145548 = DIRECTION ( 'NONE',  ( 0.000000000000000000, 0.9908441862701782288, 0.1350103645450542456 ) ) ;
#145549 = DIRECTION ( 'NONE',  ( 0.000000000000000000, 0.000000000000000000, -1.000000000000000000 ) ) ;
#145550 = VECTOR ( 'NONE', #191077, 1000.000000000000000 ) ;
#145551 = VECTOR ( 'NONE', #213574, 1000.000000000000000 ) ;
#145553 = ORIENTED_EDGE ( 'NONE', *, *, #147099, .T. ) ;
#145552 = AXIS2_PLACEMENT_3D ( 'NONE', #159608, #215697, #233989 ) ;
#145554 = ORIENTED_EDGE ( 'NONE', *, *, #167737, .F. ) ;
#145555 = CIRCLE ( 'NONE', #66464, 0.1000000000000001860 ) ;
#145556 = DIRECTION ( 'NONE',  ( 1.000000000000000000, 0.000000000000000000, 0.000000000000000000 ) ) ;
#145557 = CARTESIAN_POINT ( 'NONE',  ( 22.47071067811864964, 0.09909245471376176839, -126.2799252555019649 ) ) ;
#145558 = CARTESIAN_POINT ( 'NONE',  ( -20.00857864376270001, 30.18117236077229038, -235.7011183606462339 ) ) ;
#145559 = ADVANCED_FACE ( 'NONE', ( #253545 ), #194891, .F. ) ;
#145560 = AXIS2_PLACEMENT_3D ( 'NONE', #217287, #38677, #118211 ) ;
#145561 = DIRECTION ( 'NONE',  ( 1.000000000000000000, 0.000000000000000000, 0.000000000000000000 ) ) ;
#145562 = EDGE_CURVE ( 'NONE', #137697, #257538, #13667, .T. ) ;
#145563 = CARTESIAN_POINT ( 'NONE',  ( 22.37643362114956247, 7.625789993958378865, 0.09908137368138185408 ) ) ;
#145564 = CARTESIAN_POINT ( 'NONE',  ( 20.85000000000000142, -1.736705739456431807, -179.0174225876237415 ) ) ;
#145565 = CARTESIAN_POINT ( 'NONE',  ( -21.05000000000000071, 16.98881331171929787, -224.4946931418895701 ) ) ;
#145566 = ORIENTED_EDGE ( 'NONE', *, *, #149297, .T. ) ;
#145567 = DIRECTION ( 'NONE',  ( -0.000000000000000000, -0.9371753822965315228, 0.3488585713686134238 ) ) ;
#145568 = EDGE_CURVE ( 'NONE', #43098, #35500, #41212, .T. ) ;
#145569 = ORIENTED_EDGE ( 'NONE', *, *, #105269, .F. ) ;
#145570 = EDGE_CURVE ( 'NONE', #174346, #249207, #203690, .T. ) ;
#145571 = PLANE ( 'NONE',  #114166 ) ;
#145572 = ADVANCED_FACE ( 'NONE', ( #95748 ), #151920, .F. ) ;
#145573 = DIRECTION ( 'NONE',  ( -1.000000000000000000, 4.624352451196580357E-15, 3.439547145395922042E-14 ) ) ;
#145574 = CARTESIAN_POINT ( 'NONE',  ( 20.94999999999999574, 1.148907358139439339E-11, -201.0000000000015064 ) ) ;
#145575 = DIRECTION ( 'NONE',  ( 0.000000000000000000, 1.000000000000000000, 6.608470384673536824E-15 ) ) ;
#145576 = CARTESIAN_POINT ( 'NONE',  ( -20.65000000000000568, 5.650000000011139001, -113.1500000000000341 ) ) ;
#145577 = CARTESIAN_POINT ( 'NONE',  ( 23.24999999999999645, 11.74999999999998224, -9.250000000000001776 ) ) ;
#145578 = CARTESIAN_POINT ( 'NONE',  ( -18.48550754432028143, -9.463399778559915987, -7.048789752415359544 ) ) ;
#145579 = DIRECTION ( 'NONE',  ( -3.265361837132813093E-16, 1.000000000000000000, 0.000000000000000000 ) ) ;
#145580 = CIRCLE ( 'NONE', #228989, 0.09999999999999939493 ) ;
#145581 = CARTESIAN_POINT ( 'NONE',  ( 22.47007471830798764, 1.115784145324971765E-11, -92.77928934807357564 ) ) ;
#145582 = CARTESIAN_POINT ( 'NONE',  ( 20.94999999999999929, 72.02722222756959525, -225.1832529173024398 ) ) ;
#145583 = AXIS2_PLACEMENT_3D ( 'NONE', #9487, #69492, #249404 ) ;
#145584 = CARTESIAN_POINT ( 'NONE',  ( 18.54999999999999716, 29.63969710739366903, -235.8648393122026334 ) ) ;
#145586 = EDGE_CURVE ( 'NONE', #151026, #205485, #73669, .T. ) ;
#145585 = DIRECTION ( 'NONE',  ( 0.000000000000000000, -0.9126074666063545004, -0.4088369013363783999 ) ) ;
#145587 = CARTESIAN_POINT ( 'NONE',  ( 20.94999999999999929, 8.926614585098256782, -175.9716830192231214 ) ) ;
#145588 = AXIS2_PLACEMENT_3D ( 'NONE', #98009, #180161, #198421 ) ;
#145589 = ORIENTED_EDGE ( 'NONE', *, *, #244249, .T. ) ;
#145590 = DIRECTION ( 'NONE',  ( -0.000000000000000000, -0.000000000000000000, -1.000000000000000000 ) ) ;
#145591 = CARTESIAN_POINT ( 'NONE',  ( 23.25000000000000000, 69.45000000001186891, -90.67310748452435121 ) ) ;
#145592 = ORIENTED_EDGE ( 'NONE', *, *, #94810, .F. ) ;
#145593 = CARTESIAN_POINT ( 'NONE',  ( -16.93301857435215396, 51.64075575048902778, -231.9078325284192204 ) ) ;
#145594 = FACE_OUTER_BOUND ( 'NONE', #28754, .T. ) ;
#145595 = CIRCLE ( 'NONE', #195716, 0.1000000000000069861 ) ;
#145596 = EDGE_CURVE ( 'NONE', #209272, #190690, #86940, .T. ) ;
#145597 = CARTESIAN_POINT ( 'NONE',  ( 18.39999999999999503, 64.25000000001151079, -45.27310748452440237 ) ) ;
#145598 = AXIS2_PLACEMENT_3D ( 'NONE', #136747, #177206, #241005 ) ;
#145599 = ORIENTED_EDGE ( 'NONE', *, *, #171016, .F. ) ;
#145600 = DIRECTION ( 'NONE',  ( 1.000000000000000000, 0.000000000000000000, 0.000000000000000000 ) ) ;
#145601 = LINE ( 'NONE', #206874, #26843 ) ;
#145602 = ORIENTED_EDGE ( 'NONE', *, *, #210018, .F. ) ;
#145603 = AXIS2_PLACEMENT_3D ( 'NONE', #108885, #249691, #128457 ) ;
#145604 = DIRECTION ( 'NONE',  ( 0.000000000000000000, 0.9908441862701596881, 0.1350103645451904977 ) ) ;
#145605 = EDGE_CURVE ( 'NONE', #64314, #3674, #145406, .T. ) ;
#145606 = VERTEX_POINT ( 'NONE', #189740 ) ;
#145607 = DIRECTION ( 'NONE',  ( -1.000000000000000000, -0.000000000000000000, 0.000000000000000000 ) ) ;
#145608 = DIRECTION ( 'NONE',  ( -1.836970198721030427E-16, -0.4088369013363281623, 0.9126074666063771490 ) ) ;
#145609 = DIRECTION ( 'NONE',  ( 0.000000000000000000, 0.8814952561688437216, -0.4721928772777334582 ) ) ;
#145610 = CARTESIAN_POINT ( 'NONE',  ( -21.05000000000000071, 87.29603075034764004, -166.9752083248604038 ) ) ;
#145611 = EDGE_CURVE ( 'NONE', #74964, #40351, #237010, .T. ) ;
#145612 = CARTESIAN_POINT ( 'NONE',  ( -23.15000000000000213, 64.25000000001219291, -143.5379132551784096 ) ) ;
#145613 = CARTESIAN_POINT ( 'NONE',  ( -22.59999999999999787, 55.86495732666938352, -232.8769840133977880 ) ) ;
#145614 = CARTESIAN_POINT ( 'NONE',  ( -20.94999999999999574, 11.62071067812980907, -194.1315833476589887 ) ) ;
#145615 = CARTESIAN_POINT ( 'NONE',  ( 23.25000000000000000, 49.61306877027904250, -254.2671747026441551 ) ) ;
#145616 = DIRECTION ( 'NONE',  ( 0.000000000000000000, 0.9998779222360100194, 0.01562499999998606150 ) ) ;
#145618 = EDGE_LOOP ( 'NONE', ( #65766, #79072, #116984, #133001 ) ) ;
#145617 = DIRECTION ( 'NONE',  ( 1.000000000000000000, 0.000000000000000000, 0.000000000000000000 ) ) ;
#145620 = VERTEX_POINT ( 'NONE', #249714 ) ;
#145619 = B_SPLINE_CURVE_WITH_KNOTS ( 'NONE', 3,
 ( #257920, #78043, #157636, #218830, #238412, #197989, #19372, #79315, #21944, #155060, #195465, #59744, #234559, #237133, #58463, #217543, #138008, #38943, #118482 ),
 .UNSPECIFIED., .F., .F.,
 ( 4, 3, 3, 3, 3, 3, 4 ),
 ( 0.000000000000000000, 1.655171619026035414E-05, 2.773500582848522787E-05, 5.941817267378589329E-05, 0.0001114174635873550078, 0.0001914169455916382733, 0.0002627181070750683224 ),
 .UNSPECIFIED. ) ;
#145622 = FACE_OUTER_BOUND ( 'NONE', #74522, .T. ) ;
#145621 = AXIS2_PLACEMENT_3D ( 'NONE', #23814, #55478, #135030 ) ;
#145623 = CIRCLE ( 'NONE', #33244, 0.1000000000000028644 ) ;
#145625 = ORIENTED_EDGE ( 'NONE', *, *, #7311, .T. ) ;
#145624 = CARTESIAN_POINT ( 'NONE',  ( 20.95512820512820440, 8.876151316299271343, -109.0586289951409924 ) ) ;
#145626 = VERTEX_POINT ( 'NONE', #71091 ) ;
#145627 = DIRECTION ( 'NONE',  ( -1.000000000000000000, -0.000000000000000000, -0.000000000000000000 ) ) ;
#145628 = EDGE_CURVE ( 'NONE', #13286, #88928, #228650, .T. ) ;
#145629 = EDGE_CURVE ( 'NONE', #160806, #93811, #82837, .T. ) ;
#145630 = DIRECTION ( 'NONE',  ( -1.000000000000000000, 0.000000000000000000, 0.000000000000000000 ) ) ;
#145631 = DIRECTION ( 'NONE',  ( 0.000000000000000000, 0.000000000000000000, -1.000000000000000000 ) ) ;
#145632 = DIRECTION ( 'NONE',  ( 0.000000000000000000, 0.000000000000000000, -1.000000000000000000 ) ) ;
#145633 = CARTESIAN_POINT ( 'NONE',  ( -22.39999999999999858, 76.00000000001219291, -144.3138870828977076 ) ) ;
#145634 = DIRECTION ( 'NONE',  ( 0.000000000000000000, 0.000000000000000000, -1.000000000000000000 ) ) ;
#145635 = AXIS2_PLACEMENT_3D ( 'NONE', #51582, #69925, #133717 ) ;
#145637 = ORIENTED_EDGE ( 'NONE', *, *, #66005, .F. ) ;
#145636 = EDGE_CURVE ( 'NONE', #102120, #100958, #149540, .T. ) ;
#145638 = VERTEX_POINT ( 'NONE', #215696 ) ;
#145639 = TOROIDAL_SURFACE ( 'NONE', #187365, 11.65000000000000036, 0.1000000000000000056 ) ;
#145640 = LINE ( 'NONE', #186070, #214606 ) ;
#145641 = CIRCLE ( 'NONE', #103934, 0.1000000000000001027 ) ;
#145642 = VECTOR ( 'NONE', #227927, 1000.000000000000227 ) ;
#145643 = ORIENTED_EDGE ( 'NONE', *, *, #206206, .F. ) ;
#145644 = CYLINDRICAL_SURFACE ( 'NONE', #1179, 4.049999999999998046 ) ;
#145646 = EDGE_CURVE ( 'NONE', #2598, #81779, #120501, .T. ) ;
#145645 = EDGE_LOOP ( 'NONE', ( #192985, #33757, #26880, #208487 ) ) ;
#145647 = DIRECTION ( 'NONE',  ( 0.000000000000000000, -0.9994937237965558774, -0.03181660087586650476 ) ) ;
#145648 = AXIS2_PLACEMENT_3D ( 'NONE', #207454, #87474, #31407 ) ;
#145649 = DIRECTION ( 'NONE',  ( -1.000000000000000000, 0.000000000000000000, 0.000000000000000000 ) ) ;
#145650 = EDGE_CURVE ( 'NONE', #57263, #147844, #142750, .T. ) ;
#145651 = DIRECTION ( 'NONE',  ( 0.000000000000000000, 0.000000000000000000, 1.000000000000000000 ) ) ;
#145652 = CARTESIAN_POINT ( 'NONE',  ( 23.25000000000000000, 75.39949836213487799, -250.2448839681187849 ) ) ;
#145653 = ORIENTED_EDGE ( 'NONE', *, *, #117380, .F. ) ;
#145654 = APPLICATION_CONTEXT ( 'automotive_design' ) ;
#145655 = CARTESIAN_POINT ( 'NONE',  ( 19.88284271247461987, 11.69142135624847256, -125.2500000000000284 ) ) ;
#145656 = ORIENTED_EDGE ( 'NONE', *, *, #1005, .T. ) ;
#145657 = CARTESIAN_POINT ( 'NONE',  ( -20.09999999999999787, 4.547418889303922462, 21.90000000000000213 ) ) ;
#145658 = CIRCLE ( 'NONE', #66584, 12.97500000000000320 ) ;
#145659 = CARTESIAN_POINT ( 'NONE',  ( 20.12500000000000355, 66.74195072709477472, -128.1597686473819238 ) ) ;
#145660 = EDGE_CURVE ( 'NONE', #125626, #42728, #230072, .T. ) ;
#145661 = DIRECTION ( 'NONE',  ( -1.000000000000000000, -2.885090398161910739E-16, -6.283419270304611573E-17 ) ) ;
#145663 = ORIENTED_EDGE ( 'NONE', *, *, #76367, .F. ) ;
#145662 = EDGE_CURVE ( 'NONE', #174189, #68442, #119194, .T. ) ;
#145664 = PLANE ( 'NONE',  #186020 ) ;
#145665 = ORIENTED_EDGE ( 'NONE', *, *, #245424, .T. ) ;
#145668 = ORIENTED_EDGE ( 'NONE', *, *, #197557, .F. ) ;
#145667 = CARTESIAN_POINT ( 'NONE',  ( -23.25000000000000000, 74.08971962618051066, -157.3917396293254285 ) ) ;
#145666 = DIRECTION ( 'NONE',  ( 0.000000000000000000, 0.5000000000000078826, -0.8660254037844340447 ) ) ;
#145669 = VECTOR ( 'NONE', #70496, 999.9999999999998863 ) ;
#145670 = DIRECTION ( 'NONE',  ( -1.000000000000000000, 0.000000000000000000, 0.000000000000000000 ) ) ;
#145671 = ORIENTED_EDGE ( 'NONE', *, *, #22118, .T. ) ;
#145672 = DIRECTION ( 'NONE',  ( 1.000000000000000000, 7.304098846218134667E-16, 0.000000000000000000 ) ) ;
#145673 = ORIENTED_EDGE ( 'NONE', *, *, #199509, .T. ) ;
#145674 = CARTESIAN_POINT ( 'NONE',  ( 20.85000000000000142, 1.115600667400684642E-11, -74.80000000000001137 ) ) ;
#145675 = CARTESIAN_POINT ( 'NONE',  ( -15.55912972643741199, 62.34761478309390981, -221.4236593165597071 ) ) ;
#145676 = EDGE_CURVE ( 'NONE', #170589, #129684, #195338, .T. ) ;
#145677 = DIRECTION ( 'NONE',  ( 0.000000000000000000, -1.000000000000000000, 0.000000000000000000 ) ) ;
#145678 = EDGE_CURVE ( 'NONE', #26573, #53843, #3068, .T. ) ;
#145679 = CARTESIAN_POINT ( 'NONE',  ( -17.29838795459091116, 52.59160405768363233, -231.0487749297699622 ) ) ;
#145680 = DIRECTION ( 'NONE',  ( -0.000000000000000000, 0.9908441862701591329, 0.1350103645451946055 ) ) ;
#145681 = VERTEX_POINT ( 'NONE', #160900 ) ;
#145682 = CARTESIAN_POINT ( 'NONE',  ( 20.94999999999999929, 1.115600667400684642E-11, -167.5000000000000284 ) ) ;
#145683 = SURFACE_STYLE_USAGE ( .BOTH. , #66162 ) ;
#145684 = CARTESIAN_POINT ( 'NONE',  ( -18.46154800491015635, -9.480206274230829067, -140.6574508383815214 ) ) ;
#145685 = AXIS2_PLACEMENT_3D ( 'NONE', #214890, #16709, #20566 ) ;
#145686 = ORIENTED_EDGE ( 'NONE', *, *, #231013, .F. ) ;
#145687 = DIRECTION ( 'NONE',  ( 1.000000000000000000, 0.000000000000000000, 0.000000000000000000 ) ) ;
#145688 = ORIENTED_EDGE ( 'NONE', *, *, #27033, .T. ) ;
#145689 = DIRECTION ( 'NONE',  ( 0.000000000000000000, 0.000000000000000000, 1.000000000000000000 ) ) ;
#145690 = DIRECTION ( 'NONE',  ( 0.000000000000000000, 0.2128009952263588966, -0.9770955615653318382 ) ) ;
#145691 = DIRECTION ( 'NONE',  ( 0.000000000000000000, 0.000000000000000000, 1.000000000000000000 ) ) ;
#145692 = AXIS2_PLACEMENT_3D ( 'NONE', #169286, #131393, #27203 ) ;
#145694 = ORIENTED_EDGE ( 'NONE', *, *, #239559, .T. ) ;
#145693 = CARTESIAN_POINT ( 'NONE',  ( -16.94445028196807002, 66.00793639031407167, -82.13043766294282477 ) ) ;
#145695 = DIRECTION ( 'NONE',  ( 0.000000000000000000, 6.982962677686266711E-15, -1.000000000000000000 ) ) ;
#145696 = AXIS2_PLACEMENT_3D ( 'NONE', #24447, #23164, #124810 ) ;
#145697 = CARTESIAN_POINT ( 'NONE',  ( -15.69373346032659811, 62.70412490954451101, -216.8009802157223476 ) ) ;
#145698 = LINE ( 'NONE', #186125, #118764 ) ;
#145699 = ORIENTED_EDGE ( 'NONE', *, *, #12597, .F. ) ;
#145700 = FACE_OUTER_BOUND ( 'NONE', #71332, .T. ) ;
#145701 = CARTESIAN_POINT ( 'NONE',  ( 21.05000000000000071, -11.64999999998883595, -67.00000000000004263 ) ) ;
#145702 = ORIENTED_EDGE ( 'NONE', *, *, #180779, .T. ) ;
#145703 = CARTESIAN_POINT ( 'NONE',  ( 22.48660254037843842, 64.25000000001237765, -170.0731074845244279 ) ) ;
#145704 = EDGE_CURVE ( 'NONE', #35313, #108264, #218262, .T. ) ;
#145705 = AXIS2_PLACEMENT_3D ( 'NONE', #29877, #88507, #109362 ) ;
#145706 = ORIENTED_EDGE ( 'NONE', *, *, #61335, .F. ) ;
#145707 = CARTESIAN_POINT ( 'NONE',  ( -16.81453046979152433, 44.19626918183404030, -235.2836408652933642 ) ) ;
#145709 = ORIENTED_EDGE ( 'NONE', *, *, #61692, .F. ) ;
#145708 = DIRECTION ( 'NONE',  ( -1.000000000000000000, 0.000000000000000000, 0.000000000000000000 ) ) ;
#145710 = AXIS2_PLACEMENT_3D ( 'NONE', #136184, #77500, #18835 ) ;
#145711 = AXIS2_PLACEMENT_3D ( 'NONE', #223450, #123095, #143920 ) ;
#145712 = CIRCLE ( 'NONE', #249792, 0.1000000000000028644 ) ;
#145715 = ORIENTED_EDGE ( 'NONE', *, *, #62855, .F. ) ;
#145714 = ORIENTED_EDGE ( 'NONE', *, *, #231246, .F. ) ;
#145713 = CARTESIAN_POINT ( 'NONE',  ( -20.94999999999999929, 1.115600667400684642E-11, -200.9999999999999432 ) ) ;
#145716 = CARTESIAN_POINT ( 'NONE',  ( 18.39999999999999503, 5.649999999999983480, -12.65000000000000213 ) ) ;
#145717 = CARTESIAN_POINT ( 'NONE',  ( -20.54999999999999716, 73.50000000001156764, -56.29848556176223440 ) ) ;
#145718 = DIRECTION ( 'NONE',  ( 0.000000000000000000, 0.000000000000000000, 1.000000000000000000 ) ) ;
#145720 = FACE_OUTER_BOUND ( 'NONE', #152491, .T. ) ;
#145719 = PLANE ( 'NONE',  #139954 ) ;
#145722 = EDGE_CURVE ( 'NONE', #143709, #68824, #61778, .T. ) ;
#145721 = LINE ( 'NONE', #10078, #194610 ) ;
#145723 = CYLINDRICAL_SURFACE ( 'NONE', #165562, 0.09999999999999939493 ) ;
#145724 = DIRECTION ( 'NONE',  ( -0.000000000000000000, 1.000000000000000000, 0.000000000000000000 ) ) ;
#145725 = VECTOR ( 'NONE', #184313, 1000.000000000000227 ) ;
#145726 = DIRECTION ( 'NONE',  ( 1.000000000000000000, 0.000000000000000000, 0.000000000000000000 ) ) ;
#145727 = LINE ( 'NONE', #66212, #164043 ) ;
#145728 = VECTOR ( 'NONE', #159726, 1000.000000000000000 ) ;
#145729 = CIRCLE ( 'NONE', #33362, 0.1999999999999997335 ) ;
#145730 = VERTEX_POINT ( 'NONE', #220844 ) ;
#145732 = EDGE_LOOP ( 'NONE', ( #210153, #41522, #54467, #85943 ) ) ;
#145731 = CIRCLE ( 'NONE', #233074, 0.5000000000000007772 ) ;
#145733 = FACE_OUTER_BOUND ( 'NONE', #164901, .T. ) ;
#145735 = VERTEX_POINT ( 'NONE', #38370 ) ;
#145734 = CARTESIAN_POINT ( 'NONE',  ( -23.15000000000000213, 11.65000000001115588, -155.3500000000000227 ) ) ;
#145736 = ORIENTED_EDGE ( 'NONE', *, *, #203050, .T. ) ;
#145737 = AXIS2_PLACEMENT_3D ( 'NONE', #248427, #168936, #33267 ) ;
#145738 = LINE ( 'NONE', #220163, #14502 ) ;
#145739 = VERTEX_POINT ( 'NONE', #18789 ) ;
#145740 = FACE_OUTER_BOUND ( 'NONE', #186201, .T. ) ;
#145741 = ORIENTED_EDGE ( 'NONE', *, *, #210585, .F. ) ;
#145742 = CARTESIAN_POINT ( 'NONE',  ( -16.87331047859649757, 9.949999999999983302, -20.85000000000000142 ) ) ;
#145743 = CARTESIAN_POINT ( 'NONE',  ( 20.94999999999999929, 87.24382154048164750, -206.5725299160771726 ) ) ;
#145745 = ORIENTED_EDGE ( 'NONE', *, *, #90536, .F. ) ;
#145744 = ORIENTED_EDGE ( 'NONE', *, *, #222939, .F. ) ;
#145746 = VERTEX_POINT ( 'NONE', #37108 ) ;
#145747 = DIRECTION ( 'NONE',  ( 0.000000000000000000, 0.8814952561688438326, -0.4721928772777334582 ) ) ;
#145748 = VERTEX_POINT ( 'NONE', #39678 ) ;
#145749 = ORIENTED_EDGE ( 'NONE', *, *, #142597, .F. ) ;
#145750 = DIRECTION ( 'NONE',  ( 0.000000000000000000, 0.000000000000000000, -1.000000000000000000 ) ) ;
#145751 = CARTESIAN_POINT ( 'NONE',  ( 18.54286124688534088, -9.623917578786652882, -73.74120233186270923 ) ) ;
#145753 = ORIENTED_EDGE ( 'NONE', *, *, #93076, .T. ) ;
#145752 = CARTESIAN_POINT ( 'NONE',  ( 22.39999999999999503, 12.71802988599559647, -223.5105008658000258 ) ) ;
#145754 = DIRECTION ( 'NONE',  ( 1.000000000000000000, 0.000000000000000000, 0.000000000000000000 ) ) ;
#145755 = CARTESIAN_POINT ( 'NONE',  ( 21.05000000000000071, 4.252251777740766236, -211.8999245327126744 ) ) ;
#145757 = VERTEX_POINT ( 'NONE', #201286 ) ;
#145756 = PLANE ( 'NONE',  #147347 ) ;
#145758 = CARTESIAN_POINT ( 'NONE',  ( -23.25000000000000000, 78.45218979564165807, -232.7313097695096076 ) ) ;
#145759 = EDGE_LOOP ( 'NONE', ( #151944, #147976, #222384, #15950 ) ) ;
#145760 = FACE_OUTER_BOUND ( 'NONE', #82508, .T. ) ;
#145761 = CIRCLE ( 'NONE', #16802, 0.09999999999998898659 ) ;
#145762 = ORIENTED_EDGE ( 'NONE', *, *, #24055, .F. ) ;
#145763 = FACE_OUTER_BOUND ( 'NONE', #130335, .T. ) ;
#145764 = DIRECTION ( 'NONE',  ( 0.000000000000000000, 0.1568667991644863147, 0.9876197685951252359 ) ) ;
#145765 = EDGE_CURVE ( 'NONE', #171007, #86432, #82587, .T. ) ;
#145766 = ORIENTED_EDGE ( 'NONE', *, *, #127069, .T. ) ;
#145768 = DIRECTION ( 'NONE',  ( -1.000000000000000000, 3.265361837132813093E-16, 2.280189983783949500E-30 ) ) ;
#145767 = CARTESIAN_POINT ( 'NONE',  ( -23.15000000000000213, 63.84823067483194592, -203.4394279312818981 ) ) ;
#145769 = AXIS2_PLACEMENT_3D ( 'NONE', #9209, #148737, #170910 ) ;
#145770 = DIRECTION ( 'NONE',  ( 0.000000000000000000, 0.000000000000000000, 1.000000000000000000 ) ) ;
#145771 = CARTESIAN_POINT ( 'NONE',  ( -20.94999999999999929, 0.5450571430110628945, -208.9664790259058691 ) ) ;
#145772 = ORIENTED_EDGE ( 'NONE', *, *, #159782, .T. ) ;
#145773 = ORIENTED_EDGE ( 'NONE', *, *, #130416, .F. ) ;
#145774 = EDGE_CURVE ( 'NONE', #75549, #75787, #197428, .T. ) ;
#145775 = CARTESIAN_POINT ( 'NONE',  ( -21.65000000000000213, 7.250000000011138646, -76.25000000000004263 ) ) ;
#145776 = LINE ( 'NONE', #66262, #27671 ) ;
#145777 = EDGE_LOOP ( 'NONE', ( #255906, #166548, #113018, #241002 ) ) ;
#145778 = CARTESIAN_POINT ( 'NONE',  ( -20.94999999999999929, 0.2561057921033771945, -133.9651035583277121 ) ) ;
#145779 = ORIENTED_EDGE ( 'NONE', *, *, #35491, .T. ) ;
#145780 = LINE ( 'NONE', #104075, #35881 ) ;
#145781 = ORIENTED_EDGE ( 'NONE', *, *, #116202, .F. ) ;
#145782 = DIRECTION ( 'NONE',  ( 1.000000000000000000, -1.836970198721029934E-16, -1.282749433769087582E-30 ) ) ;
#145783 = ADVANCED_FACE ( 'NONE', ( #80020 ), #176613, .F. ) ;
#145784 = AXIS2_PLACEMENT_3D ( 'NONE', #252066, #235085, #74761 ) ;
#145785 = FACE_OUTER_BOUND ( 'NONE', #200707, .T. ) ;
#145786 = DIRECTION ( 'NONE',  ( 0.000000000000000000, 0.000000000000000000, 1.000000000000000000 ) ) ;
#145787 = CIRCLE ( 'NONE', #66703, 4.299999999999970512 ) ;
#145788 = ORIENTED_EDGE ( 'NONE', *, *, #142487, .F. ) ;
#145789 = EDGE_CURVE ( 'NONE', #249188, #39196, #77460, .T. ) ;
#145790 = CARTESIAN_POINT ( 'NONE',  ( 18.40916198585732388, -9.499999999988844479, -207.6001896318236390 ) ) ;
#145791 = SHAPE_REPRESENTATION_RELATIONSHIP ( 'NONE' , 'NONE' ,  #178537, #250584 ) ;
#145792 = AXIS2_PLACEMENT_3D ( 'NONE', #195859, #58862, #95444 ) ;
#145794 = ORIENTED_EDGE ( 'NONE', *, *, #12239, .F. ) ;
#145793 = STYLED_ITEM ( 'NONE', ( #100224 ), #107560 ) ;
#145795 = ORIENTED_EDGE ( 'NONE', *, *, #156509, .F. ) ;
#145796 = ORIENTED_EDGE ( 'NONE', *, *, #77058, .T. ) ;
#145797 = DIRECTION ( 'NONE',  ( 0.000000000000000000, 0.000000000000000000, 1.000000000000000000 ) ) ;
#145798 = FACE_OUTER_BOUND ( 'NONE', #112006, .T. ) ;
#145799 = CARTESIAN_POINT ( 'NONE',  ( 21.14999999999999858, 8.786607556611267356, -45.75000000000000711 ) ) ;
#145800 = FACE_OUTER_BOUND ( 'NONE', #4724, .T. ) ;
#145801 = DIRECTION ( 'NONE',  ( -2.827886303505248766E-16, 0.7397890806274223241, 0.6728388485993012091 ) ) ;
#145802 = EDGE_CURVE ( 'NONE', #87344, #235293, #207811, .T. ) ;
#145804 = DIRECTION ( 'NONE',  ( 1.000000000000000000, -0.000000000000000000, -0.000000000000000000 ) ) ;
#145803 = CARTESIAN_POINT ( 'NONE',  ( -18.40000000000000213, 11.47316190337362940, -113.1085786437627263 ) ) ;
#145806 = ORIENTED_EDGE ( 'NONE', *, *, #151671, .F. ) ;
#145805 = DIRECTION ( 'NONE',  ( 1.000000000000000000, -0.000000000000000000, -0.000000000000000000 ) ) ;
#145807 = CARTESIAN_POINT ( 'NONE',  ( 21.05000000000000071, 5.850000000011105428, -144.1324972242779836 ) ) ;
#145808 = VERTEX_POINT ( 'NONE', #27826 ) ;
#145809 = DIRECTION ( 'NONE',  ( -0.000000000000000000, 0.1350103645451626311, 0.9908441862701635738 ) ) ;
#145810 = ORIENTED_EDGE ( 'NONE', *, *, #193771, .F. ) ;
#145811 = ORIENTED_EDGE ( 'NONE', *, *, #81952, .T. ) ;
#145812 = DIRECTION ( 'NONE',  ( -1.000000000000000000, 0.000000000000000000, 0.000000000000000000 ) ) ;
#145813 = CARTESIAN_POINT ( 'NONE',  ( -16.94309007106720344, 9.992226192581140864, -46.10579128255550785 ) ) ;
#145814 = CYLINDRICAL_SURFACE ( 'NONE', #183537, 0.1000000000000055844 ) ;
#145815 = CYLINDRICAL_SURFACE ( 'NONE', #191724, 0.09999999999998898659 ) ;
#145816 = AXIS2_PLACEMENT_3D ( 'NONE', #46647, #148337, #49230 ) ;
#145817 = CIRCLE ( 'NONE', #66725, 0.09999999999999996392 ) ;
#145818 = CARTESIAN_POINT ( 'NONE',  ( 20.94999999999999574, -1.162701749938009677, -8.099999999999999645 ) ) ;
#145819 = ORIENTED_EDGE ( 'NONE', *, *, #111258, .T. ) ;
#145820 = ORIENTED_EDGE ( 'NONE', *, *, #141251, .F. ) ;
#145821 = CARTESIAN_POINT ( 'NONE',  ( -16.94445028196807002, 9.992063609708893068, -188.3926698215815350 ) ) ;
#145822 = ORIENTED_EDGE ( 'NONE', *, *, #446, .T. ) ;
#145823 = DIRECTION ( 'NONE',  ( -4.408576920032447355E-17, -0.8096735173027155286, 0.5868805631290315850 ) ) ;
#145824 = DIRECTION ( 'NONE',  ( 0.000000000000000000, 0.000000000000000000, 1.000000000000000000 ) ) ;
#145825 = DIRECTION ( 'NONE',  ( 0.000000000000000000, -0.03803313543129139412, 0.9992764785629977276 ) ) ;
#145826 = DIRECTION ( 'NONE',  ( 0.000000000000000000, -0.8700118002898359348, 0.4930308989875165082 ) ) ;
#145827 = LINE ( 'NONE', #44191, #57158 ) ;
#145828 = CARTESIAN_POINT ( 'NONE',  ( 23.40000000000005187, 77.83551161375991967, -47.52760213295649550 ) ) ;
#145829 = ORIENTED_EDGE ( 'NONE', *, *, #190744, .F. ) ;
#145830 = DIRECTION ( 'NONE',  ( 0.000000000000000000, 0.000000000000000000, 1.000000000000000000 ) ) ;
#145831 = DIRECTION ( 'NONE',  ( 0.000000000000000000, 0.8660254037844411501, 0.4999999999999956701 ) ) ;
#145832 = LINE ( 'NONE', #225366, #83396 ) ;
#145833 = CARTESIAN_POINT ( 'NONE',  ( -18.50000000000000000, 13.96869538424788004, -210.3925794786332233 ) ) ;
#145834 = CIRCLE ( 'NONE', #20976, 11.79999999999999716 ) ;
#145835 = CIRCLE ( 'NONE', #200012, 0.09999999999999031886 ) ;
#145836 = CARTESIAN_POINT ( 'NONE',  ( -18.40000000000000213, 8.822561741677553471, -91.25000000000005684 ) ) ;
#145837 = CIRCLE ( 'NONE', #220685, 12.87499999999999822 ) ;
#145838 = VECTOR ( 'NONE', #67565, 1000.000000000000000 ) ;
#145839 = DIRECTION ( 'NONE',  ( 0.000000000000000000, -4.336808689942043768E-15, 1.000000000000000000 ) ) ;
#145840 = EDGE_CURVE ( 'NONE', #133804, #96700, #103450, .T. ) ;
#145841 = EDGE_LOOP ( 'NONE', ( #46076, #204494, #142895, #227552 ) ) ;
#145842 = AXIS2_PLACEMENT_3D ( 'NONE', #255182, #14084, #154895 ) ;
#145843 = CARTESIAN_POINT ( 'NONE',  ( -21.07016717456945898, 69.67905916191187998, -136.5231074845243597 ) ) ;
#145844 = VERTEX_POINT ( 'NONE', #242976 ) ;
#145845 = ADVANCED_FACE ( 'NONE', ( #47331 ), #168643, .F. ) ;
#145846 = CARTESIAN_POINT ( 'NONE',  ( 21.14999999999999858, 87.75000000001186606, -90.77310748452423184 ) ) ;
#145847 = LINE ( 'NONE', #46747, #152208 ) ;
#145848 = CARTESIAN_POINT ( 'NONE',  ( 20.97462148592295961, 61.87364552196481782, -221.7047524508823528 ) ) ;
#145849 = AXIS2_PLACEMENT_3D ( 'NONE', #47704, #166417, #225048 ) ;
#145850 = ORIENTED_EDGE ( 'NONE', *, *, #229524, .T. ) ;
#145852 = VECTOR ( 'NONE', #90605, 1000.000000000000000 ) ;
#145851 = CARTESIAN_POINT ( 'NONE',  ( 23.14999999999999858, 6.650000000011155876, -179.8499999999999943 ) ) ;
#145853 = ADVANCED_FACE ( 'NONE', ( #85155 ), #44789, .F. ) ;
#145854 = EDGE_CURVE ( 'NONE', #58814, #106717, #191240, .T. ) ;
#145855 = DIRECTION ( 'NONE',  ( -3.440080580676165868E-14, 0.9579639084728162057, 0.2868887416115976086 ) ) ;
#145856 = CARTESIAN_POINT ( 'NONE',  ( 21.05000000000005400, 87.75000000001119815, -51.02310748452479316 ) ) ;
#145857 = CARTESIAN_POINT ( 'NONE',  ( -21.10257677756356998, 69.60161825747967157, -170.0480582340924514 ) ) ;
#145858 = CARTESIAN_POINT ( 'NONE',  ( 22.48508240969612615, 75.95372358549553837, -181.6731182160979188 ) ) ;
#145859 = ORIENTED_EDGE ( 'NONE', *, *, #4667, .F. ) ;
#145860 = ORIENTED_EDGE ( 'NONE', *, *, #84730, .T. ) ;
#145861 = CARTESIAN_POINT ( 'NONE',  ( -23.25000000000000000, -1.149570369564537842, -108.3159124845020074 ) ) ;
#145863 = ORIENTED_EDGE ( 'NONE', *, *, #182879, .T. ) ;
#145862 = CARTESIAN_POINT ( 'NONE',  ( 21.05000000000000071, 4.999999999999997335, -21.59473398108690390 ) ) ;
#145864 = DIRECTION ( 'NONE',  ( 0.000000000000000000, 0.5000000000000128786, 0.8660254037844311581 ) ) ;
#145865 = ADVANCED_FACE ( 'NONE', ( #43510 ), #125600, .F. ) ;
#145866 = CARTESIAN_POINT ( 'NONE',  ( -23.15000000000000213, 1.115600667400684642E-11, -167.4999999999999716 ) ) ;
#145867 = ADVANCED_FACE ( 'NONE', ( #89038 ), #23960, .F. ) ;
#145868 = ORIENTED_EDGE ( 'NONE', *, *, #14638, .T. ) ;
#145869 = CYLINDRICAL_SURFACE ( 'NONE', #88882, 0.09999999999999939493 ) ;
#145870 = EDGE_CURVE ( 'NONE', #49052, #173202, #33047, .T. ) ;
#145871 = DIRECTION ( 'NONE',  ( 1.000000000000000000, 0.000000000000000000, 0.000000000000000000 ) ) ;
#145872 = ORIENTED_EDGE ( 'NONE', *, *, #115883, .F. ) ;
#145873 = CARTESIAN_POINT ( 'NONE',  ( -18.59999999999999787, 77.63717271298298783, -191.9409541190523214 ) ) ;
#145874 = VECTOR ( 'NONE', #136007, 1000.000000000000114 ) ;
#145875 = EDGE_CURVE ( 'NONE', #4110, #131063, #143871, .T. ) ;
#145876 = EDGE_LOOP ( 'NONE', ( #13713, #200218, #26307, #121273 ) ) ;
#145877 = EDGE_CURVE ( 'NONE', #245302, #89895, #245393, .T. ) ;
#145878 = AXIS2_PLACEMENT_3D ( 'NONE', #110546, #227937, #210941 ) ;
#145879 = ORIENTED_EDGE ( 'NONE', *, *, #138964, .F. ) ;
#145880 = EDGE_CURVE ( 'NONE', #24943, #236296, #4359, .T. ) ;
#145881 = CARTESIAN_POINT ( 'NONE',  ( 21.05000000000000071, 10.72371710471868056, -74.66491356908764487 ) ) ;
#145882 = ADVANCED_FACE ( 'NONE', ( #26524 ), #12352, .F. ) ;
#145883 = CARTESIAN_POINT ( 'NONE',  ( 18.59999999999999076, 1.750000000011155743, -179.1695115579016147 ) ) ;
#145884 = DIRECTION ( 'NONE',  ( 0.000000000000000000, 0.000000000000000000, 1.000000000000000000 ) ) ;
#145885 = DIRECTION ( 'NONE',  ( -1.000000000000000000, 0.000000000000000000, 0.000000000000000000 ) ) ;
#145886 = CARTESIAN_POINT ( 'NONE',  ( 21.05000000000000071, 1.148907358139439339E-11, -201.0000000000015064 ) ) ;
#145887 = DIRECTION ( 'NONE',  ( 0.000000000000000000, -6.467318590049456648E-15, 1.000000000000000000 ) ) ;
#145888 = CARTESIAN_POINT ( 'NONE',  ( -18.40000000000000213, 9.957490673325212427, -220.1701168356097469 ) ) ;
#145890 = CARTESIAN_POINT ( 'NONE',  ( 21.05000000000000071, 1.115600667400684642E-11, -167.5000000000000284 ) ) ;
#145889 = DIRECTION ( 'NONE',  ( 1.000000000000000000, -1.186688945009009831E-16, -8.286604613020806758E-31 ) ) ;
#145891 = DIRECTION ( 'NONE',  ( 1.000000000000000000, -0.000000000000000000, -0.000000000000000000 ) ) ;
#145892 = CARTESIAN_POINT ( 'NONE',  ( 18.39999999999999147, 61.13752757784637026, -224.6182967272386009 ) ) ;
#145893 = CARTESIAN_POINT ( 'NONE',  ( -20.90000000000000213, -1.212568896937008089, -8.000000000000000000 ) ) ;
#145894 = CIRCLE ( 'NONE', #179247, 0.09999999999999939493 ) ;
#145895 = ORIENTED_EDGE ( 'NONE', *, *, #174213, .T. ) ;
#145896 = ORIENTED_EDGE ( 'NONE', *, *, #149060, .T. ) ;
#145897 = CARTESIAN_POINT ( 'NONE',  ( -20.15000000000000568, 66.70857864377498458, -157.7731074845244166 ) ) ;
#145898 = AXIS2_PLACEMENT_3D ( 'NONE', #175485, #254935, #58060 ) ;
#145899 = DIRECTION ( 'NONE',  ( 0.000000000000000000, 0.8103668758649577031, -0.5859227990963212784 ) ) ;
#145901 = CARTESIAN_POINT ( 'NONE',  ( -20.54999999999999716, 4.350000000011156054, -188.6499999999999488 ) ) ;
#145900 = CYLINDRICAL_SURFACE ( 'NONE', #246320, 0.09999999999998898659 ) ;
#145902 = ADVANCED_FACE ( 'NONE', ( #184287 ), #207732, .T. ) ;
#145903 = CONICAL_SURFACE ( 'NONE', #179257, 6.250000000000005329, 0.7853981633974431720 ) ;
#145904 = DIRECTION ( 'NONE',  ( 1.000000000000000000, 0.000000000000000000, 0.000000000000000000 ) ) ;
#145906 = ADVANCED_FACE ( 'NONE', ( #188156 ), #5628, .F. ) ;
#145905 = FACE_OUTER_BOUND ( 'NONE', #64295, .T. ) ;
#145907 = CARTESIAN_POINT ( 'NONE',  ( -21.93642651522410247, 7.159341611308074782, -199.4407717320839879 ) ) ;
#145908 = AXIS2_PLACEMENT_3D ( 'NONE', #69548, #192066, #13418 ) ;
#145909 = VERTEX_POINT ( 'NONE', #202576 ) ;
#145910 = AXIS2_PLACEMENT_3D ( 'NONE', #247609, #75419, #96223 ) ;
#145911 = VERTEX_POINT ( 'NONE', #223404 ) ;
#145912 = ADVANCED_FACE ( 'NONE', ( #166044 ), #49916, .F. ) ;
#145913 = CARTESIAN_POINT ( 'NONE',  ( 23.25000000000000000, 87.75000000001216449, -139.6231074845242688 ) ) ;
#145914 = ORIENTED_EDGE ( 'NONE', *, *, #242505, .F. ) ;
#145915 = AXIS2_PLACEMENT_3D ( 'NONE', #59553, #21768, #179563 ) ;
#145916 = AXIS2_PLACEMENT_3D ( 'NONE', #244105, #224544, #83715 ) ;
#145918 = VECTOR ( 'NONE', #136857, 1000.000000000000000 ) ;
#145917 = CARTESIAN_POINT ( 'NONE',  ( 18.59999996954842771, 85.52320413787028031, -29.14006577260792596 ) ) ;
#145919 = VECTOR ( 'NONE', #147738, 1000.000000000000000 ) ;
#145920 = AXIS2_PLACEMENT_3D ( 'NONE', #229840, #51169, #208990 ) ;
#145921 = ORIENTED_EDGE ( 'NONE', *, *, #106560, .F. ) ;
#145922 = DIRECTION ( 'NONE',  ( -0.000000000000000000, 0.6046243595031743912, 0.7965107556683563850 ) ) ;
#145923 = ORIENTED_EDGE ( 'NONE', *, *, #121322, .F. ) ;
#145924 = DIRECTION ( 'NONE',  ( -1.000000000000000000, 0.000000000000000000, 0.000000000000000000 ) ) ;
#145925 = DIRECTION ( 'NONE',  ( 0.000000000000000000, -0.4999999999999088507, -0.8660254037844913322 ) ) ;
#145926 = ADVANCED_FACE ( 'NONE', ( #126896 ), #116395, .F. ) ;
#145927 = DIRECTION ( 'NONE',  ( -1.000000000000000000, 0.000000000000000000, 0.000000000000000000 ) ) ;
#145928 = DIRECTION ( 'NONE',  ( 1.000000000000000000, 0.000000000000000000, 0.000000000000000000 ) ) ;
#145929 = TOROIDAL_SURFACE ( 'NONE', #200113, 0.2000000000000000111, 0.1000000000000000056 ) ;
#145930 = CARTESIAN_POINT ( 'NONE',  ( -17.11825945287481332, 10.04999999999998295, -20.85000000000000142 ) ) ;
#145931 = DIRECTION ( 'NONE',  ( 0.000000000000000000, -0.4999999999999929501, -0.8660254037844427044 ) ) ;
#145932 = CARTESIAN_POINT ( 'NONE',  ( -21.65000000000000213, 51.52760218553059701, -231.9873527057832234 ) ) ;
#145933 = ADVANCED_FACE ( 'NONE', ( #14682 ), #13375, .T. ) ;
#145935 = VERTEX_POINT ( 'NONE', #34247 ) ;
#145934 = SPHERICAL_SURFACE ( 'NONE', #181822, 0.1000000000000000056 ) ;
#145937 = DIRECTION ( 'NONE',  ( 1.000000000000000000, 0.000000000000000000, 0.000000000000000000 ) ) ;
#145936 = CARTESIAN_POINT ( 'NONE',  ( -20.94999999999999929, -1.164121893230052995, -208.9148480855715775 ) ) ;
#145938 = VERTEX_POINT ( 'NONE', #208995 ) ;
#145940 = ORIENTED_EDGE ( 'NONE', *, *, #125439, .F. ) ;
#145939 = CYLINDRICAL_SURFACE ( 'NONE', #69291, 0.09999999999999939493 ) ;
#145941 = VERTEX_POINT ( 'NONE', #12107 ) ;
#145942 = DIRECTION ( 'NONE',  ( 1.000000000000000000, 0.000000000000000000, 0.000000000000000000 ) ) ;
#145943 = DIRECTION ( 'NONE',  ( 1.000000000000000000, 0.000000000000000000, 0.000000000000000000 ) ) ;
#145944 = EDGE_CURVE ( 'NONE', #10839, #40972, #99778, .T. ) ;
#145945 = EDGE_CURVE ( 'NONE', #113101, #96338, #112481, .T. ) ;
#145946 = CARTESIAN_POINT ( 'NONE',  ( 21.04999999999999716, 1.115141236730093910E-11, -127.4593430482987912 ) ) ;
#145947 = DIRECTION ( 'NONE',  ( 0.000000000000000000, 0.4721928772776973204, 0.8814952561688629284 ) ) ;
#145948 = CARTESIAN_POINT ( 'NONE',  ( -23.15000000000000213, 1.115600667400684642E-11, -167.4999999999999716 ) ) ;
#145949 = ADVANCED_FACE ( 'NONE', ( #249419 ), #91451, .F. ) ;
#145950 = DIRECTION ( 'NONE',  ( 0.000000000000000000, -6.938893903907222067E-15, 1.000000000000000000 ) ) ;
#145951 = AXIS2_PLACEMENT_3D ( 'NONE', #125187, #186446, #48201 ) ;
#145952 = CARTESIAN_POINT ( 'NONE',  ( 23.40000000000005542, 83.97335046823651794, -34.66234602115918051 ) ) ;
#145953 = CIRCLE ( 'NONE', #208347, 4.300000000000025580 ) ;
#145954 = CYLINDRICAL_SURFACE ( 'NONE', #39378, 0.09999999999999939493 ) ;
#145955 = ORIENTED_EDGE ( 'NONE', *, *, #7854, .F. ) ;
#145956 = EDGE_LOOP ( 'NONE', ( #108501, #19075, #96911, #69050 ) ) ;
#145957 = CARTESIAN_POINT ( 'NONE',  ( 23.15000000000000213, -11.74999999998883737, -54.85000000000000142 ) ) ;
#145958 = CIRCLE ( 'NONE', #162560, 0.1000000000000001860 ) ;
#145959 = ADVANCED_FACE ( 'NONE', ( #109881 ), #172494, .T. ) ;
#145960 = ORIENTED_EDGE ( 'NONE', *, *, #210429, .F. ) ;
#145961 = CARTESIAN_POINT ( 'NONE',  ( -20.64999999999999858, 7.150000000011155876, -146.3500000000000227 ) ) ;
#145963 = ADVANCED_FACE ( 'NONE', ( #192027 ), #91618, .T. ) ;
#145962 = ORIENTED_EDGE ( 'NONE', *, *, #123182, .F. ) ;
#145964 = DIRECTION ( 'NONE',  ( 0.000000000000000000, 0.2262561206234166566, 0.9740678456249555195 ) ) ;
#145965 = AXIS2_PLACEMENT_3D ( 'NONE', #200658, #161546, #241084 ) ;
#145966 = CARTESIAN_POINT ( 'NONE',  ( 19.75857864376269291, 11.75000000000000533, -24.75000000000000000 ) ) ;
#145967 = DIRECTION ( 'NONE',  ( 0.000000000000000000, 0.9126074666063783702, 0.4088369013363252757 ) ) ;
#145968 = ADVANCED_FACE ( 'NONE', ( #232438 ), #94173, .T. ) ;
#145969 = DIRECTION ( 'NONE',  ( 0.000000000000000000, 0.2617529984165030132, 0.9651348961777158619 ) ) ;
#145970 = CARTESIAN_POINT ( 'NONE',  ( 21.05000000000000071, 10.72371710471867701, -179.6499999999999773 ) ) ;
#145971 = ORIENTED_EDGE ( 'NONE', *, *, #184376, .F. ) ;
#145972 = CARTESIAN_POINT ( 'NONE',  ( 20.94999999999999574, 79.38304387823771435, -235.9388060597213723 ) ) ;
#145973 = AXIS2_PLACEMENT_3D ( 'NONE', #128129, #148991, #46007 ) ;
#145974 = CARTESIAN_POINT ( 'NONE',  ( -17.11825945287481332, 51.57797924205760864, -231.8552082689889460 ) ) ;
#145975 = CARTESIAN_POINT ( 'NONE',  ( 18.39999999999999858, 85.50000000001161027, -62.49103808782459879 ) ) ;
#145976 = CARTESIAN_POINT ( 'NONE',  ( -21.05000000000000071, 74.63912941282058000, -195.4501095574334215 ) ) ;
#145978 = EDGE_LOOP ( 'NONE', ( #6300, #140155, #256732, #250613 ) ) ;
#145977 = EDGE_CURVE ( 'NONE', #123203, #93557, #124764, .T. ) ;
#145981 = DIRECTION ( 'NONE',  ( 1.000000000000000000, 0.000000000000000000, 0.000000000000000000 ) ) ;
#145980 = CARTESIAN_POINT ( 'NONE',  ( 21.09316766718128022, 61.07293998390336753, -234.2256142562819718 ) ) ;
#145979 = AXIS2_PLACEMENT_3D ( 'NONE', #226953, #88697, #48312 ) ;
#145982 = EDGE_LOOP ( 'NONE', ( #89900, #252452, #64964, #203908 ) ) ;
#145985 = VERTEX_POINT ( 'NONE', #111185 ) ;
#145984 = LINE ( 'NONE', #61326, #8932 ) ;
#145983 = CARTESIAN_POINT ( 'NONE',  ( 21.14999999999999858, 69.45934304831071415, -103.0231074845243597 ) ) ;
#145986 = AXIS2_PLACEMENT_3D ( 'NONE', #50523, #210908, #74001 ) ;
#145987 = ORIENTED_EDGE ( 'NONE', *, *, #134984, .F. ) ;
#145988 = CARTESIAN_POINT ( 'NONE',  ( -21.64999999999999858, 68.65000000001157332, -57.17310748452437252 ) ) ;
#145989 = AXIS2_PLACEMENT_3D ( 'NONE', #30971, #110466, #190014 ) ;
#145990 = CARTESIAN_POINT ( 'NONE',  ( -21.05000000000000071, 34.04175893161810507, -243.6660727135796662 ) ) ;
#145991 = EDGE_CURVE ( 'NONE', #26378, #131057, #78929, .T. ) ;
#145992 = FACE_OUTER_BOUND ( 'NONE', #115452, .T. ) ;
#145993 = ORIENTED_EDGE ( 'NONE', *, *, #204991, .T. ) ;
#145994 = DIRECTION ( 'NONE',  ( 0.000000000000000000, 0.9126074666063769270, 0.4088369013363280513 ) ) ;
#145995 = CARTESIAN_POINT ( 'NONE',  ( -20.54999999999999716, 68.85000000001205933, -124.1731074845243370 ) ) ;
#145996 = EDGE_CURVE ( 'NONE', #115380, #143707, #190751, .T. ) ;
#145998 = DIRECTION ( 'NONE',  ( 1.000000000000000000, -3.265361837132813093E-16, -2.280189983783949500E-30 ) ) ;
#145997 = CARTESIAN_POINT ( 'NONE',  ( -20.85000000000000142, 1.115600667400684642E-11, -67.00000000000000000 ) ) ;
#145999 = ADVANCED_FACE ( 'NONE', ( #55036 ), #90315, .T. ) ;
#146001 = ORIENTED_EDGE ( 'NONE', *, *, #158365, .T. ) ;
#146000 = CARTESIAN_POINT ( 'NONE',  ( -18.43569575749026512, 46.91436717984745997, -255.3877622108296634 ) ) ;
#146002 = VECTOR ( 'NONE', #7451, 1000.000000000000000 ) ;
#146003 = ORIENTED_EDGE ( 'NONE', *, *, #89025, .T. ) ;
#146004 = CARTESIAN_POINT ( 'NONE',  ( 19.75857864376268935, 64.25000000001176659, -78.27310748452438816 ) ) ;
#146005 = DIRECTION ( 'NONE',  ( -1.000000000000000000, 0.000000000000000000, 0.000000000000000000 ) ) ;
#146006 = CARTESIAN_POINT ( 'NONE',  ( -23.25000000000000000, 1.115600667400684642E-11, -134.0000000000000284 ) ) ;
#146007 = EDGE_LOOP ( 'NONE', ( #243592, #191781, #40350, #101922, #90815, #46706, #255505, #10765, #53806, #46535, #251030, #161210 ) ) ;
#146008 = LINE ( 'NONE', #87312, #81164 ) ;
#146009 = ORIENTED_EDGE ( 'NONE', *, *, #177127, .T. ) ;
#146010 = CARTESIAN_POINT ( 'NONE',  ( 20.95512820512820440, 18.86447962780959386, -229.9497396848627488 ) ) ;
#146012 = EDGE_CURVE ( 'NONE', #25360, #89072, #214140, .T. ) ;
#146011 = CARTESIAN_POINT ( 'NONE',  ( 20.94999999999999574, 67.23127455305841238, -235.8551265064783991 ) ) ;
#146013 = LINE ( 'NONE', #180030, #26658 ) ;
#146014 = ORIENTED_EDGE ( 'NONE', *, *, #183292, .F. ) ;
#146015 = CARTESIAN_POINT ( 'NONE',  ( -18.40000000000000213, 16.37079970714667354, -222.2530670965321065 ) ) ;
#146016 = CIRCLE ( 'NONE', #250089, 11.90000000000000036 ) ;
#146017 = CIRCLE ( 'NONE', #25417, 7.720710678118663850 ) ;
#146018 = ORIENTED_EDGE ( 'NONE', *, *, #183317, .T. ) ;
#146019 = AXIS2_PLACEMENT_3D ( 'NONE', #200049, #120534, #163486 ) ;
#146020 = DIRECTION ( 'NONE',  ( -1.836970198721029934E-16, 1.000000000000000000, 0.000000000000000000 ) ) ;
#146021 = SPHERICAL_SURFACE ( 'NONE', #81395, 0.1000000000000000056 ) ;
#146022 = ORIENTED_EDGE ( 'NONE', *, *, #178367, .T. ) ;
#146023 = CIRCLE ( 'NONE', #91861, 7.800000000000002487 ) ;
#146024 = VERTEX_POINT ( 'NONE', #115036 ) ;
#146025 = CARTESIAN_POINT ( 'NONE',  ( -23.15000000000000213, 1.925233644859811521, -20.76975646687386501 ) ) ;
#146026 = ADVANCED_FACE ( 'NONE', ( #194603 ), #149043, .T. ) ;
#146027 = ORIENTED_EDGE ( 'NONE', *, *, #127930, .T. ) ;
#146029 = EDGE_LOOP ( 'NONE', ( #181898, #75122, #59083, #175598, #250880, #180831, #121999, #60839, #180764, #217391, #91269, #134313, #248024, #134616 ) ) ;
#146028 = CARTESIAN_POINT ( 'NONE',  ( 23.24999999999997513, 11.75000000001116263, -193.9851942293460070 ) ) ;
#146030 = EDGE_LOOP ( 'NONE', ( #37033, #250218, #96405 ) ) ;
#146031 = CIRCLE ( 'NONE', #75151, 0.09999999999999939493 ) ;
#146033 = ORIENTED_EDGE ( 'NONE', *, *, #234202, .T. ) ;
#146032 = ORIENTED_EDGE ( 'NONE', *, *, #250051, .F. ) ;
#146034 = FACE_OUTER_BOUND ( 'NONE', #200539, .T. ) ;
#146035 = ORIENTED_EDGE ( 'NONE', *, *, #108970, .T. ) ;
#146036 = DIRECTION ( 'NONE',  ( 1.000000000000000000, 0.000000000000000000, 0.000000000000000000 ) ) ;
#146038 = EDGE_CURVE ( 'NONE', #84702, #94226, #112302, .T. ) ;
#146037 = CARTESIAN_POINT ( 'NONE',  ( 21.05000000000000071, 68.22899648672319017, -213.7884437866858889 ) ) ;
#146039 = SPHERICAL_SURFACE ( 'NONE', #63803, 0.1000000000000000056 ) ;
#146040 = CARTESIAN_POINT ( 'NONE',  ( -18.40000000000000213, 11.33174054713631662, -146.6500000000000341 ) ) ;
#146041 = VERTEX_POINT ( 'NONE', #237556 ) ;
#146042 = ORIENTED_EDGE ( 'NONE', *, *, #224924, .T. ) ;
#146043 = DIRECTION ( 'NONE',  ( 0.000000000000000000, 0.000000000000000000, -1.000000000000000000 ) ) ;
#146044 =( BOUNDED_CURVE ( )  B_SPLINE_CURVE ( 3, ( #80977, #45720, #240080, #224354 ),
 .UNSPECIFIED., .F., .F. ) 
 B_SPLINE_CURVE_WITH_KNOTS ( ( 4, 4 ),
 ( 1.570796326794896558, 3.141592653589793116 ),
 .UNSPECIFIED. ) 
 CURVE ( )  GEOMETRIC_REPRESENTATION_ITEM ( )  RATIONAL_B_SPLINE_CURVE ( ( 1.000000000000000000, 0.8047378541243649375, 0.8047378541243649375, 1.000000000000000000 ) ) 
 REPRESENTATION_ITEM ( '' )  );
#146046 = VERTEX_POINT ( 'NONE', #178901 ) ;
#146045 = CARTESIAN_POINT ( 'NONE',  ( 18.49999999999999289, 63.74705046376995199, -209.1848118361201330 ) ) ;
#146047 = CARTESIAN_POINT ( 'NONE',  ( -16.77828822508139694, 9.946229374931901290, -180.1626282513739170 ) ) ;
#146049 = VERTEX_POINT ( 'NONE', #77183 ) ;
#146048 = DIRECTION ( 'NONE',  ( 4.026293107431335996E-15, -0.9550021345545530727, 0.2965989261549131228 ) ) ;
#146050 = TOROIDAL_SURFACE ( 'NONE', #179391, 0.2000000000000000111, 0.1000000000000000056 ) ;
#146051 = ORIENTED_EDGE ( 'NONE', *, *, #147731, .F. ) ;
#146052 = CARTESIAN_POINT ( 'NONE',  ( 18.59999999999999076, 6.450000000000001066, -21.15000000000000213 ) ) ;
#146053 = CIRCLE ( 'NONE', #250124, 11.90000000000000746 ) ;
#146054 = ORIENTED_EDGE ( 'NONE', *, *, #125324, .T. ) ;
#146055 = EDGE_LOOP ( 'NONE', ( #35336, #122790, #174542, #160164 ) ) ;
#146057 = AXIS2_PLACEMENT_3D ( 'NONE', #25102, #241551, #26366 ) ;
#146056 = CARTESIAN_POINT ( 'NONE',  ( 20.94999999999999929, 11.65000000001115943, -194.2161343370218560 ) ) ;
#146058 = DIRECTION ( 'NONE',  ( -0.000000000000000000, -0.8660254037844420383, 0.4999999999999943379 ) ) ;
#146060 = ORIENTED_EDGE ( 'NONE', *, *, #59916, .T. ) ;
#146059 = ORIENTED_EDGE ( 'NONE', *, *, #153106, .F. ) ;
#146061 = ORIENTED_EDGE ( 'NONE', *, *, #29726, .T. ) ;
#146062 = CARTESIAN_POINT ( 'NONE',  ( -20.54999999999999716, 1.115600667400684642E-11, -134.0000000000000000 ) ) ;
#146063 = ORIENTED_EDGE ( 'NONE', *, *, #200680, .F. ) ;
#146064 = EDGE_LOOP ( 'NONE', ( #133170, #223014, #72658, #136310 ) ) ;
#146065 = CARTESIAN_POINT ( 'NONE',  ( 23.14999999999999858, 70.50000000001151079, -48.42837350343745584 ) ) ;
#146066 = AXIS2_PLACEMENT_3D ( 'NONE', #247840, #207445, #91349 ) ;
#146068 = ORIENTED_EDGE ( 'NONE', *, *, #171361, .F. ) ;
#146067 = DIRECTION ( 'NONE',  ( 0.000000000000000000, -7.172728831056617961E-15, 1.000000000000000000 ) ) ;
#146069 = LINE ( 'NONE', #161822, #198093 ) ;
#146071 = LINE ( 'NONE', #41873, #69247 ) ;
#146070 = FACE_OUTER_BOUND ( 'NONE', #79228, .T. ) ;
#146072 = CARTESIAN_POINT ( 'NONE',  ( 18.52165635395186172, 85.48115071129494424, -196.4982699016619563 ) ) ;
#146073 = CARTESIAN_POINT ( 'NONE',  ( 20.94999999999999929, 76.00000000001244871, -170.0231074845243597 ) ) ;
#146074 = VERTEX_POINT ( 'NONE', #60187 ) ;
#146075 = EDGE_CURVE ( 'NONE', #588, #42521, #19806, .T. ) ;
#146076 = VERTEX_POINT ( 'NONE', #117603 ) ;
#146077 = DIRECTION ( 'NONE',  ( -1.000000000000000000, -1.836970198721029934E-16, 0.000000000000000000 ) ) ;
#146078 = DIRECTION ( 'NONE',  ( 0.000000000000000000, 0.2128009952263601179, -0.9770955615653315052 ) ) ;
#146080 = ORIENTED_EDGE ( 'NONE', *, *, #205978, .T. ) ;
#146079 = AXIS2_PLACEMENT_3D ( 'NONE', #238276, #59616, #253990 ) ;
#146081 = VECTOR ( 'NONE', #155312, 1000.000000000000000 ) ;
#146082 = VECTOR ( 'NONE', #216824, 1000.000000000000000 ) ;
#146083 = CARTESIAN_POINT ( 'NONE',  ( -23.15000000000000213, 1.115600667400684642E-11, -134.0000000000000000 ) ) ;
#146084 = VERTEX_POINT ( 'NONE', #199732 ) ;
#146085 = ORIENTED_EDGE ( 'NONE', *, *, #55285, .T. ) ;
#146086 = CIRCLE ( 'NONE', #233592, 0.1000000000000028644 ) ;
#146087 = EDGE_CURVE ( 'NONE', #169204, #40901, #56325, .T. ) ;
#146088 = CARTESIAN_POINT ( 'NONE',  ( -21.12844524849339223, 64.25000000001264766, -196.6186940136820169 ) ) ;
#146089 = FACE_OUTER_BOUND ( 'NONE', #222506, .T. ) ;
#146090 = ORIENTED_EDGE ( 'NONE', *, *, #211550, .T. ) ;
#146091 = CARTESIAN_POINT ( 'NONE',  ( 23.14999999999999858, 71.00000000001205080, -124.1178414656112352 ) ) ;
#146092 = DIRECTION ( 'NONE',  ( 0.000000000000000000, 0.2605042016806672911, -0.9654727137038716656 ) ) ;
#146093 = VERTEX_POINT ( 'NONE', #99297 ) ;
#146094 = VECTOR ( 'NONE', #152186, 1000.000000000000000 ) ;
#146096 = B_SPLINE_CURVE_WITH_KNOTS ( 'NONE', 3,
 ( #126172, #27124, #106600, #239727, #61073, #140607, #21968, #101437, #229149, #152199, #127473, #92186, #210863 ),
 .UNSPECIFIED., .F., .F.,
 ( 4, 3, 3, 3, 4 ),
 ( 1.110900444313928445E-16, 1.946463881814531607E-05, 3.922356109944008404E-05, 4.215060953238765177E-05, 4.415117091092261940E-05 ),
 .UNSPECIFIED. ) ;
#146095 = CARTESIAN_POINT ( 'NONE',  ( 19.97071067811865674, 64.27928932189354327, -145.3731074845244109 ) ) ;
#146098 = AXIS2_PLACEMENT_3D ( 'NONE', #179338, #196299, #22837 ) ;
#146097 = DIRECTION ( 'NONE',  ( 0.000000000000000000, 0.4088369013363281623, -0.9126074666063771490 ) ) ;
#146100 = DIRECTION ( 'NONE',  ( 1.000000000000000000, 0.000000000000000000, 0.000000000000000000 ) ) ;
#146099 = LINE ( 'NONE', #69163, #198645 ) ;
#146101 = EDGE_CURVE ( 'NONE', #170976, #57537, #54016, .T. ) ;
#146102 = LINE ( 'NONE', #204781, #119053 ) ;
#146103 = CARTESIAN_POINT ( 'NONE',  ( -20.65000000000000568, 68.75000000001159606, -56.87310748452436826 ) ) ;
#146104 = CARTESIAN_POINT ( 'NONE',  ( 18.47654891039378455, -9.465274948371156682, -174.6259759051946219 ) ) ;
#146105 = DIRECTION ( 'NONE',  ( 0.000000000000000000, 7.056502275159890832E-15, -1.000000000000000000 ) ) ;
#146107 = EDGE_CURVE ( 'NONE', #144289, #188520, #177610, .T. ) ;
#146106 = B_SPLINE_CURVE_WITH_KNOTS ( 'NONE', 3,
 ( #82311, #40694, #84869, #220576, #203574, #21115, #83587, #64061, #43224, #2785, #105726, #182747, #242691, #143599, #146158, #202296, #161907, #100586, #22392 ),
 .UNSPECIFIED., .F., .F.,
 ( 4, 3, 3, 3, 3, 3, 4 ),
 ( 0.000000000000000000, 2.646747978908414649E-05, 5.271166642128387010E-05, 9.008788829884412921E-05, 0.0001426648776560982164, 0.0001897378458659780261, 0.0001917382627806345728 ),
 .UNSPECIFIED. ) ;
#146108 = VERTEX_POINT ( 'NONE', #197128 ) ;
#146109 = AXIS2_PLACEMENT_3D ( 'NONE', #242071, #82969, #102531 ) ;
#146110 = VECTOR ( 'NONE', #168484, 1000.000000000000000 ) ;
#146111 = CIRCLE ( 'NONE', #71116, 4.049999999999998046 ) ;
#146112 = VECTOR ( 'NONE', #162866, 1000.000000000000000 ) ;
#146114 = VERTEX_POINT ( 'NONE', #159319 ) ;
#146113 = ORIENTED_EDGE ( 'NONE', *, *, #100078, .T. ) ;
#146115 = ORIENTED_EDGE ( 'NONE', *, *, #209770, .T. ) ;
#146116 = CARTESIAN_POINT ( 'NONE',  ( 21.14999999999999858, 1.115600667400684642E-11, -93.95934304829877703 ) ) ;
#146117 = FACE_OUTER_BOUND ( 'NONE', #91275, .T. ) ;
#146118 = EDGE_CURVE ( 'NONE', #204695, #12612, #49745, .T. ) ;
#146119 =( BOUNDED_SURFACE ( )  B_SPLINE_SURFACE ( 3, 2, ( 
 ( #10754, #90263, #95422 ),
 ( #94131, #175011, #114984 ),
 ( #34199, #54984, #215362 ),
 ( #113701, #32927, #231105 ),
 ( #13326, #91572, #75859 ),
 ( #92843, #135815, #193248 ) ),
 .UNSPECIFIED., .F., .F., .F. ) 
 B_SPLINE_SURFACE_WITH_KNOTS ( ( 4, 2, 4 ),
 ( 3, 3 ),
 ( 3.141592653589793116, 3.926990816987244948, 4.712388980384696779 ),
 ( 0.000000000000000000, 1.000000000000000000 ),
 .UNSPECIFIED. ) 
 GEOMETRIC_REPRESENTATION_ITEM ( )  RATIONAL_B_SPLINE_SURFACE ( (
 ( 1.000000000000000000, 0.9238795325112884038, 1.000000000000000000),
 ( 1.000000000000000000, 0.9240297172241500601, 1.000000000000000000),
 ( 1.000000000000000000, 0.9038128468041866093, 1.000000000000000000),
 ( 1.000000000000000000, 0.8282379607647167852, 1.000000000000000000),
 ( 1.000000000000000000, 0.7727932973493061297, 1.000000000000000000),
 ( 1.000000000000000000, 0.7071067811865475727, 1.000000000000000000) ) ) 
 REPRESENTATION_ITEM ( '' )  SURFACE ( )  );
#146121 = CARTESIAN_POINT ( 'NONE',  ( -16.91049119928364775, 9.950000000011138823, -146.6182796068091818 ) ) ;
#146120 = CARTESIAN_POINT ( 'NONE',  ( 22.88900146558018989, 67.29609520889972885, -182.6731074845244223 ) ) ;
#146122 = CARTESIAN_POINT ( 'NONE',  ( 21.05000000000000071, 67.07338541492521244, -161.5514244653012952 ) ) ;
#146123 = ORIENTED_EDGE ( 'NONE', *, *, #140077, .F. ) ;
#146124 = LINE ( 'NONE', #148713, #175747 ) ;
#146125 = CARTESIAN_POINT ( 'NONE',  ( -21.05000000000000071, -0.02110330805904066936, 6.304516329263973873 ) ) ;
#146126 = EDGE_CURVE ( 'NONE', #216196, #35027, #40679, .T. ) ;
#146127 = DIRECTION ( 'NONE',  ( 1.000000000000000000, -0.000000000000000000, -0.000000000000000000 ) ) ;
#146128 = CARTESIAN_POINT ( 'NONE',  ( -16.94445028196808778, 66.00793639031455484, -157.4157773061059800 ) ) ;
#146129 = VERTEX_POINT ( 'NONE', #18511 ) ;
#146130 = CARTESIAN_POINT ( 'NONE',  ( -20.85000000000000142, 0.000000000000000000, -33.50000000000000000 ) ) ;
#146131 = CARTESIAN_POINT ( 'NONE',  ( 18.59999999999999076, 18.51199663233068193, -231.2535697180530292 ) ) ;
#146132 = ORIENTED_EDGE ( 'NONE', *, *, #148277, .T. ) ;
#146133 = EDGE_LOOP ( 'NONE', ( #138346, #173880, #137798, #107934 ) ) ;
#146134 = CARTESIAN_POINT ( 'NONE',  ( 19.88284271247461987, 64.30857864377446731, -78.27310748452438816 ) ) ;
#146135 = CARTESIAN_POINT ( 'NONE',  ( 20.04999999999999716, 8.750000000011173285, -146.6500000000000341 ) ) ;
#146136 = CARTESIAN_POINT ( 'NONE',  ( -22.59999999999999787, 76.00000000001165290, -69.52310748452431710 ) ) ;
#146137 = FACE_OUTER_BOUND ( 'NONE', #223210, .T. ) ;
#146138 = CARTESIAN_POINT ( 'NONE',  ( 20.85000000000000142, 77.14957036958777792, -128.7071950000224092 ) ) ;
#146139 = CARTESIAN_POINT ( 'NONE',  ( -21.13435531349809082, 6.493721063592104770, 4.741518362104077497E-16 ) ) ;
#146140 = ORIENTED_EDGE ( 'NONE', *, *, #194888, .T. ) ;
#146141 = DIRECTION ( 'NONE',  ( -1.073024830501117725E-15, -6.982962677686266711E-15, 1.000000000000000000 ) ) ;
#146143 = EDGE_CURVE ( 'NONE', #111006, #253599, #257979, .T. ) ;
#146142 = LINE ( 'NONE', #6632, #237525 ) ;
#146145 = DIRECTION ( 'NONE',  ( 0.000000000000000000, -0.4930308989874729320, -0.8700118002898605818 ) ) ;
#146144 = DIRECTION ( 'NONE',  ( -0.000000000000000000, -0.1350103645451835865, -0.9908441862701606873 ) ) ;
#146146 = CARTESIAN_POINT ( 'NONE',  ( 18.59999999999999076, 74.16465844978819177, -191.9679561919613775 ) ) ;
#146147 = FACE_OUTER_BOUND ( 'NONE', #94086, .T. ) ;
#146148 = CARTESIAN_POINT ( 'NONE',  ( 23.14999999999999858, 73.90000000001190017, -103.0231074845243171 ) ) ;
#146149 = CARTESIAN_POINT ( 'NONE',  ( 23.24999999999999645, 1.115600667400684642E-11, -134.0000000000000000 ) ) ;
#146152 = ORIENTED_EDGE ( 'NONE', *, *, #55266, .F. ) ;
#146151 = AXIS2_PLACEMENT_3D ( 'NONE', #116544, #38292, #39607 ) ;
#146150 = DIRECTION ( 'NONE',  ( -1.000000000000000000, 0.000000000000000000, 0.000000000000000000 ) ) ;
#146153 =( BOUNDED_CURVE ( )  B_SPLINE_CURVE ( 3, ( #164001, #63601, #6188, #162723 ),
 .UNSPECIFIED., .F., .F. ) 
 B_SPLINE_CURVE_WITH_KNOTS ( ( 4, 4 ),
 ( 3.141592653589793116, 4.712388980384689674 ),
 .UNSPECIFIED. ) 
 CURVE ( )  GEOMETRIC_REPRESENTATION_ITEM ( )  RATIONAL_B_SPLINE_CURVE ( ( 1.000000000000000000, 0.8047378541243649375, 0.8047378541243649375, 1.000000000000000000 ) ) 
 REPRESENTATION_ITEM ( '' )  );
#146154 = EDGE_CURVE ( 'NONE', #223354, #113374, #236263, .T. ) ;
#146155 = CIRCLE ( 'NONE', #229566, 0.09999999999999939493 ) ;
#146156 = EDGE_CURVE ( 'NONE', #52860, #20901, #83023, .T. ) ;
#146157 = CARTESIAN_POINT ( 'NONE',  ( -11.59999999999994458, 67.75000000001118394, -23.62310748452479103 ) ) ;
#146158 = CARTESIAN_POINT ( 'NONE',  ( -18.50016250449483479, 65.70233904876970144, -30.54874109119680625 ) ) ;
#146159 = EDGE_CURVE ( 'NONE', #96642, #33467, #199796, .T. ) ;
#146160 = CARTESIAN_POINT ( 'NONE',  ( 14.22821877134046709, 9.456028260519072859, -149.0111980350657745 ) ) ;
#146161 = AXIS2_PLACEMENT_3D ( 'NONE', #136506, #135229, #94829 ) ;
#146162 = ORIENTED_EDGE ( 'NONE', *, *, #118274, .T. ) ;
#146163 = EDGE_CURVE ( 'NONE', #189424, #161055, #239309, .T. ) ;
#146164 = DIRECTION ( 'NONE',  ( 0.000000000000000000, 0.000000000000000000, -1.000000000000000000 ) ) ;
#146165 = DIRECTION ( 'NONE',  ( 0.000000000000000000, -0.4088369013363281068, 0.9126074666063770380 ) ) ;
#146167 = CARTESIAN_POINT ( 'NONE',  ( -20.54999999999999716, -9.499999999988846255, -157.6060308773475924 ) ) ;
#146166 = CIRCLE ( 'NONE', #125336, 0.5999999999999978684 ) ;
#146168 = ORIENTED_EDGE ( 'NONE', *, *, #82528, .F. ) ;
#146169 = CARTESIAN_POINT ( 'NONE',  ( -12.25000000000000178, 66.15000000001204228, -119.7731074845243739 ) ) ;
#146171 = ORIENTED_EDGE ( 'NONE', *, *, #201604, .T. ) ;
#146170 = CARTESIAN_POINT ( 'NONE',  ( -20.85000000000000142, 43.08613539620618837, -254.3146655184800409 ) ) ;
#146173 = DIRECTION ( 'NONE',  ( 1.000000000000000000, 0.000000000000000000, 0.000000000000000000 ) ) ;
#146172 = DIRECTION ( 'NONE',  ( 1.000000000000000000, 0.000000000000000000, -0.000000000000000000 ) ) ;
#146174 = EDGE_CURVE ( 'NONE', #29748, #128048, #121489, .T. ) ;
#146175 = DIRECTION ( 'NONE',  ( 0.000000000000000000, 0.000000000000000000, -1.000000000000000000 ) ) ;
#146176 = ORIENTED_EDGE ( 'NONE', *, *, #252174, .F. ) ;
#146177 = FACE_OUTER_BOUND ( 'NONE', #256688, .T. ) ;
#146178 = EDGE_CURVE ( 'NONE', #92492, #116426, #70629, .T. ) ;
#146179 = CARTESIAN_POINT ( 'NONE',  ( 0.000000000000000000, 0.000000000000000000, 0.000000000000000000 ) ) ;
#146180 = CARTESIAN_POINT ( 'NONE',  ( -20.93975676684922504, 65.68895814178220860, -64.00265578621380769 ) ) ;
#146181 = EDGE_CURVE ( 'NONE', #57243, #31610, #234993, .T. ) ;
#146182 = PLANE ( 'NONE',  #189731 ) ;
#146183 = CARTESIAN_POINT ( 'NONE',  ( 20.94999999999999574, 14.00000000001115730, -105.9270925303825663 ) ) ;
#146184 = CIRCLE ( 'NONE', #112872, 0.09999999999998807065 ) ;
#146185 = EDGE_LOOP ( 'NONE', ( #32261, #175666, #185426, #139908 ) ) ;
#146186 = DIRECTION ( 'NONE',  ( 0.000000000000000000, -0.9908441862701596881, 0.1350103645451904977 ) ) ;
#146187 = CYLINDRICAL_SURFACE ( 'NONE', #9821, 11.75000000000000533 ) ;
#146188 = EDGE_CURVE ( 'NONE', #93761, #242949, #216328, .T. ) ;
#146189 = CARTESIAN_POINT ( 'NONE',  ( 23.15000000000000213, -11.48912529306489816, -197.8999999999999773 ) ) ;
#146190 = ORIENTED_EDGE ( 'NONE', *, *, #4350, .T. ) ;
#146191 = EDGE_LOOP ( 'NONE', ( #208185, #84106, #16401, #182276 ) ) ;
#146192 = EDGE_CURVE ( 'NONE', #236846, #69740, #103881, .T. ) ;
#146193 = LINE ( 'NONE', #108371, #236221 ) ;
#146194 = CARTESIAN_POINT ( 'NONE',  ( -20.54999999999999716, 1.999999999999998224, -13.22462192276210224 ) ) ;
#146195 = CARTESIAN_POINT ( 'NONE',  ( 21.05563370358598263, 13.07117173248338560, -210.6219170696655283 ) ) ;
#146197 = LINE ( 'NONE', #247874, #24404 ) ;
#146196 = CIRCLE ( 'NONE', #221205, 0.2000000000000057288 ) ;
#146198 = CIRCLE ( 'NONE', #62997, 0.09999999999998898659 ) ;
#146199 = LINE ( 'NONE', #144905, #24208 ) ;
#146200 = DIRECTION ( 'NONE',  ( 0.000000000000000000, 0.000000000000000000, -1.000000000000000000 ) ) ;
#146201 = DIRECTION ( 'NONE',  ( -1.000000000000000000, 0.000000000000000000, -0.000000000000000000 ) ) ;
#146202 = CARTESIAN_POINT ( 'NONE',  ( -18.43473496883443374, 46.97092634935879829, -255.3357148657918856 ) ) ;
#146203 = DIRECTION ( 'NONE',  ( 0.000000000000000000, 0.000000000000000000, -1.000000000000000000 ) ) ;
#146205 = ORIENTED_EDGE ( 'NONE', *, *, #55112, .F. ) ;
#146204 = CARTESIAN_POINT ( 'NONE',  ( 15.73863059295127087, 62.65035202501399425, -217.0198313409406978 ) ) ;
#146206 = AXIS2_PLACEMENT_3D ( 'NONE', #56676, #77532, #136217 ) ;
#146207 = DIRECTION ( 'NONE',  ( 0.000000000000000000, 0.000000000000000000, -1.000000000000000000 ) ) ;
#146208 = CARTESIAN_POINT ( 'NONE',  ( 23.14999999999999503, 64.35000000001258513, -191.3731074845244393 ) ) ;
#146210 = LINE ( 'NONE', #105779, #215819 ) ;
#146209 = FACE_OUTER_BOUND ( 'NONE', #163290, .T. ) ;
#146211 = EDGE_CURVE ( 'NONE', #44979, #147959, #141324, .T. ) ;
#146212 = ORIENTED_EDGE ( 'NONE', *, *, #209059, .F. ) ;
#146213 = CARTESIAN_POINT ( 'NONE',  ( 20.85000000000000142, 7.120270961708750512, -171.1595630418393625 ) ) ;
#146215 = EDGE_CURVE ( 'NONE', #145192, #130316, #223113, .T. ) ;
#146214 = CARTESIAN_POINT ( 'NONE',  ( -20.94999999999999929, 70.15000000001252545, -180.1556047088023149 ) ) ;
#146216 = DIRECTION ( 'NONE',  ( -1.000000000000000000, 0.000000000000000000, 0.000000000000000000 ) ) ;
#146217 = CARTESIAN_POINT ( 'NONE',  ( -20.94999999999999929, 1.250000000011155299, -175.4999999999999716 ) ) ;
#146218 = VERTEX_POINT ( 'NONE', #245265 ) ;
#146220 = VERTEX_POINT ( 'NONE', #47032 ) ;
#146219 = CIRCLE ( 'NONE', #200397, 0.09999999999998898659 ) ;
#146222 = ADVANCED_FACE ( 'NONE', ( #167039 ), #142296, .T. ) ;
#146221 = B_SPLINE_CURVE_WITH_KNOTS ( 'NONE', 3,
 ( #183431, #243387, #187291, #169032, #223814, #8639, #84260, #49040, #88133, #167736 ),
 .UNSPECIFIED., .F., .F.,
 ( 4, 3, 3, 4 ),
 ( 1.893216038736613966E-15, 3.877043166999528430E-05, 7.336897548476726920E-05, 7.659383120240106035E-05 ),
 .UNSPECIFIED. ) ;
#146223 = LINE ( 'NONE', #225745, #9377 ) ;
#146224 = ORIENTED_EDGE ( 'NONE', *, *, #28808, .F. ) ;
#146225 = CARTESIAN_POINT ( 'NONE',  ( -22.57320508075687115, 11.65000000001115588, -100.5000000000000568 ) ) ;
#146226 = ORIENTED_EDGE ( 'NONE', *, *, #178612, .F. ) ;
#146227 = CARTESIAN_POINT ( 'NONE',  ( -18.40000000000000213, 64.52683809664929981, -78.84905355133234650 ) ) ;
#146228 = DIRECTION ( 'NONE',  ( 0.000000000000000000, -1.000000000000000000, 0.000000000000000000 ) ) ;
#146229 = DIRECTION ( 'NONE',  ( 0.000000000000000000, 0.8814952561688429444, -0.4721928772777349015 ) ) ;
#146230 = ORIENTED_EDGE ( 'NONE', *, *, #198737, .T. ) ;
#146231 = CIRCLE ( 'NONE', #142147, 0.09999999999998898659 ) ;
#146232 = DIRECTION ( 'NONE',  ( 1.836970198721029934E-16, 0.9651348961777157509, -0.2617529984165031243 ) ) ;
#146233 = CARTESIAN_POINT ( 'NONE',  ( -18.59999999999999787, 2.838478681111047841, -208.5693404029859437 ) ) ;
#146234 = CARTESIAN_POINT ( 'NONE',  ( 20.99749315643149217, 11.75000000001115907, -160.4851942312420761 ) ) ;
#146235 = TOROIDAL_SURFACE ( 'NONE', #225340, 1.900000000000002576, 0.1000000000000000056 ) ;
#146236 = EDGE_CURVE ( 'NONE', #23326, #154058, #221810, .T. ) ;
#146237 = LINE ( 'NONE', #206227, #12484 ) ;
#146238 = CARTESIAN_POINT ( 'NONE',  ( -20.94999999999999929, 64.35000000001190301, -96.00830171387039513 ) ) ;
#146239 = CARTESIAN_POINT ( 'NONE',  ( -23.15000000000000213, -8.663551401858001100, -191.4758988819326646 ) ) ;
#146240 = DIRECTION ( 'NONE',  ( 1.000000000000000000, -0.000000000000000000, 0.000000000000000000 ) ) ;
#146241 = EDGE_CURVE ( 'NONE', #64921, #178236, #44501, .T. ) ;
#146242 = ORIENTED_EDGE ( 'NONE', *, *, #173967, .T. ) ;
#146244 = CARTESIAN_POINT ( 'NONE',  ( 20.94999999999999929, 68.48451787451661232, -224.2224406095231757 ) ) ;
#146243 = DIRECTION ( 'NONE',  ( -1.000000000000000000, 0.000000000000000000, -0.000000000000000000 ) ) ;
#146245 = VERTEX_POINT ( 'NONE', #143587 ) ;
#146247 = VERTEX_POINT ( 'NONE', #82297 ) ;
#146246 = CARTESIAN_POINT ( 'NONE',  ( -23.15000000000000213, -9.000000000000003553, -9.893969122652444881 ) ) ;
#146248 = EDGE_LOOP ( 'NONE', ( #7007, #55998, #55511, #249461 ) ) ;
#146249 = DIRECTION ( 'NONE',  ( 1.000000000000000000, 0.000000000000000000, 0.000000000000000000 ) ) ;
#146250 = CIRCLE ( 'NONE', #54665, 0.6000000000000033085 ) ;
#146251 = CARTESIAN_POINT ( 'NONE',  ( 18.50016250449482413, 10.29766095125186176, -72.47436639332788388 ) ) ;
#146252 = CARTESIAN_POINT ( 'NONE',  ( 18.53691006697109955, 65.69784844286137115, -78.32090876722591588 ) ) ;
#146253 = DIRECTION ( 'NONE',  ( 0.000000000000000000, -6.997203936713171069E-15, 1.000000000000000000 ) ) ;
#146254 = AXIS2_PLACEMENT_3D ( 'NONE', #96445, #234701, #153933 ) ;
#146255 = VERTEX_POINT ( 'NONE', #4070 ) ;
#146256 = EDGE_CURVE ( 'NONE', #113968, #164187, #245572, .T. ) ;
#146257 = SPHERICAL_SURFACE ( 'NONE', #18246, 0.1000000000000000056 ) ;
#146258 = CARTESIAN_POINT ( 'NONE',  ( 18.49999999999999645, 10.28015861706802347, -158.7245720712022319 ) ) ;
#146259 = ADVANCED_FACE ( 'NONE', ( #104431 ), #243965, .F. ) ;
#146260 = EDGE_LOOP ( 'NONE', ( #198856, #69008, #228697, #209197 ) ) ;
#146261 = CIRCLE ( 'NONE', #230033, 0.1000000000000028644 ) ;
#146262 = CARTESIAN_POINT ( 'NONE',  ( -16.94165728009537375, 9.987869755934932314, -154.8910550085101931 ) ) ;
#146263 = ADVANCED_FACE ( 'NONE', ( #65328 ), #66686, .T. ) ;
#146264 = FACE_OUTER_BOUND ( 'NONE', #81941, .T. ) ;
#146265 = AXIS2_PLACEMENT_3D ( 'NONE', #174872, #226096, #189580 ) ;
#146266 = EDGE_LOOP ( 'NONE', ( #54310, #26035, #196726, #135662 ) ) ;
#146267 = CARTESIAN_POINT ( 'NONE',  ( -18.50000000000000000, 11.65000000001115232, -107.5148057706540357 ) ) ;
#146268 = AXIS2_PLACEMENT_3D ( 'NONE', #134106, #190261, #35066 ) ;
#146269 = EDGE_CURVE ( 'NONE', #128506, #178267, #62769, .T. ) ;
#146270 = ORIENTED_EDGE ( 'NONE', *, *, #126757, .F. ) ;
#146271 = CARTESIAN_POINT ( 'NONE',  ( 20.94999999999999929, 70.10000000001149090, -46.24220724918073699 ) ) ;
#146274 = EDGE_CURVE ( 'NONE', #247168, #81511, #48334, .T. ) ;
#146273 = EDGE_CURVE ( 'NONE', #98003, #111790, #124948, .T. ) ;
#146272 = ORIENTED_EDGE ( 'NONE', *, *, #36737, .F. ) ;
#146275 = DIRECTION ( 'NONE',  ( 0.000000000000000000, 0.4721928772776973204, 0.8814952561688629284 ) ) ;
#146276 = AXIS2_PLACEMENT_3D ( 'NONE', #177974, #235351, #174154 ) ;
#146277 = FACE_OUTER_BOUND ( 'NONE', #11388, .T. ) ;
#146278 = DIRECTION ( 'NONE',  ( -0.000000000000000000, -1.000000000000000000, 0.000000000000000000 ) ) ;
#146279 = CIRCLE ( 'NONE', #21413, 4.000000000000003553 ) ;
#146280 = CARTESIAN_POINT ( 'NONE',  ( -22.00356870143295041, 7.088088014903060063, -199.4562900056665455 ) ) ;
#146281 = DIRECTION ( 'NONE',  ( 0.000000000000000000, 0.000000000000000000, 1.000000000000000000 ) ) ;
#146282 = DIRECTION ( 'NONE',  ( -0.000000000000000000, -0.000000000000000000, -1.000000000000000000 ) ) ;
#146283 = EDGE_CURVE ( 'NONE', #227495, #56183, #248526, .T. ) ;
#146286 = EDGE_CURVE ( 'NONE', #97198, #139578, #182702, .T. ) ;
#146285 = DIRECTION ( 'NONE',  ( 1.000000000000000000, -0.000000000000000000, -0.000000000000000000 ) ) ;
#146284 = VECTOR ( 'NONE', #9050, 1000.000000000000000 ) ;
#146287 = AXIS2_PLACEMENT_3D ( 'NONE', #75012, #249771, #213192 ) ;
#146288 = ORIENTED_EDGE ( 'NONE', *, *, #35833, .T. ) ;
#146290 = CARTESIAN_POINT ( 'NONE',  ( -23.25000000000000000, 80.78317333349157536, -192.9003134612049166 ) ) ;
#146289 = CARTESIAN_POINT ( 'NONE',  ( -21.05000000000000071, 69.74115727647316021, -170.0551211777118112 ) ) ;
#146291 = VECTOR ( 'NONE', #59609, 1000.000000000000000 ) ;
#146292 = VERTEX_POINT ( 'NONE', #241415 ) ;
#146293 = DIRECTION ( 'NONE',  ( 0.000000000000000000, 0.9908441862701600211, -0.1350103645451876666 ) ) ;
#146294 = DIRECTION ( 'NONE',  ( -0.000000000000000000, 0.000000000000000000, 1.000000000000000000 ) ) ;
#146295 = EDGE_CURVE ( 'NONE', #163061, #67224, #204035, .T. ) ;
#146296 = DIRECTION ( 'NONE',  ( -1.000000000000000000, 0.000000000000000000, 0.000000000000000000 ) ) ;
#146298 = VERTEX_POINT ( 'NONE', #182731 ) ;
#146297 = CARTESIAN_POINT ( 'NONE',  ( -18.44232395689746085, -9.552282557039976751, -207.8422519848059551 ) ) ;
#146300 = VERTEX_POINT ( 'NONE', #168336 ) ;
#146299 = CARTESIAN_POINT ( 'NONE',  ( 6.000000000000060396, 64.75000000001119815, -26.02310748452479316 ) ) ;
#146301 = DIRECTION ( 'NONE',  ( 1.000000000000000000, 2.952720810173289112E-16, -0.000000000000000000 ) ) ;
#146302 = EDGE_CURVE ( 'NONE', #96628, #226768, #127553, .T. ) ;
#146303 = FACE_OUTER_BOUND ( 'NONE', #46413, .T. ) ;
#146304 = EDGE_CURVE ( 'NONE', #223652, #163056, #95702, .T. ) ;
#146306 = ORIENTED_EDGE ( 'NONE', *, *, #180584, .F. ) ;
#146305 = DIRECTION ( 'NONE',  ( 1.000000000000000000, -0.000000000000000000, -0.000000000000000000 ) ) ;
#146307 = CYLINDRICAL_SURFACE ( 'NONE', #214307, 0.09999999999999939493 ) ;
#146308 = ORIENTED_EDGE ( 'NONE', *, *, #192515, .T. ) ;
#146309 = DIRECTION ( 'NONE',  ( 0.000000000000000000, -3.469446951953635015E-14, 1.000000000000000000 ) ) ;
#146310 = ORIENTED_EDGE ( 'NONE', *, *, #10817, .F. ) ;
#146312 = EDGE_CURVE ( 'NONE', #13982, #177501, #173482, .T. ) ;
#146311 = DIRECTION ( 'NONE',  ( 0.000000000000000000, -0.2617529984165031243, -0.9651348961777157509 ) ) ;
#146313 = CARTESIAN_POINT ( 'NONE',  ( 23.14999999999999503, 69.35000000001180354, -81.67310748452436542 ) ) ;
#146314 = ORIENTED_EDGE ( 'NONE', *, *, #251890, .T. ) ;
#146315 = CYLINDRICAL_SURFACE ( 'NONE', #212433, 11.80000000000000249 ) ;
#146316 = AXIS2_PLACEMENT_3D ( 'NONE', #188382, #248361, #91853 ) ;
#146317 = DIRECTION ( 'NONE',  ( -1.000000000000000000, -0.000000000000000000, -0.000000000000000000 ) ) ;
#146318 = EDGE_CURVE ( 'NONE', #141859, #82762, #50878, .T. ) ;
#146319 = ORIENTED_EDGE ( 'NONE', *, *, #102568, .F. ) ;
#146320 = DIRECTION ( 'NONE',  ( -3.469446951953605354E-14, 1.000000000000000000, 0.000000000000000000 ) ) ;
#146322 = ORIENTED_EDGE ( 'NONE', *, *, #234840, .T. ) ;
#146321 = AXIS2_PLACEMENT_3D ( 'NONE', #531, #218283, #60498 ) ;
#146323 = ORIENTED_EDGE ( 'NONE', *, *, #76682, .T. ) ;
#146324 = CARTESIAN_POINT ( 'NONE',  ( -18.37151313414709008, -9.571014125767069558, -73.81666290923895701 ) ) ;
#146325 = ORIENTED_EDGE ( 'NONE', *, *, #108841, .F. ) ;
#146327 = ADVANCED_FACE ( 'NONE', ( #252943 ), #33962, .T. ) ;
#146326 = CARTESIAN_POINT ( 'NONE',  ( -16.87372386987899020, 23.38540140777922716, -231.2319906532857203 ) ) ;
#146328 = ORIENTED_EDGE ( 'NONE', *, *, #94918, .F. ) ;
#146330 = ORIENTED_EDGE ( 'NONE', *, *, #113753, .T. ) ;
#146329 = CARTESIAN_POINT ( 'NONE',  ( 6.100000000000060929, 64.25000000001119815, -25.92310748452479174 ) ) ;
#146331 = DIRECTION ( 'NONE',  ( 1.000000000000000000, 0.000000000000000000, 0.000000000000000000 ) ) ;
#146332 = ORIENTED_EDGE ( 'NONE', *, *, #199109, .T. ) ;
#146333 = DIRECTION ( 'NONE',  ( 1.000000000000000000, 0.000000000000000000, 0.000000000000000000 ) ) ;
#146334 = ORIENTED_EDGE ( 'NONE', *, *, #170199, .F. ) ;
#146336 = VERTEX_POINT ( 'NONE', #133024 ) ;
#146335 = VERTEX_POINT ( 'NONE', #54748 ) ;
#146337 = DIRECTION ( 'NONE',  ( 1.000000000000000000, 0.000000000000000000, 0.000000000000000000 ) ) ;
#146338 = CARTESIAN_POINT ( 'NONE',  ( -20.54999999999999716, 81.91411460262999356, -215.0718681741873013 ) ) ;
#146339 = CIRCLE ( 'NONE', #167236, 0.1000000000000096922 ) ;
#146340 = ORIENTED_EDGE ( 'NONE', *, *, #44655, .T. ) ;
#146341 = AXIS2_PLACEMENT_3D ( 'NONE', #155760, #189720, #249695 ) ;
#146342 = TOROIDAL_SURFACE ( 'NONE', #200524, 12.97499999999999609, 0.1000000000000000056 ) ;
#146343 = ORIENTED_EDGE ( 'NONE', *, *, #34109, .T. ) ;
#146344 = DIRECTION ( 'NONE',  ( -1.000000000000000000, 0.000000000000000000, 0.000000000000000000 ) ) ;
#146345 = DIRECTION ( 'NONE',  ( 0.000000000000000000, 1.000000000000000000, 0.000000000000000000 ) ) ;
#146347 = ORIENTED_EDGE ( 'NONE', *, *, #112902, .F. ) ;
#146346 = DIRECTION ( 'NONE',  ( 1.000000000000000000, -0.000000000000000000, -0.000000000000000000 ) ) ;
#146348 = CARTESIAN_POINT ( 'NONE',  ( 20.85000000000000142, 77.83585931145546510, -91.51866831572576189 ) ) ;
#146349 = ORIENTED_EDGE ( 'NONE', *, *, #204511, .F. ) ;
#146350 = CARTESIAN_POINT ( 'NONE',  ( -2.995603634470891112E-16, 6.650000000011155876, -121.7500000000000426 ) ) ;
#146351 = DIRECTION ( 'NONE',  ( -0.000000000000000000, 1.000000000000000000, -0.000000000000000000 ) ) ;
#146352 = VERTEX_POINT ( 'NONE', #30090 ) ;
#146353 = FACE_OUTER_BOUND ( 'NONE', #225847, .T. ) ;
#146354 = CARTESIAN_POINT ( 'NONE',  ( 23.14999999999999503, 64.35000000001254250, -182.1731074845244507 ) ) ;
#146355 = AXIS2_PLACEMENT_3D ( 'NONE', #54490, #55741, #173215 ) ;
#146356 = ORIENTED_EDGE ( 'NONE', *, *, #65461, .T. ) ;
#146357 = CARTESIAN_POINT ( 'NONE',  ( 19.80993210785419834, 54.45774741499781868, -228.7023132931329030 ) ) ;
#146359 = ORIENTED_EDGE ( 'NONE', *, *, #141917, .T. ) ;
#146358 = ORIENTED_EDGE ( 'NONE', *, *, #137973, .T. ) ;
#146360 = ORIENTED_EDGE ( 'NONE', *, *, #27657, .F. ) ;
#146361 = ORIENTED_EDGE ( 'NONE', *, *, #47014, .F. ) ;
#146362 = DIRECTION ( 'NONE',  ( 0.000000000000000000, 0.000000000000000000, 1.000000000000000000 ) ) ;
#146363 = VERTEX_POINT ( 'NONE', #11810 ) ;
#146364 = DIRECTION ( 'NONE',  ( 0.000000000000000000, -0.000000000000000000, -1.000000000000000000 ) ) ;
#146365 = DIRECTION ( 'NONE',  ( 1.000000000000000000, -1.207181226542539700E-16, 2.694675058168174199E-16 ) ) ;
#146366 = EDGE_LOOP ( 'NONE', ( #163273, #167265, #60091, #61242 ) ) ;
#146367 = AXIS2_PLACEMENT_3D ( 'NONE', #190566, #154038, #69328 ) ;
#146369 = EDGE_CURVE ( 'NONE', #184107, #153506, #152608, .T. ) ;
#146368 = CIRCLE ( 'NONE', #154796, 0.09999999999999892308 ) ;
#146370 = ORIENTED_EDGE ( 'NONE', *, *, #188048, .F. ) ;
#146371 = VECTOR ( 'NONE', #123424, 1000.000000000000114 ) ;
#146372 = ORIENTED_EDGE ( 'NONE', *, *, #224227, .T. ) ;
#146373 = CARTESIAN_POINT ( 'NONE',  ( -18.58671080940899856, 85.40693285883877195, -129.3989530196196256 ) ) ;
#146374 = ORIENTED_EDGE ( 'NONE', *, *, #136852, .F. ) ;
#146375 = EDGE_CURVE ( 'NONE', #1901, #158699, #187312, .T. ) ;
#146376 = DIRECTION ( 'NONE',  ( 1.000000000000000000, 0.000000000000000000, 0.000000000000000000 ) ) ;
#146378 = ORIENTED_EDGE ( 'NONE', *, *, #543, .F. ) ;
#146377 = FACE_OUTER_BOUND ( 'NONE', #251092, .T. ) ;
#146379 = CYLINDRICAL_SURFACE ( 'NONE', #226050, 0.1000000000000075273 ) ;
#146380 = LINE ( 'NONE', #229790, #60081 ) ;
#146381 = DIRECTION ( 'NONE',  ( 0.000000000000000000, 0.000000000000000000, -1.000000000000000000 ) ) ;
#146382 = AXIS2_PLACEMENT_3D ( 'NONE', #60893, #20516, #218676 ) ;
#146383 = DIRECTION ( 'NONE',  ( -3.265361837132812600E-16, -0.4088369013363246096, 0.9126074666063785923 ) ) ;
#146384 = EDGE_CURVE ( 'NONE', #117008, #89222, #79126, .T. ) ;
#146385 = CARTESIAN_POINT ( 'NONE',  ( 20.04142135623730070, 64.35000000001220144, -145.3731074845244109 ) ) ;
#146387 = CARTESIAN_POINT ( 'NONE',  ( 20.94999999999999929, 76.49733069700262433, -201.6893511817872309 ) ) ;
#146386 = CARTESIAN_POINT ( 'NONE',  ( -21.05000000000000426, -0.02103547652895406198, -60.69554417805237989 ) ) ;
#146388 = DIRECTION ( 'NONE',  ( -1.000000000000000000, 0.000000000000000000, 0.000000000000000000 ) ) ;
#146389 = CARTESIAN_POINT ( 'NONE',  ( -20.54999999999999716, -6.688413578037177842, -212.5825622730469036 ) ) ;
#146390 = CARTESIAN_POINT ( 'NONE',  ( -23.15000000000000213, 11.75000000001115552, -179.6499999999999773 ) ) ;
#146391 = VERTEX_POINT ( 'NONE', #134275 ) ;
#146392 = EDGE_CURVE ( 'NONE', #164553, #65207, #92585, .T. ) ;
#146394 = ORIENTED_EDGE ( 'NONE', *, *, #218500, .F. ) ;
#146393 = DIRECTION ( 'NONE',  ( 0.000000000000000000, 0.000000000000000000, -1.000000000000000000 ) ) ;
#146395 = EDGE_CURVE ( 'NONE', #88661, #121232, #154036, .T. ) ;
#146396 = ORIENTED_EDGE ( 'NONE', *, *, #247005, .F. ) ;
#146397 = CARTESIAN_POINT ( 'NONE',  ( -21.04999999999994387, 67.75000000001118394, -4.623107484524796362 ) ) ;
#146398 = CIRCLE ( 'NONE', #113108, 0.2000000000000003997 ) ;
#146399 = CARTESIAN_POINT ( 'NONE',  ( 20.13684514580102913, 9.495855392761558988, -142.1430316856892091 ) ) ;
#146400 = EDGE_CURVE ( 'NONE', #47876, #146335, #41580, .T. ) ;
#146402 = DIRECTION ( 'NONE',  ( 1.000000000000000000, 0.000000000000000000, 0.000000000000000000 ) ) ;
#146401 = CARTESIAN_POINT ( 'NONE',  ( 20.22516295850462598, 39.83048402819590450, -237.2830021754640200 ) ) ;
#146403 = ORIENTED_EDGE ( 'NONE', *, *, #45311, .F. ) ;
#146404 = VECTOR ( 'NONE', #203557, 1000.000000000000000 ) ;
#146405 = FACE_OUTER_BOUND ( 'NONE', #226720, .T. ) ;
#146406 = EDGE_CURVE ( 'NONE', #249890, #148418, #108320, .T. ) ;
#146407 = AXIS2_PLACEMENT_3D ( 'NONE', #207926, #150507, #51356 ) ;
#146408 = DIRECTION ( 'NONE',  ( -1.000000000000000000, 0.000000000000000000, 0.000000000000000000 ) ) ;
#146409 = ORIENTED_EDGE ( 'NONE', *, *, #196357, .F. ) ;
#146410 = CARTESIAN_POINT ( 'NONE',  ( 20.94999999999999929, 85.00000000001232081, -160.1291383618718385 ) ) ;
#146411 = CARTESIAN_POINT ( 'NONE',  ( -16.83199030136657370, 9.930648033124622742, -180.2724010226574194 ) ) ;
#146412 = AXIS2_PLACEMENT_3D ( 'NONE', #108351, #6662, #186611 ) ;
#146413 = EDGE_CURVE ( 'NONE', #80704, #149698, #249839, .T. ) ;
#146414 = CARTESIAN_POINT ( 'NONE',  ( 20.95429693346637734, 65.45669512011546942, -61.96222494621114407 ) ) ;
#146415 = AXIS2_PLACEMENT_3D ( 'NONE', #213531, #75352, #221225 ) ;
#146416 = CARTESIAN_POINT ( 'NONE',  ( 20.04142135623730070, 11.65000000001115943, -188.8499999999999659 ) ) ;
#146418 = ORIENTED_EDGE ( 'NONE', *, *, #40766, .F. ) ;
#146417 = LINE ( 'NONE', #68193, #127052 ) ;
#146419 = CARTESIAN_POINT ( 'NONE',  ( -23.15000000000000213, 87.48912529308749697, -39.12310748452424747 ) ) ;
#146420 = DIRECTION ( 'NONE',  ( -1.000000000000000000, -0.000000000000000000, 0.000000000000000000 ) ) ;
#146421 = FACE_OUTER_BOUND ( 'NONE', #244198, .T. ) ;
#146423 = CIRCLE ( 'NONE', #75564, 11.70000000000001528 ) ;
#146422 = DIRECTION ( 'NONE',  ( -1.836970198721029934E-16, 0.9770955615653315052, 0.2128009952263603954 ) ) ;
#146424 = ORIENTED_EDGE ( 'NONE', *, *, #225066, .T. ) ;
#146425 = CARTESIAN_POINT ( 'NONE',  ( 15.74999999999999645, 66.65000000001185754, -86.27310748452437394 ) ) ;
#146427 = EDGE_CURVE ( 'NONE', #240172, #87594, #158298, .T. ) ;
#146426 = DIRECTION ( 'NONE',  ( 1.000000000000000000, 7.304098846218133681E-16, 4.639676173203992654E-30 ) ) ;
#146428 = CIRCLE ( 'NONE', #225714, 0.09999999999999939493 ) ;
#146430 = CARTESIAN_POINT ( 'NONE',  ( 21.14999999999999858, 45.06922343725926083, -238.6062154437373124 ) ) ;
#146429 = DIRECTION ( 'NONE',  ( 0.000000000000000000, 0.000000000000000000, -1.000000000000000000 ) ) ;
#146431 = DIRECTION ( 'NONE',  ( 1.000000000000000000, 0.000000000000000000, 0.000000000000000000 ) ) ;
#146432 = DIRECTION ( 'NONE',  ( 0.000000000000000000, 0.9126074666063769270, 0.4088369013363280513 ) ) ;
#146434 = DIRECTION ( 'NONE',  ( 0.000000000000000000, -0.9654727137038715545, -0.2605042016806676242 ) ) ;
#146433 = AXIS2_PLACEMENT_3D ( 'NONE', #255268, #140494, #58375 ) ;
#146435 = CARTESIAN_POINT ( 'NONE',  ( -16.80117486205003630, 66.05034273169920311, -48.67425261159890937 ) ) ;
#146436 = DIRECTION ( 'NONE',  ( 0.000000000000000000, -1.000000000000000000, 0.000000000000000000 ) ) ;
#146437 = DIRECTION ( 'NONE',  ( 1.000000000000000000, 0.000000000000000000, -0.000000000000000000 ) ) ;
#146438 = AXIS2_PLACEMENT_3D ( 'NONE', #70014, #107829, #149552 ) ;
#146439 = VERTEX_POINT ( 'NONE', #129168 ) ;
#146440 = ORIENTED_EDGE ( 'NONE', *, *, #19507, .T. ) ;
#146441 = VECTOR ( 'NONE', #20490, 1000.000000000000114 ) ;
#146442 = EDGE_LOOP ( 'NONE', ( #225860, #169854, #68, #50444 ) ) ;
#146443 = CARTESIAN_POINT ( 'NONE',  ( 20.13684514580104334, 66.50414460725923504, -94.88007579883958442 ) ) ;
#146444 = DIRECTION ( 'NONE',  ( -1.000000000000000000, -0.000000000000000000, 0.000000000000000000 ) ) ;
#146445 = VERTEX_POINT ( 'NONE', #208718 ) ;
#146446 = CIRCLE ( 'NONE', #34084, 0.8750000000000007772 ) ;
#146447 = ORIENTED_EDGE ( 'NONE', *, *, #125718, .T. ) ;
#146449 = VERTEX_POINT ( 'NONE', #90020 ) ;
#146448 = AXIS2_PLACEMENT_3D ( 'NONE', #83357, #185051, #247597 ) ;
#146450 = DIRECTION ( 'NONE',  ( 0.000000000000000000, 0.4930308989874980785, 0.8700118002898462599 ) ) ;
#146451 = AXIS2_PLACEMENT_3D ( 'NONE', #207467, #152646, #229590 ) ;
#146452 = ORIENTED_EDGE ( 'NONE', *, *, #92597, .F. ) ;
#146453 =( BOUNDED_SURFACE ( )  B_SPLINE_SURFACE ( 3, 2, ( 
 ( #51502, #249739, #71121 ),
 ( #131066, #69837, #149379 ),
 ( #172813, #153239, #189762 ),
 ( #50233, #151947, #150638 ),
 ( #213169, #230167, #232756 ),
 ( #210608, #256085, #197455 ) ),
 .UNSPECIFIED., .F., .F., .T. ) 
 B_SPLINE_SURFACE_WITH_KNOTS ( ( 4, 2, 4 ),
 ( 3, 3 ),
 ( 6.719893378901017553E-05, 0.0002757154632485577309, 0.0004842319927081052862 ),
 ( 0.000000000000000000, 1.000000000000000000 ),
 .UNSPECIFIED. ) 
 GEOMETRIC_REPRESENTATION_ITEM ( )  RATIONAL_B_SPLINE_SURFACE ( (
 ( 1.000000000000000000, 0.7250110520819756932, 1.000000000000000000),
 ( 1.000000000000000000, 0.7277932058359009027, 1.000000000000000000),
 ( 1.000000000000000000, 0.7278452872617788838, 1.000000000000000000),
 ( 1.000000000000000000, 0.7221445671549024947, 1.000000000000000000),
 ( 1.000000000000000000, 0.7163662143779696567, 1.000000000000000000),
 ( 1.000000000000000000, 0.7071067811865475727, 1.000000000000000000) ) ) 
 REPRESENTATION_ITEM ( '' )  SURFACE ( )  );
#146454 = VECTOR ( 'NONE', #103874, 1000.000000000000000 ) ;
#146455 = ADVANCED_FACE ( 'NONE', ( #71778 ), #49924, .T. ) ;
#146456 = CARTESIAN_POINT ( 'NONE',  ( -23.24999999999999645, 38.03205796367814173, -261.1772988674111957 ) ) ;
#146457 = DIRECTION ( 'NONE',  ( 0.000000000000000000, 0.9126074666063660468, 0.4088369013363524762 ) ) ;
#146459 = CARTESIAN_POINT ( 'NONE',  ( -16.93353400591625757, 30.30500211285577450, -234.7979474545380754 ) ) ;
#146458 = CIRCLE ( 'NONE', #117270, 0.1000000000000040579 ) ;
#146460 = DIRECTION ( 'NONE',  ( -2.812466655313719426E-14, -0.1350103645451835865, -0.9908441862701605762 ) ) ;
#146461 = CARTESIAN_POINT ( 'NONE',  ( -21.07971444708686093, 1.590621248691514555, -230.6664026343516127 ) ) ;
#146462 = B_SPLINE_CURVE_WITH_KNOTS ( 'NONE', 3,
 ( #13977, #93492, #173090, #252558 ),
 .UNSPECIFIED., .F., .F.,
 ( 4, 4 ),
 ( 0.000000000000000000, 0.001767853679387130974 ),
 .UNSPECIFIED. ) ;
#146463 = CARTESIAN_POINT ( 'NONE',  ( 21.15000000000005187, 76.00000000001119815, -36.02310748452479316 ) ) ;
#146464 = DIRECTION ( 'NONE',  ( 0.000000000000000000, 0.000000000000000000, 1.000000000000000000 ) ) ;
#146466 = ORIENTED_EDGE ( 'NONE', *, *, #221273, .F. ) ;
#146465 = DIRECTION ( 'NONE',  ( -1.000000000000000000, 0.000000000000000000, 0.000000000000000000 ) ) ;
#146468 = CARTESIAN_POINT ( 'NONE',  ( -20.64999999999999858, 1.115600667400684642E-11, -200.9999999999999432 ) ) ;
#146467 = CYLINDRICAL_SURFACE ( 'NONE', #225347, 0.09999999999999939493 ) ;
#146469 = FACE_OUTER_BOUND ( 'NONE', #96640, .T. ) ;
#146470 = EDGE_CURVE ( 'NONE', #248444, #29621, #74901, .T. ) ;
#146471 = EDGE_LOOP ( 'NONE', ( #71231, #205987, #125174, #191217 ) ) ;
#146472 = DIRECTION ( 'NONE',  ( 0.000000000000000000, -0.2617529984165022361, -0.9651348961777160840 ) ) ;
#146473 = DIRECTION ( 'NONE',  ( 0.000000000000000000, -0.9651348961777157509, 0.2617529984165031243 ) ) ;
#146474 = DIRECTION ( 'NONE',  ( 0.000000000000000000, 0.000000000000000000, 1.000000000000000000 ) ) ;
#146475 = ORIENTED_EDGE ( 'NONE', *, *, #226356, .T. ) ;
#146476 = ADVANCED_FACE ( 'NONE', ( #131727 ), #112186, .F. ) ;
#146477 = CARTESIAN_POINT ( 'NONE',  ( 21.00023020733503643, 76.00000000001170974, -75.91397672979269373 ) ) ;
#146478 = ADVANCED_FACE ( 'NONE', ( #159025 ), #196826, .T. ) ;
#146479 = ADVANCED_FACE ( 'NONE', ( #156466 ), #18199, .T. ) ;
#146480 = DIRECTION ( 'NONE',  ( -1.000000000000000000, 0.000000000000000000, 0.000000000000000000 ) ) ;
#146481 = EDGE_CURVE ( 'NONE', #86183, #588, #100275, .T. ) ;
#146482 = ORIENTED_EDGE ( 'NONE', *, *, #101979, .F. ) ;
#146483 = FACE_OUTER_BOUND ( 'NONE', #67487, .T. ) ;
#146484 = ADVANCED_FACE ( 'NONE', ( #234680 ), #245744, .T. ) ;
#146485 = CARTESIAN_POINT ( 'NONE',  ( -18.41809261886926308, -0.9152170315146264112, -242.2974986608316499 ) ) ;
#146486 = DIRECTION ( 'NONE',  ( 1.000000000000000000, 0.000000000000000000, 0.000000000000000000 ) ) ;
#146487 = VERTEX_POINT ( 'NONE', #139406 ) ;
#146488 = EDGE_LOOP ( 'NONE', ( #174980, #175175, #55053, #49701 ) ) ;
#146489 = DIRECTION ( 'NONE',  ( -1.000000000000000000, 0.000000000000000000, 0.000000000000000000 ) ) ;
#146490 = DIRECTION ( 'NONE',  ( 0.000000000000000000, 0.1332476588733636502, 0.9910827722268044093 ) ) ;
#146491 = DIRECTION ( 'NONE',  ( 0.000000000000000000, -0.8490545835447238510, -0.5283051335749973099 ) ) ;
#146492 = CARTESIAN_POINT ( 'NONE',  ( -2.995603634470891112E-16, 87.75000000001259082, -191.2731074845242745 ) ) ;
#146493 = CARTESIAN_POINT ( 'NONE',  ( 21.12757541349815682, 6.473380571262609351, -167.4948387841902218 ) ) ;
#146494 = CARTESIAN_POINT ( 'NONE',  ( 21.14999999999999858, 6.650000000011155876, -112.6500000000000341 ) ) ;
#146495 = ORIENTED_EDGE ( 'NONE', *, *, #134162, .F. ) ;
#146496 = CARTESIAN_POINT ( 'NONE',  ( -20.91682497891422798, 65.67736539654943329, -97.46251168765718376 ) ) ;
#146497 = EDGE_CURVE ( 'NONE', #23197, #3673, #129043, .T. ) ;
#146498 = CIRCLE ( 'NONE', #142424, 0.09999999999998898659 ) ;
#146500 = ORIENTED_EDGE ( 'NONE', *, *, #114491, .F. ) ;
#146499 = DIRECTION ( 'NONE',  ( 0.000000000000000000, -0.2617529984164915779, -0.9651348961777189706 ) ) ;
#146501 = CARTESIAN_POINT ( 'NONE',  ( -21.05000000000000071, -11.48912529306490349, -70.00000000000004263 ) ) ;
#146502 = FACE_OUTER_BOUND ( 'NONE', #169350, .T. ) ;
#146503 = CARTESIAN_POINT ( 'NONE',  ( -18.59999999999999787, 23.42819724844703444, -229.2476443247244902 ) ) ;
#146504 = CARTESIAN_POINT ( 'NONE',  ( 20.94999999999999929, 43.16354019706792400, -239.5695141926698284 ) ) ;
#146505 = ADVANCED_FACE ( 'NONE', ( #254221 ), #37784, .F. ) ;
#146507 = ORIENTED_EDGE ( 'NONE', *, *, #180240, .T. ) ;
#146506 = CARTESIAN_POINT ( 'NONE',  ( 20.94999999999999929, 69.35000000001207354, -126.5060803140843291 ) ) ;
#146508 = CYLINDRICAL_SURFACE ( 'NONE', #34372, 0.09999999999999939493 ) ;
#146510 = EDGE_CURVE ( 'NONE', #14565, #119881, #104927, .T. ) ;
#146509 = DIRECTION ( 'NONE',  ( 1.000000000000000000, -3.151514657663852580E-16, 8.547182517843349904E-17 ) ) ;
#146511 = CARTESIAN_POINT ( 'NONE',  ( 22.59999985501178799, 11.74986979301414181, -66.93440133020047256 ) ) ;
#146512 = DIRECTION ( 'NONE',  ( 0.000000000000000000, -0.9908441862701420355, -0.1350103645453197554 ) ) ;
#146513 =( BOUNDED_CURVE ( )  B_SPLINE_CURVE ( 3, ( #170362, #33409, #71232, #114185 ),
 .UNSPECIFIED., .F., .F. ) 
 B_SPLINE_CURVE_WITH_KNOTS ( ( 4, 4 ),
 ( 4.712388980384689674, 6.231880751915385375 ),
 .UNSPECIFIED. ) 
 CURVE ( )  GEOMETRIC_REPRESENTATION_ITEM ( )  RATIONAL_B_SPLINE_CURVE ( ( 1.000000000000000000, 0.8166740347213230500, 0.8166740347213230500, 1.000000000000000000 ) ) 
 REPRESENTATION_ITEM ( '' )  );
#146514 = ORIENTED_EDGE ( 'NONE', *, *, #254001, .T. ) ;
#146515 = CARTESIAN_POINT ( 'NONE',  ( -18.50000000000000000, 9.350000000011156942, -88.15000000000004832 ) ) ;
#146516 = FACE_OUTER_BOUND ( 'NONE', #235173, .T. ) ;
#146517 = DIRECTION ( 'NONE',  ( 0.000000000000000000, 0.000000000000000000, -1.000000000000000000 ) ) ;
#146519 = AXIS2_PLACEMENT_3D ( 'NONE', #36528, #153930, #176032 ) ;
#146518 = CARTESIAN_POINT ( 'NONE',  ( 22.60000000000000142, 11.74956712350054744, -167.3991416309012550 ) ) ;
#146520 = ORIENTED_EDGE ( 'NONE', *, *, #254182, .T. ) ;
#146522 = AXIS2_PLACEMENT_3D ( 'NONE', #74328, #243623, #83239 ) ;
#146521 = CARTESIAN_POINT ( 'NONE',  ( -16.87998658237752991, 9.950000000011197443, -87.63636043226256334 ) ) ;
#146523 = ORIENTED_EDGE ( 'NONE', *, *, #21953, .T. ) ;
#146524 = AXIS2_PLACEMENT_3D ( 'NONE', #160729, #218077, #257169 ) ;
#146525 = DIRECTION ( 'NONE',  ( 0.000000000000000000, 0.000000000000000000, -1.000000000000000000 ) ) ;
#146526 = DIRECTION ( 'NONE',  ( 0.000000000000000000, 0.000000000000000000, 1.000000000000000000 ) ) ;
#146527 = CARTESIAN_POINT ( 'NONE',  ( 23.24999999999999289, 11.65000000001116298, -112.6500000000000341 ) ) ;
#146528 = CARTESIAN_POINT ( 'NONE',  ( -18.59999999999999787, 74.13328508995475374, -124.7704322382423072 ) ) ;
#146529 = ORIENTED_EDGE ( 'NONE', *, *, #32269, .F. ) ;
#146530 = LINE ( 'NONE', #203954, #162797 ) ;
#146531 = AXIS2_PLACEMENT_3D ( 'NONE', #205863, #32402, #194033 ) ;
#146532 = CARTESIAN_POINT ( 'NONE',  ( -21.12642695952773764, 6.208582294788165257, -199.5466152643390387 ) ) ;
#146533 = CARTESIAN_POINT ( 'NONE',  ( 15.66039659514496130, 9.360749169915104417, -17.31457014060726962 ) ) ;
#146534 = DIRECTION ( 'NONE',  ( 0.000000000000000000, -0.9594490217226032680, -0.2818822000686448392 ) ) ;
#146535 = LINE ( 'NONE', #48734, #40757 ) ;
#146536 = VERTEX_POINT ( 'NONE', #199425 ) ;
#146538 = EDGE_LOOP ( 'NONE', ( #48276, #54080, #55593, #208823, #209685, #190185, #78446, #111765 ) ) ;
#146537 = CARTESIAN_POINT ( 'NONE',  ( 20.91682497891422798, 10.32263460347359363, -106.0605957968672328 ) ) ;
#146539 = ORIENTED_EDGE ( 'NONE', *, *, #131491, .F. ) ;
#146540 = CARTESIAN_POINT ( 'NONE',  ( -16.87683809663752399, 52.34166666667924517, -186.7731074845245303 ) ) ;
#146541 = ORIENTED_EDGE ( 'NONE', *, *, #4283, .T. ) ;
#146542 = FACE_OUTER_BOUND ( 'NONE', #172503, .T. ) ;
#146543 = CARTESIAN_POINT ( 'NONE',  ( 20.85000000000000142, 1.115600667400684642E-11, -100.5000000000000426 ) ) ;
#146544 = DIRECTION ( 'NONE',  ( -2.940209281316621016E-16, 1.000000000000000000, 0.000000000000000000 ) ) ;
#146545 = EDGE_LOOP ( 'NONE', ( #190906, #21169 ) ) ;
#146546 = B_SPLINE_CURVE_WITH_KNOTS ( 'NONE', 3,
 ( #34166, #229758, #51084, #193217, #14591, #233625, #129378, #134488, #15880, #111096, #171122, #250597, #248035, #208911, #32890, #13288, #92802, #139620, #57521 ),
 .UNSPECIFIED., .F., .F.,
 ( 4, 3, 3, 3, 3, 3, 4 ),
 ( -2.000416914655141542E-06, 0.000000000000000000, 4.714008503747371182E-05, 9.979203887777928774E-05, 0.0001372215519229508436, 0.0001635031576221009011, 0.0001900083748504142458 ),
 .UNSPECIFIED. ) ;
#146547 = CYLINDRICAL_SURFACE ( 'NONE', #149020, 0.09999999999999939493 ) ;
#146548 = DIRECTION ( 'NONE',  ( 0.000000000000000000, 0.000000000000000000, -1.000000000000000000 ) ) ;
#146549 = CARTESIAN_POINT ( 'NONE',  ( 20.97565083910961548, 10.47461740128996510, -41.07794317658855476 ) ) ;
#146550 = ORIENTED_EDGE ( 'NONE', *, *, #120076, .F. ) ;
#146551 = CARTESIAN_POINT ( 'NONE',  ( -20.94999999999999929, 87.48912529308769592, -66.62310748452424036 ) ) ;
#146552 = EDGE_CURVE ( 'NONE', #127250, #241724, #20920, .T. ) ;
#146554 = ORIENTED_EDGE ( 'NONE', *, *, #71366, .T. ) ;
#146553 = DIRECTION ( 'NONE',  ( 0.000000000000000000, -1.000000000000000000, 0.000000000000000000 ) ) ;
#146555 = VECTOR ( 'NONE', #31206, 1000.000000000000000 ) ;
#146556 = CIRCLE ( 'NONE', #204827, 0.09999999999999939493 ) ;
#146557 = DIRECTION ( 'NONE',  ( 0.000000000000000000, 0.000000000000000000, -1.000000000000000000 ) ) ;
#146558 = DIRECTION ( 'NONE',  ( 0.1538461538461510236, 0.9880948137434718559, 0.000000000000000000 ) ) ;
#146559 = AXIS2_PLACEMENT_3D ( 'NONE', #17578, #153293, #137520 ) ;
#146560 = EDGE_CURVE ( 'NONE', #19570, #97016, #140706, .T. ) ;
#146561 = ORIENTED_EDGE ( 'NONE', *, *, #55286, .T. ) ;
#146562 = DIRECTION ( 'NONE',  ( 1.000000000000000000, 0.000000000000000000, 0.000000000000000000 ) ) ;
#146564 = EDGE_CURVE ( 'NONE', #245093, #1731, #135562, .T. ) ;
#146563 = CARTESIAN_POINT ( 'NONE',  ( 20.94999999999999574, 67.07338541492450190, -61.05142446530125966 ) ) ;
#146565 = CYLINDRICAL_SURFACE ( 'NONE', #122542, 0.1000000000000070832 ) ;
#146567 = ADVANCED_FACE ( 'NONE', ( #138123 ), #16627, .T. ) ;
#146566 = ORIENTED_EDGE ( 'NONE', *, *, #171350, .T. ) ;
#146568 = CARTESIAN_POINT ( 'NONE',  ( 20.94999999999999929, 23.68770167995059239, -252.8127582590406348 ) ) ;
#146569 = AXIS2_PLACEMENT_3D ( 'NONE', #97111, #256160, #39784 ) ;
#146570 = EDGE_LOOP ( 'NONE', ( #226962, #72064, #237373, #112986 ) ) ;
#146571 = EDGE_CURVE ( 'NONE', #168985, #229125, #83211, .T. ) ;
#146572 = EDGE_CURVE ( 'NONE', #17833, #69101, #228998, .T. ) ;
#146573 = ORIENTED_EDGE ( 'NONE', *, *, #60124, .F. ) ;
#146574 = CARTESIAN_POINT ( 'NONE',  ( 22.42357213249528769, 68.32706761365277259, -203.6221944485259598 ) ) ;
#146575 = ORIENTED_EDGE ( 'NONE', *, *, #209131, .F. ) ;
#146576 = LINE ( 'NONE', #144020, #118449 ) ;
#146577 = CYLINDRICAL_SURFACE ( 'NONE', #179552, 0.09999999999999939493 ) ;
#146578 = AXIS2_PLACEMENT_3D ( 'NONE', #170814, #247724, #191643 ) ;
#146580 = ORIENTED_EDGE ( 'NONE', *, *, #4873, .T. ) ;
#146579 = DIRECTION ( 'NONE',  ( -1.000000000000000000, 0.000000000000000000, 0.000000000000000000 ) ) ;
#146581 = CARTESIAN_POINT ( 'NONE',  ( 20.94999999999999929, -11.39257802170566869, -30.42605042016806394 ) ) ;
#146582 = DIRECTION ( 'NONE',  ( -1.000000000000000000, -1.836970198721029934E-16, 0.000000000000000000 ) ) ;
#146583 = FACE_OUTER_BOUND ( 'NONE', #60623, .T. ) ;
#146584 = CARTESIAN_POINT ( 'NONE',  ( -21.55000000000000426, 68.25000000001205080, -124.1731074845243512 ) ) ;
#146585 = CARTESIAN_POINT ( 'NONE',  ( 18.49999999999999645, 5.950000000011100632, -177.8057023050348278 ) ) ;
#146586 = DIRECTION ( 'NONE',  ( 0.000000000000000000, -6.769652589177795712E-15, 1.000000000000000000 ) ) ;
#146587 = CIRCLE ( 'NONE', #79936, 0.09999999999999939493 ) ;
#146589 = ADVANCED_FACE ( 'NONE', ( #61172 ), #35230, .T. ) ;
#146588 = CARTESIAN_POINT ( 'NONE',  ( -18.54159361262949091, -9.463132135481851392, -107.5491222162930569 ) ) ;
#146591 = ORIENTED_EDGE ( 'NONE', *, *, #165346, .F. ) ;
#146590 = DIRECTION ( 'NONE',  ( -0.000000000000000000, 0.2128009952263603677, -0.9770955615653313941 ) ) ;
#146592 = CARTESIAN_POINT ( 'NONE',  ( 22.39999999999999503, 25.97741635855165754, -254.4468634167653249 ) ) ;
#146593 = AXIS2_PLACEMENT_3D ( 'NONE', #95328, #54899, #157921 ) ;
#146594 = ORIENTED_EDGE ( 'NONE', *, *, #230259, .F. ) ;
#146595 = CIRCLE ( 'NONE', #254881, 0.1000000000000000888 ) ;
#146596 = AXIS2_PLACEMENT_3D ( 'NONE', #130665, #91551, #109813 ) ;
#146597 = EDGE_CURVE ( 'NONE', #151179, #195444, #87506, .T. ) ;
#146598 = AXIS2_PLACEMENT_3D ( 'NONE', #139437, #182455, #22097 ) ;
#146599 = CYLINDRICAL_SURFACE ( 'NONE', #114146, 0.09999999999999939493 ) ;
#146600 = DIRECTION ( 'NONE',  ( 0.000000000000000000, 0.000000000000000000, -1.000000000000000000 ) ) ;
#146602 = EDGE_CURVE ( 'NONE', #121663, #34375, #233294, .T. ) ;
#146601 = CARTESIAN_POINT ( 'NONE',  ( 20.22516295850462598, 66.10063570456237869, -195.6130417724336041 ) ) ;
#146603 = DIRECTION ( 'NONE',  ( 1.000000000000000000, 0.000000000000000000, 0.000000000000000000 ) ) ;
#146604 = VECTOR ( 'NONE', #218916, 1000.000000000000000 ) ;
#146605 = VERTEX_POINT ( 'NONE', #23367 ) ;
#146606 = EDGE_CURVE ( 'NONE', #165639, #68414, #25011, .T. ) ;
#146607 = DIRECTION ( 'NONE',  ( 0.000000000000000000, 1.000000000000000000, 0.000000000000000000 ) ) ;
#146608 = VECTOR ( 'NONE', #119231, 1000.000000000000000 ) ;
#146609 = CARTESIAN_POINT ( 'NONE',  ( -21.08479644141223019, 6.345038657743049093, -100.4414455574359124 ) ) ;
#146611 = EDGE_CURVE ( 'NONE', #164805, #116663, #164140, .T. ) ;
#146610 = CIRCLE ( 'NONE', #179975, 0.1000000000000013933 ) ;
#146612 = ORIENTED_EDGE ( 'NONE', *, *, #151876, .F. ) ;
#146613 = AXIS2_PLACEMENT_3D ( 'NONE', #189501, #113806, #193363 ) ;
#146614 = CARTESIAN_POINT ( 'NONE',  ( -21.05000000000000071, -1.851028230140860487, -11.65391326942249428 ) ) ;
#146615 = CIRCLE ( 'NONE', #196524, 12.87499999999999289 ) ;
#146616 = CARTESIAN_POINT ( 'NONE',  ( -16.89020380669787613, 60.96747295614021311, -220.9380614883060900 ) ) ;
#146617 = ORIENTED_EDGE ( 'NONE', *, *, #210907, .T. ) ;
#146618 = CARTESIAN_POINT ( 'NONE',  ( -21.04999999999999716, 6.440770893673031239, -67.01759718700851920 ) ) ;
#146619 = ORIENTED_EDGE ( 'NONE', *, *, #106835, .F. ) ;
#146620 = ADVANCED_FACE ( 'NONE', ( #162869 ), #201977, .T. ) ;
#146622 = AXIS2_PLACEMENT_3D ( 'NONE', #145657, #27042, #49131 ) ;
#146621 = CARTESIAN_POINT ( 'NONE',  ( 20.94999999999999929, 65.27628289530399286, -48.27310748452439526 ) ) ;
#146623 = ORIENTED_EDGE ( 'NONE', *, *, #149451, .T. ) ;
#146624 = DIRECTION ( 'NONE',  ( -0.000000000000000000, -0.000000000000000000, 1.000000000000000000 ) ) ;
#146625 = ADVANCED_FACE ( 'NONE', ( #41635 ), #200693, .T. ) ;
#146626 = CARTESIAN_POINT ( 'NONE',  ( -20.94999999999999929, 45.93315328338058379, -256.6017782078560003 ) ) ;
#146627 = ORIENTED_EDGE ( 'NONE', *, *, #225781, .T. ) ;
#146628 = ORIENTED_EDGE ( 'NONE', *, *, #221981, .T. ) ;
#146629 = CARTESIAN_POINT ( 'NONE',  ( 20.94999999999999574, 74.25000000001205080, -124.8535959266226598 ) ) ;
#146631 = EDGE_LOOP ( 'NONE', ( #182755, #109342, #142073, #90886 ) ) ;
#146630 =( NAMED_UNIT ( * ) PLANE_ANGLE_UNIT ( ) SI_UNIT ( $, .RADIAN. ) );
#146632 = VECTOR ( 'NONE', #56739, 1000.000000000000000 ) ;
#146633 = CARTESIAN_POINT ( 'NONE',  ( 21.05000005001280172, 67.12872030824237868, -191.3451598962783464 ) ) ;
#146635 = ORIENTED_EDGE ( 'NONE', *, *, #212325, .T. ) ;
#146634 = AXIS2_PLACEMENT_3D ( 'NONE', #194021, #15379, #156183 ) ;
#146636 = AXIS2_PLACEMENT_3D ( 'NONE', #187014, #246952, #46185 ) ;
#146637 = AXIS2_PLACEMENT_3D ( 'NONE', #181128, #102829, #182408 ) ;
#146638 = ORIENTED_EDGE ( 'NONE', *, *, #104340, .F. ) ;
#146639 = CYLINDRICAL_SURFACE ( 'NONE', #174536, 0.09999999999999108213 ) ;
#146640 = DIRECTION ( 'NONE',  ( 0.000000000000000000, 0.000000000000000000, 1.000000000000000000 ) ) ;
#146641 = DIRECTION ( 'NONE',  ( -1.000000000000000000, 0.000000000000000000, -0.000000000000000000 ) ) ;
#146642 = CARTESIAN_POINT ( 'NONE',  ( -16.81744102076748959, 9.949999999999983302, -20.85000000000000142 ) ) ;
#146643 = CARTESIAN_POINT ( 'NONE',  ( -14.56556274378148430, 66.55344247694006299, -188.4331655301785986 ) ) ;
#146644 = DIRECTION ( 'NONE',  ( 1.073024830501117923E-15, 0.9126074666063771490, 0.4088369013363281623 ) ) ;
#146645 = EDGE_LOOP ( 'NONE', ( #189727, #56086, #188731, #22535, #54347 ) ) ;
#146646 = CARTESIAN_POINT ( 'NONE',  ( -20.65000000000000568, 70.35000000001181775, -82.17310748452435121 ) ) ;
#146647 = CARTESIAN_POINT ( 'NONE',  ( -21.14999999999999858, 87.65000000001163016, -66.62310748452424036 ) ) ;
#146648 = DIRECTION ( 'NONE',  ( 0.000000000000000000, 0.9126074666063660468, 0.4088369013363524762 ) ) ;
#146649 = CYLINDRICAL_SURFACE ( 'NONE', #84598, 0.09999999999999939493 ) ;
#146650 = VERTEX_POINT ( 'NONE', #184975 ) ;
#146652 = CARTESIAN_POINT ( 'NONE',  ( 20.94999999999999574, 87.48912529308871910, -200.4231074845242802 ) ) ;
#146651 = AXIS2_PLACEMENT_3D ( 'NONE', #35211, #75608, #232106 ) ;
#146653 = ORIENTED_EDGE ( 'NONE', *, *, #53311, .T. ) ;
#146654 = DIRECTION ( 'NONE',  ( 1.000000000000000000, 7.304098846218133681E-16, 5.100424963727255128E-30 ) ) ;
#146655 = ORIENTED_EDGE ( 'NONE', *, *, #233382, .F. ) ;
#146656 = CARTESIAN_POINT ( 'NONE',  ( -23.25000000000000000, 48.31748480764120046, -244.3282712866738962 ) ) ;
#146657 = EDGE_LOOP ( 'NONE', ( #26546, #38208, #4999, #143471 ) ) ;
#146658 = VERTEX_POINT ( 'NONE', #102841 ) ;
#146660 = ORIENTED_EDGE ( 'NONE', *, *, #28495, .F. ) ;
#146659 = CARTESIAN_POINT ( 'NONE',  ( -22.50000000000000000, 76.00000000001267608, -203.5231074845243597 ) ) ;
#146661 = FACE_OUTER_BOUND ( 'NONE', #120828, .T. ) ;
#146662 = ORIENTED_EDGE ( 'NONE', *, *, #134654, .T. ) ;
#146663 = CARTESIAN_POINT ( 'NONE',  ( 23.14999999999999858, 69.35000000001205933, -124.1731074845243370 ) ) ;
#146664 = DIRECTION ( 'NONE',  ( 0.000000000000000000, 0.000000000000000000, -1.000000000000000000 ) ) ;
#146665 = ORIENTED_EDGE ( 'NONE', *, *, #110384, .F. ) ;
#146666 = DIRECTION ( 'NONE',  ( 0.000000000000000000, 0.000000000000000000, 1.000000000000000000 ) ) ;
#146667 = EDGE_CURVE ( 'NONE', #38262, #118710, #122442, .T. ) ;
#146668 = DIRECTION ( 'NONE',  ( 0.000000000000000000, 0.000000000000000000, 1.000000000000000000 ) ) ;
#146669 = ORIENTED_EDGE ( 'NONE', *, *, #9084, .T. ) ;
#146670 = VECTOR ( 'NONE', #41674, 1000.000000000000000 ) ;
#146671 = CARTESIAN_POINT ( 'NONE',  ( 20.94999999999999574, 87.65000000001192859, -100.0231074845242318 ) ) ;
#146673 = EDGE_CURVE ( 'NONE', #127119, #29625, #100144, .T. ) ;
#146672 = CARTESIAN_POINT ( 'NONE',  ( 23.40000000000005542, 85.84984265665381997, -47.78991727088349251 ) ) ;
#146674 = LINE ( 'NONE', #185827, #192583 ) ;
#146676 = EDGE_LOOP ( 'NONE', ( #102444, #95659, #121527, #41550 ) ) ;
#146675 = CARTESIAN_POINT ( 'NONE',  ( -16.80468759584938354, 9.942153675145293690, -46.19001886620164044 ) ) ;
#146677 = ADVANCED_FACE ( 'NONE', ( #183701 ), #241119, .T. ) ;
#146678 = DIRECTION ( 'NONE',  ( 0.000000000000000000, -1.000000000000000000, 0.000000000000000000 ) ) ;
#146679 = EDGE_CURVE ( 'NONE', #214102, #7443, #225053, .T. ) ;
#146680 = CARTESIAN_POINT ( 'NONE',  ( -22.48479450179659977, 75.95300841882485088, -81.17310593077593239 ) ) ;
#146681 = CARTESIAN_POINT ( 'NONE',  ( -16.86445178670638612, 9.962211629127159185, -121.3907774381173681 ) ) ;
#146683 = CARTESIAN_POINT ( 'NONE',  ( -18.44085059012131822, 58.54245214771228234, -223.9044447480369513 ) ) ;
#146682 = CARTESIAN_POINT ( 'NONE',  ( 18.79999999999999716, 0.000000000000000000, 0.000000000000000000 ) ) ;
#146684 = CARTESIAN_POINT ( 'NONE',  ( 21.04999999999660432, 39.27454047675113458, -236.7319953479758965 ) ) ;
#146685 = DIRECTION ( 'NONE',  ( 0.000000000000000000, 0.4930308989875575865, 0.8700118002898125091 ) ) ;
#146686 = VECTOR ( 'NONE', #218657, 1000.000000000000000 ) ;
#146687 = DIRECTION ( 'NONE',  ( 0.000000000000000000, -0.2617529984165031243, -0.9651348961777157509 ) ) ;
#146688 = CARTESIAN_POINT ( 'NONE',  ( 18.59999999999999787, 42.96960653111219131, -254.4772109693542745 ) ) ;
#146689 = AXIS2_PLACEMENT_3D ( 'NONE', #15775, #135669, #36623 ) ;
#146690 = EDGE_LOOP ( 'NONE', ( #165440, #136813, #68396, #171860 ) ) ;
#146692 = ORIENTED_EDGE ( 'NONE', *, *, #35300, .T. ) ;
#146691 = VECTOR ( 'NONE', #49277, 1000.000000000000000 ) ;
#146693 = EDGE_CURVE ( 'NONE', #242494, #253135, #116742, .T. ) ;
#146694 = LINE ( 'NONE', #178849, #202100 ) ;
#146695 = ORIENTED_EDGE ( 'NONE', *, *, #73552, .F. ) ;
#146696 = EDGE_CURVE ( 'NONE', #219800, #178493, #145958, .T. ) ;
#146697 = LINE ( 'NONE', #7198, #256661 ) ;
#146698 = ORIENTED_EDGE ( 'NONE', *, *, #105550, .T. ) ;
#146699 = AXIS2_PLACEMENT_3D ( 'NONE', #10082, #145726, #164029 ) ;
#146701 = CIRCLE ( 'NONE', #200903, 2.000000000000001776 ) ;
#146700 =( NAMED_UNIT ( * ) PLANE_ANGLE_UNIT ( ) SI_UNIT ( $, .RADIAN. ) );
#146702 = FACE_OUTER_BOUND ( 'NONE', #236748, .T. ) ;
#146703 = DIRECTION ( 'NONE',  ( -1.000000000000000000, 0.000000000000000000, 0.000000000000000000 ) ) ;
#146704 = ORIENTED_EDGE ( 'NONE', *, *, #132674, .T. ) ;
#146705 = DIRECTION ( 'NONE',  ( 0.000000000000000000, 0.000000000000000000, -1.000000000000000000 ) ) ;
#146706 = EDGE_LOOP ( 'NONE', ( #215713, #57194, #195684 ) ) ;
#146707 = ORIENTED_EDGE ( 'NONE', *, *, #63000, .T. ) ;
#146708 = DIRECTION ( 'NONE',  ( -0.000000000000000000, -0.000000000000000000, 1.000000000000000000 ) ) ;
#146709 = DIRECTION ( 'NONE',  ( -2.561896900575096800E-15, -0.4948392722769219265, -0.8689845192018362807 ) ) ;
#146711 = VERTEX_POINT ( 'NONE', #204526 ) ;
#146710 = DIRECTION ( 'NONE',  ( 0.000000000000000000, -0.000000000000000000, 1.000000000000000000 ) ) ;
#146712 = EDGE_CURVE ( 'NONE', #253858, #129965, #6323, .T. ) ;
#146713 = DIRECTION ( 'NONE',  ( 0.000000000000000000, -1.000000000000000000, 0.000000000000000000 ) ) ;
#146715 = VERTEX_POINT ( 'NONE', #221510 ) ;
#146714 = CARTESIAN_POINT ( 'NONE',  ( -23.15000000000000213, 26.34635675162282098, -241.8429480539297174 ) ) ;
#146716 = CARTESIAN_POINT ( 'NONE',  ( -16.89081410710458542, 9.951318529858268036, -121.3544059198363954 ) ) ;
#146718 = ORIENTED_EDGE ( 'NONE', *, *, #68109, .F. ) ;
#146717 = CARTESIAN_POINT ( 'NONE',  ( -18.39999999999999858, 64.52683809664961245, -127.1971614177164156 ) ) ;
#146719 = LINE ( 'NONE', #204140, #113926 ) ;
#146720 = FILL_AREA_STYLE_COLOUR ( '', #62366 ) ;
#146721 = CIRCLE ( 'NONE', #117534, 0.1999999999999987899 ) ;
#146722 = AXIS2_PLACEMENT_3D ( 'NONE', #5716, #106101, #125687 ) ;
#146724 = EDGE_CURVE ( 'NONE', #104599, #81676, #5023, .T. ) ;
#146723 = CARTESIAN_POINT ( 'NONE',  ( -16.84421487269769813, 9.950000000011140600, -113.1695021224450386 ) ) ;
#146725 = VECTOR ( 'NONE', #139333, 1000.000000000000000 ) ;
#146727 = FACE_OUTER_BOUND ( 'NONE', #244805, .T. ) ;
#146726 = DIRECTION ( 'NONE',  ( -3.787827842127534447E-15, -0.7397360091702729346, -0.6728971962616859814 ) ) ;
#146728 = CARTESIAN_POINT ( 'NONE',  ( 18.56308993302899069, 10.38069115533549969, -91.73922263893888385 ) ) ;
#146729 = CARTESIAN_POINT ( 'NONE',  ( 18.52326479938723480, 85.64236444492753719, -163.3083500711181273 ) ) ;
#146730 = CARTESIAN_POINT ( 'NONE',  ( 18.49999999999998934, 6.650000000011155876, -79.35000000000005116 ) ) ;
#146731 = VERTEX_POINT ( 'NONE', #144548 ) ;
#146732 = ORIENTED_EDGE ( 'NONE', *, *, #172376, .F. ) ;
#146733 = ORIENTED_EDGE ( 'NONE', *, *, #138350, .T. ) ;
#146734 = CARTESIAN_POINT ( 'NONE',  ( 20.94999999999999929, -1.835341550213257733, -45.05515129256298223 ) ) ;
#146735 = ORIENTED_EDGE ( 'NONE', *, *, #521, .F. ) ;
#146736 = DIRECTION ( 'NONE',  ( 0.000000000000000000, 0.000000000000000000, -1.000000000000000000 ) ) ;
#146737 = ORIENTED_EDGE ( 'NONE', *, *, #543, .T. ) ;
#146738 = DIRECTION ( 'NONE',  ( 1.000000000000000000, 0.000000000000000000, 0.000000000000000000 ) ) ;
#146739 = CARTESIAN_POINT ( 'NONE',  ( 21.05000000000000071, 68.05808644172607558, -213.7045301755741491 ) ) ;
#146740 = EDGE_CURVE ( 'NONE', #5738, #124163, #45462, .T. ) ;
#146741 = ORIENTED_EDGE ( 'NONE', *, *, #63303, .T. ) ;
#146742 = CARTESIAN_POINT ( 'NONE',  ( 15.07585980824112148, 9.417632963117448242, -152.1489484657322748 ) ) ;
#146743 = VECTOR ( 'NONE', #136426, 1000.000000000000000 ) ;
#146744 = VECTOR ( 'NONE', #57242, 1000.000000000000000 ) ;
#146745 = ORIENTED_EDGE ( 'NONE', *, *, #154731, .F. ) ;
#146746 = ORIENTED_EDGE ( 'NONE', *, *, #135063, .T. ) ;
#146747 = ORIENTED_EDGE ( 'NONE', *, *, #141710, .F. ) ;
#146748 = EDGE_CURVE ( 'NONE', #243446, #234900, #85838, .T. ) ;
#146749 = LINE ( 'NONE', #148074, #67057 ) ;
#146750 = CARTESIAN_POINT ( 'NONE',  ( -16.97683809663752186, 66.05000000001207638, -123.1207434663278804 ) ) ;
#146751 = CARTESIAN_POINT ( 'NONE',  ( 17.23472005113826810, 10.30788195451192202, -156.0465768600687113 ) ) ;
#146752 = EDGE_CURVE ( 'NONE', #74012, #157279, #145832, .T. ) ;
#146753 = LINE ( 'NONE', #105044, #107281 ) ;
#146754 = CARTESIAN_POINT ( 'NONE',  ( -18.59999999999999787, -10.74999999999999289, 31.59999999999999787 ) ) ;
#146755 = PLANE ( 'NONE',  #1140 ) ;
#146756 = VECTOR ( 'NONE', #177210, 1000.000000000000000 ) ;
#146758 = CARTESIAN_POINT ( 'NONE',  ( 18.52130828395272033, 85.48139550263843489, -196.4986007606406986 ) ) ;
#146757 = DIRECTION ( 'NONE',  ( 0.000000000000000000, 0.000000000000000000, -1.000000000000000000 ) ) ;
#146759 = FACE_OUTER_BOUND ( 'NONE', #95131, .T. ) ;
#146761 = VERTEX_POINT ( 'NONE', #205818 ) ;
#146760 = FACE_OUTER_BOUND ( 'NONE', #173771, .T. ) ;
#146763 = CARTESIAN_POINT ( 'NONE',  ( -18.39999999999999858, 85.51932773110506503, -196.5501311079649724 ) ) ;
#146762 = CARTESIAN_POINT ( 'NONE',  ( 20.50589344625181809, 10.48318793148705019, -74.57299497867310833 ) ) ;
#146764 = EDGE_CURVE ( 'NONE', #103375, #75051, #191794, .T. ) ;
#146765 = CARTESIAN_POINT ( 'NONE',  ( -18.49999999999997158, -9.321008403350129257, -141.2359382490778614 ) ) ;
#146766 = EDGE_CURVE ( 'NONE', #247339, #127698, #66861, .T. ) ;
#146767 = VERTEX_POINT ( 'NONE', #88413 ) ;
#146768 = CARTESIAN_POINT ( 'NONE',  ( -21.06715728752538652, 57.72708596674831938, -226.0092949359175236 ) ) ;
#146769 = VECTOR ( 'NONE', #38743, 1000.000000000000227 ) ;
#146770 = FACE_OUTER_BOUND ( 'NONE', #71411, .T. ) ;
#146771 = DIRECTION ( 'NONE',  ( 1.000000000000000000, 0.000000000000000000, 0.000000000000000000 ) ) ;
#146772 = ORIENTED_EDGE ( 'NONE', *, *, #131192, .F. ) ;
#146773 = AXIS2_PLACEMENT_3D ( 'NONE', #214959, #136695, #157601 ) ;
#146774 = EDGE_CURVE ( 'NONE', #158981, #186471, #168024, .T. ) ;
#146776 = CARTESIAN_POINT ( 'NONE',  ( -16.93301857435210067, 30.25028764630435418, -234.8007464032908445 ) ) ;
#146775 = CIRCLE ( 'NONE', #51087, 0.1000000000000028644 ) ;
#146777 = AXIS2_PLACEMENT_3D ( 'NONE', #182655, #238763, #139633 ) ;
#146778 = EDGE_CURVE ( 'NONE', #106650, #62040, #104254, .T. ) ;
#146779 = PLANE ( 'NONE',  #181813 ) ;
#146780 = CYLINDRICAL_SURFACE ( 'NONE', #117624, 0.09999999999999920064 ) ;
#146783 = EDGE_CURVE ( 'NONE', #206263, #136054, #220, .T. ) ;
#146782 = EDGE_CURVE ( 'NONE', #191642, #43027, #250022, .T. ) ;
#146781 = VECTOR ( 'NONE', #239538, 1000.000000000000114 ) ;
#146784 = ORIENTED_EDGE ( 'NONE', *, *, #20589, .T. ) ;
#146785 = VERTEX_POINT ( 'NONE', #51856 ) ;
#146786 = AXIS2_PLACEMENT_3D ( 'NONE', #209809, #120999, #59683 ) ;
#146787 = CARTESIAN_POINT ( 'NONE',  ( -18.40000000000000213, 64.52683809664938508, -90.47310748452439100 ) ) ;
#146788 = ORIENTED_EDGE ( 'NONE', *, *, #88758, .T. ) ;
#146789 = DIRECTION ( 'NONE',  ( -1.000000000000000000, -0.000000000000000000, 0.000000000000000000 ) ) ;
#146790 = CARTESIAN_POINT ( 'NONE',  ( -18.59999999999999787, -9.480686695267820596, -174.4411151687578467 ) ) ;
#146791 = CARTESIAN_POINT ( 'NONE',  ( 20.94999999999999929, 40.27305497204160645, -251.4871534980821082 ) ) ;
#146792 = DIRECTION ( 'NONE',  ( 1.000000000000000000, -0.000000000000000000, 0.000000000000000000 ) ) ;
#146793 = ORIENTED_EDGE ( 'NONE', *, *, #36546, .T. ) ;
#146794 = CIRCLE ( 'NONE', #67708, 0.1000000000000028644 ) ;
#146796 = AXIS2_PLACEMENT_3D ( 'NONE', #134299, #31408, #13107 ) ;
#146795 = CARTESIAN_POINT ( 'NONE',  ( -15.39126916658602973, 9.389571634557565716, -118.3176407123691689 ) ) ;
#146797 = EDGE_CURVE ( 'NONE', #176380, #193155, #150094, .T. ) ;
#146798 = DIRECTION ( 'NONE',  ( 0.000000000000000000, 0.9908441862701596881, 0.1350103645451904977 ) ) ;
#146799 = LINE ( 'NONE', #185949, #245136 ) ;
#146800 = AXIS2_PLACEMENT_3D ( 'NONE', #114678, #211209, #110816 ) ;
#146801 = DIRECTION ( 'NONE',  ( 1.000000000000000000, 0.000000000000000000, 0.000000000000000000 ) ) ;
#146802 = EDGE_CURVE ( 'NONE', #94835, #113369, #29792, .T. ) ;
#146803 = EDGE_CURVE ( 'NONE', #198340, #32767, #137569, .T. ) ;
#146804 = EDGE_LOOP ( 'NONE', ( #212155, #99163, #14054, #211243 ) ) ;
#146805 = CARTESIAN_POINT ( 'NONE',  ( 20.94983749550516450, 10.29766095124176850, -38.97436639332756414 ) ) ;
#146806 = AXIS2_PLACEMENT_3D ( 'NONE', #205005, #30265, #168524 ) ;
#146807 = TOROIDAL_SURFACE ( 'NONE', #134161, 0.2000000000000000111, 0.1000000000000000056 ) ;
#146808 = ADVANCED_FACE ( 'NONE', ( #50574 ), #8909, .T. ) ;
#146810 = EDGE_LOOP ( 'NONE', ( #223191, #45191, #14483, #67542 ) ) ;
#146809 = CARTESIAN_POINT ( 'NONE',  ( -23.15000000000000213, 0.000000000000000000, -29.50000000000000355 ) ) ;
#146811 = DIRECTION ( 'NONE',  ( 0.000000000000000000, -0.8777080977375715243, 0.4791956752370512551 ) ) ;
#146812 = DIRECTION ( 'NONE',  ( 1.000000000000000000, -2.952720810173289112E-16, -2.061873921506763405E-30 ) ) ;
#146813 = FACE_OUTER_BOUND ( 'NONE', #70165, .T. ) ;
#146814 = AXIS2_PLACEMENT_3D ( 'NONE', #201568, #205412, #159906 ) ;
#146815 = DIRECTION ( 'NONE',  ( 1.875376730785737719E-16, 1.000000000000000000, 6.982962677686266711E-15 ) ) ;
#146816 = CARTESIAN_POINT ( 'NONE',  ( -23.15000000000000213, 59.07123845373075000, -221.0531397865252075 ) ) ;
#146817 = ADVANCED_FACE ( 'NONE', ( #108010 ), #152292, .T. ) ;
#146818 = DIRECTION ( 'NONE',  ( 1.000000000000000000, 0.000000000000000000, 0.000000000000000000 ) ) ;
#146819 = DIRECTION ( 'NONE',  ( 0.000000000000000000, 0.8814952561688442767, -0.4721928772777324035 ) ) ;
#146820 = ORIENTED_EDGE ( 'NONE', *, *, #26193, .T. ) ;
#146821 = DIRECTION ( 'NONE',  ( -1.000000000000000000, 0.000000000000000000, 0.000000000000000000 ) ) ;
#146822 = CARTESIAN_POINT ( 'NONE',  ( -23.25000000000000000, 73.40000000001199965, -116.2477294072864140 ) ) ;
#146823 = CARTESIAN_POINT ( 'NONE',  ( -18.40000000000000213, 11.41458325961095177, -188.3499999999999943 ) ) ;
#146824 = DIRECTION ( 'NONE',  ( -1.000000000000000000, -1.631532756632575455E-14, -2.455126404641516337E-15 ) ) ;
#146825 = AXIS2_PLACEMENT_3D ( 'NONE', #29514, #149448, #146836 ) ;
#146826 = FACE_OUTER_BOUND ( 'NONE', #54199, .T. ) ;
#146827 = CIRCLE ( 'NONE', #188538, 0.09999999999998898659 ) ;
#146828 = AXIS2_PLACEMENT_3D ( 'NONE', #202924, #244614, #108951 ) ;
#146829 = ORIENTED_EDGE ( 'NONE', *, *, #68430, .T. ) ;
#146830 = ORIENTED_EDGE ( 'NONE', *, *, #216977, .F. ) ;
#146831 = DIRECTION ( 'NONE',  ( 0.000000000000000000, 1.000000000000000000, 6.938893903907222067E-15 ) ) ;
#146832 = DIRECTION ( 'NONE',  ( 0.000000000000000000, 0.000000000000000000, -1.000000000000000000 ) ) ;
#146833 = CYLINDRICAL_SURFACE ( 'NONE', #25028, 11.80000000000000426 ) ;
#146834 =( BOUNDED_CURVE ( )  B_SPLINE_CURVE ( 3, ( #98968, #160293, #177292, #79418 ),
 .UNSPECIFIED., .F., .F. ) 
 B_SPLINE_CURVE_WITH_KNOTS ( ( 4, 4 ),
 ( 3.141592653589791784, 4.712388980384661252 ),
 .UNSPECIFIED. ) 
 CURVE ( )  GEOMETRIC_REPRESENTATION_ITEM ( )  RATIONAL_B_SPLINE_CURVE ( ( 1.000000000000000000, 0.8047378541243714878, 0.8047378541243714878, 1.000000000000000000 ) ) 
 REPRESENTATION_ITEM ( '' )  );
#146835 = CARTESIAN_POINT ( 'NONE',  ( 20.94999999999999929, 61.88149656937974896, -248.1136133839584090 ) ) ;
#146836 = DIRECTION ( 'NONE',  ( 0.000000000000000000, 0.9126074666063660468, 0.4088369013363524762 ) ) ;
#146837 = CYLINDRICAL_SURFACE ( 'NONE', #238158, 0.09999999999999939493 ) ;
#146838 = CARTESIAN_POINT ( 'NONE',  ( -20.94999999999999929, 17.04749343158673014, -224.5908524457887268 ) ) ;
#146839 = AXIS2_PLACEMENT_3D ( 'NONE', #54075, #11111, #51480 ) ;
#146840 = ORIENTED_EDGE ( 'NONE', *, *, #177754, .F. ) ;
#146841 = CARTESIAN_POINT ( 'NONE',  ( -20.85000000000000142, -1.835859311432481045, -145.5044391687985694 ) ) ;
#146842 = AXIS2_PLACEMENT_3D ( 'NONE', #151380, #129231, #230917 ) ;
#146843 = EDGE_LOOP ( 'NONE', ( #80623, #242560, #251376, #215688, #193196 ) ) ;
#146844 = CARTESIAN_POINT ( 'NONE',  ( 20.95512820512820440, 30.05186296287165248, -235.9425146762463328 ) ) ;
#146845 = FACE_OUTER_BOUND ( 'NONE', #78640, .T. ) ;
#146846 = DIRECTION ( 'NONE',  ( -0.000000000000000000, -1.000000000000000000, -6.982962677686266711E-15 ) ) ;
#146847 = LINE ( 'NONE', #6064, #61342 ) ;
#146848 = CARTESIAN_POINT ( 'NONE',  ( -21.05000000000000071, 7.128833340093095217, -233.7327013124392749 ) ) ;
#146849 = FACE_OUTER_BOUND ( 'NONE', #182210, .T. ) ;
#146850 = DIRECTION ( 'NONE',  ( 0.000000000000000000, 0.1350103645451904977, 0.9908441862701596881 ) ) ;
#146851 = VERTEX_POINT ( 'NONE', #148428 ) ;
#146852 = CARTESIAN_POINT ( 'NONE',  ( 21.05000000000000071, 67.23127455305835554, -235.8551265064784559 ) ) ;
#146853 = EDGE_CURVE ( 'NONE', #99703, #43253, #237562, .T. ) ;
#146854 = CARTESIAN_POINT ( 'NONE',  ( -20.94999999999999929, 70.47363787294415260, -228.3418745167492432 ) ) ;
#146855 = CARTESIAN_POINT ( 'NONE',  ( -20.05000000000000426, 66.75000000001205080, -124.1731074845243654 ) ) ;
#146856 = CARTESIAN_POINT ( 'NONE',  ( -17.11825945287482753, 66.05000000001230376, -157.2731074845244166 ) ) ;
#146857 = EDGE_CURVE ( 'NONE', #223804, #13993, #50095, .T. ) ;
#146858 = CARTESIAN_POINT ( 'NONE',  ( 21.30000000000002558, 76.00000000001165290, -69.52310748452431710 ) ) ;
#146859 = CARTESIAN_POINT ( 'NONE',  ( 21.05000000000000071, 8.776282648982402179, -175.9875923785215832 ) ) ;
#146860 = AXIS2_PLACEMENT_3D ( 'NONE', #214230, #298, #175150 ) ;
#146861 = ORIENTED_EDGE ( 'NONE', *, *, #54873, .T. ) ;
#146862 = FACE_OUTER_BOUND ( 'NONE', #99826, .T. ) ;
#146864 = EDGE_CURVE ( 'NONE', #103901, #179560, #187568, .T. ) ;
#146863 = DIRECTION ( 'NONE',  ( 1.301042606982683734E-14, 0.8660254037844367092, -0.5000000000000037748 ) ) ;
#146865 = ADVANCED_FACE ( 'NONE', ( #130126 ), #31075, .T. ) ;
#146866 = ORIENTED_EDGE ( 'NONE', *, *, #194335, .T. ) ;
#146867 = CARTESIAN_POINT ( 'NONE',  ( -20.54999999999999716, 4.350000000011156054, -146.3500000000000227 ) ) ;
#146868 = DIRECTION ( 'NONE',  ( 1.000000000000000000, 7.304098846218134667E-16, -0.000000000000000000 ) ) ;
#146869 = DIRECTION ( 'NONE',  ( 0.000000000000000000, 0.000000000000000000, 1.000000000000000000 ) ) ;
#146870 = VERTEX_POINT ( 'NONE', #210962 ) ;
#146871 = CARTESIAN_POINT ( 'NONE',  ( 20.99551997958372596, 64.25000000001146816, -42.87144834683482486 ) ) ;
#146872 = PLANE ( 'NONE',  #243276 ) ;
#146873 = AXIS2_PLACEMENT_3D ( 'NONE', #128563, #107707, #208120 ) ;
#146874 = ORIENTED_EDGE ( 'NONE', *, *, #32683, .T. ) ;
#146875 = AXIS2_PLACEMENT_3D ( 'NONE', #216181, #97498, #254028 ) ;
#146876 = ADVANCED_FACE ( 'NONE', ( #32353 ), #111865, .T. ) ;
#146877 = ADVANCED_FACE ( 'NONE', ( #181953 ), #64558, .F. ) ;
#146878 = LINE ( 'NONE', #236400, #227121 ) ;
#146879 = VECTOR ( 'NONE', #221176, 1000.000000000000000 ) ;
#146880 = ORIENTED_EDGE ( 'NONE', *, *, #140322, .T. ) ;
#146881 = FACE_OUTER_BOUND ( 'NONE', #30072, .T. ) ;
#146882 = CARTESIAN_POINT ( 'NONE',  ( 22.50046968638084621, 0.04516984715173071041, -21.74995484552572833 ) ) ;
#146883 = CARTESIAN_POINT ( 'NONE',  ( 20.94999999999999574, 2.817198581588411077, -208.4716308468294130 ) ) ;
#146885 = DIRECTION ( 'NONE',  ( 1.000000000000000000, 0.000000000000000000, 0.000000000000000000 ) ) ;
#146884 = UNCERTAINTY_MEASURE_WITH_UNIT (LENGTH_MEASURE( 1.000000000000000082E-05 ), #123024, 'distance_accuracy_value', 'NONE');
#146886 = CYLINDRICAL_SURFACE ( 'NONE', #58601, 0.09999999999999939493 ) ;
#146887 = CARTESIAN_POINT ( 'NONE',  ( -23.15000000000000213, 1.115651490242849210E-11, -129.8500000000000227 ) ) ;
#146888 = DIRECTION ( 'NONE',  ( 0.000000000000000000, 0.2617529984165152257, 0.9651348961777124202 ) ) ;
#146889 = AXIS2_PLACEMENT_3D ( 'NONE', #81275, #61744, #201242 ) ;
#146890 = LINE ( 'NONE', #28290, #255307 ) ;
#146892 = DIRECTION ( 'NONE',  ( 0.000000000000000000, 0.000000000000000000, -1.000000000000000000 ) ) ;
#146891 = CIRCLE ( 'NONE', #5424, 0.09999999999998898659 ) ;
#146895 = EDGE_LOOP ( 'NONE', ( #244152, #95447, #35317, #224865, #214027, #199292, #180936, #3455, #126388, #225275, #101683, #182850 ) ) ;
#146894 = EDGE_CURVE ( 'NONE', #187034, #186207, #166857, .T. ) ;
#146893 = DIRECTION ( 'NONE',  ( 1.000000000000000000, 0.000000000000000000, 0.000000000000000000 ) ) ;
#146896 = VERTEX_POINT ( 'NONE', #146646 ) ;
#146898 = CARTESIAN_POINT ( 'NONE',  ( -23.25000000000000000, 73.40000000001228386, -156.7984855617622770 ) ) ;
#146897 = DIRECTION ( 'NONE',  ( 1.000000000000000000, 0.000000000000000000, -0.000000000000000000 ) ) ;
#146900 = EDGE_LOOP ( 'NONE', ( #92504, #116775, #212512, #199952 ) ) ;
#146899 = DIRECTION ( 'NONE',  ( 0.000000000000000000, -1.000000000000000000, 0.000000000000000000 ) ) ;
#146901 = VERTEX_POINT ( 'NONE', #205340 ) ;
#146902 = EDGE_CURVE ( 'NONE', #77358, #208902, #170969, .T. ) ;
#146903 = DIRECTION ( 'NONE',  ( 1.000000000000000000, 0.000000000000000000, 0.000000000000000000 ) ) ;
#146904 = CARTESIAN_POINT ( 'NONE',  ( 18.59999999999998721, 56.14960075277880946, -167.7428044267231257 ) ) ;
#146905 = CYLINDRICAL_SURFACE ( 'NONE', #46663, 0.1000000000000055844 ) ;
#146906 = CIRCLE ( 'NONE', #134262, 14.30833333333333890 ) ;
#146907 = CYLINDRICAL_SURFACE ( 'NONE', #248520, 0.09999999999999982514 ) ;
#146908 = CARTESIAN_POINT ( 'NONE',  ( -18.58222699835055280, 67.49225400653517681, -195.4205142095401584 ) ) ;
#146910 = EDGE_CURVE ( 'NONE', #113296, #100104, #242046, .T. ) ;
#146909 = CARTESIAN_POINT ( 'NONE',  ( -23.15000000000000213, 76.00000000001244871, -170.0231074845243597 ) ) ;
#146911 = AXIS2_PLACEMENT_3D ( 'NONE', #93259, #253608, #176676 ) ;
#146912 = CIRCLE ( 'NONE', #250967, 0.09999999999999344136 ) ;
#146913 = CIRCLE ( 'NONE', #230139, 4.000000000000003553 ) ;
#146914 = EDGE_CURVE ( 'NONE', #251279, #125644, #220795, .T. ) ;
#146916 = AXIS2_PLACEMENT_3D ( 'NONE', #68588, #12476, #151997 ) ;
#146915 = DIRECTION ( 'NONE',  ( 1.000000000000000000, -0.000000000000000000, -0.000000000000000000 ) ) ;
#146917 = ORIENTED_EDGE ( 'NONE', *, *, #153372, .F. ) ;
#146918 = ORIENTED_EDGE ( 'NONE', *, *, #167375, .F. ) ;
#146919 = DIRECTION ( 'NONE',  ( -1.000000000000000000, 7.304098846218135653E-16, 0.000000000000000000 ) ) ;
#146920 = EDGE_CURVE ( 'NONE', #165929, #239420, #200140, .T. ) ;
#146921 = ORIENTED_EDGE ( 'NONE', *, *, #233033, .T. ) ;
#146922 = CARTESIAN_POINT ( 'NONE',  ( -21.05000000000000071, 1.148907358139439339E-11, -201.0000000000015064 ) ) ;
#146923 = ORIENTED_EDGE ( 'NONE', *, *, #120611, .F. ) ;
#146924 = CARTESIAN_POINT ( 'NONE',  ( 23.14999999999999858, 5.000000000011153745, -188.5947339810868755 ) ) ;
#146925 = EDGE_CURVE ( 'NONE', #122271, #129700, #102371, .T. ) ;
#146926 =( BOUNDED_CURVE ( )  B_SPLINE_CURVE ( 3, ( #116232, #253142, #113642, #138312 ),
 .UNSPECIFIED., .F., .T. ) 
 B_SPLINE_CURVE_WITH_KNOTS ( ( 4, 4 ),
 ( 0.000000000000000000, 1.570796326794908992 ),
 .UNSPECIFIED. ) 
 CURVE ( )  GEOMETRIC_REPRESENTATION_ITEM ( )  RATIONAL_B_SPLINE_CURVE ( ( 1.000000000000000000, 0.8047378541243619399, 0.8047378541243619399, 1.000000000000000000 ) ) 
 REPRESENTATION_ITEM ( '' )  );
#146927 = CARTESIAN_POINT ( 'NONE',  ( -20.94999999999999929, 1.115600667400684642E-11, -33.50000000000000000 ) ) ;
#146928 = CARTESIAN_POINT ( 'NONE',  ( 18.39999999999999858, -9.599999999988845900, -73.70018939122203960 ) ) ;
#146929 = DIRECTION ( 'NONE',  ( 1.000000000000000000, 0.000000000000000000, 0.000000000000000000 ) ) ;
#146930 = ORIENTED_EDGE ( 'NONE', *, *, #7601, .T. ) ;
#146931 = EDGE_CURVE ( 'NONE', #179208, #109066, #67133, .T. ) ;
#146932 = CARTESIAN_POINT ( 'NONE',  ( -21.00448002041601114, 11.75000000000000000, -6.848340862310549504 ) ) ;
#146933 = VERTEX_POINT ( 'NONE', #183237 ) ;
#146934 = CARTESIAN_POINT ( 'NONE',  ( -16.97683809663753252, 66.05000000001152216, -49.29463665241382131 ) ) ;
#146935 = CARTESIAN_POINT ( 'NONE',  ( 23.14999999999999858, 67.44464249442897597, -214.0562211244547655 ) ) ;
#146936 = PLANE ( 'NONE',  #79794 ) ;
#146937 = EDGE_CURVE ( 'NONE', #28183, #174500, #120876, .T. ) ;
#146938 = CARTESIAN_POINT ( 'NONE',  ( -21.05000000000000071, -1.835341550224411922, -11.55515129256297868 ) ) ;
#146939 = ORIENTED_EDGE ( 'NONE', *, *, #12374, .F. ) ;
#146940 = AXIS2_PLACEMENT_3D ( 'NONE', #23947, #162172, #38358 ) ;
#146941 = CARTESIAN_POINT ( 'NONE',  ( -18.39999999999999858, -9.600000000000001421, -7.032069396699667685 ) ) ;
#146942 = ORIENTED_EDGE ( 'NONE', *, *, #14946, .F. ) ;
#146945 = ORIENTED_EDGE ( 'NONE', *, *, #192717, .F. ) ;
#146944 = FACE_OUTER_BOUND ( 'NONE', #114852, .T. ) ;
#146943 = DIRECTION ( 'NONE',  ( 0.000000000000000000, -0.7397360091702647189, -0.6728971962616949742 ) ) ;
#146946 = DIRECTION ( 'NONE',  ( 0.000000000000000000, 0.000000000000000000, 1.000000000000000000 ) ) ;
#146947 = ORIENTED_EDGE ( 'NONE', *, *, #241130, .F. ) ;
#146948 = CYLINDRICAL_SURFACE ( 'NONE', #100370, 0.5000000000000008882 ) ;
#146949 = EDGE_LOOP ( 'NONE', ( #170361, #59759, #254664, #109788, #235444, #95837, #96100, #161782, #169888, #9492, #55607, #219479, #33329, #121339, #47682, #214644, #195885, #158230 ) ) ;
#146950 = AXIS2_PLACEMENT_3D ( 'NONE', #71327, #110425, #111717 ) ;
#146951 = EDGE_CURVE ( 'NONE', #211620, #243100, #127105, .T. ) ;
#146952 = AXIS2_PLACEMENT_3D ( 'NONE', #35481, #74614, #92840 ) ;
#146953 = DIRECTION ( 'NONE',  ( 0.000000000000000000, -6.652207440891584540E-15, 1.000000000000000000 ) ) ;
#146954 = CYLINDRICAL_SURFACE ( 'NONE', #92998, 0.09999999999999939493 ) ;
#146955 = DIRECTION ( 'NONE',  ( -1.000000000000000000, 0.000000000000000000, 0.000000000000000000 ) ) ;
#146956 = AXIS2_PLACEMENT_3D ( 'NONE', #245297, #27567, #151347 ) ;
#146957 = DIRECTION ( 'NONE',  ( 1.000000000000000000, 0.000000000000000000, -0.000000000000000000 ) ) ;
#146958 = VECTOR ( 'NONE', #47539, 1000.000000000000000 ) ;
#146959 = VERTEX_POINT ( 'NONE', #144081 ) ;
#146960 = VECTOR ( 'NONE', #163405, 1000.000000000000000 ) ;
#146961 = CIRCLE ( 'NONE', #117938, 0.09999999999999939493 ) ;
#146962 = CYLINDRICAL_SURFACE ( 'NONE', #135948, 7.900000000000007461 ) ;
#146963 = CARTESIAN_POINT ( 'NONE',  ( -16.91776028072577631, 9.963400393640901243, -188.3750240147020918 ) ) ;
#146964 = CARTESIAN_POINT ( 'NONE',  ( -13.12432614554023935, 66.56923500458995591, -154.7925700897739887 ) ) ;
#146965 = ORIENTED_EDGE ( 'NONE', *, *, #77801, .F. ) ;
#146966 = CARTESIAN_POINT ( 'NONE',  ( 20.94999999999999929, 11.60058429089262333, -246.3380203656811887 ) ) ;
#146967 = ORIENTED_EDGE ( 'NONE', *, *, #54871, .F. ) ;
#146968 = CARTESIAN_POINT ( 'NONE',  ( -22.50000000000000000, 1.115600667400684642E-11, -88.85042919245522341 ) ) ;
#146969 = CIRCLE ( 'NONE', #34585, 5.000000000000000888 ) ;
#146970 = CARTESIAN_POINT ( 'NONE',  ( -20.94999999999999929, 33.13294339707397995, -247.6623911921324463 ) ) ;
#146971 = CARTESIAN_POINT ( 'NONE',  ( -20.64999999999999858, 4.349999999999999645, -21.14999999999999858 ) ) ;
#146973 = VERTEX_POINT ( 'NONE', #87952 ) ;
#146972 = PLANE ( 'NONE',  #111145 ) ;
#146974 = DIRECTION ( 'NONE',  ( 0.000000000000000000, -0.2617529984165152257, -0.9651348961777124202 ) ) ;
#146975 = CARTESIAN_POINT ( 'NONE',  ( -12.33960340485503693, 62.72902952540357546, -216.6940264888115166 ) ) ;
#146976 = AXIS2_PLACEMENT_3D ( 'NONE', #164167, #62498, #85869 ) ;
#146977 = CARTESIAN_POINT ( 'NONE',  ( -23.25000000000000000, 7.567413955921500346, -241.6205176796878504 ) ) ;
#146978 = ORIENTED_EDGE ( 'NONE', *, *, #238731, .F. ) ;
#146979 = AXIS2_PLACEMENT_3D ( 'NONE', #102374, #243196, #3288 ) ;
#146980 = CARTESIAN_POINT ( 'NONE',  ( -20.64999999999999858, 68.85000000001151932, -48.37310748452436826 ) ) ;
#146981 = CARTESIAN_POINT ( 'NONE',  ( -22.45354308602221138, -3.229117406951398372, -228.1842304028190540 ) ) ;
#146982 = ORIENTED_EDGE ( 'NONE', *, *, #70820, .T. ) ;
#146983 = CARTESIAN_POINT ( 'NONE',  ( -21.07016717457011268, 65.57674933587216515, -241.9556870860043603 ) ) ;
#146984 = TOROIDAL_SURFACE ( 'NONE', #34430, 11.89999999999999858, 0.1000000000000000056 ) ;
#146985 = ORIENTED_EDGE ( 'NONE', *, *, #161025, .F. ) ;
#146986 = AXIS2_PLACEMENT_3D ( 'NONE', #169999, #69583, #107399 ) ;
#146987 = AXIS2_PLACEMENT_3D ( 'NONE', #63903, #121350, #3932 ) ;
#146988 = CARTESIAN_POINT ( 'NONE',  ( -16.77683809663752257, 44.14991418685006153, -235.2970290647049580 ) ) ;
#146989 = AXIS2_PLACEMENT_3D ( 'NONE', #69551, #49962, #109933 ) ;
#146991 = ORIENTED_EDGE ( 'NONE', *, *, #137013, .T. ) ;
#146990 = DIRECTION ( 'NONE',  ( 0.000000000000000000, -1.000000000000000000, 0.000000000000000000 ) ) ;
#146992 = EDGE_CURVE ( 'NONE', #246301, #147579, #216871, .T. ) ;
#146995 = VERTEX_POINT ( 'NONE', #121977 ) ;
#146994 = ORIENTED_EDGE ( 'NONE', *, *, #34015, .T. ) ;
#146993 = CARTESIAN_POINT ( 'NONE',  ( 20.12500000000000000, 66.25000000001151079, -48.27310748452438816 ) ) ;
#146996 = EDGE_CURVE ( 'NONE', #104540, #129072, #201499, .T. ) ;
#146997 = DIRECTION ( 'NONE',  ( -3.265361837132813093E-16, -1.000000000000000000, 7.445645354460596589E-46 ) ) ;
#146998 = ADVANCED_FACE ( 'NONE', ( #142792 ), #25454, .F. ) ;
#146999 = FACE_BOUND ( 'NONE', #184206, .T. ) ;
#147000 = DIRECTION ( 'NONE',  ( 0.000000000000000000, 1.000000000000000000, 6.982962677686266711E-15 ) ) ;
#147002 = CARTESIAN_POINT ( 'NONE',  ( -23.15000000000000213, 6.780748427709700543, -212.1627259556213403 ) ) ;
#147001 = CARTESIAN_POINT ( 'NONE',  ( 22.39999999999999503, 11.65000000001116298, -33.60000000000000142 ) ) ;
#147003 = CARTESIAN_POINT ( 'NONE',  ( -18.79999999999999716, 0.000000000000000000, 0.000000000000000000 ) ) ;
#147004 = DIRECTION ( 'NONE',  ( 1.000000000000000000, 0.000000000000000000, 0.000000000000000000 ) ) ;
#147005 = VECTOR ( 'NONE', #80873, 1000.000000000000114 ) ;
#147006 = LINE ( 'NONE', #182317, #159857 ) ;
#147007 = VECTOR ( 'NONE', #233209, 1000.000000000000000 ) ;
#147008 = LINE ( 'NONE', #227839, #59208 ) ;
#147009 = VECTOR ( 'NONE', #89542, 1000.000000000000000 ) ;
#147010 = AXIS2_PLACEMENT_3D ( 'NONE', #189021, #152490, #93760 ) ;
#147011 = VERTEX_POINT ( 'NONE', #65843 ) ;
#147012 = ORIENTED_EDGE ( 'NONE', *, *, #13614, .T. ) ;
#147013 = CARTESIAN_POINT ( 'NONE',  ( -21.02374657821586013, 64.39999999919189122, -76.45131071432655290 ) ) ;
#147015 = VERTEX_POINT ( 'NONE', #224904 ) ;
#147014 = DIRECTION ( 'NONE',  ( 0.000000000000000000, -1.000000000000000000, 0.000000000000000000 ) ) ;
#147016 = ORIENTED_EDGE ( 'NONE', *, *, #71783, .T. ) ;
#147017 = ADVANCED_FACE ( 'NONE', ( #171415 ), #116930, .F. ) ;
#147018 = DIRECTION ( 'NONE',  ( -0.000000000000000000, -0.1332476588733650935, 0.9910827722268042983 ) ) ;
#147019 = EDGE_LOOP ( 'NONE', ( #66797, #18972, #185194, #230767 ) ) ;
#147020 = CARTESIAN_POINT ( 'NONE',  ( -21.05000000000000071, 69.69503888732714358, -136.5017219185863837 ) ) ;
#147021 = VERTEX_POINT ( 'NONE', #232654 ) ;
#147022 = DIRECTION ( 'NONE',  ( 0.000000000000000000, 0.000000000000000000, 1.000000000000000000 ) ) ;
#147023 = DIRECTION ( 'NONE',  ( 0.000000000000000000, -0.9964539953858966292, -0.08413937888696132461 ) ) ;
#147025 = ORIENTED_EDGE ( 'NONE', *, *, #39002, .F. ) ;
#147024 = VERTEX_POINT ( 'NONE', #51388 ) ;
#147026 = ORIENTED_EDGE ( 'NONE', *, *, #125672, .F. ) ;
#147027 = CARTESIAN_POINT ( 'NONE',  ( 23.14999999999998437, 1.148907358139439339E-11, -201.0000000000015064 ) ) ;
#147028 = ORIENTED_EDGE ( 'NONE', *, *, #72688, .F. ) ;
#147029 = VERTEX_POINT ( 'NONE', #132247 ) ;
#147030 = DIRECTION ( 'NONE',  ( 0.000000000000000000, -0.000000000000000000, -1.000000000000000000 ) ) ;
#147031 = TOROIDAL_SURFACE ( 'NONE', #92874, 4.149999999999999467, 0.1000000000000000056 ) ;
#147032 = CARTESIAN_POINT ( 'NONE',  ( -20.85000000000000142, 62.42744096235649920, -225.1319887738535499 ) ) ;
#147034 = EDGE_LOOP ( 'NONE', ( #112040, #63676, #32811, #141949 ) ) ;
#147033 = FACE_OUTER_BOUND ( 'NONE', #205033, .T. ) ;
#147035 = EDGE_CURVE ( 'NONE', #201510, #138550, #187688, .T. ) ;
#147036 = EDGE_CURVE ( 'NONE', #206570, #231923, #41948, .T. ) ;
#147037 = B_SPLINE_CURVE_WITH_KNOTS ( 'NONE', 3,
 ( #205655, #11324, #206959, #10035, #166575, #27067, #106549, #67438, #25753, #128712, #89561, #144383, #208255, #204376 ),
 .UNSPECIFIED., .F., .F.,
 ( 4, 2, 2, 2, 2, 2, 4 ),
 ( 1.734723475976807094E-18, 0.0003823333598417674945, 0.0005735000397626501033, 0.0006690833797230904319, 0.0007168750497033101084, 0.0007407708846934187540, 0.0007646667196835271827 ),
 .UNSPECIFIED. ) ;
#147038 = FACE_OUTER_BOUND ( 'NONE', #97208, .T. ) ;
#147039 = DIRECTION ( 'NONE',  ( 0.000000000000000000, -1.000000000000000000, -0.000000000000000000 ) ) ;
#147041 = VERTEX_POINT ( 'NONE', #89254 ) ;
#147040 = DIRECTION ( 'NONE',  ( 0.7071067811865473507, 0.3338907855510733769, 0.6233112732207618523 ) ) ;
#147042 = DIRECTION ( 'NONE',  ( 0.000000000000000000, 0.000000000000000000, -1.000000000000000000 ) ) ;
#147043 = EDGE_LOOP ( 'NONE', ( #171793, #76381, #99772, #95413 ) ) ;
#147044 = CARTESIAN_POINT ( 'NONE',  ( -21.05000000000000071, 69.74218538953043378, -103.1208977758335834 ) ) ;
#147045 = ORIENTED_EDGE ( 'NONE', *, *, #14831, .F. ) ;
#147046 = CARTESIAN_POINT ( 'NONE',  ( -21.14999999893457527, 18.71048982429471508, -226.6070540022291482 ) ) ;
#147047 = FACE_OUTER_BOUND ( 'NONE', #169164, .T. ) ;
#147048 = ADVANCED_FACE ( 'NONE', ( #173994 ), #191971, .F. ) ;
#147049 = ORIENTED_EDGE ( 'NONE', *, *, #68782, .F. ) ;
#147051 = DIRECTION ( 'NONE',  ( 1.000000000000000000, 0.000000000000000000, 0.000000000000000000 ) ) ;
#147050 = CARTESIAN_POINT ( 'NONE',  ( 19.99999999999998934, 11.65000000001115943, -121.7500000000000426 ) ) ;
#147052 = AXIS2_PLACEMENT_3D ( 'NONE', #238341, #8412, #204026 ) ;
#147053 = TOROIDAL_SURFACE ( 'NONE', #34664, 0.6000000000000006439, 0.1000000000000000056 ) ;
#147054 = DIRECTION ( 'NONE',  ( -0.000000000000000000, -6.982962677686266711E-15, 1.000000000000000000 ) ) ;
#147055 = CARTESIAN_POINT ( 'NONE',  ( -12.25000000000000178, 12.70026017068886404, -215.3766613508543628 ) ) ;
#147056 = ORIENTED_EDGE ( 'NONE', *, *, #161715, .T. ) ;
#147057 = VERTEX_POINT ( 'NONE', #249640 ) ;
#147058 = CYLINDRICAL_SURFACE ( 'NONE', #192914, 0.1000000000000124678 ) ;
#147059 = LINE ( 'NONE', #67535, #198311 ) ;
#147060 = VERTEX_POINT ( 'NONE', #113959 ) ;
#147061 = DIRECTION ( 'NONE',  ( 0.000000000000000000, -0.5000000000000014433, 0.8660254037844378194 ) ) ;
#147062 = ORIENTED_EDGE ( 'NONE', *, *, #88382, .T. ) ;
#147063 = FACE_OUTER_BOUND ( 'NONE', #50546, .T. ) ;
#147064 = ORIENTED_EDGE ( 'NONE', *, *, #203096, .F. ) ;
#147065 = CARTESIAN_POINT ( 'NONE',  ( -20.95000000000000284, 64.37928932189282705, -42.89152413686537813 ) ) ;
#147066 = EDGE_CURVE ( 'NONE', #55645, #31259, #91976, .T. ) ;
#147067 = DIRECTION ( 'NONE',  ( 1.000000000000000000, -0.000000000000000000, -0.000000000000000000 ) ) ;
#147068 = VERTEX_POINT ( 'NONE', #211795 ) ;
#147069 = AXIS2_PLACEMENT_3D ( 'NONE', #22458, #117681, #137242 ) ;
#147070 = CARTESIAN_POINT ( 'NONE',  ( 18.31325810956164801, -9.536388475995789094, -207.8684402063061896 ) ) ;
#147071 = AXIS2_PLACEMENT_3D ( 'NONE', #254949, #136317, #213308 ) ;
#147072 = ORIENTED_EDGE ( 'NONE', *, *, #97624, .T. ) ;
#147073 = ORIENTED_EDGE ( 'NONE', *, *, #172509, .T. ) ;
#147074 = VERTEX_POINT ( 'NONE', #52696 ) ;
#147075 = VECTOR ( 'NONE', #217973, 1000.000000000000000 ) ;
#147076 = EDGE_CURVE ( 'NONE', #176425, #133237, #237730, .T. ) ;
#147077 = CARTESIAN_POINT ( 'NONE',  ( 22.49999999999999645, 64.25043287652275126, -136.6239658536231332 ) ) ;
#147078 = CARTESIAN_POINT ( 'NONE',  ( 16.87683809663749557, 9.949999999999976197, -20.85000000000000142 ) ) ;
#147079 = DIRECTION ( 'NONE',  ( -1.000000000000000000, -2.952720810173289112E-16, 0.000000000000000000 ) ) ;
#147080 = CARTESIAN_POINT ( 'NONE',  ( -13.39999999999994529, 67.75000000001118394, -21.02310748452479316 ) ) ;
#147081 = FACE_OUTER_BOUND ( 'NONE', #244164, .T. ) ;
#147083 = CARTESIAN_POINT ( 'NONE',  ( 20.85000000000000142, -11.64999999998883595, -200.9999999999999432 ) ) ;
#147082 = CARTESIAN_POINT ( 'NONE',  ( 23.14999999999999858, 36.65892442174935439, -249.5511627012433848 ) ) ;
#147085 = ORIENTED_EDGE ( 'NONE', *, *, #150804, .T. ) ;
#147084 = CARTESIAN_POINT ( 'NONE',  ( -21.05000000000000071, 18.82290990851281975, -233.3604470821920529 ) ) ;
#147086 = CARTESIAN_POINT ( 'NONE',  ( -13.39999999999994529, 63.75000000001119815, -21.02310748452479316 ) ) ;
#147087 = ORIENTED_EDGE ( 'NONE', *, *, #146914, .T. ) ;
#147088 = EDGE_CURVE ( 'NONE', #203694, #69974, #42487, .T. ) ;
#147089 = EDGE_CURVE ( 'NONE', #40483, #156131, #252180, .T. ) ;
#147090 = ORIENTED_EDGE ( 'NONE', *, *, #217240, .F. ) ;
#147091 = ORIENTED_EDGE ( 'NONE', *, *, #88344, .F. ) ;
#147092 = CARTESIAN_POINT ( 'NONE',  ( -18.40000000000000213, 70.35000000001207354, -123.8731074845243398 ) ) ;
#147094 = AXIS2_PLACEMENT_3D ( 'NONE', #164701, #205083, #26482 ) ;
#147093 = FACE_BOUND ( 'NONE', #57509, .T. ) ;
#147095 = CARTESIAN_POINT ( 'NONE',  ( 20.94999999999999929, 84.73084112150731073, -112.6211822035085675 ) ) ;
#147096 = AXIS2_PLACEMENT_3D ( 'NONE', #244173, #119119, #81243 ) ;
#147097 = CARTESIAN_POINT ( 'NONE',  ( -23.15000000000000213, 74.95298800634525094, -207.3836470692357636 ) ) ;
#147098 = AXIS2_PLACEMENT_3D ( 'NONE', #65747, #145267, #166170 ) ;
#147099 = EDGE_CURVE ( 'NONE', #194221, #193203, #21280, .T. ) ;
#147100 = CARTESIAN_POINT ( 'NONE',  ( 21.14999999999999503, -3.187427350888460076, -228.3200064793908837 ) ) ;
#147101 = ADVANCED_FACE ( 'NONE', ( #34467 ), #228793, .T. ) ;
#147102 = ORIENTED_EDGE ( 'NONE', *, *, #21700, .T. ) ;
#147103 = VERTEX_POINT ( 'NONE', #11016 ) ;
#147104 = CIRCLE ( 'NONE', #63726, 0.09999999999999939493 ) ;
#147105 = CARTESIAN_POINT ( 'NONE',  ( 20.27550659511089037, 9.216043722508848290, -20.84999999999999787 ) ) ;
#147106 = ORIENTED_EDGE ( 'NONE', *, *, #62654, .F. ) ;
#147107 = DIRECTION ( 'NONE',  ( 0.000000000000000000, 0.000000000000000000, 1.000000000000000000 ) ) ;
#147108 = DIRECTION ( 'NONE',  ( 0.000000000000000000, 0.000000000000000000, -1.000000000000000000 ) ) ;
#147109 = ORIENTED_EDGE ( 'NONE', *, *, #256031, .F. ) ;
#147110 = FACE_OUTER_BOUND ( 'NONE', #45194, .T. ) ;
#147112 = ADVANCED_FACE ( 'NONE', ( #153139 ), #91837, .F. ) ;
#147111 = DIRECTION ( 'NONE',  ( -0.000000000000000000, 0.2128009952263603677, -0.9770955615653313941 ) ) ;
#147113 = CARTESIAN_POINT ( 'NONE',  ( -17.04295772865479464, 65.97510057475051326, -123.8731074845243683 ) ) ;
#147114 = DIRECTION ( 'NONE',  ( 0.000000000000000000, 1.000000000000000000, 1.387778780781444413E-14 ) ) ;
#147115 = ORIENTED_EDGE ( 'NONE', *, *, #162849, .T. ) ;
#147116 = DIRECTION ( 'NONE',  ( -1.020425574104004196E-15, -1.210927747993693964E-31, -1.000000000000000000 ) ) ;
#147117 = CIRCLE ( 'NONE', #80437, 12.97500000000000320 ) ;
#147119 = DIRECTION ( 'NONE',  ( 0.000000000000000000, 6.982962677686266711E-15, -1.000000000000000000 ) ) ;
#147118 = CIRCLE ( 'NONE', #163696, 12.87499999999999822 ) ;
#147121 = DIRECTION ( 'NONE',  ( 0.000000000000000000, -1.000000000000000000, -6.982962677686265922E-15 ) ) ;
#147120 = AXIS2_PLACEMENT_3D ( 'NONE', #96206, #216152, #177066 ) ;
#147122 = AXIS2_PLACEMENT_3D ( 'NONE', #24032, #25319, #200084 ) ;
#147123 = CARTESIAN_POINT ( 'NONE',  ( -18.50000000000000000, 66.75000000001260503, -191.1731074845244223 ) ) ;
#147124 = EDGE_CURVE ( 'NONE', #16250, #172639, #130964, .T. ) ;
#147125 = CARTESIAN_POINT ( 'NONE',  ( -18.54118089899631983, 85.46353763186000663, -95.97452988665611429 ) ) ;
#147126 = DIRECTION ( 'NONE',  ( 0.000000000000000000, 6.982962677686267499E-15, -1.000000000000000000 ) ) ;
#147127 = EDGE_CURVE ( 'NONE', #177471, #55818, #100337, .T. ) ;
#147128 = ADVANCED_FACE ( 'NONE', ( #48851 ), #225230, .F. ) ;
#147129 = ORIENTED_EDGE ( 'NONE', *, *, #183154, .F. ) ;
#147130 = EDGE_CURVE ( 'NONE', #135192, #162626, #112832, .T. ) ;
#147131 = CARTESIAN_POINT ( 'NONE',  ( 21.05000000000000071, 31.98723526783714988, -238.8784020251475511 ) ) ;
#147132 = ORIENTED_EDGE ( 'NONE', *, *, #33415, .F. ) ;
#147133 = DIRECTION ( 'NONE',  ( 0.000000000000000000, 0.000000000000000000, -1.000000000000000000 ) ) ;
#147134 = ADVANCED_FACE ( 'NONE', ( #214354 ), #100775, .T. ) ;
#147135 = LINE ( 'NONE', #165438, #235373 ) ;
#147136 = DIRECTION ( 'NONE',  ( 0.000000000000000000, 1.000000000000000000, 6.938893903907222067E-15 ) ) ;
#147137 = CARTESIAN_POINT ( 'NONE',  ( 20.75572585718182239, 67.11768327161492209, -161.5258490858113873 ) ) ;
#147138 = EDGE_CURVE ( 'NONE', #87594, #63693, #254713, .T. ) ;
#147139 = ORIENTED_EDGE ( 'NONE', *, *, #233995, .T. ) ;
#147140 = DIRECTION ( 'NONE',  ( 0.000000000000000000, 0.000000000000000000, 1.000000000000000000 ) ) ;
#147141 = VECTOR ( 'NONE', #126681, 1000.000000000000000 ) ;
#147142 = LINE ( 'NONE', #110587, #160675 ) ;
#147144 = EDGE_CURVE ( 'NONE', #23243, #83831, #33773, .T. ) ;
#147143 = FILL_AREA_STYLE ('',( #105416 ) ) ;
#147146 = VECTOR ( 'NONE', #190424, 1000.000000000000000 ) ;
#147145 = LINE ( 'NONE', #152318, #138234 ) ;
#147147 = CARTESIAN_POINT ( 'NONE',  ( 23.15000000000000213, 49.36776662947724503, -253.7196102226803021 ) ) ;
#147148 = CARTESIAN_POINT ( 'NONE',  ( 22.43288208788031568, 75.99510014512706846, -181.6727593282434157 ) ) ;
#147149 = ORIENTED_EDGE ( 'NONE', *, *, #95404, .T. ) ;
#147150 = VERTEX_POINT ( 'NONE', #194818 ) ;
#147151 = CARTESIAN_POINT ( 'NONE',  ( 20.85000000000000142, 64.35000000001245724, -170.0231074845244166 ) ) ;
#147152 = CYLINDRICAL_SURFACE ( 'NONE', #167694, 0.1000000000000028644 ) ;
#147153 = CIRCLE ( 'NONE', #138733, 0.1000000000000033223 ) ;
#147154 = DIRECTION ( 'NONE',  ( 1.000000000000000000, 0.000000000000000000, 0.000000000000000000 ) ) ;
#147155 = DIRECTION ( 'NONE',  ( -1.000000000000000000, -0.000000000000000000, 0.000000000000000000 ) ) ;
#147156 = VECTOR ( 'NONE', #209947, 1000.000000000000000 ) ;
#147157 = DIRECTION ( 'NONE',  ( 0.000000000000000000, -0.8660254037844468122, -0.4999999999999859557 ) ) ;
#147158 = EDGE_CURVE ( 'NONE', #22805, #100463, #384, .T. ) ;
#147159 = ORIENTED_EDGE ( 'NONE', *, *, #168509, .T. ) ;
#147160 = DIRECTION ( 'NONE',  ( -0.000000000000000000, -0.000000000000000000, -1.000000000000000000 ) ) ;
#147161 = TOROIDAL_SURFACE ( 'NONE', #251397, 0.2000000000000000111, 0.1000000000000000056 ) ;
#147163 = VECTOR ( 'NONE', #139921, 1000.000000000000000 ) ;
#147162 = CARTESIAN_POINT ( 'NONE',  ( -18.39999999999999858, 13.44928205424795564, -207.5377222505711075 ) ) ;
#147164 = VERTEX_POINT ( 'NONE', #180370 ) ;
#147165 = AXIS2_PLACEMENT_3D ( 'NONE', #31918, #110141, #111432 ) ;
#147166 = DIRECTION ( 'NONE',  ( -0.000000000000000000, 0.9651348961777157509, -0.2617529984165031243 ) ) ;
#147167 = CIRCLE ( 'NONE', #188866, 12.87500000000000178 ) ;
#147168 = AXIS2_PLACEMENT_3D ( 'NONE', #123012, #463, #25204 ) ;
#147169 = PRODUCT ( 'Drag Chain Support Tray Channel', 'Drag Chain Support Tray Channel', '', ( #155213 ) ) ;
#147170 = CIRCLE ( 'NONE', #13905, 0.1000000000000028644 ) ;
#147171 = ORIENTED_EDGE ( 'NONE', *, *, #159548, .T. ) ;
#147172 = ORIENTED_EDGE ( 'NONE', *, *, #191280, .T. ) ;
#147173 = EDGE_LOOP ( 'NONE', ( #67114, #204989, #91751, #3340 ) ) ;
#147174 = CARTESIAN_POINT ( 'NONE',  ( -15.55912972643740488, 67.50912972644943011, -115.6731074845243654 ) ) ;
#147175 = CARTESIAN_POINT ( 'NONE',  ( -20.94999999999999929, 87.48912529308749697, -38.92310748452424463 ) ) ;
#147177 = VECTOR ( 'NONE', #201020, 1000.000000000000000 ) ;
#147176 = DIRECTION ( 'NONE',  ( -0.000000000000000000, 1.265107689135680095E-16, -1.000000000000000000 ) ) ;
#147178 = CARTESIAN_POINT ( 'NONE',  ( 21.05000000000000071, 8.776282895303632259, -176.0586289951409071 ) ) ;
#147179 = DIRECTION ( 'NONE',  ( 0.000000000000000000, 0.000000000000000000, -1.000000000000000000 ) ) ;
#147180 = DIRECTION ( 'NONE',  ( 0.000000000000000000, -0.9673461469267405910, 0.2534589355812664757 ) ) ;
#147181 = CARTESIAN_POINT ( 'NONE',  ( 21.05000000000000071, 23.45160524131172153, -253.2535058871250726 ) ) ;
#147183 = CARTESIAN_POINT ( 'NONE',  ( -23.15000000000000213, 11.65000000001115588, -126.9851942293460922 ) ) ;
#147182 = CARTESIAN_POINT ( 'NONE',  ( 20.95052659398289308, 10.47982436779105875, -108.0752387558656409 ) ) ;
#147184 = AXIS2_PLACEMENT_3D ( 'NONE', #46274, #207957, #226172 ) ;
#147185 = EDGE_CURVE ( 'NONE', #35657, #70952, #176531, .T. ) ;
#147186 = DIRECTION ( 'NONE',  ( 0.000000000000000000, 0.000000000000000000, -1.000000000000000000 ) ) ;
#147187 = CARTESIAN_POINT ( 'NONE',  ( 18.59999999999999076, 10.49142135624846439, -192.3499999999999659 ) ) ;
#147188 = FACE_OUTER_BOUND ( 'NONE', #112339, .T. ) ;
#147189 = PLANE ( 'NONE',  #227977 ) ;
#147190 = EDGE_LOOP ( 'NONE', ( #246477, #99631, #53715, #63183 ) ) ;
#147191 = EDGE_CURVE ( 'NONE', #170111, #170516, #255991, .T. ) ;
#147192 = ORIENTED_EDGE ( 'NONE', *, *, #41182, .T. ) ;
#147193 = CARTESIAN_POINT ( 'NONE',  ( 23.15000000000000213, -12.41227409413852811, -131.0000000000000284 ) ) ;
#147194 = CIRCLE ( 'NONE', #213648, 0.1000000000000024342 ) ;
#147195 = FACE_OUTER_BOUND ( 'NONE', #142783, .T. ) ;
#147197 = CARTESIAN_POINT ( 'NONE',  ( 15.48841904831874849, 8.561580951692381092, -146.6500000000000341 ) ) ;
#147196 = DIRECTION ( 'NONE',  ( -1.000000000000000000, -3.265361837132813093E-16, 0.000000000000000000 ) ) ;
#147198 = VECTOR ( 'NONE', #181525, 1000.000000000000000 ) ;
#147199 = AXIS2_PLACEMENT_3D ( 'NONE', #120696, #140205, #106214 ) ;
#147200 = CIRCLE ( 'NONE', #55572, 0.09999999999999971412 ) ;
#147201 = CARTESIAN_POINT ( 'NONE',  ( -20.54999999999999716, 34.98408343502854478, -248.6539962344157004 ) ) ;
#147202 = DIRECTION ( 'NONE',  ( 0.000000000000000000, 1.000000000000000000, 0.000000000000000000 ) ) ;
#147203 = DIRECTION ( 'NONE',  ( 0.000000000000000000, 7.086529944415894657E-15, -1.000000000000000000 ) ) ;
#147204 = EDGE_LOOP ( 'NONE', ( #214103, #103381, #166962, #166925, #186085, #66901, #93036 ) ) ;
#147205 = ORIENTED_EDGE ( 'NONE', *, *, #207387, .T. ) ;
#147206 = CARTESIAN_POINT ( 'NONE',  ( -15.75000000000000000, 9.349999999999983658, -16.86426760761610311 ) ) ;
#147207 = ORIENTED_EDGE ( 'NONE', *, *, #175125, .F. ) ;
#147208 = ADVANCED_FACE ( 'NONE', ( #76119 ), #96933, .F. ) ;
#147209 = CARTESIAN_POINT ( 'NONE',  ( 23.04999999999999716, 67.17743825834622839, -194.2731074845244166 ) ) ;
#147210 = AXIS2_PLACEMENT_3D ( 'NONE', #16153, #172680, #38264 ) ;
#147211 = VECTOR ( 'NONE', #162345, 1000.000000000000000 ) ;
#147212 = TOROIDAL_SURFACE ( 'NONE', #234704, 3.899999999999999467, 0.1000000000000000056 ) ;
#147213 = AXIS2_PLACEMENT_3D ( 'NONE', #93443, #129994, #173042 ) ;
#147214 = SPHERICAL_SURFACE ( 'NONE', #46497, 0.1000000000000000056 ) ;
#147215 = VERTEX_POINT ( 'NONE', #81236 ) ;
#147216 = DIRECTION ( 'NONE',  ( 0.000000000000000000, 0.2128009952263603677, -0.9770955615653313941 ) ) ;
#147217 = ORIENTED_EDGE ( 'NONE', *, *, #229644, .F. ) ;
#147218 = DIRECTION ( 'NONE',  ( 0.000000000000000000, -0.8446299136406466568, 0.5353506411534347809 ) ) ;
#147219 = FACE_OUTER_BOUND ( 'NONE', #234805, .T. ) ;
#147220 = CARTESIAN_POINT ( 'NONE',  ( -20.94999999999999929, 74.73788286442776041, -233.7359682632885267 ) ) ;
#147221 = FACE_OUTER_BOUND ( 'NONE', #143281, .T. ) ;
#147222 = CYLINDRICAL_SURFACE ( 'NONE', #30830, 2.599999999999998312 ) ;
#147223 = CARTESIAN_POINT ( 'NONE',  ( 20.94999999999999929, 4.813084112160684214, -88.55848224347622022 ) ) ;
#147224 = CARTESIAN_POINT ( 'NONE',  ( 18.60000000000000142, 85.32100840337290037, -62.28716923544637041 ) ) ;
#147225 = DIRECTION ( 'NONE',  ( 4.026293107431335996E-15, 0.8700118002898393765, -0.4930308989875104575 ) ) ;
#147227 = ORIENTED_EDGE ( 'NONE', *, *, #237023, .T. ) ;
#147226 = FACE_OUTER_BOUND ( 'NONE', #124063, .T. ) ;
#147229 = SPHERICAL_SURFACE ( 'NONE', #14454, 0.1000000000000000056 ) ;
#147228 = CARTESIAN_POINT ( 'NONE',  ( 23.14999999999999858, -3.999999999999999112, -33.50000000000000000 ) ) ;
#147230 = ORIENTED_EDGE ( 'NONE', *, *, #34653, .F. ) ;
#147232 = ORIENTED_EDGE ( 'NONE', *, *, #158908, .F. ) ;
#147231 = DIRECTION ( 'NONE',  ( 0.000000000000000000, 0.000000000000000000, 1.000000000000000000 ) ) ;
#147233 = ORIENTED_EDGE ( 'NONE', *, *, #80351, .T. ) ;
#147234 = LINE ( 'NONE', #183799, #78262 ) ;
#147235 = DIRECTION ( 'NONE',  ( 1.000000000000000000, 0.000000000000000000, 0.000000000000000000 ) ) ;
#147236 = VECTOR ( 'NONE', #22495, 999.9999999999998863 ) ;
#147237 = CARTESIAN_POINT ( 'NONE',  ( 23.40000000000005542, 77.26165318615413469, -44.00978271863746016 ) ) ;
#147238 = DIRECTION ( 'NONE',  ( 0.000000000000000000, 1.000000000000000000, 0.000000000000000000 ) ) ;
#147239 = FACE_OUTER_BOUND ( 'NONE', #4474, .T. ) ;
#147240 = CARTESIAN_POINT ( 'NONE',  ( -14.00000000000000178, 66.15000000001228386, -153.2731074845244166 ) ) ;
#147242 = EDGE_CURVE ( 'NONE', #86886, #182252, #200318, .T. ) ;
#147241 = FACE_OUTER_BOUND ( 'NONE', #125845, .T. ) ;
#147243 = DIRECTION ( 'NONE',  ( 1.000000000000000000, -0.000000000000000000, -0.000000000000000000 ) ) ;
#147244 = EDGE_CURVE ( 'NONE', #97897, #235714, #8781, .T. ) ;
#147245 = CARTESIAN_POINT ( 'NONE',  ( 20.12500000000000000, 66.25000000001232081, -161.9113362024101548 ) ) ;
#147246 = ORIENTED_EDGE ( 'NONE', *, *, #22388, .F. ) ;
#147247 = VERTEX_POINT ( 'NONE', #423 ) ;
#147248 = DIRECTION ( 'NONE',  ( -0.000000000000000000, 0.1350103645451807555, 0.9908441862701610203 ) ) ;
#147249 = TOROIDAL_SURFACE ( 'NONE', #55629, 0.6000000000000004219, 0.1000000000000000056 ) ;
#147250 = CIRCLE ( 'NONE', #59930, 0.1000000000000076522 ) ;
#147251 = ORIENTED_EDGE ( 'NONE', *, *, #186447, .F. ) ;
#147252 = CARTESIAN_POINT ( 'NONE',  ( -20.64999999999999858, 68.71679287596359131, -222.9654461259447658 ) ) ;
#147253 = ORIENTED_EDGE ( 'NONE', *, *, #199839, .F. ) ;
#147254 = DIRECTION ( 'NONE',  ( -1.000000000000000000, 2.952720810173289112E-16, 2.061873921506763405E-30 ) ) ;
#147255 = TOROIDAL_SURFACE ( 'NONE', #26464, 1.900000000000002576, 0.1000000000000000056 ) ;
#147256 = EDGE_CURVE ( 'NONE', #138091, #135886, #56530, .T. ) ;
#147257 = CARTESIAN_POINT ( 'NONE',  ( -16.87242674293850797, 9.950000000011138823, -180.1489097536276063 ) ) ;
#147258 = CARTESIAN_POINT ( 'NONE',  ( -22.41119224318417125, -2.479040261793999722, -189.6172560698084624 ) ) ;
#147259 = EDGE_CURVE ( 'NONE', #214748, #233400, #136070, .T. ) ;
#147260 = CARTESIAN_POINT ( 'NONE',  ( -21.05000000000000071, 1.249999999999999334, -8.000000000000000000 ) ) ;
#147261 = EDGE_LOOP ( 'NONE', ( #76472, #48531, #152194, #79397 ) ) ;
#147262 = EDGE_CURVE ( 'NONE', #159934, #157057, #108556, .T. ) ;
#147263 = DIRECTION ( 'NONE',  ( 1.000000000000000000, 0.000000000000000000, 0.000000000000000000 ) ) ;
#147265 = CIRCLE ( 'NONE', #34872, 0.4000000000000114575 ) ;
#147264 = FACE_OUTER_BOUND ( 'NONE', #6299, .T. ) ;
#147266 = EDGE_CURVE ( 'NONE', #190040, #127766, #175236, .T. ) ;
#147267 = CARTESIAN_POINT ( 'NONE',  ( 18.46947024752519795, 85.50929715716780777, -62.53641803582647896 ) ) ;
#147268 = CARTESIAN_POINT ( 'NONE',  ( 21.14999999999999858, 64.35000000001164722, -69.42310748452440805 ) ) ;
#147269 = ORIENTED_EDGE ( 'NONE', *, *, #179889, .T. ) ;
#147271 = CARTESIAN_POINT ( 'NONE',  ( 18.49999999999999645, -1.835859311432484375, -78.50443916879852679 ) ) ;
#147270 = CARTESIAN_POINT ( 'NONE',  ( 21.08884785362045378, 61.08269451800257599, -234.2391594833300701 ) ) ;
#147273 = ORIENTED_EDGE ( 'NONE', *, *, #69682, .F. ) ;
#147272 = AXIS2_PLACEMENT_3D ( 'NONE', #210971, #152307, #70204 ) ;
#147276 = EDGE_LOOP ( 'NONE', ( #38000, #255070, #102737, #38110, #23835, #172039, #206364, #139724, #49644, #92111, #57067, #226481, #203162, #105000 ) ) ;
#147275 = CARTESIAN_POINT ( 'NONE',  ( -16.83199318825829138, 51.51505883799278251, -232.0141791960918738 ) ) ;
#147274 = DIRECTION ( 'NONE',  ( 0.000000000000000000, 0.9126074666063844765, 0.4088369013363114535 ) ) ;
#147277 = ORIENTED_EDGE ( 'NONE', *, *, #236106, .T. ) ;
#147278 = DIRECTION ( 'NONE',  ( 4.239556034732057360E-17, 0.9579639084728132081, 0.2868887416116073785 ) ) ;
#147279 = AXIS2_PLACEMENT_3D ( 'NONE', #165744, #27537, #150032 ) ;
#147280 = AXIS2_PLACEMENT_3D ( 'NONE', #72945, #196697, #114604 ) ;
#147281 = CARTESIAN_POINT ( 'NONE',  ( 20.94999999999999929, -8.663551401858002876, -43.02410111806730697 ) ) ;
#147282 = VERTEX_POINT ( 'NONE', #98213 ) ;
#147283 = CARTESIAN_POINT ( 'NONE',  ( 20.94999999999999574, 87.41227409416235616, -200.5231074845242745 ) ) ;
#147284 = EDGE_CURVE ( 'NONE', #196636, #105532, #159530, .T. ) ;
#147285 = DIRECTION ( 'NONE',  ( -5.603264701231743991E-32, -7.172728831056617961E-15, 1.000000000000000000 ) ) ;
#147287 = CARTESIAN_POINT ( 'NONE',  ( 0.9000000000000547562, 67.72071067812984779, -6.052396806406134644 ) ) ;
#147286 = DIRECTION ( 'NONE',  ( -4.408576920032448588E-17, -0.1350103645451807832, -0.9908441862701610203 ) ) ;
#147289 = VERTEX_POINT ( 'NONE', #138631 ) ;
#147288 = PLANE ( 'NONE',  #97384 ) ;
#147290 = AXIS2_PLACEMENT_3D ( 'NONE', #122068, #240735, #202877 ) ;
#147291 = CIRCLE ( 'NONE', #205717, 0.1999999999999987899 ) ;
#147292 = CIRCLE ( 'NONE', #34905, 0.09999999999999939493 ) ;
#147293 = ORIENTED_EDGE ( 'NONE', *, *, #177250, .F. ) ;
#147294 = CARTESIAN_POINT ( 'NONE',  ( -16.87383368123029825, 9.950000000011138823, -79.65000000000004832 ) ) ;
#147295 = DIRECTION ( 'NONE',  ( -1.000000000000000000, 0.000000000000000000, -0.000000000000000000 ) ) ;
#147296 = CYLINDRICAL_SURFACE ( 'NONE', #109698, 0.09999999999999939493 ) ;
#147297 = ORIENTED_EDGE ( 'NONE', *, *, #61382, .T. ) ;
#147298 = DIRECTION ( 'NONE',  ( 0.000000000000000000, 0.9090645160163607352, 0.4166553800443956734 ) ) ;
#147299 = VECTOR ( 'NONE', #128490, 1000.000000000000000 ) ;
#147300 = LINE ( 'NONE', #127753, #174451 ) ;
#147301 = DIRECTION ( 'NONE',  ( 0.000000000000000000, 0.000000000000000000, 1.000000000000000000 ) ) ;
#147302 = ORIENTED_EDGE ( 'NONE', *, *, #68307, .T. ) ;
#147303 = DIRECTION ( 'NONE',  ( 0.000000000000000000, 0.000000000000000000, 1.000000000000000000 ) ) ;
#147304 = AXIS2_PLACEMENT_3D ( 'NONE', #204888, #30143, #8002 ) ;
#147305 = VECTOR ( 'NONE', #238281, 1000.000000000000000 ) ;
#147306 = VECTOR ( 'NONE', #67639, 1000.000000000000000 ) ;
#147307 = ORIENTED_EDGE ( 'NONE', *, *, #221318, .F. ) ;
#147308 = LINE ( 'NONE', #71645, #80609 ) ;
#147309 = CARTESIAN_POINT ( 'NONE',  ( -22.50000000000000000, 0.1000000000111554016, -33.50000000000000000 ) ) ;
#147310 = EDGE_CURVE ( 'NONE', #30650, #46758, #141861, .T. ) ;
#147311 = ORIENTED_EDGE ( 'NONE', *, *, #18626, .T. ) ;
#147312 = ORIENTED_EDGE ( 'NONE', *, *, #237778, .F. ) ;
#147313 = CARTESIAN_POINT ( 'NONE',  ( -21.05000000000000071, 87.48912529308842068, -166.9231074845242802 ) ) ;
#147314 = ORIENTED_EDGE ( 'NONE', *, *, #126500, .T. ) ;
#147316 = ORIENTED_EDGE ( 'NONE', *, *, #236349, .T. ) ;
#147315 = CARTESIAN_POINT ( 'NONE',  ( -22.60000000000094289, 0.1008583691096561347, -155.7504328765105583 ) ) ;
#147317 = ADVANCED_FACE ( 'NONE', ( #219473 ), #21319, .F. ) ;
#147318 = ORIENTED_EDGE ( 'NONE', *, *, #227647, .T. ) ;
#147320 = ORIENTED_EDGE ( 'NONE', *, *, #167446, .T. ) ;
#147319 = VERTEX_POINT ( 'NONE', #3903 ) ;
#147321 = VECTOR ( 'NONE', #179322, 1000.000000000000000 ) ;
#147322 = EDGE_CURVE ( 'NONE', #36755, #119497, #62774, .T. ) ;
#147323 = EDGE_CURVE ( 'NONE', #90063, #7857, #221645, .T. ) ;
#147324 = AXIS2_PLACEMENT_3D ( 'NONE', #91471, #152758, #213986 ) ;
#147325 = FACE_OUTER_BOUND ( 'NONE', #75544, .T. ) ;
#147326 = ORIENTED_EDGE ( 'NONE', *, *, #162538, .F. ) ;
#147327 = CYLINDRICAL_SURFACE ( 'NONE', #35766, 0.09999999999999939493 ) ;
#147328 = CARTESIAN_POINT ( 'NONE',  ( -21.07928932188134041, 76.00000000001237765, -170.0231074845243597 ) ) ;
#147329 = AXIS2_PLACEMENT_3D ( 'NONE', #57079, #96224, #197892 ) ;
#147330 = FACE_OUTER_BOUND ( 'NONE', #200935, .T. ) ;
#147331 = CARTESIAN_POINT ( 'NONE',  ( -23.15000000000000213, 76.00000000001170974, -69.52310748452431710 ) ) ;
#147332 = ORIENTED_EDGE ( 'NONE', *, *, #73181, .F. ) ;
#147334 = ORIENTED_EDGE ( 'NONE', *, *, #178964, .T. ) ;
#147333 = TOROIDAL_SURFACE ( 'NONE', #209705, 0.2000000000000000111, 0.1000000000000000056 ) ;
#147335 = CYLINDRICAL_SURFACE ( 'NONE', #257995, 0.09999999999999939493 ) ;
#147336 = CIRCLE ( 'NONE', #18352, 0.09999999999998898659 ) ;
#147338 = ORIENTED_EDGE ( 'NONE', *, *, #114043, .T. ) ;
#147337 = DIRECTION ( 'NONE',  ( 1.000000000000000000, 7.304098846218133681E-16, -4.217023435051677501E-16 ) ) ;
#147339 = CARTESIAN_POINT ( 'NONE',  ( 18.49999999999999289, 69.55000000001253113, -182.3731074845244109 ) ) ;
#147341 = ORIENTED_EDGE ( 'NONE', *, *, #190234, .T. ) ;
#147340 = CARTESIAN_POINT ( 'NONE',  ( -23.25000000000000000, -11.64999999998884483, -170.5999999999999659 ) ) ;
#147342 = EDGE_CURVE ( 'NONE', #128410, #212963, #83581, .T. ) ;
#147343 = VERTEX_POINT ( 'NONE', #162997 ) ;
#147344 = FACE_OUTER_BOUND ( 'NONE', #14488, .T. ) ;
#147345 = AXIS2_PLACEMENT_3D ( 'NONE', #51568, #115422, #93293 ) ;
#147346 = EDGE_CURVE ( 'NONE', #193318, #70041, #4488, .T. ) ;
#147347 = AXIS2_PLACEMENT_3D ( 'NONE', #89635, #27148, #244863 ) ;
#147348 = CIRCLE ( 'NONE', #201500, 0.09999999999999939493 ) ;
#147349 = ORIENTED_EDGE ( 'NONE', *, *, #23592, .F. ) ;
#147350 = CIRCLE ( 'NONE', #9788, 0.09999999999999892308 ) ;
#147351 = DIRECTION ( 'NONE',  ( 1.000000000000000000, 0.000000000000000000, 0.000000000000000000 ) ) ;
#147352 = CARTESIAN_POINT ( 'NONE',  ( -21.04999999999999716, -0.01771943329755231583, -161.0589153115292902 ) ) ;
#147353 = CIRCLE ( 'NONE', #64163, 0.1000000000000002554 ) ;
#147355 = ORIENTED_EDGE ( 'NONE', *, *, #162199, .F. ) ;
#147354 = VERTEX_POINT ( 'NONE', #222936 ) ;
#147356 = ORIENTED_EDGE ( 'NONE', *, *, #198815, .F. ) ;
#147357 = LINE ( 'NONE', #69125, #74320 ) ;
#147358 = EDGE_LOOP ( 'NONE', ( #132899, #134011, #29614, #234570 ) ) ;
#147359 = VERTEX_POINT ( 'NONE', #161718 ) ;
#147360 = EDGE_CURVE ( 'NONE', #27579, #86605, #31528, .T. ) ;
#147361 = CARTESIAN_POINT ( 'NONE',  ( -23.15000000000000213, 1.115600667400684642E-11, -100.5000000000000284 ) ) ;
#147363 = VERTEX_POINT ( 'NONE', #101681 ) ;
#147362 = CYLINDRICAL_SURFACE ( 'NONE', #134870, 12.87499999999999822 ) ;
#147364 = ADVANCED_FACE ( 'NONE', ( #80849 ), #189703, .F. ) ;
#147365 = CYLINDRICAL_SURFACE ( 'NONE', #148399, 0.09999999999999939493 ) ;
#147366 = ADVANCED_FACE ( 'NONE', ( #2606 ), #241245, .T. ) ;
#147367 = TOROIDAL_SURFACE ( 'NONE', #205608, 0.4000000000000017431, 0.1000000000000000056 ) ;
#147369 = CARTESIAN_POINT ( 'NONE',  ( 21.13461538461538325, 11.30999384151886211, -211.1763045966511640 ) ) ;
#147368 = CARTESIAN_POINT ( 'NONE',  ( 19.97071067811865674, 11.72071067812981759, -192.2085786437626496 ) ) ;
#147370 = DIRECTION ( 'NONE',  ( -0.000000000000000000, 6.982962677686266711E-15, -1.000000000000000000 ) ) ;
#147371 = DIRECTION ( 'NONE',  ( 0.000000000000000000, 0.000000000000000000, 1.000000000000000000 ) ) ;
#147372 = ORIENTED_EDGE ( 'NONE', *, *, #60124, .T. ) ;
#147373 = ORIENTED_EDGE ( 'NONE', *, *, #54045, .F. ) ;
#147374 = VECTOR ( 'NONE', #208610, 1000.000000000000000 ) ;
#147375 = CARTESIAN_POINT ( 'NONE',  ( -18.59999999999999787, 66.75000000001253397, -182.2731074845244166 ) ) ;
#147376 = DIRECTION ( 'NONE',  ( 1.000000000000000000, 0.000000000000000000, 0.000000000000000000 ) ) ;
#147377 = VERTEX_POINT ( 'NONE', #43039 ) ;
#147378 = B_SPLINE_CURVE_WITH_KNOTS ( 'NONE', 3,
 ( #30413, #229888, #89075, #13414, #12147, #51210, #109921, #70839, #172532, #111219 ),
 .UNSPECIFIED., .F., .F.,
 ( 4, 2, 2, 2, 4 ),
 ( 5.329075035707888194E-16, 9.930191194501786309E-05, 0.0001986038238895028137, 0.0003972076477784323555, 0.0007944152955563318257 ),
 .UNSPECIFIED. ) ;
#147379 = CIRCLE ( 'NONE', #201353, 3.899999999999999467 ) ;
#147380 = AXIS2_PLACEMENT_3D ( 'NONE', #167728, #12501, #247225 ) ;
#147381 = CARTESIAN_POINT ( 'NONE',  ( -18.79999999999999716, 11.61130914238355771, 16.50000000000000000 ) ) ;
#147382 = EDGE_LOOP ( 'NONE', ( #117932, #193687, #137032, #43864, #54586 ) ) ;
#147383 = ORIENTED_EDGE ( 'NONE', *, *, #138194, .T. ) ;
#147384 = CARTESIAN_POINT ( 'NONE',  ( -20.94999999999999929, 64.40000000001263913, -196.5949042542488883 ) ) ;
#147385 = DIRECTION ( 'NONE',  ( 0.000000000000000000, 0.2617529984165152257, 0.9651348961777124202 ) ) ;
#147386 = EDGE_LOOP ( 'NONE', ( #174661, #251163, #222550, #179769 ) ) ;
#147387 = DIRECTION ( 'NONE',  ( 0.000000000000000000, 7.086529944415886769E-15, -1.000000000000000000 ) ) ;
#147388 = CARTESIAN_POINT ( 'NONE',  ( 21.15000000000005542, 74.83745509109094485, -43.92310748452479885 ) ) ;
#147389 = ORIENTED_EDGE ( 'NONE', *, *, #19240, .F. ) ;
#147390 = DIRECTION ( 'NONE',  ( 1.000000000000000000, 0.000000000000000000, 0.000000000000000000 ) ) ;
#147391 = CARTESIAN_POINT ( 'NONE',  ( -22.50000000000000000, 76.00000000001271871, -209.7731074845243597 ) ) ;
#147393 = CARTESIAN_POINT ( 'NONE',  ( -21.05000000000000071, 1.115653327213047955E-11, -129.7000000000000455 ) ) ;
#147392 = CARTESIAN_POINT ( 'NONE',  ( -21.64999999999999858, 10.04999999999998295, -12.65000000000000213 ) ) ;
#147394 = CARTESIAN_POINT ( 'NONE',  ( -21.05000000000000071, -1.261786168553869603, -175.5864989635454378 ) ) ;
#147395 = DIRECTION ( 'NONE',  ( 0.000000000000000000, 0.000000000000000000, 1.000000000000000000 ) ) ;
#147396 = SPHERICAL_SURFACE ( 'NONE', #240547, 0.1000000000000000056 ) ;
#147397 = EDGE_CURVE ( 'NONE', #150102, #169429, #173274, .T. ) ;
#147398 = DIRECTION ( 'NONE',  ( -1.000000000000000000, 0.000000000000000000, 0.000000000000000000 ) ) ;
#147400 = ORIENTED_EDGE ( 'NONE', *, *, #45882, .T. ) ;
#147399 = AXIS2_PLACEMENT_3D ( 'NONE', #73532, #35691, #74824 ) ;
#147401 = AXIS2_PLACEMENT_3D ( 'NONE', #206899, #28297, #249876 ) ;
#147402 = CIRCLE ( 'NONE', #35013, 0.09999999999999939493 ) ;
#147404 = VERTEX_POINT ( 'NONE', #224222 ) ;
#147403 = ORIENTED_EDGE ( 'NONE', *, *, #59065, .F. ) ;
#147405 = ORIENTED_EDGE ( 'NONE', *, *, #175002, .T. ) ;
#147406 = EDGE_CURVE ( 'NONE', #51771, #70810, #69100, .T. ) ;
#147407 = DIRECTION ( 'NONE',  ( 1.000000000000000000, 0.000000000000000000, 0.000000000000000000 ) ) ;
#147408 = CARTESIAN_POINT ( 'NONE',  ( -16.86337532320260735, 66.02003279578745776, -82.07418301554156415 ) ) ;
#147409 = B_SPLINE_CURVE_WITH_KNOTS ( 'NONE', 3,
 ( #152730, #212680, #227082, #52285, #113567, #193119, #79554, #237372, #194415, #178713, #99111, #39195, #233533, #198229, #95285, #117423, #114849, #234803, #17055 ),
 .UNSPECIFIED., .F., .F.,
 ( 4, 3, 3, 3, 3, 3, 4 ),
 ( 0.000000000000000000, 7.110282409889887435E-05, 0.0001508797727291436692, 0.0002027344179858470120, 0.0002343294522349037394, 0.0002454816334821225830, 0.0002619873080085598845 ),
 .UNSPECIFIED. ) ;
#147411 = DIRECTION ( 'NONE',  ( 1.000000000000000000, 0.000000000000000000, 0.000000000000000000 ) ) ;
#147410 = CARTESIAN_POINT ( 'NONE',  ( 13.99999999999999822, 9.850000000011137402, -184.2499999999999716 ) ) ;
#147412 = CARTESIAN_POINT ( 'NONE',  ( -21.08621493067320429, 75.94380516053614372, -142.8724017756962326 ) ) ;
#147413 = EDGE_LOOP ( 'NONE', ( #245456, #114581, #129228, #243567, #224758, #58036, #186332, #34647, #105964, #64502, #193097, #126183, #225645, #52611 ) ) ;
#147414 = EDGE_CURVE ( 'NONE', #120740, #181396, #6461, .T. ) ;
#147415 = DIRECTION ( 'NONE',  ( 1.000000000000000000, 0.000000000000000000, 0.000000000000000000 ) ) ;
#147416 = CARTESIAN_POINT ( 'NONE',  ( -21.07928932188134397, 0.09889514565439470883, 6.328516656393301076 ) ) ;
#147417 = CARTESIAN_POINT ( 'NONE',  ( -20.54999999999999716, 11.36448785225375602, -246.7787679937655980 ) ) ;
#147418 = EDGE_CURVE ( 'NONE', #252143, #250175, #23129, .T. ) ;
#147419 = CARTESIAN_POINT ( 'NONE',  ( -21.07928932188134397, 1.596973512272237716, -230.6572452218043736 ) ) ;
#147420 = VERTEX_POINT ( 'NONE', #61309 ) ;
#147421 = CYLINDRICAL_SURFACE ( 'NONE', #209697, 0.1000000000000038219 ) ;
#147422 = EDGE_CURVE ( 'NONE', #67836, #75919, #118991, .T. ) ;
#147424 = B_SPLINE_CURVE_WITH_KNOTS ( 'NONE', 3,
 ( #179394, #121971, #256268, #77685, #704, #80231, #159828, #3281, #82799, #239352 ),
 .UNSPECIFIED., .F., .F.,
 ( 4, 3, 3, 4 ),
 ( 7.632826238681696029E-06, 4.756916949875625587E-05, 9.484459048150268483E-05, 0.0001435500935099809469 ),
 .UNSPECIFIED. ) ;
#147423 = VECTOR ( 'NONE', #66426, 1000.000000000000000 ) ;
#147425 = DIRECTION ( 'NONE',  ( 1.000000000000000000, 0.000000000000000000, 0.000000000000000000 ) ) ;
#147426 = ADVANCED_FACE ( 'NONE', ( #148557 ), #194004, .T. ) ;
#147427 = VERTEX_POINT ( 'NONE', #168158 ) ;
#147428 = EDGE_LOOP ( 'NONE', ( #166718, #28069, #137108, #245348 ) ) ;
#147429 = DIRECTION ( 'NONE',  ( 1.000000000000000000, 0.000000000000000000, 0.000000000000000000 ) ) ;
#147430 = FACE_OUTER_BOUND ( 'NONE', #210238, .T. ) ;
#147431 = CARTESIAN_POINT ( 'NONE',  ( 20.95083306685154056, 67.08315735812139735, -61.04578263126603588 ) ) ;
#147432 = CARTESIAN_POINT ( 'NONE',  ( 23.14999999999999858, 1.115600667400684642E-11, -200.9999999999999432 ) ) ;
#147433 = DIRECTION ( 'NONE',  ( -1.073024830501117725E-15, 0.000000000000000000, 1.000000000000000000 ) ) ;
#147434 = ORIENTED_EDGE ( 'NONE', *, *, #153056, .F. ) ;
#147435 = SPHERICAL_SURFACE ( 'NONE', #67317, 0.1000000000000000056 ) ;
#147436 = CARTESIAN_POINT ( 'NONE',  ( 21.04999999999902371, 11.91025941954771739, -206.1395922244702490 ) ) ;
#147438 = DIRECTION ( 'NONE',  ( 0.000000000000000000, -1.000000000000000000, 0.000000000000000000 ) ) ;
#147437 = LINE ( 'NONE', #225656, #112053 ) ;
#147439 = DIRECTION ( 'NONE',  ( 0.000000000000000000, 0.9126074666063772600, 0.4088369013363274407 ) ) ;
#147440 = CARTESIAN_POINT ( 'NONE',  ( -18.49499033040907037, -9.438148771744673482, -7.198153225923435095 ) ) ;
#147441 = DIRECTION ( 'NONE',  ( 0.000000000000000000, 0.9126074666063660468, 0.4088369013363524762 ) ) ;
#147442 = DIRECTION ( 'NONE',  ( 1.000000000000000000, 0.000000000000000000, 0.000000000000000000 ) ) ;
#147443 = VECTOR ( 'NONE', #171075, 1000.000000000000000 ) ;
#147445 = ORIENTED_EDGE ( 'NONE', *, *, #194948, .F. ) ;
#147444 = FACE_OUTER_BOUND ( 'NONE', #180919, .T. ) ;
#147446 = EDGE_CURVE ( 'NONE', #80509, #131693, #77269, .T. ) ;
#147447 = EDGE_CURVE ( 'NONE', #20946, #44944, #148266, .T. ) ;
#147448 = AXIS2_PLACEMENT_3D ( 'NONE', #106991, #70489, #247799 ) ;
#147449 = ADVANCED_FACE ( 'NONE', ( #209812 ), #210552, .T. ) ;
#147450 = EDGE_CURVE ( 'NONE', #188235, #41396, #27432, .T. ) ;
#147452 = CARTESIAN_POINT ( 'NONE',  ( -18.59999999999999787, 76.00000000001267608, -203.5231074845243597 ) ) ;
#147451 = AXIS2_PLACEMENT_3D ( 'NONE', #36645, #217789, #15797 ) ;
#147453 = EDGE_CURVE ( 'NONE', #141252, #162376, #71600, .T. ) ;
#147454 = SPHERICAL_SURFACE ( 'NONE', #21219, 0.1000000000000000056 ) ;
#147455 = ORIENTED_EDGE ( 'NONE', *, *, #144182, .F. ) ;
#147456 = DIRECTION ( 'NONE',  ( -0.000000000000000000, -1.000000000000000000, -0.000000000000000000 ) ) ;
#147457 = TOROIDAL_SURFACE ( 'NONE', #151587, 0.2000000000000000111, 0.1000000000000000056 ) ;
#147458 = CARTESIAN_POINT ( 'NONE',  ( 23.25000000000000000, 29.86062094194855376, -263.1160279713685100 ) ) ;
#147459 = CARTESIAN_POINT ( 'NONE',  ( -21.05000000000000071, 4.459011116736869340, -245.2267018908137857 ) ) ;
#147460 = TOROIDAL_SURFACE ( 'NONE', #35080, 0.2000000000000000111, 0.1000000000000000056 ) ;
#147461 = EDGE_CURVE ( 'NONE', #168923, #123853, #181537, .T. ) ;
#147462 = CIRCLE ( 'NONE', #30970, 0.5999999999999894307 ) ;
#147463 = EDGE_LOOP ( 'NONE', ( #78063, #119939, #255956, #187575 ) ) ;
#147464 = CARTESIAN_POINT ( 'NONE',  ( -16.86337532320262156, 12.42226302398836069, -211.1398532408442748 ) ) ;
#147466 = ORIENTED_EDGE ( 'NONE', *, *, #52031, .F. ) ;
#147465 = DIRECTION ( 'NONE',  ( 0.000000000000000000, 1.000000000000000000, 2.891205793294679805E-16 ) ) ;
#147467 = CARTESIAN_POINT ( 'NONE',  ( -20.54999999999999716, 85.40000000001198543, -112.9170766071766820 ) ) ;
#147468 = VERTEX_POINT ( 'NONE', #251488 ) ;
#147469 = CARTESIAN_POINT ( 'NONE',  ( 22.39999999999999858, 59.68594599439719417, -233.9123800762197902 ) ) ;
#147470 = EDGE_CURVE ( 'NONE', #240969, #53603, #252229, .T. ) ;
#147471 = TOROIDAL_SURFACE ( 'NONE', #243140, 11.65000000000000036, 0.1000000000000000056 ) ;
#147472 = DIRECTION ( 'NONE',  ( 0.000000000000000000, 0.000000000000000000, 1.000000000000000000 ) ) ;
#147474 = FACE_OUTER_BOUND ( 'NONE', #244146, .T. ) ;
#147473 = AXIS2_PLACEMENT_3D ( 'NONE', #123179, #86584, #48765 ) ;
#147475 = B_SPLINE_CURVE_WITH_KNOTS ( 'NONE', 3,
 ( #160969, #64428, #121840, #183099, #163522, #61859 ),
 .UNSPECIFIED., .F., .F.,
 ( 4, 2, 4 ),
 ( 0.000000000000000000, 0.0001895189928937344179, 0.0003790379857874688358 ),
 .UNSPECIFIED. ) ;
#147477 = AXIS2_PLACEMENT_3D ( 'NONE', #91434, #167150, #211382 ) ;
#147476 = CARTESIAN_POINT ( 'NONE',  ( -22.16821283564876666, 68.44102665923190898, -203.5231074845243882 ) ) ;
#147478 = DIRECTION ( 'NONE',  ( 0.000000000000000000, 0.000000000000000000, 1.000000000000000000 ) ) ;
#147479 = ORIENTED_EDGE ( 'NONE', *, *, #111459, .F. ) ;
#147480 = CARTESIAN_POINT ( 'NONE',  ( 21.14999999999999858, 8.786607556611267356, -112.7500000000000284 ) ) ;
#147481 = DIRECTION ( 'NONE',  ( -0.000000000000000000, 6.982962677686266711E-15, -1.000000000000000000 ) ) ;
#147482 = AXIS2_PLACEMENT_3D ( 'NONE', #19972, #194765, #94338 ) ;
#147483 = CARTESIAN_POINT ( 'NONE',  ( -20.94999999999999929, -11.29603075032412995, -170.5478991596638423 ) ) ;
#147484 = VECTOR ( 'NONE', #60052, 1000.000000000000114 ) ;
#147485 = LINE ( 'NONE', #190491, #49361 ) ;
#147486 = ORIENTED_EDGE ( 'NONE', *, *, #143500, .F. ) ;
#147487 = ORIENTED_EDGE ( 'NONE', *, *, #78851, .F. ) ;
#147488 = CIRCLE ( 'NONE', #251533, 11.75000000000000000 ) ;
#147489 = CARTESIAN_POINT ( 'NONE',  ( 21.09793522318408066, 65.27537548979928772, -124.2838166135473017 ) ) ;
#147490 = CIRCLE ( 'NONE', #5813, 0.09999999999999939493 ) ;
#147491 = AXIS2_PLACEMENT_3D ( 'NONE', #238257, #59595, #154911 ) ;
#147492 = CARTESIAN_POINT ( 'NONE',  ( 20.94999999999999929, 71.00000000001223555, -148.9283735034374843 ) ) ;
#147493 = FACE_OUTER_BOUND ( 'NONE', #185965, .T. ) ;
#147494 = DIRECTION ( 'NONE',  ( 1.000000000000000000, 1.186688945009009831E-16, 0.000000000000000000 ) ) ;
#147495 = CARTESIAN_POINT ( 'NONE',  ( 21.12400222705959507, 8.778511907088271116, -146.2500000000000568 ) ) ;
#147497 = CARTESIAN_POINT ( 'NONE',  ( -20.85000000000000142, 45.93315328338058379, -256.6017782078560003 ) ) ;
#147496 = DIRECTION ( 'NONE',  ( -0.000000000000000000, 1.000000000000000000, 6.982962677686266711E-15 ) ) ;
#147498 = DIRECTION ( 'NONE',  ( 1.000000000000000000, 0.000000000000000000, 0.000000000000000000 ) ) ;
#147499 = DIRECTION ( 'NONE',  ( 1.000000000000000000, 0.000000000000000000, 0.000000000000000000 ) ) ;
#147500 = CARTESIAN_POINT ( 'NONE',  ( -18.45037301276714459, 46.93868734354772698, -255.3449505252505389 ) ) ;
#147501 = CARTESIAN_POINT ( 'NONE',  ( 23.24999999999999645, 78.02678328198446422, -204.0727887811995629 ) ) ;
#147503 = ORIENTED_EDGE ( 'NONE', *, *, #63254, .F. ) ;
#147502 = FACE_OUTER_BOUND ( 'NONE', #186976, .T. ) ;
#147504 = SPHERICAL_SURFACE ( 'NONE', #139329, 0.1000000000000000056 ) ;
#147505 = CARTESIAN_POINT ( 'NONE',  ( -21.08198257630413508, -1.277454622087745850, -194.7930808841681198 ) ) ;
#147507 = DIRECTION ( 'NONE',  ( 0.000000000000000000, 0.000000000000000000, 1.000000000000000000 ) ) ;
#147506 = CARTESIAN_POINT ( 'NONE',  ( -23.15000000000000213, 64.35000000001222986, -148.6731074845244507 ) ) ;
#147508 = EDGE_CURVE ( 'NONE', #178023, #226447, #98093, .T. ) ;
#147509 = ORIENTED_EDGE ( 'NONE', *, *, #227022, .F. ) ;
#147510 = FACE_OUTER_BOUND ( 'NONE', #221348, .T. ) ;
#147511 = CARTESIAN_POINT ( 'NONE',  ( -22.50000000000000000, 65.59531831295525706, -241.8872196075891168 ) ) ;
#147512 = DIRECTION ( 'NONE',  ( 0.000000000000000000, -7.116814260417668513E-15, 1.000000000000000000 ) ) ;
#147513 = CARTESIAN_POINT ( 'NONE',  ( 16.27683809663749770, 11.10425270649115959, -208.0484446391143649 ) ) ;
#147514 = DIRECTION ( 'NONE',  ( -0.000000000000000000, 1.000000000000000000, -0.000000000000000000 ) ) ;
#147515 = VERTEX_POINT ( 'NONE', #231959 ) ;
#147516 = EDGE_LOOP ( 'NONE', ( #145602, #93524, #154788, #172100 ) ) ;
#147517 = AXIS2_PLACEMENT_3D ( 'NONE', #236258, #34242, #212854 ) ;
#147518 = AXIS2_PLACEMENT_3D ( 'NONE', #221008, #131875, #113596 ) ;
#147519 = CARTESIAN_POINT ( 'NONE',  ( -16.81744102076748959, 9.950000000011138823, -54.35000000000000142 ) ) ;
#147520 = ORIENTED_EDGE ( 'NONE', *, *, #188941, .F. ) ;
#147521 = EDGE_CURVE ( 'NONE', #151038, #154603, #239784, .T. ) ;
#147522 = CARTESIAN_POINT ( 'NONE',  ( 23.14999999999999503, 64.35000000001176090, -76.53791325517833855 ) ) ;
#147523 = AXIS2_PLACEMENT_3D ( 'NONE', #137910, #38843, #14160 ) ;
#147524 = ORIENTED_EDGE ( 'NONE', *, *, #237264, .F. ) ;
#147525 = DIRECTION ( 'NONE',  ( 0.7071067811865475727, -0.6824534298470373850, 0.1850873201762210096 ) ) ;
#147526 = CARTESIAN_POINT ( 'NONE',  ( -17.71734398241074615, 65.15764277154752904, -126.2482457375299560 ) ) ;
#147527 = AXIS2_PLACEMENT_3D ( 'NONE', #100415, #35375, #60011 ) ;
#147528 = AXIS2_PLACEMENT_3D ( 'NONE', #222420, #90630, #9823 ) ;
#147529 = CARTESIAN_POINT ( 'NONE',  ( 21.05000000000000071, 7.128833340093095217, -233.7327013124392749 ) ) ;
#147530 = EDGE_LOOP ( 'NONE', ( #177446, #13865, #18726, #28977, #154772 ) ) ;
#147531 = CIRCLE ( 'NONE', #1761, 4.049999999999998046 ) ;
#147532 = CARTESIAN_POINT ( 'NONE',  ( 18.54999999999999716, 52.10946721379481517, -233.0415979755771900 ) ) ;
#147534 = CIRCLE ( 'NONE', #197585, 0.09999999999998898659 ) ;
#147533 = CARTESIAN_POINT ( 'NONE',  ( -18.58222699835055280, 68.11153784908182729, -224.1393723182492579 ) ) ;
#147535 = DIRECTION ( 'NONE',  ( 0.000000000000000000, -6.982962677686266711E-15, 1.000000000000000000 ) ) ;
#147537 = VECTOR ( 'NONE', #89455, 1000.000000000000000 ) ;
#147536 = DIRECTION ( 'NONE',  ( -1.040834085586103947E-13, 0.9770955615653551529, 0.2128009952262517601 ) ) ;
#147538 = DIRECTION ( 'NONE',  ( 0.000000000000000000, 0.000000000000000000, 1.000000000000000000 ) ) ;
#147539 = AXIS2_PLACEMENT_3D ( 'NONE', #214737, #174386, #235577 ) ;
#147540 = LINE ( 'NONE', #105816, #57301 ) ;
#147541 = VERTEX_POINT ( 'NONE', #152430 ) ;
#147543 = CARTESIAN_POINT ( 'NONE',  ( -22.42253884134832020, 75.99806764887745203, -215.1727131818727798 ) ) ;
#147542 = CARTESIAN_POINT ( 'NONE',  ( -18.59999999999999787, 77.73625713160970463, -158.4544551555068495 ) ) ;
#147544 = ORIENTED_EDGE ( 'NONE', *, *, #212414, .F. ) ;
#147546 = ORIENTED_EDGE ( 'NONE', *, *, #252873, .T. ) ;
#147545 = DIRECTION ( 'NONE',  ( 8.673617379884087537E-15, -0.000000000000000000, 1.000000000000000000 ) ) ;
#147547 = AXIS2_PLACEMENT_3D ( 'NONE', #256285, #38598, #42441 ) ;
#147548 = ORIENTED_EDGE ( 'NONE', *, *, #176470, .T. ) ;
#147549 = FACE_OUTER_BOUND ( 'NONE', #87990, .T. ) ;
#147550 = DIRECTION ( 'NONE',  ( -0.000000000000000000, 1.000000000000000000, 0.000000000000000000 ) ) ;
#147551 = CARTESIAN_POINT ( 'NONE',  ( -20.64999999999999858, 74.00000000001151079, -49.24772940728643533 ) ) ;
#147552 = ORIENTED_EDGE ( 'NONE', *, *, #154764, .T. ) ;
#147553 = CARTESIAN_POINT ( 'NONE',  ( -21.05000000000000071, 76.00000000001142553, -36.02310748452432421 ) ) ;
#147555 = DIRECTION ( 'NONE',  ( 1.000000000000000000, 0.000000000000000000, 0.000000000000000000 ) ) ;
#147554 = AXIS2_PLACEMENT_3D ( 'NONE', #38433, #98357, #119270 ) ;
#147556 = B_SPLINE_CURVE_WITH_KNOTS ( 'NONE', 3,
 ( #131786, #251737, #30144, #90078, #150095, #109644, #189204, #170970, #229613, #211332 ),
 .UNSPECIFIED., .F., .F.,
 ( 4, 3, 3, 4 ),
 ( 1.953413405799106337E-15, 8.145022132829330989E-06, 1.905645951092428095E-05, 2.061107371225752284E-05 ),
 .UNSPECIFIED. ) ;
#147557 = ORIENTED_EDGE ( 'NONE', *, *, #240003, .T. ) ;
#147558 = CARTESIAN_POINT ( 'NONE',  ( 20.94999999999999929, -11.64999999998883595, -164.5000000000000000 ) ) ;
#147559 = AXIS2_PLACEMENT_3D ( 'NONE', #2050, #164996, #180720 ) ;
#147560 = ADVANCED_FACE ( 'NONE', ( #53301 ), #186407, .F. ) ;
#147561 = LINE ( 'NONE', #14497, #139080 ) ;
#147562 = ORIENTED_EDGE ( 'NONE', *, *, #57969, .T. ) ;
#147563 = CARTESIAN_POINT ( 'NONE',  ( -20.94999999999999929, 87.75000000001173817, -72.62310748452422615 ) ) ;
#147564 = CIRCLE ( 'NONE', #239142, 0.09999999999999967248 ) ;
#147565 = AXIS2_PLACEMENT_3D ( 'NONE', #229736, #250573, #27725 ) ;
#147566 = ORIENTED_EDGE ( 'NONE', *, *, #135504, .F. ) ;
#147567 = CIRCLE ( 'NONE', #185161, 0.09999999999999939493 ) ;
#147568 = DIRECTION ( 'NONE',  ( -1.000000000000000000, -0.000000000000000000, 0.000000000000000000 ) ) ;
#147569 = ORIENTED_EDGE ( 'NONE', *, *, #187437, .T. ) ;
#147570 = DIRECTION ( 'NONE',  ( 1.000000000000000000, 0.000000000000000000, 0.000000000000000000 ) ) ;
#147571 = ADVANCED_FACE ( 'NONE', ( #187696 ), #7763, .T. ) ;
#147572 = CARTESIAN_POINT ( 'NONE',  ( -20.94999999999999929, 68.51069317435826633, -224.1259271199053842 ) ) ;
#147573 = CARTESIAN_POINT ( 'NONE',  ( 21.10000000000000142, 6.322468214605804882, 12.11686199900910310 ) ) ;
#147574 = EDGE_CURVE ( 'NONE', #15812, #144708, #139806, .T. ) ;
#147575 = FACE_OUTER_BOUND ( 'NONE', #16464, .T. ) ;
#147576 = EDGE_CURVE ( 'NONE', #211620, #149376, #256261, .T. ) ;
#147577 = DIRECTION ( 'NONE',  ( 0.000000000000000000, 6.982962677686266711E-15, -1.000000000000000000 ) ) ;
#147578 = CARTESIAN_POINT ( 'NONE',  ( 21.05000000000000071, 11.41170713998153019, -246.6906184681487275 ) ) ;
#147579 = VERTEX_POINT ( 'NONE', #70330 ) ;
#147580 = AXIS2_PLACEMENT_3D ( 'NONE', #172434, #56274, #15914 ) ;
#147581 = CARTESIAN_POINT ( 'NONE',  ( 21.05000000000000071, -1.249999999988843369, -175.3999999999999773 ) ) ;
#147582 = ORIENTED_EDGE ( 'NONE', *, *, #169483, .F. ) ;
#147584 = CARTESIAN_POINT ( 'NONE',  ( -21.05000000000000071, 67.23127455305835554, -235.8551265064784559 ) ) ;
#147583 = DIRECTION ( 'NONE',  ( 0.000000000000000000, -0.9654421110809058293, -0.2606175937108693996 ) ) ;
#147585 = ORIENTED_EDGE ( 'NONE', *, *, #162865, .F. ) ;
#147586 = LINE ( 'NONE', #240587, #97148 ) ;
#147587 = CARTESIAN_POINT ( 'NONE',  ( 20.84999999999999432, 70.22659352830977753, -197.9852579278363578 ) ) ;
#147588 = DIRECTION ( 'NONE',  ( -1.000000000000000000, 0.000000000000000000, 0.000000000000000000 ) ) ;
#147589 = AXIS2_PLACEMENT_3D ( 'NONE', #115729, #94869, #93596 ) ;
#147591 = ORIENTED_EDGE ( 'NONE', *, *, #13256, .T. ) ;
#147590 =( BOUNDED_CURVE ( )  B_SPLINE_CURVE ( 3, ( #244247, #143866, #186881, #121772 ),
 .UNSPECIFIED., .F., .F. ) 
 B_SPLINE_CURVE_WITH_KNOTS ( ( 4, 4 ),
 ( 0.3000847527772381729, 0.5497968875596822569 ),
 .UNSPECIFIED. ) 
 CURVE ( )  GEOMETRIC_REPRESENTATION_ITEM ( )  RATIONAL_B_SPLINE_CURVE ( ( 1.000000000000000000, 0.9948104011409419911, 0.9948104011409419911, 1.000000000000000000 ) ) 
 REPRESENTATION_ITEM ( '' )  );
#147593 = ORIENTED_EDGE ( 'NONE', *, *, #129542, .F. ) ;
#147592 = DIRECTION ( 'NONE',  ( 0.000000000000000000, -0.9910465087640866200, 0.1335171055202867274 ) ) ;
#147594 = ADVANCED_FACE ( 'NONE', ( #149852 ), #152322, .F. ) ;
#147595 = DIRECTION ( 'NONE',  ( 0.000000000000000000, 0.9889818879709272315, 0.1480365673253073999 ) ) ;
#147596 = DIRECTION ( 'NONE',  ( -1.000000000000000000, 0.000000000000000000, 0.000000000000000000 ) ) ;
#147598 = EDGE_LOOP ( 'NONE', ( #27788, #95080, #215708, #88628 ) ) ;
#147597 = CARTESIAN_POINT ( 'NONE',  ( -18.59999999999999787, 7.021664781911246322, -204.8335654018972605 ) ) ;
#147599 = ORIENTED_EDGE ( 'NONE', *, *, #180026, .T. ) ;
#147600 = FACE_OUTER_BOUND ( 'NONE', #247557, .T. ) ;
#147601 = AXIS2_PLACEMENT_3D ( 'NONE', #189605, #10961, #13532 ) ;
#147602 = CARTESIAN_POINT ( 'NONE',  ( 21.14999999999999503, 87.65000000001235492, -167.1231074845242688 ) ) ;
#147603 = ORIENTED_EDGE ( 'NONE', *, *, #113492, .T. ) ;
#147604 = DIRECTION ( 'NONE',  ( 7.304098846218132695E-16, 0.4721928772777346794, 0.8814952561688431665 ) ) ;
#147605 = ORIENTED_EDGE ( 'NONE', *, *, #208626, .T. ) ;
#147606 = CARTESIAN_POINT ( 'NONE',  ( -18.50000000000000355, 85.41908450282468834, -29.19319967749884626 ) ) ;
#147607 = EDGE_LOOP ( 'NONE', ( #15203, #33680, #179960, #56887 ) ) ;
#147608 = CARTESIAN_POINT ( 'NONE',  ( 23.14999999999999858, 1.115600667400684642E-11, -134.0000000000000284 ) ) ;
#147609 = ADVANCED_FACE ( 'NONE', ( #229382 ), #98800, .F. ) ;
#147610 = DIRECTION ( 'NONE',  ( 1.000000000000000000, -0.000000000000000000, -0.000000000000000000 ) ) ;
#147611 = ORIENTED_EDGE ( 'NONE', *, *, #251225, .T. ) ;
#147612 = AXIS2_PLACEMENT_3D ( 'NONE', #84393, #2327, #1027 ) ;
#147613 = DIRECTION ( 'NONE',  ( 1.000000000000000000, 0.000000000000000000, 0.000000000000000000 ) ) ;
#147614 = CIRCLE ( 'NONE', #35238, 0.09999999999999939493 ) ;
#147615 = AXIS2_PLACEMENT_3D ( 'NONE', #131391, #132693, #32331 ) ;
#147616 = CIRCLE ( 'NONE', #197492, 0.09999999999999761857 ) ;
#147617 = EDGE_CURVE ( 'NONE', #134077, #189474, #18998, .T. ) ;
#147618 = ORIENTED_EDGE ( 'NONE', *, *, #45698, .F. ) ;
#147619 = ORIENTED_EDGE ( 'NONE', *, *, #194647, .F. ) ;
#147620 = CARTESIAN_POINT ( 'NONE',  ( -18.31331870001056572, -9.536294719169660539, -73.86857869098540164 ) ) ;
#147621 = ORIENTED_EDGE ( 'NONE', *, *, #157000, .F. ) ;
#147622 =( GEOMETRIC_REPRESENTATION_CONTEXT ( 3 ) GLOBAL_UNCERTAINTY_ASSIGNED_CONTEXT ( ( #112922 ) ) GLOBAL_UNIT_ASSIGNED_CONTEXT ( ( #184562, #146700, #69783 ) ) REPRESENTATION_CONTEXT ( 'NONE', 'WORKASPACE' ) );
#147623 = CARTESIAN_POINT ( 'NONE',  ( -16.79139129368507000, 22.99352567686698023, -230.9490794793520649 ) ) ;
#147624 = ORIENTED_EDGE ( 'NONE', *, *, #104717, .T. ) ;
#147626 = ORIENTED_EDGE ( 'NONE', *, *, #64188, .F. ) ;
#147625 = PLANE ( 'NONE',  #205062 ) ;
#147627 = ADVANCED_FACE ( 'NONE', ( #178407 ), #135522, .T. ) ;
#147628 = CARTESIAN_POINT ( 'NONE',  ( 20.94999999999999574, 0.6656436123793491033, -212.6810495496487476 ) ) ;
#147629 = ORIENTED_EDGE ( 'NONE', *, *, #209788, .F. ) ;
#147630 = CYLINDRICAL_SURFACE ( 'NONE', #205620, 0.09999999999999939493 ) ;
#147631 = ORIENTED_EDGE ( 'NONE', *, *, #175706, .T. ) ;
#147634 = ORIENTED_EDGE ( 'NONE', *, *, #102294, .T. ) ;
#147633 = ORIENTED_EDGE ( 'NONE', *, *, #6655, .T. ) ;
#147632 = CARTESIAN_POINT ( 'NONE',  ( -20.12071067811865888, 66.67928932189340685, -124.1731074845243654 ) ) ;
#147636 = DIRECTION ( 'NONE',  ( 1.000000000000000000, 0.000000000000000000, 0.000000000000000000 ) ) ;
#147635 = CIRCLE ( 'NONE', #67957, 0.09999999999998898659 ) ;
#147637 = EDGE_CURVE ( 'NONE', #33354, #82065, #113271, .T. ) ;
#147638 = CARTESIAN_POINT ( 'NONE',  ( -23.15000000000000213, 64.25000000001247713, -173.1231074845244393 ) ) ;
#147639 = VERTEX_POINT ( 'NONE', #237069 ) ;
#147640 = AXIS2_PLACEMENT_3D ( 'NONE', #231749, #36118, #174378 ) ;
#147641 = AXIS2_PLACEMENT_3D ( 'NONE', #93380, #193778, #94666 ) ;
#147642 = AXIS2_PLACEMENT_3D ( 'NONE', #59414, #99828, #41204 ) ;
#147643 = AXIS2_PLACEMENT_3D ( 'NONE', #59937, #39140, #1251 ) ;
#147644 = EDGE_LOOP ( 'NONE', ( #72004, #74483, #227453, #12343 ) ) ;
#147645 = DIRECTION ( 'NONE',  ( 1.000000000000000000, 0.000000000000000000, -0.000000000000000000 ) ) ;
#147646 = CARTESIAN_POINT ( 'NONE',  ( -18.50000000000000000, -1.637172712959223952, -45.08215336547201701 ) ) ;
#147647 = EDGE_CURVE ( 'NONE', #69452, #139720, #173300, .T. ) ;
#147649 = ORIENTED_EDGE ( 'NONE', *, *, #230377, .T. ) ;
#147648 = DIRECTION ( 'NONE',  ( 3.616040088954490704E-32, 7.105427357601001859E-15, -1.000000000000000000 ) ) ;
#147650 = CARTESIAN_POINT ( 'NONE',  ( 20.94999999999999929, -11.29603075032412640, -164.4521008403361577 ) ) ;
#147651 = VERTEX_POINT ( 'NONE', #153739 ) ;
#147652 = CYLINDRICAL_SURFACE ( 'NONE', #3849, 4.000000000000003553 ) ;
#147653 = CARTESIAN_POINT ( 'NONE',  ( 18.49999999999999289, 65.50857864377465489, -111.6731074845243654 ) ) ;
#147654 = CIRCLE ( 'NONE', #31556, 1.899999999999995914 ) ;
#147655 = CIRCLE ( 'NONE', #210030, 0.5000000000000004441 ) ;
#147657 = VERTEX_POINT ( 'NONE', #238343 ) ;
#147656 = EDGE_CURVE ( 'NONE', #120355, #186437, #2321, .T. ) ;
#147658 = EDGE_CURVE ( 'NONE', #52160, #27038, #77980, .T. ) ;
#147659 = CARTESIAN_POINT ( 'NONE',  ( -20.94999999999999929, -1.164121893230052995, -141.9148480855716343 ) ) ;
#147660 = LINE ( 'NONE', #87666, #215556 ) ;
#147661 = AXIS2_PLACEMENT_3D ( 'NONE', #63192, #142732, #43657 ) ;
#147662 = EDGE_LOOP ( 'NONE', ( #75156, #108883, #54901, #195112 ) ) ;
#147664 = ORIENTED_EDGE ( 'NONE', *, *, #110111, .F. ) ;
#147663 = DIRECTION ( 'NONE',  ( -0.000000000000000000, -0.1350103645451718737, 0.9908441862701622416 ) ) ;
#147665 = VECTOR ( 'NONE', #157468, 1000.000000000000000 ) ;
#147666 = CARTESIAN_POINT ( 'NONE',  ( 22.60000000000000142, 76.00000000001195133, -103.0231074845243171 ) ) ;
#147667 = EDGE_CURVE ( 'NONE', #64945, #235108, #233245, .T. ) ;
#147670 = EDGE_LOOP ( 'NONE', ( #241003, #187654, #255924, #112287 ) ) ;
#147669 = ORIENTED_EDGE ( 'NONE', *, *, #119131, .F. ) ;
#147668 = VECTOR ( 'NONE', #117158, 1000.000000000000000 ) ;
#147671 = VERTEX_POINT ( 'NONE', #136666 ) ;
#147672 = FACE_OUTER_BOUND ( 'NONE', #160094, .T. ) ;
#147673 = ORIENTED_EDGE ( 'NONE', *, *, #218926, .T. ) ;
#147674 = FACE_OUTER_BOUND ( 'NONE', #253756, .T. ) ;
#147675 = ORIENTED_EDGE ( 'NONE', *, *, #30531, .T. ) ;
#147676 = EDGE_CURVE ( 'NONE', #83555, #147965, #52315, .T. ) ;
#147677 = DIRECTION ( 'NONE',  ( 1.000000000000000000, -2.849773892568378313E-16, 7.728835255496647986E-17 ) ) ;
#147678 = EDGE_CURVE ( 'NONE', #52039, #158841, #48232, .T. ) ;
#147679 = AXIS2_PLACEMENT_3D ( 'NONE', #141833, #257885, #101377 ) ;
#147680 = CIRCLE ( 'NONE', #130917, 0.09999999999999939493 ) ;
#147681 = CARTESIAN_POINT ( 'NONE',  ( 21.14999999999999858, 1.115600667400684642E-11, -79.15000000000004832 ) ) ;
#147682 = ORIENTED_EDGE ( 'NONE', *, *, #16825, .F. ) ;
#147683 = ORIENTED_EDGE ( 'NONE', *, *, #219163, .F. ) ;
#147684 = ORIENTED_EDGE ( 'NONE', *, *, #167428, .T. ) ;
#147685 =( BOUNDED_SURFACE ( )  B_SPLINE_SURFACE ( 3, 2, ( 
 ( #236603, #37154, #78801 ),
 ( #17553, #215753, #15021 ),
 ( #97060, #57957, #95800 ),
 ( #217033, #59216, #154549 ),
 ( #134916, #38419, #235324 ),
 ( #35871, #175393, #138758 ),
 ( #218312, #39732, #20151 ),
 ( #179239, #555, #159657 ),
 ( #26578, #61840, #146485 ),
 ( #244306, #44838, #4413 ) ),
 .UNSPECIFIED., .F., .F., .F. ) 
 B_SPLINE_SURFACE_WITH_KNOTS ( ( 4, 2, 2, 2, 4 ),
 ( 3, 3 ),
 ( 0.0001836757140119173052, 0.0004000170051583524936, 0.0005081876507315700878, 0.0005622729735181788849, 0.0006163582963047876820 ),
 ( 0.000000000000000000, 1.000000000000000000 ),
 .UNSPECIFIED. ) 
 GEOMETRIC_REPRESENTATION_ITEM ( )  RATIONAL_B_SPLINE_SURFACE ( (
 ( 1.000000000000000000, 0.7071067811865414665, 1.000000000000000000),
 ( 1.000000000000000000, 0.6461995200012695673, 1.000000000000000000),
 ( 1.000000000000000000, 0.5776453529573633006, 1.000000000000000000),
 ( 1.000000000000000000, 0.4585233068339978346, 1.000000000000000000),
 ( 1.000000000000000000, 0.4154092989970996630, 1.000000000000000000),
 ( 1.000000000000000000, 0.3550093145823429164, 1.000000000000000000),
 ( 1.000000000000000000, 0.3354498651681590560, 1.000000000000000000),
 ( 1.000000000000000000, 0.3060347992261199246, 1.000000000000000000),
 ( 1.000000000000000000, 0.2963555829624707760, 1.000000000000000000),
 ( 1.000000000000000000, 0.2966190024559251515, 1.000000000000000000) ) ) 
 REPRESENTATION_ITEM ( '' )  SURFACE ( )  );
#147686 = CARTESIAN_POINT ( 'NONE',  ( 18.39999999999999503, 70.35000000001224407, -149.1731074845243938 ) ) ;
#147687 = EDGE_CURVE ( 'NONE', #51521, #197466, #81513, .T. ) ;
#147688 = ORIENTED_EDGE ( 'NONE', *, *, #230377, .F. ) ;
#147689 = EDGE_CURVE ( 'NONE', #209275, #215804, #142279, .T. ) ;
#147690 = CARTESIAN_POINT ( 'NONE',  ( 22.39999999999999503, -0.1008583690875579364, -122.2504328765106294 ) ) ;
#147692 = EDGE_LOOP ( 'NONE', ( #10768, #28693, #14561, #121470 ) ) ;
#147691 = DIRECTION ( 'NONE',  ( -1.000000000000000000, -0.000000000000000000, 0.000000000000000000 ) ) ;
#147693 = DIRECTION ( 'NONE',  ( 0.000000000000000000, 0.4721928772776973204, 0.8814952561688629284 ) ) ;
#147694 = CARTESIAN_POINT ( 'NONE',  ( 20.94999999999999929, 64.35000000001218723, -143.3069731475025037 ) ) ;
#147695 = FACE_OUTER_BOUND ( 'NONE', #65088, .T. ) ;
#147696 = CARTESIAN_POINT ( 'NONE',  ( 18.39999999999999503, 20.94763808724815846, -234.7254930126486556 ) ) ;
#147697 = CARTESIAN_POINT ( 'NONE',  ( 21.15000000000005542, 87.75000000001119815, -43.82310748452479743 ) ) ;
#147698 = AXIS2_PLACEMENT_3D ( 'NONE', #102951, #7735, #181248 ) ;
#147700 = LINE ( 'NONE', #228531, #12144 ) ;
#147699 = DIRECTION ( 'NONE',  ( -0.000000000000000000, 0.4721928772777345684, 0.8814952561688429444 ) ) ;
#147701 = DIRECTION ( 'NONE',  ( 0.000000000000000000, 0.1568667991644355497, 0.9876197685951332295 ) ) ;
#147702 = CARTESIAN_POINT ( 'NONE',  ( 18.52326479938694703, 38.02489541698627562, -261.2215218409455133 ) ) ;
#147703 = CIRCLE ( 'NONE', #93523, 0.09999999999999939493 ) ;
#147704 = EDGE_CURVE ( 'NONE', #182680, #168528, #218912, .T. ) ;
#147705 = CARTESIAN_POINT ( 'NONE',  ( -18.59999999999999787, 68.87972903831429505, -99.36354444268502561 ) ) ;
#147706 = AXIS2_PLACEMENT_3D ( 'NONE', #120652, #1941, #181892 ) ;
#147707 = VERTEX_POINT ( 'NONE', #192822 ) ;
#147708 = CIRCLE ( 'NONE', #185127, 0.09999999999998898659 ) ;
#147709 = ORIENTED_EDGE ( 'NONE', *, *, #159403, .T. ) ;
#147710 = AXIS2_PLACEMENT_3D ( 'NONE', #208047, #108917, #188457 ) ;
#147712 = ORIENTED_EDGE ( 'NONE', *, *, #156772, .F. ) ;
#147711 = DIRECTION ( 'NONE',  ( 0.000000000000000000, 0.000000000000000000, 1.000000000000000000 ) ) ;
#147713 = ORIENTED_EDGE ( 'NONE', *, *, #167151, .F. ) ;
#147714 = CARTESIAN_POINT ( 'NONE',  ( -16.94107738177415357, 65.98576071487524075, -90.47310748452439100 ) ) ;
#147715 = CARTESIAN_POINT ( 'NONE',  ( 20.51284917709620359, 10.31088662285602275, -141.6724731855920254 ) ) ;
#147717 = DIRECTION ( 'NONE',  ( 0.000000000000000000, -7.429790795770644761E-15, 1.000000000000000000 ) ) ;
#147716 = CARTESIAN_POINT ( 'NONE',  ( -23.25000000000000000, 64.25000000001190870, -103.0231074845243882 ) ) ;
#147718 = ORIENTED_EDGE ( 'NONE', *, *, #47642, .F. ) ;
#147719 = VECTOR ( 'NONE', #104703, 1000.000000000000114 ) ;
#147720 = EDGE_CURVE ( 'NONE', #183798, #196416, #235476, .T. ) ;
#147721 = AXIS2_PLACEMENT_3D ( 'NONE', #154009, #193092, #215210 ) ;
#147722 = CARTESIAN_POINT ( 'NONE',  ( 18.51997666896865624, -9.392332131507705739, -40.64340618748368428 ) ) ;
#147723 = AXIS2_PLACEMENT_3D ( 'NONE', #83867, #40965, #65626 ) ;
#147724 = EDGE_CURVE ( 'NONE', #218711, #27654, #188935, .T. ) ;
#147725 = DIRECTION ( 'NONE',  ( 1.000000000000000000, 0.000000000000000000, 0.000000000000000000 ) ) ;
#147726 = ORIENTED_EDGE ( 'NONE', *, *, #61458, .F. ) ;
#147727 = LINE ( 'NONE', #83844, #113213 ) ;
#147728 = DIRECTION ( 'NONE',  ( 0.000000000000000000, 0.000000000000000000, -1.000000000000000000 ) ) ;
#147729 = DIRECTION ( 'NONE',  ( -0.000000000000000000, -0.000000000000000000, -1.000000000000000000 ) ) ;
#147730 = DIRECTION ( 'NONE',  ( -1.000000000000000000, 0.000000000000000000, 0.000000000000000000 ) ) ;
#147731 = EDGE_CURVE ( 'NONE', #220241, #60562, #102357, .T. ) ;
#147732 = DIRECTION ( 'NONE',  ( 0.000000000000000000, 1.000000000000000000, 0.000000000000000000 ) ) ;
#147734 = ORIENTED_EDGE ( 'NONE', *, *, #217472, .T. ) ;
#147733 = DIRECTION ( 'NONE',  ( 0.7071067811865456854, 0.7071067811865493491, 4.937700262164544098E-15 ) ) ;
#147735 = AXIS2_PLACEMENT_3D ( 'NONE', #19872, #173848, #193378 ) ;
#147736 = DIRECTION ( 'NONE',  ( 0.000000000000000000, 0.9126074666063769270, 0.4088369013363280513 ) ) ;
#147737 = FACE_OUTER_BOUND ( 'NONE', #186023, .T. ) ;
#147739 = EDGE_CURVE ( 'NONE', #24027, #183601, #102178, .T. ) ;
#147738 = DIRECTION ( 'NONE',  ( 1.000000000000000000, -0.000000000000000000, 0.000000000000000000 ) ) ;
#147740 = CARTESIAN_POINT ( 'NONE',  ( 18.59999999999999076, 54.57427006634497957, -228.7596887170734306 ) ) ;
#147741 = ORIENTED_EDGE ( 'NONE', *, *, #32363, .T. ) ;
#147742 = CARTESIAN_POINT ( 'NONE',  ( 13.22461703343585526, 66.56333706821274632, -84.70007075222952153 ) ) ;
#147743 = CARTESIAN_POINT ( 'NONE',  ( -21.37071067811865532, 67.92928932189333580, -115.2731074845243455 ) ) ;
#147744 = VECTOR ( 'NONE', #233956, 1000.000000000000114 ) ;
#147746 = EDGE_CURVE ( 'NONE', #109039, #130445, #123076, .T. ) ;
#147745 = CARTESIAN_POINT ( 'NONE',  ( -21.55000000000000426, 7.750000000011159074, -88.15000000000004832 ) ) ;
#147747 = CARTESIAN_POINT ( 'NONE',  ( -16.88783316861814754, 9.950000000011137047, -54.24773595802036397 ) ) ;
#147748 = DIRECTION ( 'NONE',  ( -1.000000000000000000, 0.000000000000000000, -0.000000000000000000 ) ) ;
#147749 = CARTESIAN_POINT ( 'NONE',  ( 5.899999999999991473, -11.25000000000000000, -2.558717127065786914E-15 ) ) ;
#147750 = DIRECTION ( 'NONE',  ( 1.000000000000000000, -1.836970198721029934E-16, -1.282749433769087582E-30 ) ) ;
#147751 = DIRECTION ( 'NONE',  ( 0.000000000000000000, 0.000000000000000000, 1.000000000000000000 ) ) ;
#147752 = AXIS2_PLACEMENT_3D ( 'NONE', #90921, #110485, #50490 ) ;
#147754 = ORIENTED_EDGE ( 'NONE', *, *, #210822, .F. ) ;
#147753 = AXIS2_PLACEMENT_3D ( 'NONE', #67491, #247407, #169199 ) ;
#147755 = ADVANCED_FACE ( 'NONE', ( #243477 ), #110770, .T. ) ;
#147756 = VECTOR ( 'NONE', #109022, 1000.000000000000114 ) ;
#147758 = ADVANCED_FACE ( 'NONE', ( #42713 ), #64981, .T. ) ;
#147757 = EDGE_CURVE ( 'NONE', #113518, #225274, #101348, .T. ) ;
#147759 = ORIENTED_EDGE ( 'NONE', *, *, #199748, .F. ) ;
#147760 = ORIENTED_EDGE ( 'NONE', *, *, #102132, .F. ) ;
#147761 = CARTESIAN_POINT ( 'NONE',  ( -18.39999999999999858, 58.59921997668411819, -223.8511959880075608 ) ) ;
#147762 = DIRECTION ( 'NONE',  ( 0.000000000000000000, -1.000000000000000000, 0.000000000000000000 ) ) ;
#147763 = ORIENTED_EDGE ( 'NONE', *, *, #224514, .F. ) ;
#147764 = EDGE_CURVE ( 'NONE', #139155, #78394, #77431, .T. ) ;
#147765 = ORIENTED_EDGE ( 'NONE', *, *, #21477, .F. ) ;
#147766 = PRESENTATION_STYLE_ASSIGNMENT (( #145170 ) ) ;
#147767 = VERTEX_POINT ( 'NONE', #124828 ) ;
#147768 = EDGE_CURVE ( 'NONE', #2766, #242581, #248327, .T. ) ;
#147769 = FACE_OUTER_BOUND ( 'NONE', #210662, .T. ) ;
#147770 = VECTOR ( 'NONE', #174376, 1000.000000000000000 ) ;
#147771 = EDGE_CURVE ( 'NONE', #96642, #12745, #210727, .T. ) ;
#147772 = ORIENTED_EDGE ( 'NONE', *, *, #250735, .F. ) ;
#147773 = CARTESIAN_POINT ( 'NONE',  ( 20.95000000000005258, 65.19115966511134275, -29.92310748452479174 ) ) ;
#147774 = CARTESIAN_POINT ( 'NONE',  ( -16.93344882324368683, 30.28388429518871305, -234.7957375116174035 ) ) ;
#147775 = DIRECTION ( 'NONE',  ( -1.000000000000000000, 0.000000000000000000, -0.000000000000000000 ) ) ;
#147776 = CARTESIAN_POINT ( 'NONE',  ( -21.09813707148783735, 1.515235338312543867, -230.6900842670254690 ) ) ;
#147777 = EDGE_CURVE ( 'NONE', #57597, #149628, #194187, .T. ) ;
#147778 = CIRCLE ( 'NONE', #222766, 0.1000000000000028644 ) ;
#147779 = CARTESIAN_POINT ( 'NONE',  ( -16.89021194854739960, 30.11162787777481498, -234.7563164417510677 ) ) ;
#147780 = FACE_OUTER_BOUND ( 'NONE', #131329, .T. ) ;
#147782 = ORIENTED_EDGE ( 'NONE', *, *, #175474, .T. ) ;
#147781 = FACE_OUTER_BOUND ( 'NONE', #33062, .T. ) ;
#147784 = CARTESIAN_POINT ( 'NONE',  ( 18.49999999999999645, 1.866714910068465239, -145.7526752462820241 ) ) ;
#147783 = CARTESIAN_POINT ( 'NONE',  ( 20.94999999999999929, 11.65000000000000391, -26.71613433702190932 ) ) ;
#147785 = DIRECTION ( 'NONE',  ( -1.000000000000000000, -0.000000000000000000, -0.000000000000000000 ) ) ;
#147786 = EDGE_CURVE ( 'NONE', #257484, #248313, #31702, .T. ) ;
#147787 = VERTEX_POINT ( 'NONE', #163955 ) ;
#147788 = CARTESIAN_POINT ( 'NONE',  ( 14.22821877134046176, 66.54397173950412991, -121.5119094494586420 ) ) ;
#147789 = DIRECTION ( 'NONE',  ( -1.000000000000000000, -0.000000000000000000, 0.000000000000000000 ) ) ;
#147790 = FACE_OUTER_BOUND ( 'NONE', #114263, .T. ) ;
#147791 = ORIENTED_EDGE ( 'NONE', *, *, #185094, .F. ) ;
#147792 = ADVANCED_FACE ( 'NONE', ( #221328 ), #60879, .F. ) ;
#147793 = DIRECTION ( 'NONE',  ( 0.000000000000000000, 6.997203936713167125E-15, -1.000000000000000000 ) ) ;
#147794 = DIRECTION ( 'NONE',  ( 0.000000000000000000, 0.000000000000000000, -1.000000000000000000 ) ) ;
#147795 = ORIENTED_EDGE ( 'NONE', *, *, #147310, .T. ) ;
#147796 = TOROIDAL_SURFACE ( 'NONE', #39662, 2.100000000000002309, 0.1000000000000000056 ) ;
#147798 = DIRECTION ( 'NONE',  ( 1.000000000000000000, 0.000000000000000000, 0.000000000000000000 ) ) ;
#147797 = CIRCLE ( 'NONE', #118765, 0.09999999999999971412 ) ;
#147799 = DIRECTION ( 'NONE',  ( 0.000000000000000000, 0.1455152366551700771, 0.9893560106964479628 ) ) ;
#147800 = PLANE ( 'NONE',  #199098 ) ;
#147801 = CARTESIAN_POINT ( 'NONE',  ( -22.45437739390953169, 1.115486826172573664E-11, -122.3504291884013071 ) ) ;
#147802 = EDGE_CURVE ( 'NONE', #108265, #143721, #256452, .T. ) ;
#147803 = ORIENTED_EDGE ( 'NONE', *, *, #16228, .T. ) ;
#147804 = ORIENTED_EDGE ( 'NONE', *, *, #159946, .T. ) ;
#147806 = ADVANCED_FACE ( 'NONE', ( #144348 ), #51622, .T. ) ;
#147805 = CARTESIAN_POINT ( 'NONE',  ( -23.25000000000000000, 87.75000000001165290, -69.52310748452424605 ) ) ;
#147807 = LINE ( 'NONE', #164798, #198153 ) ;
#147808 = CARTESIAN_POINT ( 'NONE',  ( 18.59999999999999076, 69.35000000001180354, -81.87310748452435405 ) ) ;
#147809 = DIRECTION ( 'NONE',  ( 0.000000000000000000, 0.8814952561688437216, -0.4721928772777334582 ) ) ;
#147810 = AXIS2_PLACEMENT_3D ( 'NONE', #129972, #30930, #212114 ) ;
#147811 = DIRECTION ( 'NONE',  ( 1.000000000000000000, 0.000000000000000000, -0.000000000000000000 ) ) ;
#147812 = CIRCLE ( 'NONE', #122877, 7.900000000000003908 ) ;
#147813 = LINE ( 'NONE', #87799, #222566 ) ;
#147814 = CARTESIAN_POINT ( 'NONE',  ( 23.24999999999999645, 53.37686160793744250, -235.8706811220569932 ) ) ;
#147816 = ORIENTED_EDGE ( 'NONE', *, *, #187643, .F. ) ;
#147815 = CIRCLE ( 'NONE', #39862, 0.1999999999999987899 ) ;
#147817 = CARTESIAN_POINT ( 'NONE',  ( -20.94999027547553894, 65.70673848566976005, -97.56382523348287350 ) ) ;
#147818 = AXIS2_PLACEMENT_3D ( 'NONE', #73506, #90451, #168775 ) ;
#147820 = ORIENTED_EDGE ( 'NONE', *, *, #205563, .T. ) ;
#147819 = CARTESIAN_POINT ( 'NONE',  ( 21.05000000000000071, 5.000000000011153745, -179.9052660189130677 ) ) ;
#147821 = CARTESIAN_POINT ( 'NONE',  ( 20.94999999999999574, 17.02177226667169663, -224.5487030889150901 ) ) ;
#147822 = CARTESIAN_POINT ( 'NONE',  ( 16.87683809663749557, 66.05000000001155058, -48.67310748452439384 ) ) ;
#147823 = DIRECTION ( 'NONE',  ( 0.000000000000000000, 0.000000000000000000, 1.000000000000000000 ) ) ;
#147825 = CARTESIAN_POINT ( 'NONE',  ( -16.84981964351479178, 66.08268176591337806, -123.6535058705048726 ) ) ;
#147824 =( GEOMETRIC_REPRESENTATION_CONTEXT ( 3 ) GLOBAL_UNCERTAINTY_ASSIGNED_CONTEXT ( ( #6098 ) ) GLOBAL_UNIT_ASSIGNED_CONTEXT ( ( #35512, #193272, #13349 ) ) REPRESENTATION_CONTEXT ( 'NONE', 'WORKASPACE' ) );
#147826 = EDGE_CURVE ( 'NONE', #224742, #174422, #127532, .T. ) ;
#147828 = ORIENTED_EDGE ( 'NONE', *, *, #127769, .T. ) ;
#147827 = LINE ( 'NONE', #48702, #144313 ) ;
#147829 = CARTESIAN_POINT ( 'NONE',  ( -18.59999999999999787, 80.78317333349157536, -192.9003134612048882 ) ) ;
#147830 = CARTESIAN_POINT ( 'NONE',  ( -18.51697539158857353, 65.68434038414410736, -164.4866880726065972 ) ) ;
#147831 = LINE ( 'NONE', #48705, #34601 ) ;
#147832 = DIRECTION ( 'NONE',  ( 0.000000000000000000, -6.982962677686266711E-15, 1.000000000000000000 ) ) ;
#147833 = ORIENTED_EDGE ( 'NONE', *, *, #1031, .F. ) ;
#147834 = DIRECTION ( 'NONE',  ( 0.000000000000000000, 0.000000000000000000, 1.000000000000000000 ) ) ;
#147835 = CARTESIAN_POINT ( 'NONE',  ( -16.77308656112214535, 66.05000000001201954, -115.6733006762266598 ) ) ;
#147836 = EDGE_LOOP ( 'NONE', ( #257138, #6837, #107841 ) ) ;
#147838 = CYLINDRICAL_SURFACE ( 'NONE', #196129, 4.000000000000003553 ) ;
#147837 = B_SPLINE_CURVE_WITH_KNOTS ( 'NONE', 3,
 ( #110310, #213253, #73786, #191159, #188563, #30805, #49049, #9928, #171606, #34655, #131155, #189851, #248537, #209407, #251089, #132445 ),
 .UNSPECIFIED., .F., .F.,
 ( 4, 3, 3, 3, 3, 4 ),
 ( 0.000000000000000000, 2.372700795694549170E-05, 5.739057815867263442E-05, 9.073899019180726251E-05, 0.0001243544287365786784, 0.0001585386695601235239 ),
 .UNSPECIFIED. ) ;
#147839 = DIRECTION ( 'NONE',  ( 0.000000000000000000, 0.8660254037844411501, 0.4999999999999956701 ) ) ;
#147840 = ORIENTED_EDGE ( 'NONE', *, *, #8817, .T. ) ;
#147841 = EDGE_CURVE ( 'NONE', #52704, #210905, #156616, .T. ) ;
#147842 = CARTESIAN_POINT ( 'NONE',  ( -21.14999999999999858, 64.35000000001238618, -169.9231074845244507 ) ) ;
#147843 = VECTOR ( 'NONE', #112041, 1000.000000000000000 ) ;
#147844 = VERTEX_POINT ( 'NONE', #187376 ) ;
#147845 = TOROIDAL_SURFACE ( 'NONE', #35435, 0.6000000000000009770, 0.1000000000000000056 ) ;
#147846 = DIRECTION ( 'NONE',  ( 3.265361837132813093E-16, 0.4088369013363281068, -0.9126074666063770380 ) ) ;
#147848 = DIRECTION ( 'NONE',  ( 0.000000000000000000, 0.8814952561688430555, -0.4721928772777346239 ) ) ;
#147847 = TOROIDAL_SURFACE ( 'NONE', #189347, 0.2000000000000000111, 0.1000000000000000056 ) ;
#147849 = CARTESIAN_POINT ( 'NONE',  ( -20.94999999999999929, 0.000000000000000000, -33.50000000000000000 ) ) ;
#147850 = ORIENTED_EDGE ( 'NONE', *, *, #169308, .T. ) ;
#147851 = CIRCLE ( 'NONE', #160521, 0.5000000000000004441 ) ;
#147853 = DIRECTION ( 'NONE',  ( -0.000000000000000000, 0.4721928772777345684, 0.8814952561688429444 ) ) ;
#147852 = AXIS2_PLACEMENT_3D ( 'NONE', #155714, #202509, #47263 ) ;
#147854 = AXIS2_PLACEMENT_3D ( 'NONE', #207581, #9349, #188007 ) ;
#147855 = DIRECTION ( 'NONE',  ( 1.000000000000000000, -0.000000000000000000, -0.000000000000000000 ) ) ;
#147856 = DIRECTION ( 'NONE',  ( 0.000000000000000000, -0.000000000000000000, 1.000000000000000000 ) ) ;
#147857 = DIRECTION ( 'NONE',  ( 0.000000000000000000, 0.000000000000000000, -1.000000000000000000 ) ) ;
#147858 = CARTESIAN_POINT ( 'NONE',  ( 20.94999999999999929, 52.46376478296784285, -232.8540772485547450 ) ) ;
#147859 = ORIENTED_EDGE ( 'NONE', *, *, #195585, .F. ) ;
#147861 = ORIENTED_EDGE ( 'NONE', *, *, #94707, .T. ) ;
#147860 = FACE_OUTER_BOUND ( 'NONE', #83236, .T. ) ;
#147862 = VECTOR ( 'NONE', #247352, 1000.000000000000000 ) ;
#147863 = ORIENTED_EDGE ( 'NONE', *, *, #112146, .T. ) ;
#147864 = DIRECTION ( 'NONE',  ( 0.000000000000000000, -0.8814952561688430555, 0.4721928772777346239 ) ) ;
#147865 = ORIENTED_EDGE ( 'NONE', *, *, #33963, .T. ) ;
#147866 = FACE_OUTER_BOUND ( 'NONE', #175955, .T. ) ;
#147867 = CIRCLE ( 'NONE', #35462, 0.09999999999999939493 ) ;
#147868 = CARTESIAN_POINT ( 'NONE',  ( -21.29999999999995808, 68.29137419664525055, -231.9463301769586394 ) ) ;
#147869 = DIRECTION ( 'NONE',  ( 0.000000000000000000, -0.5378121776619179117, 0.8430646840892729310 ) ) ;
#147870 = ORIENTED_EDGE ( 'NONE', *, *, #133298, .F. ) ;
#147872 = AXIS2_PLACEMENT_3D ( 'NONE', #60689, #158553, #62007 ) ;
#147871 = CARTESIAN_POINT ( 'NONE',  ( 22.39999999999999503, 64.25000000001165290, -69.62310748452439668 ) ) ;
#147873 = CARTESIAN_POINT ( 'NONE',  ( 23.14999999999999858, 1.148907358139439339E-11, -201.0000000000015064 ) ) ;
#147874 = CARTESIAN_POINT ( 'NONE',  ( 23.14999999999999503, 64.35000000001222986, -148.6731074845244507 ) ) ;
#147875 = ORIENTED_EDGE ( 'NONE', *, *, #223299, .T. ) ;
#147876 = DIRECTION ( 'NONE',  ( 0.000000000000000000, 0.000000000000000000, 1.000000000000000000 ) ) ;
#147878 = ORIENTED_EDGE ( 'NONE', *, *, #128933, .T. ) ;
#147877 = DIRECTION ( 'NONE',  ( 1.000000000000000000, 0.000000000000000000, 0.000000000000000000 ) ) ;
#147879 = ADVANCED_FACE ( 'NONE', ( #92108 ), #88228, .T. ) ;
#147880 = CARTESIAN_POINT ( 'NONE',  ( -18.40000000000000213, 5.650000000011139001, -79.65000000000004832 ) ) ;
#147881 = DIRECTION ( 'NONE',  ( 0.000000000000000000, -0.9908441862701596881, -0.1350103645451904977 ) ) ;
#147882 = VERTEX_POINT ( 'NONE', #146928 ) ;
#147883 = DIRECTION ( 'NONE',  ( 1.000000000000000000, 0.000000000000000000, 0.000000000000000000 ) ) ;
#147884 = CARTESIAN_POINT ( 'NONE',  ( -13.22483237240078502, 66.56332574816921976, -121.3462455535252076 ) ) ;
#147885 = CARTESIAN_POINT ( 'NONE',  ( 21.05000000000000426, 39.20539516596018359, -236.6597403278730383 ) ) ;
#147886 = ORIENTED_EDGE ( 'NONE', *, *, #219705, .T. ) ;
#147887 = FACE_OUTER_BOUND ( 'NONE', #228213, .T. ) ;
#147888 = EDGE_CURVE ( 'NONE', #61221, #153341, #231583, .T. ) ;
#147889 = CARTESIAN_POINT ( 'NONE',  ( 20.99780126800950342, 64.39461131213610656, -176.9357549128194194 ) ) ;
#147890 = EDGE_CURVE ( 'NONE', #91949, #152443, #152503, .T. ) ;
#147891 = CIRCLE ( 'NONE', #177126, 2.000000000000001776 ) ;
#147892 = ORIENTED_EDGE ( 'NONE', *, *, #209466, .T. ) ;
#147893 = CIRCLE ( 'NONE', #43650, 0.09999999999999939493 ) ;
#147894 = CIRCLE ( 'NONE', #256143, 0.09999999999998898659 ) ;
#147895 = EDGE_CURVE ( 'NONE', #227236, #29243, #131234, .T. ) ;
#147896 = VERTEX_POINT ( 'NONE', #210772 ) ;
#147897 = CARTESIAN_POINT ( 'NONE',  ( 21.07928932188134397, 0.09889514566555242248, -94.17148334360672379 ) ) ;
#147898 = CIRCLE ( 'NONE', #218594, 0.1999999999999987899 ) ;
#147899 = EDGE_CURVE ( 'NONE', #161400, #102756, #144069, .T. ) ;
#147900 = ORIENTED_EDGE ( 'NONE', *, *, #40911, .F. ) ;
#147901 = EDGE_CURVE ( 'NONE', #27502, #169538, #49126, .T. ) ;
#147902 = CARTESIAN_POINT ( 'NONE',  ( -16.95709691156997323, 9.950000000011497647, -188.3399424374871103 ) ) ;
#147903 = CARTESIAN_POINT ( 'NONE',  ( -16.80621392010912629, 66.05779742250483366, -182.7126994499415957 ) ) ;
#147905 = EDGE_LOOP ( 'NONE', ( #11848, #223194, #223731, #248671, #205877, #138608, #13444, #63330, #30821, #165502, #70957, #81585 ) ) ;
#147904 = CARTESIAN_POINT ( 'NONE',  ( 20.85000000000000142, 1.115600667400684642E-11, -200.9999999999999432 ) ) ;
#147907 = LINE ( 'NONE', #27983, #136789 ) ;
#147906 = B_SPLINE_CURVE_WITH_KNOTS ( 'NONE', 3,
 ( #227047, #48408, #169698, #30161, #150111, #8023 ),
 .UNSPECIFIED., .F., .F.,
 ( 4, 2, 4 ),
 ( 0.000000000000000000, 0.0001895189928937381313, 0.0003790379857874762626 ),
 .UNSPECIFIED. ) ;
#147908 = DIRECTION ( 'NONE',  ( 1.000000000000000000, 0.000000000000000000, 0.000000000000000000 ) ) ;
#147909 = ADVANCED_FACE ( 'NONE', ( #188639 ), #27035, .F. ) ;
#147910 = CARTESIAN_POINT ( 'NONE',  ( -21.14999999999994174, 87.50449464844290048, -37.85861909827351468 ) ) ;
#147911 = CARTESIAN_POINT ( 'NONE',  ( 21.05000000000000071, 6.540656951712400691, -67.10000000000005116 ) ) ;
#147912 = FACE_BOUND ( 'NONE', #38039, .T. ) ;
#147913 = AXIS2_PLACEMENT_3D ( 'NONE', #151609, #35525, #231141 ) ;
#147914 = CARTESIAN_POINT ( 'NONE',  ( -17.05016517656043362, 9.950000000011138823, -79.67269799600136082 ) ) ;
#147915 = CARTESIAN_POINT ( 'NONE',  ( -18.43599941264906050, -9.519327428583675754, -107.4729767895213115 ) ) ;
#147917 = ORIENTED_EDGE ( 'NONE', *, *, #48496, .T. ) ;
#147916 = CARTESIAN_POINT ( 'NONE',  ( 23.25000000000000000, -9.599999999988845900, -177.3939691226524076 ) ) ;
#147918 = CARTESIAN_POINT ( 'NONE',  ( 21.05000000000000071, 71.00000000001158185, -57.11784146561126363 ) ) ;
#147919 = EDGE_CURVE ( 'NONE', #185124, #58187, #131619, .T. ) ;
#147920 = CIRCLE ( 'NONE', #22848, 0.1000000000000072220 ) ;
#147921 = AXIS2_PLACEMENT_3D ( 'NONE', #37585, #117110, #54556 ) ;
#147922 = DIRECTION ( 'NONE',  ( 0.000000000000000000, 0.000000000000000000, -1.000000000000000000 ) ) ;
#147923 = CARTESIAN_POINT ( 'NONE',  ( 21.14999999999999858, 6.650000000011155876, -146.2500000000000284 ) ) ;
#147924 = DIRECTION ( 'NONE',  ( 0.000000000000000000, 0.000000000000000000, -1.000000000000000000 ) ) ;
#147925 = FACE_OUTER_BOUND ( 'NONE', #123642, .T. ) ;
#147926 = VERTEX_POINT ( 'NONE', #169119 ) ;
#147927 = ADVANCED_FACE ( 'NONE', ( #248616 ), #51671, .F. ) ;
#147928 = CARTESIAN_POINT ( 'NONE',  ( 20.85000000000000142, 62.42744096235649920, -225.1319887738535499 ) ) ;
#147929 = DIRECTION ( 'NONE',  ( 0.000000000000000000, -0.1350103645451876666, 0.9908441862701600211 ) ) ;
#147930 = VERTEX_POINT ( 'NONE', #229066 ) ;
#147931 = CARTESIAN_POINT ( 'NONE',  ( 21.05000000000000426, 76.01759718702115265, -209.9638783781857683 ) ) ;
#147932 = AXIS2_PLACEMENT_3D ( 'NONE', #104845, #1911, #202695 ) ;
#147933 = CARTESIAN_POINT ( 'NONE',  ( -16.97048326478265778, 61.06790646447517901, -220.5677433478223861 ) ) ;
#147934 = ADVANCED_FACE ( 'NONE', ( #50389 ), #171684, .T. ) ;
#147935 = ORIENTED_EDGE ( 'NONE', *, *, #208134, .F. ) ;
#147936 = ORIENTED_EDGE ( 'NONE', *, *, #84462, .T. ) ;
#147937 = DIRECTION ( 'NONE',  ( 1.000000000000000000, 0.000000000000000000, 0.000000000000000000 ) ) ;
#147938 = EDGE_LOOP ( 'NONE', ( #197675, #134444, #209589, #177726 ) ) ;
#147939 = CARTESIAN_POINT ( 'NONE',  ( -11.59999999999994458, 64.25000000001119815, -18.32310748452479388 ) ) ;
#147940 = CARTESIAN_POINT ( 'NONE',  ( 0.9000000000000000222, -12.25000000000000355, 26.00000000000000355 ) ) ;
#147941 = ORIENTED_EDGE ( 'NONE', *, *, #195750, .F. ) ;
#147942 = ORIENTED_EDGE ( 'NONE', *, *, #210197, .T. ) ;
#147943 = DIRECTION ( 'NONE',  ( 1.836970198721029934E-16, -1.000000000000000000, -0.000000000000000000 ) ) ;
#147945 = ORIENTED_EDGE ( 'NONE', *, *, #24420, .T. ) ;
#147944 = PRESENTATION_STYLE_ASSIGNMENT (( #85358 ) ) ;
#147946 = DIRECTION ( 'NONE',  ( 0.000000000000000000, 0.000000000000000000, 1.000000000000000000 ) ) ;
#147947 = AXIS2_PLACEMENT_3D ( 'NONE', #167617, #189732, #11096 ) ;
#147948 = ORIENTED_EDGE ( 'NONE', *, *, #36342, .T. ) ;
#147949 = EDGE_CURVE ( 'NONE', #235211, #119302, #23327, .T. ) ;
#147950 = AXIS2_PLACEMENT_3D ( 'NONE', #128920, #45524, #6390 ) ;
#147951 = ORIENTED_EDGE ( 'NONE', *, *, #233641, .T. ) ;
#147952 = CARTESIAN_POINT ( 'NONE',  ( 21.05000000000000071, 61.00122447389660607, -225.2976766370351527 ) ) ;
#147953 = EDGE_CURVE ( 'NONE', #12740, #77748, #7428, .T. ) ;
#147954 = CARTESIAN_POINT ( 'NONE',  ( 21.05000000000000071, 0.09779029130879170195, 6.257814610476124528 ) ) ;
#147955 = CARTESIAN_POINT ( 'NONE',  ( -16.79363873026997922, 9.948850229418431113, -20.84615378144547293 ) ) ;
#147956 = CARTESIAN_POINT ( 'NONE',  ( 21.05000000000000071, 65.27628289530404970, -57.37310748452439668 ) ) ;
#147957 = DIRECTION ( 'NONE',  ( 0.000000000000000000, 0.000000000000000000, 1.000000000000000000 ) ) ;
#147959 = VERTEX_POINT ( 'NONE', #17692 ) ;
#147958 = EDGE_CURVE ( 'NONE', #74683, #205943, #252399, .T. ) ;
#147961 = EDGE_CURVE ( 'NONE', #184556, #171093, #212075, .T. ) ;
#147960 = DIRECTION ( 'NONE',  ( -0.000000000000000000, 1.000000000000000000, 0.000000000000000000 ) ) ;
#147962 = FACE_OUTER_BOUND ( 'NONE', #21782, .T. ) ;
#147963 = DIRECTION ( 'NONE',  ( 1.000000000000000000, -0.000000000000000000, -0.000000000000000000 ) ) ;
#147964 = DIRECTION ( 'NONE',  ( -1.000000000000000000, 0.000000000000000000, 0.000000000000000000 ) ) ;
#147965 = VERTEX_POINT ( 'NONE', #132527 ) ;
#147966 = CARTESIAN_POINT ( 'NONE',  ( 18.58222699835054570, 10.33200063080772324, -106.0931674956643320 ) ) ;
#147968 = EDGE_CURVE ( 'NONE', #68342, #117271, #192499, .T. ) ;
#147967 = ORIENTED_EDGE ( 'NONE', *, *, #112716, .F. ) ;
#147969 = DIRECTION ( 'NONE',  ( 1.000000000000000000, 0.000000000000000000, 0.000000000000000000 ) ) ;
#147970 = EDGE_LOOP ( 'NONE', ( #128660, #69380, #92501, #158383 ) ) ;
#147971 = VECTOR ( 'NONE', #184524, 1000.000000000000000 ) ;
#147972 = DIRECTION ( 'NONE',  ( -1.000000000000000000, 0.000000000000000000, 0.000000000000000000 ) ) ;
#147973 = DIRECTION ( 'NONE',  ( 0.000000000000000000, 0.4088369013363783999, -0.9126074666063545004 ) ) ;
#147974 = ADVANCED_FACE ( 'NONE', ( #33466 ), #19197, .F. ) ;
#147975 = EDGE_LOOP ( 'NONE', ( #92795, #61678, #133203, #25928 ) ) ;
#147976 = ORIENTED_EDGE ( 'NONE', *, *, #12975, .F. ) ;
#147978 = EDGE_LOOP ( 'NONE', ( #31263, #222033, #118567, #167634 ) ) ;
#147977 = FACE_OUTER_BOUND ( 'NONE', #202504, .T. ) ;
#147979 = CARTESIAN_POINT ( 'NONE',  ( -21.65000000000000213, 7.750000000000000000, -12.34999999999999964 ) ) ;
#147980 = ORIENTED_EDGE ( 'NONE', *, *, #203527, .F. ) ;
#147981 = DIRECTION ( 'NONE',  ( 1.000000000000000000, 0.000000000000000000, 0.000000000000000000 ) ) ;
#147982 = CARTESIAN_POINT ( 'NONE',  ( -20.94999999999999929, -1.835341550213255957, -78.55515129256303908 ) ) ;
#147983 = ORIENTED_EDGE ( 'NONE', *, *, #147158, .F. ) ;
#147984 = LINE ( 'NONE', #108847, #47842 ) ;
#147986 = CARTESIAN_POINT ( 'NONE',  ( -23.15000000000000213, 5.256951610580939516, -213.3897168960460533 ) ) ;
#147985 = AXIS2_PLACEMENT_3D ( 'NONE', #216606, #177523, #151850 ) ;
#147987 = AXIS2_PLACEMENT_3D ( 'NONE', #100081, #6126, #158830 ) ;
#147988 = ORIENTED_EDGE ( 'NONE', *, *, #80970, .F. ) ;
#147989 = VECTOR ( 'NONE', #546, 1000.000000000000000 ) ;
#147990 = EDGE_CURVE ( 'NONE', #172095, #134186, #164937, .T. ) ;
#147991 = DIRECTION ( 'NONE',  ( 0.000000000000000000, -2.428612866367527723E-14, -1.000000000000000000 ) ) ;
#147992 = MECHANICAL_DESIGN_GEOMETRIC_PRESENTATION_REPRESENTATION (  '', ( #98073 ), #156408 ) ;
#147993 = DIRECTION ( 'NONE',  ( 0.000000000000000000, 0.000000000000000000, -1.000000000000000000 ) ) ;
#147994 = EDGE_CURVE ( 'NONE', #224903, #212285, #136337, .T. ) ;
#147995 = ADVANCED_FACE ( 'NONE', ( #133798 ), #135067, .T. ) ;
#147996 = CARTESIAN_POINT ( 'NONE',  ( 21.05000000000000071, -9.399999999988844834, -90.60603087734760663 ) ) ;
#147998 = ORIENTED_EDGE ( 'NONE', *, *, #192474, .T. ) ;
#147997 = LINE ( 'NONE', #129711, #209962 ) ;
#147999 = DIRECTION ( 'NONE',  ( 0.000000000000000000, 0.000000000000000000, -1.000000000000000000 ) ) ;
#148000 = CARTESIAN_POINT ( 'NONE',  ( -22.57320508075687115, 11.75000000001115552, -134.0000000000000000 ) ) ;
#148001 = CARTESIAN_POINT ( 'NONE',  ( -18.59999999999999787, 78.48087866980282001, -232.8271061603568910 ) ) ;
#148003 = LINE ( 'NONE', #108869, #232540 ) ;
#148002 = DIRECTION ( 'NONE',  ( 0.000000000000000000, 0.000000000000000000, 1.000000000000000000 ) ) ;
#148004 = CARTESIAN_POINT ( 'NONE',  ( -20.90851465518106167, 65.67467670974468774, -164.4531731826884879 ) ) ;
#148005 = DIRECTION ( 'NONE',  ( 1.000000000000000000, 0.000000000000000000, 0.000000000000000000 ) ) ;
#148006 = DIRECTION ( 'NONE',  ( -1.000000000000000000, 0.000000000000000000, 0.000000000000000000 ) ) ;
#148007 = CYLINDRICAL_SURFACE ( 'NONE', #30235, 4.000000000000003553 ) ;
#148008 = VECTOR ( 'NONE', #118459, 1000.000000000000000 ) ;
#148009 = ORIENTED_EDGE ( 'NONE', *, *, #105025, .T. ) ;
#148010 =( GEOMETRIC_REPRESENTATION_CONTEXT ( 3 ) GLOBAL_UNCERTAINTY_ASSIGNED_CONTEXT ( ( #73822 ) ) GLOBAL_UNIT_ASSIGNED_CONTEXT ( ( #175605, #116900, #156058 ) ) REPRESENTATION_CONTEXT ( 'NONE', 'WORKASPACE' ) );
#148011 = VECTOR ( 'NONE', #98734, 1000.000000000000114 ) ;
#148012 = ORIENTED_EDGE ( 'NONE', *, *, #155678, .F. ) ;
#148013 = ORIENTED_EDGE ( 'NONE', *, *, #174070, .T. ) ;
#148014 = CARTESIAN_POINT ( 'NONE',  ( 21.13461538461538325, 11.30999384151886211, -211.1763045966511640 ) ) ;
#148015 = CIRCLE ( 'NONE', #35632, 12.87500000000000000 ) ;
#148016 = CIRCLE ( 'NONE', #68940, 0.1000000000000028644 ) ;
#148017 = AXIS2_PLACEMENT_3D ( 'NONE', #184220, #206370, #145087 ) ;
#148018 = LINE ( 'NONE', #199342, #111102 ) ;
#148020 = EDGE_CURVE ( 'NONE', #231975, #40984, #193785, .T. ) ;
#148019 = ORIENTED_EDGE ( 'NONE', *, *, #95349, .F. ) ;
#148021 = DIRECTION ( 'NONE',  ( 1.296989514748957922E-15, -0.9887567792719341719, 0.1495327102803664099 ) ) ;
#148022 = DIRECTION ( 'NONE',  ( 0.000000000000000000, 0.2128009952263485993, -0.9770955615653341697 ) ) ;
#148023 = EDGE_CURVE ( 'NONE', #156064, #163980, #253735, .T. ) ;
#148024 = DIRECTION ( 'NONE',  ( 0.000000000000000000, -0.5000000000000016653, 0.8660254037844377084 ) ) ;
#148025 = ORIENTED_EDGE ( 'NONE', *, *, #46542, .T. ) ;
#148026 = ORIENTED_EDGE ( 'NONE', *, *, #23842, .T. ) ;
#148028 = CARTESIAN_POINT ( 'NONE',  ( -16.86757978335471364, 9.965650379045438712, -46.09800465316752138 ) ) ;
#148027 = TOROIDAL_SURFACE ( 'NONE', #35645, 0.2000000000000000111, 0.1000000000000000056 ) ;
#148029 = DIRECTION ( 'NONE',  ( 1.000000000000000000, 0.000000000000000000, -0.000000000000000000 ) ) ;
#148030 = ORIENTED_EDGE ( 'NONE', *, *, #130285, .F. ) ;
#148031 = CIRCLE ( 'NONE', #135550, 0.09999999999999986677 ) ;
#148032 = EDGE_CURVE ( 'NONE', #87352, #201117, #35957, .T. ) ;
#148033 = DIRECTION ( 'NONE',  ( 0.000000000000000000, 0.8814952561688429444, -0.4721928772777348460 ) ) ;
#148035 = EDGE_LOOP ( 'NONE', ( #136520, #83461, #195778, #110860 ) ) ;
#148034 = CARTESIAN_POINT ( 'NONE',  ( -17.04761207306817283, 65.97354912661403148, -82.17310748452439384 ) ) ;
#148036 = DIRECTION ( 'NONE',  ( 0.000000000000000000, 6.982962677686266711E-15, -1.000000000000000000 ) ) ;
#148037 = CARTESIAN_POINT ( 'NONE',  ( -16.87665923198281348, 9.950000000011138823, -121.3500000000000369 ) ) ;
#148038 = TOROIDAL_SURFACE ( 'NONE', #60538, 0.2000000000000000111, 0.1000000000000000056 ) ;
#148040 = ORIENTED_EDGE ( 'NONE', *, *, #137099, .T. ) ;
#148039 = CARTESIAN_POINT ( 'NONE',  ( 20.94999999999999574, 16.44800918141279666, -240.8068063186265135 ) ) ;
#148042 = EDGE_CURVE ( 'NONE', #240802, #10416, #197649, .T. ) ;
#148041 = CARTESIAN_POINT ( 'NONE',  ( -20.54999999999999716, 1.115624548013267999E-11, -98.60000000000005116 ) ) ;
#148043 = CYLINDRICAL_SURFACE ( 'NONE', #216574, 0.1000000000000028644 ) ;
#148044 = FACE_OUTER_BOUND ( 'NONE', #38813, .T. ) ;
#148045 = CARTESIAN_POINT ( 'NONE',  ( -23.25000000000000000, 43.35377423437995503, -245.1717807829448930 ) ) ;
#148047 = CARTESIAN_POINT ( 'NONE',  ( -21.14999999999999858, 87.75000000001266187, -200.6231074845242688 ) ) ;
#148046 = FACE_OUTER_BOUND ( 'NONE', #37012, .T. ) ;
#148049 = EDGE_CURVE ( 'NONE', #143950, #152244, #139970, .T. ) ;
#148048 = FACE_OUTER_BOUND ( 'NONE', #9685, .T. ) ;
#148050 = CARTESIAN_POINT ( 'NONE',  ( -20.94999999999999929, 46.59314322379660922, -243.1831726892433210 ) ) ;
#148051 = LINE ( 'NONE', #163766, #226548 ) ;
#148052 = DIRECTION ( 'NONE',  ( 0.000000000000000000, -0.1350103645451807555, -0.9908441862701609093 ) ) ;
#148053 = ORIENTED_EDGE ( 'NONE', *, *, #52345, .F. ) ;
#148054 = EDGE_LOOP ( 'NONE', ( #178692, #243007, #115627, #241151 ) ) ;
#148055 = EDGE_CURVE ( 'NONE', #169097, #220497, #102545, .T. ) ;
#148056 = DIRECTION ( 'NONE',  ( 1.000000000000000000, -0.000000000000000000, 0.000000000000000000 ) ) ;
#148057 = EDGE_CURVE ( 'NONE', #241619, #41069, #202362, .T. ) ;
#148058 = VERTEX_POINT ( 'NONE', #159802 ) ;
#148059 = CARTESIAN_POINT ( 'NONE',  ( -20.64999999999999858, 9.614325556249161409, -211.5456030694648746 ) ) ;
#148060 = EDGE_LOOP ( 'NONE', ( #58314, #34444, #68737, #219441 ) ) ;
#148061 = CARTESIAN_POINT ( 'NONE',  ( 20.85000000000000142, 76.00000000001170974, -69.52310748452431710 ) ) ;
#148062 = DIRECTION ( 'NONE',  ( 1.000000000000000000, 0.000000000000000000, 0.000000000000000000 ) ) ;
#148063 = CIRCLE ( 'NONE', #56462, 0.1000000000000028644 ) ;
#148064 = AXIS2_PLACEMENT_3D ( 'NONE', #29320, #188352, #213046 ) ;
#148065 = ORIENTED_EDGE ( 'NONE', *, *, #45110, .T. ) ;
#148066 = CARTESIAN_POINT ( 'NONE',  ( -23.25000000000000000, 77.25000000001209344, -128.7226267301092548 ) ) ;
#148067 = PRESENTATION_STYLE_ASSIGNMENT (( #68533 ) ) ;
#148068 = CIRCLE ( 'NONE', #39940, 0.4000000000000114575 ) ;
#148069 = ORIENTED_EDGE ( 'NONE', *, *, #58820, .F. ) ;
#148070 = EDGE_CURVE ( 'NONE', #120061, #151479, #120127, .T. ) ;
#148071 = ORIENTED_EDGE ( 'NONE', *, *, #162717, .T. ) ;
#148072 = EDGE_CURVE ( 'NONE', #229408, #131894, #202537, .T. ) ;
#148073 = VERTEX_POINT ( 'NONE', #119385 ) ;
#148074 = CARTESIAN_POINT ( 'NONE',  ( 20.94999999999999929, 70.15000000001221281, -146.6556047088023149 ) ) ;
#148075 = CARTESIAN_POINT ( 'NONE',  ( 18.59999999999999076, 1.115600667400684642E-11, -200.9999999999999432 ) ) ;
#148076 = DIRECTION ( 'NONE',  ( 0.000000000000000000, 0.000000000000000000, 1.000000000000000000 ) ) ;
#148077 = CARTESIAN_POINT ( 'NONE',  ( 23.24999999999999645, 41.49355468354239207, -237.7178856438439141 ) ) ;
#148078 = DIRECTION ( 'NONE',  ( 0.000000000000000000, -0.000000000000000000, 1.000000000000000000 ) ) ;
#148080 = DIRECTION ( 'NONE',  ( 0.000000000000000000, 0.2128009952263601456, -0.9770955615653315052 ) ) ;
#148079 = DIRECTION ( 'NONE',  ( -1.000000000000000000, -0.000000000000000000, -0.000000000000000000 ) ) ;
#148082 = ORIENTED_EDGE ( 'NONE', *, *, #126979, .T. ) ;
#148081 = DIRECTION ( 'NONE',  ( 0.000000000000000000, 0.2617529984165031243, 0.9651348961777157509 ) ) ;
#148084 = CARTESIAN_POINT ( 'NONE',  ( 23.40000000000005187, 64.25000000001119815, -3.123107484524795474 ) ) ;
#148083 = CARTESIAN_POINT ( 'NONE',  ( 20.52683494730037239, 8.980530818312608687, -75.50525272253725007 ) ) ;
#148085 = CARTESIAN_POINT ( 'NONE',  ( 18.59999999999999787, 77.36242903720516040, -95.13422623660308375 ) ) ;
#148086 = VECTOR ( 'NONE', #193250, 1000.000000000000000 ) ;
#148087 = ORIENTED_EDGE ( 'NONE', *, *, #164449, .F. ) ;
#148088 = PLANE ( 'NONE',  #75648 ) ;
#148089 = CARTESIAN_POINT ( 'NONE',  ( -5.899999999999938183, 64.35000000001120668, -22.02310748452479316 ) ) ;
#148090 = FACE_OUTER_BOUND ( 'NONE', #87574, .T. ) ;
#148091 = ORIENTED_EDGE ( 'NONE', *, *, #139706, .F. ) ;
#148092 = ADVANCED_FACE ( 'NONE', ( #200205 ), #223370, .F. ) ;
#148093 = AXIS2_PLACEMENT_3D ( 'NONE', #110581, #190135, #74061 ) ;
#148094 = CARTESIAN_POINT ( 'NONE',  ( -16.81453046979151367, 60.96603263716392007, -220.9850058241458726 ) ) ;
#148095 = EDGE_CURVE ( 'NONE', #62075, #202760, #202761, .T. ) ;
#148096 = AXIS2_PLACEMENT_3D ( 'NONE', #42696, #199216, #963 ) ;
#148097 = CYLINDRICAL_SURFACE ( 'NONE', #227589, 0.09999999999999810429 ) ;
#148098 = DIRECTION ( 'NONE',  ( -1.000000000000000000, -0.000000000000000000, -0.000000000000000000 ) ) ;
#148099 = ORIENTED_EDGE ( 'NONE', *, *, #146803, .F. ) ;
#148100 = ORIENTED_EDGE ( 'NONE', *, *, #17523, .F. ) ;
#148101 = CARTESIAN_POINT ( 'NONE',  ( -20.54999999999999716, 1.115600667400684642E-11, -188.1249999999999716 ) ) ;
#148102 = CARTESIAN_POINT ( 'NONE',  ( -18.59999999999999787, 10.33248238083634440, -173.0948465439131496 ) ) ;
#148103 = CIRCLE ( 'NONE', #193894, 0.09999999999998898659 ) ;
#148104 = DIRECTION ( 'NONE',  ( 1.000000000000000000, 0.000000000000000000, 0.000000000000000000 ) ) ;
#148106 = EDGE_CURVE ( 'NONE', #32893, #236679, #23691, .T. ) ;
#148105 = CARTESIAN_POINT ( 'NONE',  ( -20.94983749550516450, 10.29766095125288494, -206.4743663933275286 ) ) ;
#148107 = ORIENTED_EDGE ( 'NONE', *, *, #24991, .T. ) ;
#148108 = CARTESIAN_POINT ( 'NONE',  ( -20.85000000000000142, 77.16412189325258453, -28.10825939895270764 ) ) ;
#148109 = CARTESIAN_POINT ( 'NONE',  ( 21.05000000000005400, 67.73741572762334329, -25.54575917482290848 ) ) ;
#148111 = EDGE_CURVE ( 'NONE', #145447, #216520, #190073, .T. ) ;
#148110 = CARTESIAN_POINT ( 'NONE',  ( 20.94999999999999929, 5.000000000011153745, -54.59473398108690390 ) ) ;
#148112 = CARTESIAN_POINT ( 'NONE',  ( -23.25000000000000000, 85.68240343348880117, -163.3662641071115047 ) ) ;
#148113 = AXIS2_PLACEMENT_3D ( 'NONE', #243022, #203899, #64399 ) ;
#148114 = VERTEX_POINT ( 'NONE', #181922 ) ;
#148115 = CIRCLE ( 'NONE', #156529, 0.09999999999999939493 ) ;
#148116 = DIRECTION ( 'NONE',  ( 1.000000000000000000, 0.000000000000000000, 0.000000000000000000 ) ) ;
#148118 = ORIENTED_EDGE ( 'NONE', *, *, #3460, .F. ) ;
#148117 = CARTESIAN_POINT ( 'NONE',  ( -23.15000000000000213, -9.599999999988845900, -90.60603087734760663 ) ) ;
#148119 = CARTESIAN_POINT ( 'NONE',  ( -16.93589915522259304, 10.00862525870701170, -121.4405601019603438 ) ) ;
#148120 = DIRECTION ( 'NONE',  ( -0.7071067811865475727, 0.2890913453342130457, -0.6453109281988448354 ) ) ;
#148121 = CARTESIAN_POINT ( 'NONE',  ( -23.25000000000000000, 6.738188228664430568, -211.9673068433082790 ) ) ;
#148122 = EDGE_CURVE ( 'NONE', #114870, #47719, #161083, .T. ) ;
#148123 = DIRECTION ( 'NONE',  ( 1.000000000000000000, 0.000000000000000000, 0.000000000000000000 ) ) ;
#148124 = CARTESIAN_POINT ( 'NONE',  ( 23.24999999999999645, 5.600000000011153389, -121.5947339810869465 ) ) ;
#148125 = CARTESIAN_POINT ( 'NONE',  ( -21.05000000000000071, 77.16270174995034381, -162.1231074845243540 ) ) ;
#148126 = DIRECTION ( 'NONE',  ( -0.7071067811865302533, 0.6909108974501196876, 0.1504730267679053324 ) ) ;
#148127 = EDGE_LOOP ( 'NONE', ( #221070, #97283, #71244, #70008 ) ) ;
#148128 = DIRECTION ( 'NONE',  ( 2.557131231893036985E-16, -0.8660254037844383745, 0.5000000000000003331 ) ) ;
#148129 = DIRECTION ( 'NONE',  ( 0.000000000000000000, -1.000000000000000000, -5.551115123125777653E-14 ) ) ;
#148130 = DIRECTION ( 'NONE',  ( -1.000000000000000000, 0.000000000000000000, 0.000000000000000000 ) ) ;
#148131 = AXIS2_PLACEMENT_3D ( 'NONE', #113737, #14673, #159311 ) ;
#148132 = DIRECTION ( 'NONE',  ( -0.000000000000000000, 0.4721928772777345684, 0.8814952561688429444 ) ) ;
#148133 = EDGE_LOOP ( 'NONE', ( #171506, #121142 ) ) ;
#148134 = ORIENTED_EDGE ( 'NONE', *, *, #145117, .F. ) ;
#148135 = DIRECTION ( 'NONE',  ( 0.000000000000000000, 0.9126074666063660468, 0.4088369013363524762 ) ) ;
#148137 = CARTESIAN_POINT ( 'NONE',  ( -16.92507428761700439, 66.05000000001207638, -123.8097100249028131 ) ) ;
#148136 = VECTOR ( 'NONE', #144279, 1000.000000000000114 ) ;
#148138 = FACE_OUTER_BOUND ( 'NONE', #130848, .T. ) ;
#148139 = DIRECTION ( 'NONE',  ( 1.000000000000000000, 0.000000000000000000, 0.000000000000000000 ) ) ;
#148140 = DIRECTION ( 'NONE',  ( 1.000000000000000000, 0.000000000000000000, 0.000000000000000000 ) ) ;
#148141 = DIRECTION ( 'NONE',  ( -0.000000000000000000, -0.9770955615653313941, -0.2128009952263603677 ) ) ;
#148142 = DIRECTION ( 'NONE',  ( 0.000000000000000000, 0.8814952561688398358, -0.4721928772777406746 ) ) ;
#148143 = CIRCLE ( 'NONE', #52453, 0.1000000000000028644 ) ;
#148144 = AXIS2_PLACEMENT_3D ( 'NONE', #169981, #31744, #248191 ) ;
#148145 = EDGE_LOOP ( 'NONE', ( #14191, #20417, #32186, #158508 ) ) ;
#148146 = CARTESIAN_POINT ( 'NONE',  ( -20.54999999999999716, 45.00644278977874535, -237.9768835835062077 ) ) ;
#148147 = ORIENTED_EDGE ( 'NONE', *, *, #236614, .F. ) ;
#148148 = PLANE ( 'NONE',  #139269 ) ;
#148149 = SPHERICAL_SURFACE ( 'NONE', #245268, 0.1000000000000000056 ) ;
#148150 = CARTESIAN_POINT ( 'NONE',  ( 21.05000000000000071, 19.00443933019177223, -232.7770257915295531 ) ) ;
#148151 = CARTESIAN_POINT ( 'NONE',  ( -22.48970261584618058, 11.65000000000000036, 0.05536948821740890481 ) ) ;
#148152 = PLANE ( 'NONE',  #41347 ) ;
#148153 = CARTESIAN_POINT ( 'NONE',  ( -20.94999999999999929, 46.45388641681647357, -243.1520440498138385 ) ) ;
#148154 = EDGE_LOOP ( 'NONE', ( #37270, #24407, #5436, #160999 ) ) ;
#148155 = DIRECTION ( 'NONE',  ( -0.000000000000000000, -0.000000000000000000, -1.000000000000000000 ) ) ;
#148156 = CARTESIAN_POINT ( 'NONE',  ( -20.05000000000000426, 9.250000000011157297, -188.6499999999999488 ) ) ;
#148157 = EDGE_CURVE ( 'NONE', #243144, #50473, #221031, .T. ) ;
#148158 = DIRECTION ( 'NONE',  ( 1.000000000000000000, 0.000000000000000000, -0.000000000000000000 ) ) ;
#148159 = FACE_OUTER_BOUND ( 'NONE', #167317, .T. ) ;
#148160 = AXIS2_PLACEMENT_3D ( 'NONE', #225569, #122666, #46936 ) ;
#148161 = CIRCLE ( 'NONE', #27408, 0.1000000000000026007 ) ;
#148162 = CARTESIAN_POINT ( 'NONE',  ( -16.94107738177414291, 10.01423928514777373, -154.9500000000000455 ) ) ;
#148163 = AXIS2_PLACEMENT_3D ( 'NONE', #133998, #213529, #75349 ) ;
#148164 = ORIENTED_EDGE ( 'NONE', *, *, #57942, .T. ) ;
#148166 = CARTESIAN_POINT ( 'NONE',  ( -16.77683809663752257, 63.08573235307424198, -213.1276215869287967 ) ) ;
#148165 = STYLED_ITEM ( 'NONE', ( #120520 ), #119926 ) ;
#148167 = CARTESIAN_POINT ( 'NONE',  ( -18.50000000000000000, 68.97833521811233481, -166.3895420826271163 ) ) ;
#148168 = ORIENTED_EDGE ( 'NONE', *, *, #65801, .F. ) ;
#148169 = VERTEX_POINT ( 'NONE', #162373 ) ;
#148170 = CARTESIAN_POINT ( 'NONE',  ( -16.94445028196807002, 51.64060657411747712, -231.8906364537310196 ) ) ;
#148171 = DIRECTION ( 'NONE',  ( 0.000000000000000000, 0.9126074666063769270, 0.4088369013363280513 ) ) ;
#148172 = EDGE_CURVE ( 'NONE', #252099, #234093, #106855, .T. ) ;
#148173 = DIRECTION ( 'NONE',  ( 1.000000000000000000, 0.000000000000000000, 0.000000000000000000 ) ) ;
#148174 = VERTEX_POINT ( 'NONE', #121950 ) ;
#148175 = FACE_OUTER_BOUND ( 'NONE', #128818, .T. ) ;
#148176 = CARTESIAN_POINT ( 'NONE',  ( -20.94999999999999929, 1.115600667400684642E-11, -200.9999999999999432 ) ) ;
#148177 = ORIENTED_EDGE ( 'NONE', *, *, #250212, .F. ) ;
#148178 = CIRCLE ( 'NONE', #35785, 0.2000000000000057288 ) ;
#148179 = AXIS2_PLACEMENT_3D ( 'NONE', #169437, #109405, #248945 ) ;
#148180 = DIRECTION ( 'NONE',  ( -1.000000000000000000, 0.000000000000000000, 0.000000000000000000 ) ) ;
#148181 = EDGE_CURVE ( 'NONE', #198338, #170976, #144251, .T. ) ;
#148182 = ORIENTED_EDGE ( 'NONE', *, *, #34867, .F. ) ;
#148183 = EDGE_CURVE ( 'NONE', #90961, #22950, #31878, .T. ) ;
#148184 = VECTOR ( 'NONE', #198526, 1000.000000000000000 ) ;
#148185 = DIRECTION ( 'NONE',  ( 0.000000000000000000, 0.000000000000000000, -1.000000000000000000 ) ) ;
#148186 = LINE ( 'NONE', #25683, #150146 ) ;
#148188 = ORIENTED_EDGE ( 'NONE', *, *, #234756, .T. ) ;
#148187 = CARTESIAN_POINT ( 'NONE',  ( -21.45000000000000284, 63.02410583447655767, -221.9179669651492759 ) ) ;
#148189 = CARTESIAN_POINT ( 'NONE',  ( -20.94999999999999929, 1.115600667400684642E-11, -100.5000000000000426 ) ) ;
#148191 = CIRCLE ( 'NONE', #252234, 2.000000000000003109 ) ;
#148190 = CARTESIAN_POINT ( 'NONE',  ( 21.08078803292165659, 33.99748930211067943, -243.8039819374040178 ) ) ;
#148192 = EDGE_CURVE ( 'NONE', #18309, #4224, #173559, .T. ) ;
#148193 = DIRECTION ( 'NONE',  ( 0.000000000000000000, -0.9126074666063660468, -0.4088369013363524762 ) ) ;
#148194 = AXIS2_PLACEMENT_3D ( 'NONE', #21026, #134504, #234921 ) ;
#148195 = CARTESIAN_POINT ( 'NONE',  ( 21.14999999999999858, 8.786607556611267356, -179.7499999999999716 ) ) ;
#148196 = LINE ( 'NONE', #212042, #8540 ) ;
#148197 = DIRECTION ( 'NONE',  ( 0.000000000000000000, -1.000000000000000000, -6.982962677686265922E-15 ) ) ;
#148199 = VERTEX_POINT ( 'NONE', #87925 ) ;
#148198 = CARTESIAN_POINT ( 'NONE',  ( 22.39999999999999858, 7.790779598373383408, 0.09999999999999939493 ) ) ;
#148200 = ORIENTED_EDGE ( 'NONE', *, *, #236304, .F. ) ;
#148202 = DIRECTION ( 'NONE',  ( 1.000000000000000000, 0.000000000000000000, 0.000000000000000000 ) ) ;
#148201 = PLANE ( 'NONE',  #108094 ) ;
#148203 = EDGE_CURVE ( 'NONE', #188385, #125626, #166773, .T. ) ;
#148205 = ORIENTED_EDGE ( 'NONE', *, *, #19230, .F. ) ;
#148204 = CARTESIAN_POINT ( 'NONE',  ( -18.59999999999999787, 76.00000000001244871, -170.0231074845243597 ) ) ;
#148206 = ORIENTED_EDGE ( 'NONE', *, *, #244222, .T. ) ;
#148207 = DIRECTION ( 'NONE',  ( 0.000000000000000000, 0.000000000000000000, 1.000000000000000000 ) ) ;
#148208 = DIRECTION ( 'NONE',  ( 0.000000000000000000, -1.000000000000000000, 0.000000000000000000 ) ) ;
#148209 = AXIS2_PLACEMENT_3D ( 'NONE', #102725, #122323, #201854 ) ;
#148210 = EDGE_CURVE ( 'NONE', #124122, #115941, #123436, .T. ) ;
#148211 = CIRCLE ( 'NONE', #135736, 0.09999999999999990841 ) ;
#148212 = CARTESIAN_POINT ( 'NONE',  ( -20.64999999999999858, 49.53130139001177668, -254.0846532093228802 ) ) ;
#148213 = CARTESIAN_POINT ( 'NONE',  ( -21.44999999999999929, 68.65000000001157332, -57.27310748452437394 ) ) ;
#148214 = VECTOR ( 'NONE', #66388, 1000.000000000000000 ) ;
#148215 = CARTESIAN_POINT ( 'NONE',  ( 18.39999999999999858, -9.499999999988842703, -207.6001893912220169 ) ) ;
#148216 = CIRCLE ( 'NONE', #85636, 6.329289321881352848 ) ;
#148217 = DIRECTION ( 'NONE',  ( 0.000000000000000000, -6.982962677686266711E-15, 1.000000000000000000 ) ) ;
#148218 = EDGE_CURVE ( 'NONE', #33201, #45900, #240149, .T. ) ;
#148219 = CARTESIAN_POINT ( 'NONE',  ( -23.15000000000000213, 40.35498466150055918, -247.8953732508333587 ) ) ;
#148220 = ORIENTED_EDGE ( 'NONE', *, *, #109759, .T. ) ;
#148222 = VERTEX_POINT ( 'NONE', #125784 ) ;
#148221 = B_SPLINE_CURVE_WITH_KNOTS ( 'NONE', 3,
 ( #135282, #64744, #240827, #139112, #222514, #218671, #84252, #124731, #144257, #81702 ),
 .UNSPECIFIED., .F., .F.,
 ( 4, 2, 2, 2, 4 ),
 ( 0.000000000000000000, 0.0003916577441626793482, 0.0005874866162440234947, 0.0006854010522846912040, 0.0007833154883253590217 ),
 .UNSPECIFIED. ) ;
#148223 = DIRECTION ( 'NONE',  ( -0.000000000000000000, -0.2617529984165031243, -0.9651348961777157509 ) ) ;
#148224 = ORIENTED_EDGE ( 'NONE', *, *, #171915, .T. ) ;
#148225 = CARTESIAN_POINT ( 'NONE',  ( 23.14999999999999503, 6.450000000000001066, 11.75000000000000000 ) ) ;
#148226 = ORIENTED_EDGE ( 'NONE', *, *, #183954, .T. ) ;
#148227 = DIRECTION ( 'NONE',  ( 0.000000000000000000, -0.9998779222360097974, 0.01562500000000363945 ) ) ;
#148228 = DIRECTION ( 'NONE',  ( 1.000000000000000000, 0.000000000000000000, 0.000000000000000000 ) ) ;
#148229 = DIRECTION ( 'NONE',  ( 0.000000000000000000, -1.000000000000000000, 0.000000000000000000 ) ) ;
#148230 = DIRECTION ( 'NONE',  ( -1.000000000000000000, -0.000000000000000000, -0.000000000000000000 ) ) ;
#148231 = EDGE_LOOP ( 'NONE', ( #249271, #43967, #94522, #130639, #147455 ) ) ;
#148232 = CARTESIAN_POINT ( 'NONE',  ( -20.94999999999999929, 11.59999999999999787, -6.928203230275557623 ) ) ;
#148233 = ORIENTED_EDGE ( 'NONE', *, *, #134145, .T. ) ;
#148234 = AXIS2_PLACEMENT_3D ( 'NONE', #89856, #208553, #188973 ) ;
#148235 = LINE ( 'NONE', #206932, #21767 ) ;
#148236 = DIRECTION ( 'NONE',  ( 1.000000000000000000, 0.000000000000000000, 0.000000000000000000 ) ) ;
#148237 = AXIS2_PLACEMENT_3D ( 'NONE', #151821, #192223, #147946 ) ;
#148238 = CARTESIAN_POINT ( 'NONE',  ( 18.46947024752518018, 8.797344559918837348, -245.4141666393988714 ) ) ;
#148239 = AXIS2_PLACEMENT_3D ( 'NONE', #20731, #100217, #3706 ) ;
#148240 = VECTOR ( 'NONE', #21581, 1000.000000000000000 ) ;
#148241 = EDGE_LOOP ( 'NONE', ( #116510, #111711, #58941, #198355 ) ) ;
#148242 = DIRECTION ( 'NONE',  ( -1.000000000000000000, 2.952720810173289112E-16, 2.061873921506763405E-30 ) ) ;
#148243 = ORIENTED_EDGE ( 'NONE', *, *, #243572, .T. ) ;
#148246 = ORIENTED_EDGE ( 'NONE', *, *, #143159, .T. ) ;
#148245 = CARTESIAN_POINT ( 'NONE',  ( 23.25000000000000000, -8.596261682231828516, -124.5498724828497501 ) ) ;
#148244 = FACE_OUTER_BOUND ( 'NONE', #209030, .T. ) ;
#148247 = DIRECTION ( 'NONE',  ( 1.000000000000000000, 0.000000000000000000, 0.000000000000000000 ) ) ;
#148248 = ORIENTED_EDGE ( 'NONE', *, *, #36860, .F. ) ;
#148249 = AXIS2_PLACEMENT_3D ( 'NONE', #157625, #58453, #137997 ) ;
#148250 = ADVANCED_FACE ( 'NONE', ( #248312 ), #143035, .T. ) ;
#148251 = DIRECTION ( 'NONE',  ( -1.000000000000000000, -0.000000000000000000, 0.000000000000000000 ) ) ;
#148252 = ORIENTED_EDGE ( 'NONE', *, *, #115673, .T. ) ;
#148253 = ADVANCED_FACE ( 'NONE', ( #207924 ), #29304, .F. ) ;
#148254 = FACE_OUTER_BOUND ( 'NONE', #25694, .T. ) ;
#148255 = EDGE_CURVE ( 'NONE', #182409, #245093, #235846, .T. ) ;
#148256 = CARTESIAN_POINT ( 'NONE',  ( 20.85000000000000142, -11.64999999998883595, -131.1000000000000227 ) ) ;
#148258 = ADVANCED_FACE ( 'NONE', ( #110076 ), #187075, .T. ) ;
#148257 = CIRCLE ( 'NONE', #35855, 0.2000000000000057288 ) ;
#148259 = DIRECTION ( 'NONE',  ( 0.000000000000000000, 0.1568667991644355497, 0.9876197685951332295 ) ) ;
#148260 = FACE_OUTER_BOUND ( 'NONE', #64205, .T. ) ;
#148261 = AXIS2_PLACEMENT_3D ( 'NONE', #29176, #65685, #86501 ) ;
#148263 = EDGE_LOOP ( 'NONE', ( #122597, #252536, #68136, #212785 ) ) ;
#148262 = EDGE_CURVE ( 'NONE', #139316, #55604, #152692, .T. ) ;
#148264 = CARTESIAN_POINT ( 'NONE',  ( -16.90987985657661952, 9.957807518190888274, -188.3692870888836239 ) ) ;
#148265 = CARTESIAN_POINT ( 'NONE',  ( 21.08078803292165659, 6.333012964448271553, -33.42081401284222153 ) ) ;
#148267 = EDGE_CURVE ( 'NONE', #47237, #9696, #36148, .T. ) ;
#148266 = B_SPLINE_CURVE_WITH_KNOTS ( 'NONE', 3,
 ( #112004, #27363, #228097, #91138, #10337, #28657 ),
 .UNSPECIFIED., .F., .F.,
 ( 4, 2, 4 ),
 ( 0.000000000000000000, 0.0001891491689349594741, 0.0003782983378699189482 ),
 .UNSPECIFIED. ) ;
#148268 = ORIENTED_EDGE ( 'NONE', *, *, #125284, .T. ) ;
#148269 = DIRECTION ( 'NONE',  ( 0.000000000000000000, 0.2128009952263605342, -0.9770955615653315052 ) ) ;
#148272 = EDGE_CURVE ( 'NONE', #234821, #81658, #166240, .T. ) ;
#148271 = EDGE_CURVE ( 'NONE', #154055, #39978, #51354, .T. ) ;
#148270 = ORIENTED_EDGE ( 'NONE', *, *, #130095, .T. ) ;
#148273 = CARTESIAN_POINT ( 'NONE',  ( 23.04999999999999716, 67.17743825834546101, -90.37310748452436826 ) ) ;
#148274 = VERTEX_POINT ( 'NONE', #73560 ) ;
#148275 = CARTESIAN_POINT ( 'NONE',  ( 23.15000000000000213, -11.39257802169451139, -63.92605042016806749 ) ) ;
#148276 = CARTESIAN_POINT ( 'NONE',  ( 21.05000000000000071, 76.00000000001170974, -69.52310748452431710 ) ) ;
#148277 = EDGE_CURVE ( 'NONE', #188373, #113738, #181877, .T. ) ;
#148278 = CIRCLE ( 'NONE', #239873, 0.09999999999999543976 ) ;
#148280 = EDGE_LOOP ( 'NONE', ( #20032, #123691, #138310, #188227 ) ) ;
#148279 = DIRECTION ( 'NONE',  ( 1.000000000000000000, 0.000000000000000000, 0.000000000000000000 ) ) ;
#148281 = CARTESIAN_POINT ( 'NONE',  ( -17.11825945287481332, 66.05000000001255955, -182.7731074845244450 ) ) ;
#148282 = CARTESIAN_POINT ( 'NONE',  ( -13.77083647240106146, 62.94600569631032982, -215.5247064183336363 ) ) ;
#148283 = EDGE_CURVE ( 'NONE', #237528, #199335, #254680, .T. ) ;
#148284 = CARTESIAN_POINT ( 'NONE',  ( 23.24999999999999289, 11.75000000001116263, -146.1500000000000341 ) ) ;
#148285 = ORIENTED_EDGE ( 'NONE', *, *, #2026, .F. ) ;
#148286 = CARTESIAN_POINT ( 'NONE',  ( 21.07016717456945187, 69.67905916191242000, -203.5231074845244450 ) ) ;
#148287 = DIRECTION ( 'NONE',  ( -1.000000000000000000, -3.190570557967288949E-16, -6.948722487160392945E-17 ) ) ;
#148289 = ORIENTED_EDGE ( 'NONE', *, *, #237862, .F. ) ;
#148288 = EDGE_CURVE ( 'NONE', #153900, #211628, #198440, .T. ) ;
#148291 = EDGE_CURVE ( 'NONE', #36945, #47998, #72253, .T. ) ;
#148290 = LINE ( 'NONE', #129987, #69889 ) ;
#148292 = CIRCLE ( 'NONE', #52412, 7.900000000000003908 ) ;
#148293 = AXIS2_PLACEMENT_3D ( 'NONE', #217300, #16574, #58229 ) ;
#148294 = AXIS2_PLACEMENT_3D ( 'NONE', #114848, #216512, #73189 ) ;
#148295 = AXIS2_PLACEMENT_3D ( 'NONE', #110836, #151269, #52132 ) ;
#148296 = EDGE_LOOP ( 'NONE', ( #244950, #37819, #112101, #239992 ) ) ;
#148297 = EDGE_CURVE ( 'NONE', #236905, #167762, #127730, .T. ) ;
#148298 = CARTESIAN_POINT ( 'NONE',  ( -16.87372386987899375, 44.61949230436924552, -235.1581464042268408 ) ) ;
#148299 = CARTESIAN_POINT ( 'NONE',  ( -20.64999999999999858, 54.70975502726918194, -239.2730902609777104 ) ) ;
#148300 = EDGE_CURVE ( 'NONE', #97885, #239248, #2792, .T. ) ;
#148301 = EDGE_CURVE ( 'NONE', #94706, #3474, #15303, .T. ) ;
#148304 = EDGE_LOOP ( 'NONE', ( #125689, #125499, #154506, #99715 ) ) ;
#148303 = ORIENTED_EDGE ( 'NONE', *, *, #250682, .F. ) ;
#148302 = CARTESIAN_POINT ( 'NONE',  ( -12.25000000000000178, 9.350000000011139178, -184.2499999999999716 ) ) ;
#148305 = CARTESIAN_POINT ( 'NONE',  ( -20.85000000000000142, -1.164121893241208960, -41.31484808557160449 ) ) ;
#148306 = CYLINDRICAL_SURFACE ( 'NONE', #131458, 0.1000000000000028644 ) ;
#148307 = FACE_OUTER_BOUND ( 'NONE', #91442, .T. ) ;
#148309 = CARTESIAN_POINT ( 'NONE',  ( -15.69373346032659100, 66.64320997496565724, -52.31828097591049698 ) ) ;
#148308 = LINE ( 'NONE', #109159, #10811 ) ;
#148310 = CYLINDRICAL_SURFACE ( 'NONE', #119583, 0.09999999999999939493 ) ;
#148311 = DIRECTION ( 'NONE',  ( 0.000000000000000000, -0.4999999999999608646, -0.8660254037844612451 ) ) ;
#148312 = CIRCLE ( 'NONE', #35908, 0.09999999999999993616 ) ;
#148313 = DIRECTION ( 'NONE',  ( 1.000000000000000000, -1.186688945009009831E-16, -8.286604613020806758E-31 ) ) ;
#148314 = CARTESIAN_POINT ( 'NONE',  ( -22.48970261584618058, 11.65000000001115588, -33.44463051178259150 ) ) ;
#148315 = ORIENTED_EDGE ( 'NONE', *, *, #247298, .T. ) ;
#148316 = VERTEX_POINT ( 'NONE', #232626 ) ;
#148317 = AXIS2_PLACEMENT_3D ( 'NONE', #9634, #104844, #107451 ) ;
#148319 = ORIENTED_EDGE ( 'NONE', *, *, #15201, .T. ) ;
#148318 = DIRECTION ( 'NONE',  ( 0.000000000000000000, -0.9667078373770149335, -0.2558827019434000150 ) ) ;
#148320 = ORIENTED_EDGE ( 'NONE', *, *, #246276, .T. ) ;
#148321 = CARTESIAN_POINT ( 'NONE',  ( -21.05000000000000071, 79.10508929521364507, -235.9670348125907537 ) ) ;
#148322 = ORIENTED_EDGE ( 'NONE', *, *, #45596, .T. ) ;
#148323 = CARTESIAN_POINT ( 'NONE',  ( -18.59999999999999787, 11.64999999999999680, -7.014805770653998351 ) ) ;
#148324 = EDGE_LOOP ( 'NONE', ( #70434, #132203, #198806, #238488, #182954 ) ) ;
#148325 = CARTESIAN_POINT ( 'NONE',  ( -21.52071067811865746, 7.779289321892505882, -112.8500000000000369 ) ) ;
#148326 = CYLINDRICAL_SURFACE ( 'NONE', #186424, 0.1000000000000055844 ) ;
#148329 = ORIENTED_EDGE ( 'NONE', *, *, #28283, .T. ) ;
#148328 = ORIENTED_EDGE ( 'NONE', *, *, #198319, .T. ) ;
#148327 = AXIS2_PLACEMENT_3D ( 'NONE', #71702, #92515, #172108 ) ;
#148330 = ORIENTED_EDGE ( 'NONE', *, *, #247831, .T. ) ;
#148331 = CARTESIAN_POINT ( 'NONE',  ( 21.06490991615909536, 10.72489134759826790, -45.70371135353313008 ) ) ;
#148332 = ORIENTED_EDGE ( 'NONE', *, *, #197164, .T. ) ;
#148333 = ORIENTED_EDGE ( 'NONE', *, *, #43516, .F. ) ;
#148334 = DIRECTION ( 'NONE',  ( 0.000000000000000000, -0.4930308989875248349, -0.8700118002898312719 ) ) ;
#148335 = DIRECTION ( 'NONE',  ( 0.000000000000000000, 6.982962677686266711E-15, -1.000000000000000000 ) ) ;
#148336 = CARTESIAN_POINT ( 'NONE',  ( 21.05000000000000071, 8.776282895303632259, -75.48800072158441310 ) ) ;
#148338 = ORIENTED_EDGE ( 'NONE', *, *, #215419, .F. ) ;
#148337 = DIRECTION ( 'NONE',  ( 0.000000000000000000, -0.8660254037844247188, 0.5000000000000245359 ) ) ;
#148339 = LINE ( 'NONE', #97308, #103473 ) ;
#148340 = DIRECTION ( 'NONE',  ( 0.000000000000000000, 1.000000000000000000, 1.265107689135680095E-16 ) ) ;
#148342 = ORIENTED_EDGE ( 'NONE', *, *, #58039, .F. ) ;
#148341 = CARTESIAN_POINT ( 'NONE',  ( -20.54999999999999716, 67.23127455305835554, -235.8551265064784559 ) ) ;
#148343 = LINE ( 'NONE', #32274, #213573 ) ;
#148344 = ORIENTED_EDGE ( 'NONE', *, *, #2888, .F. ) ;
#148345 = DIRECTION ( 'NONE',  ( -1.000000000000000000, -0.000000000000000000, -0.000000000000000000 ) ) ;
#148346 = VERTEX_POINT ( 'NONE', #111369 ) ;
#148347 = CARTESIAN_POINT ( 'NONE',  ( 22.37643362114956247, 68.37421000605401389, -170.1221888582057886 ) ) ;
#148349 = EDGE_CURVE ( 'NONE', #47116, #167911, #157550, .T. ) ;
#148348 = FACE_OUTER_BOUND ( 'NONE', #142024, .T. ) ;
#148350 = AXIS2_PLACEMENT_3D ( 'NONE', #26275, #86207, #67955 ) ;
#148351 = ORIENTED_EDGE ( 'NONE', *, *, #246424, .F. ) ;
#148353 = CARTESIAN_POINT ( 'NONE',  ( -18.49513951962167724, -9.437725026666550221, -140.7780725750292277 ) ) ;
#148352 = LINE ( 'NONE', #173100, #186333 ) ;
#148354 = ADVANCED_FACE ( 'NONE', ( #236444 ), #252596, .T. ) ;
#148355 = CARTESIAN_POINT ( 'NONE',  ( -20.85000000000000142, -1.835859311432479268, -179.0044391687985410 ) ) ;
#148356 = AXIS2_PLACEMENT_3D ( 'NONE', #162268, #240500, #99673 ) ;
#148357 = AXIS2_PLACEMENT_3D ( 'NONE', #132601, #49200, #67477 ) ;
#148358 = FACE_OUTER_BOUND ( 'NONE', #129047, .T. ) ;
#148359 = FACE_BOUND ( 'NONE', #146538, .T. ) ;
#148360 = ORIENTED_EDGE ( 'NONE', *, *, #109150, .F. ) ;
#148361 = ORIENTED_EDGE ( 'NONE', *, *, #22648, .F. ) ;
#148362 = EDGE_CURVE ( 'NONE', #221833, #94457, #165129, .T. ) ;
#148363 = DIRECTION ( 'NONE',  ( 1.000000000000000000, 0.000000000000000000, 0.000000000000000000 ) ) ;
#148365 = EDGE_CURVE ( 'NONE', #229799, #171759, #250864, .T. ) ;
#148364 = LINE ( 'NONE', #11434, #6779 ) ;
#148366 = ORIENTED_EDGE ( 'NONE', *, *, #95333, .F. ) ;
#148367 = PLANE ( 'NONE',  #26935 ) ;
#148368 = EDGE_LOOP ( 'NONE', ( #123401, #224478, #65262, #1457 ) ) ;
#148369 = CARTESIAN_POINT ( 'NONE',  ( -20.94999999999999929, 74.75000000001207923, -128.5231074845243029 ) ) ;
#148370 = ORIENTED_EDGE ( 'NONE', *, *, #53986, .F. ) ;
#148371 = DIRECTION ( 'NONE',  ( 2.952720810173290591E-16, -0.4721928772777342354, -0.8814952561688433885 ) ) ;
#148372 = CARTESIAN_POINT ( 'NONE',  ( 18.49999999999999289, 55.04793976901536467, -229.8170162380219494 ) ) ;
#148373 = CARTESIAN_POINT ( 'NONE',  ( 23.15000000000000213, -11.48912529306489994, -97.50000000000004263 ) ) ;
#148374 = ORIENTED_EDGE ( 'NONE', *, *, #27564, .F. ) ;
#148375 = CYLINDRICAL_SURFACE ( 'NONE', #248435, 0.09999999999999935330 ) ;
#148376 =( LENGTH_UNIT ( ) NAMED_UNIT ( * ) SI_UNIT ( .MILLI., .METRE. ) );
#148377 = AXIS2_PLACEMENT_3D ( 'NONE', #224745, #201345, #103512 ) ;
#148378 = EDGE_CURVE ( 'NONE', #164610, #116921, #96899, .T. ) ;
#148379 = EDGE_LOOP ( 'NONE', ( #71202, #255047, #178819, #192143 ) ) ;
#148380 = ORIENTED_EDGE ( 'NONE', *, *, #140659, .F. ) ;
#148382 = EDGE_CURVE ( 'NONE', #240443, #205367, #211762, .T. ) ;
#148381 = VECTOR ( 'NONE', #118092, 1000.000000000000000 ) ;
#148383 = VERTEX_POINT ( 'NONE', #112658 ) ;
#148384 = CARTESIAN_POINT ( 'NONE',  ( -20.54999999999999716, 49.02191564284679970, -236.1780012176263881 ) ) ;
#148385 = DIRECTION ( 'NONE',  ( -0.000000000000000000, -0.2128009952263603677, 0.9770955615653313941 ) ) ;
#148386 = CARTESIAN_POINT ( 'NONE',  ( -21.08884785362073089, 0.04978309507788075683, -127.6428066325744055 ) ) ;
#148387 = DIRECTION ( 'NONE',  ( -1.000000000000000000, -0.000000000000000000, -0.000000000000000000 ) ) ;
#148388 = VECTOR ( 'NONE', #66418, 1000.000000000000000 ) ;
#148389 = FACE_OUTER_BOUND ( 'NONE', #164551, .T. ) ;
#148390 =( BOUNDED_SURFACE ( )  B_SPLINE_SURFACE ( 3, 2, ( 
 ( #203955, #4465, #202670 ),
 ( #185688, #227373, #164846 ),
 ( #48730, #128288, #108717 ),
 ( #3171, #24064, #103553 ),
 ( #7039, #82691, #125704 ),
 ( #183128, #162285, #205225 ) ),
 .UNSPECIFIED., .F., .F., .F. ) 
 B_SPLINE_SURFACE_WITH_KNOTS ( ( 4, 2, 4 ),
 ( 3, 3 ),
 ( 0.0001342700090130058096, 0.0002909192928057405345, 0.0004475685765984752595 ),
 ( 0.000000000000000000, 1.000000000000000000 ),
 .UNSPECIFIED. ) 
 GEOMETRIC_REPRESENTATION_ITEM ( )  RATIONAL_B_SPLINE_SURFACE ( (
 ( 1.000000000000000000, 0.7250110520819763593, 1.000000000000000000),
 ( 1.000000000000000000, 0.7257599279143153170, 1.000000000000000000),
 ( 1.000000000000000000, 0.7137594617271856290, 1.000000000000000000),
 ( 1.000000000000000000, 0.6959270178822787312, 1.000000000000000000),
 ( 1.000000000000000000, 0.6919879549328636914, 1.000000000000000000),
 ( 1.000000000000000000, 0.7071067811866138531, 1.000000000000000000) ) ) 
 REPRESENTATION_ITEM ( '' )  SURFACE ( )  );
#148392 = CARTESIAN_POINT ( 'NONE',  ( 21.05095171578076574, 8.776179878771037224, -12.16587327663788187 ) ) ;
#148391 = CARTESIAN_POINT ( 'NONE',  ( 22.47110162079221141, -3.126931989555618241, -228.2062997596194975 ) ) ;
#148394 = EDGE_LOOP ( 'NONE', ( #195808, #120407, #37699, #59270 ) ) ;
#148393 = DIRECTION ( 'NONE',  ( 0.000000000000000000, -0.000000000000000000, 1.000000000000000000 ) ) ;
#148395 = CARTESIAN_POINT ( 'NONE',  ( -23.25000000000000355, 5.649999999999983480, -12.65000000000000213 ) ) ;
#148396 = VERTEX_POINT ( 'NONE', #154388 ) ;
#148397 = CIRCLE ( 'NONE', #160871, 11.90000000000000213 ) ;
#148398 = DIRECTION ( 'NONE',  ( -1.000000000000000000, 0.000000000000000000, 0.000000000000000000 ) ) ;
#148399 = AXIS2_PLACEMENT_3D ( 'NONE', #32595, #9144, #209923 ) ;
#148400 = ORIENTED_EDGE ( 'NONE', *, *, #235663, .T. ) ;
#148401 = ORIENTED_EDGE ( 'NONE', *, *, #217591, .T. ) ;
#148402 = DIRECTION ( 'NONE',  ( 0.000000000000000000, 0.000000000000000000, -1.000000000000000000 ) ) ;
#148403 = DIRECTION ( 'NONE',  ( 0.000000000000000000, -0.9126074666063660468, -0.4088369013363524762 ) ) ;
#148404 = CARTESIAN_POINT ( 'NONE',  ( 23.24999999999999289, 64.25000000001156764, -57.37310748452440379 ) ) ;
#148405 = EDGE_CURVE ( 'NONE', #181843, #240894, #148572, .T. ) ;
#148406 = DIRECTION ( 'NONE',  ( -1.000000000000000000, 0.000000000000000000, 0.000000000000000000 ) ) ;
#148407 = ADVANCED_FACE ( 'NONE', ( #93078 ), #8277, .T. ) ;
#148408 = CIRCLE ( 'NONE', #202554, 0.1000000000000024342 ) ;
#148409 = CYLINDRICAL_SURFACE ( 'NONE', #167537, 0.09999999999999976963 ) ;
#148410 = VERTEX_POINT ( 'NONE', #64235 ) ;
#148411 = ORIENTED_EDGE ( 'NONE', *, *, #129883, .T. ) ;
#148413 =( BOUNDED_SURFACE ( )  B_SPLINE_SURFACE ( 3, 2, ( 
 ( #151241, #53407, #250322 ),
 ( #170844, #112121, #71708 ),
 ( #230781, #175951, #135490 ),
 ( #156394, #32604, #16863 ),
 ( #251607, #54684, #13025 ),
 ( #191669, #52104, #152544 ),
 ( #92520, #18132, #173410 ),
 ( #252882, #37721, #172117 ),
 ( #131659, #73007, #74289 ),
 ( #55948, #136782, #215048 ) ),
 .UNSPECIFIED., .F., .F., .F. ) 
 B_SPLINE_SURFACE_WITH_KNOTS ( ( 4, 2, 2, 2, 4 ),
 ( 3, 3 ),
 ( 0.0001701955120502373817, 0.0002247052511886135672, 0.0002792149903269897527, 0.0003882344686037421779, 0.0006062734251572470283 ),
 ( 0.000000000000000000, 1.000000000000000000 ),
 .UNSPECIFIED. ) 
 GEOMETRIC_REPRESENTATION_ITEM ( )  RATIONAL_B_SPLINE_SURFACE ( (
 ( 1.000000000000000000, 0.2966190024560231286, 1.000000000000000000),
 ( 1.000000000000000000, 0.2964522492704981804, 1.000000000000000000),
 ( 1.000000000000000000, 0.3059923531895626936, 1.000000000000000000),
 ( 1.000000000000000000, 0.3355751146933140805, 1.000000000000000000),
 ( 1.000000000000000000, 0.3550672384963000638, 1.000000000000000000),
 ( 1.000000000000000000, 0.4157034672182242652, 1.000000000000000000),
 ( 1.000000000000000000, 0.4588031877651267965, 1.000000000000000000),
 ( 1.000000000000000000, 0.5771441759666575688, 1.000000000000000000),
 ( 1.000000000000000000, 0.6469377121768220551, 1.000000000000000000),
 ( 1.000000000000000000, 0.7071067811865475727, 1.000000000000000000) ) ) 
 REPRESENTATION_ITEM ( '' )  SURFACE ( )  );
#148412 = AXIS2_PLACEMENT_3D ( 'NONE', #247234, #210689, #72481 ) ;
#148414 = DIRECTION ( 'NONE',  ( 0.000000000000000000, -0.000000000000000000, -1.000000000000000000 ) ) ;
#148415 = ORIENTED_EDGE ( 'NONE', *, *, #25635, .T. ) ;
#148416 = CARTESIAN_POINT ( 'NONE',  ( -21.30740335185486245, 0.09893452578700702438, -127.4433420779720336 ) ) ;
#148417 = CARTESIAN_POINT ( 'NONE',  ( 22.39999999999999503, 0.000000000000000000, 7.790779598373379855 ) ) ;
#148418 = VERTEX_POINT ( 'NONE', #59060 ) ;
#148419 = CARTESIAN_POINT ( 'NONE',  ( -18.50000000000000000, -1.164121893241208960, -41.41484808557160591 ) ) ;
#148420 = CARTESIAN_POINT ( 'NONE',  ( 18.59999999999999432, 1.637172712970381694, -11.58215336547201879 ) ) ;
#148421 = VECTOR ( 'NONE', #201522, 999.9999999999998863 ) ;
#148422 = DIRECTION ( 'NONE',  ( 0.000000000000000000, 1.000000000000000000, 0.000000000000000000 ) ) ;
#148424 = EDGE_CURVE ( 'NONE', #112510, #46212, #231776, .T. ) ;
#148423 = CARTESIAN_POINT ( 'NONE',  ( 21.72449340488909897, 10.28395627750227703, -188.3499999999999659 ) ) ;
#148425 = ORIENTED_EDGE ( 'NONE', *, *, #7318, .T. ) ;
#148426 = CYLINDRICAL_SURFACE ( 'NONE', #241789, 3.999999999999996447 ) ;
#148427 = DIRECTION ( 'NONE',  ( 0.000000000000000000, -0.1618390714546045217, -0.9868171638914230437 ) ) ;
#148428 = CARTESIAN_POINT ( 'NONE',  ( -20.85000000000000142, 67.85125148167622910, -227.9794913823769491 ) ) ;
#148429 = EDGE_CURVE ( 'NONE', #142529, #93777, #169264, .T. ) ;
#148430 = CYLINDRICAL_SURFACE ( 'NONE', #29443, 0.09999999999999939493 ) ;
#148431 = DIRECTION ( 'NONE',  ( 0.000000000000000000, 0.000000000000000000, -1.000000000000000000 ) ) ;
#148432 = AXIS2_PLACEMENT_3D ( 'NONE', #25497, #127154, #164995 ) ;
#148433 = EDGE_CURVE ( 'NONE', #107953, #58399, #79906, .T. ) ;
#148434 = DIRECTION ( 'NONE',  ( -0.000000000000000000, 0.9770955615653316162, 0.2128009952263604232 ) ) ;
#148435 = ORIENTED_EDGE ( 'NONE', *, *, #17466, .T. ) ;
#148436 = CARTESIAN_POINT ( 'NONE',  ( 21.04999999999999716, 10.62872031400434913, -12.15000000000000036 ) ) ;
#148437 = EDGE_LOOP ( 'NONE', ( #102060, #24458, #189778, #167463 ) ) ;
#148438 = EDGE_CURVE ( 'NONE', #175441, #150487, #56748, .T. ) ;
#148439 = LINE ( 'NONE', #127582, #33545 ) ;
#148441 = AXIS2_PLACEMENT_3D ( 'NONE', #213336, #235468, #198918 ) ;
#148440 = FACE_OUTER_BOUND ( 'NONE', #182084, .T. ) ;
#148442 = CARTESIAN_POINT ( 'NONE',  ( -21.44999999999999929, 7.250000000011155521, -179.8499999999999943 ) ) ;
#148443 = LINE ( 'NONE', #91024, #223522 ) ;
#148445 = ORIENTED_EDGE ( 'NONE', *, *, #165318, .F. ) ;
#148444 = AXIS2_PLACEMENT_3D ( 'NONE', #205654, #161433, #85682 ) ;
#148446 = CARTESIAN_POINT ( 'NONE',  ( 21.05000000000000071, 76.00000000001195133, -103.0231074845243171 ) ) ;
#148447 = ADVANCED_FACE ( 'NONE', ( #119081 ), #121662, .F. ) ;
#148448 = DIRECTION ( 'NONE',  ( 1.000000000000000000, -0.000000000000000000, -0.000000000000000000 ) ) ;
#148449 = VECTOR ( 'NONE', #172481, 1000.000000000000000 ) ;
#148450 = VECTOR ( 'NONE', #146331, 1000.000000000000000 ) ;
#148451 = DIRECTION ( 'NONE',  ( 1.000000000000000000, -0.000000000000000000, 0.000000000000000000 ) ) ;
#148452 = DIRECTION ( 'NONE',  ( 1.000000000000000000, 0.000000000000000000, 0.000000000000000000 ) ) ;
#148453 = DIRECTION ( 'NONE',  ( 1.000000000000000000, 0.000000000000000000, 0.000000000000000000 ) ) ;
#148454 = VECTOR ( 'NONE', #168566, 1000.000000000000000 ) ;
#148455 = ORIENTED_EDGE ( 'NONE', *, *, #93623, .F. ) ;
#148456 = VERTEX_POINT ( 'NONE', #242870 ) ;
#148457 = CARTESIAN_POINT ( 'NONE',  ( 18.49999999999999289, 64.35000000001251408, -178.6731074845244507 ) ) ;
#148458 = CARTESIAN_POINT ( 'NONE',  ( 22.50046968638161005, 0.04516984715173957138, -122.2499548455251812 ) ) ;
#148459 = CARTESIAN_POINT ( 'NONE',  ( 18.49999999999999289, 10.49142135624846439, -91.85000000000003695 ) ) ;
#148460 = DIRECTION ( 'NONE',  ( 0.000000000000000000, 0.2617529984165031243, 0.9651348961777157509 ) ) ;
#148461 = CIRCLE ( 'NONE', #106736, 0.09999999999998802902 ) ;
#148462 = ORIENTED_EDGE ( 'NONE', *, *, #58773, .F. ) ;
#148463 = DIRECTION ( 'NONE',  ( 0.7071067811865487940, 8.659560562354918067E-17, 0.7071067811865463515 ) ) ;
#148464 = CIRCLE ( 'NONE', #152768, 0.1000000000000028644 ) ;
#148465 = DIRECTION ( 'NONE',  ( 1.000000000000000000, 0.000000000000000000, 0.000000000000000000 ) ) ;
#148466 = EDGE_LOOP ( 'NONE', ( #149853, #146541, #92181, #243869 ) ) ;
#148467 = FACE_OUTER_BOUND ( 'NONE', #115741, .T. ) ;
#148468 = EDGE_LOOP ( 'NONE', ( #116212, #256978, #102696, #45847 ) ) ;
#148469 = VERTEX_POINT ( 'NONE', #159499 ) ;
#148470 = CIRCLE ( 'NONE', #202624, 11.80000000000000426 ) ;
#148471 = ORIENTED_EDGE ( 'NONE', *, *, #96738, .F. ) ;
#148472 = CARTESIAN_POINT ( 'NONE',  ( -20.64999999999999858, -8.999999999988846255, -76.89396912265249284 ) ) ;
#148473 = DIRECTION ( 'NONE',  ( -0.000000000000000000, 0.000000000000000000, 1.000000000000000000 ) ) ;
#148474 = FACE_OUTER_BOUND ( 'NONE', #60417, .T. ) ;
#148475 = CARTESIAN_POINT ( 'NONE',  ( -23.25000000000000000, 68.66552716081216090, -214.3300732090495444 ) ) ;
#148476 = CARTESIAN_POINT ( 'NONE',  ( 18.39999999999999503, 16.37079970714666999, -222.2530670965321065 ) ) ;
#148477 = CARTESIAN_POINT ( 'NONE',  ( -16.94309007106719989, 9.992226192569980014, -12.60579128255550607 ) ) ;
#148479 = CARTESIAN_POINT ( 'NONE',  ( -23.25000000000000000, 42.94477010600543565, -254.3363632230312703 ) ) ;
#148478 = CARTESIAN_POINT ( 'NONE',  ( 20.95576188350343116, 65.39101945504849311, -95.41187376177008161 ) ) ;
#148480 = DIRECTION ( 'NONE',  ( 1.000000000000000000, 0.000000000000000000, 0.000000000000000000 ) ) ;
#148481 = CARTESIAN_POINT ( 'NONE',  ( 20.94999999999999929, 1.115600667400684642E-11, -167.5000000000000284 ) ) ;
#148482 = LINE ( 'NONE', #8965, #92059 ) ;
#148483 = CARTESIAN_POINT ( 'NONE',  ( -21.64999999999999858, 29.24307565605548120, -237.2405905340223455 ) ) ;
#148484 = CIRCLE ( 'NONE', #36058, 0.1000000000000028644 ) ;
#148485 = VERTEX_POINT ( 'NONE', #4240 ) ;
#148486 = AXIS2_PLACEMENT_3D ( 'NONE', #221158, #106332, #242016 ) ;
#148487 = ORIENTED_EDGE ( 'NONE', *, *, #35859, .F. ) ;
#148488 = AXIS2_PLACEMENT_3D ( 'NONE', #155935, #140172, #41122 ) ;
#148489 = CARTESIAN_POINT ( 'NONE',  ( -20.99780126800925117, 11.60538868788787070, -93.58735257170555144 ) ) ;
#148490 = CIRCLE ( 'NONE', #123533, 0.09999999999998898659 ) ;
#148491 = CARTESIAN_POINT ( 'NONE',  ( 23.25000000000000000, 31.49702336731128582, -233.4564499823349877 ) ) ;
#148493 = CARTESIAN_POINT ( 'NONE',  ( -15.66061380678751824, 12.83074261044330022, -215.9253900757177291 ) ) ;
#148492 = CARTESIAN_POINT ( 'NONE',  ( -20.64999999999999858, 48.40874555430183079, -244.2873875965402704 ) ) ;
#148494 = CARTESIAN_POINT ( 'NONE',  ( 20.95575313997065336, 39.27455013993715482, -236.7483772272189810 ) ) ;
#148495 = DIRECTION ( 'NONE',  ( 0.000000000000000000, 0.000000000000000000, -1.000000000000000000 ) ) ;
#148497 = EDGE_CURVE ( 'NONE', #17064, #32708, #131988, .T. ) ;
#148496 = DIRECTION ( 'NONE',  ( 1.000000000000000000, -0.000000000000000000, -0.000000000000000000 ) ) ;
#148498 = ORIENTED_EDGE ( 'NONE', *, *, #9708, .F. ) ;
#148499 = ORIENTED_EDGE ( 'NONE', *, *, #33260, .F. ) ;
#148500 = EDGE_CURVE ( 'NONE', #201510, #71510, #103338, .T. ) ;
#148501 = EDGE_CURVE ( 'NONE', #190865, #203670, #2979, .T. ) ;
#148502 = DIRECTION ( 'NONE',  ( -1.000000000000000000, 0.000000000000000000, 0.000000000000000000 ) ) ;
#148503 = ORIENTED_EDGE ( 'NONE', *, *, #202058, .T. ) ;
#148504 = LINE ( 'NONE', #109346, #97327 ) ;
#148505 = AXIS2_PLACEMENT_3D ( 'NONE', #256747, #58580, #138115 ) ;
#148506 = CIRCLE ( 'NONE', #231713, 0.09999999999999635569 ) ;
#148507 = CARTESIAN_POINT ( 'NONE',  ( -23.15000000000000213, -11.64999999998884483, -67.00000000000004263 ) ) ;
#148508 = AXIS2_PLACEMENT_3D ( 'NONE', #194081, #192785, #55790 ) ;
#148509 = ORIENTED_EDGE ( 'NONE', *, *, #196893, .T. ) ;
#148510 = CARTESIAN_POINT ( 'NONE',  ( -18.57399277249657032, 18.41291479239798434, -236.9963116028434058 ) ) ;
#148511 = ADVANCED_FACE ( 'NONE', ( #237735 ), #127904, .T. ) ;
#148512 = ORIENTED_EDGE ( 'NONE', *, *, #17181, .T. ) ;
#148513 = FACE_OUTER_BOUND ( 'NONE', #182047, .T. ) ;
#148514 = B_SPLINE_CURVE_WITH_KNOTS ( 'NONE', 3,
 ( #48669, #89076, #70840, #130778, #205162, #30414, #225992, #47374 ),
 .UNSPECIFIED., .F., .F.,
 ( 4, 2, 2, 4 ),
 ( 0.000000000000000000, 0.0001881495939909140220, 0.0002822243909863799641, 0.0003762991879818459334 ),
 .UNSPECIFIED. ) ;
#148515 = CARTESIAN_POINT ( 'NONE',  ( 20.94999999999999929, 7.980037321000004624, -237.6410835587014390 ) ) ;
#148516 = CARTESIAN_POINT ( 'NONE',  ( -18.38639463286148867, 64.51980042617562106, -60.27310748452440947 ) ) ;
#148517 = CARTESIAN_POINT ( 'NONE',  ( -23.25000000000000000, 69.14775023293175593, -234.9965690136722003 ) ) ;
#148518 = CARTESIAN_POINT ( 'NONE',  ( 23.14999999999999503, 6.650000000011155876, -54.65000000000000568 ) ) ;
#148519 = CARTESIAN_POINT ( 'NONE',  ( -22.00411653889206676, 0.09903810579716695872, -59.74655713235966914 ) ) ;
#148520 = DIRECTION ( 'NONE',  ( 0.000000000000000000, 0.000000000000000000, 1.000000000000000000 ) ) ;
#148521 = CARTESIAN_POINT ( 'NONE',  ( 23.15000000000000213, -9.599999999988842347, -191.1060308773475072 ) ) ;
#148523 = ORIENTED_EDGE ( 'NONE', *, *, #222718, .T. ) ;
#148522 = CARTESIAN_POINT ( 'NONE',  ( 18.48413544395651442, -0.8919438430603255918, -242.3193070551389496 ) ) ;
#148525 = DIRECTION ( 'NONE',  ( -0.000000000000000000, 1.000000000000000000, 6.982962677686266711E-15 ) ) ;
#148524 = CARTESIAN_POINT ( 'NONE',  ( -18.52139480978221897, 85.48135884507952653, -196.4985509174051970 ) ) ;
#148526 = ORIENTED_EDGE ( 'NONE', *, *, #220011, .T. ) ;
#148528 = ORIENTED_EDGE ( 'NONE', *, *, #52299, .F. ) ;
#148527 = DIRECTION ( 'NONE',  ( 1.000000000000000000, 0.000000000000000000, 0.000000000000000000 ) ) ;
#148529 = TOROIDAL_SURFACE ( 'NONE', #23657, 0.4000000000000012990, 0.1000000000000000056 ) ;
#148530 = VERTEX_POINT ( 'NONE', #240314 ) ;
#148531 = DIRECTION ( 'NONE',  ( 0.7071067811865474617, 0.7071067811865474617, -0.000000000000000000 ) ) ;
#148532 = CARTESIAN_POINT ( 'NONE',  ( -18.34374000495060386, 11.47316190337362585, -143.2500000000000284 ) ) ;
#148533 = EDGE_CURVE ( 'NONE', #182048, #42426, #7078, .T. ) ;
#148535 = ADVANCED_FACE ( 'NONE', ( #60370 ), #98623, .F. ) ;
#148534 = CARTESIAN_POINT ( 'NONE',  ( 21.02374657821570025, 62.99095723451777928, -207.1734234075709651 ) ) ;
#148536 = DIRECTION ( 'NONE',  ( -1.000000000000000000, 0.000000000000000000, 0.000000000000000000 ) ) ;
#148537 = CARTESIAN_POINT ( 'NONE',  ( -20.54999999999999716, 0.000000000000000000, -33.50000000000000000 ) ) ;
#148539 = DIRECTION ( 'NONE',  ( 1.000000000000000000, -0.000000000000000000, -0.000000000000000000 ) ) ;
#148538 = AXIS2_PLACEMENT_3D ( 'NONE', #152948, #233744, #74701 ) ;
#148540 = DIRECTION ( 'NONE',  ( 3.469446951953728416E-14, 0.7049548389604960441, -0.7092521942343085195 ) ) ;
#148541 = CARTESIAN_POINT ( 'NONE',  ( -16.77732147262506146, 51.60818360671130733, -231.9556725012951119 ) ) ;
#148542 = EDGE_CURVE ( 'NONE', #197466, #21234, #160799, .T. ) ;
#148544 = AXIS2_PLACEMENT_3D ( 'NONE', #32076, #111593, #211989 ) ;
#148543 = CYLINDRICAL_SURFACE ( 'NONE', #243345, 12.87499999999999822 ) ;
#148545 = ORIENTED_EDGE ( 'NONE', *, *, #95847, .T. ) ;
#148546 = EDGE_LOOP ( 'NONE', ( #169393, #34195, #9142, #107929 ) ) ;
#148547 = CARTESIAN_POINT ( 'NONE',  ( -18.50000000000000000, 74.65925378207906249, -213.7959699899455472 ) ) ;
#148548 = VECTOR ( 'NONE', #48270, 1000.000000000000000 ) ;
#148549 = CIRCLE ( 'NONE', #15281, 11.75000000000001066 ) ;
#148550 = ORIENTED_EDGE ( 'NONE', *, *, #163318, .T. ) ;
#148551 = DIRECTION ( 'NONE',  ( 1.000000000000000000, 0.000000000000000000, 0.000000000000000000 ) ) ;
#148552 = ORIENTED_EDGE ( 'NONE', *, *, #244393, .T. ) ;
#148553 = DIRECTION ( 'NONE',  ( 1.000000000000000000, -0.000000000000000000, 0.000000000000000000 ) ) ;
#148554 = AXIS2_PLACEMENT_3D ( 'NONE', #48367, #147472, #127919 ) ;
#148555 = CARTESIAN_POINT ( 'NONE',  ( -17.05016517655662156, 9.950000000014890489, -180.1726979959937580 ) ) ;
#148556 = DIRECTION ( 'NONE',  ( 0.000000000000000000, -1.000000000000000000, -6.982962677686266711E-15 ) ) ;
#148557 = FACE_OUTER_BOUND ( 'NONE', #243415, .T. ) ;
#148558 = CARTESIAN_POINT ( 'NONE',  ( 21.04999999999998650, 21.06723286205836487, -233.6551206055687260 ) ) ;
#148559 = ORIENTED_EDGE ( 'NONE', *, *, #206828, .T. ) ;
#148560 = ADVANCED_FACE ( 'NONE', ( #18686 ), #201173, .T. ) ;
#148561 = CARTESIAN_POINT ( 'NONE',  ( 19.97071067811864609, 51.35123479868923368, -230.1260867789306701 ) ) ;
#148562 = FACE_OUTER_BOUND ( 'NONE', #178830, .T. ) ;
#148563 = CARTESIAN_POINT ( 'NONE',  ( 18.41789779300691876, 85.50000000001161027, -62.49103781816362613 ) ) ;
#148564 = CARTESIAN_POINT ( 'NONE',  ( -20.94999999999999929, -1.835341550213257733, -78.55515129256303908 ) ) ;
#148565 = VERTEX_POINT ( 'NONE', #221994 ) ;
#148566 = CARTESIAN_POINT ( 'NONE',  ( 21.11927991906888025, 61.00523113630152494, -234.1759810734909877 ) ) ;
#148567 = ORIENTED_EDGE ( 'NONE', *, *, #88989, .F. ) ;
#148570 = EDGE_LOOP ( 'NONE', ( #70731, #252165, #110400, #37247 ) ) ;
#148569 = CARTESIAN_POINT ( 'NONE',  ( -18.36973785203555920, 64.52449679952776762, -112.2731074845243739 ) ) ;
#148568 = DIRECTION ( 'NONE',  ( 1.000000000000000000, 0.000000000000000000, -0.000000000000000000 ) ) ;
#148571 = DIRECTION ( 'NONE',  ( 0.000000000000000000, 0.8660254037844411501, 0.4999999999999956701 ) ) ;
#148572 = CIRCLE ( 'NONE', #48593, 0.5000000000000004441 ) ;
#148573 = CARTESIAN_POINT ( 'NONE',  ( -21.13435531349763963, 34.00405162396337033, -243.6249443725523918 ) ) ;
#148574 = ADVANCED_FACE ( 'NONE', ( #122935 ), #131630, .T. ) ;
#148575 = CIRCLE ( 'NONE', #19388, 11.79999999999999005 ) ;
#148576 = DIRECTION ( 'NONE',  ( 0.000000000000000000, 0.000000000000000000, 1.000000000000000000 ) ) ;
#148577 = ORIENTED_EDGE ( 'NONE', *, *, #2239, .T. ) ;
#148579 = EDGE_CURVE ( 'NONE', #233201, #121101, #186157, .T. ) ;
#148578 = DIRECTION ( 'NONE',  ( 0.000000000000000000, -0.9915357197604853789, 0.1298341882520022694 ) ) ;
#148580 = AXIS2_PLACEMENT_3D ( 'NONE', #127038, #50066, #7080 ) ;
#148581 = FACE_OUTER_BOUND ( 'NONE', #151813, .T. ) ;
#148582 = AXIS2_PLACEMENT_3D ( 'NONE', #107493, #29291, #228748 ) ;
#148583 = EDGE_CURVE ( 'NONE', #116241, #120691, #94564, .T. ) ;
#148585 = SPHERICAL_SURFACE ( 'NONE', #221785, 0.1000000000000000056 ) ;
#148584 = CARTESIAN_POINT ( 'NONE',  ( -22.49533356619861379, 11.65000000630418597, 0.06512258032272708053 ) ) ;
#148586 = ADVANCED_FACE ( 'NONE', ( #167221 ), #44683, .T. ) ;
#148587 = TOROIDAL_SURFACE ( 'NONE', #81891, 0.9750000000000019762, 0.1000000000000000056 ) ;
#148589 = VERTEX_POINT ( 'NONE', #223291 ) ;
#148588 = FACE_OUTER_BOUND ( 'NONE', #83388, .T. ) ;
#148590 = EDGE_LOOP ( 'NONE', ( #22542, #24090, #6161, #128320, #82176 ) ) ;
#148591 = DIRECTION ( 'NONE',  ( -0.000000000000000000, -0.1618390714546045217, 0.9868171638914230437 ) ) ;
#148592 = CARTESIAN_POINT ( 'NONE',  ( 21.05000000000000071, 7.980037321000004624, -237.6410835587014390 ) ) ;
#148593 = ADVANCED_FACE ( 'NONE', ( #205001 ), #26409, .F. ) ;
#148594 = CIRCLE ( 'NONE', #2815, 11.74999999999999645 ) ;
#148595 = CARTESIAN_POINT ( 'NONE',  ( -2.995603634470891112E-16, 69.35000000001254250, -182.3731074845244109 ) ) ;
#148597 = ADVANCED_FACE ( 'NONE', ( #247996 ), #107203, .T. ) ;
#148596 = ORIENTED_EDGE ( 'NONE', *, *, #168309, .T. ) ;
#148599 = AXIS2_PLACEMENT_3D ( 'NONE', #189457, #10816, #193309 ) ;
#148598 = CARTESIAN_POINT ( 'NONE',  ( -16.83794479845801817, 9.926357419362650703, -188.1964447042223014 ) ) ;
#148600 = CIRCLE ( 'NONE', #248530, 7.900000000000000355 ) ;
#148601 = DIRECTION ( 'NONE',  ( 0.000000000000000000, 1.000000000000000000, 0.000000000000000000 ) ) ;
#148602 = PLANE ( 'NONE',  #189319 ) ;
#148603 = ADVANCED_FACE ( 'NONE', ( #104606 ), #69961, .T. ) ;
#148604 = ORIENTED_EDGE ( 'NONE', *, *, #88053, .F. ) ;
#148605 = DIRECTION ( 'NONE',  ( 1.000000000000000000, 0.000000000000000000, 0.000000000000000000 ) ) ;
#148606 = B_SPLINE_CURVE_WITH_KNOTS ( 'NONE', 3,
 ( #73799, #33398, #112900, #192438, #133735, #94604 ),
 .UNSPECIFIED., .F., .F.,
 ( 4, 2, 4 ),
 ( 0.000000000000000000, 0.0001568709654583423218, 0.0003137419309166846436 ),
 .UNSPECIFIED. ) ;
#148607 = EDGE_CURVE ( 'NONE', #60113, #137137, #207206, .T. ) ;
#148608 = TOROIDAL_SURFACE ( 'NONE', #181915, 0.2000000000000000111, 0.1000000000000000056 ) ;
#148609 = ORIENTED_EDGE ( 'NONE', *, *, #17851, .T. ) ;
#148610 = CARTESIAN_POINT ( 'NONE',  ( -21.65000000000000213, 68.75000000001153921, -48.67310748452437252 ) ) ;
#148611 = FACE_OUTER_BOUND ( 'NONE', #214937, .T. ) ;
#148612 = EDGE_CURVE ( 'NONE', #177351, #80403, #96603, .T. ) ;
#148613 = ADVANCED_FACE ( 'NONE', ( #134456 ), #106465, .T. ) ;
#148614 = ORIENTED_EDGE ( 'NONE', *, *, #38500, .F. ) ;
#148615 = ORIENTED_EDGE ( 'NONE', *, *, #7219, .T. ) ;
#148616 = EDGE_CURVE ( 'NONE', #107956, #193635, #53659, .T. ) ;
#148617 = LINE ( 'NONE', #144731, #29298 ) ;
#148618 = ORIENTED_EDGE ( 'NONE', *, *, #19012, .T. ) ;
#148620 = ORIENTED_EDGE ( 'NONE', *, *, #57051, .T. ) ;
#148619 = FACE_OUTER_BOUND ( 'NONE', #207768, .T. ) ;
#148622 = ADVANCED_FACE ( 'NONE', ( #193189 ), #14557, .T. ) ;
#148621 = ORIENTED_EDGE ( 'NONE', *, *, #211949, .F. ) ;
#148623 = VECTOR ( 'NONE', #64250, 1000.000000000000114 ) ;
#148624 = CIRCLE ( 'NONE', #81935, 0.2000000000000057288 ) ;
#148627 = ORIENTED_EDGE ( 'NONE', *, *, #215128, .F. ) ;
#148626 = ORIENTED_EDGE ( 'NONE', *, *, #167423, .F. ) ;
#148625 = CARTESIAN_POINT ( 'NONE',  ( 22.16821283564876666, 59.93584560259384375, -233.8765425695785893 ) ) ;
#148628 = VECTOR ( 'NONE', #224680, 1000.000000000000000 ) ;
#148629 = AXIS2_PLACEMENT_3D ( 'NONE', #161549, #199394, #158994 ) ;
#148630 = EDGE_CURVE ( 'NONE', #36655, #237217, #63598, .T. ) ;
#148631 = CARTESIAN_POINT ( 'NONE',  ( -18.49999999999998579, -9.480686695267827702, -107.4411151687578752 ) ) ;
#148632 = ORIENTED_EDGE ( 'NONE', *, *, #194515, .T. ) ;
#148633 = DIRECTION ( 'NONE',  ( 0.000000000000000000, -6.308085367188393199E-16, -1.000000000000000000 ) ) ;
#148634 = DIRECTION ( 'NONE',  ( 1.000000000000000000, 0.000000000000000000, 0.000000000000000000 ) ) ;
#148635 = DIRECTION ( 'NONE',  ( 0.000000000000000000, 0.9908441862701791170, -0.1350103645450472789 ) ) ;
#148636 = AXIS2_PLACEMENT_3D ( 'NONE', #229466, #74269, #50793 ) ;
#148637 = FACE_OUTER_BOUND ( 'NONE', #128192, .T. ) ;
#148638 = ORIENTED_EDGE ( 'NONE', *, *, #95341, .F. ) ;
#148639 = ORIENTED_EDGE ( 'NONE', *, *, #91788, .F. ) ;
#148640 = CARTESIAN_POINT ( 'NONE',  ( -18.59999999999999787, 43.62273694548321856, -253.2814864317374770 ) ) ;
#148642 = ORIENTED_EDGE ( 'NONE', *, *, #244944, .T. ) ;
#148641 = DIRECTION ( 'NONE',  ( -2.602085213965226419E-14, -0.000000000000000000, -1.000000000000000000 ) ) ;
#148643 = CARTESIAN_POINT ( 'NONE',  ( 18.39999999999999858, -9.599999999988845900, -174.1001893912220737 ) ) ;
#148645 = ORIENTED_EDGE ( 'NONE', *, *, #232293, .F. ) ;
#148644 = CARTESIAN_POINT ( 'NONE',  ( 18.50000000000000000, 78.21362219944488459, -231.2727646510690533 ) ) ;
#148646 = EDGE_CURVE ( 'NONE', #187889, #118509, #161355, .T. ) ;
#148647 = AXIS2_PLACEMENT_3D ( 'NONE', #132023, #212855, #30375 ) ;
#148648 = VERTEX_POINT ( 'NONE', #97886 ) ;
#148649 = LINE ( 'NONE', #165646, #83556 ) ;
#148650 = VECTOR ( 'NONE', #140631, 1000.000000000000000 ) ;
#148651 = AXIS2_PLACEMENT_3D ( 'NONE', #142040, #217713, #36570 ) ;
#148652 = ORIENTED_EDGE ( 'NONE', *, *, #108514, .F. ) ;
#148653 = FACE_OUTER_BOUND ( 'NONE', #192056, .T. ) ;
#148654 = CARTESIAN_POINT ( 'NONE',  ( 18.59999999999999787, -10.84999999999999076, 32.89999999999999858 ) ) ;
#148656 = ORIENTED_EDGE ( 'NONE', *, *, #68953, .F. ) ;
#148655 = ORIENTED_EDGE ( 'NONE', *, *, #191678, .T. ) ;
#148657 = ORIENTED_EDGE ( 'NONE', *, *, #157742, .T. ) ;
#148658 = CARTESIAN_POINT ( 'NONE',  ( 23.14999999999999503, 6.550000000011156231, -179.8499999999999943 ) ) ;
#148659 = ORIENTED_EDGE ( 'NONE', *, *, #94238, .T. ) ;
#148660 = ORIENTED_EDGE ( 'NONE', *, *, #106727, .F. ) ;
#148661 = CARTESIAN_POINT ( 'NONE',  ( -21.04999999999999716, 85.60000000001160458, -62.49103808782458458 ) ) ;
#148663 = ORIENTED_EDGE ( 'NONE', *, *, #236295, .F. ) ;
#148662 = CARTESIAN_POINT ( 'NONE',  ( 21.05000000000000071, 62.92003201576280702, -207.2439188921395612 ) ) ;
#148664 = CARTESIAN_POINT ( 'NONE',  ( 5.900000000000060751, 64.25000000001119815, -22.02310748452479316 ) ) ;
#148666 = CARTESIAN_POINT ( 'NONE',  ( -23.15000000000000213, 85.00000000001222134, -146.4170766071767389 ) ) ;
#148665 = FACE_OUTER_BOUND ( 'NONE', #129354, .T. ) ;
#148667 = DIRECTION ( 'NONE',  ( -1.000000000000000000, 0.000000000000000000, 0.000000000000000000 ) ) ;
#148668 = CARTESIAN_POINT ( 'NONE',  ( 21.30000000000002558, 1.115600667400684642E-11, -100.5000000000000284 ) ) ;
#148669 = VERTEX_POINT ( 'NONE', #64879 ) ;
#148670 = ORIENTED_EDGE ( 'NONE', *, *, #106119, .F. ) ;
#148671 = CARTESIAN_POINT ( 'NONE',  ( 20.95000000000005258, 66.15000000001114699, -51.02310748452476474 ) ) ;
#148673 = EDGE_CURVE ( 'NONE', #87211, #101761, #85692, .T. ) ;
#148672 = DIRECTION ( 'NONE',  ( 1.000000000000000000, -7.304098846218134667E-16, -4.217023435051625732E-16 ) ) ;
#148674 = ORIENTED_EDGE ( 'NONE', *, *, #223238, .T. ) ;
#148675 = AXIS2_PLACEMENT_3D ( 'NONE', #224419, #109608, #6654 ) ;
#148676 = VECTOR ( 'NONE', #55044, 1000.000000000000000 ) ;
#148677 = ADVANCED_FACE ( 'NONE', ( #182282 ), #2329, .F. ) ;
#148678 = AXIS2_PLACEMENT_3D ( 'NONE', #103316, #182893, #231010 ) ;
#148679 = AXIS2_PLACEMENT_3D ( 'NONE', #245883, #226286, #222428 ) ;
#148680 = DIRECTION ( 'NONE',  ( 0.000000000000000000, -0.9908441862701791170, 0.1350103645450472789 ) ) ;
#148681 = VERTEX_POINT ( 'NONE', #242228 ) ;
#148682 = ORIENTED_EDGE ( 'NONE', *, *, #139074, .T. ) ;
#148683 = ADVANCED_FACE ( 'NONE', ( #137049 ), #106558, .F. ) ;
#148684 = CYLINDRICAL_SURFACE ( 'NONE', #175882, 0.09999999999999939493 ) ;
#148686 = EDGE_CURVE ( 'NONE', #49221, #143978, #117146, .T. ) ;
#148685 = DIRECTION ( 'NONE',  ( -1.000000000000000000, 0.000000000000000000, 0.000000000000000000 ) ) ;
#148687 = VERTEX_POINT ( 'NONE', #45324 ) ;
#148688 = DIRECTION ( 'NONE',  ( 0.000000000000000000, 0.3427706569149635563, -0.9394191166662964054 ) ) ;
#148689 = CARTESIAN_POINT ( 'NONE',  ( 21.14999999999999858, 8.786607556611267356, -112.7500000000000284 ) ) ;
#148690 = VERTEX_POINT ( 'NONE', #23225 ) ;
#148691 = CARTESIAN_POINT ( 'NONE',  ( 18.52326479938690440, -9.642364444904249154, -140.7147574134058061 ) ) ;
#148692 = DIRECTION ( 'NONE',  ( 0.000000000000000000, 0.000000000000000000, -1.000000000000000000 ) ) ;
#148694 = DIRECTION ( 'NONE',  ( 0.000000000000000000, -7.056502275159890832E-15, 1.000000000000000000 ) ) ;
#148693 = CARTESIAN_POINT ( 'NONE',  ( -21.14999999999999858, 69.45934304831071415, -103.0231074845243597 ) ) ;
#148695 = LINE ( 'NONE', #228226, #231664 ) ;
#148696 = LINE ( 'NONE', #189094, #145222 ) ;
#148697 = DIRECTION ( 'NONE',  ( 0.000000000000000000, 0.000000000000000000, -1.000000000000000000 ) ) ;
#148698 = DIRECTION ( 'NONE',  ( -1.000000000000000000, -0.000000000000000000, -0.000000000000000000 ) ) ;
#148699 = AXIS2_PLACEMENT_3D ( 'NONE', #254, #77219, #81064 ) ;
#148700 = AXIS2_PLACEMENT_3D ( 'NONE', #119569, #20468, #19160 ) ;
#148701 = CIRCLE ( 'NONE', #44631, 0.09999999999999939493 ) ;
#148702 = VERTEX_POINT ( 'NONE', #24500 ) ;
#148704 = EDGE_LOOP ( 'NONE', ( #138935, #122698, #22459, #221754 ) ) ;
#148703 = EDGE_LOOP ( 'NONE', ( #214961, #69789, #212960, #202225 ) ) ;
#148705 = CIRCLE ( 'NONE', #36277, 11.70000000000000284 ) ;
#148706 = VERTEX_POINT ( 'NONE', #25763 ) ;
#148707 = DIRECTION ( 'NONE',  ( 0.000000000000000000, 0.000000000000000000, -1.000000000000000000 ) ) ;
#148708 = DIRECTION ( 'NONE',  ( -1.000000000000000000, 0.000000000000000000, -0.000000000000000000 ) ) ;
#148710 = DIRECTION ( 'NONE',  ( 0.000000000000000000, 0.000000000000000000, 1.000000000000000000 ) ) ;
#148709 = CARTESIAN_POINT ( 'NONE',  ( 20.94999999999999574, -1.349084418615859482, -108.4864989635455146 ) ) ;
#148711 = DIRECTION ( 'NONE',  ( 1.000000000000000000, 0.000000000000000000, 0.000000000000000000 ) ) ;
#148712 = VERTEX_POINT ( 'NONE', #124866 ) ;
#148713 = CARTESIAN_POINT ( 'NONE',  ( 23.15000000000000213, -11.74999999998883737, -146.2500000000000284 ) ) ;
#148714 = ORIENTED_EDGE ( 'NONE', *, *, #242615, .T. ) ;
#148715 = CARTESIAN_POINT ( 'NONE',  ( -21.05000000000000071, -0.08579911627410685693, 6.413978881488484163 ) ) ;
#148716 = LINE ( 'NONE', #228251, #226516 ) ;
#148717 = CARTESIAN_POINT ( 'NONE',  ( -21.04999999999859739, 1.395114419150890628, -230.6779314796784206 ) ) ;
#148718 = VERTEX_POINT ( 'NONE', #105254 ) ;
#148719 = AXIS2_PLACEMENT_3D ( 'NONE', #220820, #196131, #100832 ) ;
#148720 = ADVANCED_FACE ( 'NONE', ( #143120 ), #222658, .T. ) ;
#148721 = FACE_OUTER_BOUND ( 'NONE', #876, .T. ) ;
#148722 = CARTESIAN_POINT ( 'NONE',  ( -23.15000000000000213, -4.892732937820631456, -233.2805462221312496 ) ) ;
#148723 = ORIENTED_EDGE ( 'NONE', *, *, #132380, .T. ) ;
#148724 = ORIENTED_EDGE ( 'NONE', *, *, #5008, .T. ) ;
#148725 = CARTESIAN_POINT ( 'NONE',  ( -18.35663730107557257, 64.52609257350069072, -93.77310748452438816 ) ) ;
#148726 = DIRECTION ( 'NONE',  ( -1.073024830501117725E-15, -0.000000000000000000, -1.000000000000000000 ) ) ;
#148727 = DIRECTION ( 'NONE',  ( 0.000000000000000000, 0.000000000000000000, -1.000000000000000000 ) ) ;
#148728 = DIRECTION ( 'NONE',  ( -3.469446951953515108E-14, 0.000000000000000000, 1.000000000000000000 ) ) ;
#148729 = LINE ( 'NONE', #250381, #19314 ) ;
#148730 = TOROIDAL_SURFACE ( 'NONE', #165474, 0.6000000000000004219, 0.1000000000000000056 ) ;
#148731 = CARTESIAN_POINT ( 'NONE',  ( -18.59999999999999787, 68.22930980752001062, -227.7331931781284879 ) ) ;
#148732 = VERTEX_POINT ( 'NONE', #145693 ) ;
#148733 = ADVANCED_FACE ( 'NONE', ( #216582 ), #18383, .F. ) ;
#148734 = DIRECTION ( 'NONE',  ( 1.000000000000000000, 0.000000000000000000, 0.000000000000000000 ) ) ;
#148736 = DIRECTION ( 'NONE',  ( -1.000000000000000000, 7.304098846218134667E-16, 5.100424963727256530E-30 ) ) ;
#148735 = DIRECTION ( 'NONE',  ( 0.000000000000000000, -0.9209589331071864615, 0.3896596508878908960 ) ) ;
#148737 = DIRECTION ( 'NONE',  ( 1.000000000000000000, -0.000000000000000000, 0.000000000000000000 ) ) ;
#148738 = ADVANCED_FACE ( 'NONE', ( #163998 ), #229885, .F. ) ;
#148739 = AXIS2_PLACEMENT_3D ( 'NONE', #116434, #190859, #154317 ) ;
#148740 = DIRECTION ( 'NONE',  ( -1.000000000000000000, 0.000000000000000000, 0.000000000000000000 ) ) ;
#148741 = DIRECTION ( 'NONE',  ( 0.000000000000000000, -1.000000000000000000, -6.982962677686265922E-15 ) ) ;
#148742 = CARTESIAN_POINT ( 'NONE',  ( 20.87600722750343252, 10.33112638556969465, -139.5901228926975080 ) ) ;
#148744 = VERTEX_POINT ( 'NONE', #227803 ) ;
#148743 = CARTESIAN_POINT ( 'NONE',  ( 21.00023020733502932, 30.82656943040776554, -252.1639858803266918 ) ) ;
#148745 = AXIS2_PLACEMENT_3D ( 'NONE', #59129, #40921, #1743 ) ;
#148746 = DIRECTION ( 'NONE',  ( -1.000000000000000000, 0.000000000000000000, -0.000000000000000000 ) ) ;
#148747 = ADVANCED_FACE ( 'NONE', ( #170459 ), #51713, .T. ) ;
#148748 = CIRCLE ( 'NONE', #53036, 0.09999999999999693856 ) ;
#148749 = VECTOR ( 'NONE', #11477, 1000.000000000000000 ) ;
#148750 = EDGE_CURVE ( 'NONE', #14880, #61925, #240334, .T. ) ;
#148751 = EDGE_CURVE ( 'NONE', #93645, #64897, #198619, .T. ) ;
#148752 = CARTESIAN_POINT ( 'NONE',  ( -22.50000000000000000, 64.35042919246716053, -103.1231074845243825 ) ) ;
#148753 = DIRECTION ( 'NONE',  ( 0.000000000000000000, 0.000000000000000000, 1.000000000000000000 ) ) ;
#148754 = ADVANCED_FACE ( 'NONE', ( #246104 ), #10046, .F. ) ;
#148755 = CARTESIAN_POINT ( 'NONE',  ( 18.59999999999999432, 78.48087866980282001, -232.8271061603568910 ) ) ;
#148756 = ORIENTED_EDGE ( 'NONE', *, *, #17575, .F. ) ;
#148757 = FACE_OUTER_BOUND ( 'NONE', #117446, .T. ) ;
#148758 = AXIS2_PLACEMENT_3D ( 'NONE', #114281, #154723, #54296 ) ;
#148759 = CARTESIAN_POINT ( 'NONE',  ( -18.59999999999999787, 70.44746257310249860, -228.4383880063670347 ) ) ;
#148760 = CARTESIAN_POINT ( 'NONE',  ( -18.59999999999999787, 7.128833340094563376, -233.7327013124401276 ) ) ;
#148761 = VECTOR ( 'NONE', #243959, 1000.000000000000114 ) ;
#148762 = EDGE_LOOP ( 'NONE', ( #13556, #133423, #106289, #19557 ) ) ;
#148763 = CARTESIAN_POINT ( 'NONE',  ( -16.87242674293850797, 66.05000000001159322, -56.87419773089673924 ) ) ;
#148766 = ORIENTED_EDGE ( 'NONE', *, *, #179036, .T. ) ;
#148765 = DIRECTION ( 'NONE',  ( 0.000000000000000000, -1.000000000000000000, 0.000000000000000000 ) ) ;
#148764 = STYLED_ITEM ( 'NONE', ( #81166 ), #189925 ) ;
#148767 = CARTESIAN_POINT ( 'NONE',  ( 21.13614978966382196, -1.383015948619066959, -194.6497536416913761 ) ) ;
#148768 = EDGE_CURVE ( 'NONE', #118445, #128224, #221479, .T. ) ;
#148769 = DIRECTION ( 'NONE',  ( 0.000000000000000000, -0.3738317757008748909, -0.9274965247785733613 ) ) ;
#148771 = EDGE_LOOP ( 'NONE', ( #166133, #3400, #167561, #133898 ) ) ;
#148770 = CIRCLE ( 'NONE', #2990, 0.1000000000000018374 ) ;
#148772 = FACE_OUTER_BOUND ( 'NONE', #88717, .T. ) ;
#148773 = SHAPE_DEFINITION_REPRESENTATION ( #111915, #36900 ) ;
#148774 = CARTESIAN_POINT ( 'NONE',  ( -18.59999999999999787, 9.250000000011157297, -146.3500000000000227 ) ) ;
#148775 = CARTESIAN_POINT ( 'NONE',  ( -18.59999999999999787, 77.83585931145570669, -125.0186683157258329 ) ) ;
#148776 = FACE_OUTER_BOUND ( 'NONE', #18526, .T. ) ;
#148777 = ORIENTED_EDGE ( 'NONE', *, *, #28010, .F. ) ;
#148778 = DIRECTION ( 'NONE',  ( 1.186688945009009831E-16, 1.000000000000000000, 6.982962677686266711E-15 ) ) ;
#148779 = CARTESIAN_POINT ( 'NONE',  ( -20.64999999999999858, 7.250000000011155521, -179.8499999999999943 ) ) ;
#148780 = VECTOR ( 'NONE', #241369, 1000.000000000000000 ) ;
#148781 = AXIS2_PLACEMENT_3D ( 'NONE', #193970, #111860, #110562 ) ;
#148782 = CARTESIAN_POINT ( 'NONE',  ( -5.900000000000002132, -11.34999999999999964, 13.90000000000000213 ) ) ;
#148783 = ORIENTED_EDGE ( 'NONE', *, *, #216038, .F. ) ;
#148784 = ORIENTED_EDGE ( 'NONE', *, *, #206876, .T. ) ;
#148785 = DIRECTION ( 'NONE',  ( 1.000000000000000000, 0.000000000000000000, 0.000000000000000000 ) ) ;
#148786 = CARTESIAN_POINT ( 'NONE',  ( -22.47071067811865319, 68.27992525551387359, -103.1221999392269737 ) ) ;
#148787 = CIRCLE ( 'NONE', #11995, 0.09999999999999982514 ) ;
#148788 = DIRECTION ( 'NONE',  ( 0.000000000000000000, -0.9770955615653316162, -0.2128009952263604232 ) ) ;
#148789 = CIRCLE ( 'NONE', #115641, 0.09999999999998898659 ) ;
#148791 = CARTESIAN_POINT ( 'NONE',  ( 22.48508240969612615, -2.433917398835509616, -189.6069785549278208 ) ) ;
#148790 = LINE ( 'NONE', #30137, #49320 ) ;
#148792 = CARTESIAN_POINT ( 'NONE',  ( -23.39999999999994529, 74.25000000001119815, -47.64205752314703801 ) ) ;
#148793 = DIRECTION ( 'NONE',  ( 0.000000000000000000, 0.2128009952263603677, -0.9770955615653313941 ) ) ;
#148794 = CARTESIAN_POINT ( 'NONE',  ( -18.46946985241332939, 46.92276463528965280, -255.3730311325347770 ) ) ;
#148795 = EDGE_CURVE ( 'NONE', #234572, #225274, #107029, .T. ) ;
#148796 = B_SPLINE_CURVE_WITH_KNOTS ( 'NONE', 3,
 ( #177397, #237345, #58675, #238622, #34043, #253040, #194388, #74452 ),
 .UNSPECIFIED., .F., .F.,
 ( 4, 2, 2, 4 ),
 ( 0.000000000000000000, 0.0001881495939909227498, 0.0002822243909863841383, 0.0003762991879818454997 ),
 .UNSPECIFIED. ) ;
#148798 = EDGE_LOOP ( 'NONE', ( #225478, #71618, #140057, #129584, #140998, #39916, #136610, #115492, #17481, #147016, #76495 ) ) ;
#148797 = CARTESIAN_POINT ( 'NONE',  ( 12.25000000000000000, 62.59162599727320497, -217.2417264603073761 ) ) ;
#148799 = CYLINDRICAL_SURFACE ( 'NONE', #255829, 0.09999999999999939493 ) ;
#148800 = CARTESIAN_POINT ( 'NONE',  ( -21.08884785362073089, -1.304174234192418069, -194.7778206845017337 ) ) ;
#148802 = CARTESIAN_POINT ( 'NONE',  ( 21.05000000000000071, -5.637547571910522137, -233.4427589080015650 ) ) ;
#148801 = DIRECTION ( 'NONE',  ( 0.000000000000000000, 7.086529944415894657E-15, -1.000000000000000000 ) ) ;
#148803 = VECTOR ( 'NONE', #16515, 1000.000000000000000 ) ;
#148804 = ORIENTED_EDGE ( 'NONE', *, *, #165081, .T. ) ;
#148805 = CARTESIAN_POINT ( 'NONE',  ( -16.87665923198281348, 66.05000000001201954, -115.6731074845243796 ) ) ;
#148806 = DIRECTION ( 'NONE',  ( -1.000000000000000000, 0.000000000000000000, 0.000000000000000000 ) ) ;
#148807 = DIRECTION ( 'NONE',  ( -0.000000000000000000, 1.000000000000000000, 0.000000000000000000 ) ) ;
#148808 = CARTESIAN_POINT ( 'NONE',  ( -21.04999999999999716, 69.69982018209508112, -103.0745903664065395 ) ) ;
#148810 = EDGE_CURVE ( 'NONE', #114130, #10085, #191286, .T. ) ;
#148809 = SPHERICAL_SURFACE ( 'NONE', #143930, 0.1000000000000000056 ) ;
#148811 = ORIENTED_EDGE ( 'NONE', *, *, #167200, .T. ) ;
#148812 = AXIS2_PLACEMENT_3D ( 'NONE', #201188, #142486, #184183 ) ;
#148813 = ORIENTED_EDGE ( 'NONE', *, *, #25120, .F. ) ;
#148814 = AXIS2_PLACEMENT_3D ( 'NONE', #239057, #139931, #71980 ) ;
#148815 = EDGE_CURVE ( 'NONE', #248851, #201727, #61260, .T. ) ;
#148817 = EDGE_CURVE ( 'NONE', #109970, #633, #115414, .T. ) ;
#148816 = AXIS2_PLACEMENT_3D ( 'NONE', #144845, #185275, #204816 ) ;
#148818 = AXIS2_PLACEMENT_3D ( 'NONE', #81639, #80362, #62125 ) ;
#148819 = FACE_OUTER_BOUND ( 'NONE', #82705, .T. ) ;
#148820 = VERTEX_POINT ( 'NONE', #72613 ) ;
#148821 = DIRECTION ( 'NONE',  ( 0.000000000000000000, -0.9126074666063660468, -0.4088369013363524762 ) ) ;
#148822 = ORIENTED_EDGE ( 'NONE', *, *, #25365, .T. ) ;
#148823 = CIRCLE ( 'NONE', #178042, 0.09999999999999939493 ) ;
#148824 = FACE_OUTER_BOUND ( 'NONE', #257298, .T. ) ;
#148825 = CARTESIAN_POINT ( 'NONE',  ( -17.22361732159832215, 65.65484434140965675, -125.1523229586572512 ) ) ;
#148826 = DIRECTION ( 'NONE',  ( 0.1538461538461484146, -0.9880948137434723000, 0.000000000000000000 ) ) ;
#148827 = ORIENTED_EDGE ( 'NONE', *, *, #247899, .T. ) ;
#148828 = ADVANCED_FACE ( 'NONE', ( #212115, #33511 ), #146972, .T. ) ;
#148829 = EDGE_CURVE ( 'NONE', #115507, #119750, #190274, .T. ) ;
#148830 = CARTESIAN_POINT ( 'NONE',  ( -22.39999999999999858, 7.790779598384560245, -33.50000000000000000 ) ) ;
#148831 = CARTESIAN_POINT ( 'NONE',  ( -18.59117750673696889, 68.11287320386161070, -224.1382462126928488 ) ) ;
#148832 = AXIS2_PLACEMENT_3D ( 'NONE', #169358, #228006, #12832 ) ;
#148833 = CARTESIAN_POINT ( 'NONE',  ( 18.79999999999999716, 3.461118860469513336, 28.84309995045515507 ) ) ;
#148834 = FACE_OUTER_BOUND ( 'NONE', #72184, .T. ) ;
#148835 = PRODUCT_DEFINITION ( 'UNKNOWN', '', #190452, #243437 ) ;
#148836 = CARTESIAN_POINT ( 'NONE',  ( -21.14999999999999858, -0.09999999998884338825, -26.95934304829875927 ) ) ;
#148837 = CARTESIAN_POINT ( 'NONE',  ( -17.11825945287482753, 10.04999999999998295, -12.75000000000000178 ) ) ;
#148838 = VERTEX_POINT ( 'NONE', #195134 ) ;
#148840 = DIRECTION ( 'NONE',  ( 0.000000000000000000, 1.000000000000000000, 0.000000000000000000 ) ) ;
#148839 = CARTESIAN_POINT ( 'NONE',  ( 18.59999999999999076, 63.83083047455526327, -209.3924252461221158 ) ) ;
#148841 = ORIENTED_EDGE ( 'NONE', *, *, #252339, .F. ) ;
#148843 = VERTEX_POINT ( 'NONE', #16488 ) ;
#148842 = FACE_OUTER_BOUND ( 'NONE', #220176, .T. ) ;
#148844 = AXIS2_PLACEMENT_3D ( 'NONE', #168755, #69614, #228691 ) ;
#148845 = EDGE_LOOP ( 'NONE', ( #96741, #82104, #35323, #46001 ) ) ;
#148846 = FACE_OUTER_BOUND ( 'NONE', #6724, .T. ) ;
#148847 = DIRECTION ( 'NONE',  ( 0.000000000000000000, 0.000000000000000000, -1.000000000000000000 ) ) ;
#148848 = CARTESIAN_POINT ( 'NONE',  ( -20.65000000000000568, 70.35000000001255671, -182.6731074845243938 ) ) ;
#148849 = EDGE_CURVE ( 'NONE', #10686, #226489, #161219, .T. ) ;
#148850 = CARTESIAN_POINT ( 'NONE',  ( -22.01447462590973103, 60.19480426826893193, -234.0493890886782822 ) ) ;
#148851 = VERTEX_POINT ( 'NONE', #174310 ) ;
#148852 = EDGE_CURVE ( 'NONE', #75516, #237169, #176847, .T. ) ;
#148853 = ADVANCED_FACE ( 'NONE', ( #15199 ), #153462, .F. ) ;
#148854 = CARTESIAN_POINT ( 'NONE',  ( 21.05000000000000071, 76.10000000001238618, -170.0231074845243313 ) ) ;
#148855 = CARTESIAN_POINT ( 'NONE',  ( 21.56666275994540172, 1.115600667400684642E-11, -127.0426315931066910 ) ) ;
#148856 = ORIENTED_EDGE ( 'NONE', *, *, #125586, .T. ) ;
#148857 = CARTESIAN_POINT ( 'NONE',  ( 21.05000000000000071, 1.115600667400684642E-11, -79.15000000000004832 ) ) ;
#148858 = EDGE_CURVE ( 'NONE', #134685, #167063, #194565, .T. ) ;
#148859 = DIRECTION ( 'NONE',  ( -0.000000000000000000, 0.9887567792719327286, 0.1495327102803745423 ) ) ;
#148860 = AXIS2_PLACEMENT_3D ( 'NONE', #157786, #221527, #118628 ) ;
#148861 = ORIENTED_EDGE ( 'NONE', *, *, #141209, .T. ) ;
#148862 = CIRCLE ( 'NONE', #36445, 0.09999999999999990841 ) ;
#148863 = LINE ( 'NONE', #133138, #185222 ) ;
#148864 = VECTOR ( 'NONE', #27694, 999.9999999999998863 ) ;
#148865 = AXIS2_PLACEMENT_3D ( 'NONE', #177315, #20794, #181145 ) ;
#148866 = B_SPLINE_CURVE_WITH_KNOTS ( 'NONE', 3,
 ( #41184, #120722, #240639, #200234, #62017, #211800, #248347, #67141, #110117, #187113, #71021, #206653, #129681, #86671, #91843, #226174, #147966, #28046, #9727 ),
 .UNSPECIFIED., .F., .F.,
 ( 4, 3, 3, 3, 3, 3, 4 ),
 ( -2.000416914650301595E-06, 0.000000000000000000, 4.714008503747321038E-05, 9.979203887779781405E-05, 0.0001372215519229620922, 0.0001635031576221085176, 0.0001900083748504240578 ),
 .UNSPECIFIED. ) ;
#148867 = ORIENTED_EDGE ( 'NONE', *, *, #141366, .T. ) ;
#148868 = CARTESIAN_POINT ( 'NONE',  ( -17.29158576265543346, 65.63525233399408876, -114.4403492397321997 ) ) ;
#148869 = VERTEX_POINT ( 'NONE', #55552 ) ;
#148870 = CARTESIAN_POINT ( 'NONE',  ( 20.27550659511088682, 66.78395627750344943, -157.3731074845244393 ) ) ;
#148871 = CARTESIAN_POINT ( 'NONE',  ( -18.40000000000000213, 64.25000000001261924, -190.8731074845244393 ) ) ;
#148872 = DIRECTION ( 'NONE',  ( 0.000000000000000000, 0.9875055080513743810, -0.1575844902526802316 ) ) ;
#148873 = DIRECTION ( 'NONE',  ( 1.000000000000000000, 0.000000000000000000, 0.000000000000000000 ) ) ;
#148874 = ADVANCED_FACE ( 'NONE', ( #118135 ), #115560, .F. ) ;
#148875 = CIRCLE ( 'NONE', #157259, 11.80000000000000426 ) ;
#148876 = FACE_OUTER_BOUND ( 'NONE', #201965, .T. ) ;
#148877 = LINE ( 'NONE', #32808, #59828 ) ;
#148878 = ORIENTED_EDGE ( 'NONE', *, *, #120672, .F. ) ;
#148879 = CARTESIAN_POINT ( 'NONE',  ( 18.39999999999999858, -9.600000000000003197, -40.10018939122204529 ) ) ;
#148880 = ORIENTED_EDGE ( 'NONE', *, *, #179746, .F. ) ;
#148881 = DIRECTION ( 'NONE',  ( 1.000000000000000000, 0.000000000000000000, 0.000000000000000000 ) ) ;
#148882 = ORIENTED_EDGE ( 'NONE', *, *, #241288, .F. ) ;
#148883 = CIRCLE ( 'NONE', #11515, 0.1000000000000013933 ) ;
#148884 = CARTESIAN_POINT ( 'NONE',  ( -20.64999999999999858, 76.00000000001244871, -170.0231074845243597 ) ) ;
#148885 = DIRECTION ( 'NONE',  ( -1.073024830501117725E-15, -6.982962677686266711E-15, 1.000000000000000000 ) ) ;
#148886 = EDGE_CURVE ( 'NONE', #227165, #13242, #69649, .T. ) ;
#148887 = DIRECTION ( 'NONE',  ( 0.000000000000000000, 7.086529944415894657E-15, -1.000000000000000000 ) ) ;
#148888 = VERTEX_POINT ( 'NONE', #93423 ) ;
#148890 = ORIENTED_EDGE ( 'NONE', *, *, #217815, .F. ) ;
#148889 = DIRECTION ( 'NONE',  ( -4.408576920032448588E-17, 0.1350103645451876944, -0.9908441862701601321 ) ) ;
#148891 = CARTESIAN_POINT ( 'NONE',  ( 18.59999999999999432, 74.83729825007360148, -61.42310748452432989 ) ) ;
#148892 = ADVANCED_FACE ( 'NONE', ( #157287 ), #217212, .F. ) ;
#148894 = CARTESIAN_POINT ( 'NONE',  ( 18.49999999999999289, 15.23147493058208113, -222.9643141222125848 ) ) ;
#148893 = DIRECTION ( 'NONE',  ( 0.000000000000000000, 0.000000000000000000, -1.000000000000000000 ) ) ;
#148896 = ORIENTED_EDGE ( 'NONE', *, *, #198988, .F. ) ;
#148895 = DIRECTION ( 'NONE',  ( 0.000000000000000000, -0.5000000000000078826, 0.8660254037844340447 ) ) ;
#148897 = ORIENTED_EDGE ( 'NONE', *, *, #72936, .F. ) ;
#148898 = AXIS2_PLACEMENT_3D ( 'NONE', #196795, #18169, #36480 ) ;
#148899 = AXIS2_PLACEMENT_3D ( 'NONE', #141522, #221053, #200224 ) ;
#148901 = EDGE_CURVE ( 'NONE', #155690, #90469, #57136, .T. ) ;
#148900 = LINE ( 'NONE', #10667, #47687 ) ;
#148902 = FACE_OUTER_BOUND ( 'NONE', #122482, .T. ) ;
#148904 = EDGE_CURVE ( 'NONE', #164268, #113546, #197660, .T. ) ;
#148903 = EDGE_LOOP ( 'NONE', ( #190746, #67189, #207211, #85886 ) ) ;
#148905 = CARTESIAN_POINT ( 'NONE',  ( -20.94999999999999929, -11.29603075032412640, -164.4521008403361577 ) ) ;
#148906 = ORIENTED_EDGE ( 'NONE', *, *, #46695, .F. ) ;
#148907 = CARTESIAN_POINT ( 'NONE',  ( 21.05000000000000071, -0.09999999999999939493, 11.64957080754479968 ) ) ;
#148908 = CARTESIAN_POINT ( 'NONE',  ( 20.00000000000001421, 34.40595771266847436, -235.0146864773514892 ) ) ;
#148909 = AXIS2_PLACEMENT_3D ( 'NONE', #19188, #180838, #40069 ) ;
#148910 = EDGE_LOOP ( 'NONE', ( #229376, #255337, #199363, #122370 ) ) ;
#148911 = SPHERICAL_SURFACE ( 'NONE', #54184, 0.1000000000000000056 ) ;
#148912 = AXIS2_PLACEMENT_3D ( 'NONE', #178691, #82090, #195680 ) ;
#148913 = ORIENTED_EDGE ( 'NONE', *, *, #206780, .T. ) ;
#148914 = CIRCLE ( 'NONE', #253120, 7.900000000000011013 ) ;
#148915 = CIRCLE ( 'NONE', #103090, 0.2000000000000057288 ) ;
#148916 = CARTESIAN_POINT ( 'NONE',  ( -16.94107738177414291, 10.01423928514777373, -121.4500000000000313 ) ) ;
#148917 = EDGE_CURVE ( 'NONE', #174276, #117062, #213369, .T. ) ;
#148918 = VECTOR ( 'NONE', #200471, 1000.000000000000000 ) ;
#148919 = VERTEX_POINT ( 'NONE', #98519 ) ;
#148920 = ORIENTED_EDGE ( 'NONE', *, *, #166193, .T. ) ;
#148922 = CARTESIAN_POINT ( 'NONE',  ( -21.05000000000000071, 61.16604239670572696, -234.3115055913001470 ) ) ;
#148921 = CIRCLE ( 'NONE', #36520, 2.000000000000002665 ) ;
#148923 = EDGE_LOOP ( 'NONE', ( #194419, #137229, #614, #212533 ) ) ;
#148924 = EDGE_CURVE ( 'NONE', #167941, #251797, #165509, .T. ) ;
#148925 = DIRECTION ( 'NONE',  ( 0.000000000000000000, -0.8660254037844377084, -0.5000000000000016653 ) ) ;
#148926 = CIRCLE ( 'NONE', #244578, 0.1000000000000001860 ) ;
#148927 = VERTEX_POINT ( 'NONE', #34780 ) ;
#148929 = ORIENTED_EDGE ( 'NONE', *, *, #32895, .T. ) ;
#148928 = DIRECTION ( 'NONE',  ( 0.000000000000000000, 1.000000000000000000, 6.982962677686266711E-15 ) ) ;
#148930 = CARTESIAN_POINT ( 'NONE',  ( 20.94999999999999574, -1.835341550213255957, -45.05515129256298223 ) ) ;
#148931 = ORIENTED_EDGE ( 'NONE', *, *, #147418, .T. ) ;
#148932 = DIRECTION ( 'NONE',  ( 0.000000000000000000, -6.997203936713175802E-15, 1.000000000000000000 ) ) ;
#148934 = VERTEX_POINT ( 'NONE', #235503 ) ;
#148933 = EDGE_CURVE ( 'NONE', #250075, #198238, #228036, .T. ) ;
#148937 = EDGE_LOOP ( 'NONE', ( #3919, #89959, #194752 ) ) ;
#148936 = ORIENTED_EDGE ( 'NONE', *, *, #227151, .F. ) ;
#148935 = CARTESIAN_POINT ( 'NONE',  ( 21.14999999999999858, 6.650000000011155876, -146.3500000000000227 ) ) ;
#148938 = LINE ( 'NONE', #188057, #165560 ) ;
#148939 = ADVANCED_FACE ( 'NONE', ( #257580 ), #215930, .F. ) ;
#148940 = SPHERICAL_SURFACE ( 'NONE', #227355, 0.1000000000000000056 ) ;
#148942 = ORIENTED_EDGE ( 'NONE', *, *, #245976, .T. ) ;
#148941 = AXIS2_PLACEMENT_3D ( 'NONE', #65074, #200738, #221554 ) ;
#148943 = AXIS2_PLACEMENT_3D ( 'NONE', #90554, #190981, #48865 ) ;
#148944 = AXIS2_PLACEMENT_3D ( 'NONE', #232057, #208644, #230774 ) ;
#148945 = CIRCLE ( 'NONE', #36539, 0.1000000000000028783 ) ;
#148946 = ORIENTED_EDGE ( 'NONE', *, *, #221852, .F. ) ;
#148947 = TOROIDAL_SURFACE ( 'NONE', #211295, 0.6000000000000017542, 0.1000000000000000056 ) ;
#148948 = DIRECTION ( 'NONE',  ( 0.000000000000000000, -0.4930308989874980785, -0.8700118002898462599 ) ) ;
#148949 = CARTESIAN_POINT ( 'NONE',  ( -16.97683809663752186, 62.98531230502843670, -213.8799296553602005 ) ) ;
#148951 = ORIENTED_EDGE ( 'NONE', *, *, #166976, .T. ) ;
#148950 = CARTESIAN_POINT ( 'NONE',  ( -20.64999999999999858, 4.349999999999999645, -12.25000000000000000 ) ) ;
#148952 = CARTESIAN_POINT ( 'NONE',  ( -21.05000000000000071, 1.115600667400684642E-11, -96.50000000000004263 ) ) ;
#148953 = ORIENTED_EDGE ( 'NONE', *, *, #231615, .F. ) ;
#148954 = ADVANCED_FACE ( 'NONE', ( #193830 ), #73907, .F. ) ;
#148955 = AXIS2_PLACEMENT_3D ( 'NONE', #168183, #230689, #109427 ) ;
#148956 = CARTESIAN_POINT ( 'NONE',  ( -18.79999999999999716, -1.212568896937008089, -7.900000000000000355 ) ) ;
#148957 = CARTESIAN_POINT ( 'NONE',  ( 23.14999999999999147, 1.148907358139439339E-11, -201.0000000000015064 ) ) ;
#148958 = EDGE_CURVE ( 'NONE', #148565, #163993, #113004, .T. ) ;
#148959 = ORIENTED_EDGE ( 'NONE', *, *, #90077, .F. ) ;
#148960 = FACE_OUTER_BOUND ( 'NONE', #255203, .T. ) ;
#148961 = CYLINDRICAL_SURFACE ( 'NONE', #199178, 0.09999999999998898659 ) ;
#148962 = VERTEX_POINT ( 'NONE', #103677 ) ;
#148964 = VERTEX_POINT ( 'NONE', #80252 ) ;
#148963 = DIRECTION ( 'NONE',  ( 0.000000000000000000, -0.8068669527897506244, -0.5907332058516622242 ) ) ;
#148965 = CYLINDRICAL_SURFACE ( 'NONE', #140033, 0.1000000000000038219 ) ;
#148966 = CIRCLE ( 'NONE', #215573, 0.1000000000000013933 ) ;
#148967 = CIRCLE ( 'NONE', #28177, 0.1000000000000054040 ) ;
#148968 = AXIS2_PLACEMENT_3D ( 'NONE', #234042, #232789, #55372 ) ;
#148970 = EDGE_LOOP ( 'NONE', ( #49286, #85521, #87872, #106409 ) ) ;
#148969 = EDGE_LOOP ( 'NONE', ( #117213, #13595, #52067, #113788 ) ) ;
#148971 = ORIENTED_EDGE ( 'NONE', *, *, #252854, .F. ) ;
#148972 = CARTESIAN_POINT ( 'NONE',  ( 23.14999999999999503, 53.33306769324366314, -234.7945388949160872 ) ) ;
#148973 = EDGE_LOOP ( 'NONE', ( #227178, #254654 ) ) ;
#148974 = VERTEX_POINT ( 'NONE', #63286 ) ;
#148975 = CARTESIAN_POINT ( 'NONE',  ( -21.05000000000000071, 87.65000000001215597, -139.6231074845242688 ) ) ;
#148976 = VERTEX_POINT ( 'NONE', #123275 ) ;
#148977 = DIRECTION ( 'NONE',  ( 0.000000000000000000, 0.9651348961777259650, -0.2617529984164657098 ) ) ;
#148978 = DIRECTION ( 'NONE',  ( -1.000000000000000000, -0.000000000000000000, -0.000000000000000000 ) ) ;
#148979 = VERTEX_POINT ( 'NONE', #65861 ) ;
#148980 = VECTOR ( 'NONE', #166694, 1000.000000000000114 ) ;
#148981 = VECTOR ( 'NONE', #13048, 1000.000000000000000 ) ;
#148982 = ORIENTED_EDGE ( 'NONE', *, *, #60668, .F. ) ;
#148983 = CARTESIAN_POINT ( 'NONE',  ( 21.72449340488910607, 59.72708471423849375, -224.2357723256170061 ) ) ;
#148985 = CIRCLE ( 'NONE', #45091, 0.1000000000000000056 ) ;
#148984 = B_SPLINE_CURVE_WITH_KNOTS ( 'NONE', 3,
 ( #187763, #166936, #125212, #223003, #84749, #144746 ),
 .UNSPECIFIED., .F., .F.,
 ( 4, 2, 4 ),
 ( 0.000000000000000000, 0.0001895189928937412213, 0.0003790379857874824425 ),
 .UNSPECIFIED. ) ;
#148986 = ORIENTED_EDGE ( 'NONE', *, *, #177993, .F. ) ;
#148987 = EDGE_CURVE ( 'NONE', #122992, #113629, #190465, .T. ) ;
#148988 = CIRCLE ( 'NONE', #228093, 0.09999999999998986089 ) ;
#148989 = CARTESIAN_POINT ( 'NONE',  ( -23.15000000000000213, 51.38014393322265505, -230.1906178717505611 ) ) ;
#148990 = ORIENTED_EDGE ( 'NONE', *, *, #206020, .F. ) ;
#148991 = DIRECTION ( 'NONE',  ( 0.000000000000000000, 1.000000000000000000, 0.000000000000000000 ) ) ;
#148993 = EDGE_LOOP ( 'NONE', ( #88583, #24207, #40474, #128467 ) ) ;
#148992 = PLANE ( 'NONE',  #58480 ) ;
#148994 = CARTESIAN_POINT ( 'NONE',  ( 21.05000000000005400, 76.00000000001119815, -40.17310748452479174 ) ) ;
#148995 = CARTESIAN_POINT ( 'NONE',  ( -21.59142135623730852, 12.17094120733686680, -219.9950833145813363 ) ) ;
#148996 = VECTOR ( 'NONE', #210830, 1000.000000000000000 ) ;
#148997 = DIRECTION ( 'NONE',  ( 0.000000000000000000, 1.000000000000000000, 6.853228547068871147E-15 ) ) ;
#148998 = DIRECTION ( 'NONE',  ( 0.000000000000000000, 1.000000000000000000, 0.000000000000000000 ) ) ;
#148999 = DIRECTION ( 'NONE',  ( 1.000000000000000000, 0.000000000000000000, 0.000000000000000000 ) ) ;
#149000 = DIRECTION ( 'NONE',  ( 1.000000000000000000, 0.000000000000000000, 0.000000000000000000 ) ) ;
#149002 = TOROIDAL_SURFACE ( 'NONE', #36594, 0.2000000000000000111, 0.1000000000000000056 ) ;
#149001 = CARTESIAN_POINT ( 'NONE',  ( -21.05000000000000426, 6.332272273946811580, -33.53753606328567116 ) ) ;
#149003 = AXIS2_PLACEMENT_3D ( 'NONE', #176641, #117915, #197457 ) ;
#149004 = CARTESIAN_POINT ( 'NONE',  ( 22.49999999999999645, 75.90000000001245439, -181.6726782920691505 ) ) ;
#149006 = DIRECTION ( 'NONE',  ( 0.000000000000000000, 0.000000000000000000, -1.000000000000000000 ) ) ;
#149005 = VECTOR ( 'NONE', #25398, 1000.000000000000000 ) ;
#149007 = ADVANCED_FACE ( 'NONE', ( #20340 ), #163689, .T. ) ;
#149009 = ORIENTED_EDGE ( 'NONE', *, *, #194888, .F. ) ;
#149008 = AXIS2_PLACEMENT_3D ( 'NONE', #55602, #176899, #214710 ) ;
#149010 = ORIENTED_EDGE ( 'NONE', *, *, #176528, .F. ) ;
#149012 = VERTEX_POINT ( 'NONE', #99818 ) ;
#149011 = DIRECTION ( 'NONE',  ( 0.000000000000000000, 1.734723475976757554E-14, -1.000000000000000000 ) ) ;
#149013 = ORIENTED_EDGE ( 'NONE', *, *, #58330, .F. ) ;
#149014 = CARTESIAN_POINT ( 'NONE',  ( -18.41431012584569160, 64.51252797080373114, -93.79634349762605439 ) ) ;
#149015 = DIRECTION ( 'NONE',  ( 0.000000000000000000, -0.9916376685811618685, 0.1290532225514649800 ) ) ;
#149017 = LINE ( 'NONE', #130707, #107178 ) ;
#149016 = DIRECTION ( 'NONE',  ( 2.952720810173289605E-16, 0.4088369013363286064, -0.9126074666063768159 ) ) ;
#149018 = ORIENTED_EDGE ( 'NONE', *, *, #253487, .F. ) ;
#149019 = ORIENTED_EDGE ( 'NONE', *, *, #160345, .F. ) ;
#149020 = AXIS2_PLACEMENT_3D ( 'NONE', #164861, #121888, #83975 ) ;
#149021 = SHAPE_REPRESENTATION_RELATIONSHIP ( 'NONE' , 'NONE' ,  #241717, #63721 ) ;
#149022 = CARTESIAN_POINT ( 'NONE',  ( -22.39999999999999858, 68.20922040163824818, -69.62310748452438247 ) ) ;
#149023 = DIRECTION ( 'NONE',  ( 0.000000000000000000, 0.000000000000000000, 1.000000000000000000 ) ) ;
#149024 = ORIENTED_EDGE ( 'NONE', *, *, #37965, .F. ) ;
#149025 = VERTEX_POINT ( 'NONE', #144097 ) ;
#149026 = AXIS2_PLACEMENT_3D ( 'NONE', #230961, #171015, #56127 ) ;
#149027 = DIRECTION ( 'NONE',  ( 1.000000000000000000, 0.000000000000000000, 0.000000000000000000 ) ) ;
#149028 = CARTESIAN_POINT ( 'NONE',  ( 20.94999999999999929, 87.29603075034741266, -133.4752083248603469 ) ) ;
#149029 = DIRECTION ( 'NONE',  ( -1.000000000000000000, 0.000000000000000000, 0.000000000000000000 ) ) ;
#149030 = DIRECTION ( 'NONE',  ( -1.000000000000000000, -0.000000000000000000, 0.000000000000000000 ) ) ;
#149031 = CARTESIAN_POINT ( 'NONE',  ( -20.00857864376270001, 9.150000000011157653, -112.8500000000000369 ) ) ;
#149033 = ORIENTED_EDGE ( 'NONE', *, *, #64454, .T. ) ;
#149032 = DIRECTION ( 'NONE',  ( -1.000000000000000000, 0.000000000000000000, 0.000000000000000000 ) ) ;
#149034 = DIRECTION ( 'NONE',  ( 1.000000000000000000, 0.000000000000000000, 0.000000000000000000 ) ) ;
#149035 = CARTESIAN_POINT ( 'NONE',  ( 23.14999999999999858, 70.10000000001251408, -180.2422072491807796 ) ) ;
#149036 = DIRECTION ( 'NONE',  ( 2.259780016855444678E-14, 0.9984213852963244040, 0.05616704890742149625 ) ) ;
#149037 = CARTESIAN_POINT ( 'NONE',  ( 18.59999999999999787, 85.32100840337319880, -95.78716923544638462 ) ) ;
#149038 = ORIENTED_EDGE ( 'NONE', *, *, #109479, .F. ) ;
#149039 = SPHERICAL_SURFACE ( 'NONE', #77806, 0.1000000000000000056 ) ;
#149040 = DIRECTION ( 'NONE',  ( 0.000000000000000000, 0.000000000000000000, -1.000000000000000000 ) ) ;
#149042 = FACE_OUTER_BOUND ( 'NONE', #236121, .T. ) ;
#149041 = CARTESIAN_POINT ( 'NONE',  ( 18.59999999999999076, 16.67126802362266247, -222.8016931105129004 ) ) ;
#149043 = CYLINDRICAL_SURFACE ( 'NONE', #166480, 0.1000000000000124678 ) ;
#149045 = ADVANCED_FACE ( 'NONE', ( #240648 ), #111332, .T. ) ;
#149044 = DIRECTION ( 'NONE',  ( 0.7071067811865474617, -0.7071067811865474617, -4.937700262164531476E-15 ) ) ;
#149046 = CARTESIAN_POINT ( 'NONE',  ( -18.50000000000000000, 9.350000000011156942, -155.3500000000000227 ) ) ;
#149047 = CARTESIAN_POINT ( 'NONE',  ( -21.05000000000000071, 1.835341550235567887, -112.1551512925630192 ) ) ;
#149048 = CIRCLE ( 'NONE', #178078, 7.800000000000001599 ) ;
#149049 = AXIS2_PLACEMENT_3D ( 'NONE', #243028, #6987, #106064 ) ;
#149050 = DIRECTION ( 'NONE',  ( 0.000000000000000000, 0.000000000000000000, -1.000000000000000000 ) ) ;
#149051 = DIRECTION ( 'NONE',  ( 1.000000000000000000, -0.000000000000000000, -0.000000000000000000 ) ) ;
#149052 = CIRCLE ( 'NONE', #144911, 0.09999999999999681366 ) ;
#149053 = ORIENTED_EDGE ( 'NONE', *, *, #87763, .T. ) ;
#149054 = ORIENTED_EDGE ( 'NONE', *, *, #134976, .T. ) ;
#149055 = EDGE_LOOP ( 'NONE', ( #237467, #252895, #233684, #229652 ) ) ;
#149056 = EDGE_CURVE ( 'NONE', #142484, #175914, #132174, .T. ) ;
#149057 = CARTESIAN_POINT ( 'NONE',  ( 20.97565083910961548, 65.52538259873308846, -95.44516430793582629 ) ) ;
#149058 = FACE_OUTER_BOUND ( 'NONE', #232427, .T. ) ;
#149059 = ORIENTED_EDGE ( 'NONE', *, *, #220573, .F. ) ;
#149060 = EDGE_CURVE ( 'NONE', #89853, #61020, #221072, .T. ) ;
#149061 = ORIENTED_EDGE ( 'NONE', *, *, #232758, .F. ) ;
#149062 = AXIS2_PLACEMENT_3D ( 'NONE', #158847, #97529, #239649 ) ;
#149063 = AXIS2_PLACEMENT_3D ( 'NONE', #116436, #112583, #16070 ) ;
#149064 = EDGE_CURVE ( 'NONE', #170209, #2973, #164966, .T. ) ;
#149065 = ORIENTED_EDGE ( 'NONE', *, *, #207913, .F. ) ;
#149066 = FACE_OUTER_BOUND ( 'NONE', #192632, .T. ) ;
#149067 = EDGE_LOOP ( 'NONE', ( #23976, #16419, #257441, #89622 ) ) ;
#149068 = VECTOR ( 'NONE', #147370, 1000.000000000000000 ) ;
#149069 = CARTESIAN_POINT ( 'NONE',  ( -16.81744102076748959, 66.05000000001182059, -82.17310748452439384 ) ) ;
#149070 = CARTESIAN_POINT ( 'NONE',  ( -18.59999999999999787, 76.00000000001213607, -136.5231074845243313 ) ) ;
#149071 = DIRECTION ( 'NONE',  ( -1.000000000000000000, -3.190570557967288949E-16, -6.948722487160392945E-17 ) ) ;
#149072 = FACE_OUTER_BOUND ( 'NONE', #33614, .T. ) ;
#149073 = CARTESIAN_POINT ( 'NONE',  ( -23.25000000000000000, 1.115600667400684642E-11, -167.4999999999999716 ) ) ;
#149075 = VERTEX_POINT ( 'NONE', #162416 ) ;
#149074 = CARTESIAN_POINT ( 'NONE',  ( -21.05000000000000071, 46.45388641681647357, -243.1520440498138385 ) ) ;
#149077 = CARTESIAN_POINT ( 'NONE',  ( 21.08804582317315379, 8.878166167103044515, -79.34999982940649943 ) ) ;
#149076 = CARTESIAN_POINT ( 'NONE',  ( 20.99551997958397109, 11.75000000000023626, -26.65165913768949579 ) ) ;
#149078 = EDGE_CURVE ( 'NONE', #248843, #212292, #721, .T. ) ;
#149079 = EDGE_LOOP ( 'NONE', ( #52363, #134724 ) ) ;
#149080 = DIRECTION ( 'NONE',  ( 1.000000000000000000, 0.000000000000000000, -0.000000000000000000 ) ) ;
#149081 = CARTESIAN_POINT ( 'NONE',  ( -12.29659703204451660, 9.355888454513701546, -116.7886428967780290 ) ) ;
#149082 = FACE_OUTER_BOUND ( 'NONE', #178521, .T. ) ;
#149083 = EDGE_LOOP ( 'NONE', ( #41409, #30036, #92754, #99497, #171829, #90091, #88071, #60728, #37458, #70724, #190732, #127951, #208758, #50401, #255347, #125821, #112753, #65644 ) ) ;
#149084 = CYLINDRICAL_SURFACE ( 'NONE', #145908, 0.1000000000000028644 ) ;
#149085 = B_SPLINE_CURVE_WITH_KNOTS ( 'NONE', 3,
 ( #250587, #116242, #134477, #254421, #34156, #13280, #233615, #214043, #32877, #96623, #191943, #193208, #75814, #172395, #57512, #210204 ),
 .UNSPECIFIED., .F., .F.,
 ( 4, 3, 3, 3, 3, 4 ),
 ( 0.000000000000000000, 1.810570668010836920E-05, 2.740575833572790496E-05, 4.256816319437009604E-05, 5.213463471025706227E-05, 6.641585710719227482E-05 ),
 .UNSPECIFIED. ) ;
#149086 = CIRCLE ( 'NONE', #165840, 0.1000000000000028644 ) ;
#149087 = DIRECTION ( 'NONE',  ( 1.000000000000000000, -0.000000000000000000, -0.000000000000000000 ) ) ;
#149088 = ORIENTED_EDGE ( 'NONE', *, *, #141236, .T. ) ;
#149089 = AXIS2_PLACEMENT_3D ( 'NONE', #158393, #74997, #16304 ) ;
#149090 = CARTESIAN_POINT ( 'NONE',  ( 20.94999999999999929, 53.66153320161009788, -235.9075159595686841 ) ) ;
#149091 = CARTESIAN_POINT ( 'NONE',  ( 20.85000000000000142, 77.13501884592258762, -162.3061306010920362 ) ) ;
#149092 = DIRECTION ( 'NONE',  ( 1.000000000000000000, 3.469446951953704435E-14, -2.003086131649669752E-14 ) ) ;
#149093 = PLANE ( 'NONE',  #161631 ) ;
#149094 = ORIENTED_EDGE ( 'NONE', *, *, #94197, .F. ) ;
#149095 = CIRCLE ( 'NONE', #119886, 12.97499999999999964 ) ;
#149096 = EDGE_LOOP ( 'NONE', ( #36565, #63144, #40240, #14598 ) ) ;
#149097 = CARTESIAN_POINT ( 'NONE',  ( -21.14999999999999858, 69.74218538953553548, -69.62089777583315708 ) ) ;
#149098 = CARTESIAN_POINT ( 'NONE',  ( -23.25000000000000000, 77.83585931145526615, -58.01866831572577610 ) ) ;
#149099 = CYLINDRICAL_SURFACE ( 'NONE', #186822, 0.09999999999998898659 ) ;
#149100 = CARTESIAN_POINT ( 'NONE',  ( -18.59999999999999787, 64.35000000001205933, -124.2731074845243882 ) ) ;
#149102 = CARTESIAN_POINT ( 'NONE',  ( 21.05000000000000071, 23.34004772283015683, -229.2004250369967338 ) ) ;
#149101 = CARTESIAN_POINT ( 'NONE',  ( 23.24999999999999645, 76.00000000001237765, -170.0231074845243597 ) ) ;
#149103 = AXIS2_PLACEMENT_3D ( 'NONE', #165914, #5503, #28991 ) ;
#149105 = CARTESIAN_POINT ( 'NONE',  ( 21.14999999999999858, 6.540656951712400691, -167.4999999999999716 ) ) ;
#149104 = AXIS2_PLACEMENT_3D ( 'NONE', #52771, #209291, #187186 ) ;
#149106 = VECTOR ( 'NONE', #105163, 1000.000000000000000 ) ;
#149107 = ORIENTED_EDGE ( 'NONE', *, *, #82862, .T. ) ;
#149108 = CARTESIAN_POINT ( 'NONE',  ( -20.94999999999999929, 65.70729864261004138, -97.56574559737244101 ) ) ;
#149109 = EDGE_CURVE ( 'NONE', #119848, #95340, #203083, .T. ) ;
#149111 = ORIENTED_EDGE ( 'NONE', *, *, #53736, .T. ) ;
#149110 = CARTESIAN_POINT ( 'NONE',  ( 20.94999999999999574, -1.835341550213255957, -112.0551512925630249 ) ) ;
#149112 = DIRECTION ( 'NONE',  ( 1.000000000000000000, 0.000000000000000000, 0.000000000000000000 ) ) ;
#149113 = AXIS2_PLACEMENT_3D ( 'NONE', #58934, #176375, #159370 ) ;
#149114 = CARTESIAN_POINT ( 'NONE',  ( -21.05000000000000071, -11.74999999998884448, -64.10000000000000853 ) ) ;
#149115 = DIRECTION ( 'NONE',  ( 0.000000000000000000, 0.4088369013363205573, -0.9126074666063803686 ) ) ;
#149116 = DIRECTION ( 'NONE',  ( 0.000000000000000000, 0.9651348961777379554, -0.2617529984164210233 ) ) ;
#149118 = ORIENTED_EDGE ( 'NONE', *, *, #9864, .F. ) ;
#149117 = DIRECTION ( 'NONE',  ( -1.000000000000000000, 0.000000000000000000, 0.000000000000000000 ) ) ;
#149120 = CARTESIAN_POINT ( 'NONE',  ( -23.15000000000000213, 81.82295291318693842, -214.8938525951558915 ) ) ;
#149119 =( REPRESENTATION_RELATIONSHIP ('NONE','NONE', #36900, #45219 ) REPRESENTATION_RELATIONSHIP_WITH_TRANSFORMATION ( #190160 )SHAPE_REPRESENTATION_RELATIONSHIP( ) );
#149121 = CARTESIAN_POINT ( 'NONE',  ( 21.07189867249812210, 10.72498027010430377, -179.7124514422767163 ) ) ;
#149122 = DIRECTION ( 'NONE',  ( 7.304098846218134667E-16, -1.000000000000000000, 0.000000000000000000 ) ) ;
#149123 = DIRECTION ( 'NONE',  ( -1.000000000000000000, -1.541880601228652843E-16, -2.878400969107353907E-16 ) ) ;
#149124 = EDGE_CURVE ( 'NONE', #224921, #140287, #236223, .T. ) ;
#149125 = ORIENTED_EDGE ( 'NONE', *, *, #158826, .T. ) ;
#149126 = CARTESIAN_POINT ( 'NONE',  ( -15.75000000000000355, 66.65000000001228386, -153.2731074845243882 ) ) ;
#149127 = ORIENTED_EDGE ( 'NONE', *, *, #89079, .F. ) ;
#149128 = EDGE_CURVE ( 'NONE', #236311, #173065, #145392, .T. ) ;
#149129 = SPHERICAL_SURFACE ( 'NONE', #180092, 0.1000000000000000056 ) ;
#149130 = CIRCLE ( 'NONE', #99191, 0.1000000000000000888 ) ;
#149131 = VERTEX_POINT ( 'NONE', #124567 ) ;
#149132 = DIRECTION ( 'NONE',  ( 0.000000000000000000, 0.000000000000000000, 1.000000000000000000 ) ) ;
#149133 = AXIS2_PLACEMENT_3D ( 'NONE', #44726, #99521, #81249 ) ;
#149134 = ORIENTED_EDGE ( 'NONE', *, *, #184384, .T. ) ;
#149135 = AXIS2_PLACEMENT_3D ( 'NONE', #187486, #169223, #208334 ) ;
#149136 = DIRECTION ( 'NONE',  ( -0.7071067811865456854, 0.6909108974501254608, 0.1504730267678059674 ) ) ;
#149138 = DIRECTION ( 'NONE',  ( 1.000000000000000000, -7.136802563874199107E-16, -1.554319503706929991E-16 ) ) ;
#149137 = AXIS2_PLACEMENT_3D ( 'NONE', #176227, #197033, #255693 ) ;
#149139 = CIRCLE ( 'NONE', #3336, 0.1000000000000054040 ) ;
#149141 = EDGE_CURVE ( 'NONE', #84197, #50827, #140534, .T. ) ;
#149140 =( BOUNDED_SURFACE ( )  B_SPLINE_SURFACE ( 3, 2, ( 
 ( #130490, #108379, #110936 ),
 ( #190503, #186640, #206188 ),
 ( #11866, #210056, #168399 ),
 ( #8001, #109640, #91383 ) ),
 .UNSPECIFIED., .F., .F., .T. ) 
 B_SPLINE_SURFACE_WITH_KNOTS ( ( 4, 4 ),
 ( 3, 3 ),
 ( 0.3000847527772385059, 0.5552748953338751958 ),
 ( 0.000000000000000000, 1.000000000000000000 ),
 .UNSPECIFIED. ) 
 GEOMETRIC_REPRESENTATION_ITEM ( )  RATIONAL_B_SPLINE_SURFACE ( (
 ( 1.000000000000000000, 0.9152888060719408525, 1.000000000000000000),
 ( 1.000000000000000000, 0.9104333467450372863, 1.000000000000000000),
 ( 1.000000000000000000, 0.9035312726220605661, 1.000000000000000000),
 ( 1.000000000000000000, 0.8946697475932182675, 1.000000000000000000) ) ) 
 REPRESENTATION_ITEM ( '' )  SURFACE ( )  );
#149142 = CARTESIAN_POINT ( 'NONE',  ( -18.50000000000000000, 1.162701749949165642, -41.60000000000000142 ) ) ;
#149143 = ORIENTED_EDGE ( 'NONE', *, *, #41375, .T. ) ;
#149144 = CIRCLE ( 'NONE', #182458, 14.30833333333333890 ) ;
#149145 = EDGE_CURVE ( 'NONE', #2330, #36582, #204079, .T. ) ;
#149146 = CARTESIAN_POINT ( 'NONE',  ( -16.84981964351498718, 9.917318234098837948, -12.86960161401949065 ) ) ;
#149147 = CARTESIAN_POINT ( 'NONE',  ( -22.24259225415828567, 7.299257922272452959, -199.3089113299467954 ) ) ;
#149148 = CARTESIAN_POINT ( 'NONE',  ( 12.33938619321247288, 9.360723793986032604, -17.31392719460670193 ) ) ;
#149149 = DIRECTION ( 'NONE',  ( -0.000000000000000000, 0.8660254037844411501, 0.4999999999999956146 ) ) ;
#149150 = LINE ( 'NONE', #106125, #144932 ) ;
#149151 = TOROIDAL_SURFACE ( 'NONE', #211695, 12.77500000000000036, 0.1000000000000000056 ) ;
#149152 = ORIENTED_EDGE ( 'NONE', *, *, #8659, .F. ) ;
#149154 = ORIENTED_EDGE ( 'NONE', *, *, #120034, .F. ) ;
#149153 = CARTESIAN_POINT ( 'NONE',  ( 20.94999675878240808, 10.29307482169070909, -105.9586421466940749 ) ) ;
#149155 = ADVANCED_FACE ( 'NONE', ( #21615 ), #44702, .T. ) ;
#149156 = ORIENTED_EDGE ( 'NONE', *, *, #236818, .F. ) ;
#149157 = CARTESIAN_POINT ( 'NONE',  ( 20.73486653747088582, 7.250000000000026645, -9.250000000000001776 ) ) ;
#149158 = EDGE_LOOP ( 'NONE', ( #196855, #249535, #187782, #28293 ) ) ;
#149159 = DIRECTION ( 'NONE',  ( 1.000000000000000000, -7.304098846218134667E-16, -5.100424963727256530E-30 ) ) ;
#149160 = CARTESIAN_POINT ( 'NONE',  ( 21.07094088545369104, 0.09889370256337753906, -27.17983277808285791 ) ) ;
#149161 = CARTESIAN_POINT ( 'NONE',  ( 23.24999999999999645, 0.000000000000000000, -33.50000000000000000 ) ) ;
#149162 = ORIENTED_EDGE ( 'NONE', *, *, #192345, .F. ) ;
#149163 = ADVANCED_FACE ( 'NONE', ( #2018 ), #82820, .F. ) ;
#149164 = EDGE_CURVE ( 'NONE', #163442, #216204, #177980, .T. ) ;
#149165 = CYLINDRICAL_SURFACE ( 'NONE', #124254, 0.1000000000000028644 ) ;
#149166 = CARTESIAN_POINT ( 'NONE',  ( 22.57320508075687115, 64.25000000001269029, -203.5231074845244166 ) ) ;
#149167 = CARTESIAN_POINT ( 'NONE',  ( -23.15000000000000213, 76.00000000001143974, -38.02310748452432421 ) ) ;
#149168 = ORIENTED_EDGE ( 'NONE', *, *, #168996, .F. ) ;
#149169 = TOROIDAL_SURFACE ( 'NONE', #82466, 0.2000000000000000111, 0.1000000000000000056 ) ;
#149172 = EDGE_LOOP ( 'NONE', ( #220366, #253691, #102754, #133301 ) ) ;
#149171 = PLANE ( 'NONE',  #34271 ) ;
#149170 = B_SPLINE_CURVE_WITH_KNOTS ( 'NONE', 3,
 ( #91631, #188168, #171217, #227281 ),
 .UNSPECIFIED., .F., .F.,
 ( 4, 4 ),
 ( 0.000000000000000000, 0.001767853679387143117 ),
 .UNSPECIFIED. ) ;
#149173 = DIRECTION ( 'NONE',  ( 0.000000000000000000, -0.7071067811865479058, 0.7071067811865472397 ) ) ;
#149174 = VECTOR ( 'NONE', #50525, 1000.000000000000000 ) ;
#149175 = DIRECTION ( 'NONE',  ( 1.000000000000000000, 3.190570557967288949E-16, 6.948722487160392945E-17 ) ) ;
#149176 = VECTOR ( 'NONE', #27598, 1000.000000000000000 ) ;
#149177 = ORIENTED_EDGE ( 'NONE', *, *, #524, .F. ) ;
#149178 = CIRCLE ( 'NONE', #178402, 0.09999999999999799327 ) ;
#149179 = CARTESIAN_POINT ( 'NONE',  ( 21.14999999999999858, 1.115600667400684642E-11, -167.5999999999999659 ) ) ;
#149180 = CARTESIAN_POINT ( 'NONE',  ( -18.41431012584568094, 40.38283566019376281, -235.2953683571930412 ) ) ;
#149181 = CARTESIAN_POINT ( 'NONE',  ( -20.91682497891423154, 18.39833411442327105, -236.9692678682430085 ) ) ;
#149182 = EDGE_LOOP ( 'NONE', ( #255920, #251937, #163242, #201296 ) ) ;
#149183 = FACE_OUTER_BOUND ( 'NONE', #160281, .T. ) ;
#149184 = EDGE_CURVE ( 'NONE', #75595, #218226, #61445, .T. ) ;
#149185 = EDGE_CURVE ( 'NONE', #228315, #25987, #166287, .T. ) ;
#149186 = FACE_OUTER_BOUND ( 'NONE', #18249, .T. ) ;
#149187 = CIRCLE ( 'NONE', #186772, 0.1000000000000028644 ) ;
#149188 = ORIENTED_EDGE ( 'NONE', *, *, #140216, .T. ) ;
#149189 = CIRCLE ( 'NONE', #94989, 0.09999999999999939493 ) ;
#149190 = AXIS2_PLACEMENT_3D ( 'NONE', #130764, #169946, #72095 ) ;
#149191 = EDGE_CURVE ( 'NONE', #116070, #184680, #128084, .T. ) ;
#149192 = AXIS2_PLACEMENT_3D ( 'NONE', #98152, #235141, #236416 ) ;
#149193 = AXIS2_PLACEMENT_3D ( 'NONE', #206026, #109470, #209886 ) ;
#149194 = ORIENTED_EDGE ( 'NONE', *, *, #251064, .T. ) ;
#149195 = LINE ( 'NONE', #90467, #177811 ) ;
#149196 = ORIENTED_EDGE ( 'NONE', *, *, #230159, .T. ) ;
#149197 = FACE_OUTER_BOUND ( 'NONE', #184897, .T. ) ;
#149198 = FACE_OUTER_BOUND ( 'NONE', #157916, .T. ) ;
#149200 = ORIENTED_EDGE ( 'NONE', *, *, #106662, .F. ) ;
#149199 = CARTESIAN_POINT ( 'NONE',  ( 15.15590539855245034, 25.17497023110846044, -232.7237055342689303 ) ) ;
#149201 = DIRECTION ( 'NONE',  ( 0.000000000000000000, 0.000000000000000000, -1.000000000000000000 ) ) ;
#149202 = CARTESIAN_POINT ( 'NONE',  ( 21.07888907270776002, 65.27493078649635549, -57.30191389769120747 ) ) ;
#149203 = LINE ( 'NONE', #252124, #39297 ) ;
#149204 = DIRECTION ( 'NONE',  ( 0.000000000000000000, 0.9126074666063545004, 0.4088369013363783999 ) ) ;
#149205 = FACE_OUTER_BOUND ( 'NONE', #9361, .T. ) ;
#149206 = EDGE_CURVE ( 'NONE', #81995, #26532, #19768, .T. ) ;
#149207 = CARTESIAN_POINT ( 'NONE',  ( -17.11825945287482753, 9.950000000011138823, -79.75000000000005684 ) ) ;
#149208 = DIRECTION ( 'NONE',  ( 0.000000000000000000, 6.982962677686267499E-15, -1.000000000000000000 ) ) ;
#149210 = ORIENTED_EDGE ( 'NONE', *, *, #54077, .T. ) ;
#149209 = CARTESIAN_POINT ( 'NONE',  ( -22.47120815636973745, 75.97109617810814086, -114.6730394732778109 ) ) ;
#149211 = CARTESIAN_POINT ( 'NONE',  ( 20.93284271247462414, 17.11694853917244075, -224.3781540347815735 ) ) ;
#149212 = EDGE_CURVE ( 'NONE', #192399, #87006, #223732, .T. ) ;
#149213 = VECTOR ( 'NONE', #101656, 1000.000000000000000 ) ;
#149215 = EDGE_CURVE ( 'NONE', #80255, #40557, #111420, .T. ) ;
#149214 = CARTESIAN_POINT ( 'NONE',  ( 20.85000000000000142, 6.933893972137497030, -204.7856458343735255 ) ) ;
#149216 = DIRECTION ( 'NONE',  ( 0.000000000000000000, 0.7397360091702755991, -0.6728971962616832059 ) ) ;
#149217 = EDGE_CURVE ( 'NONE', #157514, #11174, #98817, .T. ) ;
#149218 = DIRECTION ( 'NONE',  ( 0.000000000000000000, 0.2128009952263601456, -0.9770955615653316162 ) ) ;
#149219 = CARTESIAN_POINT ( 'NONE',  ( -20.85000000000000142, 0.1610488207187191212, -33.21581015563977957 ) ) ;
#149220 = ADVANCED_FACE ( 'NONE', ( #227496 ), #228807, .F. ) ;
#149221 = ORIENTED_EDGE ( 'NONE', *, *, #251364, .F. ) ;
#149222 = DIRECTION ( 'NONE',  ( -1.000000000000000000, 7.304098846218135653E-16, 4.639676173203994055E-30 ) ) ;
#149223 = CARTESIAN_POINT ( 'NONE',  ( 23.15000000000000213, 82.09643798151613225, -215.4278993322501208 ) ) ;
#149224 = CARTESIAN_POINT ( 'NONE',  ( -20.85000000000000497, 62.84855743180813903, -207.1254202119976640 ) ) ;
#149225 = AXIS2_PLACEMENT_3D ( 'NONE', #30149, #189209, #48396 ) ;
#149226 = AXIS2_PLACEMENT_3D ( 'NONE', #236307, #216740, #117650 ) ;
#149227 = AXIS2_PLACEMENT_3D ( 'NONE', #22938, #179436, #62049 ) ;
#149228 = VERTEX_POINT ( 'NONE', #188380 ) ;
#149230 = ADVANCED_FACE ( 'NONE', ( #106252 ), #47568, .F. ) ;
#149229 = CARTESIAN_POINT ( 'NONE',  ( 21.05000000000000071, 76.00000000001271871, -210.0637644362255685 ) ) ;
#149231 = EDGE_CURVE ( 'NONE', #204085, #65207, #107224, .T. ) ;
#149232 =( BOUNDED_CURVE ( )  B_SPLINE_CURVE ( 3, ( #169769, #167195, #108470, #129317 ),
 .UNSPECIFIED., .F., .F. ) 
 B_SPLINE_CURVE_WITH_KNOTS ( ( 4, 4 ),
 ( 4.336808689942047397E-14, 1.570796326794915432 ),
 .UNSPECIFIED. ) 
 CURVE ( )  GEOMETRIC_REPRESENTATION_ITEM ( )  RATIONAL_B_SPLINE_CURVE ( ( 1.000000000000000000, 0.8047378541243708217, 0.8047378541243708217, 1.000000000000000000 ) ) 
 REPRESENTATION_ITEM ( '' )  );
#149233 = CARTESIAN_POINT ( 'NONE',  ( 18.49999999999999289, 6.650000000011155876, -121.6500000000000341 ) ) ;
#149234 = ORIENTED_EDGE ( 'NONE', *, *, #173188, .F. ) ;
#149235 = DIRECTION ( 'NONE',  ( 0.000000000000000000, 0.000000000000000000, -1.000000000000000000 ) ) ;
#149236 = ORIENTED_EDGE ( 'NONE', *, *, #191646, .T. ) ;
#149237 = EDGE_CURVE ( 'NONE', #231485, #47571, #28146, .T. ) ;
#149238 = FACE_OUTER_BOUND ( 'NONE', #76569, .T. ) ;
#149239 = ORIENTED_EDGE ( 'NONE', *, *, #248273, .F. ) ;
#149240 = PLANE ( 'NONE',  #235723 ) ;
#149241 = CARTESIAN_POINT ( 'NONE',  ( 19.97071067811864609, 64.27928932189387012, -182.1731074845244507 ) ) ;
#149242 = CIRCLE ( 'NONE', #107515, 0.2000000000000111688 ) ;
#149243 = ORIENTED_EDGE ( 'NONE', *, *, #153643, .F. ) ;
#149244 = ORIENTED_EDGE ( 'NONE', *, *, #147418, .F. ) ;
#149246 = DIRECTION ( 'NONE',  ( 0.000000000000000000, 0.9998779222360096863, -0.01562500000001061998 ) ) ;
#149245 = CIRCLE ( 'NONE', #224229, 0.2000000000000057288 ) ;
#149247 = ORIENTED_EDGE ( 'NONE', *, *, #221157, .T. ) ;
#149248 = ADVANCED_FACE ( 'NONE', ( #209223 ), #206664, .F. ) ;
#149249 = CARTESIAN_POINT ( 'NONE',  ( 18.39999999999999503, 65.08943781962308606, -222.1672656287770451 ) ) ;
#149250 = ORIENTED_EDGE ( 'NONE', *, *, #193963, .F. ) ;
#149251 = VECTOR ( 'NONE', #225281, 1000.000000000000000 ) ;
#149252 = ADVANCED_FACE ( 'NONE', ( #167563 ), #185810, .T. ) ;
#149253 = ORIENTED_EDGE ( 'NONE', *, *, #40974, .F. ) ;
#149254 = DIRECTION ( 'NONE',  ( 7.304098846218134667E-16, -1.000000000000000000, 0.000000000000000000 ) ) ;
#149255 = LINE ( 'NONE', #145372, #213607 ) ;
#149257 = EDGE_CURVE ( 'NONE', #131402, #207317, #15685, .T. ) ;
#149256 = CARTESIAN_POINT ( 'NONE',  ( 23.15000000000000213, -3.664072692419559907, -226.4691047342518857 ) ) ;
#149258 = CARTESIAN_POINT ( 'NONE',  ( 23.14999999999999858, 28.32080209959243788, -238.8452605374484676 ) ) ;
#149259 = CARTESIAN_POINT ( 'NONE',  ( -18.41799967126732795, -9.499999999988851584, -74.03206981325584479 ) ) ;
#149260 = ADVANCED_FACE ( 'NONE', ( #147977 ), #9736, .F. ) ;
#149261 = B_SPLINE_CURVE_WITH_KNOTS ( 'NONE', 3,
 ( #57689, #192105, #13456, #235072, #58957, #77256, #194687, #135941 ),
 .UNSPECIFIED., .F., .F.,
 ( 4, 2, 2, 4 ),
 ( 0.000000000000000000, 0.0001094981963948514188, 0.0002189963927897028376, 0.0004379927855794013927 ),
 .UNSPECIFIED. ) ;
#149262 = DIRECTION ( 'NONE',  ( -1.000000000000000000, -0.000000000000000000, 0.000000000000000000 ) ) ;
#149263 = ORIENTED_EDGE ( 'NONE', *, *, #75747, .T. ) ;
#149264 = CARTESIAN_POINT ( 'NONE',  ( -18.59999999999999787, -1.162701749926853712, -75.10000000000003695 ) ) ;
#149265 = DIRECTION ( 'NONE',  ( 0.000000000000000000, 1.000000000000000000, -1.224646799147353207E-16 ) ) ;
#149266 = CARTESIAN_POINT ( 'NONE',  ( -18.50000000000000000, 70.05000000001267324, -193.2174051794895320 ) ) ;
#149267 = DIRECTION ( 'NONE',  ( 0.000000000000000000, 0.1686199900910313187, -0.9856811345164828708 ) ) ;
#149268 = MECHANICAL_DESIGN_GEOMETRIC_PRESENTATION_REPRESENTATION (  '', ( #120252 ), #103426 ) ;
#149269 = EDGE_LOOP ( 'NONE', ( #196263, #172405, #115553, #206015 ) ) ;
#149270 = CARTESIAN_POINT ( 'NONE',  ( -18.69999999999999929, -10.74999999999999289, 32.89999999999999858 ) ) ;
#149271 = EDGE_LOOP ( 'NONE', ( #26095, #251565, #36668, #212905 ) ) ;
#149272 = CARTESIAN_POINT ( 'NONE',  ( -18.50000000000000355, -7.567701079425762423, -210.0537230116848377 ) ) ;
#149273 = AXIS2_PLACEMENT_3D ( 'NONE', #132927, #151204, #134183 ) ;
#149274 = VERTEX_POINT ( 'NONE', #71029 ) ;
#149275 = VECTOR ( 'NONE', #228004, 1000.000000000000000 ) ;
#149276 = FACE_OUTER_BOUND ( 'NONE', #219855, .T. ) ;
#149277 = LINE ( 'NONE', #68441, #89712 ) ;
#149278 = ORIENTED_EDGE ( 'NONE', *, *, #58547, .F. ) ;
#149279 = ORIENTED_EDGE ( 'NONE', *, *, #54973, .F. ) ;
#149281 = EDGE_LOOP ( 'NONE', ( #222430, #56638, #227334, #210899, #155673, #154773, #249158, #246723 ) ) ;
#149280 = CARTESIAN_POINT ( 'NONE',  ( -22.50000000000000000, 1.115600667400684642E-11, -33.50000000000000000 ) ) ;
#149282 = EDGE_CURVE ( 'NONE', #146074, #197727, #248891, .T. ) ;
#149283 = DIRECTION ( 'NONE',  ( -6.938893903907222856E-15, 1.000000000000000000, 2.891205793294679805E-16 ) ) ;
#149284 = ORIENTED_EDGE ( 'NONE', *, *, #239019, .F. ) ;
#149285 = VECTOR ( 'NONE', #40749, 1000.000000000000000 ) ;
#149286 = CARTESIAN_POINT ( 'NONE',  ( -21.44999999999999929, 68.85000000001156195, -57.17310748452437252 ) ) ;
#149287 = CYLINDRICAL_SURFACE ( 'NONE', #164718, 3.999999999999996447 ) ;
#149289 = ORIENTED_EDGE ( 'NONE', *, *, #142725, .F. ) ;
#149288 = EDGE_CURVE ( 'NONE', #174236, #248548, #130979, .T. ) ;
#149290 = DIRECTION ( 'NONE',  ( 0.000000000000000000, -1.734723475983068283E-15, 1.000000000000000000 ) ) ;
#149291 = FACE_OUTER_BOUND ( 'NONE', #62512, .T. ) ;
#149292 = AXIS2_PLACEMENT_3D ( 'NONE', #82163, #99165, #178771 ) ;
#149294 = EDGE_LOOP ( 'NONE', ( #97904, #115783, #87951 ) ) ;
#149293 = AXIS2_PLACEMENT_3D ( 'NONE', #183182, #222259, #20251 ) ;
#149296 = CARTESIAN_POINT ( 'NONE',  ( 18.59999999999999787, 85.40000000001208491, -129.6410656363516125 ) ) ;
#149295 = AXIS2_PLACEMENT_3D ( 'NONE', #224452, #125370, #103207 ) ;
#149297 = EDGE_CURVE ( 'NONE', #16537, #78455, #72304, .T. ) ;
#149298 = DIRECTION ( 'NONE',  ( 0.000000000000000000, 0.000000000000000000, -1.000000000000000000 ) ) ;
#149299 = DIRECTION ( 'NONE',  ( 0.000000000000000000, -0.9968797965484670343, -0.07893460099023182075 ) ) ;
#149301 = VERTEX_POINT ( 'NONE', #54005 ) ;
#149300 = DIRECTION ( 'NONE',  ( -0.000000000000000000, -6.982962677686266711E-15, 1.000000000000000000 ) ) ;
#149303 = AXIS2_PLACEMENT_3D ( 'NONE', #236008, #211323, #53526 ) ;
#149302 = FACE_OUTER_BOUND ( 'NONE', #128677, .T. ) ;
#149304 = CARTESIAN_POINT ( 'NONE',  ( -20.94999999999999929, 0.6656436123793491033, -212.6810495496487476 ) ) ;
#149305 = SPHERICAL_SURFACE ( 'NONE', #165210, 0.1000000000000000056 ) ;
#149306 = CARTESIAN_POINT ( 'NONE',  ( -23.15000000000000213, 1.115600667400684642E-11, -121.1250000000000426 ) ) ;
#149307 = DIRECTION ( 'NONE',  ( 1.000000000000000000, -0.000000000000000000, -0.000000000000000000 ) ) ;
#149308 = DIRECTION ( 'NONE',  ( -0.5932847527679299127, -0.8049926720990051576, -6.257843056355997642E-15 ) ) ;
#149309 = VECTOR ( 'NONE', #150123, 1000.000000000000000 ) ;
#149310 = CARTESIAN_POINT ( 'NONE',  ( -23.25000000000000000, 80.80934863333322937, -192.8037999715871535 ) ) ;
#149311 = EDGE_CURVE ( 'NONE', #75851, #61384, #24048, .T. ) ;
#149312 = CARTESIAN_POINT ( 'NONE',  ( -20.94999999999999929, 77.85102823015292017, -124.8691942151017855 ) ) ;
#149313 = ORIENTED_EDGE ( 'NONE', *, *, #187938, .T. ) ;
#149314 = VECTOR ( 'NONE', #182023, 1000.000000000000000 ) ;
#149315 = AXIS2_PLACEMENT_3D ( 'NONE', #112239, #49676, #54800 ) ;
#149316 = AXIS2_PLACEMENT_3D ( 'NONE', #152564, #229508, #91281 ) ;
#149317 = TOROIDAL_SURFACE ( 'NONE', #91040, 11.65000000000000036, 0.1000000000000000056 ) ;
#149318 = ORIENTED_EDGE ( 'NONE', *, *, #31914, .T. ) ;
#149319 = ORIENTED_EDGE ( 'NONE', *, *, #93560, .T. ) ;
#149320 = VECTOR ( 'NONE', #72332, 1000.000000000000000 ) ;
#149321 = CARTESIAN_POINT ( 'NONE',  ( -20.94999999999999929, -11.29603075032412640, -63.95210084033612929 ) ) ;
#149322 = DIRECTION ( 'NONE',  ( -1.000000000000000000, 0.000000000000000000, 0.000000000000000000 ) ) ;
#149323 = ORIENTED_EDGE ( 'NONE', *, *, #19898, .F. ) ;
#149324 = FACE_OUTER_BOUND ( 'NONE', #133563, .T. ) ;
#149325 = CARTESIAN_POINT ( 'NONE',  ( -14.00000000000000178, 26.54497872210690090, -232.9592037335782209 ) ) ;
#149326 = PRODUCT ( 'Snap Open Cable Crossbars ', 'Snap Open Cable Crossbars ', '', ( #18241 ) ) ;
#149327 = DIRECTION ( 'NONE',  ( -1.000000000000000000, -7.304098846218134667E-16, -5.311601492717084346E-30 ) ) ;
#149328 = VERTEX_POINT ( 'NONE', #235217 ) ;
#149329 = CIRCLE ( 'NONE', #65918, 0.09999999999998898659 ) ;
#149330 = AXIS2_PLACEMENT_3D ( 'NONE', #167082, #191779, #189187 ) ;
#149331 = EDGE_LOOP ( 'NONE', ( #59764, #94684, #22053, #78350, #205071, #177834, #233932, #35429, #72121, #20761, #226562, #250749, #12828, #44828, #248481, #173313, #98096, #116064, #103034, #65705, #129162, #171955, #32040 ) ) ;
#149332 = CARTESIAN_POINT ( 'NONE',  ( 23.24999999999999289, 9.083217576421224848, -211.4565844547649931 ) ) ;
#149333 = CARTESIAN_POINT ( 'NONE',  ( 23.24999999999999645, 9.374458193048763377, -220.5475659691911119 ) ) ;
#149334 = ORIENTED_EDGE ( 'NONE', *, *, #1584, .F. ) ;
#149335 = B_SPLINE_CURVE_WITH_KNOTS ( 'NONE', 3,
 ( #158119, #21160, #257117, #100625, #61542, #240190 ),
 .UNSPECIFIED., .F., .F.,
 ( 4, 2, 4 ),
 ( 0.000000000000000000, 0.0001497467027049230307, 0.0002994934054098460615 ),
 .UNSPECIFIED. ) ;
#149336 = SPHERICAL_SURFACE ( 'NONE', #141049, 0.1000000000000000056 ) ;
#149338 = ORIENTED_EDGE ( 'NONE', *, *, #165111, .F. ) ;
#149337 = DIRECTION ( 'NONE',  ( 0.000000000000000000, 0.9651348961777148627, -0.2617529984165062329 ) ) ;
#149339 = FACE_OUTER_BOUND ( 'NONE', #204041, .T. ) ;
#149340 = CYLINDRICAL_SURFACE ( 'NONE', #58984, 0.09999999999999939493 ) ;
#149342 = ORIENTED_EDGE ( 'NONE', *, *, #222018, .T. ) ;
#149341 = DIRECTION ( 'NONE',  ( 0.000000000000000000, -1.000000000000000000, -6.982962677686266711E-15 ) ) ;
#149343 = AXIS2_PLACEMENT_3D ( 'NONE', #162217, #65649, #5651 ) ;
#149344 = CARTESIAN_POINT ( 'NONE',  ( -18.40000000000000213, 30.85877660472528916, -233.5890472672530507 ) ) ;
#149345 = CARTESIAN_POINT ( 'NONE',  ( -16.86133551771148831, 9.950000000011137047, -87.80134343454673740 ) ) ;
#149346 = EDGE_CURVE ( 'NONE', #32118, #132728, #65721, .T. ) ;
#149347 = DIRECTION ( 'NONE',  ( 0.000000000000000000, 0.000000000000000000, -1.000000000000000000 ) ) ;
#149348 = AXIS2_PLACEMENT_3D ( 'NONE', #33607, #140009, #219554 ) ;
#149349 = LINE ( 'NONE', #228863, #223264 ) ;
#149351 = DIRECTION ( 'NONE',  ( 0.000000000000000000, 0.8660254037844419273, -0.4999999999999942824 ) ) ;
#149350 = FACE_OUTER_BOUND ( 'NONE', #219860, .T. ) ;
#149352 = CARTESIAN_POINT ( 'NONE',  ( 18.49999999999999289, 10.25000000001115730, -91.65000000000003411 ) ) ;
#149353 = AXIS2_PLACEMENT_3D ( 'NONE', #211030, #191493, #166797 ) ;
#149354 = CARTESIAN_POINT ( 'NONE',  ( 23.24999999999999289, 11.75000000001116263, -134.1000000000000227 ) ) ;
#149355 = DIRECTION ( 'NONE',  ( 0.000000000000000000, 0.000000000000000000, 1.000000000000000000 ) ) ;
#149356 = CARTESIAN_POINT ( 'NONE',  ( 21.05000000000000071, 76.00000000001193712, -107.1231074845243114 ) ) ;
#149357 = ORIENTED_EDGE ( 'NONE', *, *, #163792, .T. ) ;
#149359 = EDGE_LOOP ( 'NONE', ( #248506, #10492, #140580, #27729 ) ) ;
#149358 = VECTOR ( 'NONE', #48293, 1000.000000000000227 ) ;
#149360 = DIRECTION ( 'NONE',  ( 0.000000000000000000, 6.982962677686266711E-15, -1.000000000000000000 ) ) ;
#149361 = VERTEX_POINT ( 'NONE', #98226 ) ;
#149362 = DIRECTION ( 'NONE',  ( -1.000000000000000000, -7.304098846218135653E-16, 4.607487905232624742E-31 ) ) ;
#149363 = ORIENTED_EDGE ( 'NONE', *, *, #248684, .F. ) ;
#149364 = EDGE_CURVE ( 'NONE', #43405, #54821, #214365, .T. ) ;
#149365 = CYLINDRICAL_SURFACE ( 'NONE', #81793, 0.09999999999999939493 ) ;
#149366 = VECTOR ( 'NONE', #187842, 1000.000000000000000 ) ;
#149367 = ADVANCED_FACE ( 'NONE', ( #34478 ), #253148, .T. ) ;
#149368 = AXIS2_PLACEMENT_3D ( 'NONE', #217032, #121820, #100906 ) ;
#149369 = AXIS2_PLACEMENT_3D ( 'NONE', #75026, #134934, #73735 ) ;
#149370 = VERTEX_POINT ( 'NONE', #252192 ) ;
#149371 = CIRCLE ( 'NONE', #16104, 4.049999999999998934 ) ;
#149372 = DIRECTION ( 'NONE',  ( 0.000000000000000000, 0.9126074666063660468, 0.4088369013363524762 ) ) ;
#149373 = EDGE_CURVE ( 'NONE', #158624, #136985, #82435, .T. ) ;
#149374 = ORIENTED_EDGE ( 'NONE', *, *, #127393, .T. ) ;
#149375 = EDGE_LOOP ( 'NONE', ( #37514, #104312, #70221, #81313 ) ) ;
#149376 = VERTEX_POINT ( 'NONE', #116554 ) ;
#149377 = ADVANCED_FACE ( 'NONE', ( #94409 ), #33207, .F. ) ;
#149378 = CARTESIAN_POINT ( 'NONE',  ( -20.15000000000000568, 63.79987548357193816, -213.0104660527734382 ) ) ;
#149379 = CARTESIAN_POINT ( 'NONE',  ( 20.95595624212412744, 10.62389120310530544, -41.12963291412692257 ) ) ;
#149380 = DIRECTION ( 'NONE',  ( 0.000000000000000000, 0.000000000000000000, -1.000000000000000000 ) ) ;
#149382 = EDGE_CURVE ( 'NONE', #92185, #166165, #60745, .T. ) ;
#149381 = SPHERICAL_SURFACE ( 'NONE', #240385, 0.1000000000000000056 ) ;
#149383 = CARTESIAN_POINT ( 'NONE',  ( -23.25000000000000000, 64.35000000001222986, -148.2731074845243882 ) ) ;
#149385 = CARTESIAN_POINT ( 'NONE',  ( 22.39999999999999503, 11.65000000000000746, 0.09999999999999592548 ) ) ;
#149384 = SPHERICAL_SURFACE ( 'NONE', #87286, 0.1000000000000000056 ) ;
#149386 = CARTESIAN_POINT ( 'NONE',  ( -15.70407651835961005, 9.355806591641286474, -83.29110253154621546 ) ) ;
#149388 = ORIENTED_EDGE ( 'NONE', *, *, #250120, .T. ) ;
#149387 = DIRECTION ( 'NONE',  ( 1.000000000000000000, 2.986185139342073343E-16, -6.665775143889692774E-16 ) ) ;
#149390 = CARTESIAN_POINT ( 'NONE',  ( -20.94999999999999929, 10.29270135741298731, -72.45736188715193293 ) ) ;
#149389 = CARTESIAN_POINT ( 'NONE',  ( 20.21494484322224849, 9.303170737879936425, -75.34026519177028547 ) ) ;
#149391 = EDGE_CURVE ( 'NONE', #232261, #17815, #35756, .T. ) ;
#149392 = FACE_OUTER_BOUND ( 'NONE', #95002, .T. ) ;
#149393 = ORIENTED_EDGE ( 'NONE', *, *, #57890, .F. ) ;
#149394 = CARTESIAN_POINT ( 'NONE',  ( 19.58285714285715073, 10.38499851035142107, -7.629684667389950548 ) ) ;
#149395 = AXIS2_PLACEMENT_3D ( 'NONE', #119661, #195360, #158803 ) ;
#149396 = CARTESIAN_POINT ( 'NONE',  ( 23.14999999999999503, 56.45527679911575802, -225.2871936083021467 ) ) ;
#149397 = DIRECTION ( 'NONE',  ( 0.000000000000000000, -1.000000000000000000, 0.000000000000000000 ) ) ;
#149398 = VERTEX_POINT ( 'NONE', #233929 ) ;
#149399 = EDGE_CURVE ( 'NONE', #217170, #63340, #211468, .T. ) ;
#149400 = CARTESIAN_POINT ( 'NONE',  ( 20.85000000000000142, 76.00000000001126921, -203.5231074845248997 ) ) ;
#149401 = DIRECTION ( 'NONE',  ( 1.000000000000000000, 7.049440681616512959E-16, -1.911869773728117674E-16 ) ) ;
#149402 = ORIENTED_EDGE ( 'NONE', *, *, #111961, .T. ) ;
#149403 = EDGE_LOOP ( 'NONE', ( #72776, #201082, #228031, #16705 ) ) ;
#149404 = DIRECTION ( 'NONE',  ( -1.000000000000000000, 0.000000000000000000, 0.000000000000000000 ) ) ;
#149405 = CARTESIAN_POINT ( 'NONE',  ( -18.52643265882458579, 10.31973158071402530, -173.0505334713354841 ) ) ;
#149406 = FACE_OUTER_BOUND ( 'NONE', #90638, .T. ) ;
#149407 = CARTESIAN_POINT ( 'NONE',  ( -21.05000000000000071, -1.162701749926853712, -142.1000000000000227 ) ) ;
#149408 = VERTEX_POINT ( 'NONE', #112703 ) ;
#149409 = EDGE_CURVE ( 'NONE', #137027, #145382, #232338, .T. ) ;
#149410 = CARTESIAN_POINT ( 'NONE',  ( -14.22969084473440304, 9.456007326080463571, -118.9886334941467823 ) ) ;
#149411 = CARTESIAN_POINT ( 'NONE',  ( 18.59999999999999787, 77.83534155023700407, -191.9679561919613491 ) ) ;
#149412 = CARTESIAN_POINT ( 'NONE',  ( -22.39999999999999858, 12.71802988599559292, -223.5105008658000258 ) ) ;
#149413 = AXIS2_PLACEMENT_3D ( 'NONE', #37855, #234748, #56082 ) ;
#149414 = FACE_OUTER_BOUND ( 'NONE', #122900, .T. ) ;
#149415 = AXIS2_PLACEMENT_3D ( 'NONE', #29179, #89100, #133377 ) ;
#149416 = ORIENTED_EDGE ( 'NONE', *, *, #36456, .F. ) ;
#149417 = EDGE_CURVE ( 'NONE', #40045, #108024, #132344, .T. ) ;
#149419 = ORIENTED_EDGE ( 'NONE', *, *, #139381, .T. ) ;
#149418 = CARTESIAN_POINT ( 'NONE',  ( -18.50000000000000000, 0.000000000000000000, 0.000000000000000000 ) ) ;
#149420 = CIRCLE ( 'NONE', #61917, 4.300000000000025580 ) ;
#149421 = CARTESIAN_POINT ( 'NONE',  ( -23.25000000000000000, 64.25000000001260503, -191.3731074845244393 ) ) ;
#149422 = FACE_OUTER_BOUND ( 'NONE', #255263, .T. ) ;
#149423 = DIRECTION ( 'NONE',  ( 3.469446951953635015E-14, 6.982962677686266711E-15, -1.000000000000000000 ) ) ;
#149424 = DIRECTION ( 'NONE',  ( 0.000000000000000000, 1.000000000000000000, 0.000000000000000000 ) ) ;
#149425 = DIRECTION ( 'NONE',  ( -1.000000000000000000, 0.000000000000000000, 0.000000000000000000 ) ) ;
#149426 = FACE_OUTER_BOUND ( 'NONE', #121085, .T. ) ;
#149427 = SPHERICAL_SURFACE ( 'NONE', #177945, 0.1000000000000000056 ) ;
#149428 = EDGE_LOOP ( 'NONE', ( #1758, #231759, #127638, #45886 ) ) ;
#149429 = CARTESIAN_POINT ( 'NONE',  ( 23.24999999999999289, 64.35000000001254250, -182.1731074845244507 ) ) ;
#149430 = CARTESIAN_POINT ( 'NONE',  ( 20.85000000000000142, 1.115600667400684642E-11, -200.9999999999999432 ) ) ;
#149431 = DIRECTION ( 'NONE',  ( -0.000000000000000000, 0.1335171055202867274, -0.9910465087640865089 ) ) ;
#149432 = AXIS2_PLACEMENT_3D ( 'NONE', #56526, #14886, #156969 ) ;
#149433 = AXIS2_PLACEMENT_3D ( 'NONE', #31352, #109547, #151277 ) ;
#149434 = DIRECTION ( 'NONE',  ( -0.000000000000000000, 0.000000000000000000, 1.000000000000000000 ) ) ;
#149435 = AXIS2_PLACEMENT_3D ( 'NONE', #151092, #51959, #131517 ) ;
#149436 = EDGE_CURVE ( 'NONE', #215091, #197810, #111508, .T. ) ;
#149437 = CARTESIAN_POINT ( 'NONE',  ( -20.64999999999999858, 71.65000000001199965, -115.3731074845243256 ) ) ;
#149438 = EDGE_CURVE ( 'NONE', #227124, #21586, #219828, .T. ) ;
#149439 = CARTESIAN_POINT ( 'NONE',  ( 12.84435279558020859, 9.410708747058238899, -185.5692084058441083 ) ) ;
#149440 = CIRCLE ( 'NONE', #87025, 0.09999999999999939493 ) ;
#149441 = ORIENTED_EDGE ( 'NONE', *, *, #103030, .T. ) ;
#149442 = ORIENTED_EDGE ( 'NONE', *, *, #88298, .F. ) ;
#149443 = CYLINDRICAL_SURFACE ( 'NONE', #180143, 0.4999999999999944489 ) ;
#149444 = DIRECTION ( 'NONE',  ( 1.000000000000000000, 0.000000000000000000, 0.000000000000000000 ) ) ;
#149445 = CARTESIAN_POINT ( 'NONE',  ( -18.59999999999999787, 68.92903212821357783, -166.2765432626560766 ) ) ;
#149446 = ADVANCED_FACE ( 'NONE', ( #155709 ), #161610, .F. ) ;
#149447 = CARTESIAN_POINT ( 'NONE',  ( -11.60000000000000320, -8.350000000000004974, 10.95857864376268864 ) ) ;
#149448 = DIRECTION ( 'NONE',  ( 0.000000000000000000, 0.4088369013363281623, -0.9126074666063771490 ) ) ;
#149449 = EDGE_CURVE ( 'NONE', #135040, #206383, #28344, .T. ) ;
#149451 = EDGE_CURVE ( 'NONE', #3745, #73958, #154112, .T. ) ;
#149450 = DIRECTION ( 'NONE',  ( 0.000000000000000000, -7.056502275159890832E-15, 1.000000000000000000 ) ) ;
#149452 = SPHERICAL_SURFACE ( 'NONE', #232982, 0.1000000000000000056 ) ;
#149453 = CIRCLE ( 'NONE', #174433, 11.75000000000001066 ) ;
#149455 = DIRECTION ( 'NONE',  ( -3.265361837132813093E-16, -0.4088369013363281068, 0.9126074666063770380 ) ) ;
#149454 = TOROIDAL_SURFACE ( 'NONE', #182770, 0.2000000000000000111, 0.1000000000000000056 ) ;
#149456 = EDGE_LOOP ( 'NONE', ( #128306, #225403, #248563, #131218 ) ) ;
#149457 = FACE_OUTER_BOUND ( 'NONE', #95146, .T. ) ;
#149458 = EDGE_CURVE ( 'NONE', #232107, #225466, #61714, .T. ) ;
#149459 = ORIENTED_EDGE ( 'NONE', *, *, #69070, .T. ) ;
#149460 = DIRECTION ( 'NONE',  ( 0.000000000000000000, 0.000000000000000000, -1.000000000000000000 ) ) ;
#149461 = CIRCLE ( 'NONE', #166034, 0.09999999999998807065 ) ;
#149462 = LINE ( 'NONE', #210693, #166027 ) ;
#149463 = DIRECTION ( 'NONE',  ( -0.4999999999999799050, 0.000000000000000000, -0.8660254037844502539 ) ) ;
#149464 = CARTESIAN_POINT ( 'NONE',  ( 21.05000000000000071, 1.115600667400684642E-11, -33.50000000000000000 ) ) ;
#149465 = CARTESIAN_POINT ( 'NONE',  ( -18.59999999999999787, 11.65000000001115232, -54.85000000000000142 ) ) ;
#149466 = DIRECTION ( 'NONE',  ( 0.000000000000000000, 0.2617529984165031243, 0.9651348961777157509 ) ) ;
#149467 = ORIENTED_EDGE ( 'NONE', *, *, #2294, .T. ) ;
#149468 = DIRECTION ( 'NONE',  ( 1.000000000000000000, 0.000000000000000000, 0.000000000000000000 ) ) ;
#149469 = DIRECTION ( 'NONE',  ( 1.000000000000000000, 0.000000000000000000, -0.000000000000000000 ) ) ;
#149470 = DIRECTION ( 'NONE',  ( 0.000000000000000000, 0.000000000000000000, -1.000000000000000000 ) ) ;
#149471 = CARTESIAN_POINT ( 'NONE',  ( 21.05000000000000071, 87.48912529308798014, -99.92310748452423752 ) ) ;
#149472 = VECTOR ( 'NONE', #181946, 1000.000000000000000 ) ;
#149473 = VECTOR ( 'NONE', #108318, 1000.000000000000227 ) ;
#149474 = VECTOR ( 'NONE', #245082, 1000.000000000000000 ) ;
#149475 = CARTESIAN_POINT ( 'NONE',  ( 18.39999999999999503, 11.47316190336248454, -20.85000000000000142 ) ) ;
#149476 = AXIS2_PLACEMENT_3D ( 'NONE', #59922, #139469, #199480 ) ;
#149477 = ORIENTED_EDGE ( 'NONE', *, *, #77889, .F. ) ;
#149478 = DIRECTION ( 'NONE',  ( 0.000000000000000000, 0.000000000000000000, -1.000000000000000000 ) ) ;
#149479 = CARTESIAN_POINT ( 'NONE',  ( -18.40000000000000213, 11.47316190337364183, -154.8914213562373448 ) ) ;
#149480 = EDGE_LOOP ( 'NONE', ( #37265, #202495, #61752, #40543 ) ) ;
#149481 = ADVANCED_FACE ( 'NONE', ( #59104 ), #115788, .T. ) ;
#149482 = EDGE_CURVE ( 'NONE', #154908, #143756, #54271, .T. ) ;
#149483 = ORIENTED_EDGE ( 'NONE', *, *, #109540, .F. ) ;
#149484 = CYLINDRICAL_SURFACE ( 'NONE', #72329, 0.09999999999998898659 ) ;
#149485 = DIRECTION ( 'NONE',  ( -1.000000000000000000, 0.000000000000000000, 0.000000000000000000 ) ) ;
#149486 = CONICAL_SURFACE ( 'NONE', #253499, 7.750000000000033751, 0.7853981633974531640 ) ;
#149487 = VECTOR ( 'NONE', #50630, 1000.000000000000000 ) ;
#149488 = ORIENTED_EDGE ( 'NONE', *, *, #8485, .F. ) ;
#149489 = DIRECTION ( 'NONE',  ( 0.000000000000000000, 0.000000000000000000, 1.000000000000000000 ) ) ;
#149490 = FACE_OUTER_BOUND ( 'NONE', #214886, .T. ) ;
#149491 = EDGE_CURVE ( 'NONE', #136008, #222564, #198987, .T. ) ;
#149492 = VECTOR ( 'NONE', #66405, 1000.000000000000000 ) ;
#149493 = ORIENTED_EDGE ( 'NONE', *, *, #198651, .T. ) ;
#149494 = AXIS2_PLACEMENT_3D ( 'NONE', #14350, #112159, #169592 ) ;
#149495 = TOROIDAL_SURFACE ( 'NONE', #220228, 11.65000000000000036, 0.1000000000000000056 ) ;
#149496 = VECTOR ( 'NONE', #112122, 1000.000000000000000 ) ;
#149497 = CARTESIAN_POINT ( 'NONE',  ( -20.54999999999999716, -9.499999999988846255, -57.10603087734755690 ) ) ;
#149498 = ORIENTED_EDGE ( 'NONE', *, *, #31614, .T. ) ;
#149499 = DIRECTION ( 'NONE',  ( 0.000000000000000000, 0.000000000000000000, -1.000000000000000000 ) ) ;
#149500 = VECTOR ( 'NONE', #176568, 1000.000000000000000 ) ;
#149501 = CARTESIAN_POINT ( 'NONE',  ( -11.59999999999994458, 64.35000000001120668, -18.42310748452479174 ) ) ;
#149503 = ORIENTED_EDGE ( 'NONE', *, *, #129343, .T. ) ;
#149502 = FACE_OUTER_BOUND ( 'NONE', #255510, .T. ) ;
#149504 = FACE_OUTER_BOUND ( 'NONE', #166750, .T. ) ;
#149506 = UNCERTAINTY_MEASURE_WITH_UNIT (LENGTH_MEASURE( 1.000000000000000082E-05 ), #59879, 'distance_accuracy_value', 'NONE');
#149505 = CARTESIAN_POINT ( 'NONE',  ( 21.05000000000000071, 68.16863917788211324, -213.8681745540812926 ) ) ;
#149507 = CARTESIAN_POINT ( 'NONE',  ( -23.49999999999994316, 74.16448838626247664, -47.52760213295649550 ) ) ;
#149508 = CARTESIAN_POINT ( 'NONE',  ( 18.79999999999999361, -11.75000000000000000, 32.89999999999999858 ) ) ;
#149509 = DIRECTION ( 'NONE',  ( 0.000000000000000000, 0.000000000000000000, 1.000000000000000000 ) ) ;
#149510 = CARTESIAN_POINT ( 'NONE',  ( -21.05000000000000071, -1.162701749926853712, -142.0000000000000284 ) ) ;
#149512 = ORIENTED_EDGE ( 'NONE', *, *, #50415, .T. ) ;
#149511 = CARTESIAN_POINT ( 'NONE',  ( -18.39999999999999858, 85.60000000001240039, -163.3229180933022633 ) ) ;
#149513 = EDGE_LOOP ( 'NONE', ( #183890, #47558, #152301, #103546 ) ) ;
#149515 = CARTESIAN_POINT ( 'NONE',  ( -12.68215100488889924, 9.396630376328870327, -84.90705739281833075 ) ) ;
#149514 = CARTESIAN_POINT ( 'NONE',  ( -22.16821283564876666, 68.44102665923088580, -69.52310748452437394 ) ) ;
#149517 = ORIENTED_EDGE ( 'NONE', *, *, #170301, .T. ) ;
#149516 = DIRECTION ( 'NONE',  ( 0.000000000000000000, 0.000000000000000000, -1.000000000000000000 ) ) ;
#149518 = EDGE_CURVE ( 'NONE', #56940, #232936, #4287, .T. ) ;
#149519 = VERTEX_POINT ( 'NONE', #79955 ) ;
#149520 = PRESENTATION_LAYER_ASSIGNMENT (  '', '', ( #191221 ) ) ;
#149521 = DIRECTION ( 'NONE',  ( 0.000000000000000000, -0.9651348961777155289, 0.2617529984165036794 ) ) ;
#149522 = DIRECTION ( 'NONE',  ( 1.000000000000000000, 0.000000000000000000, 0.000000000000000000 ) ) ;
#149523 = CARTESIAN_POINT ( 'NONE',  ( 23.40000000000005542, 64.35000000001120668, -3.023107484524792277 ) ) ;
#149524 = ADVANCED_FACE ( 'NONE', ( #122983 ), #153235, .T. ) ;
#149525 = CARTESIAN_POINT ( 'NONE',  ( 21.14999999999999858, -11.74999999998884448, -45.75000000000000711 ) ) ;
#149526 = LINE ( 'NONE', #106495, #140504 ) ;
#149527 = CIRCLE ( 'NONE', #78747, 0.2000000000000122791 ) ;
#149528 = EDGE_CURVE ( 'NONE', #148316, #255690, #25176, .T. ) ;
#149529 = VECTOR ( 'NONE', #86286, 1000.000000000000000 ) ;
#149530 = DIRECTION ( 'NONE',  ( 0.000000000000000000, -1.000000000000000000, -6.982962677686265922E-15 ) ) ;
#149531 = ORIENTED_EDGE ( 'NONE', *, *, #150307, .F. ) ;
#149532 = VERTEX_POINT ( 'NONE', #62989 ) ;
#149533 = ADVANCED_FACE ( 'NONE', ( #218191 ), #201215, .T. ) ;
#149534 = CARTESIAN_POINT ( 'NONE',  ( -22.39999999999999858, 7.790779598373403836, 0.09999999999999939493 ) ) ;
#149535 = AXIS2_PLACEMENT_3D ( 'NONE', #182171, #100022, #120934 ) ;
#149536 = ORIENTED_EDGE ( 'NONE', *, *, #207365, .T. ) ;
#149537 = CARTESIAN_POINT ( 'NONE',  ( 20.12500000000000355, 65.75804927292965374, -162.1629037574383290 ) ) ;
#149538 = ORIENTED_EDGE ( 'NONE', *, *, #89592, .F. ) ;
#149539 = CYLINDRICAL_SURFACE ( 'NONE', #39340, 0.1000000000000118433 ) ;
#149540 = CIRCLE ( 'NONE', #37113, 0.09999999999999939493 ) ;
#149541 = ADVANCED_FACE ( 'NONE', ( #60415 ), #242908, .T. ) ;
#149543 = ADVANCED_FACE ( 'NONE', ( #181670 ), #74129, .F. ) ;
#149542 = EDGE_CURVE ( 'NONE', #184002, #32289, #160836, .T. ) ;
#149544 = CARTESIAN_POINT ( 'NONE',  ( -16.89268316805466341, 9.951721813253341153, -79.64424752145448849 ) ) ;
#149545 = DIRECTION ( 'NONE',  ( 0.000000000000000000, 0.000000000000000000, 1.000000000000000000 ) ) ;
#149546 = ORIENTED_EDGE ( 'NONE', *, *, #105900, .T. ) ;
#149547 = FACE_OUTER_BOUND ( 'NONE', #180500, .T. ) ;
#149548 = VERTEX_POINT ( 'NONE', #3001 ) ;
#149549 = CARTESIAN_POINT ( 'NONE',  ( -16.97683809663752186, 66.05000000001155058, -49.42547150272071121 ) ) ;
#149550 = AXIS2_PLACEMENT_3D ( 'NONE', #247551, #168056, #188856 ) ;
#149551 = CARTESIAN_POINT ( 'NONE',  ( -16.88593481969334320, 9.950560090095466492, -87.85187225694454582 ) ) ;
#149552 = DIRECTION ( 'NONE',  ( 0.000000000000000000, -0.1575844902526687130, -0.9875055080513762684 ) ) ;
#149553 = VECTOR ( 'NONE', #29028, 1000.000000000000000 ) ;
#149554 = EDGE_LOOP ( 'NONE', ( #62165, #159935, #154968 ) ) ;
#149555 = LINE ( 'NONE', #129943, #19444 ) ;
#149556 = VERTEX_POINT ( 'NONE', #162116 ) ;
#149559 = ORIENTED_EDGE ( 'NONE', *, *, #57006, .T. ) ;
#149558 = DIRECTION ( 'NONE',  ( 1.000000000000000000, -0.000000000000000000, -0.000000000000000000 ) ) ;
#149557 = CARTESIAN_POINT ( 'NONE',  ( 20.94999999999999574, -1.162701749926853712, -142.0000000000000284 ) ) ;
#149560 = EDGE_CURVE ( 'NONE', #109286, #239010, #253341, .T. ) ;
#149561 = CARTESIAN_POINT ( 'NONE',  ( -23.25000000000000000, 68.18350826420393673, -222.4110246041809091 ) ) ;
#149563 = ADVANCED_FACE ( 'NONE', ( #47258 ), #36712, .T. ) ;
#149562 = AXIS2_PLACEMENT_3D ( 'NONE', #202429, #66776, #69354 ) ;
#149564 = VERTEX_POINT ( 'NONE', #49843 ) ;
#149565 = ORIENTED_EDGE ( 'NONE', *, *, #234516, .F. ) ;
#149566 = EDGE_CURVE ( 'NONE', #113296, #104084, #231413, .T. ) ;
#149567 = CARTESIAN_POINT ( 'NONE',  ( -20.64999999999999858, -8.999999999988846255, -110.3939691226524786 ) ) ;
#149568 = CARTESIAN_POINT ( 'NONE',  ( 11.60000000000006182, 67.72071067812984779, -24.99381816264344636 ) ) ;
#149569 = CARTESIAN_POINT ( 'NONE',  ( -16.94107738177414291, 65.98576071487519812, -82.07310748452438531 ) ) ;
#149570 = CARTESIAN_POINT ( 'NONE',  ( -23.25000000000000000, 2.600000000011156054, -113.7246219227621395 ) ) ;
#149571 = ADVANCED_FACE ( 'NONE', ( #227197 ), #168571, .F. ) ;
#149572 = ORIENTED_EDGE ( 'NONE', *, *, #114224, .T. ) ;
#149574 = ADVANCED_FACE ( 'NONE', ( #126821 ), #61624, .T. ) ;
#149573 = DIRECTION ( 'NONE',  ( -1.000000000000000000, 0.000000000000000000, -0.000000000000000000 ) ) ;
#149575 =( NAMED_UNIT ( * ) SI_UNIT ( $, .STERADIAN. ) SOLID_ANGLE_UNIT ( ) );
#149576 = DIRECTION ( 'NONE',  ( -1.000000000000000000, 0.000000000000000000, 0.000000000000000000 ) ) ;
#149577 = ORIENTED_EDGE ( 'NONE', *, *, #60318, .T. ) ;
#149578 = DIRECTION ( 'NONE',  ( 0.000000000000000000, 0.8814952561688429444, -0.4721928772777345684 ) ) ;
#149579 = ORIENTED_EDGE ( 'NONE', *, *, #69778, .F. ) ;
#149580 = CYLINDRICAL_SURFACE ( 'NONE', #31520, 0.09999999999999939493 ) ;
#149581 = ORIENTED_EDGE ( 'NONE', *, *, #132738, .F. ) ;
#149582 = FACE_OUTER_BOUND ( 'NONE', #138470, .T. ) ;
#149583 = DIRECTION ( 'NONE',  ( 0.000000000000000000, -3.469446951953611033E-15, -1.000000000000000000 ) ) ;
#149585 = EDGE_LOOP ( 'NONE', ( #45177, #218732, #130974, #103966 ) ) ;
#149584 = CARTESIAN_POINT ( 'NONE',  ( -16.82055514392434148, 44.15993782893624342, -235.2879755648503703 ) ) ;
#149586 = EDGE_CURVE ( 'NONE', #152553, #105430, #90237, .T. ) ;
#149587 = CARTESIAN_POINT ( 'NONE',  ( -20.64999999999999858, 76.00000000001155342, -56.54810748452432279 ) ) ;
#149588 = VERTEX_POINT ( 'NONE', #87674 ) ;
#149589 = FACE_OUTER_BOUND ( 'NONE', #112953, .T. ) ;
#149590 = CARTESIAN_POINT ( 'NONE',  ( -16.80891096016346964, 9.950000000011137047, -113.1323371927329333 ) ) ;
#149591 = ORIENTED_EDGE ( 'NONE', *, *, #183081, .T. ) ;
#149592 = ADVANCED_FACE ( 'NONE', ( #130662 ), #15865, .T. ) ;
#149593 = TOROIDAL_SURFACE ( 'NONE', #70509, 11.89999999999999858, 0.1000000000000000056 ) ;
#149595 = AXIS2_PLACEMENT_3D ( 'NONE', #139657, #142248, #4021 ) ;
#149594 = PLANE ( 'NONE',  #26865 ) ;
#149596 = ORIENTED_EDGE ( 'NONE', *, *, #102553, .T. ) ;
#149597 = CIRCLE ( 'NONE', #249552, 0.09999999999998898659 ) ;
#149599 = LINE ( 'NONE', #229113, #36592 ) ;
#149598 = VECTOR ( 'NONE', #245850, 1000.000000000000000 ) ;
#149600 = EDGE_LOOP ( 'NONE', ( #58311, #179775, #204727, #11680 ) ) ;
#149601 = CARTESIAN_POINT ( 'NONE',  ( 15.39170923737819585, 9.389529397477893724, -118.3171079128937464 ) ) ;
#149602 = VECTOR ( 'NONE', #197153, 1000.000000000000000 ) ;
#149603 = DIRECTION ( 'NONE',  ( -1.000000000000000000, 0.000000000000000000, 0.000000000000000000 ) ) ;
#149604 = EDGE_CURVE ( 'NONE', #129105, #149548, #49143, .T. ) ;
#149607 = ORIENTED_EDGE ( 'NONE', *, *, #181322, .T. ) ;
#149606 = ORIENTED_EDGE ( 'NONE', *, *, #85324, .F. ) ;
#149605 = SPHERICAL_SURFACE ( 'NONE', #80544, 0.1000000000000000056 ) ;
#149609 = AXIS2_PLACEMENT_3D ( 'NONE', #225242, #144418, #223970 ) ;
#149608 = FACE_OUTER_BOUND ( 'NONE', #99291, .T. ) ;
#149610 = TOROIDAL_SURFACE ( 'NONE', #37186, 4.149999999999999467, 0.1000000000000000056 ) ;
#149611 = DIRECTION ( 'NONE',  ( 0.000000000000000000, 0.8814952561687762200, -0.4721928772778593575 ) ) ;
#149612 = DIRECTION ( 'NONE',  ( -1.000000000000000000, 0.000000000000000000, 0.000000000000000000 ) ) ;
#149613 = CIRCLE ( 'NONE', #12249, 0.09999999999999824307 ) ;
#149615 = DIRECTION ( 'NONE',  ( 0.000000000000000000, 0.000000000000000000, -1.000000000000000000 ) ) ;
#149614 = DIRECTION ( 'NONE',  ( 0.000000000000000000, 0.7397360091702755991, -0.6728971962616832059 ) ) ;
#149616 = CARTESIAN_POINT ( 'NONE',  ( -23.25000000000000000, 1.148907358139439339E-11, -201.0000000000015064 ) ) ;
#149617 = CARTESIAN_POINT ( 'NONE',  ( -21.05000000000000071, -11.48912529306490349, -137.1000000000000227 ) ) ;
#149618 = CARTESIAN_POINT ( 'NONE',  ( -20.65000000000000568, 7.249999999999983125, -20.85000000000000142 ) ) ;
#149619 = CARTESIAN_POINT ( 'NONE',  ( -20.64999999999999858, 1.115600667400684642E-11, -132.0000000000000284 ) ) ;
#149620 = AXIS2_PLACEMENT_3D ( 'NONE', #221797, #219247, #121475 ) ;
#149621 = ORIENTED_EDGE ( 'NONE', *, *, #82486, .F. ) ;
#149622 = EDGE_LOOP ( 'NONE', ( #107923, #202307, #77946, #60746 ) ) ;
#149623 = FACE_OUTER_BOUND ( 'NONE', #29551, .T. ) ;
#149625 = ORIENTED_EDGE ( 'NONE', *, *, #191687, .F. ) ;
#149624 = DIRECTION ( 'NONE',  ( 1.000000000000000000, 0.000000000000000000, 0.000000000000000000 ) ) ;
#149626 = ORIENTED_EDGE ( 'NONE', *, *, #7795, .T. ) ;
#149627 = CARTESIAN_POINT ( 'NONE',  ( -18.34374000495059676, 64.52683809665003878, -179.2731074845244450 ) ) ;
#149628 = VERTEX_POINT ( 'NONE', #69432 ) ;
#149629 = CARTESIAN_POINT ( 'NONE',  ( 21.12400247839527978, 43.45502593803676206, -234.7584006177618221 ) ) ;
#149630 = ORIENTED_EDGE ( 'NONE', *, *, #213404, .T. ) ;
#149631 = CARTESIAN_POINT ( 'NONE',  ( 18.39999999999999503, 70.35000000001255671, -182.6731074845243938 ) ) ;
#149632 = CARTESIAN_POINT ( 'NONE',  ( -23.15000000000000213, 4.898587196589414801E-16, -37.50000000000000000 ) ) ;
#149633 = CIRCLE ( 'NONE', #45373, 0.1000000000000028644 ) ;
#149635 = EDGE_LOOP ( 'NONE', ( #220785, #27774, #117483, #53577 ) ) ;
#149634 = VERTEX_POINT ( 'NONE', #246753 ) ;
#149636 = EDGE_LOOP ( 'NONE', ( #11181, #40688, #163682, #130463, #25741, #10727, #80629, #237724, #126875, #222390, #149666 ) ) ;
#149637 = ORIENTED_EDGE ( 'NONE', *, *, #129038, .T. ) ;
#149638 = VERTEX_POINT ( 'NONE', #208923 ) ;
#149639 = CARTESIAN_POINT ( 'NONE',  ( -16.88853107394619357, 14.16048480777639362, -219.2577547055215064 ) ) ;
#149640 = CARTESIAN_POINT ( 'NONE',  ( 21.13507111622890022, 43.45582266793360304, -234.7622126887535785 ) ) ;
#149641 = CARTESIAN_POINT ( 'NONE',  ( -18.59999999999999787, 74.26374286841418382, -57.95445515550683524 ) ) ;
#149643 = ORIENTED_EDGE ( 'NONE', *, *, #76250, .T. ) ;
#149642 = DIRECTION ( 'NONE',  ( 1.000000000000000000, 0.000000000000000000, 0.000000000000000000 ) ) ;
#149644 = CIRCLE ( 'NONE', #166226, 0.09999999999999939493 ) ;
#149645 = DIRECTION ( 'NONE',  ( 0.000000000000000000, 0.000000000000000000, -1.000000000000000000 ) ) ;
#149646 = CARTESIAN_POINT ( 'NONE',  ( -21.05000000000000071, 43.44873802792533724, -245.1397081572968659 ) ) ;
#149648 = EDGE_LOOP ( 'NONE', ( #253444, #4225, #257987, #74679, #72014 ) ) ;
#149647 = CARTESIAN_POINT ( 'NONE',  ( -20.64999999999999858, 4.350000000011156054, -45.85000000000000142 ) ) ;
#149649 = DIRECTION ( 'NONE',  ( 0.000000000000000000, 0.000000000000000000, -1.000000000000000000 ) ) ;
#149650 = ORIENTED_EDGE ( 'NONE', *, *, #86419, .F. ) ;
#149651 = LINE ( 'NONE', #195201, #53593 ) ;
#149652 = EDGE_LOOP ( 'NONE', ( #61359, #15237, #2189, #215922 ) ) ;
#149653 = DIRECTION ( 'NONE',  ( 0.000000000000000000, -1.000000000000000000, 0.000000000000000000 ) ) ;
#149654 = FACE_OUTER_BOUND ( 'NONE', #44421, .T. ) ;
#149655 = ADVANCED_FACE ( 'NONE', ( #147672 ), #68133, .F. ) ;
#149656 = ORIENTED_EDGE ( 'NONE', *, *, #204020, .T. ) ;
#149659 = CARTESIAN_POINT ( 'NONE',  ( -21.14999999999994174, 82.84256550613280012, -26.34830530078816935 ) ) ;
#149658 = DIRECTION ( 'NONE',  ( 0.000000000000000000, 0.1022405907414166287, 0.9947597004326452774 ) ) ;
#149657 = AXIS2_PLACEMENT_3D ( 'NONE', #234034, #18839, #97051 ) ;
#149660 = TOROIDAL_SURFACE ( 'NONE', #12285, 2.100000000000002309, 0.1000000000000000056 ) ;
#149661 = FACE_OUTER_BOUND ( 'NONE', #86692, .T. ) ;
#149662 = CARTESIAN_POINT ( 'NONE',  ( 21.00000000000000000, 12.15477401631902232, -210.9923204818763622 ) ) ;
#149663 = FACE_OUTER_BOUND ( 'NONE', #129073, .T. ) ;
#149664 = CIRCLE ( 'NONE', #216081, 0.09999999999999939493 ) ;
#149665 = ORIENTED_EDGE ( 'NONE', *, *, #239184, .F. ) ;
#149666 = ORIENTED_EDGE ( 'NONE', *, *, #136712, .T. ) ;
#149667 = LINE ( 'NONE', #154809, #155349 ) ;
#149668 = DIRECTION ( 'NONE',  ( -1.000000000000000000, 0.000000000000000000, -0.000000000000000000 ) ) ;
#149669 = VERTEX_POINT ( 'NONE', #229767 ) ;
#149670 = CARTESIAN_POINT ( 'NONE',  ( 18.59999999999999432, -1.835859311443640340, -45.00443916879852679 ) ) ;
#149671 = VERTEX_POINT ( 'NONE', #148972 ) ;
#149672 = ADVANCED_FACE ( 'NONE', ( #70726 ), #30302, .T. ) ;
#149673 = FACE_OUTER_BOUND ( 'NONE', #90749, .T. ) ;
#149674 = DIRECTION ( 'NONE',  ( 0.000000000000000000, -6.028164079019231987E-13, 1.000000000000000000 ) ) ;
#149675 = AXIS2_PLACEMENT_3D ( 'NONE', #241414, #125316, #240128 ) ;
#149676 = VECTOR ( 'NONE', #245981, 1000.000000000000000 ) ;
#149677 = EDGE_CURVE ( 'NONE', #115886, #154024, #111106, .T. ) ;
#149678 = CARTESIAN_POINT ( 'NONE',  ( 21.05000000000000071, 1.115625160336667635E-11, -165.5000000000000284 ) ) ;
#149679 = ORIENTED_EDGE ( 'NONE', *, *, #131453, .F. ) ;
#149680 = CARTESIAN_POINT ( 'NONE',  ( -22.50000000000000000, 55.98745301258801987, -232.8057040749261262 ) ) ;
#149682 = EDGE_LOOP ( 'NONE', ( #215334, #25856, #249824, #38276 ) ) ;
#149681 = CIRCLE ( 'NONE', #120470, 11.74999999999999289 ) ;
#149683 = ORIENTED_EDGE ( 'NONE', *, *, #198319, .F. ) ;
#149684 = VECTOR ( 'NONE', #92031, 1000.000000000000114 ) ;
#149685 = VECTOR ( 'NONE', #247464, 1000.000000000000000 ) ;
#149686 = ORIENTED_EDGE ( 'NONE', *, *, #212414, .T. ) ;
#149687 = EDGE_CURVE ( 'NONE', #251809, #119943, #136616, .T. ) ;
#149688 = CARTESIAN_POINT ( 'NONE',  ( -18.79999999999999716, -8.250000000000005329, 16.39999999999999858 ) ) ;
#149689 = DIRECTION ( 'NONE',  ( 0.000000000000000000, -1.000000000000000000, -6.352154140967427193E-15 ) ) ;
#149690 = CARTESIAN_POINT ( 'NONE',  ( 20.94999999999999574, 4.272272088314021943, -245.4186996786394843 ) ) ;
#149692 = ADVANCED_FACE ( 'NONE', ( #5562 ), #90826, .T. ) ;
#149691 = CARTESIAN_POINT ( 'NONE',  ( 21.05000000000000071, 67.22371710471966821, -136.5231074845243597 ) ) ;
#149693 = CARTESIAN_POINT ( 'NONE',  ( 23.14999999999999503, 11.65000000001116298, -59.98519422934606382 ) ) ;
#149694 = AXIS2_PLACEMENT_3D ( 'NONE', #212192, #89646, #252571 ) ;
#149696 = FACE_OUTER_BOUND ( 'NONE', #225503, .T. ) ;
#149695 = CYLINDRICAL_SURFACE ( 'NONE', #191189, 1.749999999999999778 ) ;
#149698 = VERTEX_POINT ( 'NONE', #224624 ) ;
#149697 = DIRECTION ( 'NONE',  ( 1.000000000000000000, 0.000000000000000000, 0.000000000000000000 ) ) ;
#149699 = CARTESIAN_POINT ( 'NONE',  ( 18.59999999999999076, 64.35000000001177511, -78.27310748452438816 ) ) ;
#149700 = ORIENTED_EDGE ( 'NONE', *, *, #161726, .T. ) ;
#149701 = EDGE_CURVE ( 'NONE', #104276, #152549, #124181, .T. ) ;
#149702 = CARTESIAN_POINT ( 'NONE',  ( -21.14999999999999858, 76.00000000001271871, -210.0637644362255969 ) ) ;
#149703 = ORIENTED_EDGE ( 'NONE', *, *, #26683, .F. ) ;
#149704 = VERTEX_POINT ( 'NONE', #32899 ) ;
#149705 = CARTESIAN_POINT ( 'NONE',  ( -17.11825945287482753, 10.05000000001113847, -46.25000000000000711 ) ) ;
#149706 = CARTESIAN_POINT ( 'NONE',  ( 21.05000000000000071, 87.65000000001192859, -105.9231074845242091 ) ) ;
#149707 = DIRECTION ( 'NONE',  ( 0.000000000000000000, 0.000000000000000000, -1.000000000000000000 ) ) ;
#149708 = DIRECTION ( 'NONE',  ( 0.000000000000000000, 6.938893903907270030E-14, 1.000000000000000000 ) ) ;
#149709 = EDGE_CURVE ( 'NONE', #188810, #120125, #11574, .T. ) ;
#149710 = CIRCLE ( 'NONE', #120665, 0.09999999999999939493 ) ;
#149711 = DIRECTION ( 'NONE',  ( 0.000000000000000000, 1.000000000000000000, -1.224646799147353207E-16 ) ) ;
#149712 = ORIENTED_EDGE ( 'NONE', *, *, #73739, .F. ) ;
#149714 = EDGE_LOOP ( 'NONE', ( #252439, #41759, #194762, #208637, #123245 ) ) ;
#149713 = EDGE_CURVE ( 'NONE', #204570, #158859, #78176, .T. ) ;
#149715 = CARTESIAN_POINT ( 'NONE',  ( -21.05000000000000071, 87.39257802171783851, -139.5970570643562212 ) ) ;
#149716 = EDGE_LOOP ( 'NONE', ( #38268, #236558 ) ) ;
#149717 = DIRECTION ( 'NONE',  ( -0.000000000000000000, -0.9126074666063770380, -0.4088369013363281068 ) ) ;
#149718 = CARTESIAN_POINT ( 'NONE',  ( 21.14999999999999858, 0.000000000000000000, 6.540656951701244282 ) ) ;
#149719 = EDGE_LOOP ( 'NONE', ( #134211, #171596, #232562 ) ) ;
#149720 = LINE ( 'NONE', #33647, #198722 ) ;
#149721 = CARTESIAN_POINT ( 'NONE',  ( -21.55000000000000426, 63.02410583447655767, -221.9179669651492759 ) ) ;
#149722 = CARTESIAN_POINT ( 'NONE',  ( -18.39999999999999858, -9.682403433465239573, -207.6568433774127413 ) ) ;
#149723 = CARTESIAN_POINT ( 'NONE',  ( 18.59999999999999076, 6.550000000011156231, -155.2500000000000284 ) ) ;
#149724 = ORIENTED_EDGE ( 'NONE', *, *, #211313, .F. ) ;
#149725 = CARTESIAN_POINT ( 'NONE',  ( -20.94999999999999929, 76.00000000001126921, -203.5231074845248997 ) ) ;
#149726 = FACE_OUTER_BOUND ( 'NONE', #241598, .T. ) ;
#149727 = CARTESIAN_POINT ( 'NONE',  ( 21.05000000000000071, 5.021051876504147385E-16, -29.40000000000000213 ) ) ;
#149728 = TOROIDAL_SURFACE ( 'NONE', #78751, 14.20833333333334103, 0.1000000000000000056 ) ;
#149729 = ADVANCED_FACE ( 'NONE', ( #234916 ), #257200, .F. ) ;
#149730 = DIRECTION ( 'NONE',  ( -1.000000000000000000, 0.000000000000000000, 0.000000000000000000 ) ) ;
#149731 = DIRECTION ( 'NONE',  ( -2.952720810173289112E-16, -1.000000000000000000, -6.982962677686266711E-15 ) ) ;
#149732 = CIRCLE ( 'NONE', #187307, 0.09999999999999939493 ) ;
#149733 = CARTESIAN_POINT ( 'NONE',  ( -21.03922262424669753, 57.80806069346814979, -226.1924746198927778 ) ) ;
#149734 = AXIS2_PLACEMENT_3D ( 'NONE', #142580, #108611, #106014 ) ;
#149735 = ORIENTED_EDGE ( 'NONE', *, *, #130595, .T. ) ;
#149736 = CARTESIAN_POINT ( 'NONE',  ( -16.93388492042258164, 66.01145817749640798, -157.4236526077106078 ) ) ;
#149737 = ORIENTED_EDGE ( 'NONE', *, *, #165644, .T. ) ;
#149738 = CARTESIAN_POINT ( 'NONE',  ( -23.25000000000000000, 1.910280373831774847, -20.86863214480106166 ) ) ;
#149739 = CARTESIAN_POINT ( 'NONE',  ( 23.14999999999999858, 67.23127455305835554, -235.8551265064784559 ) ) ;
#149740 = DIRECTION ( 'NONE',  ( 0.000000000000000000, 0.8814952561688722543, -0.4721928772776801675 ) ) ;
#149741 = DIRECTION ( 'NONE',  ( 0.000000000000000000, 7.056502275159890832E-15, -1.000000000000000000 ) ) ;
#149742 = CARTESIAN_POINT ( 'NONE',  ( 20.59588692710267921, 65.63127657884321309, -162.3840263900140144 ) ) ;
#149743 = AXIS2_PLACEMENT_3D ( 'NONE', #182138, #3479, #244659 ) ;
#149744 = ORIENTED_EDGE ( 'NONE', *, *, #41818, .T. ) ;
#149745 = DIRECTION ( 'NONE',  ( 1.000000000000000000, 0.000000000000000000, 0.000000000000000000 ) ) ;
#149746 = DIRECTION ( 'NONE',  ( 0.000000000000000000, 1.000000000000000000, 0.000000000000000000 ) ) ;
#149747 = CARTESIAN_POINT ( 'NONE',  ( -21.14999999999994174, 77.83551161375991967, -47.52760213295649550 ) ) ;
#149748 = AXIS2_PLACEMENT_3D ( 'NONE', #11080, #192291, #168911 ) ;
#149749 = LINE ( 'NONE', #192708, #57427 ) ;
#149750 = EDGE_CURVE ( 'NONE', #38996, #22560, #240313, .T. ) ;
#149751 = VERTEX_POINT ( 'NONE', #74589 ) ;
#149752 = VERTEX_POINT ( 'NONE', #154131 ) ;
#149753 = DIRECTION ( 'NONE',  ( -0.000000000000000000, 0.000000000000000000, -1.000000000000000000 ) ) ;
#149754 = DIRECTION ( 'NONE',  ( 0.000000000000000000, 0.008583690987127625890, 0.9999631594459055250 ) ) ;
#149755 = CARTESIAN_POINT ( 'NONE',  ( 23.25000000000000000, -11.48912529306489994, -197.8999999999999773 ) ) ;
#149756 = DIRECTION ( 'NONE',  ( 1.000000000000000000, 3.403959061552269104E-14, 2.112458025737858499E-14 ) ) ;
#149757 = EDGE_CURVE ( 'NONE', #117140, #1657, #17164, .T. ) ;
#149758 = EDGE_CURVE ( 'NONE', #82204, #169606, #133239, .T. ) ;
#149759 = ORIENTED_EDGE ( 'NONE', *, *, #190670, .F. ) ;
#149760 = CARTESIAN_POINT ( 'NONE',  ( -23.25000000000000000, -1.736705739456431807, -212.5174225876236846 ) ) ;
#149761 = DIRECTION ( 'NONE',  ( 1.000000000000000000, 0.000000000000000000, 0.000000000000000000 ) ) ;
#149762 = EDGE_CURVE ( 'NONE', #37339, #68945, #132542, .T. ) ;
#149763 = ORIENTED_EDGE ( 'NONE', *, *, #108636, .F. ) ;
#149765 = EDGE_CURVE ( 'NONE', #203961, #236269, #199175, .T. ) ;
#149764 = CARTESIAN_POINT ( 'NONE',  ( -18.59999999999999787, -9.500000000000005329, -8.099999999999999645 ) ) ;
#149766 = AXIS2_PLACEMENT_3D ( 'NONE', #178370, #257822, #2251 ) ;
#149767 = EDGE_CURVE ( 'NONE', #180612, #75872, #127894, .T. ) ;
#149768 = ADVANCED_FACE ( 'NONE', ( #54958 ), #36742, .F. ) ;
#149769 = ORIENTED_EDGE ( 'NONE', *, *, #185552, .T. ) ;
#149770 = ORIENTED_EDGE ( 'NONE', *, *, #147949, .F. ) ;
#149771 = EDGE_CURVE ( 'NONE', #242949, #185471, #19563, .T. ) ;
#149772 = ORIENTED_EDGE ( 'NONE', *, *, #91235, .F. ) ;
#149773 = FACE_OUTER_BOUND ( 'NONE', #2710, .T. ) ;
#149774 = DIRECTION ( 'NONE',  ( 0.000000000000000000, 1.000000000000000000, 0.000000000000000000 ) ) ;
#149775 = FACE_OUTER_BOUND ( 'NONE', #55428, .T. ) ;
#149776 = DIRECTION ( 'NONE',  ( 1.000000000000000000, 0.000000000000000000, 0.000000000000000000 ) ) ;
#149777 = DIRECTION ( 'NONE',  ( 1.000000000000000000, -0.000000000000000000, -0.000000000000000000 ) ) ;
#149778 = DIRECTION ( 'NONE',  ( 0.000000000000000000, 0.000000000000000000, -1.000000000000000000 ) ) ;
#149779 = CARTESIAN_POINT ( 'NONE',  ( -16.93440969289731157, 9.995185175813954714, -12.59123418501079605 ) ) ;
#149781 = DIRECTION ( 'NONE',  ( 0.2834754621636439431, 0.2834754621636471628, 0.9161240771326858434 ) ) ;
#149780 = DIRECTION ( 'NONE',  ( 0.000000000000000000, -0.8660254037844445918, -0.4999999999999897304 ) ) ;
#149782 = CIRCLE ( 'NONE', #95590, 0.5000000000000004441 ) ;
#149783 = DIRECTION ( 'NONE',  ( -1.646408749285562691E-14, 1.000000000000000000, 0.000000000000000000 ) ) ;
#149784 = VECTOR ( 'NONE', #161529, 1000.000000000000000 ) ;
#149785 = DIRECTION ( 'NONE',  ( 0.000000000000000000, -1.000000000000000000, 0.000000000000000000 ) ) ;
#149786 = CARTESIAN_POINT ( 'NONE',  ( -18.40000000000000213, 11.48667500176882861, -91.25000000000005684 ) ) ;
#149787 = AXIS2_PLACEMENT_3D ( 'NONE', #184388, #44892, #222212 ) ;
#149789 = DIRECTION ( 'NONE',  ( -1.000000000000000000, -8.673617379884087537E-15, 0.000000000000000000 ) ) ;
#149788 = CIRCLE ( 'NONE', #174760, 11.64999999999999325 ) ;
#149790 = ORIENTED_EDGE ( 'NONE', *, *, #27008, .F. ) ;
#149791 = ORIENTED_EDGE ( 'NONE', *, *, #122890, .T. ) ;
#149792 = CARTESIAN_POINT ( 'NONE',  ( -18.37151313414685561, -9.571014125778372517, -40.31666290923867280 ) ) ;
#149793 = CARTESIAN_POINT ( 'NONE',  ( -23.25000000000000000, 64.25000000001165290, -69.52310748452440237 ) ) ;
#149794 = CARTESIAN_POINT ( 'NONE',  ( -20.85000000000000142, -11.74999999998884448, -134.0000000000000284 ) ) ;
#149795 = EDGE_CURVE ( 'NONE', #59439, #161343, #28542, .T. ) ;
#149796 = CIRCLE ( 'NONE', #187200, 0.1000000000000054040 ) ;
#149797 = CARTESIAN_POINT ( 'NONE',  ( -20.64999999999999858, 71.65000000001187175, -90.77310748452434552 ) ) ;
#149798 = CARTESIAN_POINT ( 'NONE',  ( -20.94999999999999929, -1.849153571976047239, -45.10596661979705146 ) ) ;
#149799 = ADVANCED_FACE ( 'NONE', ( #216620 ), #40437, .F. ) ;
#149800 = EDGE_CURVE ( 'NONE', #26422, #114396, #99194, .T. ) ;
#149801 = ORIENTED_EDGE ( 'NONE', *, *, #243078, .F. ) ;
#149802 = EDGE_LOOP ( 'NONE', ( #102282, #200137, #122926, #176626 ) ) ;
#149804 = CIRCLE ( 'NONE', #74971, 11.65000000000001457 ) ;
#149803 = CARTESIAN_POINT ( 'NONE',  ( -23.15000000000000213, 54.34471204062663219, -239.4366250215122420 ) ) ;
#149805 = ORIENTED_EDGE ( 'NONE', *, *, #111931, .F. ) ;
#149806 = DIRECTION ( 'NONE',  ( -1.000000000000000000, -2.952720810173289112E-16, 0.000000000000000000 ) ) ;
#149807 = AXIS2_PLACEMENT_3D ( 'NONE', #21720, #77816, #180795 ) ;
#149808 = CARTESIAN_POINT ( 'NONE',  ( 21.12757541349815682, 6.473380571262609351, -133.9948387841902786 ) ) ;
#149809 = VERTEX_POINT ( 'NONE', #214059 ) ;
#149810 = CYLINDRICAL_SURFACE ( 'NONE', #35272, 4.000000000000003553 ) ;
#149811 = VERTEX_POINT ( 'NONE', #35460 ) ;
#149812 = DIRECTION ( 'NONE',  ( 0.000000000000000000, -7.272083257015735086E-15, 1.000000000000000000 ) ) ;
#149813 = LINE ( 'NONE', #7724, #116169 ) ;
#149814 = CARTESIAN_POINT ( 'NONE',  ( 18.59999999999999787, -9.321008403350148797, -141.2359382490778614 ) ) ;
#149815 = PLANE ( 'NONE',  #55710 ) ;
#149816 = DIRECTION ( 'NONE',  ( -0.000000000000000000, 0.8127272543710891695, -0.5826443254700338636 ) ) ;
#149817 = CARTESIAN_POINT ( 'NONE',  ( 23.14999999999999858, 70.40000000001222702, -148.9283735034374843 ) ) ;
#149818 = LINE ( 'NONE', #228056, #57951 ) ;
#149820 = EDGE_LOOP ( 'NONE', ( #87883, #250770, #83791, #6864, #229259 ) ) ;
#149819 = DIRECTION ( 'NONE',  ( 0.000000000000000000, 0.000000000000000000, 1.000000000000000000 ) ) ;
#149822 = DIRECTION ( 'NONE',  ( 0.000000000000000000, -0.2128009952263603677, 0.9770955615653313941 ) ) ;
#149821 = DIRECTION ( 'NONE',  ( -0.000000000000000000, 0.8814952561688430555, -0.4721928772777346239 ) ) ;
#149823 = EDGE_LOOP ( 'NONE', ( #114231, #247091, #235599 ) ) ;
#149825 = ORIENTED_EDGE ( 'NONE', *, *, #213636, .F. ) ;
#149824 = CARTESIAN_POINT ( 'NONE',  ( 21.13461538461538325, 10.61458296203669249, -45.85000000000000142 ) ) ;
#149826 = AXIS2_PLACEMENT_3D ( 'NONE', #71561, #173254, #151078 ) ;
#149827 = ORIENTED_EDGE ( 'NONE', *, *, #38552, .F. ) ;
#149828 = DIRECTION ( 'NONE',  ( 1.000000000000000000, 0.000000000000000000, 0.000000000000000000 ) ) ;
#149829 = CARTESIAN_POINT ( 'NONE',  ( -18.34804628011471195, 11.47316190337353525, -143.2500000000000284 ) ) ;
#149830 = CARTESIAN_POINT ( 'NONE',  ( -22.50000000000000000, 11.64957080755595520, -100.4000000000000483 ) ) ;
#149831 = LINE ( 'NONE', #188944, #102366 ) ;
#149832 = CARTESIAN_POINT ( 'NONE',  ( -21.05000000000000071, -11.39257802169451672, -137.0739495798319467 ) ) ;
#149833 = CARTESIAN_POINT ( 'NONE',  ( -16.81744102076748959, 9.950000000011138823, -54.35000000000000142 ) ) ;
#149834 = DIRECTION ( 'NONE',  ( 0.000000000000000000, 0.2128009952263603677, -0.9770955615653313941 ) ) ;
#149835 = ADVANCED_FACE ( 'NONE', ( #194520 ), #156687, .T. ) ;
#149836 = LINE ( 'NONE', #230649, #160172 ) ;
#149837 = ORIENTED_EDGE ( 'NONE', *, *, #252944, .F. ) ;
#149838 = ORIENTED_EDGE ( 'NONE', *, *, #47232, .F. ) ;
#149839 = ADVANCED_FACE ( 'NONE', ( #77111 ), #52398, .T. ) ;
#149840 = LINE ( 'NONE', #69021, #101983 ) ;
#149841 = VECTOR ( 'NONE', #142368, 1000.000000000000000 ) ;
#149842 = ORIENTED_EDGE ( 'NONE', *, *, #34975, .F. ) ;
#149843 = CARTESIAN_POINT ( 'NONE',  ( -21.44999999999999929, 7.250000000011155521, -188.7499999999999716 ) ) ;
#149845 = ORIENTED_EDGE ( 'NONE', *, *, #109616, .T. ) ;
#149844 = CIRCLE ( 'NONE', #228935, 0.1000000000000002692 ) ;
#149846 = CARTESIAN_POINT ( 'NONE',  ( 18.48197441911561612, -9.517954794705673294, -40.39021164220778104 ) ) ;
#149847 = EDGE_CURVE ( 'NONE', #103697, #25805, #117525, .T. ) ;
#149848 = ADVANCED_FACE ( 'NONE', ( #238760 ), #83497, .F. ) ;
#149849 = AXIS2_PLACEMENT_3D ( 'NONE', #67261, #131083, #146771 ) ;
#149850 = DIRECTION ( 'NONE',  ( 0.000000000000000000, -1.000000000000000000, -7.272083257015735086E-15 ) ) ;
#149851 = PLANE ( 'NONE',  #235129 ) ;
#149852 = FACE_OUTER_BOUND ( 'NONE', #85097, .T. ) ;
#149853 = ORIENTED_EDGE ( 'NONE', *, *, #89774, .F. ) ;
#149854 = AXIS2_PLACEMENT_3D ( 'NONE', #11900, #151406, #76974 ) ;
#149855 = CARTESIAN_POINT ( 'NONE',  ( 23.14999999999999858, 76.00000000001165290, -69.52310748452431710 ) ) ;
#149856 = DIRECTION ( 'NONE',  ( 0.000000000000000000, 0.4930308989875575865, 0.8700118002898125091 ) ) ;
#149857 = CARTESIAN_POINT ( 'NONE',  ( 21.14999999999999858, 0.000000000000000000, -12.15000000000000036 ) ) ;
#149858 = CARTESIAN_POINT ( 'NONE',  ( -21.05000000000000071, 6.257814610487270279, -133.9022097086912311 ) ) ;
#149859 = DIRECTION ( 'NONE',  ( 1.186688945009010077E-16, -0.9770955615653315052, -0.2128009952263603954 ) ) ;
#149860 = VERTEX_POINT ( 'NONE', #140956 ) ;
#149862 = CARTESIAN_POINT ( 'NONE',  ( -23.25000000000000000, 46.15118611352045974, -240.5321844900040844 ) ) ;
#149861 = DIRECTION ( 'NONE',  ( 1.000000000000000000, -0.000000000000000000, 0.000000000000000000 ) ) ;
#149863 = ORIENTED_EDGE ( 'NONE', *, *, #184448, .T. ) ;
#149866 = EDGE_LOOP ( 'NONE', ( #225408, #241470, #51522, #55739 ) ) ;
#149865 = CARTESIAN_POINT ( 'NONE',  ( -16.87683809663752399, 50.97313360171294505, -232.3453239361865315 ) ) ;
#149864 = DIRECTION ( 'NONE',  ( 0.000000000000000000, -0.9126074666063660468, -0.4088369013363524762 ) ) ;
#149867 = AXIS2_PLACEMENT_3D ( 'NONE', #12437, #148079, #48966 ) ;
#149868 = EDGE_CURVE ( 'NONE', #239804, #187157, #119521, .T. ) ;
#149869 = DIRECTION ( 'NONE',  ( 2.952720810173289112E-16, 1.000000000000000000, 6.530723674265620862E-15 ) ) ;
#149871 = EDGE_CURVE ( 'NONE', #234461, #144289, #178821, .T. ) ;
#149870 = AXIS2_PLACEMENT_3D ( 'NONE', #214546, #134992, #158464 ) ;
#149872 = AXIS2_PLACEMENT_3D ( 'NONE', #94175, #35538, #14683 ) ;
#149873 =( GEOMETRIC_REPRESENTATION_CONTEXT ( 3 ) GLOBAL_UNCERTAINTY_ASSIGNED_CONTEXT ( ( #131189 ) ) GLOBAL_UNIT_ASSIGNED_CONTEXT ( ( #9804, #188438, #150611 ) ) REPRESENTATION_CONTEXT ( 'NONE', 'WORKASPACE' ) );
#149874 = AXIS2_PLACEMENT_3D ( 'NONE', #117103, #119677, #17984 ) ;
#149875 = CARTESIAN_POINT ( 'NONE',  ( -23.25000000000000000, 1.115650265596050101E-11, -129.9500000000000171 ) ) ;
#149876 = DIRECTION ( 'NONE',  ( 1.000000000000000000, 0.000000000000000000, 0.000000000000000000 ) ) ;
#149877 = VERTEX_POINT ( 'NONE', #60102 ) ;
#149878 = PLANE ( 'NONE',  #192832 ) ;
#149879 = AXIS2_PLACEMENT_3D ( 'NONE', #109211, #73986, #251287 ) ;
#149880 = DIRECTION ( 'NONE',  ( 2.715809747126117987E-16, 1.000000000000000000, 1.032007703907924707E-14 ) ) ;
#149882 = CARTESIAN_POINT ( 'NONE',  ( -20.65000000000000568, 70.35000000001159037, -56.87310748452436115 ) ) ;
#149881 = CARTESIAN_POINT ( 'NONE',  ( -23.49999999999994316, 64.25000000001119815, -26.12310748452479103 ) ) ;
#149884 = ORIENTED_EDGE ( 'NONE', *, *, #43772, .F. ) ;
#149883 = DIRECTION ( 'NONE',  ( 0.7071067811865474617, -0.7071067811865474617, -4.937700262164531476E-15 ) ) ;
#149885 = EDGE_CURVE ( 'NONE', #90455, #245420, #174283, .T. ) ;
#149886 = VERTEX_POINT ( 'NONE', #200911 ) ;
#149888 = EDGE_CURVE ( 'NONE', #77841, #181022, #48766, .T. ) ;
#149887 = CARTESIAN_POINT ( 'NONE',  ( 21.05000000000000071, 6.649999999999999467, -10.01702717044001822 ) ) ;
#149889 = FACE_OUTER_BOUND ( 'NONE', #63764, .T. ) ;
#149890 = CARTESIAN_POINT ( 'NONE',  ( 18.59999999999999076, 65.75000000001176659, -78.27310748452438816 ) ) ;
#149891 = ORIENTED_EDGE ( 'NONE', *, *, #1133, .T. ) ;
#149892 = CARTESIAN_POINT ( 'NONE',  ( 21.14999999999999503, 11.65000000001116298, -100.5000000000000284 ) ) ;
#149893 = FACE_OUTER_BOUND ( 'NONE', #214217, .T. ) ;
#149894 = FACE_OUTER_BOUND ( 'NONE', #109765, .T. ) ;
#149895 = EDGE_LOOP ( 'NONE', ( #226861, #98927, #164922, #49652 ) ) ;
#149896 = EDGE_CURVE ( 'NONE', #250042, #58070, #222372, .T. ) ;
#149897 = CARTESIAN_POINT ( 'NONE',  ( 20.51284917709620004, 59.28817092441780545, -225.7512494052134855 ) ) ;
#149898 = EDGE_CURVE ( 'NONE', #150237, #242521, #78360, .T. ) ;
#149899 = AXIS2_PLACEMENT_3D ( 'NONE', #66505, #164330, #168210 ) ;
#149900 = ORIENTED_EDGE ( 'NONE', *, *, #210526, .T. ) ;
#149901 = EDGE_CURVE ( 'NONE', #84841, #182741, #121416, .T. ) ;
#149902 = DIRECTION ( 'NONE',  ( -1.000000000000000000, -1.040834085586090568E-13, 0.000000000000000000 ) ) ;
#149903 = DIRECTION ( 'NONE',  ( 0.000000000000000000, -1.000000000000000000, 0.000000000000000000 ) ) ;
#149904 = VECTOR ( 'NONE', #20785, 1000.000000000000000 ) ;
#149905 = ORIENTED_EDGE ( 'NONE', *, *, #70821, .T. ) ;
#149906 = ORIENTED_EDGE ( 'NONE', *, *, #157953, .F. ) ;
#149907 = CARTESIAN_POINT ( 'NONE',  ( -20.54999999999999716, 63.53703427598990316, -222.1606900896233583 ) ) ;
#149908 = ORIENTED_EDGE ( 'NONE', *, *, #48951, .T. ) ;
#149910 = EDGE_LOOP ( 'NONE', ( #197392, #254111, #76017, #16944, #58867 ) ) ;
#149909 = DIRECTION ( 'NONE',  ( 0.000000000000000000, 0.9908441862701791170, -0.1350103645450472789 ) ) ;
#149911 = EDGE_CURVE ( 'NONE', #197986, #131327, #86717, .T. ) ;
#149912 = ORIENTED_EDGE ( 'NONE', *, *, #119032, .F. ) ;
#149913 = AXIS2_PLACEMENT_3D ( 'NONE', #92007, #89436, #30785 ) ;
#149916 = ORIENTED_EDGE ( 'NONE', *, *, #158669, .F. ) ;
#149915 = ORIENTED_EDGE ( 'NONE', *, *, #160148, .T. ) ;
#149914 = CARTESIAN_POINT ( 'NONE',  ( -23.15000000000000213, 1.115600667400684642E-11, -200.9999999999999432 ) ) ;
#149917 = EDGE_CURVE ( 'NONE', #233060, #223851, #232530, .T. ) ;
#149918 = CIRCLE ( 'NONE', #178988, 12.77499999999999503 ) ;
#149919 = B_SPLINE_CURVE_WITH_KNOTS ( 'NONE', 3,
 ( #206769, #228902, #107659, #144204, #50239, #223744, #110223, #189770, #249746, #187225, #185917, #45126, #7270, #124672, #5979, #85492, #175372, #33305, #72411 ),
 .UNSPECIFIED., .F., .F.,
 ( 4, 3, 3, 3, 3, 3, 4 ),
 ( -2.000416914645579387E-06, 0.000000000000000000, 4.714008503745887181E-05, 9.979203887778629440E-05, 0.0001372215519229621735, 0.0001635031576221138031, 0.0001900083748504299125 ),
 .UNSPECIFIED. ) ;
#149920 = DIRECTION ( 'NONE',  ( 0.000000000000000000, 0.000000000000000000, 1.000000000000000000 ) ) ;
#149921 = ORIENTED_EDGE ( 'NONE', *, *, #208054, .F. ) ;
#149922 = DIRECTION ( 'NONE',  ( 0.000000000000000000, 0.000000000000000000, -1.000000000000000000 ) ) ;
#149923 = CARTESIAN_POINT ( 'NONE',  ( -20.64999999999999858, 4.350000000011156054, -45.75000000000000711 ) ) ;
#149924 = AXIS2_PLACEMENT_3D ( 'NONE', #149022, #128160, #30354 ) ;
#149925 = CARTESIAN_POINT ( 'NONE',  ( -18.59999999999999787, 77.16270174994961906, -61.52310748452431710 ) ) ;
#149926 = CYLINDRICAL_SURFACE ( 'NONE', #246744, 0.09999999999999520384 ) ;
#149927 = VERTEX_POINT ( 'NONE', #118826 ) ;
#149928 = VERTEX_POINT ( 'NONE', #221730 ) ;
#149929 = VERTEX_POINT ( 'NONE', #160532 ) ;
#149930 = FACE_OUTER_BOUND ( 'NONE', #116417, .T. ) ;
#149932 = EDGE_LOOP ( 'NONE', ( #10487, #229042, #210745 ) ) ;
#149931 = DIRECTION ( 'NONE',  ( 1.186688945009009831E-16, -1.000000000000000000, 0.000000000000000000 ) ) ;
#149933 = DIRECTION ( 'NONE',  ( 0.000000000000000000, 0.000000000000000000, 1.000000000000000000 ) ) ;
#149935 = ORIENTED_EDGE ( 'NONE', *, *, #90000, .F. ) ;
#149934 = CARTESIAN_POINT ( 'NONE',  ( 18.49505832270841310, 78.22446672510398002, -231.3780609907616679 ) ) ;
#149936 =( BOUNDED_SURFACE ( )  B_SPLINE_SURFACE ( 3, 2, ( 
 ( #44787, #219550, #43508 ),
 ( #141315, #5626, #160898 ),
 ( #140006, #224688, #220841 ),
 ( #120499, #99587, #21394 ) ),
 .UNSPECIFIED., .F., .F., .F. ) 
 B_SPLINE_SURFACE_WITH_KNOTS ( ( 4, 4 ),
 ( 3, 3 ),
 ( 0.3000847527772385059, 0.5552748953338751958 ),
 ( 0.000000000000000000, 1.000000000000000000 ),
 .UNSPECIFIED. ) 
 GEOMETRIC_REPRESENTATION_ITEM ( )  RATIONAL_B_SPLINE_SURFACE ( (
 ( 1.000000000000000000, 0.9152888060719408525, 1.000000000000000000),
 ( 1.000000000000000000, 0.9104333467450348438, 1.000000000000000000),
 ( 1.000000000000000000, 0.9035312726220574575, 1.000000000000000000),
 ( 1.000000000000000000, 0.8946697475932264831, 1.000000000000000000) ) ) 
 REPRESENTATION_ITEM ( '' )  SURFACE ( )  );
#149937 = EDGE_LOOP ( 'NONE', ( #126545, #41511, #84039, #21621 ) ) ;
#149938 = DIRECTION ( 'NONE',  ( 1.000000000000000000, -0.000000000000000000, -0.000000000000000000 ) ) ;
#149939 = VERTEX_POINT ( 'NONE', #62694 ) ;
#149940 = VECTOR ( 'NONE', #4203, 1000.000000000000000 ) ;
#149941 = CIRCLE ( 'NONE', #112341, 11.75000000000000000 ) ;
#149942 = CARTESIAN_POINT ( 'NONE',  ( 18.54999999999999716, 66.05000000001228955, -157.3731074845244962 ) ) ;
#149943 = CARTESIAN_POINT ( 'NONE',  ( -20.94999999999994600, 65.36599112033563586, -30.02023607076051803 ) ) ;
#149945 = EDGE_LOOP ( 'NONE', ( #127682, #248244, #54815 ) ) ;
#149944 = ORIENTED_EDGE ( 'NONE', *, *, #236602, .T. ) ;
#149946 = B_SPLINE_CURVE_WITH_KNOTS ( 'NONE', 3,
 ( #246889, #231213, #250745, #52540, #112540, #192085, #82977, #63440, #142960, #222499, #43892, #107379, #186957, #8309, #167392, #94240, #14742, #155543, #17294, #254574, #253312, #95527, #13438, #232500, #74729, #154274, #214203, #75972, #35590, #116391 ),
 .UNSPECIFIED., .F., .F.,
 ( 4, 2, 2, 2, 2, 2, 2, 2, 2, 2, 2, 2, 2, 2, 4 ),
 ( 0.000000000000000000, 0.0003422764154113336690, 0.0006845528308226673381, 0.001026829246234001007, 0.001369105661645334676, 0.002053658492468005917, 0.002738211323290676725, 0.003080487738702009960, 0.003422764154113342762, 0.003765040569524675997, 0.004107316984936009233, 0.004449593400347342034, 0.004791869815758674836, 0.005134146231170008505, 0.005476422646581341307 ),
 .UNSPECIFIED. ) ;
#149947 = ORIENTED_EDGE ( 'NONE', *, *, #103082, .T. ) ;
#149948 = CARTESIAN_POINT ( 'NONE',  ( -18.34804628011471195, 13.17878477875115806, -207.5966336730521675 ) ) ;
#149949 = ORIENTED_EDGE ( 'NONE', *, *, #38698, .T. ) ;
#149950 =( BOUNDED_CURVE ( )  B_SPLINE_CURVE ( 3, ( #7277, #149394, #108944, #45131 ),
 .UNSPECIFIED., .F., .F. ) 
 B_SPLINE_CURVE_WITH_KNOTS ( ( 4, 4 ),
 ( 0.06456096931748320222, 3.077031684272310219 ),
 .UNSPECIFIED. ) 
 CURVE ( )  GEOMETRIC_REPRESENTATION_ITEM ( )  RATIONAL_B_SPLINE_CURVE ( ( 1.000000000000000000, 0.3763440860215094830, 0.3763440860215094830, 1.000000000000000000 ) ) 
 REPRESENTATION_ITEM ( '' )  );
#149951 = ORIENTED_EDGE ( 'NONE', *, *, #174805, .F. ) ;
#149952 = CARTESIAN_POINT ( 'NONE',  ( 20.12500000000000355, 65.75804927292892899, -61.66290375743827212 ) ) ;
#149954 = ORIENTED_EDGE ( 'NONE', *, *, #141236, .F. ) ;
#149953 = CARTESIAN_POINT ( 'NONE',  ( 21.14999999999999858, 0.09779029130879170195, 6.257814610476124528 ) ) ;
#149955 = CYLINDRICAL_SURFACE ( 'NONE', #10844, 11.74999999999999645 ) ;
#149957 = DIRECTION ( 'NONE',  ( 0.000000000000000000, 0.000000000000000000, -1.000000000000000000 ) ) ;
#149956 = DIRECTION ( 'NONE',  ( 0.000000000000000000, 0.000000000000000000, -1.000000000000000000 ) ) ;
#149958 = LINE ( 'NONE', #115953, #161542 ) ;
#149959 = CARTESIAN_POINT ( 'NONE',  ( -20.94999999999999929, 1.115600667400684642E-11, -122.3000000000000398 ) ) ;
#149960 = EDGE_LOOP ( 'NONE', ( #87133, #115065, #127406, #66441 ) ) ;
#149961 = ORIENTED_EDGE ( 'NONE', *, *, #156602, .F. ) ;
#149963 = VECTOR ( 'NONE', #3184, 1000.000000000000000 ) ;
#149962 = DIRECTION ( 'NONE',  ( 0.000000000000000000, 0.000000000000000000, -1.000000000000000000 ) ) ;
#149964 = DIRECTION ( 'NONE',  ( 0.000000000000000000, 0.000000000000000000, 1.000000000000000000 ) ) ;
#149965 = CIRCLE ( 'NONE', #12405, 0.1000000000000024342 ) ;
#149966 = ADVANCED_FACE ( 'NONE', ( #242593 ), #123249, .T. ) ;
#149967 = AXIS2_PLACEMENT_3D ( 'NONE', #25530, #162478, #187180 ) ;
#149968 = VECTOR ( 'NONE', #49281, 1000.000000000000000 ) ;
#149970 = ORIENTED_EDGE ( 'NONE', *, *, #240682, .F. ) ;
#149969 = B_SPLINE_CURVE_WITH_KNOTS ( 'NONE', 3,
 ( #53734, #78426, #57569, #134533, #18463, #214095, #77144, #158022, #137132, #113707, #251932, #216659, #133276, #13333, #194561, #73333 ),
 .UNSPECIFIED., .F., .F.,
 ( 4, 3, 3, 3, 3, 4 ),
 ( 0.000000000000000000, 2.209833635978099498E-05, 5.595056164119025226E-05, 8.979992002654954499E-05, 0.0001236482757198867745, 0.0001574984039362969023 ),
 .UNSPECIFIED. ) ;
#149971 = B_SPLINE_CURVE_WITH_KNOTS ( 'NONE', 3,
 ( #73281, #100479, #241320, #18404, #97907, #178806, #3974, #220473, #40579, #112 ),
 .UNSPECIFIED., .F., .F.,
 ( 4, 3, 3, 4 ),
 ( 0.000000000000000000, 0.0002000000000002884074, 0.001000000000045112589, 0.001967863649472103085 ),
 .UNSPECIFIED. ) ;
#149972 =( BOUNDED_CURVE ( )  B_SPLINE_CURVE ( 3, ( #1334, #99147, #79584, #17089 ),
 .UNSPECIFIED., .F., .F. ) 
 B_SPLINE_CURVE_WITH_KNOTS ( ( 4, 4 ),
 ( 1.289024775538054608E-13, 1.570796326794793529 ),
 .UNSPECIFIED. ) 
 CURVE ( )  GEOMETRIC_REPRESENTATION_ITEM ( )  RATIONAL_B_SPLINE_CURVE ( ( 1.000000000000000000, 0.8047378541244196715, 0.8047378541244196715, 1.000000000000000000 ) ) 
 REPRESENTATION_ITEM ( '' )  );
#149973 = DIRECTION ( 'NONE',  ( 1.000000000000000000, 0.000000000000000000, 0.000000000000000000 ) ) ;
#149974 = CIRCLE ( 'NONE', #66754, 0.09999999999999939493 ) ;
#149975 = CARTESIAN_POINT ( 'NONE',  ( 12.25000000000000000, 66.15000000001258229, -186.7731074845244450 ) ) ;
#149976 = ORIENTED_EDGE ( 'NONE', *, *, #98409, .F. ) ;
#149977 = ORIENTED_EDGE ( 'NONE', *, *, #247540, .F. ) ;
#149978 = CARTESIAN_POINT ( 'NONE',  ( -21.00250684356849362, 64.25000000001264766, -196.5083017157664358 ) ) ;
#149979 = ADVANCED_FACE ( 'NONE', ( #86064 ), #108240, .T. ) ;
#149980 = FACE_OUTER_BOUND ( 'NONE', #141704, .T. ) ;
#149981 = VERTEX_POINT ( 'NONE', #6557 ) ;
#149982 = DIRECTION ( 'NONE',  ( -1.000000000000000000, 0.000000000000000000, 0.000000000000000000 ) ) ;
#149983 = ORIENTED_EDGE ( 'NONE', *, *, #102026, .T. ) ;
#149984 = CARTESIAN_POINT ( 'NONE',  ( 23.25000000000000355, -20.49622690151871396, -212.4170162771926016 ) ) ;
#149985 = CARTESIAN_POINT ( 'NONE',  ( -16.77828822459933633, 9.946229375067616729, -154.8373717490810861 ) ) ;
#149987 = CARTESIAN_POINT ( 'NONE',  ( 20.84999999999998721, 67.49222854868494892, -195.4187676019683693 ) ) ;
#149986 = CARTESIAN_POINT ( 'NONE',  ( -21.55000000000000426, 68.25000000001199396, -115.3731074845243540 ) ) ;
#149988 = CARTESIAN_POINT ( 'NONE',  ( -17.01764560440454233, 9.950000000011138823, -87.75000000078685503 ) ) ;
#149989 = EDGE_CURVE ( 'NONE', #215894, #71372, #135084, .T. ) ;
#149992 = EDGE_CURVE ( 'NONE', #139553, #221299, #219434, .T. ) ;
#149991 = CARTESIAN_POINT ( 'NONE',  ( 21.05000000000000071, 87.65000000001266756, -200.6231074845242688 ) ) ;
#149990 = TOROIDAL_SURFACE ( 'NONE', #112564, 0.2000000000000000111, 0.1000000000000000056 ) ;
#149993 = PLANE ( 'NONE',  #165543 ) ;
#149994 = AXIS2_PLACEMENT_3D ( 'NONE', #204663, #109415, #84689 ) ;
#149995 = DIRECTION ( 'NONE',  ( -1.000000000000000000, 0.000000000000000000, 0.000000000000000000 ) ) ;
#149997 = VERTEX_POINT ( 'NONE', #186494 ) ;
#149996 = DIRECTION ( 'NONE',  ( 0.000000000000000000, 1.000000000000000000, 0.000000000000000000 ) ) ;
#149999 = ORIENTED_EDGE ( 'NONE', *, *, #84262, .T. ) ;
#149998 = ORIENTED_EDGE ( 'NONE', *, *, #46136, .T. ) ;
#150000 = ORIENTED_EDGE ( 'NONE', *, *, #3728, .F. ) ;
#150001 = EDGE_CURVE ( 'NONE', #98538, #238064, #153432, .T. ) ;
#150002 = CARTESIAN_POINT ( 'NONE',  ( 20.85000000000000142, 76.32388570108278714, -170.0655178952103768 ) ) ;
#150003 = DIRECTION ( 'NONE',  ( 0.000000000000000000, 0.000000000000000000, 1.000000000000000000 ) ) ;
#150005 = CARTESIAN_POINT ( 'NONE',  ( -23.15000000000000213, 1.115600667400684642E-11, -167.5000000000000284 ) ) ;
#150004 = DIRECTION ( 'NONE',  ( 0.000000000000000000, 0.000000000000000000, -1.000000000000000000 ) ) ;
#150006 = CYLINDRICAL_SURFACE ( 'NONE', #162250, 0.09999999999999939493 ) ;
#150007 = ORIENTED_EDGE ( 'NONE', *, *, #195527, .F. ) ;
#150008 = DIRECTION ( 'NONE',  ( 0.000000000000000000, 0.9126074666063757057, 0.4088369013363309379 ) ) ;
#150009 = EDGE_LOOP ( 'NONE', ( #224578, #29217, #232005, #115556 ) ) ;
#150010 = CARTESIAN_POINT ( 'NONE',  ( -21.05000000000000071, 0.03175835305540354592, 6.258847123079506858 ) ) ;
#150011 = CARTESIAN_POINT ( 'NONE',  ( 17.23472005113828232, 65.69211804551183320, -192.0696843445931563 ) ) ;
#150012 = ORIENTED_EDGE ( 'NONE', *, *, #142338, .T. ) ;
#150013 = AXIS2_PLACEMENT_3D ( 'NONE', #148187, #29563, #229023 ) ;
#150014 = CARTESIAN_POINT ( 'NONE',  ( -20.64999999999999858, 4.625797360122408719, -213.1224017332881431 ) ) ;
#150015 = DIRECTION ( 'NONE',  ( -2.952720810173289605E-16, -1.000000000000000000, -7.086529944415894657E-15 ) ) ;
#150016 = ORIENTED_EDGE ( 'NONE', *, *, #202652, .T. ) ;
#150018 = ORIENTED_EDGE ( 'NONE', *, *, #92240, .F. ) ;
#150017 = EDGE_CURVE ( 'NONE', #166364, #220255, #88640, .T. ) ;
#150019 = CARTESIAN_POINT ( 'NONE',  ( 18.59999999999999076, 34.44688795055758135, -235.1500552906961730 ) ) ;
#150020 = FACE_OUTER_BOUND ( 'NONE', #162543, .T. ) ;
#150021 = AXIS2_PLACEMENT_3D ( 'NONE', #143255, #238509, #182403 ) ;
#150022 = CARTESIAN_POINT ( 'NONE',  ( -14.00000000000000178, 9.850000000011133849, -50.25000000000000711 ) ) ;
#150023 = DIRECTION ( 'NONE',  ( -1.000000000000000000, 0.000000000000000000, 0.000000000000000000 ) ) ;
#150024 = CARTESIAN_POINT ( 'NONE',  ( -21.15000000000000213, 6.540656951701243393, 6.098637220230962441E-16 ) ) ;
#150025 = ORIENTED_EDGE ( 'NONE', *, *, #92615, .F. ) ;
#150026 = CYLINDRICAL_SURFACE ( 'NONE', #183852, 0.5000000000000004441 ) ;
#150028 = CARTESIAN_POINT ( 'NONE',  ( -20.94999999999999929, 11.60000000001115339, -174.4282032302755283 ) ) ;
#150027 = CARTESIAN_POINT ( 'NONE',  ( -16.93521499325732549, 9.994786119814676795, -87.90710854109359218 ) ) ;
#150029 = DIRECTION ( 'NONE',  ( -1.000000000000000000, -2.952720810173289112E-16, 0.000000000000000000 ) ) ;
#150030 = EDGE_CURVE ( 'NONE', #86816, #157570, #40983, .T. ) ;
#150031 = FACE_OUTER_BOUND ( 'NONE', #160721, .T. ) ;
#150032 = DIRECTION ( 'NONE',  ( 1.000000000000000000, 0.000000000000000000, 0.000000000000000000 ) ) ;
#150033 = CARTESIAN_POINT ( 'NONE',  ( 18.50000000000000000, -10.35479209691423996, -161.2565409830737906 ) ) ;
#150034 = AXIS2_PLACEMENT_3D ( 'NONE', #24721, #185043, #45537 ) ;
#150036 = ORIENTED_EDGE ( 'NONE', *, *, #151227, .F. ) ;
#150035 = FACE_OUTER_BOUND ( 'NONE', #67194, .T. ) ;
#150037 = VECTOR ( 'NONE', #71567, 1000.000000000000000 ) ;
#150038 = CIRCLE ( 'NONE', #104205, 0.09999999999999939493 ) ;
#150039 = AXIS2_PLACEMENT_3D ( 'NONE', #41634, #121186, #200692 ) ;
#150040 = VECTOR ( 'NONE', #40465, 999.9999999999998863 ) ;
#150041 = CARTESIAN_POINT ( 'NONE',  ( -22.59999985501179154, 64.25013020700896504, -103.0887061543239582 ) ) ;
#150042 = EDGE_CURVE ( 'NONE', #217695, #175273, #147357, .T. ) ;
#150043 = CARTESIAN_POINT ( 'NONE',  ( -23.25000000000000000, 1.115600667400684642E-11, -104.6500000000000341 ) ) ;
#150044 = DIRECTION ( 'NONE',  ( 0.5932847527679310229, 0.8049926720990042694, 5.621233785078285907E-15 ) ) ;
#150045 = VERTEX_POINT ( 'NONE', #148658 ) ;
#150046 = AXIS2_PLACEMENT_3D ( 'NONE', #74983, #133642, #154530 ) ;
#150047 = FACE_OUTER_BOUND ( 'NONE', #87351, .T. ) ;
#150048 = VECTOR ( 'NONE', #95525, 1000.000000000000000 ) ;
#150049 = CIRCLE ( 'NONE', #16777, 11.74999999999999645 ) ;
#150050 = DIRECTION ( 'NONE',  ( -1.000000000000000000, 0.000000000000000000, -0.000000000000000000 ) ) ;
#150051 = CYLINDRICAL_SURFACE ( 'NONE', #256934, 0.09999999999999939493 ) ;
#150052 = AXIS2_PLACEMENT_3D ( 'NONE', #82581, #104707, #121770 ) ;
#150053 = AXIS2_PLACEMENT_3D ( 'NONE', #95163, #174749, #196820 ) ;
#150054 = EDGE_CURVE ( 'NONE', #71575, #102037, #28748, .T. ) ;
#150055 = EDGE_CURVE ( 'NONE', #13961, #22426, #23393, .T. ) ;
#150056 = ORIENTED_EDGE ( 'NONE', *, *, #64222, .F. ) ;
#150057 = CARTESIAN_POINT ( 'NONE',  ( -16.86578989773641624, 12.42364512751820982, -211.1234428391631752 ) ) ;
#150059 = ORIENTED_EDGE ( 'NONE', *, *, #148542, .T. ) ;
#150058 = DIRECTION ( 'NONE',  ( 0.000000000000000000, 0.000000000000000000, 1.000000000000000000 ) ) ;
#150060 = DIRECTION ( 'NONE',  ( -1.000000000000000000, -1.394253735153569469E-16, -2.602809386958778209E-16 ) ) ;
#150062 = EDGE_CURVE ( 'NONE', #82079, #144652, #129126, .T. ) ;
#150061 = CARTESIAN_POINT ( 'NONE',  ( -21.05000000000000071, 1.115600667400684642E-11, -33.50000000000000000 ) ) ;
#150063 = ADVANCED_FACE ( 'NONE', ( #123957 ), #203486, .T. ) ;
#150064 = EDGE_LOOP ( 'NONE', ( #201363, #229733 ) ) ;
#150065 = CARTESIAN_POINT ( 'NONE',  ( -16.83233564386403813, 66.06977820342787311, -190.7476281480005014 ) ) ;
#150066 = APPLICATION_PROTOCOL_DEFINITION ( 'draft international standard', 'automotive_design', 1998, #52359 ) ;
#150067 = DIRECTION ( 'NONE',  ( 1.000000000000000000, 0.000000000000000000, 0.000000000000000000 ) ) ;
#150068 = DIRECTION ( 'NONE',  ( 1.000000000000000000, 0.000000000000000000, 0.000000000000000000 ) ) ;
#150069 = EDGE_CURVE ( 'NONE', #144828, #112680, #164365, .T. ) ;
#150070 = VERTEX_POINT ( 'NONE', #151224 ) ;
#150071 = CARTESIAN_POINT ( 'NONE',  ( -23.15000000000000213, 76.00000000001170974, -69.52310748452431710 ) ) ;
#150072 = DIRECTION ( 'NONE',  ( 0.000000000000000000, -1.000000000000000000, -6.982962677686266711E-15 ) ) ;
#150073 = EDGE_CURVE ( 'NONE', #118267, #112231, #170829, .T. ) ;
#150075 = EDGE_CURVE ( 'NONE', #141594, #4508, #94543, .T. ) ;
#150074 = EDGE_CURVE ( 'NONE', #13016, #254308, #107584, .T. ) ;
#150076 = CARTESIAN_POINT ( 'NONE',  ( 20.95159278453404283, 8.907896337960206523, -175.9847201851092109 ) ) ;
#150077 = ORIENTED_EDGE ( 'NONE', *, *, #104102, .F. ) ;
#150078 = ORIENTED_EDGE ( 'NONE', *, *, #118159, .F. ) ;
#150079 = CARTESIAN_POINT ( 'NONE',  ( -20.65000000000000568, 68.75000000001232081, -157.3731074845244109 ) ) ;
#150080 = AXIS2_PLACEMENT_3D ( 'NONE', #169786, #131902, #15841 ) ;
#150081 = CARTESIAN_POINT ( 'NONE',  ( 20.94999999999999574, 76.00000000001165290, -69.52310748452431710 ) ) ;
#150082 = DIRECTION ( 'NONE',  ( 1.000000000000000000, 0.000000000000000000, 0.000000000000000000 ) ) ;
#150083 = ADVANCED_FACE ( 'NONE', ( #110792 ), #96346, .F. ) ;
#150084 = CARTESIAN_POINT ( 'NONE',  ( -20.64999999999999858, 7.150000000000000355, -21.15000000000000213 ) ) ;
#150085 = CIRCLE ( 'NONE', #250017, 11.64999999999999325 ) ;
#150087 = CARTESIAN_POINT ( 'NONE',  ( 20.05000000000002913, 68.75000000001149658, -48.67310748452437963 ) ) ;
#150086 = FACE_OUTER_BOUND ( 'NONE', #132184, .T. ) ;
#150088 = FACE_OUTER_BOUND ( 'NONE', #16198, .T. ) ;
#150090 = ADVANCED_FACE ( 'NONE', ( #55932 ), #32587, .T. ) ;
#150089 = CARTESIAN_POINT ( 'NONE',  ( 20.99999999999999645, 66.25000000001233502, -160.7731074845244166 ) ) ;
#150092 = EDGE_CURVE ( 'NONE', #85754, #30250, #230765, .T. ) ;
#150091 = CARTESIAN_POINT ( 'NONE',  ( 20.94999999999999574, 18.26942912180536638, -237.6183358664095238 ) ) ;
#150093 = ORIENTED_EDGE ( 'NONE', *, *, #125577, .F. ) ;
#150094 = CIRCLE ( 'NONE', #4300, 0.09999999999999939493 ) ;
#150096 = ORIENTED_EDGE ( 'NONE', *, *, #4086, .F. ) ;
#150095 = CARTESIAN_POINT ( 'NONE',  ( -16.88219499860498019, 12.41408822593690964, -211.2421705250320088 ) ) ;
#150097 = CARTESIAN_POINT ( 'NONE',  ( -23.15000000000000213, -11.74999999998884448, -130.9000000000000341 ) ) ;
#150099 = DIRECTION ( 'NONE',  ( 0.000000000000000000, 0.000000000000000000, -1.000000000000000000 ) ) ;
#150098 = DIRECTION ( 'NONE',  ( 0.000000000000000000, 1.000000000000000000, 0.000000000000000000 ) ) ;
#150100 = ADVANCED_FACE ( 'NONE', ( #134198 ), #131967, .F. ) ;
#150101 = B_SPLINE_CURVE_WITH_KNOTS ( 'NONE', 3,
 ( #142189, #240018, #144738, #63942, #61368, #203456, #122651, #24844, #164336, #140916, #221702, #202169, #121387 ),
 .UNSPECIFIED., .F., .F.,
 ( 4, 3, 3, 3, 4 ),
 ( 1.084999851846394431E-16, 1.946463881814305957E-05, 3.922356109944007726E-05, 4.215060953238855979E-05, 4.415117091092329025E-05 ),
 .UNSPECIFIED. ) ;
#150102 = VERTEX_POINT ( 'NONE', #131642 ) ;
#150103 = DIRECTION ( 'NONE',  ( -1.000000000000000000, -0.000000000000000000, -0.000000000000000000 ) ) ;
#150104 = DIRECTION ( 'NONE',  ( 0.000000000000000000, 0.000000000000000000, 1.000000000000000000 ) ) ;
#150105 = DIRECTION ( 'NONE',  ( 0.000000000000000000, 0.4088369013363783999, -0.9126074666063545004 ) ) ;
#150106 = VERTEX_POINT ( 'NONE', #112104 ) ;
#150107 = EDGE_CURVE ( 'NONE', #110910, #258034, #114649, .T. ) ;
#150108 = VERTEX_POINT ( 'NONE', #255385 ) ;
#150109 = AXIS2_PLACEMENT_3D ( 'NONE', #132610, #111759, #210857 ) ;
#150110 = EDGE_CURVE ( 'NONE', #55374, #90768, #182051, .T. ) ;
#150111 = CARTESIAN_POINT ( 'NONE',  ( 21.05000000000000426, 6.258817194692619879, -100.4663672646664168 ) ) ;
#150112 = VERTEX_POINT ( 'NONE', #254142 ) ;
#150113 = LINE ( 'NONE', #112265, #163829 ) ;
#150114 = CIRCLE ( 'NONE', #145979, 0.09999999999999907574 ) ;
#150115 = CIRCLE ( 'NONE', #99984, 0.09999999999999939493 ) ;
#150116 = DIRECTION ( 'NONE',  ( 0.000000000000000000, 0.000000000000000000, 1.000000000000000000 ) ) ;
#150117 = CARTESIAN_POINT ( 'NONE',  ( -21.11101077989000174, 65.53510346643489015, -242.0508478410367275 ) ) ;
#150118 = AXIS2_PLACEMENT_3D ( 'NONE', #124913, #225258, #123626 ) ;
#150119 = CARTESIAN_POINT ( 'NONE',  ( 21.00000000000000000, 6.356682116888462630, 11.91686199900910381 ) ) ;
#150120 = ORIENTED_EDGE ( 'NONE', *, *, #3716, .T. ) ;
#150121 = DIRECTION ( 'NONE',  ( 0.000000000000000000, -0.1298341882520124002, -0.9915357197604841577 ) ) ;
#150122 = DIRECTION ( 'NONE',  ( 0.5000000000001141309, 0.7903412497644213275, 0.3540631425617453143 ) ) ;
#150123 = DIRECTION ( 'NONE',  ( 1.000000000000000000, -7.304098846218134667E-16, 4.607487905232622991E-31 ) ) ;
#150124 = CARTESIAN_POINT ( 'NONE',  ( -23.25000000000000000, 45.93315328338058379, -256.6017782078560003 ) ) ;
#150125 = DIRECTION ( 'NONE',  ( 0.000000000000000000, 0.000000000000000000, -1.000000000000000000 ) ) ;
#150127 = TOROIDAL_SURFACE ( 'NONE', #12570, 0.2000000000000000111, 0.1000000000000000056 ) ;
#150126 = FACE_OUTER_BOUND ( 'NONE', #24885, .T. ) ;
#150128 = AXIS2_PLACEMENT_3D ( 'NONE', #111030, #58731, #100425 ) ;
#150129 = LINE ( 'NONE', #11903, #53223 ) ;
#150130 = VERTEX_POINT ( 'NONE', #190356 ) ;
#150132 = DIRECTION ( 'NONE',  ( 1.000000000000000000, 0.000000000000000000, 0.000000000000000000 ) ) ;
#150131 = DIRECTION ( 'NONE',  ( 1.000000000000000000, 0.000000000000000000, 0.000000000000000000 ) ) ;
#150133 = ORIENTED_EDGE ( 'NONE', *, *, #218514, .F. ) ;
#150135 = ORIENTED_EDGE ( 'NONE', *, *, #141443, .T. ) ;
#150134 = DIRECTION ( 'NONE',  ( 1.000000000000000000, 0.000000000000000000, -0.000000000000000000 ) ) ;
#150136 = ORIENTED_EDGE ( 'NONE', *, *, #14765, .F. ) ;
#150137 = LINE ( 'NONE', #229655, #132437 ) ;
#150138 = CARTESIAN_POINT ( 'NONE',  ( 14.88075390448864255, 66.56831044948815190, -151.7438174522883685 ) ) ;
#150139 = DIRECTION ( 'NONE',  ( -0.000000000000000000, 0.000000000000000000, 1.000000000000000000 ) ) ;
#150140 = CARTESIAN_POINT ( 'NONE',  ( -20.00857864376270001, 66.75000000001205080, -124.1731074845243654 ) ) ;
#150141 = EDGE_LOOP ( 'NONE', ( #247184, #205673 ) ) ;
#150142 = CARTESIAN_POINT ( 'NONE',  ( -21.59142135623730852, 68.15000000001150227, -48.37310748452437537 ) ) ;
#150143 = DIRECTION ( 'NONE',  ( 0.000000000000000000, 0.9770955615653551529, 0.2128009952262517601 ) ) ;
#150144 = EDGE_LOOP ( 'NONE', ( #110511, #154653, #78662 ) ) ;
#150145 = CARTESIAN_POINT ( 'NONE',  ( 18.45036689428329524, -9.490184143317863530, -174.5126958274863114 ) ) ;
#150146 = VECTOR ( 'NONE', #8681, 1000.000000000000000 ) ;
#150147 = EDGE_CURVE ( 'NONE', #9223, #11705, #119698, .T. ) ;
#150149 = AXIS2_PLACEMENT_3D ( 'NONE', #254822, #56640, #93230 ) ;
#150148 = CARTESIAN_POINT ( 'NONE',  ( 23.25000000000000000, -11.74999999999999112, -12.15000000000000036 ) ) ;
#150150 = VERTEX_POINT ( 'NONE', #251592 ) ;
#150151 = EDGE_CURVE ( 'NONE', #111166, #38307, #192911, .T. ) ;
#150152 = DIRECTION ( 'NONE',  ( 1.000000000000000000, 0.000000000000000000, 0.000000000000000000 ) ) ;
#150153 = EDGE_LOOP ( 'NONE', ( #112070, #255418, #68664, #92760 ) ) ;
#150154 = TOROIDAL_SURFACE ( 'NONE', #216761, 11.90000000000000391, 0.1000000000000000056 ) ;
#150155 = CARTESIAN_POINT ( 'NONE',  ( 18.47654891039379521, -9.465274948371149577, -141.1259759051946219 ) ) ;
#150156 = ORIENTED_EDGE ( 'NONE', *, *, #230819, .T. ) ;
#150157 = CARTESIAN_POINT ( 'NONE',  ( 21.05000000000000071, 76.10000000001241460, -176.5637644362255969 ) ) ;
#150158 = ADVANCED_FACE ( 'NONE', ( #53393 ), #14293, .T. ) ;
#150159 = EDGE_CURVE ( 'NONE', #114284, #139879, #94445, .T. ) ;
#150160 = FACE_OUTER_BOUND ( 'NONE', #153388, .T. ) ;
#150161 = CARTESIAN_POINT ( 'NONE',  ( 18.39999999999999858, -9.599999999988845900, -207.6001893912220169 ) ) ;
#150162 = CARTESIAN_POINT ( 'NONE',  ( 33.80000000000000426, 3.175288713399626594, -347.0000000000001137 ) ) ;
#150163 = VECTOR ( 'NONE', #60226, 1000.000000000000227 ) ;
#150164 = LINE ( 'NONE', #124179, #3084 ) ;
#150165 = FACE_OUTER_BOUND ( 'NONE', #192447, .T. ) ;
#150166 = ORIENTED_EDGE ( 'NONE', *, *, #106681, .T. ) ;
#150167 = DIRECTION ( 'NONE',  ( 0.000000000000000000, 1.000000000000000000, 0.000000000000000000 ) ) ;
#150168 = ORIENTED_EDGE ( 'NONE', *, *, #252743, .T. ) ;
#150170 = DIRECTION ( 'NONE',  ( 0.000000000000000000, 0.008583690987128059571, -0.9999631594459056361 ) ) ;
#150169 = CARTESIAN_POINT ( 'NONE',  ( 12.25000000000000000, 66.15000000001155911, -52.77310748452439526 ) ) ;
#150171 = EDGE_CURVE ( 'NONE', #55997, #175744, #44682, .T. ) ;
#150172 = ORIENTED_EDGE ( 'NONE', *, *, #28374, .T. ) ;
#150173 = LINE ( 'NONE', #3238, #209882 ) ;
#150174 = CARTESIAN_POINT ( 'NONE',  ( -20.85000000000000142, 77.83585931145526615, -58.01866831572577610 ) ) ;
#150175 = DIRECTION ( 'NONE',  ( 0.000000000000000000, -1.000000000000000000, 0.000000000000000000 ) ) ;
#150176 = CARTESIAN_POINT ( 'NONE',  ( 20.95539060131842746, 58.98120222732934792, -225.6874131423334404 ) ) ;
#150177 = ORIENTED_EDGE ( 'NONE', *, *, #227532, .T. ) ;
#150179 = ORIENTED_EDGE ( 'NONE', *, *, #45193, .T. ) ;
#150178 = DIRECTION ( 'NONE',  ( -1.000000000000000000, 1.638248138805453496E-14, 3.058301029676582006E-14 ) ) ;
#150181 = CARTESIAN_POINT ( 'NONE',  ( -16.89318236219977010, 66.04846474213746887, -190.8782371166302880 ) ) ;
#150180 = SPHERICAL_SURFACE ( 'NONE', #205257, 0.1000000000000000056 ) ;
#150183 = ORIENTED_EDGE ( 'NONE', *, *, #150943, .F. ) ;
#150182 = LINE ( 'NONE', #206294, #148864 ) ;
#150184 = CIRCLE ( 'NONE', #37765, 0.5999999999999894307 ) ;
#150185 = ORIENTED_EDGE ( 'NONE', *, *, #145977, .F. ) ;
#150186 = B_SPLINE_CURVE_WITH_KNOTS ( 'NONE', 3,
 ( #84003, #226110, #22830, #1932, #163606, #82736, #166205, #47483, #220988, #25393, #206578, #222255, #184438, #27979, #81456, #5781, #161040, #42366, #181882 ),
 .UNSPECIFIED., .F., .F.,
 ( 4, 3, 3, 3, 3, 3, 4 ),
 ( -2.000416914656963086E-06, 0.000000000000000000, 4.714008503746661030E-05, 9.979203887778580651E-05, 0.0001372215519229558309, 0.0001635031576221024189, 0.0001900083748504180947 ),
 .UNSPECIFIED. ) ;
#150187 = EDGE_CURVE ( 'NONE', #111286, #118730, #50798, .T. ) ;
#150188 = LINE ( 'NONE', #28987, #255940 ) ;
#150189 = CARTESIAN_POINT ( 'NONE',  ( 21.05000000000000071, 67.18479819544494092, -94.60256998784034010 ) ) ;
#150190 = EDGE_LOOP ( 'NONE', ( #64527, #233014, #1698, #127728, #151496 ) ) ;
#150191 = CARTESIAN_POINT ( 'NONE',  ( -18.40000000000000213, 54.02969457822032950, -229.1974241798695004 ) ) ;
#150192 = ORIENTED_EDGE ( 'NONE', *, *, #46402, .F. ) ;
#150193 = VECTOR ( 'NONE', #125624, 1000.000000000000000 ) ;
#150194 = CARTESIAN_POINT ( 'NONE',  ( -18.59999999999999787, 64.40000000001208491, -129.5949042542488314 ) ) ;
#150195 = CYLINDRICAL_SURFACE ( 'NONE', #201588, 0.1000000000000028644 ) ;
#150196 = ORIENTED_EDGE ( 'NONE', *, *, #173531, .T. ) ;
#150197 = EDGE_CURVE ( 'NONE', #182384, #184113, #252955, .T. ) ;
#150198 = DIRECTION ( 'NONE',  ( 0.000000000000000000, 0.000000000000000000, -1.000000000000000000 ) ) ;
#150199 = ADVANCED_FACE ( 'NONE', ( #59779 ), #38980, .F. ) ;
#150200 = ORIENTED_EDGE ( 'NONE', *, *, #17698, .T. ) ;
#150201 = CIRCLE ( 'NONE', #129333, 1.749999999999998002 ) ;
#150202 = CARTESIAN_POINT ( 'NONE',  ( -20.94999999999999929, 5.900000000011102586, -177.7190997646563915 ) ) ;
#150203 = AXIS2_PLACEMENT_3D ( 'NONE', #203027, #2249, #42677 ) ;
#150204 = EDGE_CURVE ( 'NONE', #106325, #62255, #36316, .T. ) ;
#150205 = VERTEX_POINT ( 'NONE', #196744 ) ;
#150206 = ORIENTED_EDGE ( 'NONE', *, *, #253933, .F. ) ;
#150207 = CARTESIAN_POINT ( 'NONE',  ( -18.41809261886924887, -9.682403314745313239, -73.65684355009136652 ) ) ;
#150208 = VECTOR ( 'NONE', #167069, 1000.000000000000000 ) ;
#150209 = ORIENTED_EDGE ( 'NONE', *, *, #32133, .T. ) ;
#150210 = CYLINDRICAL_SURFACE ( 'NONE', #158869, 0.09999999999999939493 ) ;
#150211 = EDGE_LOOP ( 'NONE', ( #209265, #32573, #137938, #116830 ) ) ;
#150213 = ORIENTED_EDGE ( 'NONE', *, *, #256705, .F. ) ;
#150212 = DIRECTION ( 'NONE',  ( 1.000000000000000000, 0.000000000000000000, 0.000000000000000000 ) ) ;
#150214 = ADVANCED_FACE ( 'NONE', ( #239739 ), #218865, .F. ) ;
#150215 = AXIS2_PLACEMENT_3D ( 'NONE', #207780, #151666, #30419 ) ;
#150216 = EDGE_CURVE ( 'NONE', #46719, #203112, #19747, .T. ) ;
#150217 = CIRCLE ( 'NONE', #191926, 0.1000000000000032391 ) ;
#150218 = ORIENTED_EDGE ( 'NONE', *, *, #126881, .F. ) ;
#150219 = CYLINDRICAL_SURFACE ( 'NONE', #1794, 0.09999999999999939493 ) ;
#150220 = ORIENTED_EDGE ( 'NONE', *, *, #232934, .F. ) ;
#150223 = EDGE_LOOP ( 'NONE', ( #195493, #192943, #10952, #223311, #108773, #107095, #242222, #221489, #77041, #115909, #71342, #35212, #112173, #8474 ) ) ;
#150222 = VERTEX_POINT ( 'NONE', #40282 ) ;
#150221 = CYLINDRICAL_SURFACE ( 'NONE', #10502, 0.1000000000000028644 ) ;
#150224 = EDGE_CURVE ( 'NONE', #92785, #179371, #173908, .T. ) ;
#150225 = DIRECTION ( 'NONE',  ( -1.000000000000000000, -3.265361837132813093E-16, 0.000000000000000000 ) ) ;
#150226 = ORIENTED_EDGE ( 'NONE', *, *, #39101, .T. ) ;
#150227 = CIRCLE ( 'NONE', #62733, 11.74999999999999822 ) ;
#150228 = CIRCLE ( 'NONE', #75218, 0.1000000000000002554 ) ;
#150229 = AXIS2_PLACEMENT_3D ( 'NONE', #142942, #178276, #137813 ) ;
#150230 = VECTOR ( 'NONE', #184954, 1000.000000000000000 ) ;
#150231 = CIRCLE ( 'NONE', #246084, 11.64999999999999325 ) ;
#150232 = DIRECTION ( 'NONE',  ( 0.7071359030027619674, 0.6908824414808002468, 0.1504668293611484409 ) ) ;
#150233 = ORIENTED_EDGE ( 'NONE', *, *, #228535, .T. ) ;
#150234 = DIRECTION ( 'NONE',  ( 0.000000000000000000, 1.734723475976807292E-15, -1.000000000000000000 ) ) ;
#150235 = EDGE_CURVE ( 'NONE', #216303, #229799, #40619, .T. ) ;
#150237 = VERTEX_POINT ( 'NONE', #98901 ) ;
#150236 = DIRECTION ( 'NONE',  ( 1.000000000000000000, -0.000000000000000000, -0.000000000000000000 ) ) ;
#150238 = DIRECTION ( 'NONE',  ( 7.304098846218134667E-16, -1.000000000000000000, 0.000000000000000000 ) ) ;
#150239 = ORIENTED_EDGE ( 'NONE', *, *, #53569, .T. ) ;
#150240 = CARTESIAN_POINT ( 'NONE',  ( 18.54999999999999716, 8.750000000011182166, -76.25000000000004263 ) ) ;
#150241 = CARTESIAN_POINT ( 'NONE',  ( -18.59999999999999787, -1.866714910046153308, -78.75267524628205251 ) ) ;
#150242 = ORIENTED_EDGE ( 'NONE', *, *, #164123, .T. ) ;
#150243 = DIRECTION ( 'NONE',  ( 0.000000000000000000, 7.086529944415894657E-15, -1.000000000000000000 ) ) ;
#150244 = VECTOR ( 'NONE', #88312, 1000.000000000000000 ) ;
#150245 = DIRECTION ( 'NONE',  ( 1.000000000000000000, 0.000000000000000000, 0.000000000000000000 ) ) ;
#150246 = ORIENTED_EDGE ( 'NONE', *, *, #119760, .F. ) ;
#150248 = ORIENTED_EDGE ( 'NONE', *, *, #145945, .T. ) ;
#150247 = DIRECTION ( 'NONE',  ( 1.000000000000000000, 0.000000000000000000, 0.000000000000000000 ) ) ;
#150249 = LINE ( 'NONE', #189366, #36022 ) ;
#150251 = ORIENTED_EDGE ( 'NONE', *, *, #69120, .T. ) ;
#150250 = ORIENTED_EDGE ( 'NONE', *, *, #44466, .F. ) ;
#150252 = VERTEX_POINT ( 'NONE', #23281 ) ;
#150253 = CARTESIAN_POINT ( 'NONE',  ( -17.04761207306817283, 65.97354912661477044, -182.6731074845243938 ) ) ;
#150254 = ORIENTED_EDGE ( 'NONE', *, *, #251362, .F. ) ;
#150255 = ORIENTED_EDGE ( 'NONE', *, *, #34728, .F. ) ;
#150256 = DIRECTION ( 'NONE',  ( -3.469446951953515108E-14, -1.000000000000000000, 0.000000000000000000 ) ) ;
#150257 = ORIENTED_EDGE ( 'NONE', *, *, #82646, .F. ) ;
#150258 = CARTESIAN_POINT ( 'NONE',  ( 20.94999999999999574, 6.400000000011158541, -143.9304246300615944 ) ) ;
#150259 = DIRECTION ( 'NONE',  ( 0.000000000000000000, 0.4999999999999956701, -0.8660254037844411501 ) ) ;
#150260 = AXIS2_PLACEMENT_3D ( 'NONE', #122636, #104306, #5200 ) ;
#150261 = ORIENTED_EDGE ( 'NONE', *, *, #221935, .F. ) ;
#150262 = EDGE_LOOP ( 'NONE', ( #41583, #215453, #130634, #101674 ) ) ;
#150263 = DIRECTION ( 'NONE',  ( -1.000000000000000000, 0.000000000000000000, 0.000000000000000000 ) ) ;
#150264 = ORIENTED_EDGE ( 'NONE', *, *, #148297, .F. ) ;
#150265 = AXIS2_PLACEMENT_3D ( 'NONE', #23505, #83405, #225488 ) ;
#150266 = AXIS2_PLACEMENT_3D ( 'NONE', #234323, #111829, #135212 ) ;
#150267 = DIRECTION ( 'NONE',  ( 0.000000000000000000, -1.000000000000000000, -0.000000000000000000 ) ) ;
#150268 = ORIENTED_EDGE ( 'NONE', *, *, #135677, .T. ) ;
#150269 = FACE_OUTER_BOUND ( 'NONE', #122493, .T. ) ;
#150270 = EDGE_CURVE ( 'NONE', #194241, #114996, #19407, .T. ) ;
#150272 = ORIENTED_EDGE ( 'NONE', *, *, #222541, .F. ) ;
#150271 = CYLINDRICAL_SURFACE ( 'NONE', #254477, 0.09999999999998898659 ) ;
#150273 = CARTESIAN_POINT ( 'NONE',  ( 21.10257677756356642, 0.02495074957914743610, -127.6016182574673508 ) ) ;
#150274 = CARTESIAN_POINT ( 'NONE',  ( -18.59999999999999787, 1.115600667400684642E-11, -167.4999999999999716 ) ) ;
#150275 = DIRECTION ( 'NONE',  ( 0.000000000000000000, 0.000000000000000000, 1.000000000000000000 ) ) ;
#150276 = CARTESIAN_POINT ( 'NONE',  ( -21.05000000000000071, -11.74999999998884448, -197.9999999999999432 ) ) ;
#150277 = CARTESIAN_POINT ( 'NONE',  ( -16.89060415895971090, 66.04877923721008415, -157.3771872602539474 ) ) ;
#150278 = AXIS2_PLACEMENT_3D ( 'NONE', #240072, #40623, #100514 ) ;
#150279 = EDGE_CURVE ( 'NONE', #247441, #14757, #157674, .T. ) ;
#150280 = CARTESIAN_POINT ( 'NONE',  ( -18.59999999999999787, 1.115600667400684642E-11, -134.0000000000000284 ) ) ;
#150282 = ADVANCED_FACE ( 'NONE', ( #37707 ), #42816, .T. ) ;
#150281 = CARTESIAN_POINT ( 'NONE',  ( -21.05000000000000071, 6.257814610487270279, -33.40220970869120265 ) ) ;
#150283 = CARTESIAN_POINT ( 'NONE',  ( 18.33996824403459414, 38.15118265298796274, -261.2066690643014226 ) ) ;
#150284 = DIRECTION ( 'NONE',  ( -1.000000000000000000, 0.000000000000000000, 0.000000000000000000 ) ) ;
#150285 = CIRCLE ( 'NONE', #158673, 0.09999999999999939493 ) ;
#150286 = ORIENTED_EDGE ( 'NONE', *, *, #185225, .T. ) ;
#150287 = AXIS2_PLACEMENT_3D ( 'NONE', #106645, #102790, #83224 ) ;
#150288 = CIRCLE ( 'NONE', #237, 0.09999999999999939493 ) ;
#150289 = EDGE_LOOP ( 'NONE', ( #157738, #94823, #149441, #52151 ) ) ;
#150291 = ORIENTED_EDGE ( 'NONE', *, *, #86441, .T. ) ;
#150290 = CARTESIAN_POINT ( 'NONE',  ( 23.25000000000000000, -11.48912529306489994, -97.40000000000004832 ) ) ;
#150292 = ORIENTED_EDGE ( 'NONE', *, *, #97469, .F. ) ;
#150293 = EDGE_CURVE ( 'NONE', #156376, #44654, #2381, .T. ) ;
#150294 = DIRECTION ( 'NONE',  ( -3.712277463076317983E-14, -0.1686199900910448357, 0.9856811345164804283 ) ) ;
#150295 = DIRECTION ( 'NONE',  ( 0.000000000000000000, -0.8814952561679687548, 0.4721928772793668183 ) ) ;
#150297 = CARTESIAN_POINT ( 'NONE',  ( 21.05000000000000071, -8.999999999988842703, -158.0060308773475697 ) ) ;
#150296 = CARTESIAN_POINT ( 'NONE',  ( 18.79999999999999716, -1.800000000000000044, -11.61130914238355771 ) ) ;
#150298 = ORIENTED_EDGE ( 'NONE', *, *, #224031, .F. ) ;
#150299 = EDGE_LOOP ( 'NONE', ( #250619, #64658, #182283, #164887 ) ) ;
#150300 = CARTESIAN_POINT ( 'NONE',  ( -16.87683809663752399, 9.850000000011144508, -154.0976359818037054 ) ) ;
#150301 = CYLINDRICAL_SURFACE ( 'NONE', #116495, 2.000000000000001776 ) ;
#150302 = ORIENTED_EDGE ( 'NONE', *, *, #43529, .T. ) ;
#150303 = ORIENTED_EDGE ( 'NONE', *, *, #102329, .T. ) ;
#150304 = LINE ( 'NONE', #107303, #158953 ) ;
#150305 = CYLINDRICAL_SURFACE ( 'NONE', #253726, 0.09999999999999939493 ) ;
#150306 = DIRECTION ( 'NONE',  ( -1.000000000000000000, 2.952720810173289112E-16, 2.061873921506763405E-30 ) ) ;
#150307 = EDGE_CURVE ( 'NONE', #206012, #38559, #115396, .T. ) ;
#150308 = CARTESIAN_POINT ( 'NONE',  ( -18.59999999999999787, 70.10000000001163301, -59.30400771986794695 ) ) ;
#150310 = ORIENTED_EDGE ( 'NONE', *, *, #59368, .F. ) ;
#150309 = CARTESIAN_POINT ( 'NONE',  ( 20.85000000000000142, 77.83585931145498193, -24.51866831572578675 ) ) ;
#150311 = EDGE_CURVE ( 'NONE', #227184, #207317, #80630, .T. ) ;
#150312 = CARTESIAN_POINT ( 'NONE',  ( 23.24999999999999289, 62.92003201576280702, -207.2439188921395612 ) ) ;
#150313 = DIRECTION ( 'NONE',  ( 0.000000000000000000, -0.9550021345545530727, 0.2965989261549131228 ) ) ;
#150314 = CARTESIAN_POINT ( 'NONE',  ( -22.50000000000000000, 75.90000000001273861, -211.3138870828977645 ) ) ;
#150315 = LINE ( 'NONE', #125594, #54243 ) ;
#150316 = ORIENTED_EDGE ( 'NONE', *, *, #193392, .T. ) ;
#150317 = CARTESIAN_POINT ( 'NONE',  ( 22.39999999999999503, 76.00000000001246292, -181.6726782920691505 ) ) ;
#150318 = CARTESIAN_POINT ( 'NONE',  ( 22.50000000000000000, 7.750000000011162626, -167.3999999999999773 ) ) ;
#150319 = VECTOR ( 'NONE', #132481, 1000.000000000000000 ) ;
#150322 = CARTESIAN_POINT ( 'NONE',  ( 11.60000000000006004, 64.35000000001120668, -21.02310748452479316 ) ) ;
#150321 = AXIS2_PLACEMENT_3D ( 'NONE', #168330, #66617, #247817 ) ;
#150320 = CARTESIAN_POINT ( 'NONE',  ( 21.05000000000000071, 5.500000000011153745, -79.40526601891313874 ) ) ;
#150323 = DIRECTION ( 'NONE',  ( 0.000000000000000000, 0.000000000000000000, 1.000000000000000000 ) ) ;
#150324 = EDGE_CURVE ( 'NONE', #187769, #78774, #102757, .T. ) ;
#150325 = AXIS2_PLACEMENT_3D ( 'NONE', #19836, #99324, #181477 ) ;
#150326 = FACE_OUTER_BOUND ( 'NONE', #106668, .T. ) ;
#150327 = CARTESIAN_POINT ( 'NONE',  ( -16.77779411440718604, 66.05389855290391665, -48.68616490152893306 ) ) ;
#150328 = CARTESIAN_POINT ( 'NONE',  ( -18.59999999999999787, 52.81534179157634412, -244.1198638051726277 ) ) ;
#150329 = CARTESIAN_POINT ( 'NONE',  ( 21.30000000000002558, 76.00000000001210765, -132.4731074845242915 ) ) ;
#150330 = ORIENTED_EDGE ( 'NONE', *, *, #38548, .T. ) ;
#150331 = VERTEX_POINT ( 'NONE', #62382 ) ;
#150333 = ORIENTED_EDGE ( 'NONE', *, *, #120685, .F. ) ;
#150332 = B_SPLINE_CURVE_WITH_KNOTS ( 'NONE', 3,
 ( #71897, #14505, #88850, #131850, #130560, #251799, #249245, #191863, #93997, #133141, #168471, #108443, #32793, #109706, #207556, #228401, #171036, #229677, #232262 ),
 .UNSPECIFIED., .F., .F.,
 ( 4, 3, 3, 3, 3, 3, 4 ),
 ( -2.000416914662652606E-06, 0.000000000000000000, 4.714008503746095890E-05, 9.979203887777572343E-05, 0.0001372215519229490546, 0.0001635031576220952632, 0.0001900083748504098548 ),
 .UNSPECIFIED. ) ;
#150334 = CARTESIAN_POINT ( 'NONE',  ( 20.30466543256828160, 66.69576306075641980, -94.76944483313239687 ) ) ;
#150335 = DIRECTION ( 'NONE',  ( 0.7071067811865485719, -0.6233112732207607420, 0.3338907855510729328 ) ) ;
#150336 = EDGE_LOOP ( 'NONE', ( #239948, #67440, #93028, #37397 ) ) ;
#150337 = CIRCLE ( 'NONE', #12977, 0.1000000000000124678 ) ;
#150339 = EDGE_CURVE ( 'NONE', #196889, #135153, #82232, .T. ) ;
#150338 = ORIENTED_EDGE ( 'NONE', *, *, #200956, .F. ) ;
#150340 =( NAMED_UNIT ( * ) PLANE_ANGLE_UNIT ( ) SI_UNIT ( $, .RADIAN. ) );
#150341 = ORIENTED_EDGE ( 'NONE', *, *, #112888, .T. ) ;
#150342 = CARTESIAN_POINT ( 'NONE',  ( 23.14999999999999503, 64.35000000001258513, -191.2731074845244450 ) ) ;
#150343 = ORIENTED_EDGE ( 'NONE', *, *, #90030, .F. ) ;
#150344 = CARTESIAN_POINT ( 'NONE',  ( -20.64999999999999858, 2.000000000011154189, -87.67537807723795140 ) ) ;
#150345 = CARTESIAN_POINT ( 'NONE',  ( -23.15000000000000213, 76.00000000001210765, -132.3731074845242972 ) ) ;
#150346 = FACE_OUTER_BOUND ( 'NONE', #135877, .T. ) ;
#150347 = EDGE_CURVE ( 'NONE', #2383, #222373, #219626, .T. ) ;
#150348 = CARTESIAN_POINT ( 'NONE',  ( 23.14999999999999503, 64.25000000001172396, -81.27310748452440237 ) ) ;
#150349 = CARTESIAN_POINT ( 'NONE',  ( -18.59999999999999787, 1.006414599850383507, -224.3937905772586703 ) ) ;
#150351 = ORIENTED_EDGE ( 'NONE', *, *, #160941, .F. ) ;
#150350 = CARTESIAN_POINT ( 'NONE',  ( 23.24999999999999645, 71.22429906543206357, -47.87187558857032599 ) ) ;
#150353 = CARTESIAN_POINT ( 'NONE',  ( 21.05000005001280172, 8.871279691782060439, -79.17794758824591383 ) ) ;
#150352 = DIRECTION ( 'NONE',  ( -1.000000000000000000, 0.000000000000000000, 0.000000000000000000 ) ) ;
#150355 = CARTESIAN_POINT ( 'NONE',  ( -18.40000000000000213, 64.66825945288707089, -149.1731074845244507 ) ) ;
#150354 = AXIS2_PLACEMENT_3D ( 'NONE', #82044, #24708, #65083 ) ;
#150356 = ORIENTED_EDGE ( 'NONE', *, *, #110454, .T. ) ;
#150357 = CARTESIAN_POINT ( 'NONE',  ( 13.43443725621852991, 66.55344247693950877, -121.4331655301785133 ) ) ;
#150358 = CARTESIAN_POINT ( 'NONE',  ( -13.12432614554022869, 9.430764995433476017, -115.7305373947504989 ) ) ;
#150359 = EDGE_CURVE ( 'NONE', #62504, #163148, #148748, .T. ) ;
#150360 = EDGE_CURVE ( 'NONE', #136156, #18425, #198026, .T. ) ;
#150361 = ORIENTED_EDGE ( 'NONE', *, *, #629, .F. ) ;
#150362 = AXIS2_PLACEMENT_3D ( 'NONE', #132100, #111254, #92962 ) ;
#150363 = DIRECTION ( 'NONE',  ( 0.000000000000000000, -1.000000000000000000, 6.308085367188393199E-16 ) ) ;
#150364 = AXIS2_PLACEMENT_3D ( 'NONE', #122904, #160766, #204970 ) ;
#150365 = CARTESIAN_POINT ( 'NONE',  ( 20.04999999999999716, 67.25000000001185185, -90.37310748452436826 ) ) ;
#150366 = EDGE_LOOP ( 'NONE', ( #138904, #223513, #133128, #32134 ) ) ;
#150368 = EDGE_CURVE ( 'NONE', #187906, #168580, #64932, .T. ) ;
#150367 = ADVANCED_FACE ( 'NONE', ( #124926 ), #4934, .T. ) ;
#150369 = FACE_OUTER_BOUND ( 'NONE', #215260, .T. ) ;
#150371 = EDGE_CURVE ( 'NONE', #11889, #145377, #157119, .T. ) ;
#150370 = AXIS2_PLACEMENT_3D ( 'NONE', #68238, #129498, #150352 ) ;
#150372 = FACE_OUTER_BOUND ( 'NONE', #155683, .T. ) ;
#150373 = CARTESIAN_POINT ( 'NONE',  ( -21.00857864376268935, 64.40000000001234071, -163.0949042542488883 ) ) ;
#150374 = ORIENTED_EDGE ( 'NONE', *, *, #193849, .F. ) ;
#150375 = ADVANCED_FACE ( 'NONE', ( #164052 ), #61423, .T. ) ;
#150376 = VERTEX_POINT ( 'NONE', #28427 ) ;
#150377 = CARTESIAN_POINT ( 'NONE',  ( -20.64999999999999858, 68.75000000001260503, -191.1731074845243938 ) ) ;
#150378 = CARTESIAN_POINT ( 'NONE',  ( -23.15000000000000213, 11.65000000001115588, -193.9851942293460070 ) ) ;
#150379 = EDGE_CURVE ( 'NONE', #239691, #121060, #223720, .T. ) ;
#150380 = CARTESIAN_POINT ( 'NONE',  ( 20.90851465518106167, 65.67467670974468774, -164.4531731826884879 ) ) ;
#150381 = DIRECTION ( 'NONE',  ( 1.000000000000000000, 0.000000000000000000, 0.000000000000000000 ) ) ;
#150383 = CARTESIAN_POINT ( 'NONE',  ( -20.94999999999999929, -1.164121893230052995, -108.2148480855716457 ) ) ;
#150382 = LINE ( 'NONE', #112536, #209173 ) ;
#150384 = CIRCLE ( 'NONE', #37966, 0.09999999999999939493 ) ;
#150385 = DIRECTION ( 'NONE',  ( 0.000000000000000000, 0.000000000000000000, -1.000000000000000000 ) ) ;
#150387 = EDGE_CURVE ( 'NONE', #208354, #135788, #94730, .T. ) ;
#150386 = PLANE ( 'NONE',  #214236 ) ;
#150390 = ADVANCED_FACE ( 'NONE', ( #225273 ), #6236, .F. ) ;
#150389 = CARTESIAN_POINT ( 'NONE',  ( 21.04999999999999361, 30.92254191997125190, -252.0827843769733931 ) ) ;
#150388 = VECTOR ( 'NONE', #18946, 1000.000000000000000 ) ;
#150391 = ORIENTED_EDGE ( 'NONE', *, *, #73520, .F. ) ;
#150392 = DIRECTION ( 'NONE',  ( -1.000000000000000000, 0.000000000000000000, 0.000000000000000000 ) ) ;
#150393 = VECTOR ( 'NONE', #43345, 1000.000000000000114 ) ;
#150394 = ORIENTED_EDGE ( 'NONE', *, *, #202755, .F. ) ;
#150395 = CARTESIAN_POINT ( 'NONE',  ( 20.94999999999999929, 17.06838326776701109, -224.6250846885016870 ) ) ;
#150396 = CARTESIAN_POINT ( 'NONE',  ( -18.59999999999999787, 76.00000000001165290, -69.52310748452431710 ) ) ;
#150397 = DIRECTION ( 'NONE',  ( 0.000000000000000000, 0.000000000000000000, -1.000000000000000000 ) ) ;
#150398 = CONICAL_SURFACE ( 'NONE', #133619, 6.250000000000005329, 0.7853981633974431720 ) ;
#150399 = DIRECTION ( 'NONE',  ( 0.000000000000000000, 0.000000000000000000, -1.000000000000000000 ) ) ;
#150400 = EDGE_CURVE ( 'NONE', #203545, #72122, #212707, .T. ) ;
#150401 = CARTESIAN_POINT ( 'NONE',  ( 23.14999999999999858, 72.23597390491818260, -202.5022707907005497 ) ) ;
#150403 = ORIENTED_EDGE ( 'NONE', *, *, #240596, .F. ) ;
#150402 = DIRECTION ( 'NONE',  ( 2.952720810173289112E-16, -0.9770955615653318382, -0.2128009952263588411 ) ) ;
#150404 = DIRECTION ( 'NONE',  ( 1.000000000000000000, 0.000000000000000000, 0.000000000000000000 ) ) ;
#150405 = CARTESIAN_POINT ( 'NONE',  ( 18.49999999999999289, 6.450000000011156587, -54.65000000000000568 ) ) ;
#150406 = TOROIDAL_SURFACE ( 'NONE', #191925, 0.4000000000000012990, 0.1000000000000000056 ) ;
#150407 = CARTESIAN_POINT ( 'NONE',  ( 22.39999999999999503, 11.65000000001116298, -133.9000000000000057 ) ) ;
#150408 = DIRECTION ( 'NONE',  ( 1.000000000000000000, 0.000000000000000000, -0.000000000000000000 ) ) ;
#150409 = AXIS2_PLACEMENT_3D ( 'NONE', #67078, #108769, #47490 ) ;
#150410 = ORIENTED_EDGE ( 'NONE', *, *, #97112, .F. ) ;
#150411 = CARTESIAN_POINT ( 'NONE',  ( 18.54147908293611735, -7.746487623352177110, -209.9012881796168983 ) ) ;
#150412 = ADVANCED_FACE ( 'NONE', ( #224004 ), #126186, .F. ) ;
#150413 = ORIENTED_EDGE ( 'NONE', *, *, #76968, .F. ) ;
#150414 = EDGE_CURVE ( 'NONE', #241350, #194536, #111324, .T. ) ;
#150415 = ADVANCED_FACE ( 'NONE', ( #27137 ), #227865, .T. ) ;
#150416 = DIRECTION ( 'NONE',  ( -1.000000000000000000, -0.000000000000000000, -0.000000000000000000 ) ) ;
#150417 = ORIENTED_EDGE ( 'NONE', *, *, #39788, .F. ) ;
#150419 = DIRECTION ( 'NONE',  ( 1.000000000000000000, 0.000000000000000000, 0.000000000000000000 ) ) ;
#150418 = VECTOR ( 'NONE', #231519, 1000.000000000000000 ) ;
#150420 = CIRCLE ( 'NONE', #208681, 0.5000000000000004441 ) ;
#150421 = VECTOR ( 'NONE', #104468, 1000.000000000000000 ) ;
#150422 = VERTEX_POINT ( 'NONE', #104040 ) ;
#150423 = CIRCLE ( 'NONE', #204557, 0.09999999999999939493 ) ;
#150424 = CYLINDRICAL_SURFACE ( 'NONE', #176801, 0.09999999999998898659 ) ;
#150425 = FACE_OUTER_BOUND ( 'NONE', #160600, .T. ) ;
#150426 = DIRECTION ( 'NONE',  ( -1.000000000000000000, 0.000000000000000000, 0.000000000000000000 ) ) ;
#150427 = VERTEX_POINT ( 'NONE', #203164 ) ;
#150428 = EDGE_CURVE ( 'NONE', #218866, #189305, #257003, .T. ) ;
#150429 = ADVANCED_FACE ( 'NONE', ( #183613 ), #196127, .T. ) ;
#150430 = FACE_OUTER_BOUND ( 'NONE', #128562, .T. ) ;
#150431 = DIRECTION ( 'NONE',  ( 1.000000000000000000, 0.000000000000000000, 0.000000000000000000 ) ) ;
#150432 = CARTESIAN_POINT ( 'NONE',  ( 18.49999999999999645, 1.162701749949165642, -175.5999999999999659 ) ) ;
#150433 = DIRECTION ( 'NONE',  ( 0.000000000000000000, 0.000000000000000000, -1.000000000000000000 ) ) ;
#150434 = LINE ( 'NONE', #212957, #227811 ) ;
#150435 = ORIENTED_EDGE ( 'NONE', *, *, #211034, .F. ) ;
#150436 = CARTESIAN_POINT ( 'NONE',  ( -20.64999999999999858, 29.14863708059993286, -237.4168895852561434 ) ) ;
#150437 = EDGE_LOOP ( 'NONE', ( #149656, #203816, #119443 ) ) ;
#150439 = ORIENTED_EDGE ( 'NONE', *, *, #130609, .T. ) ;
#150438 = CARTESIAN_POINT ( 'NONE',  ( -23.25000000000000000, -11.64999999998884483, -63.89999999999999858 ) ) ;
#150440 = EDGE_LOOP ( 'NONE', ( #48269, #84033, #141259, #141400, #42273 ) ) ;
#150441 = DIRECTION ( 'NONE',  ( 0.000000000000000000, 6.982962677686266711E-15, -1.000000000000000000 ) ) ;
#150442 = ORIENTED_EDGE ( 'NONE', *, *, #881, .T. ) ;
#150443 = CARTESIAN_POINT ( 'NONE',  ( 18.59999999999999076, 7.128833340094563376, -233.7327013124401276 ) ) ;
#150444 = DIRECTION ( 'NONE',  ( -0.000000000000000000, 0.7397360091702694929, 0.6728971962616898672 ) ) ;
#150445 = DIRECTION ( 'NONE',  ( 1.000000000000000000, 2.986185139342066440E-16, -6.665775143889694746E-16 ) ) ;
#150446 = ORIENTED_EDGE ( 'NONE', *, *, #25477, .F. ) ;
#150447 = CYLINDRICAL_SURFACE ( 'NONE', #153137, 0.09999999999998657185 ) ;
#150448 = DIRECTION ( 'NONE',  ( -1.000000000000000000, 0.000000000000000000, -0.000000000000000000 ) ) ;
#150449 = DIRECTION ( 'NONE',  ( -1.000000000000000000, 0.000000000000000000, 0.000000000000000000 ) ) ;
#150451 = ORIENTED_EDGE ( 'NONE', *, *, #252526, .T. ) ;
#150450 = VECTOR ( 'NONE', #220119, 1000.000000000000000 ) ;
#150453 = ORIENTED_EDGE ( 'NONE', *, *, #101079, .F. ) ;
#150452 = CARTESIAN_POINT ( 'NONE',  ( 18.52928932188133970, 65.72071067813085676, -145.3731074845244109 ) ) ;
#150454 = PLANE ( 'NONE',  #119289 ) ;
#150455 = FACE_OUTER_BOUND ( 'NONE', #51126, .T. ) ;
#150456 = EDGE_CURVE ( 'NONE', #228447, #213386, #198782, .T. ) ;
#150457 = ADVANCED_FACE ( 'NONE', ( #197396 ), #194542, .T. ) ;
#150458 = EDGE_LOOP ( 'NONE', ( #177122, #254627, #184518, #170395 ) ) ;
#150459 = DIRECTION ( 'NONE',  ( 0.000000000000000000, -0.9915357197604792727, 0.1298341882520475943 ) ) ;
#150460 = PLANE ( 'NONE',  #13028 ) ;
#150461 = AXIS2_PLACEMENT_3D ( 'NONE', #4683, #820, #19132 ) ;
#150462 = DIRECTION ( 'NONE',  ( -0.000000000000000000, -1.000000000000000000, -6.982962677686266711E-15 ) ) ;
#150463 = VERTEX_POINT ( 'NONE', #175308 ) ;
#150464 = DIRECTION ( 'NONE',  ( 0.000000000000000000, 0.000000000000000000, -1.000000000000000000 ) ) ;
#150465 = DIRECTION ( 'NONE',  ( 0.000000000000000000, 0.000000000000000000, -1.000000000000000000 ) ) ;
#150466 = LINE ( 'NONE', #155623, #130198 ) ;
#150467 = ADVANCED_FACE ( 'NONE', ( #76162 ), #69819, .T. ) ;
#150468 = VECTOR ( 'NONE', #15324, 1000.000000000000000 ) ;
#150469 = VECTOR ( 'NONE', #158628, 1000.000000000000000 ) ;
#150471 = ORIENTED_EDGE ( 'NONE', *, *, #38836, .F. ) ;
#150470 = AXIS2_PLACEMENT_3D ( 'NONE', #254457, #36766, #255728 ) ;
#150472 = CARTESIAN_POINT ( 'NONE',  ( -18.40000000000000213, 8.822561741677553471, -158.2500000000000284 ) ) ;
#150473 = ORIENTED_EDGE ( 'NONE', *, *, #85633, .F. ) ;
#150474 = CARTESIAN_POINT ( 'NONE',  ( -18.60000000000001208, -9.364240527579751117, -174.6802485818407433 ) ) ;
#150475 = CARTESIAN_POINT ( 'NONE',  ( 22.39999999999999503, 31.85509083104287598, -238.8280249686205536 ) ) ;
#150477 = ORIENTED_EDGE ( 'NONE', *, *, #154682, .T. ) ;
#150476 = CARTESIAN_POINT ( 'NONE',  ( 14.45204356427542258, 24.86276468521554150, -232.5111033352153527 ) ) ;
#150478 = DIRECTION ( 'NONE',  ( 1.000000000000000000, 0.000000000000000000, 0.000000000000000000 ) ) ;
#150479 = DIRECTION ( 'NONE',  ( 0.000000000000000000, -0.4721928772777346239, -0.8814952561688430555 ) ) ;
#150480 = CYLINDRICAL_SURFACE ( 'NONE', #85203, 0.4999999999999944489 ) ;
#150481 = FACE_OUTER_BOUND ( 'NONE', #128053, .T. ) ;
#150482 = CARTESIAN_POINT ( 'NONE',  ( 21.05000000000000071, 6.540656951712401579, -33.60000000000000142 ) ) ;
#150483 = DIRECTION ( 'NONE',  ( 0.000000000000000000, 6.769652589177772835E-15, -1.000000000000000000 ) ) ;
#150484 = CARTESIAN_POINT ( 'NONE',  ( -23.15000000000000213, 18.38993523765006444, -239.7649653196623376 ) ) ;
#150485 = B_SPLINE_CURVE_WITH_KNOTS ( 'NONE', 3,
 ( #128337, #146574, #170069, #246977, #29272, #185734, #52628, #69651, #108758, #188287 ),
 .UNSPECIFIED., .F., .F.,
 ( 4, 3, 3, 4 ),
 ( 0.000000000000000000, 0.0002000000000002908468, 0.001000000000045115191, 0.001967863649472108723 ),
 .UNSPECIFIED. ) ;
#150487 = VERTEX_POINT ( 'NONE', #17480 ) ;
#150486 = CARTESIAN_POINT ( 'NONE',  ( 23.14999999999998437, 11.75000000001115552, -134.0000000000000000 ) ) ;
#150488 = TOROIDAL_SURFACE ( 'NONE', #200366, 2.100000000000002309, 0.1000000000000000056 ) ;
#150489 = DIRECTION ( 'NONE',  ( 0.000000000000000000, 0.2128009952263604232, -0.9770955615653316162 ) ) ;
#150490 = DIRECTION ( 'NONE',  ( 0.000000000000000000, -0.2617529984165152257, -0.9651348961777124202 ) ) ;
#150491 = CARTESIAN_POINT ( 'NONE',  ( -18.59999999999999787, 77.16270174994990327, -94.92310748452430857 ) ) ;
#150492 = CARTESIAN_POINT ( 'NONE',  ( -20.54999999999999716, 73.50000000001151079, -49.24772940728643533 ) ) ;
#150493 = ORIENTED_EDGE ( 'NONE', *, *, #133590, .T. ) ;
#150494 = EDGE_CURVE ( 'NONE', #251339, #79018, #11561, .T. ) ;
#150495 = AXIS2_PLACEMENT_3D ( 'NONE', #244474, #65838, #28035 ) ;
#150496 = AXIS2_PLACEMENT_3D ( 'NONE', #189876, #191185, #152056 ) ;
#150497 = DIRECTION ( 'NONE',  ( 0.000000000000000000, 1.000000000000000000, 6.982962677686266711E-15 ) ) ;
#150498 = EDGE_CURVE ( 'NONE', #203266, #180463, #218225, .T. ) ;
#150499 = CARTESIAN_POINT ( 'NONE',  ( -18.59999999999999787, 11.74265569217025629, -210.9797313238103698 ) ) ;
#150500 = AXIS2_PLACEMENT_3D ( 'NONE', #244639, #81683, #243359 ) ;
#150501 = ORIENTED_EDGE ( 'NONE', *, *, #240682, .T. ) ;
#150502 = CARTESIAN_POINT ( 'NONE',  ( -16.94180778212362881, 9.992443055743304825, -79.60418357053329430 ) ) ;
#150503 = EDGE_CURVE ( 'NONE', #72909, #242360, #165684, .T. ) ;
#150504 = ORIENTED_EDGE ( 'NONE', *, *, #208124, .F. ) ;
#150505 = CARTESIAN_POINT ( 'NONE',  ( -21.14999999999999858, 6.540656951712397138, -134.1000000000000227 ) ) ;
#150506 = ORIENTED_EDGE ( 'NONE', *, *, #254006, .T. ) ;
#150507 = DIRECTION ( 'NONE',  ( -1.000000000000000000, -1.394253735153569469E-16, -2.602809386958778209E-16 ) ) ;
#150509 = ORIENTED_EDGE ( 'NONE', *, *, #69696, .F. ) ;
#150508 = CARTESIAN_POINT ( 'NONE',  ( 20.85000000000000142, -1.749999999988843813, -179.1189500386222733 ) ) ;
#150510 = ADVANCED_FACE ( 'NONE', ( #18762 ), #95721, .T. ) ;
#150511 = AXIS2_PLACEMENT_3D ( 'NONE', #6369, #85882, #89752 ) ;
#150512 = CARTESIAN_POINT ( 'NONE',  ( -21.05000000000000071, 1.115600667400684642E-11, -67.00000000000004263 ) ) ;
#150513 = ORIENTED_EDGE ( 'NONE', *, *, #81671, .T. ) ;
#150514 = LINE ( 'NONE', #171394, #155615 ) ;
#150515 = ORIENTED_EDGE ( 'NONE', *, *, #201408, .F. ) ;
#150516 = EDGE_LOOP ( 'NONE', ( #119856, #140212, #30717, #86470 ) ) ;
#150517 = DIRECTION ( 'NONE',  ( 0.000000000000000000, 0.01562500000001262185, 0.9998779222360095753 ) ) ;
#150518 = EDGE_CURVE ( 'NONE', #64899, #156656, #178152, .T. ) ;
#150520 = ORIENTED_EDGE ( 'NONE', *, *, #218124, .T. ) ;
#150519 = CARTESIAN_POINT ( 'NONE',  ( 13.54556439290363912, 9.450592112144857282, -48.55618831880837405 ) ) ;
#150521 = LINE ( 'NONE', #34450, #173047 ) ;
#150522 = ORIENTED_EDGE ( 'NONE', *, *, #101087, .F. ) ;
#150523 = ORIENTED_EDGE ( 'NONE', *, *, #252795, .T. ) ;
#150524 = CARTESIAN_POINT ( 'NONE',  ( 20.94999999999999574, 10.42338541491290727, -7.492051923870097774 ) ) ;
#150525 = ADVANCED_FACE ( 'NONE', ( #114004 ), #119160, .T. ) ;
#150527 = CARTESIAN_POINT ( 'NONE',  ( -20.85000000000000142, 77.14957036958777792, -128.7071950000224092 ) ) ;
#150526 = TOROIDAL_SURFACE ( 'NONE', #208795, 0.2000000000000000111, 0.1000000000000000056 ) ;
#150528 = CARTESIAN_POINT ( 'NONE',  ( -18.59999999999999787, -1.162701749938009677, -8.000000000000000000 ) ) ;
#150529 = VERTEX_POINT ( 'NONE', #55291 ) ;
#150530 = CARTESIAN_POINT ( 'NONE',  ( -23.15000000000000213, 14.06640494040441602, -210.3712993791105532 ) ) ;
#150531 = CARTESIAN_POINT ( 'NONE',  ( -23.25000000000000000, 76.00000000001239187, -162.1231074845243825 ) ) ;
#150532 = DIRECTION ( 'NONE',  ( 0.000000000000000000, -0.9651348961777028723, 0.2617529984165503087 ) ) ;
#150533 = AXIS2_PLACEMENT_3D ( 'NONE', #22373, #40675, #139710 ) ;
#150534 = ORIENTED_EDGE ( 'NONE', *, *, #30027, .F. ) ;
#150535 = CARTESIAN_POINT ( 'NONE',  ( 20.95000000000005258, 87.75000000001119815, -5.923107484524795296 ) ) ;
#150536 = FACE_OUTER_BOUND ( 'NONE', #229275, .T. ) ;
#150537 = B_SPLINE_CURVE_WITH_KNOTS ( 'NONE', 3,
 ( #175576, #15218, #30950, #12658, #192562, #96003, #170480, #249963, #32222, #111737 ),
 .UNSPECIFIED., .F., .F.,
 ( 4, 2, 2, 2, 4 ),
 ( 0.000000000000000000, 4.221631689687179134E-05, 8.443263379374358268E-05, 0.0001688652675874855933, 0.0003377305351749678797 ),
 .UNSPECIFIED. ) ;
#150538 = DIRECTION ( 'NONE',  ( 0.000000000000000000, 0.4930308989874980785, 0.8700118002898462599 ) ) ;
#150539 = AXIS2_PLACEMENT_3D ( 'NONE', #229069, #50392, #152114 ) ;
#150540 = ORIENTED_EDGE ( 'NONE', *, *, #166940, .F. ) ;
#150541 = CARTESIAN_POINT ( 'NONE',  ( 20.94999999999999929, 1.115600667400684642E-11, -79.97500000000005116 ) ) ;
#150542 = EDGE_LOOP ( 'NONE', ( #156730, #168842, #73284, #211472 ) ) ;
#150543 = CARTESIAN_POINT ( 'NONE',  ( -18.43473496883412466, -7.778107375242646171, -209.9050251632729100 ) ) ;
#150544 = VERTEX_POINT ( 'NONE', #176579 ) ;
#150545 = CARTESIAN_POINT ( 'NONE',  ( -12.60206096961791999, 25.37811339336344929, -232.8563427119264304 ) ) ;
#150546 = DIRECTION ( 'NONE',  ( 0.000000000000000000, 0.9209589331071864615, -0.3896596508878908960 ) ) ;
#150547 = ORIENTED_EDGE ( 'NONE', *, *, #135527, .T. ) ;
#150548 = AXIS2_PLACEMENT_3D ( 'NONE', #129185, #172209, #167052 ) ;
#150549 = ORIENTED_EDGE ( 'NONE', *, *, #52352, .T. ) ;
#150550 = DIRECTION ( 'NONE',  ( 0.000000000000000000, -7.124650136758292359E-15, 1.000000000000000000 ) ) ;
#150551 = CARTESIAN_POINT ( 'NONE',  ( -23.25000000000000000, -1.835859311432481045, -179.1044391687985353 ) ) ;
#150552 = ORIENTED_EDGE ( 'NONE', *, *, #207683, .T. ) ;
#150553 = CARTESIAN_POINT ( 'NONE',  ( 20.84999999999998721, 10.33248238083634440, -72.59484654391314962 ) ) ;
#150554 = AXIS2_PLACEMENT_3D ( 'NONE', #142566, #64336, #143853 ) ;
#150555 = CARTESIAN_POINT ( 'NONE',  ( -18.50000000000000000, 65.70711192142347556, -64.06510546851220056 ) ) ;
#150556 = ORIENTED_EDGE ( 'NONE', *, *, #220263, .F. ) ;
#150557 = VECTOR ( 'NONE', #54553, 1000.000000000000000 ) ;
#150558 = AXIS2_PLACEMENT_3D ( 'NONE', #149857, #71606, #152436 ) ;
#150559 = ORIENTED_EDGE ( 'NONE', *, *, #246110, .T. ) ;
#150560 = ADVANCED_FACE ( 'NONE', ( #233961 ), #232701, .T. ) ;
#150561 = CARTESIAN_POINT ( 'NONE',  ( -21.05000000000000071, 74.25000000001156764, -57.85359592662268824 ) ) ;
#150562 = AXIS2_PLACEMENT_3D ( 'NONE', #52410, #90250, #172423 ) ;
#150563 = CARTESIAN_POINT ( 'NONE',  ( -16.77683809663752257, 22.98839712131283974, -230.9453208111996503 ) ) ;
#150565 = EDGE_CURVE ( 'NONE', #183861, #115598, #153186, .T. ) ;
#150564 = CIRCLE ( 'NONE', #9102, 0.1000000000000028644 ) ;
#150566 = DIRECTION ( 'NONE',  ( 0.000000000000000000, 0.000000000000000000, -1.000000000000000000 ) ) ;
#150568 = ORIENTED_EDGE ( 'NONE', *, *, #145629, .T. ) ;
#150567 = DIRECTION ( 'NONE',  ( 0.000000000000000000, -7.487053152578128658E-15, 1.000000000000000000 ) ) ;
#150569 = DIRECTION ( 'NONE',  ( 0.000000000000000000, 0.000000000000000000, 1.000000000000000000 ) ) ;
#150570 = DIRECTION ( 'NONE',  ( -1.000000000000000000, 1.207181226542539700E-16, -2.694675058168174199E-16 ) ) ;
#150571 = DIRECTION ( 'NONE',  ( -1.000000000000000000, 1.652117596168391700E-15, 0.000000000000000000 ) ) ;
#150572 = ADVANCED_FACE ( 'NONE', ( #89624 ), #98262, .F. ) ;
#150574 = DIRECTION ( 'NONE',  ( 0.000000000000000000, -0.8660254037844420383, 0.4999999999999942824 ) ) ;
#150573 = DIRECTION ( 'NONE',  ( -1.000000000000000000, -0.000000000000000000, -0.000000000000000000 ) ) ;
#150576 = EDGE_CURVE ( 'NONE', #61948, #188649, #148921, .T. ) ;
#150575 = CARTESIAN_POINT ( 'NONE',  ( 23.14999999999999503, 10.80300742114540391, -220.2930047078982625 ) ) ;
#150577 = CARTESIAN_POINT ( 'NONE',  ( -21.05000000000000071, 1.115600667400684642E-11, -67.00000000000004263 ) ) ;
#150578 = CARTESIAN_POINT ( 'NONE',  ( -22.50000000000000000, 76.00000000001217870, -142.7731074845243029 ) ) ;
#150579 = AXIS2_PLACEMENT_3D ( 'NONE', #202642, #25320, #160970 ) ;
#150580 = DIRECTION ( 'NONE',  ( -2.952720810173288619E-16, 0.4721928772777346239, 0.8814952561688430555 ) ) ;
#150581 = AXIS2_PLACEMENT_3D ( 'NONE', #65062, #140749, #121230 ) ;
#150583 = ORIENTED_EDGE ( 'NONE', *, *, #116428, .T. ) ;
#150582 = AXIS2_PLACEMENT_3D ( 'NONE', #170344, #111608, #86876 ) ;
#150584 = CIRCLE ( 'NONE', #171464, 14.30833333333333890 ) ;
#150585 = VERTEX_POINT ( 'NONE', #257319 ) ;
#150586 = VERTEX_POINT ( 'NONE', #34508 ) ;
#150587 = ADVANCED_FACE ( 'NONE', ( #94446 ), #21361, .T. ) ;
#150588 = FACE_OUTER_BOUND ( 'NONE', #78105, .T. ) ;
#150589 = ADVANCED_FACE ( 'NONE', ( #40934 ), #85122, .T. ) ;
#150590 = PLANE ( 'NONE',  #144385 ) ;
#150591 = VERTEX_POINT ( 'NONE', #179159 ) ;
#150592 = CARTESIAN_POINT ( 'NONE',  ( -22.39999999999999858, 11.75000000001115552, -134.1000000000000227 ) ) ;
#150593 = CARTESIAN_POINT ( 'NONE',  ( 20.92356734117541706, 10.31973158071402175, -206.5505334713353989 ) ) ;
#150594 = CARTESIAN_POINT ( 'NONE',  ( 21.05000000000000071, -1.835341550224413698, -11.55515129256298046 ) ) ;
#150596 = ORIENTED_EDGE ( 'NONE', *, *, #97412, .F. ) ;
#150595 = AXIS2_PLACEMENT_3D ( 'NONE', #204801, #129140, #245242 ) ;
#150597 = VERTEX_POINT ( 'NONE', #163425 ) ;
#150598 = DIRECTION ( 'NONE',  ( 0.000000000000000000, -0.9915357197604892647, 0.1298341882519715440 ) ) ;
#150599 = DIRECTION ( 'NONE',  ( 0.000000000000000000, 0.8689845192018014197, -0.4948392722769828778 ) ) ;
#150600 = ORIENTED_EDGE ( 'NONE', *, *, #105877, .T. ) ;
#150601 = ADVANCED_FACE ( 'NONE', ( #4324, #162154, #164705 ), #120473, .T. ) ;
#150602 = ADVANCED_FACE ( 'NONE', ( #81279 ), #100826, .T. ) ;
#150603 = CARTESIAN_POINT ( 'NONE',  ( -20.94999999999999929, 74.16465844978745281, -91.46795619196133487 ) ) ;
#150605 = EDGE_LOOP ( 'NONE', ( #120810, #79452, #137967, #57576 ) ) ;
#150604 = DIRECTION ( 'NONE',  ( 0.000000000000000000, 0.8814952561688050858, -0.4721928772778054006 ) ) ;
#150606 = LINE ( 'NONE', #187179, #149598 ) ;
#150607 = EDGE_CURVE ( 'NONE', #111912, #128539, #65596, .T. ) ;
#150608 = DIRECTION ( 'NONE',  ( -1.000000000000000000, -2.952720810173289112E-16, 0.000000000000000000 ) ) ;
#150610 = EDGE_LOOP ( 'NONE', ( #56451, #101154, #113012, #215126 ) ) ;
#150609 = LINE ( 'NONE', #128470, #93766 ) ;
#150611 =( NAMED_UNIT ( * ) SI_UNIT ( $, .STERADIAN. ) SOLID_ANGLE_UNIT ( ) );
#150612 = DIRECTION ( 'NONE',  ( -1.000000000000000000, -0.000000000000000000, -0.000000000000000000 ) ) ;
#150613 = CYLINDRICAL_SURFACE ( 'NONE', #152580, 0.1000000000000002554 ) ;
#150615 = CARTESIAN_POINT ( 'NONE',  ( 21.09787244211752011, 8.775370707348422172, -179.7392533843176068 ) ) ;
#150614 = CARTESIAN_POINT ( 'NONE',  ( 18.52928932188133970, 10.27928932188134858, -24.75000000000000000 ) ) ;
#150616 = CARTESIAN_POINT ( 'NONE',  ( -21.29999999999995808, 76.00000000001213607, -136.5231074845242745 ) ) ;
#150617 = CARTESIAN_POINT ( 'NONE',  ( 23.24999999999999289, 6.550000000000000711, -21.35000000000000142 ) ) ;
#150618 = DIRECTION ( 'NONE',  ( 0.000000000000000000, 1.000000000000000000, 0.000000000000000000 ) ) ;
#150619 = FACE_OUTER_BOUND ( 'NONE', #23784, .T. ) ;
#150620 = ORIENTED_EDGE ( 'NONE', *, *, #45508, .F. ) ;
#150622 = VECTOR ( 'NONE', #77484, 1000.000000000000000 ) ;
#150621 = CARTESIAN_POINT ( 'NONE',  ( 21.72449340488910252, 12.01681723992382622, -207.8496978137663689 ) ) ;
#150623 = ORIENTED_EDGE ( 'NONE', *, *, #151462, .F. ) ;
#150624 = CARTESIAN_POINT ( 'NONE',  ( -23.15000000000000213, 76.00000000001237765, -170.0231074845243597 ) ) ;
#150625 = ORIENTED_EDGE ( 'NONE', *, *, #159691, .T. ) ;
#150626 = CARTESIAN_POINT ( 'NONE',  ( -18.59999999999999787, -7.567701079425722455, -210.0537230116848662 ) ) ;
#150627 = FACE_OUTER_BOUND ( 'NONE', #161462, .T. ) ;
#150629 = EDGE_CURVE ( 'NONE', #111004, #153822, #143836, .T. ) ;
#150628 = ORIENTED_EDGE ( 'NONE', *, *, #39161, .F. ) ;
#150630 = DIRECTION ( 'NONE',  ( -0.000000000000000000, -6.982962677686266711E-15, 1.000000000000000000 ) ) ;
#150631 = B_SPLINE_CURVE_WITH_KNOTS ( 'NONE', 3,
 ( #179570, #118302, #19192, #120891, #183409, #140407, #58295, #23069, #99977, #201673, #142959, #202955, #79144 ),
 .UNSPECIFIED., .F., .F.,
 ( 4, 3, 3, 3, 4 ),
 ( 1.110764993427085326E-16, 1.946463881814652902E-05, 3.922356109943681788E-05, 4.215060953237600338E-05, 4.415117091092905685E-05 ),
 .UNSPECIFIED. ) ;
#150632 = TOROIDAL_SURFACE ( 'NONE', #250402, 0.2000000000000000111, 0.1000000000000000056 ) ;
#150634 = ORIENTED_EDGE ( 'NONE', *, *, #73056, .T. ) ;
#150633 = AXIS2_PLACEMENT_3D ( 'NONE', #37093, #3051, #180430 ) ;
#150635 = ORIENTED_EDGE ( 'NONE', *, *, #164127, .F. ) ;
#150636 = AXIS2_PLACEMENT_3D ( 'NONE', #22138, #162934, #179925 ) ;
#150637 = DIRECTION ( 'NONE',  ( 1.000000000000000000, 0.000000000000000000, 0.000000000000000000 ) ) ;
#150638 = CARTESIAN_POINT ( 'NONE',  ( 20.95429693346636313, 10.54330487990693221, -41.06088253831304513 ) ) ;
#150639 = CYLINDRICAL_SURFACE ( 'NONE', #226079, 0.1000000000000028644 ) ;
#150640 = CARTESIAN_POINT ( 'NONE',  ( 12.48201962039796342, 27.09559348180859217, -233.7911270184620491 ) ) ;
#150641 = CARTESIAN_POINT ( 'NONE',  ( -21.05000000000000071, 1.116121084443477685E-11, -36.39999999999999147 ) ) ;
#150642 = EDGE_CURVE ( 'NONE', #241360, #152046, #1757, .T. ) ;
#150643 =( BOUNDED_SURFACE ( )  B_SPLINE_SURFACE ( 3, 2, ( 
 ( #6337, #8924, #184991 ),
 ( #85853, #27235, #46748 ),
 ( #166747, #126288, #183717 ),
 ( #145848, #88423, #243679 ),
 ( #225379, #65036, #84552 ),
 ( #222816, #203265, #142001 ) ),
 .UNSPECIFIED., .F., .F., .F. ) 
 B_SPLINE_SURFACE_WITH_KNOTS ( ( 4, 2, 4 ),
 ( 3, 3 ),
 ( 0.0001381104793128067206, 0.0002947094729387610568, 0.0004513084665647153931 ),
 ( 0.000000000000000000, 1.000000000000000000 ),
 .UNSPECIFIED. ) 
 GEOMETRIC_REPRESENTATION_ITEM ( )  RATIONAL_B_SPLINE_SURFACE ( (
 ( 1.000000000000000000, 0.7071067811865505703, 1.000000000000000000),
 ( 1.000000000000000000, 0.6919563088103167781, 1.000000000000000000),
 ( 1.000000000000000000, 0.6959445945713532700, 1.000000000000000000),
 ( 1.000000000000000000, 0.7137882985316233997, 1.000000000000000000),
 ( 1.000000000000000000, 0.7257496306093990102, 1.000000000000000000),
 ( 1.000000000000000000, 0.7250110520820101101, 1.000000000000000000) ) ) 
 REPRESENTATION_ITEM ( '' )  SURFACE ( )  );
#150645 = DIRECTION ( 'NONE',  ( 0.000000000000000000, 1.000000000000000000, 0.000000000000000000 ) ) ;
#150644 = LINE ( 'NONE', #119229, #33177 ) ;
#150646 = DIRECTION ( 'NONE',  ( 0.000000000000000000, -0.5000000000000016653, 0.8660254037844377084 ) ) ;
#150648 = VERTEX_POINT ( 'NONE', #103414 ) ;
#150647 = CARTESIAN_POINT ( 'NONE',  ( -21.05000000000000071, -1.162701749926853712, -175.3999999999999773 ) ) ;
#150650 = DIRECTION ( 'NONE',  ( 1.000000000000000000, -0.000000000000000000, -0.000000000000000000 ) ) ;
#150649 = CARTESIAN_POINT ( 'NONE',  ( 20.75572585718219898, 8.882316728409760387, -75.49725839870761490 ) ) ;
#150651 = CARTESIAN_POINT ( 'NONE',  ( 20.94999999999999929, 67.70174932746996888, -211.7710791003628401 ) ) ;
#150652 = ORIENTED_EDGE ( 'NONE', *, *, #163781, .F. ) ;
#150653 = CARTESIAN_POINT ( 'NONE',  ( 18.54999999999999716, 9.950000000011153034, -54.35000000000005826 ) ) ;
#150654 = CARTESIAN_POINT ( 'NONE',  ( 23.24999999999999645, 5.599999999999996980, -21.09473398108690390 ) ) ;
#150656 = ADVANCED_FACE ( 'NONE', ( #25211 ), #102123, .F. ) ;
#150655 = CARTESIAN_POINT ( 'NONE',  ( 23.24999999999999645, 76.00000000001267608, -203.5231074845243597 ) ) ;
#150657 = ORIENTED_EDGE ( 'NONE', *, *, #221247, .F. ) ;
#150658 = VECTOR ( 'NONE', #97440, 1000.000000000000000 ) ;
#150659 = DIRECTION ( 'NONE',  ( -1.000000000000000000, 0.000000000000000000, -0.000000000000000000 ) ) ;
#150660 = EDGE_CURVE ( 'NONE', #145138, #118915, #20069, .T. ) ;
#150661 = DIRECTION ( 'NONE',  ( 6.938893903907224433E-15, -1.000000000000000000, -2.891205793294679805E-16 ) ) ;
#150662 = CARTESIAN_POINT ( 'NONE',  ( -23.15000000000000213, 87.75000000001237765, -170.0231074845242745 ) ) ;
#150663 = ORIENTED_EDGE ( 'NONE', *, *, #144499, .T. ) ;
#150664 = ORIENTED_EDGE ( 'NONE', *, *, #189918, .T. ) ;
#150665 = EDGE_CURVE ( 'NONE', #70455, #97941, #256035, .T. ) ;
#150667 = EDGE_CURVE ( 'NONE', #223188, #153027, #236395, .T. ) ;
#150666 = DIRECTION ( 'NONE',  ( 0.000000000000000000, 0.000000000000000000, -1.000000000000000000 ) ) ;
#150668 = LINE ( 'NONE', #50260, #107324 ) ;
#150669 = DIRECTION ( 'NONE',  ( 0.000000000000000000, -0.8368562265788574983, -0.5474227397872651890 ) ) ;
#150670 = DIRECTION ( 'NONE',  ( 0.000000000000000000, -1.000000000000000000, 0.000000000000000000 ) ) ;
#150671 = ORIENTED_EDGE ( 'NONE', *, *, #48043, .T. ) ;
#150672 = CARTESIAN_POINT ( 'NONE',  ( 13.88302573338719625, 46.48157447062519765, -234.7876710066568648 ) ) ;
#150673 = AXIS2_PLACEMENT_3D ( 'NONE', #87573, #167166, #221937 ) ;
#150675 = CYLINDRICAL_SURFACE ( 'NONE', #62666, 0.09999999999999771572 ) ;
#150674 = VECTOR ( 'NONE', #26928, 999.9999999999998863 ) ;
#150676 = CIRCLE ( 'NONE', #34185, 0.09999999999999996392 ) ;
#150677 = CARTESIAN_POINT ( 'NONE',  ( -18.40000000000000213, 15.66855642289968031, -219.0286517433665381 ) ) ;
#150678 = CARTESIAN_POINT ( 'NONE',  ( -23.25000000000000000, 77.73670573947995877, -158.5056848969006182 ) ) ;
#150679 = EDGE_CURVE ( 'NONE', #48720, #72307, #232321, .T. ) ;
#150680 = ORIENTED_EDGE ( 'NONE', *, *, #189408, .F. ) ;
#150682 = EDGE_CURVE ( 'NONE', #230513, #148058, #199987, .T. ) ;
#150681 = DIRECTION ( 'NONE',  ( 0.000000000000000000, 0.1495327102803792052, -0.9887567792719320625 ) ) ;
#150684 = ORIENTED_EDGE ( 'NONE', *, *, #243558, .F. ) ;
#150683 = CARTESIAN_POINT ( 'NONE',  ( 20.94999999999999574, 77.83534155023627932, -91.36795619196132634 ) ) ;
#150685 = CARTESIAN_POINT ( 'NONE',  ( -18.39999999999999858, 11.47867410001043531, -76.27469321634069388 ) ) ;
#150686 = EDGE_CURVE ( 'NONE', #184931, #109469, #107388, .T. ) ;
#150687 = FACE_OUTER_BOUND ( 'NONE', #9186, .T. ) ;
#150688 = ORIENTED_EDGE ( 'NONE', *, *, #242167, .T. ) ;
#150689 = DIRECTION ( 'NONE',  ( 1.000000000000000000, -0.000000000000000000, -0.000000000000000000 ) ) ;
#150690 = CARTESIAN_POINT ( 'NONE',  ( 23.14999999999999858, 70.50000000001151079, -48.42837350343745584 ) ) ;
#150691 = DIRECTION ( 'NONE',  ( 1.000000000000000000, 0.000000000000000000, 0.000000000000000000 ) ) ;
#150692 = CIRCLE ( 'NONE', #121670, 0.1000000000000028644 ) ;
#150693 = ORIENTED_EDGE ( 'NONE', *, *, #223346, .F. ) ;
#150694 = CARTESIAN_POINT ( 'NONE',  ( -18.59999999999999787, -1.162701749926853712, -108.6000000000000227 ) ) ;
#150695 = CYLINDRICAL_SURFACE ( 'NONE', #235826, 0.09999999999998898659 ) ;
#150696 = FACE_OUTER_BOUND ( 'NONE', #65795, .T. ) ;
#150697 = EDGE_CURVE ( 'NONE', #122837, #207244, #139971, .T. ) ;
#150698 = CARTESIAN_POINT ( 'NONE',  ( -16.86337532320261090, 51.69689044229821917, -231.8786767479558080 ) ) ;
#150699 = EDGE_CURVE ( 'NONE', #218820, #93357, #153222, .T. ) ;
#150700 = LINE ( 'NONE', #49025, #233874 ) ;
#150701 = FACE_OUTER_BOUND ( 'NONE', #222776, .T. ) ;
#150702 = ORIENTED_EDGE ( 'NONE', *, *, #74996, .T. ) ;
#150703 = ORIENTED_EDGE ( 'NONE', *, *, #85910, .T. ) ;
#150704 = CARTESIAN_POINT ( 'NONE',  ( -23.15000000000000213, -11.41227409414968541, -30.50000000000000000 ) ) ;
#150705 = EDGE_CURVE ( 'NONE', #135773, #111692, #103093, .T. ) ;
#150706 = DIRECTION ( 'NONE',  ( 0.000000000000000000, 0.000000000000000000, -1.000000000000000000 ) ) ;
#150707 = FACE_OUTER_BOUND ( 'NONE', #5818, .T. ) ;
#150708 = VECTOR ( 'NONE', #167605, 1000.000000000000000 ) ;
#150709 = CARTESIAN_POINT ( 'NONE',  ( 18.46905048506371116, -0.7072635980893239305, -242.2718000941648882 ) ) ;
#150710 = CARTESIAN_POINT ( 'NONE',  ( -23.15000000000000213, 11.75000000001115552, -155.7499999999999716 ) ) ;
#150711 = EDGE_CURVE ( 'NONE', #129010, #110550, #98992, .T. ) ;
#150712 = CARTESIAN_POINT ( 'NONE',  ( 21.07928932188134397, 6.328516656393303741, 0.09889514565439641580 ) ) ;
#150713 = AXIS2_PLACEMENT_3D ( 'NONE', #130433, #169616, #127879 ) ;
#150714 = DIRECTION ( 'NONE',  ( 0.000000000000000000, -1.000000000000000000, 0.000000000000000000 ) ) ;
#150715 = AXIS2_PLACEMENT_3D ( 'NONE', #67395, #50372, #247304 ) ;
#150716 = FACE_OUTER_BOUND ( 'NONE', #27530, .T. ) ;
#150717 = VECTOR ( 'NONE', #29306, 1000.000000000000000 ) ;
#150718 = B_SPLINE_CURVE_WITH_KNOTS ( 'NONE', 3,
 ( #245253, #10494, #186570, #48321, #26210, #230840, #168323, #127871, #66611, #170898 ),
 .UNSPECIFIED., .F., .F.,
 ( 4, 3, 3, 4 ),
 ( 0.000000000000000000, 1.004626015991478527E-05, 1.831183478183247374E-05, 2.062343583996109511E-05 ),
 .UNSPECIFIED. ) ;
#150719 = CARTESIAN_POINT ( 'NONE',  ( -20.90000000000000213, -1.885425182446133885, -11.49641995933507843 ) ) ;
#150720 = AXIS2_PLACEMENT_3D ( 'NONE', #248841, #152325, #70224 ) ;
#150721 = ORIENTED_EDGE ( 'NONE', *, *, #43814, .F. ) ;
#150722 = LINE ( 'NONE', #230247, #27643 ) ;
#150723 = VECTOR ( 'NONE', #85542, 1000.000000000000000 ) ;
#150724 = ORIENTED_EDGE ( 'NONE', *, *, #119331, .T. ) ;
#150725 = CARTESIAN_POINT ( 'NONE',  ( 22.50000000000000000, 7.790779598384538929, -100.4000000000000341 ) ) ;
#150726 = CARTESIAN_POINT ( 'NONE',  ( 21.14999999999999858, 87.75000000001229239, -157.7731074845242745 ) ) ;
#150727 = CARTESIAN_POINT ( 'NONE',  ( 23.14999999999999503, 64.35000000001156195, -57.27310748452440237 ) ) ;
#150728 =( NAMED_UNIT ( * ) PLANE_ANGLE_UNIT ( ) SI_UNIT ( $, .RADIAN. ) );
#150729 = VECTOR ( 'NONE', #46698, 1000.000000000000000 ) ;
#150730 = FACE_OUTER_BOUND ( 'NONE', #34452, .T. ) ;
#150731 = ORIENTED_EDGE ( 'NONE', *, *, #10635, .F. ) ;
#150732 = CARTESIAN_POINT ( 'NONE',  ( 21.14999999999999858, 20.93186404871370598, -233.6960508434578401 ) ) ;
#150733 = DIRECTION ( 'NONE',  ( 0.000000000000000000, 0.000000000000000000, 1.000000000000000000 ) ) ;
#150734 = CARTESIAN_POINT ( 'NONE',  ( -22.10000000000000142, -1.467286812112899463, 28.00000000000000000 ) ) ;
#150735 = CARTESIAN_POINT ( 'NONE',  ( -18.40000000000000213, 11.75000000001113953, -191.7499999999999716 ) ) ;
#150736 = VECTOR ( 'NONE', #240903, 1000.000000000000000 ) ;
#150737 = CIRCLE ( 'NONE', #67346, 0.5000000000000004441 ) ;
#150738 = CARTESIAN_POINT ( 'NONE',  ( -22.49544290803713764, 11.74987023786927764, -167.4346880407416336 ) ) ;
#150739 = VERTEX_POINT ( 'NONE', #27793 ) ;
#150741 =( BOUNDED_SURFACE ( )  B_SPLINE_SURFACE ( 3, 2, ( 
 ( #110003, #192140, #170036 ),
 ( #211702, #91735, #250799 ),
 ( #189563, #228695, #249537 ),
 ( #127007, #171328, #149160 ) ),
 .UNSPECIFIED., .F., .F., .T. ) 
 B_SPLINE_SURFACE_WITH_KNOTS ( ( 4, 4 ),
 ( 3, 3 ),
 ( -3.469446951953614189E-18, 0.001979672783031532438 ),
 ( 0.000000000000000000, 1.000000000000000000 ),
 .UNSPECIFIED. ) 
 GEOMETRIC_REPRESENTATION_ITEM ( )  RATIONAL_B_SPLINE_SURFACE ( (
 ( 1.000000000000000000, 0.7103081912008197829, 1.000000000000000000),
 ( 1.000000000000000000, 0.7104998333558649737, 1.000000000000000000),
 ( 1.000000000000000000, 0.7107238315755179947, 1.000000000000000000),
 ( 1.000000000000000000, 0.7110073749539376209, 1.000000000000000000) ) ) 
 REPRESENTATION_ITEM ( '' )  SURFACE ( )  );
#150740 = CIRCLE ( 'NONE', #9095, 0.09999999999998898659 ) ;
#150742 = LINE ( 'NONE', #231571, #81152 ) ;
#150743 = LINE ( 'NONE', #230266, #96186 ) ;
#150744 = EDGE_CURVE ( 'NONE', #136580, #197749, #246793, .T. ) ;
#150745 = VERTEX_POINT ( 'NONE', #6904 ) ;
#150746 = CIRCLE ( 'NONE', #67540, 0.09999999999999789613 ) ;
#150747 = ORIENTED_EDGE ( 'NONE', *, *, #49493, .F. ) ;
#150748 = DIRECTION ( 'NONE',  ( -1.000000000000000000, -2.952720810173289112E-16, 0.000000000000000000 ) ) ;
#150749 = CARTESIAN_POINT ( 'NONE',  ( 20.84999999999999787, 36.10799525571641766, -235.9264213948819133 ) ) ;
#150750 = ORIENTED_EDGE ( 'NONE', *, *, #192733, .T. ) ;
#150751 = CARTESIAN_POINT ( 'NONE',  ( 18.49362639424878907, -9.442604367877251548, -174.2644409335108264 ) ) ;
#150752 = CARTESIAN_POINT ( 'NONE',  ( 21.04999999999999716, 61.15213033694344347, -234.1846142192326283 ) ) ;
#150753 = EDGE_CURVE ( 'NONE', #242104, #145844, #82423, .T. ) ;
#150754 = ORIENTED_EDGE ( 'NONE', *, *, #28656, .T. ) ;
#150755 = CIRCLE ( 'NONE', #79991, 0.5000000000000004441 ) ;
#150756 = CIRCLE ( 'NONE', #38344, 0.09999999999999939493 ) ;
#150757 = CIRCLE ( 'NONE', #242336, 11.65000000000000036 ) ;
#150758 = CARTESIAN_POINT ( 'NONE',  ( 20.85000000000000142, -11.64999999998883595, -200.9999999999999432 ) ) ;
#150759 = ORIENTED_EDGE ( 'NONE', *, *, #245437, .T. ) ;
#150760 = DIRECTION ( 'NONE',  ( 0.000000000000000000, -1.000000000000000000, 0.000000000000000000 ) ) ;
#150761 = CARTESIAN_POINT ( 'NONE',  ( -23.15000000000000213, 1.115650265596050101E-11, -29.45000000000000284 ) ) ;
#150763 = ORIENTED_EDGE ( 'NONE', *, *, #110961, .F. ) ;
#150762 = CARTESIAN_POINT ( 'NONE',  ( 20.94999999999999929, 76.00000000001126921, -203.5231074845248997 ) ) ;
#150764 = DIRECTION ( 'NONE',  ( -1.000000000000000000, -0.000000000000000000, -0.000000000000000000 ) ) ;
#150765 = CARTESIAN_POINT ( 'NONE',  ( -20.00857864376270001, 9.350000000011156942, -45.75000000000000000 ) ) ;
#150766 = CARTESIAN_POINT ( 'NONE',  ( 23.14999999999999503, 11.75000000000000711, 11.75000000000000000 ) ) ;
#150767 = CARTESIAN_POINT ( 'NONE',  ( -2.995603634470884209E-16, 6.649999999999999467, -21.15000000000000213 ) ) ;
#150768 = CARTESIAN_POINT ( 'NONE',  ( -16.79184697841823848, 66.05123833835421010, -190.8689652139219106 ) ) ;
#150769 = CARTESIAN_POINT ( 'NONE',  ( 23.14999999999999858, 11.65000000001116298, -126.9851942293460922 ) ) ;
#150770 = CARTESIAN_POINT ( 'NONE',  ( -22.57320508075687115, 11.75000000001115552, -33.50000000000000000 ) ) ;
#150772 = ORIENTED_EDGE ( 'NONE', *, *, #169866, .F. ) ;
#150771 = CARTESIAN_POINT ( 'NONE',  ( -23.15000000000000213, -11.74999999998884448, -122.2500000000000284 ) ) ;
#150773 = ORIENTED_EDGE ( 'NONE', *, *, #126837, .F. ) ;
#150775 = CARTESIAN_POINT ( 'NONE',  ( -20.94999999999999929, -11.64999999998884483, -170.4999999999999716 ) ) ;
#150774 = CARTESIAN_POINT ( 'NONE',  ( -23.24999999999999645, 85.60000000001240039, -163.4229180933022576 ) ) ;
#150777 = EDGE_LOOP ( 'NONE', ( #62429, #233327, #127972, #101635, #124425 ) ) ;
#150776 = CARTESIAN_POINT ( 'NONE',  ( 20.95000000000005258, 87.75000000001122658, -30.12310748452481235 ) ) ;
#150778 = ORIENTED_EDGE ( 'NONE', *, *, #145169, .F. ) ;
#150779 = DIRECTION ( 'NONE',  ( 0.000000000000000000, -0.9126074666063545004, -0.4088369013363783999 ) ) ;
#150780 = VECTOR ( 'NONE', #144829, 1000.000000000000000 ) ;
#150781 = LINE ( 'NONE', #71266, #17899 ) ;
#150782 = CYLINDRICAL_SURFACE ( 'NONE', #113503, 0.1000000000000028644 ) ;
#150783 = CARTESIAN_POINT ( 'NONE',  ( 20.04142135623731136, 11.75000000001116263, -58.15000000000000568 ) ) ;
#150784 = CYLINDRICAL_SURFACE ( 'NONE', #150715, 0.1000000000000028644 ) ;
#150785 = B_SPLINE_CURVE_WITH_KNOTS ( 'NONE', 3,
 ( #254229, #155189, #135569, #36522, #62480, #39078, #20797, #161597, #22077, #61185, #80726, #121196, #123736, #98993, #118614, #200700, #104143, #220278, #100283, #238535, #59874, #203260 ),
 .UNSPECIFIED., .F., .F.,
 ( 4, 3, 3, 3, 3, 3, 3, 4 ),
 ( 0.000000000000000000, 7.307836821077657032E-06, 4.161455748548155718E-05, 7.576591810647554650E-05, 0.0001098090429817538222, 0.0001438003617351105872, 0.0001777914035423655992, 0.0002117966137403026012 ),
 .UNSPECIFIED. ) ;
#150786 = SPHERICAL_SURFACE ( 'NONE', #248674, 0.1000000000000000056 ) ;
#150787 = EDGE_CURVE ( 'NONE', #163089, #182339, #128255, .T. ) ;
#150788 = CARTESIAN_POINT ( 'NONE',  ( -20.94999999999994600, 65.19115966511134275, -30.02310748452479316 ) ) ;
#150789 = ORIENTED_EDGE ( 'NONE', *, *, #155085, .T. ) ;
#150790 = ORIENTED_EDGE ( 'NONE', *, *, #29502, .F. ) ;
#150791 = DIRECTION ( 'NONE',  ( 1.073024830501117725E-15, 0.000000000000000000, 1.000000000000000000 ) ) ;
#150792 = EDGE_CURVE ( 'NONE', #197543, #36158, #66883, .T. ) ;
#150793 = ORIENTED_EDGE ( 'NONE', *, *, #249033, .F. ) ;
#150794 = FACE_OUTER_BOUND ( 'NONE', #73968, .T. ) ;
#150795 = ORIENTED_EDGE ( 'NONE', *, *, #182007, .T. ) ;
#150796 = FACE_OUTER_BOUND ( 'NONE', #121104, .T. ) ;
#150797 = AXIS2_PLACEMENT_3D ( 'NONE', #110920, #48373, #249165 ) ;
#150798 = DIRECTION ( 'NONE',  ( 0.000000000000000000, 0.000000000000000000, -1.000000000000000000 ) ) ;
#150799 = EDGE_CURVE ( 'NONE', #5409, #33881, #94914, .T. ) ;
#150800 = CARTESIAN_POINT ( 'NONE',  ( 18.56308993302896226, 65.61930884468735314, -44.78388484558566063 ) ) ;
#150801 = VERTEX_POINT ( 'NONE', #30342 ) ;
#150802 = CARTESIAN_POINT ( 'NONE',  ( 18.49999999999998934, 6.550000000011156231, -144.0170271704400307 ) ) ;
#150803 = EDGE_LOOP ( 'NONE', ( #185473, #106300, #12685, #87627 ) ) ;
#150804 = EDGE_CURVE ( 'NONE', #29169, #162073, #253129, .T. ) ;
#150805 = DIRECTION ( 'NONE',  ( 1.000000000000000000, -0.000000000000000000, -0.000000000000000000 ) ) ;
#150806 = CARTESIAN_POINT ( 'NONE',  ( 18.59999999999999787, 9.105964803472796021, -245.3658845043482586 ) ) ;
#150807 = ORIENTED_EDGE ( 'NONE', *, *, #7527, .T. ) ;
#150809 = LINE ( 'NONE', #208237, #36010 ) ;
#150808 = AXIS2_PLACEMENT_3D ( 'NONE', #42918, #25929, #183719 ) ;
#150810 = EDGE_CURVE ( 'NONE', #168386, #98749, #174080, .T. ) ;
#150811 = VERTEX_POINT ( 'NONE', #189406 ) ;
#150814 = VERTEX_POINT ( 'NONE', #225920 ) ;
#150813 = CARTESIAN_POINT ( 'NONE',  ( -23.15000000000000213, 1.115600667400684642E-11, -134.0000000000000000 ) ) ;
#150812 = CARTESIAN_POINT ( 'NONE',  ( -20.85000000000000142, 1.115600667400684642E-11, -100.5000000000000426 ) ) ;
#150815 = DIRECTION ( 'NONE',  ( 0.000000000000000000, 1.000000000000000000, -6.308085367188393199E-16 ) ) ;
#150816 = EDGE_LOOP ( 'NONE', ( #39867, #168900, #201601, #137304 ) ) ;
#150817 = AXIS2_PLACEMENT_3D ( 'NONE', #240246, #139831, #17342 ) ;
#150818 = DIRECTION ( 'NONE',  ( -1.000000000000000000, -0.000000000000000000, -0.000000000000000000 ) ) ;
#150819 = ORIENTED_EDGE ( 'NONE', *, *, #24095, .F. ) ;
#150820 = DIRECTION ( 'NONE',  ( 0.000000000000000000, -0.4791956752371546169, -0.8777080977375152360 ) ) ;
#150821 = VERTEX_POINT ( 'NONE', #47293 ) ;
#150822 = LINE ( 'NONE', #129956, #22601 ) ;
#150823 = EDGE_CURVE ( 'NONE', #236302, #8640, #240666, .T. ) ;
#150824 = DIRECTION ( 'NONE',  ( -6.938893903907222856E-15, -1.000000000000000000, -6.982962677686266711E-15 ) ) ;
#150825 = CARTESIAN_POINT ( 'NONE',  ( 18.51024323315077069, 67.49344847133113490, -195.4961807846321733 ) ) ;
#150826 = DIRECTION ( 'NONE',  ( 0.000000000000000000, 0.000000000000000000, 1.000000000000000000 ) ) ;
#150827 = VECTOR ( 'NONE', #135142, 1000.000000000000000 ) ;
#150828 = VERTEX_POINT ( 'NONE', #48595 ) ;
#150829 = AXIS2_PLACEMENT_3D ( 'NONE', #123898, #166901, #5189 ) ;
#150830 = DIRECTION ( 'NONE',  ( 1.000000000000000000, 0.000000000000000000, 0.000000000000000000 ) ) ;
#150831 = CARTESIAN_POINT ( 'NONE',  ( 18.50000000000000000, 86.87366311306882949, -199.3414869250131858 ) ) ;
#150832 = CARTESIAN_POINT ( 'NONE',  ( 21.08884785362045378, 6.357193367436396514, -33.45021690493315702 ) ) ;
#150833 = ORIENTED_EDGE ( 'NONE', *, *, #159749, .T. ) ;
#150834 = CARTESIAN_POINT ( 'NONE',  ( -20.15000000000000568, 61.49644909750671928, -221.5036531391373273 ) ) ;
#150835 = ORIENTED_EDGE ( 'NONE', *, *, #134741, .F. ) ;
#150836 = DIRECTION ( 'NONE',  ( 0.000000000000000000, 0.6728971962617388280, 0.7397360091702248619 ) ) ;
#150837 = ORIENTED_EDGE ( 'NONE', *, *, #11361, .F. ) ;
#150838 = CARTESIAN_POINT ( 'NONE',  ( -18.59999999999999787, 77.36242903720467723, -28.13422623660311217 ) ) ;
#150839 = CARTESIAN_POINT ( 'NONE',  ( -18.40000000000000213, 20.94763808724815846, -234.7254930126486556 ) ) ;
#150841 = VERTEX_POINT ( 'NONE', #206398 ) ;
#150840 = CARTESIAN_POINT ( 'NONE',  ( -16.80070461187950315, 44.13271087384504199, -235.3001729052809026 ) ) ;
#150842 = CARTESIAN_POINT ( 'NONE',  ( -20.54999999999999716, 49.36776662947724503, -253.7196102226803021 ) ) ;
#150843 = ORIENTED_EDGE ( 'NONE', *, *, #60601, .F. ) ;
#150844 = EDGE_CURVE ( 'NONE', #183504, #39117, #3136, .T. ) ;
#150845 = CARTESIAN_POINT ( 'NONE',  ( -20.99749315643147440, 36.02367272165624712, -235.8812521217649305 ) ) ;
#150846 = AXIS2_PLACEMENT_3D ( 'NONE', #147252, #170726, #250209 ) ;
#150847 = CIRCLE ( 'NONE', #217466, 0.09999999999999939493 ) ;
#150848 = DIRECTION ( 'NONE',  ( 0.000000000000000000, 0.9999631594459056361, -0.008583690987128059571 ) ) ;
#150849 = ORIENTED_EDGE ( 'NONE', *, *, #49482, .F. ) ;
#150850 = AXIS2_PLACEMENT_3D ( 'NONE', #139789, #219333, #40746 ) ;
#150851 = CARTESIAN_POINT ( 'NONE',  ( -16.87036670365549895, 66.01058118071021852, -90.50266760182643111 ) ) ;
#150852 = FACE_OUTER_BOUND ( 'NONE', #100127, .T. ) ;
#150853 = EDGE_LOOP ( 'NONE', ( #160607, #193283, #182548, #186014, #224152 ) ) ;
#150854 = CARTESIAN_POINT ( 'NONE',  ( -16.93658211146646408, 9.994108662352344297, -146.5957049300443487 ) ) ;
#150855 = ORIENTED_EDGE ( 'NONE', *, *, #85206, .T. ) ;
#150856 = EDGE_CURVE ( 'NONE', #1294, #162055, #115579, .T. ) ;
#150857 = DIRECTION ( 'NONE',  ( 0.000000000000000000, 0.000000000000000000, -1.000000000000000000 ) ) ;
#150858 = DIRECTION ( 'NONE',  ( 0.000000000000000000, -2.775557561562888827E-14, 1.000000000000000000 ) ) ;
#150859 = EDGE_CURVE ( 'NONE', #109890, #26118, #228025, .T. ) ;
#150860 = AXIS2_PLACEMENT_3D ( 'NONE', #22475, #223204, #2867 ) ;
#150863 = ORIENTED_EDGE ( 'NONE', *, *, #221212, .F. ) ;
#150862 = ORIENTED_EDGE ( 'NONE', *, *, #99767, .T. ) ;
#150861 = DIRECTION ( 'NONE',  ( 0.000000000000000000, 1.000000000000000000, 0.000000000000000000 ) ) ;
#150864 = DIRECTION ( 'NONE',  ( -1.000000000000000000, -0.000000000000000000, -0.000000000000000000 ) ) ;
#150865 = CARTESIAN_POINT ( 'NONE',  ( -22.50000000000000000, 0.1000000000111554016, -155.8504291924551808 ) ) ;
#150866 = DIRECTION ( 'NONE',  ( -1.000000000000000000, -0.000000000000000000, -0.000000000000000000 ) ) ;
#150868 = CARTESIAN_POINT ( 'NONE',  ( -21.05000000000000071, 6.400000000000003020, -9.930424630061573055 ) ) ;
#150867 = CARTESIAN_POINT ( 'NONE',  ( 22.49436431346199683, 0.06690352973341695542, -88.85004905234657713 ) ) ;
#150870 = ADVANCED_FACE ( 'NONE', ( #249388 ), #220001, .T. ) ;
#150869 = DIRECTION ( 'NONE',  ( -2.827886303505249259E-16, -0.8660254037844378194, -0.5000000000000016653 ) ) ;
#150871 = CARTESIAN_POINT ( 'NONE',  ( -18.59999999999999787, 11.65000000001115232, -112.6500000000000341 ) ) ;
#150872 = DIRECTION ( 'NONE',  ( 1.000000000000000000, 0.000000000000000000, 0.000000000000000000 ) ) ;
#150873 = VECTOR ( 'NONE', #172427, 999.9999999999998863 ) ;
#150874 = LINE ( 'NONE', #251244, #100727 ) ;
#150875 = VERTEX_POINT ( 'NONE', #150290 ) ;
#150876 = EDGE_LOOP ( 'NONE', ( #39390, #18594, #112347, #229814 ) ) ;
#150877 = DIRECTION ( 'NONE',  ( 0.000000000000000000, 0.000000000000000000, 1.000000000000000000 ) ) ;
#150879 = ORIENTED_EDGE ( 'NONE', *, *, #74636, .T. ) ;
#150878 = CARTESIAN_POINT ( 'NONE',  ( 20.85000000000000142, -1.835859311432481045, -179.0044391687985410 ) ) ;
#150880 = ORIENTED_EDGE ( 'NONE', *, *, #52105, .T. ) ;
#150882 = DIRECTION ( 'NONE',  ( -1.000000000000000000, -0.000000000000000000, -0.000000000000000000 ) ) ;
#150881 = AXIS2_PLACEMENT_3D ( 'NONE', #182637, #126494, #206036 ) ;
#150883 = ADVANCED_FACE ( 'NONE', ( #238899 ), #153413, .T. ) ;
#150884 = ORIENTED_EDGE ( 'NONE', *, *, #32806, .F. ) ;
#150885 = CYLINDRICAL_SURFACE ( 'NONE', #184369, 2.000000000000003553 ) ;
#150886 = EDGE_CURVE ( 'NONE', #1091, #83555, #107564, .T. ) ;
#150887 = EDGE_CURVE ( 'NONE', #78259, #121203, #28526, .T. ) ;
#150888 = ORIENTED_EDGE ( 'NONE', *, *, #11219, .T. ) ;
#150889 = AXIS2_PLACEMENT_3D ( 'NONE', #203421, #65179, #2631 ) ;
#150891 = TOROIDAL_SURFACE ( 'NONE', #105063, 0.2000000000000000111, 0.1000000000000000056 ) ;
#150890 = CARTESIAN_POINT ( 'NONE',  ( -20.85000000000000142, 68.97833521811233481, -166.1895420826271277 ) ) ;
#150892 = FACE_OUTER_BOUND ( 'NONE', #14885, .T. ) ;
#150894 = ORIENTED_EDGE ( 'NONE', *, *, #53194, .F. ) ;
#150893 = ORIENTED_EDGE ( 'NONE', *, *, #89728, .F. ) ;
#150895 = ORIENTED_EDGE ( 'NONE', *, *, #116796, .T. ) ;
#150896 = ORIENTED_EDGE ( 'NONE', *, *, #6118, .T. ) ;
#150898 = ORIENTED_EDGE ( 'NONE', *, *, #242989, .F. ) ;
#150897 = CIRCLE ( 'NONE', #13544, 0.1999999999999987899 ) ;
#150899 = ADVANCED_FACE ( 'NONE', ( #194661 ), #17290, .T. ) ;
#150900 = DIRECTION ( 'NONE',  ( 1.000000000000000000, 0.000000000000000000, 0.000000000000000000 ) ) ;
#150901 = DIRECTION ( 'NONE',  ( 0.000000000000000000, 0.000000000000000000, 1.000000000000000000 ) ) ;
#150902 = CARTESIAN_POINT ( 'NONE',  ( -15.69373346032659455, 9.356790025057037496, -184.7048265086138770 ) ) ;
#150904 = VERTEX_POINT ( 'NONE', #19859 ) ;
#150903 = FACE_OUTER_BOUND ( 'NONE', #143542, .T. ) ;
#150905 = CARTESIAN_POINT ( 'NONE',  ( -18.40000000000000213, 16.37093090900293646, -222.2277664635145982 ) ) ;
#150906 = EDGE_CURVE ( 'NONE', #151483, #183570, #174262, .T. ) ;
#150907 = CARTESIAN_POINT ( 'NONE',  ( 21.93340585971920831, 7.324147022865878043, -167.4999999999999432 ) ) ;
#150909 = ORIENTED_EDGE ( 'NONE', *, *, #187321, .F. ) ;
#150908 = CARTESIAN_POINT ( 'NONE',  ( -22.59999999999999787, 1.148907358139439339E-11, -201.0000000000015064 ) ) ;
#150910 = DIRECTION ( 'NONE',  ( 0.000000000000000000, 0.8068669527896844551, 0.5907332058517525963 ) ) ;
#150912 = EDGE_CURVE ( 'NONE', #252194, #68808, #253320, .T. ) ;
#150911 = EDGE_LOOP ( 'NONE', ( #31444, #196284, #172648, #145879, #134360, #15104, #159683, #187484, #197121, #255531, #114153, #186083, #181681, #76528 ) ) ;
#150913 = SPHERICAL_SURFACE ( 'NONE', #211995, 0.1000000000000000056 ) ;
#150914 = AXIS2_PLACEMENT_3D ( 'NONE', #89360, #11132, #247155 ) ;
#150915 = ORIENTED_EDGE ( 'NONE', *, *, #15424, .T. ) ;
#150916 = AXIS2_PLACEMENT_3D ( 'NONE', #91650, #231185, #92917 ) ;
#150917 = CARTESIAN_POINT ( 'NONE',  ( -23.25000000000000000, 31.85509083104287598, -238.8280249686205536 ) ) ;
#150919 = ORIENTED_EDGE ( 'NONE', *, *, #241311, .F. ) ;
#150918 = CIRCLE ( 'NONE', #234113, 0.09999999999999939493 ) ;
#150920 = VECTOR ( 'NONE', #158970, 1000.000000000000000 ) ;
#150922 = DIRECTION ( 'NONE',  ( 0.000000000000000000, 8.881784197000778021E-16, 1.000000000000000000 ) ) ;
#150921 = FACE_OUTER_BOUND ( 'NONE', #30055, .T. ) ;
#150923 = CIRCLE ( 'NONE', #100803, 11.90000000000000036 ) ;
#150924 = CARTESIAN_POINT ( 'NONE',  ( -18.79999999999999716, -6.162641848847272286, 0.4936627796039583793 ) ) ;
#150925 = DIRECTION ( 'NONE',  ( 0.000000000000000000, 0.2128009952263603122, -0.9770955615653315052 ) ) ;
#150926 = CARTESIAN_POINT ( 'NONE',  ( -21.05000000000000071, 1.162701749949165642, -41.60000000000000142 ) ) ;
#150928 = ORIENTED_EDGE ( 'NONE', *, *, #214696, .F. ) ;
#150927 = AXIS2_PLACEMENT_3D ( 'NONE', #95360, #157948, #197008 ) ;
#150929 = ORIENTED_EDGE ( 'NONE', *, *, #22322, .F. ) ;
#150930 = CIRCLE ( 'NONE', #217538, 0.09999999999999939493 ) ;
#150931 = DIRECTION ( 'NONE',  ( 0.000000000000000000, 0.000000000000000000, 1.000000000000000000 ) ) ;
#150932 = DIRECTION ( 'NONE',  ( -2.561896900575096011E-15, 0.5907332058517336115, -0.8068669527896984439 ) ) ;
#150934 = ADVANCED_FACE ( 'NONE', ( #235049 ), #56380, .F. ) ;
#150933 = EDGE_LOOP ( 'NONE', ( #36336, #216787, #230442, #236926 ) ) ;
#150935 = CARTESIAN_POINT ( 'NONE',  ( -21.14999999999999858, -0.1008583690875562017, -155.7504328765105868 ) ) ;
#150936 = ORIENTED_EDGE ( 'NONE', *, *, #251827, .T. ) ;
#150937 = EDGE_CURVE ( 'NONE', #167521, #170251, #77232, .T. ) ;
#150938 = CARTESIAN_POINT ( 'NONE',  ( 18.59999999999997655, 77.16412189325305349, -95.10825939895268277 ) ) ;
#150939 = CIRCLE ( 'NONE', #138434, 0.5999999999999987566 ) ;
#150940 = CARTESIAN_POINT ( 'NONE',  ( -18.50000000000000000, 7.021664781911246322, -137.8335654018973457 ) ) ;
#150941 = DIRECTION ( 'NONE',  ( 0.000000000000000000, -0.8660254037844420383, 0.4999999999999942824 ) ) ;
#150943 = EDGE_CURVE ( 'NONE', #68414, #32277, #178958, .T. ) ;
#150942 = VERTEX_POINT ( 'NONE', #198476 ) ;
#150944 = CARTESIAN_POINT ( 'NONE',  ( -18.79999999999999716, 6.841561409100513025, 9.675512259591560138 ) ) ;
#150945 = AXIS2_PLACEMENT_3D ( 'NONE', #134964, #76291, #56703 ) ;
#150946 = VECTOR ( 'NONE', #39509, 1000.000000000000000 ) ;
#150947 = ORIENTED_EDGE ( 'NONE', *, *, #221765, .F. ) ;
#150949 = ORIENTED_EDGE ( 'NONE', *, *, #228203, .T. ) ;
#150948 = AXIS2_PLACEMENT_3D ( 'NONE', #163815, #243330, #5996 ) ;
#150950 = ORIENTED_EDGE ( 'NONE', *, *, #172973, .T. ) ;
#150951 = DIRECTION ( 'NONE',  ( 0.000000000000000000, 0.8814952561688444987, -0.4721928772777320149 ) ) ;
#150952 = CARTESIAN_POINT ( 'NONE',  ( 14.11444803880196552, 66.54256847116262463, -54.52319054662471842 ) ) ;
#150953 = CARTESIAN_POINT ( 'NONE',  ( -21.09316766718153247, 0.03926340232583294676, -127.6298466875253013 ) ) ;
#150954 = DIRECTION ( 'NONE',  ( 0.000000000000000000, -1.000000000000000000, -6.982962677686266711E-15 ) ) ;
#150955 = CARTESIAN_POINT ( 'NONE',  ( -23.15000000000000213, 78.98983215084128062, -228.7927651294584450 ) ) ;
#150957 = CARTESIAN_POINT ( 'NONE',  ( 20.94999999999999929, 11.65000000001115943, -194.1583993101029364 ) ) ;
#150956 = CARTESIAN_POINT ( 'NONE',  ( -21.93340585970945611, 10.58724339642471612, -227.2765004563009370 ) ) ;
#150959 = ORIENTED_EDGE ( 'NONE', *, *, #232251, .F. ) ;
#150958 = CARTESIAN_POINT ( 'NONE',  ( 21.00000000000000000, 9.750000000011153745, -121.6500000000000341 ) ) ;
#150960 = CARTESIAN_POINT ( 'NONE',  ( 18.39999999999998082, 11.47316190337362585, -42.75000000000000000 ) ) ;
#150961 = ORIENTED_EDGE ( 'NONE', *, *, #10558, .T. ) ;
#150962 = DIRECTION ( 'NONE',  ( 0.000000000000000000, -0.1686199900910312910, 0.9856811345164826488 ) ) ;
#150963 = ORIENTED_EDGE ( 'NONE', *, *, #38387, .T. ) ;
#150964 = VERTEX_POINT ( 'NONE', #175118 ) ;
#150965 = CYLINDRICAL_SURFACE ( 'NONE', #4675, 5.000000000000000888 ) ;
#150966 = CARTESIAN_POINT ( 'NONE',  ( -20.54999999999999716, 76.00000000001215028, -138.5231074845243313 ) ) ;
#150968 = ADVANCED_FACE ( 'NONE', ( #36876 ), #118958, .T. ) ;
#150967 = DIRECTION ( 'NONE',  ( 0.000000000000000000, -7.056502275159890043E-15, 1.000000000000000000 ) ) ;
#150969 = DIRECTION ( 'NONE',  ( 0.000000000000000000, 1.000000000000000000, -1.387778780781454006E-13 ) ) ;
#150970 = ADVANCED_FACE ( 'NONE', ( #16019 ), #1549, .T. ) ;
#150971 = TOROIDAL_SURFACE ( 'NONE', #254948, 0.4000000000000017431, 0.1000000000000000056 ) ;
#150972 = CARTESIAN_POINT ( 'NONE',  ( 20.87600722750343252, 18.41291479239798079, -236.9963116028434058 ) ) ;
#150973 = EDGE_LOOP ( 'NONE', ( #43136, #190140, #208817, #123494 ) ) ;
#150974 = ORIENTED_EDGE ( 'NONE', *, *, #71168, .F. ) ;
#150975 = AXIS2_PLACEMENT_3D ( 'NONE', #88789, #172253, #91392 ) ;
#150977 = ADVANCED_FACE ( 'NONE', ( #137219 ), #34958, .F. ) ;
#150976 = LINE ( 'NONE', #29778, #99066 ) ;
#150978 = ORIENTED_EDGE ( 'NONE', *, *, #105516, .F. ) ;
#150979 = DIRECTION ( 'NONE',  ( -1.000000000000000000, 0.000000000000000000, 0.000000000000000000 ) ) ;
#150980 = CARTESIAN_POINT ( 'NONE',  ( 21.56666275994539816, 0.000000000000000000, 6.957368406893324142 ) ) ;
#150981 = EDGE_LOOP ( 'NONE', ( #2344, #23076, #30006, #229621, #55914, #74854 ) ) ;
#150982 = FACE_OUTER_BOUND ( 'NONE', #235913, .T. ) ;
#150983 = CARTESIAN_POINT ( 'NONE',  ( -20.94560253601877164, 11.75000000001115197, -60.01008351251526562 ) ) ;
#150984 = CARTESIAN_POINT ( 'NONE',  ( -16.87683809663752399, 9.850000000011144508, -120.5976359818037338 ) ) ;
#150985 = CARTESIAN_POINT ( 'NONE',  ( 21.13461538461538325, 65.38541703798675542, -157.7731074845244166 ) ) ;
#150986 = ORIENTED_EDGE ( 'NONE', *, *, #104678, .F. ) ;
#150987 = DIRECTION ( 'NONE',  ( 0.000000000000000000, -1.000000000000000000, 0.000000000000000000 ) ) ;
#150988 = EDGE_CURVE ( 'NONE', #167418, #71227, #40971, .T. ) ;
#150989 = DIRECTION ( 'NONE',  ( 1.000000000000000000, 0.000000000000000000, 0.000000000000000000 ) ) ;
#150990 = DIRECTION ( 'NONE',  ( 0.000000000000000000, 0.000000000000000000, -1.000000000000000000 ) ) ;
#150991 = CARTESIAN_POINT ( 'NONE',  ( 23.40000000000005187, 64.35000000001120668, -3.123107484524795474 ) ) ;
#150993 = ADVANCED_FACE ( 'NONE', ( #75969 ), #124094, .F. ) ;
#150992 = LINE ( 'NONE', #154862, #232996 ) ;
#150994 = CARTESIAN_POINT ( 'NONE',  ( -18.59999999999999787, 76.00000000001213607, -136.5231074845243313 ) ) ;
#150995 = EDGE_CURVE ( 'NONE', #222338, #34777, #22436, .T. ) ;
#150997 = ORIENTED_EDGE ( 'NONE', *, *, #228165, .F. ) ;
#150996 = CIRCLE ( 'NONE', #117664, 0.09999999999999749367 ) ;
#150999 = ADVANCED_FACE ( 'NONE', ( #202328 ), #220617, .T. ) ;
#150998 = EDGE_CURVE ( 'NONE', #94180, #94787, #95110, .T. ) ;
#151000 = DIRECTION ( 'NONE',  ( 0.000000000000000000, 0.9999631594459055250, 0.008583690987127922528 ) ) ;
#151001 = ORIENTED_EDGE ( 'NONE', *, *, #197000, .T. ) ;
#151002 = CARTESIAN_POINT ( 'NONE',  ( 15.06592377766031987, 66.58221053306006354, -154.6657229405476244 ) ) ;
#151003 = LINE ( 'NONE', #153613, #12859 ) ;
#151004 = LINE ( 'NONE', #84883, #246172 ) ;
#151005 = CARTESIAN_POINT ( 'NONE',  ( -20.64999999999999858, 7.150000000011155876, -88.15000000000004832 ) ) ;
#151006 = CARTESIAN_POINT ( 'NONE',  ( -11.60000000000000320, -9.650000000000005684, 17.60000000000000497 ) ) ;
#151007 = DIRECTION ( 'NONE',  ( -1.000000000000000000, -3.469446951953635015E-14, -2.422701857770461054E-28 ) ) ;
#151008 = ORIENTED_EDGE ( 'NONE', *, *, #11236, .T. ) ;
#151009 = LINE ( 'NONE', #28537, #200881 ) ;
#151010 = DIRECTION ( 'NONE',  ( 0.000000000000000000, 0.9126074666063545004, 0.4088369013363783999 ) ) ;
#151011 = DIRECTION ( 'NONE',  ( -0.000000000000000000, 0.03181660087583042251, -0.9994937237965568766 ) ) ;
#151012 = CARTESIAN_POINT ( 'NONE',  ( -21.55000000000000426, 7.750000000011159074, -188.7499999999999716 ) ) ;
#151013 = AXIS2_PLACEMENT_3D ( 'NONE', #148446, #149745, #208432 ) ;
#151014 = EDGE_CURVE ( 'NONE', #171657, #91388, #240861, .T. ) ;
#151015 = EDGE_CURVE ( 'NONE', #251509, #185777, #2827, .T. ) ;
#151017 = DIRECTION ( 'NONE',  ( -1.000000000000000000, -0.000000000000000000, -0.000000000000000000 ) ) ;
#151016 = AXIS2_PLACEMENT_3D ( 'NONE', #142408, #221920, #5439 ) ;
#151018 = EDGE_LOOP ( 'NONE', ( #54171, #229290, #26930 ) ) ;
#151019 = ORIENTED_EDGE ( 'NONE', *, *, #93768, .F. ) ;
#151020 = DIRECTION ( 'NONE',  ( 1.000000000000000000, 0.000000000000000000, 0.000000000000000000 ) ) ;
#151022 = CARTESIAN_POINT ( 'NONE',  ( -15.55912972643741199, 67.50912972644950116, -123.8731074845243683 ) ) ;
#151021 = CIRCLE ( 'NONE', #167595, 11.74999999999999822 ) ;
#151024 = EDGE_CURVE ( 'NONE', #58136, #58804, #143833, .T. ) ;
#151023 = DIRECTION ( 'NONE',  ( 0.000000000000000000, 0.9915357197604862671, -0.1298341882519953583 ) ) ;
#151025 = DIRECTION ( 'NONE',  ( 1.000000000000000000, 0.000000000000000000, 0.000000000000000000 ) ) ;
#151026 = VERTEX_POINT ( 'NONE', #242728 ) ;
#151028 = EDGE_CURVE ( 'NONE', #165636, #111732, #132525, .T. ) ;
#151027 = DIRECTION ( 'NONE',  ( -0.000000000000000000, 0.8660254037844502539, 0.4999999999999799605 ) ) ;
#151029 = EDGE_CURVE ( 'NONE', #111004, #24563, #161772, .T. ) ;
#151030 = DIRECTION ( 'NONE',  ( 0.000000000000000000, 0.000000000000000000, -1.000000000000000000 ) ) ;
#151031 = VECTOR ( 'NONE', #95718, 1000.000000000000000 ) ;
#151032 = ORIENTED_EDGE ( 'NONE', *, *, #26937, .F. ) ;
#151033 = CIRCLE ( 'NONE', #17716, 0.1000000000000004496 ) ;
#151034 = DIRECTION ( 'NONE',  ( 1.000000000000000000, -0.000000000000000000, -0.000000000000000000 ) ) ;
#151035 = ORIENTED_EDGE ( 'NONE', *, *, #121542, .F. ) ;
#151036 = ORIENTED_EDGE ( 'NONE', *, *, #9084, .F. ) ;
#151037 = VECTOR ( 'NONE', #73201, 1000.000000000000000 ) ;
#151038 = VERTEX_POINT ( 'NONE', #165796 ) ;
#151039 = EDGE_CURVE ( 'NONE', #221499, #64997, #146199, .T. ) ;
#151040 = DIRECTION ( 'NONE',  ( -1.073024830501117725E-15, -0.2617529984165031243, -0.9651348961777157509 ) ) ;
#151041 = CARTESIAN_POINT ( 'NONE',  ( 18.49999999999999289, 6.650000000011155876, -188.8499999999999659 ) ) ;
#151042 = DIRECTION ( 'NONE',  ( 2.952720810173290098E-16, 0.9651348961777149738, -0.2617529984165062884 ) ) ;
#151043 = CARTESIAN_POINT ( 'NONE',  ( -20.85000000000000142, 77.85161776048096272, -124.9199177649206689 ) ) ;
#151045 = CIRCLE ( 'NONE', #217652, 0.5000000000000007772 ) ;
#151044 = DIRECTION ( 'NONE',  ( -1.000000000000000000, -0.000000000000000000, 0.000000000000000000 ) ) ;
#151046 = CARTESIAN_POINT ( 'NONE',  ( 18.60000000000000497, 76.00000000001213607, -136.5231074845242745 ) ) ;
#151047 = CIRCLE ( 'NONE', #171926, 0.1000000000000000472 ) ;
#151048 = CARTESIAN_POINT ( 'NONE',  ( -16.93302609847409457, 9.996682520803211958, -12.58638849536254867 ) ) ;
#151051 = DIRECTION ( 'NONE',  ( -0.000000000000000000, 0.8814952561688430555, -0.4721928772777346239 ) ) ;
#151050 = VECTOR ( 'NONE', #29712, 1000.000000000000000 ) ;
#151049 = CARTESIAN_POINT ( 'NONE',  ( 20.95568717954149562, 65.39800594612007956, -95.42059911625572965 ) ) ;
#151052 = ADVANCED_FACE ( 'NONE', ( #23731 ), #122813, .T. ) ;
#151053 = CARTESIAN_POINT ( 'NONE',  ( -18.59999999999999787, 66.75000000001223555, -148.8731074845244393 ) ) ;
#151054 = CARTESIAN_POINT ( 'NONE',  ( 20.09999999999999787, 9.750000000011137757, -42.75000000000000000 ) ) ;
#151055 = CYLINDRICAL_SURFACE ( 'NONE', #21365, 0.1000000000000075273 ) ;
#151056 = CYLINDRICAL_SURFACE ( 'NONE', #144743, 0.09999999999999939493 ) ;
#151057 = ORIENTED_EDGE ( 'NONE', *, *, #253196, .T. ) ;
#151058 = CARTESIAN_POINT ( 'NONE',  ( -18.52309608778514161, -9.642476320055317629, -40.21459634116948223 ) ) ;
#151059 = FACE_OUTER_BOUND ( 'NONE', #94718, .T. ) ;
#151060 = CARTESIAN_POINT ( 'NONE',  ( -23.15000000000000213, -8.596261682231830292, -191.5498724828496790 ) ) ;
#151061 = CARTESIAN_POINT ( 'NONE',  ( -21.05000000000000071, 5.900000000011162093, -56.78090023534363695 ) ) ;
#151062 = DIRECTION ( 'NONE',  ( 0.000000000000000000, 0.000000000000000000, -1.000000000000000000 ) ) ;
#151063 = ADVANCED_FACE ( 'NONE', ( #225718 ), #223163, .T. ) ;
#151064 = DIRECTION ( 'NONE',  ( 0.000000000000000000, 0.5000000000000078826, 0.8660254037844340447 ) ) ;
#151065 = ORIENTED_EDGE ( 'NONE', *, *, #138298, .F. ) ;
#151066 = ORIENTED_EDGE ( 'NONE', *, *, #84902, .T. ) ;
#151067 = CARTESIAN_POINT ( 'NONE',  ( 18.49999999999999289, 11.65000000001115943, -88.75000000000004263 ) ) ;
#151068 = EDGE_LOOP ( 'NONE', ( #74561, #85625, #67399, #143352 ) ) ;
#151069 = CARTESIAN_POINT ( 'NONE',  ( 20.27550659511088682, 44.43555011622476769, -235.9687455856084739 ) ) ;
#151070 = CARTESIAN_POINT ( 'NONE',  ( 18.50000000000000000, 86.87366311306882949, -199.3414869250131858 ) ) ;
#151071 = CIRCLE ( 'NONE', #76043, 11.90000000000000746 ) ;
#151072 = CIRCLE ( 'NONE', #96857, 3.999999999999989786 ) ;
#151073 = EDGE_CURVE ( 'NONE', #130099, #174276, #184047, .T. ) ;
#151074 = ORIENTED_EDGE ( 'NONE', *, *, #189550, .F. ) ;
#151075 = DIRECTION ( 'NONE',  ( 1.000000000000000000, 0.000000000000000000, 0.000000000000000000 ) ) ;
#151076 = CIRCLE ( 'NONE', #200959, 0.1000000000000028644 ) ;
#151077 = VERTEX_POINT ( 'NONE', #164505 ) ;
#151078 = DIRECTION ( 'NONE',  ( 0.000000000000000000, 0.8814952561688438326, -0.4721928772777331251 ) ) ;
#151079 = CARTESIAN_POINT ( 'NONE',  ( -21.05000000000000071, -1.851028230129704522, -112.1539132694225316 ) ) ;
#151081 = VECTOR ( 'NONE', #198765, 1000.000000000000000 ) ;
#151080 = CARTESIAN_POINT ( 'NONE',  ( -23.25000000000000000, 62.42906104934358069, -247.8683112431566258 ) ) ;
#151082 = CYLINDRICAL_SURFACE ( 'NONE', #158, 0.09999999999999939493 ) ;
#151083 = CARTESIAN_POINT ( 'NONE',  ( 18.39999999999999503, 70.35000000001159037, -56.87310748452436115 ) ) ;
#151084 = LINE ( 'NONE', #15435, #37594 ) ;
#151085 = AXIS2_PLACEMENT_3D ( 'NONE', #242214, #103970, #101376 ) ;
#151086 = DIRECTION ( 'NONE',  ( 2.952720810173289112E-16, 1.000000000000000000, -6.088138035986627436E-46 ) ) ;
#151088 = DIRECTION ( 'NONE',  ( 0.000000000000000000, 0.9126074666063751506, 0.4088369013363318816 ) ) ;
#151087 = TOROIDAL_SURFACE ( 'NONE', #105239, 0.6000000000000015321, 0.1000000000000000056 ) ;
#151089 = AXIS2_PLACEMENT_3D ( 'NONE', #235872, #95087, #195502 ) ;
#151091 = VERTEX_POINT ( 'NONE', #27588 ) ;
#151090 = PLANE ( 'NONE',  #31996 ) ;
#151093 = CARTESIAN_POINT ( 'NONE',  ( -18.39999999999999858, 64.52683809664912928, -60.22327823605839825 ) ) ;
#151092 = CARTESIAN_POINT ( 'NONE',  ( 21.05000000000000071, 85.00000000001197975, -112.5170766071766764 ) ) ;
#151094 = EDGE_LOOP ( 'NONE', ( #162512, #69546, #201966, #73389 ) ) ;
#151096 = VERTEX_POINT ( 'NONE', #244011 ) ;
#151095 =( NAMED_UNIT ( * ) SI_UNIT ( $, .STERADIAN. ) SOLID_ANGLE_UNIT ( ) );
#151097 = ORIENTED_EDGE ( 'NONE', *, *, #155351, .F. ) ;
#151098 = LINE ( 'NONE', #32464, #16591 ) ;
#151099 = CIRCLE ( 'NONE', #225880, 0.09999999999998898659 ) ;
#151100 = CARTESIAN_POINT ( 'NONE',  ( -23.15000000000000213, 41.42187432231295219, -260.1830396872097140 ) ) ;
#151101 = AXIS2_PLACEMENT_3D ( 'NONE', #72566, #234172, #32163 ) ;
#151102 = CARTESIAN_POINT ( 'NONE',  ( 22.47110162079220785, 75.97120258720904928, -81.17304342120864646 ) ) ;
#151103 = DIRECTION ( 'NONE',  ( -0.000000000000000000, 0.1350103645451876666, 0.9908441862701600211 ) ) ;
#151104 = DIRECTION ( 'NONE',  ( 0.000000000000000000, 0.000000000000000000, 1.000000000000000000 ) ) ;
#151105 = CARTESIAN_POINT ( 'NONE',  ( 20.94999999999999929, 5.000000000011153745, -88.59473398108696074 ) ) ;
#151106 = VECTOR ( 'NONE', #215725, 1000.000000000000000 ) ;
#151107 = CARTESIAN_POINT ( 'NONE',  ( -17.80356949363338259, 12.81667427061739950, -208.7367314240743497 ) ) ;
#151108 = DIRECTION ( 'NONE',  ( 2.952720810173288126E-16, -0.9770955615653313941, -0.2128009952263603677 ) ) ;
#151109 = CIRCLE ( 'NONE', #5324, 0.1000000000000013933 ) ;
#151110 = EDGE_CURVE ( 'NONE', #110145, #6661, #236559, .T. ) ;
#151111 = CARTESIAN_POINT ( 'NONE',  ( -21.05000000000000071, 7.128833340093095217, -233.7327013124392749 ) ) ;
#151112 = CIRCLE ( 'NONE', #105263, 0.8750000000000007772 ) ;
#151113 = ORIENTED_EDGE ( 'NONE', *, *, #147958, .F. ) ;
#151114 = ORIENTED_EDGE ( 'NONE', *, *, #127661, .T. ) ;
#151115 = DIRECTION ( 'NONE',  ( 0.000000000000000000, 0.000000000000000000, 1.000000000000000000 ) ) ;
#151116 = VERTEX_POINT ( 'NONE', #228323 ) ;
#151117 = FACE_OUTER_BOUND ( 'NONE', #218664, .T. ) ;
#151118 = ORIENTED_EDGE ( 'NONE', *, *, #154585, .T. ) ;
#151120 = AXIS2_PLACEMENT_3D ( 'NONE', #177500, #135752, #77071 ) ;
#151119 = CARTESIAN_POINT ( 'NONE',  ( 18.52326479938720993, -9.642364444915429544, -40.21475741340573506 ) ) ;
#151121 = CIRCLE ( 'NONE', #255104, 0.1000000000000048489 ) ;
#151122 = AXIS2_PLACEMENT_3D ( 'NONE', #8098, #87600, #130590 ) ;
#151123 = VECTOR ( 'NONE', #4112, 1000.000000000000000 ) ;
#151124 = CARTESIAN_POINT ( 'NONE',  ( -23.25000000000000000, 11.75000000001115552, -55.25000000000004974 ) ) ;
#151125 = DIRECTION ( 'NONE',  ( -0.000000000000000000, -0.2617529984165031243, -0.9651348961777157509 ) ) ;
#151126 = EDGE_CURVE ( 'NONE', #15628, #140135, #148790, .T. ) ;
#151127 = CARTESIAN_POINT ( 'NONE',  ( -23.39999999999994529, 87.50449464844290048, -37.85861909827351468 ) ) ;
#151128 = CARTESIAN_POINT ( 'NONE',  ( -16.77683809663752257, 23.65833333334447985, -150.7500000000000284 ) ) ;
#151129 = VERTEX_POINT ( 'NONE', #169674 ) ;
#151130 = CARTESIAN_POINT ( 'NONE',  ( -18.44204374631831911, -9.491036389587209854, -207.6262012702209745 ) ) ;
#151131 = EDGE_CURVE ( 'NONE', #164268, #174107, #169989, .T. ) ;
#151132 = CARTESIAN_POINT ( 'NONE',  ( 20.94999999999999929, 6.650000000011155876, -144.0170271704400307 ) ) ;
#151133 = CYLINDRICAL_SURFACE ( 'NONE', #85478, 0.1000000000000124678 ) ;
#151134 = DIRECTION ( 'NONE',  ( 0.000000000000000000, 0.1084263158147437400, 0.9941044884914469471 ) ) ;
#151135 = CARTESIAN_POINT ( 'NONE',  ( -21.05000000000000071, 6.540656951712397138, -134.1000000000000227 ) ) ;
#151136 = DIRECTION ( 'NONE',  ( -1.000000000000000000, 0.000000000000000000, -0.000000000000000000 ) ) ;
#151137 = ORIENTED_EDGE ( 'NONE', *, *, #53381, .T. ) ;
#151139 = CARTESIAN_POINT ( 'NONE',  ( -20.64999999999999858, 76.00000000001195133, -103.0231074845243171 ) ) ;
#151138 = DIRECTION ( 'NONE',  ( -0.7071067811865389130, 8.659560562355038861E-17, -0.7071067811865561215 ) ) ;
#151141 = ADVANCED_FACE ( 'NONE', ( #211325 ), #67954, .F. ) ;
#151140 = AXIS2_PLACEMENT_3D ( 'NONE', #91477, #54894, #35391 ) ;
#151142 = ORIENTED_EDGE ( 'NONE', *, *, #13416, .T. ) ;
#151145 = ORIENTED_EDGE ( 'NONE', *, *, #19018, .F. ) ;
#151144 = CARTESIAN_POINT ( 'NONE',  ( -16.85312964099710342, 51.40816044925842476, -232.0807417151861500 ) ) ;
#151143 = CARTESIAN_POINT ( 'NONE',  ( 18.49999999999999645, 74.36282728704149747, -91.44095411905230719 ) ) ;
#151146 = VECTOR ( 'NONE', #223864, 1000.000000000000000 ) ;
#151147 = DIRECTION ( 'NONE',  ( 0.000000000000000000, -0.9651348961777157509, 0.2617529984165031243 ) ) ;
#151148 = CIRCLE ( 'NONE', #147010, 4.100000000000000533 ) ;
#151149 = ADVANCED_FACE ( 'NONE', ( #208765 ), #112238, .T. ) ;
#151150 = CARTESIAN_POINT ( 'NONE',  ( -23.15000000000000213, 11.75000000000000000, 0.000000000000000000 ) ) ;
#151151 = VERTEX_POINT ( 'NONE', #34007 ) ;
#151152 = CARTESIAN_POINT ( 'NONE',  ( -21.05000000000000071, 1.115600667400684642E-11, -167.5000000000000284 ) ) ;
#151153 = ADVANCED_FACE ( 'NONE', ( #9264 ), #88778, .F. ) ;
#151154 = FACE_OUTER_BOUND ( 'NONE', #84088, .T. ) ;
#151155 = ADVANCED_FACE ( 'NONE', ( #150086 ), #251729, .T. ) ;
#151157 = DIRECTION ( 'NONE',  ( 0.000000000000000000, 0.000000000000000000, -1.000000000000000000 ) ) ;
#151156 = CYLINDRICAL_SURFACE ( 'NONE', #122074, 0.09999999999999939493 ) ;
#151159 = VERTEX_POINT ( 'NONE', #189198 ) ;
#151158 = CARTESIAN_POINT ( 'NONE',  ( -20.05000000000000426, 66.75000000001199396, -115.2731074845243597 ) ) ;
#151160 = ADVANCED_FACE ( 'NONE', ( #127938 ), #10564, .T. ) ;
#151161 = EDGE_LOOP ( 'NONE', ( #70725, #134321, #102047, #222837 ) ) ;
#151162 = CARTESIAN_POINT ( 'NONE',  ( -20.85000000000000142, 11.65000000001115232, -67.00000000000000000 ) ) ;
#151163 = DIRECTION ( 'NONE',  ( 0.000000000000000000, 0.000000000000000000, -1.000000000000000000 ) ) ;
#151164 = DIRECTION ( 'NONE',  ( -0.000000000000000000, -0.000000000000000000, -1.000000000000000000 ) ) ;
#151165 = ORIENTED_EDGE ( 'NONE', *, *, #61470, .F. ) ;
#151166 = CARTESIAN_POINT ( 'NONE',  ( -18.40000000000000213, 5.650000000011139001, -188.3499999999999659 ) ) ;
#151167 = CARTESIAN_POINT ( 'NONE',  ( 18.60000000000000142, 85.32100840337361092, -162.7871692354463846 ) ) ;
#151168 = CARTESIAN_POINT ( 'NONE',  ( 20.85000000000000142, 69.01799029515542827, -99.32695536626806643 ) ) ;
#151169 = EDGE_CURVE ( 'NONE', #65963, #20109, #32611, .T. ) ;
#151170 = ORIENTED_EDGE ( 'NONE', *, *, #179533, .F. ) ;
#151171 = CARTESIAN_POINT ( 'NONE',  ( 20.94999999999999929, 1.115600667400684642E-11, -200.9999999999999432 ) ) ;
#151172 = EDGE_CURVE ( 'NONE', #34933, #135540, #211652, .T. ) ;
#151173 = CARTESIAN_POINT ( 'NONE',  ( -16.87683809663752399, 9.950000000011142376, -113.1500000000000341 ) ) ;
#151174 = ORIENTED_EDGE ( 'NONE', *, *, #99196, .F. ) ;
#151175 = CARTESIAN_POINT ( 'NONE',  ( -18.40000000000000213, 64.51332499825430489, -112.2731074845243739 ) ) ;
#151176 = CARTESIAN_POINT ( 'NONE',  ( -17.22361732159832215, 65.65484434140945780, -91.65232295865725121 ) ) ;
#151178 = ORIENTED_EDGE ( 'NONE', *, *, #240523, .T. ) ;
#151177 = AXIS2_PLACEMENT_3D ( 'NONE', #39473, #155571, #235081 ) ;
#151179 = VERTEX_POINT ( 'NONE', #250439 ) ;
#151180 = EDGE_CURVE ( 'NONE', #60665, #97217, #130487, .T. ) ;
#151181 = LINE ( 'NONE', #155055, #220792 ) ;
#151182 = ORIENTED_EDGE ( 'NONE', *, *, #65809, .F. ) ;
#151184 = ORIENTED_EDGE ( 'NONE', *, *, #93395, .T. ) ;
#151183 = FACE_OUTER_BOUND ( 'NONE', #19834, .T. ) ;
#151185 = VERTEX_POINT ( 'NONE', #191788 ) ;
#151188 = ORIENTED_EDGE ( 'NONE', *, *, #50290, .F. ) ;
#151187 = ORIENTED_EDGE ( 'NONE', *, *, #228724, .T. ) ;
#151186 = CARTESIAN_POINT ( 'NONE',  ( 21.87500000000000355, 9.750000000011153745, -188.7499999999999716 ) ) ;
#151189 = CARTESIAN_POINT ( 'NONE',  ( 23.24999999999999645, 9.180734019381761257, -233.2858192224647382 ) ) ;
#151190 = AXIS2_PLACEMENT_3D ( 'NONE', #134945, #15049, #12487 ) ;
#151191 = EDGE_LOOP ( 'NONE', ( #77220, #108878, #156564, #125513 ) ) ;
#151192 = DIRECTION ( 'NONE',  ( 1.441126678808781001E-14, 0.9876197685951252359, 0.1568667991644863424 ) ) ;
#151193 = DIRECTION ( 'NONE',  ( -7.304098846218490641E-16, -0.9651348961777379554, 0.2617529984164210233 ) ) ;
#151194 = CARTESIAN_POINT ( 'NONE',  ( 18.59999999999999076, 6.450000000011156587, -110.5170271704400591 ) ) ;
#151195 = AXIS2_PLACEMENT_3D ( 'NONE', #128971, #51967, #131524 ) ;
#151196 = EDGE_CURVE ( 'NONE', #25796, #114377, #53416, .T. ) ;
#151197 = DIRECTION ( 'NONE',  ( 1.000000000000000000, -3.448943450116723568E-16, -6.438528483529607644E-16 ) ) ;
#151198 = CARTESIAN_POINT ( 'NONE',  ( -22.50047199488185257, 25.91738416313705429, -254.3140340802643209 ) ) ;
#151199 = EDGE_LOOP ( 'NONE', ( #134832, #249308, #199058, #118544 ) ) ;
#151200 = ORIENTED_EDGE ( 'NONE', *, *, #168861, .T. ) ;
#151201 = ORIENTED_EDGE ( 'NONE', *, *, #48199, .T. ) ;
#151202 = CIRCLE ( 'NONE', #205149, 6.329289321881372388 ) ;
#151203 = DIRECTION ( 'NONE',  ( 0.000000000000000000, -0.000000000000000000, 1.000000000000000000 ) ) ;
#151205 = ORIENTED_EDGE ( 'NONE', *, *, #3741, .T. ) ;
#151204 = DIRECTION ( 'NONE',  ( -0.000000000000000000, -0.4856429311786292224, -0.8741572761215394838 ) ) ;
#151206 = DIRECTION ( 'NONE',  ( 1.000000000000000000, -7.304098846218133681E-16, -2.111765289898285610E-31 ) ) ;
#151208 = ORIENTED_EDGE ( 'NONE', *, *, #248812, .F. ) ;
#151207 = CARTESIAN_POINT ( 'NONE',  ( 18.41356215285960474, 78.24072131640578220, -231.5548844243369047 ) ) ;
#151209 = EDGE_CURVE ( 'NONE', #70270, #4212, #86700, .T. ) ;
#151210 = ORIENTED_EDGE ( 'NONE', *, *, #193056, .F. ) ;
#151211 = DIRECTION ( 'NONE',  ( -1.000000000000000000, 0.000000000000000000, 0.000000000000000000 ) ) ;
#151212 = AXIS2_PLACEMENT_3D ( 'NONE', #81919, #161520, #20726 ) ;
#151213 = EDGE_CURVE ( 'NONE', #174818, #244668, #71826, .T. ) ;
#151214 = CIRCLE ( 'NONE', #184498, 4.149999999999999467 ) ;
#151215 = ADVANCED_FACE ( 'NONE', ( #13131 ), #92643, .T. ) ;
#151216 = VERTEX_POINT ( 'NONE', #113501 ) ;
#151217 = VECTOR ( 'NONE', #17611, 1000.000000000000000 ) ;
#151218 = CARTESIAN_POINT ( 'NONE',  ( 22.39999999999999503, 64.25000000001165290, -69.52310748452438816 ) ) ;
#151219 = LINE ( 'NONE', #95076, #173625 ) ;
#151220 = EDGE_CURVE ( 'NONE', #46929, #164364, #193052, .T. ) ;
#151222 = ORIENTED_EDGE ( 'NONE', *, *, #141397, .F. ) ;
#151221 = VERTEX_POINT ( 'NONE', #95220 ) ;
#151223 = VERTEX_POINT ( 'NONE', #238583 ) ;
#151224 = CARTESIAN_POINT ( 'NONE',  ( -16.87683809663752399, 44.86297841676450560, -235.0825981793917947 ) ) ;
#151225 = EDGE_LOOP ( 'NONE', ( #185244, #246401, #27631, #231233 ) ) ;
#151226 = EDGE_LOOP ( 'NONE', ( #208326, #106926, #16722, #63664, #63975, #159952, #248619, #211136, #109084, #66293, #238218, #91056, #123365, #111126, #170122, #88041, #150671, #191654, #212109, #149905, #152379, #67199, #50738, #236646, #68929, #48032, #244176 ) ) ;
#151227 = EDGE_CURVE ( 'NONE', #52970, #56430, #232678, .T. ) ;
#151228 = CARTESIAN_POINT ( 'NONE',  ( 20.95512820512820440, 65.37615131629972609, -61.85819391543678591 ) ) ;
#151230 = ORIENTED_EDGE ( 'NONE', *, *, #2216, .T. ) ;
#151229 = DIRECTION ( 'NONE',  ( 1.000000000000000000, 0.000000000000000000, -0.000000000000000000 ) ) ;
#151231 = CARTESIAN_POINT ( 'NONE',  ( -23.25000000000000000, 77.85161776048127535, -158.4199177649206831 ) ) ;
#151233 = DIRECTION ( 'NONE',  ( -0.000000000000000000, 1.000000000000000000, 0.000000000000000000 ) ) ;
#151232 = DIRECTION ( 'NONE',  ( 0.000000000000000000, -0.4999999999999348299, 0.8660254037844762331 ) ) ;
#151234 = CARTESIAN_POINT ( 'NONE',  ( -21.05000000000000071, -1.162701749926853712, -75.10000000000003695 ) ) ;
#151235 = CARTESIAN_POINT ( 'NONE',  ( -20.85000000000000142, 1.115600667400684642E-11, -200.9999999999999432 ) ) ;
#151236 = ORIENTED_EDGE ( 'NONE', *, *, #228816, .F. ) ;
#151237 = AXIS2_PLACEMENT_3D ( 'NONE', #8310, #207807, #9568 ) ;
#151238 = VECTOR ( 'NONE', #78927, 1000.000000000000000 ) ;
#151239 = AXIS2_PLACEMENT_3D ( 'NONE', #17952, #15417, #213587 ) ;
#151240 = VERTEX_POINT ( 'NONE', #174811 ) ;
#151242 = CIRCLE ( 'NONE', #234610, 14.20833333333334103 ) ;
#151241 = CARTESIAN_POINT ( 'NONE',  ( 18.39999999999999858, 85.50000000001185185, -96.42291809330218655 ) ) ;
#151243 = CARTESIAN_POINT ( 'NONE',  ( 23.14999999999999858, 4.775700934590584090, -78.84876810404601599 ) ) ;
#151244 = LINE ( 'NONE', #73009, #112081 ) ;
#151245 = ORIENTED_EDGE ( 'NONE', *, *, #67027, .F. ) ;
#151246 = EDGE_CURVE ( 'NONE', #163009, #111888, #190990, .T. ) ;
#151247 = DIRECTION ( 'NONE',  ( 0.000000000000000000, 0.000000000000000000, 1.000000000000000000 ) ) ;
#151248 = DIRECTION ( 'NONE',  ( 0.000000000000000000, 0.8814952561688430555, -0.4721928772777346239 ) ) ;
#151249 = ORIENTED_EDGE ( 'NONE', *, *, #181014, .T. ) ;
#151250 = ORIENTED_EDGE ( 'NONE', *, *, #194864, .T. ) ;
#151251 = CARTESIAN_POINT ( 'NONE',  ( -18.59999999999999787, 68.49522935589659767, -224.1230159437372436 ) ) ;
#151252 = LINE ( 'NONE', #170859, #161306 ) ;
#151254 = ADVANCED_FACE ( 'NONE', ( #99046 ), #138178, .T. ) ;
#151253 = ORIENTED_EDGE ( 'NONE', *, *, #197695, .F. ) ;
#151255 = CARTESIAN_POINT ( 'NONE',  ( 20.94999999999999929, 1.115625160336667635E-11, -165.5000000000000284 ) ) ;
#151256 = EDGE_LOOP ( 'NONE', ( #13674, #186267, #115199, #208636 ) ) ;
#151257 = ADVANCED_FACE ( 'NONE', ( #233474 ), #91015, .T. ) ;
#151258 = CARTESIAN_POINT ( 'NONE',  ( 18.44208962362687387, -9.552340496897866018, -140.8421730554626095 ) ) ;
#151259 = FACE_OUTER_BOUND ( 'NONE', #154687, .T. ) ;
#151261 = CARTESIAN_POINT ( 'NONE',  ( -21.05000000000000426, -1.387982811671854444, -194.7102154522737578 ) ) ;
#151260 = CARTESIAN_POINT ( 'NONE',  ( 15.48841904831874849, 67.43841904833078615, -115.6731074845243654 ) ) ;
#151262 = CARTESIAN_POINT ( 'NONE',  ( 19.87657994472042233, 11.75000000001092992, -91.76578812462598478 ) ) ;
#151263 = CYLINDRICAL_SURFACE ( 'NONE', #61853, 0.5000000000000004441 ) ;
#151264 = CARTESIAN_POINT ( 'NONE',  ( 23.14999999999999858, 76.00000000001142553, -36.02310748452432421 ) ) ;
#151265 = CARTESIAN_POINT ( 'NONE',  ( 20.04142135623730070, 64.25000000001246292, -181.7731074845244450 ) ) ;
#151266 = CIRCLE ( 'NONE', #18153, 0.1999999999999987899 ) ;
#151267 = AXIS2_PLACEMENT_3D ( 'NONE', #46045, #208978, #105999 ) ;
#151268 = ADVANCED_FACE ( 'NONE', ( #39124 ), #58640, .F. ) ;
#151270 = EDGE_LOOP ( 'NONE', ( #161857, #208338, #92193, #110657 ) ) ;
#151269 = DIRECTION ( 'NONE',  ( 0.000000000000000000, 1.000000000000000000, 7.272083257015735086E-15 ) ) ;
#151272 = ORIENTED_EDGE ( 'NONE', *, *, #184531, .T. ) ;
#151271 = ORIENTED_EDGE ( 'NONE', *, *, #131904, .T. ) ;
#151273 = VERTEX_POINT ( 'NONE', #97758 ) ;
#151274 = CIRCLE ( 'NONE', #251181, 11.80000000000000426 ) ;
#151275 = CARTESIAN_POINT ( 'NONE',  ( -16.77683809663752257, 60.94702803318471496, -221.0293550571836647 ) ) ;
#151276 = CIRCLE ( 'NONE', #9596, 4.300000000000029132 ) ;
#151277 = DIRECTION ( 'NONE',  ( 0.000000000000000000, 0.2128009952263601456, -0.9770955615653316162 ) ) ;
#151279 = DIRECTION ( 'NONE',  ( 0.000000000000000000, -6.853228547068871147E-15, 1.000000000000000000 ) ) ;
#151278 = CARTESIAN_POINT ( 'NONE',  ( -16.87683809663752044, 66.13508655273233217, -183.2988259332204564 ) ) ;
#151280 = DIRECTION ( 'NONE',  ( -4.336808689942052446E-15, 0.03181660087581661411, -0.9994937237965575427 ) ) ;
#151281 = ORIENTED_EDGE ( 'NONE', *, *, #168780, .F. ) ;
#151282 = CIRCLE ( 'NONE', #134486, 4.049999999999998934 ) ;
#151283 = CARTESIAN_POINT ( 'NONE',  ( 21.53699400380201467, 69.21228820681596972, -69.52310748452435973 ) ) ;
#151284 = EDGE_LOOP ( 'NONE', ( #233835, #122023, #249348, #217812, #118715, #187015, #11895, #43575 ) ) ;
#151286 = ADVANCED_FACE ( 'NONE', ( #256803 ), #157700, .T. ) ;
#151285 = ORIENTED_EDGE ( 'NONE', *, *, #155090, .F. ) ;
#151287 = DIRECTION ( 'NONE',  ( 1.000000000000000000, 0.000000000000000000, 0.000000000000000000 ) ) ;
#151288 = AXIS2_PLACEMENT_3D ( 'NONE', #47850, #12622, #145677 ) ;
#151289 = DIRECTION ( 'NONE',  ( 0.000000000000000000, -0.3896596508880098009, -0.9209589331071360574 ) ) ;
#151290 = AXIS2_PLACEMENT_3D ( 'NONE', #205064, #47272, #70743 ) ;
#151291 = AXIS2_PLACEMENT_3D ( 'NONE', #158941, #242288, #59783 ) ;
#151292 = DIRECTION ( 'NONE',  ( 0.000000000000000000, 6.938893903907222067E-15, -1.000000000000000000 ) ) ;
#151293 = ORIENTED_EDGE ( 'NONE', *, *, #97871, .T. ) ;
#151294 = LINE ( 'NONE', #172171, #118103 ) ;
#151295 = AXIS2_PLACEMENT_3D ( 'NONE', #257241, #233880, #158235 ) ;
#151296 = FACE_OUTER_BOUND ( 'NONE', #134687, .T. ) ;
#151297 = ORIENTED_EDGE ( 'NONE', *, *, #50445, .F. ) ;
#151298 = VERTEX_POINT ( 'NONE', #76936 ) ;
#151299 = CARTESIAN_POINT ( 'NONE',  ( 18.39999999999999503, 11.75000000001113953, -158.2500000000000284 ) ) ;
#151300 = DIRECTION ( 'NONE',  ( -1.020425574104004196E-15, -1.210927747993693964E-31, 1.000000000000000000 ) ) ;
#151301 = CARTESIAN_POINT ( 'NONE',  ( 18.49999999999999289, 15.22030141505243961, -222.9130098973476777 ) ) ;
#151302 = CARTESIAN_POINT ( 'NONE',  ( -18.50000000000000000, 1.835341550235567887, -45.05515129256298223 ) ) ;
#151303 = DIRECTION ( 'NONE',  ( -1.040834085586090694E-13, 0.1568667991644355497, 0.9876197685951332295 ) ) ;
#151305 = VECTOR ( 'NONE', #62788, 1000.000000000000000 ) ;
#151304 = CARTESIAN_POINT ( 'NONE',  ( -21.14999999999999858, 64.25000000001215028, -136.5231074845243597 ) ) ;
#151306 = ORIENTED_EDGE ( 'NONE', *, *, #240865, .T. ) ;
#151307 = DIRECTION ( 'NONE',  ( 0.000000000000000000, 0.9126074666063844765, 0.4088369013363113980 ) ) ;
#151308 = CARTESIAN_POINT ( 'NONE',  ( -23.15000000000000213, 1.115600667400684642E-11, -196.9999999999999432 ) ) ;
#151309 = AXIS2_PLACEMENT_3D ( 'NONE', #249885, #9990, #126066 ) ;
#151310 = EDGE_CURVE ( 'NONE', #10053, #34828, #254275, .T. ) ;
#151311 = CARTESIAN_POINT ( 'NONE',  ( -18.43707690579159930, 85.68240343348850274, -129.8662641071114763 ) ) ;
#151312 = DIRECTION ( 'NONE',  ( 0.000000000000000000, 0.000000000000000000, -1.000000000000000000 ) ) ;
#151313 = DIRECTION ( 'NONE',  ( 0.000000000000000000, 0.9915357197604892647, -0.1298341882519715440 ) ) ;
#151314 = AXIS2_PLACEMENT_3D ( 'NONE', #202175, #23581, #103051 ) ;
#151316 = EDGE_CURVE ( 'NONE', #122358, #238290, #74491, .T. ) ;
#151315 = FACE_OUTER_BOUND ( 'NONE', #142472, .T. ) ;
#151317 = DIRECTION ( 'NONE',  ( -6.938893903907222067E-15, -1.000000000000000000, -6.982962677686266711E-15 ) ) ;
#151319 = ORIENTED_EDGE ( 'NONE', *, *, #144412, .F. ) ;
#151318 = CARTESIAN_POINT ( 'NONE',  ( -20.94999999999999929, 87.65000000001214175, -136.5231074845242745 ) ) ;
#151320 = VECTOR ( 'NONE', #64896, 1000.000000000000000 ) ;
#151321 = TOROIDAL_SURFACE ( 'NONE', #51305, 0.4000000000000012990, 0.1000000000000000056 ) ;
#151322 = AXIS2_PLACEMENT_3D ( 'NONE', #211117, #16460, #195097 ) ;
#151323 = EDGE_CURVE ( 'NONE', #214033, #193752, #176074, .T. ) ;
#151324 = AXIS2_PLACEMENT_3D ( 'NONE', #256459, #157469, #97420 ) ;
#151325 = EDGE_CURVE ( 'NONE', #245608, #125678, #79492, .T. ) ;
#151326 = DIRECTION ( 'NONE',  ( -3.440080580676165868E-14, -0.1298341882520124002, -0.9915357197604841577 ) ) ;
#151327 = FACE_OUTER_BOUND ( 'NONE', #104954, .T. ) ;
#151328 = CARTESIAN_POINT ( 'NONE',  ( -18.40000000000000213, 64.52683809665003878, -179.3490535513324176 ) ) ;
#151329 = CARTESIAN_POINT ( 'NONE',  ( 20.85000000000000142, 67.75954444190071513, -227.8703747234148693 ) ) ;
#151330 = DIRECTION ( 'NONE',  ( 0.000000000000000000, -0.8700118002898321601, 0.4930308989875230030 ) ) ;
#151331 = CIRCLE ( 'NONE', #5536, 0.09999999999999892308 ) ;
#151332 = AXIS2_PLACEMENT_3D ( 'NONE', #217132, #114207, #56765 ) ;
#151334 = EDGE_CURVE ( 'NONE', #156131, #108803, #20289, .T. ) ;
#151333 = AXIS2_PLACEMENT_3D ( 'NONE', #53317, #235789, #113286 ) ;
#151336 = CARTESIAN_POINT ( 'NONE',  ( -21.05000000000000071, 4.158309866074138661, -211.9342015984041439 ) ) ;
#151335 = CIRCLE ( 'NONE', #159697, 0.1000000000000028644 ) ;
#151337 = EDGE_CURVE ( 'NONE', #221237, #224632, #63091, .T. ) ;
#151338 = DIRECTION ( 'NONE',  ( 0.000000000000000000, -0.2617529984165031243, -0.9651348961777157509 ) ) ;
#151339 = FACE_OUTER_BOUND ( 'NONE', #112375, .T. ) ;
#151340 = ORIENTED_EDGE ( 'NONE', *, *, #79596, .T. ) ;
#151341 = CARTESIAN_POINT ( 'NONE',  ( -16.92209698673576668, 66.05000000001159322, -56.81247191747281988 ) ) ;
#151343 = ORIENTED_EDGE ( 'NONE', *, *, #252639, .F. ) ;
#151342 = DIRECTION ( 'NONE',  ( 0.000000000000000000, 0.9651348961777157509, -0.2617529984165031243 ) ) ;
#151344 = DIRECTION ( 'NONE',  ( 1.000000000000000000, 0.000000000000000000, 0.000000000000000000 ) ) ;
#151345 = CARTESIAN_POINT ( 'NONE',  ( -20.94999999999999929, 11.65000000001115232, -127.2161343370219413 ) ) ;
#151346 = ORIENTED_EDGE ( 'NONE', *, *, #24146, .F. ) ;
#151347 = DIRECTION ( 'NONE',  ( 0.000000000000000000, 0.000000000000000000, -1.000000000000000000 ) ) ;
#151348 = PRODUCT_CONTEXT ( 'NONE', #7431, 'mechanical' ) ;
#151349 = CARTESIAN_POINT ( 'NONE',  ( -20.94983749550516450, 65.70233904876990039, -64.04874109119681691 ) ) ;
#151350 = ADVANCED_FACE ( 'NONE', ( #173532 ), #81344, .T. ) ;
#151351 = CARTESIAN_POINT ( 'NONE',  ( -20.64999999999999858, 1.940186915899009490, -180.3291192110532961 ) ) ;
#151352 = PLANE ( 'NONE',  #183893 ) ;
#151353 = ORIENTED_EDGE ( 'NONE', *, *, #160197, .F. ) ;
#151354 = CARTESIAN_POINT ( 'NONE',  ( -15.75000000000000355, 26.54497872210690090, -232.9592037335782209 ) ) ;
#151355 = CYLINDRICAL_SURFACE ( 'NONE', #71712, 1.749999999999998002 ) ;
#151356 = EDGE_CURVE ( 'NONE', #167415, #206865, #61975, .T. ) ;
#151357 = AXIS2_PLACEMENT_3D ( 'NONE', #79849, #216810, #36940 ) ;
#151358 = DIRECTION ( 'NONE',  ( 0.000000000000000000, 0.2128009952263403282, -0.9770955615653358350 ) ) ;
#151359 = ORIENTED_EDGE ( 'NONE', *, *, #207845, .T. ) ;
#151360 = ORIENTED_EDGE ( 'NONE', *, *, #206039, .T. ) ;
#151361 = ADVANCED_FACE ( 'NONE', ( #165480 ), #142044, .T. ) ;
#151362 = LINE ( 'NONE', #191782, #192412 ) ;
#151363 = PLANE ( 'NONE',  #127901 ) ;
#151364 = CARTESIAN_POINT ( 'NONE',  ( -23.25000000000000000, 69.16514130714681130, -247.7543978865853660 ) ) ;
#151365 = DIRECTION ( 'NONE',  ( 1.000000000000000000, 0.000000000000000000, 0.000000000000000000 ) ) ;
#151367 = CARTESIAN_POINT ( 'NONE',  ( 22.46250603428203618, -2.458442580695145985, -189.6124709730212032 ) ) ;
#151366 = DIRECTION ( 'NONE',  ( 0.000000000000000000, 0.000000000000000000, -1.000000000000000000 ) ) ;
#151368 = ADVANCED_FACE ( 'NONE', ( #160365 ), #18167, .F. ) ;
#151369 = CARTESIAN_POINT ( 'NONE',  ( -21.09813707148783735, 75.96864850048297058, -176.4081695902610250 ) ) ;
#151370 = DIRECTION ( 'NONE',  ( 0.000000000000000000, 1.734723475976997999E-14, -1.000000000000000000 ) ) ;
#151372 = DIRECTION ( 'NONE',  ( 0.000000000000000000, -1.000000000000000000, 0.000000000000000000 ) ) ;
#151371 = TOROIDAL_SURFACE ( 'NONE', #255529, 12.77499999999999858, 0.1000000000000000056 ) ;
#151373 = ORIENTED_EDGE ( 'NONE', *, *, #189785, .T. ) ;
#151374 = AXIS2_PLACEMENT_3D ( 'NONE', #191815, #50960, #28909 ) ;
#151376 = ORIENTED_EDGE ( 'NONE', *, *, #237917, .F. ) ;
#151375 = CARTESIAN_POINT ( 'NONE',  ( 12.25000000000000000, 62.62153588618860311, -217.1314428046943590 ) ) ;
#151377 = DIRECTION ( 'NONE',  ( 2.710505431213777355E-16, -1.000000000000000000, 0.000000000000000000 ) ) ;
#151378 = CARTESIAN_POINT ( 'NONE',  ( 21.05000000000000071, -11.64999999998883595, -164.5000000000000000 ) ) ;
#151381 = CARTESIAN_POINT ( 'NONE',  ( -21.14999999999999858, 11.75000000001115552, -140.7838656629781724 ) ) ;
#151380 = CARTESIAN_POINT ( 'NONE',  ( 21.30000000000002558, 1.115600667400684642E-11, -67.00000000000004263 ) ) ;
#151379 = VECTOR ( 'NONE', #241996, 1000.000000000000000 ) ;
#151382 = VERTEX_POINT ( 'NONE', #204582 ) ;
#151383 = CARTESIAN_POINT ( 'NONE',  ( -21.45000000000000284, 7.708578643762696636, -21.25000000000000000 ) ) ;
#151384 = CARTESIAN_POINT ( 'NONE',  ( 20.01093837587850288, 64.25000000001196554, -111.7687100499271793 ) ) ;
#151385 = EDGE_CURVE ( 'NONE', #68820, #127120, #62520, .T. ) ;
#151386 = DIRECTION ( 'NONE',  ( 1.000000000000000000, 0.000000000000000000, 0.000000000000000000 ) ) ;
#151387 = CARTESIAN_POINT ( 'NONE',  ( 12.68104795156994413, 12.99171346507298708, -216.4962224982961345 ) ) ;
#151388 = ORIENTED_EDGE ( 'NONE', *, *, #199456, .T. ) ;
#151389 = VERTEX_POINT ( 'NONE', #61230 ) ;
#151391 = AXIS2_PLACEMENT_3D ( 'NONE', #206509, #50004, #223488 ) ;
#151390 = CARTESIAN_POINT ( 'NONE',  ( -21.64999999999999858, 68.65000000001180069, -81.87310748452436826 ) ) ;
#151392 = ORIENTED_EDGE ( 'NONE', *, *, #112439, .T. ) ;
#151393 = DIRECTION ( 'NONE',  ( 0.000000000000000000, 0.000000000000000000, -1.000000000000000000 ) ) ;
#151394 = VECTOR ( 'NONE', #119364, 1000.000000000000000 ) ;
#151395 = DIRECTION ( 'NONE',  ( 1.000000000000000000, 0.000000000000000000, 0.000000000000000000 ) ) ;
#151397 = SPHERICAL_SURFACE ( 'NONE', #81692, 0.1000000000000000056 ) ;
#151396 = CIRCLE ( 'NONE', #85265, 0.09999999999999939493 ) ;
#151398 = AXIS2_PLACEMENT_3D ( 'NONE', #98844, #139268, #179719 ) ;
#151399 = CARTESIAN_POINT ( 'NONE',  ( 20.05000000000002913, 7.250000000011171508, -188.3499999999999659 ) ) ;
#151400 = ORIENTED_EDGE ( 'NONE', *, *, #170334, .T. ) ;
#151401 = LINE ( 'NONE', #73161, #114002 ) ;
#151402 = DIRECTION ( 'NONE',  ( -1.020425574104003999E-15, 0.8814952561688429444, -0.4721928772777345684 ) ) ;
#151403 = DIRECTION ( 'NONE',  ( 0.000000000000000000, 0.2128009952263601179, -0.9770955615653315052 ) ) ;
#151404 = CIRCLE ( 'NONE', #38971, 12.87499999999999822 ) ;
#151406 = DIRECTION ( 'NONE',  ( -1.000000000000000000, 0.000000000000000000, 0.000000000000000000 ) ) ;
#151405 = AXIS2_PLACEMENT_3D ( 'NONE', #233920, #115256, #155702 ) ;
#151408 = AXIS2_PLACEMENT_3D ( 'NONE', #33092, #93013, #89153 ) ;
#151407 = PLANE ( 'NONE',  #166423 ) ;
#151409 = CARTESIAN_POINT ( 'NONE',  ( -23.25000000000000000, 8.576967729067776602, -220.8801565530754090 ) ) ;
#151410 = ORIENTED_EDGE ( 'NONE', *, *, #180822, .T. ) ;
#151412 = DIRECTION ( 'NONE',  ( 1.000000000000000000, 0.000000000000000000, 0.000000000000000000 ) ) ;
#151411 = CARTESIAN_POINT ( 'NONE',  ( 20.94999999999999929, 77.04701199367727327, -199.6625678998140359 ) ) ;
#151413 = ORIENTED_EDGE ( 'NONE', *, *, #240919, .T. ) ;
#151415 = EDGE_LOOP ( 'NONE', ( #34827, #120077, #256520, #165657 ) ) ;
#151414 = DIRECTION ( 'NONE',  ( 0.7071067811865487940, 8.659560562354918067E-17, 0.7071067811865463515 ) ) ;
#151416 = ORIENTED_EDGE ( 'NONE', *, *, #244680, .T. ) ;
#151417 = DIRECTION ( 'NONE',  ( 0.000000000000000000, 0.2617529984165031243, 0.9651348961777157509 ) ) ;
#151418 = CARTESIAN_POINT ( 'NONE',  ( 12.25000000000000355, 66.65000000001226965, -153.1588398769083028 ) ) ;
#151420 = CARTESIAN_POINT ( 'NONE',  ( 18.49999999999999289, 65.62657994473217116, -78.25731935989797705 ) ) ;
#151419 = B_SPLINE_CURVE_WITH_KNOTS ( 'NONE', 3,
 ( #62895, #103286, #182873, #159446, #238981, #90140 ),
 .UNSPECIFIED., .F., .F.,
 ( 4, 2, 4 ),
 ( 0.000000000000000000, 0.0001895189928937342824, 0.0003790379857874685648 ),
 .UNSPECIFIED. ) ;
#151421 = AXIS2_PLACEMENT_3D ( 'NONE', #200023, #38377, #21406 ) ;
#151422 = DIRECTION ( 'NONE',  ( -0.000000000000000000, -0.9875055080513799322, 0.1575844902526464253 ) ) ;
#151423 = VERTEX_POINT ( 'NONE', #66369 ) ;
#151424 = CARTESIAN_POINT ( 'NONE',  ( 21.05000000000000071, 87.75000000001190870, -100.1231074845242262 ) ) ;
#151425 = CARTESIAN_POINT ( 'NONE',  ( 21.98333005346336222, 1.115600667400684642E-11, -126.6259246709433626 ) ) ;
#151426 = CIRCLE ( 'NONE', #51410, 7.899999999999990585 ) ;
#151427 = ORIENTED_EDGE ( 'NONE', *, *, #177467, .T. ) ;
#151428 = AXIS2_PLACEMENT_3D ( 'NONE', #122625, #161755, #163034 ) ;
#151429 = AXIS2_PLACEMENT_3D ( 'NONE', #132802, #257801, #2229 ) ;
#151430 = CARTESIAN_POINT ( 'NONE',  ( -20.54999999999999716, 1.925233644870972816, -113.2302435331261563 ) ) ;
#151431 = AXIS2_PLACEMENT_3D ( 'NONE', #79485, #200736, #177358 ) ;
#151432 = EDGE_CURVE ( 'NONE', #150904, #94999, #236736, .T. ) ;
#151433 = DIRECTION ( 'NONE',  ( 1.000000000000000000, 8.034189347746079853E-16, -2.566115377699052699E-16 ) ) ;
#151434 = ORIENTED_EDGE ( 'NONE', *, *, #123567, .T. ) ;
#151435 = CYLINDRICAL_SURFACE ( 'NONE', #122699, 0.09999999999999939493 ) ;
#151436 = EDGE_LOOP ( 'NONE', ( #76203, #231291, #171902, #54804 ) ) ;
#151437 = CARTESIAN_POINT ( 'NONE',  ( -16.94107738177414291, 65.98576071487538286, -115.5731074845243711 ) ) ;
#151438 = ORIENTED_EDGE ( 'NONE', *, *, #213526, .F. ) ;
#151439 = DIRECTION ( 'NONE',  ( 0.000000000000000000, -0.2128009952263403282, 0.9770955615653358350 ) ) ;
#151440 = EDGE_CURVE ( 'NONE', #171475, #191840, #7820, .T. ) ;
#151441 = CARTESIAN_POINT ( 'NONE',  ( -21.05000000000000071, 13.71992543034163958, -238.5823796952984992 ) ) ;
#151442 = CARTESIAN_POINT ( 'NONE',  ( 21.05000000000000426, 76.10000000001167564, -76.00015386631419290 ) ) ;
#151443 = DIRECTION ( 'NONE',  ( 1.000000000000000000, -3.265361837132813093E-16, -2.280189983783949500E-30 ) ) ;
#151444 = EDGE_CURVE ( 'NONE', #188149, #42380, #46784, .T. ) ;
#151445 = VECTOR ( 'NONE', #85592, 1000.000000000000000 ) ;
#151446 = TOROIDAL_SURFACE ( 'NONE', #93154, 0.2000000000000000111, 0.1000000000000000056 ) ;
#151447 = DIRECTION ( 'NONE',  ( 1.000000000000000000, 0.000000000000000000, 0.000000000000000000 ) ) ;
#151448 = CARTESIAN_POINT ( 'NONE',  ( 18.31325810956315436, -9.536388475996043113, -73.86844020630493901 ) ) ;
#151449 = DIRECTION ( 'NONE',  ( 0.000000000000000000, 0.2128009952263403282, -0.9770955615653358350 ) ) ;
#151450 = VECTOR ( 'NONE', #7728, 1000.000000000000000 ) ;
#151451 = ORIENTED_EDGE ( 'NONE', *, *, #78780, .T. ) ;
#151452 = DIRECTION ( 'NONE',  ( 0.000000000000000000, 0.000000000000000000, -1.000000000000000000 ) ) ;
#151453 = VERTEX_POINT ( 'NONE', #25969 ) ;
#151456 = EDGE_LOOP ( 'NONE', ( #25105, #25999, #222404, #81169 ) ) ;
#151455 = CYLINDRICAL_SURFACE ( 'NONE', #250171, 0.1000000000000070832 ) ;
#151454 = DIRECTION ( 'NONE',  ( 0.000000000000000000, 0.000000000000000000, 1.000000000000000000 ) ) ;
#151457 = VERTEX_POINT ( 'NONE', #82039 ) ;
#151458 = CARTESIAN_POINT ( 'NONE',  ( 20.94999999999999929, 76.00000000001143974, -37.92310748452432989 ) ) ;
#151459 = DIRECTION ( 'NONE',  ( 0.000000000000000000, -1.616829647512364004E-14, 1.000000000000000000 ) ) ;
#151460 = CIRCLE ( 'NONE', #68232, 0.09999999999999939493 ) ;
#151461 = CARTESIAN_POINT ( 'NONE',  ( -16.94107738177415712, 60.85118289042637940, -221.1214263997032106 ) ) ;
#151462 = EDGE_CURVE ( 'NONE', #117271, #7443, #24395, .T. ) ;
#151463 = CARTESIAN_POINT ( 'NONE',  ( 20.95576188350343116, 58.98444046482349279, -225.7323267698970426 ) ) ;
#151464 = AXIS2_PLACEMENT_3D ( 'NONE', #176268, #77133, #236207 ) ;
#151465 = EDGE_LOOP ( 'NONE', ( #93719, #172288, #10526, #157209, #217602 ) ) ;
#151467 = ORIENTED_EDGE ( 'NONE', *, *, #158357, .F. ) ;
#151466 = LINE ( 'NONE', #233564, #209383 ) ;
#151468 = EDGE_CURVE ( 'NONE', #233793, #58804, #70200, .T. ) ;
#151469 =( BOUNDED_SURFACE ( )  B_SPLINE_SURFACE ( 3, 2, ( 
 ( #54379, #133913, #193909 ),
 ( #94788, #234294, #36123 ),
 ( #62090, #162486, #3374 ),
 ( #205428, #81606, #26838 ) ),
 .UNSPECIFIED., .F., .F., .F. ) 
 B_SPLINE_SURFACE_WITH_KNOTS ( ( 4, 4 ),
 ( 3, 3 ),
 ( 3.658908243880847788, 4.712388980384689674 ),
 ( 0.000000000000000000, 1.000000000000000000 ),
 .UNSPECIFIED. ) 
 GEOMETRIC_REPRESENTATION_ITEM ( )  RATIONAL_B_SPLINE_SURFACE ( (
 ( 1.000000000000000000, 0.8984936768950536612, 1.000000000000000000),
 ( 1.000000000000000000, 0.8646876308615781825, 1.000000000000000000),
 ( 1.000000000000000000, 0.7953136715913041721, 1.000000000000000000),
 ( 1.000000000000000000, 0.7071067811865475727, 1.000000000000000000) ) ) 
 REPRESENTATION_ITEM ( '' )  SURFACE ( )  );
#151470 = AXIS2_PLACEMENT_3D ( 'NONE', #202009, #61212, #23403 ) ;
#151471 = EDGE_CURVE ( 'NONE', #57915, #237421, #69049, .T. ) ;
#151473 = CARTESIAN_POINT ( 'NONE',  ( -16.90202395485728459, 66.03405545546350197, -190.9261212057837440 ) ) ;
#151472 = DIRECTION ( 'NONE',  ( 0.000000000000000000, 0.000000000000000000, 1.000000000000000000 ) ) ;
#151475 = ORIENTED_EDGE ( 'NONE', *, *, #12650, .T. ) ;
#151474 = LINE ( 'NONE', #36673, #30804 ) ;
#151476 = AXIS2_PLACEMENT_3D ( 'NONE', #65531, #225863, #69413 ) ;
#151477 = AXIS2_PLACEMENT_3D ( 'NONE', #92487, #172071, #14265 ) ;
#151478 = PRODUCT ( 'Injection Molded Chain Links 5', 'Injection Molded Chain Links 5', '', ( #112221 ) ) ;
#151479 = VERTEX_POINT ( 'NONE', #53222 ) ;
#151480 = AXIS2_PLACEMENT_3D ( 'NONE', #154385, #51352, #110073 ) ;
#151481 = DIRECTION ( 'NONE',  ( -1.000000000000000000, 0.000000000000000000, 0.000000000000000000 ) ) ;
#151482 = CARTESIAN_POINT ( 'NONE',  ( 20.95429402530583829, 67.12380584890971136, -94.50002078658648941 ) ) ;
#151483 = VERTEX_POINT ( 'NONE', #230588 ) ;
#151484 = CARTESIAN_POINT ( 'NONE',  ( -18.79999999999999716, -1.885425182446133885, -11.49641995933507843 ) ) ;
#151485 = EDGE_CURVE ( 'NONE', #244339, #47140, #207174, .T. ) ;
#151486 = ORIENTED_EDGE ( 'NONE', *, *, #228041, .F. ) ;
#151487 =( BOUNDED_SURFACE ( )  B_SPLINE_SURFACE ( 3, 2, ( 
 ( #17069, #253075, #156599 ),
 ( #54869, #136988, #117437 ),
 ( #35371, #96558, #99127 ),
 ( #18328, #58713, #178728 ) ),
 .UNSPECIFIED., .F., .F., .F. ) 
 B_SPLINE_SURFACE_WITH_KNOTS ( ( 4, 4 ),
 ( 3, 3 ),
 ( 0.0002700421466196706831, 0.0004789321604330953582 ),
 ( 0.000000000000000000, 1.000000000000000000 ),
 .UNSPECIFIED. ) 
 GEOMETRIC_REPRESENTATION_ITEM ( )  RATIONAL_B_SPLINE_SURFACE ( (
 ( 1.000000000000000000, 0.7071067811865475727, 1.000000000000000000),
 ( 1.000000000000000000, 0.7163411249510942547, 1.000000000000000000),
 ( 1.000000000000000000, 0.7221957104842546826, 1.000000000000000000),
 ( 1.000000000000000000, 0.7250110520819882387, 1.000000000000000000) ) ) 
 REPRESENTATION_ITEM ( '' )  SURFACE ( )  );
#151488 = CARTESIAN_POINT ( 'NONE',  ( -18.40000000000000213, 43.51275691321468742, -233.9088826807484622 ) ) ;
#151489 = CARTESIAN_POINT ( 'NONE',  ( 20.04142135391667168, 34.45224226563739478, -235.0394798453100691 ) ) ;
#151490 = AXIS2_PLACEMENT_3D ( 'NONE', #5044, #84561, #61199 ) ;
#151491 = ORIENTED_EDGE ( 'NONE', *, *, #98256, .T. ) ;
#151492 = CARTESIAN_POINT ( 'NONE',  ( -23.25000000000000000, 26.06832281015329755, -254.4051978787608732 ) ) ;
#151493 = EDGE_CURVE ( 'NONE', #83103, #70449, #51910, .T. ) ;
#151494 = AXIS2_PLACEMENT_3D ( 'NONE', #16827, #257928, #197999 ) ;
#151495 = B_SPLINE_CURVE_WITH_KNOTS ( 'NONE', 3,
 ( #20820, #173512, #252980, #118636, #99019, #16964, #153941, #174787, #139439, #237286 ),
 .UNSPECIFIED., .F., .F.,
 ( 4, 3, 3, 4 ),
 ( 0.000000000000000000, 0.0002000000000008537104, 0.001000000000082977483, 0.001967863649483329782 ),
 .UNSPECIFIED. ) ;
#151496 = ORIENTED_EDGE ( 'NONE', *, *, #147888, .F. ) ;
#151497 = LINE ( 'NONE', #70680, #89606 ) ;
#151498 = CIRCLE ( 'NONE', #43151, 11.65000000000000036 ) ;
#151499 =( BOUNDED_SURFACE ( )  B_SPLINE_SURFACE ( 3, 2, ( 
 ( #90966, #147077, #47984 ),
 ( #226614, #250047, #109238 ),
 ( #127534, #85796, #167978 ),
 ( #71429, #25881, #188783 ) ),
 .UNSPECIFIED., .F., .F., .F. ) 
 B_SPLINE_SURFACE_WITH_KNOTS ( ( 4, 4 ),
 ( 3, 3 ),
 ( 0.0006461284895273780972, 0.0007503702773985890034 ),
 ( 0.000000000000000000, 1.000000000000000000 ),
 .UNSPECIFIED. ) 
 GEOMETRIC_REPRESENTATION_ITEM ( )  RATIONAL_B_SPLINE_SURFACE ( (
 ( 1.000000000000000000, 0.7071067811865475727, 1.000000000000000000),
 ( 1.000000000000000000, 0.7076476444648678310, 1.000000000000000000),
 ( 1.000000000000000000, 0.7075727925192238921, 1.000000000000000000),
 ( 1.000000000000000000, 0.7071067811865475727, 1.000000000000000000) ) ) 
 REPRESENTATION_ITEM ( '' )  SURFACE ( )  );
#151500 = AXIS2_PLACEMENT_3D ( 'NONE', #196059, #73567, #237743 ) ;
#151501 = ORIENTED_EDGE ( 'NONE', *, *, #14646, .F. ) ;
#151502 = CIRCLE ( 'NONE', #205443, 0.1999999999999981515 ) ;
#151503 = ORIENTED_EDGE ( 'NONE', *, *, #233453, .F. ) ;
#151504 = CARTESIAN_POINT ( 'NONE',  ( 20.97107704358301916, 18.86446520529444726, -229.9504956209307238 ) ) ;
#151505 = ORIENTED_EDGE ( 'NONE', *, *, #7808, .T. ) ;
#151506 = DIRECTION ( 'NONE',  ( 0.000000000000000000, 0.000000000000000000, -1.000000000000000000 ) ) ;
#151507 = ORIENTED_EDGE ( 'NONE', *, *, #3743, .F. ) ;
#151509 = ORIENTED_EDGE ( 'NONE', *, *, #171306, .T. ) ;
#151508 = CARTESIAN_POINT ( 'NONE',  ( -0.8999999999999430678, 63.75000000001118394, -10.02310748452479139 ) ) ;
#151510 = ORIENTED_EDGE ( 'NONE', *, *, #178072, .T. ) ;
#151511 = CARTESIAN_POINT ( 'NONE',  ( -21.05000000000000071, 77.16270174995010223, -128.4231074845242802 ) ) ;
#151512 = ORIENTED_EDGE ( 'NONE', *, *, #101970, .F. ) ;
#151515 = ORIENTED_EDGE ( 'NONE', *, *, #60497, .F. ) ;
#151514 = ORIENTED_EDGE ( 'NONE', *, *, #14647, .F. ) ;
#151513 = CARTESIAN_POINT ( 'NONE',  ( -16.93906926870270624, 65.98785312906501588, -56.96965517729757522 ) ) ;
#151516 = DIRECTION ( 'NONE',  ( 0.000000000000000000, -0.9770955615653316162, -0.2128009952263604232 ) ) ;
#151518 = VERTEX_POINT ( 'NONE', #229303 ) ;
#151517 = AXIS2_PLACEMENT_3D ( 'NONE', #206324, #167225, #48522 ) ;
#151519 = AXIS2_PLACEMENT_3D ( 'NONE', #33137, #113909, #16122 ) ;
#151520 = AXIS2_PLACEMENT_3D ( 'NONE', #47530, #166252, #245762 ) ;
#151521 = AXIS2_PLACEMENT_3D ( 'NONE', #224940, #24212, #67173 ) ;
#151522 = ADVANCED_FACE ( 'NONE', ( #92342 ), #103460, .T. ) ;
#151523 = DIRECTION ( 'NONE',  ( 0.7070776581709139474, -0.6909393522474895910, -0.1504792239193035175 ) ) ;
#151524 = EDGE_CURVE ( 'NONE', #102379, #131057, #249246, .T. ) ;
#151525 = ORIENTED_EDGE ( 'NONE', *, *, #130679, .T. ) ;
#151526 = DIRECTION ( 'NONE',  ( 0.000000000000000000, 6.982962677686266711E-15, -1.000000000000000000 ) ) ;
#151528 = ORIENTED_EDGE ( 'NONE', *, *, #139211, .F. ) ;
#151527 = CARTESIAN_POINT ( 'NONE',  ( -23.49999999999994316, 82.84256550613280012, -26.34830530078816935 ) ) ;
#151529 = CARTESIAN_POINT ( 'NONE',  ( -20.94999999999999929, 74.73821383144687047, -94.93660852097883662 ) ) ;
#151530 = EDGE_LOOP ( 'NONE', ( #195725, #141195, #23943 ) ) ;
#151531 = EDGE_CURVE ( 'NONE', #4833, #227798, #41147, .T. ) ;
#151533 = EDGE_CURVE ( 'NONE', #2887, #80661, #11931, .T. ) ;
#151532 = LINE ( 'NONE', #119777, #16341 ) ;
#151534 = CARTESIAN_POINT ( 'NONE',  ( 21.14999999999999858, 2.272311100394802885, -217.9150152700588592 ) ) ;
#151535 = VERTEX_POINT ( 'NONE', #191482 ) ;
#151536 = DIRECTION ( 'NONE',  ( -0.000000000000000000, 0.4088369013363281623, -0.9126074666063771490 ) ) ;
#151537 = PLANE ( 'NONE',  #74325 ) ;
#151538 = EDGE_CURVE ( 'NONE', #43801, #118232, #29839, .T. ) ;
#151539 = ORIENTED_EDGE ( 'NONE', *, *, #133439, .F. ) ;
#151541 = ORIENTED_EDGE ( 'NONE', *, *, #183739, .F. ) ;
#151540 = CARTESIAN_POINT ( 'NONE',  ( 21.05000000000000071, 40.73935534331184272, -238.0635479304912678 ) ) ;
#151543 = EDGE_CURVE ( 'NONE', #144450, #10892, #70253, .T. ) ;
#151542 = CARTESIAN_POINT ( 'NONE',  ( 18.49999999999999645, 74.16465844978745281, -91.46795619196133487 ) ) ;
#151545 = EDGE_CURVE ( 'NONE', #24249, #145638, #169362, .T. ) ;
#151544 = EDGE_CURVE ( 'NONE', #29923, #45647, #182611, .T. ) ;
#151547 = ORIENTED_EDGE ( 'NONE', *, *, #133304, .F. ) ;
#151546 = ORIENTED_EDGE ( 'NONE', *, *, #232804, .F. ) ;
#151548 = CIRCLE ( 'NONE', #218129, 0.09999999999998898659 ) ;
#151549 = ORIENTED_EDGE ( 'NONE', *, *, #201915, .T. ) ;
#151550 = CARTESIAN_POINT ( 'NONE',  ( -18.59999999999999787, 67.23127455305841238, -235.8551265064783991 ) ) ;
#151551 = ORIENTED_EDGE ( 'NONE', *, *, #158963, .T. ) ;
#151552 = ORIENTED_EDGE ( 'NONE', *, *, #95038, .F. ) ;
#151553 = CARTESIAN_POINT ( 'NONE',  ( 20.94999999999999929, 28.27358281186466371, -238.9334100630653381 ) ) ;
#151554 = ORIENTED_EDGE ( 'NONE', *, *, #175832, .F. ) ;
#151555 = CARTESIAN_POINT ( 'NONE',  ( -20.85000000000000142, 76.00000000001213607, -136.5231074845243313 ) ) ;
#151556 = FACE_OUTER_BOUND ( 'NONE', #60840, .T. ) ;
#151557 = ORIENTED_EDGE ( 'NONE', *, *, #204842, .F. ) ;
#151558 = EDGE_CURVE ( 'NONE', #85698, #115079, #95293, .T. ) ;
#151559 = ORIENTED_EDGE ( 'NONE', *, *, #63669, .F. ) ;
#151560 = CARTESIAN_POINT ( 'NONE',  ( -18.59999999999999787, 11.75000000001115197, -74.01480577065404987 ) ) ;
#151561 = EDGE_CURVE ( 'NONE', #192659, #214669, #128613, .T. ) ;
#151563 = ADVANCED_FACE ( 'NONE', ( #27280 ), #246294, .F. ) ;
#151562 = CIRCLE ( 'NONE', #18629, 0.1000000000000028644 ) ;
#151564 = ORIENTED_EDGE ( 'NONE', *, *, #243291, .F. ) ;
#151565 = AXIS2_PLACEMENT_3D ( 'NONE', #89790, #126363, #211043 ) ;
#151566 = CIRCLE ( 'NONE', #68343, 1.749999999999999778 ) ;
#151567 = EDGE_CURVE ( 'NONE', #253683, #214758, #215437, .T. ) ;
#151568 = CARTESIAN_POINT ( 'NONE',  ( 18.49999999999998934, 69.45000000001181206, -81.87310748452435405 ) ) ;
#151569 = VERTEX_POINT ( 'NONE', #114477 ) ;
#151570 = CARTESIAN_POINT ( 'NONE',  ( -20.85000000000000142, 36.48445852813179613, -249.2750065094666923 ) ) ;
#151572 = ORIENTED_EDGE ( 'NONE', *, *, #219243, .F. ) ;
#151571 = CARTESIAN_POINT ( 'NONE',  ( 18.51565452909435905, 85.35285933884642873, -162.8281981632931377 ) ) ;
#151573 = CARTESIAN_POINT ( 'NONE',  ( -20.94999999999999929, 76.00000000001213607, -136.5231074845243313 ) ) ;
#151574 = DIRECTION ( 'NONE',  ( 0.000000000000000000, -0.9654727137038715545, 0.2605042016806676242 ) ) ;
#151575 = EDGE_CURVE ( 'NONE', #125531, #153341, #211825, .T. ) ;
#151576 = DIRECTION ( 'NONE',  ( 0.000000000000000000, -1.000000000000000000, 0.000000000000000000 ) ) ;
#151577 = DIRECTION ( 'NONE',  ( 1.000000000000000000, 0.000000000000000000, -0.000000000000000000 ) ) ;
#151578 = CARTESIAN_POINT ( 'NONE',  ( -21.07928932188134041, 6.328516656404449492, -133.9011048543456184 ) ) ;
#151579 = CARTESIAN_POINT ( 'NONE',  ( 23.14999999999999503, 11.65000000000000746, 11.75000000000000000 ) ) ;
#151580 = DIRECTION ( 'NONE',  ( 0.000000000000000000, -0.8814952561688476074, 0.4721928772777262417 ) ) ;
#151581 = CYLINDRICAL_SURFACE ( 'NONE', #186592, 0.09999999999999939493 ) ;
#151582 = CARTESIAN_POINT ( 'NONE',  ( 18.43630871534904969, 37.95950696621422793, -261.2289642737110853 ) ) ;
#151583 = AXIS2_PLACEMENT_3D ( 'NONE', #83995, #123183, #145292 ) ;
#151584 = DIRECTION ( 'NONE',  ( 0.000000000000000000, 0.9126074666063844765, 0.4088369013363113980 ) ) ;
#151585 = AXIS2_PLACEMENT_3D ( 'NONE', #30221, #52316, #152759 ) ;
#151586 = ORIENTED_EDGE ( 'NONE', *, *, #99036, .F. ) ;
#151587 = AXIS2_PLACEMENT_3D ( 'NONE', #201774, #162669, #242185 ) ;
#151588 = AXIS2_PLACEMENT_3D ( 'NONE', #18061, #96302, #132894 ) ;
#151590 = ORIENTED_EDGE ( 'NONE', *, *, #41055, .F. ) ;
#151589 = ORIENTED_EDGE ( 'NONE', *, *, #151524, .F. ) ;
#151591 = ORIENTED_EDGE ( 'NONE', *, *, #96784, .F. ) ;
#151592 = DIRECTION ( 'NONE',  ( 0.000000000000000000, 6.982962677686266711E-15, -1.000000000000000000 ) ) ;
#151593 = CARTESIAN_POINT ( 'NONE',  ( 21.14999999999999858, 59.16775194334852017, -221.0793150863668473 ) ) ;
#151595 = CARTESIAN_POINT ( 'NONE',  ( 23.14999999999999503, 11.65000000001116298, -88.75000000000004263 ) ) ;
#151594 = CARTESIAN_POINT ( 'NONE',  ( 25.10847955711010115, 9.068702471349586958, -347.0000000000001137 ) ) ;
#151596 = ORIENTED_EDGE ( 'NONE', *, *, #222296, .T. ) ;
#151597 = ORIENTED_EDGE ( 'NONE', *, *, #104944, .F. ) ;
#151598 = CIRCLE ( 'NONE', #30788, 0.1000000000000072220 ) ;
#151599 = VECTOR ( 'NONE', #105939, 1000.000000000000000 ) ;
#151600 = DIRECTION ( 'NONE',  ( 1.000000000000000000, -7.304098846218135653E-16, -5.100424963727256530E-30 ) ) ;
#151601 = CARTESIAN_POINT ( 'NONE',  ( 18.51024323315077069, 10.31104185824064068, -173.0204516983106089 ) ) ;
#151602 = DIRECTION ( 'NONE',  ( -1.000000000000000000, -0.000000000000000000, -0.000000000000000000 ) ) ;
#151604 = ORIENTED_EDGE ( 'NONE', *, *, #131507, .T. ) ;
#151603 = AXIS2_PLACEMENT_3D ( 'NONE', #121643, #64215, #83733 ) ;
#151605 = EDGE_LOOP ( 'NONE', ( #28848, #56586, #23117, #79337, #45114, #139392, #35016, #59892, #100360, #80941, #231396 ) ) ;
#151606 = DIRECTION ( 'NONE',  ( 0.000000000000000000, -1.000000000000000000, -6.982962677686265922E-15 ) ) ;
#151607 = FACE_OUTER_BOUND ( 'NONE', #217142, .T. ) ;
#151608 = CARTESIAN_POINT ( 'NONE',  ( 21.05000000000000071, 8.592460621936744758, -209.2032282544143698 ) ) ;
#151610 = ORIENTED_EDGE ( 'NONE', *, *, #160958, .F. ) ;
#151609 = CARTESIAN_POINT ( 'NONE',  ( 20.99999999999999645, 9.750000000011137757, -143.2500000000000284 ) ) ;
#151611 = CARTESIAN_POINT ( 'NONE',  ( -18.59999999999999787, 77.36242903720497566, -61.63422623660309796 ) ) ;
#151612 = DIRECTION ( 'NONE',  ( 0.000000000000000000, -0.9999631594459053030, -0.008583690987162452199 ) ) ;
#151613 = AXIS2_PLACEMENT_3D ( 'NONE', #144707, #40534, #239987 ) ;
#151614 = DIRECTION ( 'NONE',  ( 0.000000000000000000, 0.000000000000000000, 1.000000000000000000 ) ) ;
#151615 = CARTESIAN_POINT ( 'NONE',  ( -20.85000000000000142, 43.24695311518262031, -245.0026972281755491 ) ) ;
#151617 = ORIENTED_EDGE ( 'NONE', *, *, #250035, .F. ) ;
#151616 = VECTOR ( 'NONE', #50993, 1000.000000000000000 ) ;
#151618 = FACE_OUTER_BOUND ( 'NONE', #238723, .T. ) ;
#151619 = CARTESIAN_POINT ( 'NONE',  ( -23.15000000000000213, 4.662003332185090443, -213.0075696128765514 ) ) ;
#151620 = AXIS2_PLACEMENT_3D ( 'NONE', #79173, #55740, #36243 ) ;
#151621 = ADVANCED_FACE ( 'NONE', ( #81412 ), #63152, .T. ) ;
#151623 = LINE ( 'NONE', #48627, #103833 ) ;
#151622 = CARTESIAN_POINT ( 'NONE',  ( 18.59999999999997655, 11.75000000001115552, -167.5000000000000284 ) ) ;
#151624 = DIRECTION ( 'NONE',  ( 5.603264701231743991E-32, -0.2128009952263605620, 0.9770955615653313941 ) ) ;
#151625 = CARTESIAN_POINT ( 'NONE',  ( -16.77308656112214535, 9.950000000011137047, -54.34980680829769994 ) ) ;
#151626 = DIRECTION ( 'NONE',  ( 0.000000000000000000, 0.000000000000000000, -1.000000000000000000 ) ) ;
#151628 = EDGE_CURVE ( 'NONE', #137151, #224437, #134030, .T. ) ;
#151627 = DIRECTION ( 'NONE',  ( -1.000000000000000000, -2.952720810173289112E-16, 0.000000000000000000 ) ) ;
#151629 = DIRECTION ( 'NONE',  ( 1.000000000000000000, 0.000000000000000000, 0.000000000000000000 ) ) ;
#151630 = ORIENTED_EDGE ( 'NONE', *, *, #146215, .F. ) ;
#151631 = ORIENTED_EDGE ( 'NONE', *, *, #254001, .F. ) ;
#151632 = VERTEX_POINT ( 'NONE', #34985 ) ;
#151633 = EDGE_CURVE ( 'NONE', #94400, #163287, #176581, .T. ) ;
#151634 = LINE ( 'NONE', #132038, #52778 ) ;
#151635 = EDGE_CURVE ( 'NONE', #91128, #56702, #181835, .T. ) ;
#151636 = FACE_OUTER_BOUND ( 'NONE', #245798, .T. ) ;
#151637 = ORIENTED_EDGE ( 'NONE', *, *, #170446, .F. ) ;
#151638 = VERTEX_POINT ( 'NONE', #61889 ) ;
#151639 = VECTOR ( 'NONE', #139518, 1000.000000000000000 ) ;
#151640 = SURFACE_STYLE_FILL_AREA ( #212876 ) ;
#151641 = CONICAL_SURFACE ( 'NONE', #168219, 4.049999999999987388, 0.7853981633974604915 ) ;
#151642 = EDGE_LOOP ( 'NONE', ( #173159, #36803, #130790, #195461 ) ) ;
#151643 = AXIS2_PLACEMENT_3D ( 'NONE', #199192, #143040, #242154 ) ;
#151644 = FACE_OUTER_BOUND ( 'NONE', #222893, .T. ) ;
#151645 = ORIENTED_EDGE ( 'NONE', *, *, #148362, .F. ) ;
#151646 = ADVANCED_FACE ( 'NONE', ( #141414 ), #220941, .T. ) ;
#151647 = DIRECTION ( 'NONE',  ( 0.000000000000000000, -0.9651348961777157509, 0.2617529984165031243 ) ) ;
#151648 = EDGE_CURVE ( 'NONE', #112914, #158507, #138809, .T. ) ;
#151649 = DIRECTION ( 'NONE',  ( 0.000000000000000000, -0.9770955615653315052, -0.2128009952263603954 ) ) ;
#151650 = DIRECTION ( 'NONE',  ( -1.000000000000000000, -0.000000000000000000, -0.000000000000000000 ) ) ;
#151651 = CIRCLE ( 'NONE', #222509, 0.1000000000000028644 ) ;
#151652 = AXIS2_PLACEMENT_3D ( 'NONE', #181091, #175965, #36458 ) ;
#151653 = LINE ( 'NONE', #13405, #162511 ) ;
#151654 = CARTESIAN_POINT ( 'NONE',  ( 22.84999999999999787, 0.000000000000000000, 4.000000000000000000 ) ) ;
#151656 = ORIENTED_EDGE ( 'NONE', *, *, #201426, .T. ) ;
#151655 = CARTESIAN_POINT ( 'NONE',  ( -16.87333278164169670, 29.74859725134929889, -234.6383007634102000 ) ) ;
#151657 = CARTESIAN_POINT ( 'NONE',  ( 20.04142135623730070, 61.57587952878035509, -212.2000740415318774 ) ) ;
#151658 = CARTESIAN_POINT ( 'NONE',  ( -20.94999999999999929, 87.29603075034795268, -200.4752083248604038 ) ) ;
#151659 = CARTESIAN_POINT ( 'NONE',  ( 20.99999999999999645, 9.750000000011137757, -121.3500000000000227 ) ) ;
#151660 = AXIS2_PLACEMENT_3D ( 'NONE', #123446, #238248, #63456 ) ;
#151661 = CARTESIAN_POINT ( 'NONE',  ( 23.15000000000000213, -4.914013037343258894, -233.1828366659746905 ) ) ;
#151662 = DIRECTION ( 'NONE',  ( -0.000000000000000000, 6.982962677686266711E-15, -1.000000000000000000 ) ) ;
#151663 = ORIENTED_EDGE ( 'NONE', *, *, #117769, .F. ) ;
#151664 = AXIS2_PLACEMENT_3D ( 'NONE', #152223, #230446, #195197 ) ;
#151665 =( NAMED_UNIT ( * ) PLANE_ANGLE_UNIT ( ) SI_UNIT ( $, .RADIAN. ) );
#151666 = DIRECTION ( 'NONE',  ( 0.000000000000000000, -1.000000000000000000, 0.000000000000000000 ) ) ;
#151667 = CIRCLE ( 'NONE', #39237, 0.1000000000000052097 ) ;
#151668 = EDGE_CURVE ( 'NONE', #35121, #45034, #103634, .T. ) ;
#151669 = CIRCLE ( 'NONE', #39238, 0.09999999999999907574 ) ;
#151670 = CARTESIAN_POINT ( 'NONE',  ( 23.24999999999999289, 71.85000000001237197, -170.0231074845243882 ) ) ;
#151671 = EDGE_CURVE ( 'NONE', #230269, #47244, #136984, .T. ) ;
#151672 = ORIENTED_EDGE ( 'NONE', *, *, #145646, .F. ) ;
#151673 = AXIS2_PLACEMENT_3D ( 'NONE', #86984, #204382, #88267 ) ;
#151674 = CARTESIAN_POINT ( 'NONE',  ( -18.59999999999999787, -11.65000000000000036, 5.900000000000001243 ) ) ;
#151675 = CARTESIAN_POINT ( 'NONE',  ( 20.94999999999999574, 79.13126459505528487, -235.8705213229730191 ) ) ;
#151676 = CYLINDRICAL_SURFACE ( 'NONE', #11793, 0.1000000000000124678 ) ;
#151677 = ORIENTED_EDGE ( 'NONE', *, *, #25541, .F. ) ;
#151678 = TOROIDAL_SURFACE ( 'NONE', #147554, 0.2000000000000000111, 0.1000000000000000056 ) ;
#151679 = VERTEX_POINT ( 'NONE', #219660 ) ;
#151680 = EDGE_CURVE ( 'NONE', #19733, #99784, #41065, .T. ) ;
#151681 = EDGE_CURVE ( 'NONE', #150529, #132306, #191172, .T. ) ;
#151682 = CARTESIAN_POINT ( 'NONE',  ( -21.05000000000000071, 14.64166534854604507, -236.4381089660238331 ) ) ;
#151684 = VECTOR ( 'NONE', #171756, 1000.000000000000000 ) ;
#151683 = CARTESIAN_POINT ( 'NONE',  ( -22.39999999999999858, 1.115600667400684642E-11, -155.8504291924551808 ) ) ;
#151685 = CYLINDRICAL_SURFACE ( 'NONE', #41088, 0.09999999999999939493 ) ;
#151686 = CARTESIAN_POINT ( 'NONE',  ( -21.55000000000000071, 7.349999999999998757, -12.25000000000000000 ) ) ;
#151687 = DIRECTION ( 'NONE',  ( -3.265361837132812600E-16, -0.4088369013363282178, 0.9126074666063768159 ) ) ;
#151688 = ADVANCED_FACE ( 'NONE', ( #93631 ), #74105, .T. ) ;
#151689 = CARTESIAN_POINT ( 'NONE',  ( 20.94999999999999929, 76.00000000001237765, -170.0231074845243597 ) ) ;
#151690 = DIRECTION ( 'NONE',  ( 1.000000000000000000, -0.000000000000000000, -0.000000000000000000 ) ) ;
#151691 = DIRECTION ( 'NONE',  ( 0.000000000000000000, 6.938893903907222067E-15, -1.000000000000000000 ) ) ;
#151692 = TOROIDAL_SURFACE ( 'NONE', #26781, 11.70000000000000107, 0.1000000000000000056 ) ;
#151693 = EDGE_LOOP ( 'NONE', ( #218281, #112575, #18367, #6014 ) ) ;
#151694 = CARTESIAN_POINT ( 'NONE',  ( 18.39999999999999503, 70.35000000001255671, -182.6731074845243938 ) ) ;
#151696 = ORIENTED_EDGE ( 'NONE', *, *, #90867, .T. ) ;
#151695 = DIRECTION ( 'NONE',  ( 1.000000000000000000, -0.000000000000000000, 0.000000000000000000 ) ) ;
#151697 = VECTOR ( 'NONE', #198809, 1000.000000000000227 ) ;
#151698 = CARTESIAN_POINT ( 'NONE',  ( 21.07094088545303734, 69.67983277809588571, -170.1220011870766200 ) ) ;
#151699 = CARTESIAN_POINT ( 'NONE',  ( 18.50000000000000000, 85.50000000001209344, -129.9229180933022576 ) ) ;
#151700 = DIRECTION ( 'NONE',  ( 2.952720810173290098E-16, -0.4721928772777322370, -0.8814952561688442767 ) ) ;
#151701 = FACE_OUTER_BOUND ( 'NONE', #16044, .T. ) ;
#151702 = CARTESIAN_POINT ( 'NONE',  ( 21.05000000000000071, 71.00000000001180922, -81.92837350343744163 ) ) ;
#151704 = EDGE_LOOP ( 'NONE', ( #250983, #236153, #15186, #123129 ) ) ;
#151703 = DIRECTION ( 'NONE',  ( -1.000000000000000000, 0.000000000000000000, 0.000000000000000000 ) ) ;
#151705 = DIRECTION ( 'NONE',  ( 1.000000000000000000, -3.265361837132813093E-16, -2.280189983783949500E-30 ) ) ;
#151706 = FACE_OUTER_BOUND ( 'NONE', #208177, .T. ) ;
#151707 = EDGE_CURVE ( 'NONE', #96655, #5597, #123150, .T. ) ;
#151708 = CARTESIAN_POINT ( 'NONE',  ( 22.48660254037843842, 11.65000000001115588, -66.95000000000003126 ) ) ;
#151709 = DIRECTION ( 'NONE',  ( 2.952720810173289112E-16, -1.000000000000000000, 0.000000000000000000 ) ) ;
#151710 = ORIENTED_EDGE ( 'NONE', *, *, #159900, .T. ) ;
#151711 = DIRECTION ( 'NONE',  ( 0.000000000000000000, 0.000000000000000000, 1.000000000000000000 ) ) ;
#151712 = ORIENTED_EDGE ( 'NONE', *, *, #64661, .F. ) ;
#151713 = EDGE_CURVE ( 'NONE', #36696, #40232, #24065, .T. ) ;
#151714 = CARTESIAN_POINT ( 'NONE',  ( 22.59999999999999432, 75.89914163091404475, -215.2726746080137445 ) ) ;
#151716 = ORIENTED_EDGE ( 'NONE', *, *, #160659, .T. ) ;
#151715 = AXIS2_PLACEMENT_3D ( 'NONE', #165587, #228123, #109428 ) ;
#151717 = CARTESIAN_POINT ( 'NONE',  ( -21.14999999999994174, 87.50449464844290048, -34.18759587077607165 ) ) ;
#151718 = CIRCLE ( 'NONE', #18398, 3.899999999999987477 ) ;
#151719 = AXIS2_PLACEMENT_3D ( 'NONE', #167285, #49865, #88979 ) ;
#151720 = ORIENTED_EDGE ( 'NONE', *, *, #190993, .T. ) ;
#151721 = DIRECTION ( 'NONE',  ( 1.000000000000000000, 0.000000000000000000, 0.000000000000000000 ) ) ;
#151722 = CYLINDRICAL_SURFACE ( 'NONE', #129242, 0.5000000000000004441 ) ;
#151723 = DIRECTION ( 'NONE',  ( 0.000000000000000000, -1.000000000000000000, -6.982962677686265922E-15 ) ) ;
#151724 = ORIENTED_EDGE ( 'NONE', *, *, #216243, .F. ) ;
#151725 = CARTESIAN_POINT ( 'NONE',  ( -16.79270642812305070, 9.946244216938156413, -12.66106672143717660 ) ) ;
#151726 = DIRECTION ( 'NONE',  ( 1.000000000000000000, 0.000000000000000000, 0.000000000000000000 ) ) ;
#151727 = CARTESIAN_POINT ( 'NONE',  ( -23.25000000000000000, 11.75000000001115552, -200.9999999999999432 ) ) ;
#151728 = CARTESIAN_POINT ( 'NONE',  ( 18.59999999999999787, -1.835341550213255957, -78.55515129256302487 ) ) ;
#151729 = CARTESIAN_POINT ( 'NONE',  ( -16.94333152882356330, 66.00965798855433775, -115.6310759534228794 ) ) ;
#151730 = VERTEX_POINT ( 'NONE', #248231 ) ;
#151731 = DIRECTION ( 'NONE',  ( 0.000000000000000000, -0.2128009952263734406, 0.9770955615653287296 ) ) ;
#151732 = ORIENTED_EDGE ( 'NONE', *, *, #107405, .T. ) ;
#151734 = ORIENTED_EDGE ( 'NONE', *, *, #144634, .F. ) ;
#151733 = DIRECTION ( 'NONE',  ( -0.7071067811865214825, -0.7071067811865735520, 0.000000000000000000 ) ) ;
#151735 = ORIENTED_EDGE ( 'NONE', *, *, #151762, .T. ) ;
#151736 = AXIS2_PLACEMENT_3D ( 'NONE', #194093, #75438, #154972 ) ;
#151737 = CARTESIAN_POINT ( 'NONE',  ( 21.00000000000000000, 9.750000000011153745, -88.15000000000004832 ) ) ;
#151738 = CARTESIAN_POINT ( 'NONE',  ( 21.05000000000000071, 62.33780030268294325, -247.9091949332902516 ) ) ;
#151739 = DIRECTION ( 'NONE',  ( -0.000000000000000000, 0.000000000000000000, 1.000000000000000000 ) ) ;
#151740 = CARTESIAN_POINT ( 'NONE',  ( -20.64999999999999858, 78.17003882911672008, -228.8770135013149911 ) ) ;
#151741 = ORIENTED_EDGE ( 'NONE', *, *, #166078, .T. ) ;
#151742 = CARTESIAN_POINT ( 'NONE',  ( -18.59999999999999787, 18.18127959618848166, -237.5711165786817389 ) ) ;
#151743 = DIRECTION ( 'NONE',  ( 1.000000000000000000, 7.304098846218134667E-16, -0.000000000000000000 ) ) ;
#151744 = ORIENTED_EDGE ( 'NONE', *, *, #226859, .T. ) ;
#151746 = VERTEX_POINT ( 'NONE', #224792 ) ;
#151745 = CARTESIAN_POINT ( 'NONE',  ( 21.05000000000000071, 76.00000000001213607, -136.5231074845242745 ) ) ;
#151747 = DIRECTION ( 'NONE',  ( -1.000000000000000000, 0.000000000000000000, -0.000000000000000000 ) ) ;
#151748 = CARTESIAN_POINT ( 'NONE',  ( -21.05000000000000071, -11.48912529306490349, -70.10000000000005116 ) ) ;
#151749 = AXIS2_PLACEMENT_3D ( 'NONE', #238387, #233286, #58443 ) ;
#151750 = AXIS2_PLACEMENT_3D ( 'NONE', #257805, #197878, #4790 ) ;
#151751 = ORIENTED_EDGE ( 'NONE', *, *, #52184, .F. ) ;
#151752 = CIRCLE ( 'NONE', #93437, 0.09999999999999939493 ) ;
#151754 = CARTESIAN_POINT ( 'NONE',  ( -17.11825945287481332, 9.950000000011138823, -87.75000000000005684 ) ) ;
#151753 = CIRCLE ( 'NONE', #1845, 0.09999999999998898659 ) ;
#151755 = DIRECTION ( 'NONE',  ( 0.000000000000000000, 0.000000000000000000, 1.000000000000000000 ) ) ;
#151756 = ORIENTED_EDGE ( 'NONE', *, *, #190258, .T. ) ;
#151757 = FACE_OUTER_BOUND ( 'NONE', #141491, .T. ) ;
#151758 = EDGE_CURVE ( 'NONE', #70684, #191326, #64461, .T. ) ;
#151759 = CARTESIAN_POINT ( 'NONE',  ( 21.05000000000000071, 64.25000000001249134, -177.0379132551784096 ) ) ;
#151760 = CARTESIAN_POINT ( 'NONE',  ( 21.14999999999999858, 64.35000000001156195, -57.37310748452439668 ) ) ;
#151761 = EDGE_CURVE ( 'NONE', #160189, #155916, #249429, .T. ) ;
#151762 = EDGE_CURVE ( 'NONE', #239696, #113692, #239910, .T. ) ;
#151763 = AXIS2_PLACEMENT_3D ( 'NONE', #156395, #53408, #71709 ) ;
#151764 = EDGE_LOOP ( 'NONE', ( #37971, #40896, #158676, #174199 ) ) ;
#151765 = DIRECTION ( 'NONE',  ( 1.000000000000000000, 2.952720810173289112E-16, -0.000000000000000000 ) ) ;
#151766 = CIRCLE ( 'NONE', #89187, 0.1000000000000055844 ) ;
#151767 = VECTOR ( 'NONE', #6711, 999.9999999999998863 ) ;
#151768 = ORIENTED_EDGE ( 'NONE', *, *, #61404, .T. ) ;
#151769 = DIRECTION ( 'NONE',  ( 0.000000000000000000, 0.000000000000000000, -1.000000000000000000 ) ) ;
#151770 = ADVANCED_FACE ( 'NONE', ( #166160 ), #124437, .T. ) ;
#151771 = DIRECTION ( 'NONE',  ( 0.000000000000000000, 0.000000000000000000, -1.000000000000000000 ) ) ;
#151773 = VERTEX_POINT ( 'NONE', #222213 ) ;
#151772 = CARTESIAN_POINT ( 'NONE',  ( 13.43443725621852636, 24.89114276590144570, -232.5309687781012826 ) ) ;
#151774 = CYLINDRICAL_SURFACE ( 'NONE', #140905, 0.09999999999998898659 ) ;
#151775 = DIRECTION ( 'NONE',  ( -1.000000000000000000, -0.000000000000000000, -0.000000000000000000 ) ) ;
#151776 = CARTESIAN_POINT ( 'NONE',  ( 20.94999999999999929, 70.10000000001197407, -113.2422072491807086 ) ) ;
#151777 = CARTESIAN_POINT ( 'NONE',  ( -16.87383368123029825, 22.97806745954241947, -230.9350634111226270 ) ) ;
#151778 = DIRECTION ( 'NONE',  ( 1.000000000000000000, -3.265361837132813093E-16, -2.280189983783949500E-30 ) ) ;
#151779 = CIRCLE ( 'NONE', #247607, 0.09999999999999939493 ) ;
#151780 = FACE_OUTER_BOUND ( 'NONE', #85792, .T. ) ;
#151781 = CIRCLE ( 'NONE', #243324, 0.09999999999999939493 ) ;
#151782 = DIRECTION ( 'NONE',  ( 2.827886303505248273E-16, 0.03181660087583042251, -0.9994937237965568766 ) ) ;
#151784 = ORIENTED_EDGE ( 'NONE', *, *, #106095, .F. ) ;
#151783 = CARTESIAN_POINT ( 'NONE',  ( -22.44366136229477249, 75.99065843052596847, -114.6728260419982206 ) ) ;
#151785 = VECTOR ( 'NONE', #3219, 1000.000000000000114 ) ;
#151786 = CARTESIAN_POINT ( 'NONE',  ( -20.94999999999999929, 87.65000000001235492, -166.9231074845242802 ) ) ;
#151787 = AXIS2_PLACEMENT_3D ( 'NONE', #114264, #116832, #257887 ) ;
#151788 = DIRECTION ( 'NONE',  ( 0.000000000000000000, 0.000000000000000000, 1.000000000000000000 ) ) ;
#151789 = ADVANCED_FACE ( 'NONE', ( #9608 ), #183130, .T. ) ;
#151790 = EDGE_CURVE ( 'NONE', #54821, #140474, #236941, .T. ) ;
#151791 = CARTESIAN_POINT ( 'NONE',  ( -18.59999994787167310, 85.52363768977346581, -62.64065794975200419 ) ) ;
#151792 = LINE ( 'NONE', #248296, #26459 ) ;
#151793 = VECTOR ( 'NONE', #195425, 1000.000000000000000 ) ;
#151794 = EDGE_LOOP ( 'NONE', ( #252482, #13279, #239061, #193074 ) ) ;
#151795 = AXIS2_PLACEMENT_3D ( 'NONE', #210415, #246941, #172607 ) ;
#151796 = DIRECTION ( 'NONE',  ( 0.000000000000000000, -0.000000000000000000, -1.000000000000000000 ) ) ;
#151798 = EDGE_CURVE ( 'NONE', #97691, #90665, #244359, .T. ) ;
#151797 = CYLINDRICAL_SURFACE ( 'NONE', #24228, 0.09999999999999881206 ) ;
#151799 = ORIENTED_EDGE ( 'NONE', *, *, #94090, .T. ) ;
#151800 = CARTESIAN_POINT ( 'NONE',  ( 23.15000000000000213, 85.00000000001197975, -112.9170766071766820 ) ) ;
#151801 = FACE_OUTER_BOUND ( 'NONE', #197058, .T. ) ;
#151802 = ORIENTED_EDGE ( 'NONE', *, *, #8624, .T. ) ;
#151803 = CARTESIAN_POINT ( 'NONE',  ( -16.91256925476570672, 66.01426884188333588, -48.55546499551912376 ) ) ;
#151804 = VERTEX_POINT ( 'NONE', #48731 ) ;
#151805 = DIRECTION ( 'NONE',  ( 1.875376730785737719E-16, -1.000000000000000000, 0.000000000000000000 ) ) ;
#151807 = ORIENTED_EDGE ( 'NONE', *, *, #229619, .F. ) ;
#151806 = DIRECTION ( 'NONE',  ( 0.000000000000000000, -0.8660254037844420383, 0.4999999999999943379 ) ) ;
#151808 = CARTESIAN_POINT ( 'NONE',  ( 0.8999999999999993561, -8.350000000000004974, 26.00000000000000355 ) ) ;
#151809 = EDGE_CURVE ( 'NONE', #74968, #232547, #87074, .T. ) ;
#151810 = VERTEX_POINT ( 'NONE', #185690 ) ;
#151811 = AXIS2_PLACEMENT_3D ( 'NONE', #122553, #27331, #24752 ) ;
#151812 = LINE ( 'NONE', #8432, #55386 ) ;
#151813 = EDGE_LOOP ( 'NONE', ( #65842, #67810, #72912, #114663 ) ) ;
#151814 = AXIS2_PLACEMENT_3D ( 'NONE', #2621, #60023, #219097 ) ;
#151816 = ORIENTED_EDGE ( 'NONE', *, *, #250161, .F. ) ;
#151815 = ORIENTED_EDGE ( 'NONE', *, *, #158772, .F. ) ;
#151817 = FACE_OUTER_BOUND ( 'NONE', #255879, .T. ) ;
#151819 = VERTEX_POINT ( 'NONE', #245659 ) ;
#151818 = CARTESIAN_POINT ( 'NONE',  ( 21.05933563467872105, 10.72452471209247626, -146.1936477489559536 ) ) ;
#151820 = TOROIDAL_SURFACE ( 'NONE', #52003, 0.2000000000000000111, 0.1000000000000000056 ) ;
#151821 = CARTESIAN_POINT ( 'NONE',  ( 18.79999999999999716, 11.49641995933507843, -1.885425182446133885 ) ) ;
#151822 = ORIENTED_EDGE ( 'NONE', *, *, #240275, .T. ) ;
#151823 = AXIS2_PLACEMENT_3D ( 'NONE', #94353, #213026, #154384 ) ;
#151824 = EDGE_CURVE ( 'NONE', #188417, #49823, #149664, .T. ) ;
#151825 = AXIS2_PLACEMENT_3D ( 'NONE', #253864, #175643, #156099 ) ;
#151826 = ORIENTED_EDGE ( 'NONE', *, *, #107280, .F. ) ;
#151827 = CARTESIAN_POINT ( 'NONE',  ( 18.49999999999999289, 11.65000000001115943, -122.2500000000000284 ) ) ;
#151828 = CARTESIAN_POINT ( 'NONE',  ( 20.94999999999999929, 72.02722222756959525, -225.1832529173024398 ) ) ;
#151829 = CARTESIAN_POINT ( 'NONE',  ( 21.87500000000000355, 66.25000000001185185, -90.67310748452437963 ) ) ;
#151830 = ORIENTED_EDGE ( 'NONE', *, *, #108358, .F. ) ;
#151831 = AXIS2_PLACEMENT_3D ( 'NONE', #129565, #112574, #16061 ) ;
#151832 = EDGE_CURVE ( 'NONE', #219433, #140980, #249147, .T. ) ;
#151834 = EDGE_CURVE ( 'NONE', #47890, #187756, #232864, .T. ) ;
#151833 = CARTESIAN_POINT ( 'NONE',  ( -21.06715728752538652, 64.25000000001209344, -129.5083017138703667 ) ) ;
#151835 = CARTESIAN_POINT ( 'NONE',  ( -20.64999999999999858, 71.65000000001155911, -57.27310748452435263 ) ) ;
#151836 = CIRCLE ( 'NONE', #172708, 4.000000000000000000 ) ;
#151837 = ORIENTED_EDGE ( 'NONE', *, *, #68076, .F. ) ;
#151838 = DIRECTION ( 'NONE',  ( 0.000000000000000000, -1.000000000000000000, 0.000000000000000000 ) ) ;
#151839 = AXIS2_PLACEMENT_3D ( 'NONE', #60282, #158160, #198521 ) ;
#151840 = DIRECTION ( 'NONE',  ( -0.000000000000000000, 6.982962677686266711E-15, -1.000000000000000000 ) ) ;
#151841 = FILL_AREA_STYLE ('',( #172713 ) ) ;
#151842 = ORIENTED_EDGE ( 'NONE', *, *, #117975, .T. ) ;
#151843 = CARTESIAN_POINT ( 'NONE',  ( 22.50046968638275757, 0.04516984714972999138, -55.24995484552670888 ) ) ;
#151844 = ORIENTED_EDGE ( 'NONE', *, *, #224122, .F. ) ;
#151845 = CARTESIAN_POINT ( 'NONE',  ( -18.51555513499438987, -7.607300382162530461, -210.0206232990065587 ) ) ;
#151846 = ORIENTED_EDGE ( 'NONE', *, *, #34323, .T. ) ;
#151847 = ADVANCED_FACE ( 'NONE', ( #94280 ), #166237, .F. ) ;
#151848 = EDGE_CURVE ( 'NONE', #220627, #116826, #250789, .T. ) ;
#151849 = CYLINDRICAL_SURFACE ( 'NONE', #59629, 0.09999999999999939493 ) ;
#151850 = DIRECTION ( 'NONE',  ( 0.000000000000000000, 0.000000000000000000, 1.000000000000000000 ) ) ;
#151851 = EDGE_LOOP ( 'NONE', ( #183456, #148523, #4592, #105880 ) ) ;
#151852 = ORIENTED_EDGE ( 'NONE', *, *, #182096, .T. ) ;
#151853 = DIRECTION ( 'NONE',  ( 1.186688945009009831E-16, -1.000000000000000000, 0.000000000000000000 ) ) ;
#151854 = DIRECTION ( 'NONE',  ( 0.000000000000000000, -6.982962677686266711E-15, 1.000000000000000000 ) ) ;
#151855 = ORIENTED_EDGE ( 'NONE', *, *, #63382, .F. ) ;
#151857 = ADVANCED_FACE ( 'NONE', ( #129571 ), #193410, .F. ) ;
#151856 = AXIS2_PLACEMENT_3D ( 'NONE', #2836, #220628, #42006 ) ;
#151858 = ORIENTED_EDGE ( 'NONE', *, *, #77773, .T. ) ;
#151859 = CYLINDRICAL_SURFACE ( 'NONE', #22960, 0.1000000000000098310 ) ;
#151860 = CARTESIAN_POINT ( 'NONE',  ( -18.50000972452446035, 65.70673848566957531, -64.06382523348288771 ) ) ;
#151861 = ORIENTED_EDGE ( 'NONE', *, *, #143549, .T. ) ;
#151862 = CIRCLE ( 'NONE', #130986, 0.09999999999999939493 ) ;
#151863 = EDGE_CURVE ( 'NONE', #125361, #140961, #62163, .T. ) ;
#151864 = EDGE_CURVE ( 'NONE', #19078, #29322, #175160, .T. ) ;
#151865 = EDGE_CURVE ( 'NONE', #135784, #194512, #120451, .T. ) ;
#151867 = VERTEX_POINT ( 'NONE', #154315 ) ;
#151866 = AXIS2_PLACEMENT_3D ( 'NONE', #244858, #250004, #208332 ) ;
#151868 = AXIS2_PLACEMENT_3D ( 'NONE', #252538, #217253, #115606 ) ;
#151869 = DIRECTION ( 'NONE',  ( -2.252264143451594314E-15, 0.1298341882520054891, 0.9915357197604850459 ) ) ;
#151870 = EDGE_CURVE ( 'NONE', #208853, #204053, #207920, .T. ) ;
#151871 = DIRECTION ( 'NONE',  ( 1.000000000000000000, -0.000000000000000000, -0.000000000000000000 ) ) ;
#151872 = SHAPE_REPRESENTATION ( 'Snap Open Cable Crossbars 4', ( #2425 ), #252228 ) ;
#151873 = CARTESIAN_POINT ( 'NONE',  ( 18.39999999999999858, 85.68240343348850274, -129.8662641071115047 ) ) ;
#151875 = ORIENTED_EDGE ( 'NONE', *, *, #221841, .F. ) ;
#151874 = DIRECTION ( 'NONE',  ( 1.000000000000000000, 0.000000000000000000, -0.000000000000000000 ) ) ;
#151876 = EDGE_CURVE ( 'NONE', #57651, #160183, #96679, .T. ) ;
#151877 = CARTESIAN_POINT ( 'NONE',  ( 23.14999999999999858, 80.00000000001190870, -103.0231074845242745 ) ) ;
#151878 = CARTESIAN_POINT ( 'NONE',  ( 21.05000000000000071, 67.12338541492449906, -61.13802700567970305 ) ) ;
#151879 = EDGE_CURVE ( 'NONE', #166875, #9660, #157887, .T. ) ;
#151880 = CARTESIAN_POINT ( 'NONE',  ( -21.05000000000000071, 33.04479387145709524, -247.6151719044046899 ) ) ;
#151882 = CARTESIAN_POINT ( 'NONE',  ( -18.37013991200266005, 58.54242066476462014, -223.9590583060466997 ) ) ;
#151881 = CARTESIAN_POINT ( 'NONE',  ( -20.94999999999999929, 76.00000000001170974, -69.52310748452431710 ) ) ;
#151883 = LINE ( 'NONE', #213103, #194780 ) ;
#151885 = EDGE_CURVE ( 'NONE', #221278, #77791, #12117, .T. ) ;
#151884 = CARTESIAN_POINT ( 'NONE',  ( -21.14999999999999858, 0.09779029130879170195, 6.257814610476114758 ) ) ;
#151886 = LINE ( 'NONE', #191007, #160050 ) ;
#151887 = CARTESIAN_POINT ( 'NONE',  ( -20.64999999999999858, 68.85000000001228670, -157.6731074845243938 ) ) ;
#151888 = ORIENTED_EDGE ( 'NONE', *, *, #120406, .T. ) ;
#151889 = AXIS2_PLACEMENT_3D ( 'NONE', #219321, #223169, #1552 ) ;
#151890 = ORIENTED_EDGE ( 'NONE', *, *, #147453, .T. ) ;
#151891 = EDGE_CURVE ( 'NONE', #157381, #79099, #35638, .T. ) ;
#151892 = DIRECTION ( 'NONE',  ( 0.000000000000000000, 6.982962677686266711E-15, -1.000000000000000000 ) ) ;
#151893 = DIRECTION ( 'NONE',  ( 1.000000000000000000, 0.000000000000000000, 0.000000000000000000 ) ) ;
#151894 = ORIENTED_EDGE ( 'NONE', *, *, #139756, .F. ) ;
#151895 = SURFACE_SIDE_STYLE ('',( #253522 ) ) ;
#151896 = DIRECTION ( 'NONE',  ( 2.952720810173289112E-16, 1.000000000000000000, -6.088138035986627436E-46 ) ) ;
#151897 = DIRECTION ( 'NONE',  ( 1.000000000000000000, 0.000000000000000000, 0.000000000000000000 ) ) ;
#151898 = DIRECTION ( 'NONE',  ( 0.000000000000000000, -6.982962677686266711E-15, 1.000000000000000000 ) ) ;
#151899 = ORIENTED_EDGE ( 'NONE', *, *, #169503, .T. ) ;
#151900 = ORIENTED_EDGE ( 'NONE', *, *, #74938, .T. ) ;
#151902 = CARTESIAN_POINT ( 'NONE',  ( -18.59999999999999787, 76.00000000001213607, -136.5231074845243313 ) ) ;
#151901 = AXIS2_PLACEMENT_3D ( 'NONE', #145337, #30560, #108784 ) ;
#151903 = AXIS2_PLACEMENT_3D ( 'NONE', #179871, #200706, #97716 ) ;
#151904 = CARTESIAN_POINT ( 'NONE',  ( -23.25000000000000000, 11.65000000001115588, -79.15000000000004832 ) ) ;
#151905 = ORIENTED_EDGE ( 'NONE', *, *, #147990, .T. ) ;
#151906 = DIRECTION ( 'NONE',  ( 0.000000000000000000, -0.9908441862701600211, -0.1350103645451876666 ) ) ;
#151908 = ORIENTED_EDGE ( 'NONE', *, *, #80827, .F. ) ;
#151907 = CARTESIAN_POINT ( 'NONE',  ( 21.05000000000000071, -11.64999999998883595, -130.9000000000000341 ) ) ;
#151909 = CARTESIAN_POINT ( 'NONE',  ( -21.08078803292166725, 75.92081401285447839, -142.8561204489614624 ) ) ;
#151911 = VERTEX_POINT ( 'NONE', #16068 ) ;
#151910 = DIRECTION ( 'NONE',  ( 0.000000000000000000, -0.8368562265788574983, -0.5474227397872651890 ) ) ;
#151912 = SURFACE_STYLE_USAGE ( .BOTH. , #248421 ) ;
#151913 = CARTESIAN_POINT ( 'NONE',  ( 21.05315837477641949, 64.25000000001217870, -143.3647514783578742 ) ) ;
#151914 = DIRECTION ( 'NONE',  ( 0.000000000000000000, -1.224646799147321160E-16, 1.000000000000000000 ) ) ;
#151915 = B_SPLINE_CURVE_WITH_KNOTS ( 'NONE', 3,
 ( #55354, #197464, #235306, #231482, #112808, #252294, #77495, #157081, #133648, #37140 ),
 .UNSPECIFIED., .F., .F.,
 ( 4, 3, 3, 4 ),
 ( 0.000000000000000000, 0.0002000000000002737706, 0.001000000000045111938, 0.001967863649472118698 ),
 .UNSPECIFIED. ) ;
#151916 = CARTESIAN_POINT ( 'NONE',  ( 20.95512820512820440, 65.37615131630001031, -95.35819391543677170 ) ) ;
#151917 = EDGE_CURVE ( 'NONE', #14829, #105984, #78698, .T. ) ;
#151919 = CARTESIAN_POINT ( 'NONE',  ( -20.90000000000000213, 7.900000000000000355, -1.300000000000000044 ) ) ;
#151918 = DIRECTION ( 'NONE',  ( -0.000000000000000000, 7.109473446599835262E-15, -1.000000000000000000 ) ) ;
#151920 = SPHERICAL_SURFACE ( 'NONE', #16269, 0.1000000000000000056 ) ;
#151921 = CIRCLE ( 'NONE', #152102, 0.1000000000000002554 ) ;
#151922 = DIRECTION ( 'NONE',  ( 0.000000000000000000, 1.000000000000000000, 0.000000000000000000 ) ) ;
#151923 = EDGE_CURVE ( 'NONE', #83610, #91096, #58981, .T. ) ;
#151924 = AXIS2_PLACEMENT_3D ( 'NONE', #221936, #26342, #122878 ) ;
#151925 = DIRECTION ( 'NONE',  ( -1.000000000000000000, -0.000000000000000000, -0.000000000000000000 ) ) ;
#151926 = DIRECTION ( 'NONE',  ( 0.000000000000000000, 0.8814952561688444987, -0.4721928772777320149 ) ) ;
#151927 = VECTOR ( 'NONE', #184953, 1000.000000000000000 ) ;
#151928 = ORIENTED_EDGE ( 'NONE', *, *, #126718, .F. ) ;
#151929 = CIRCLE ( 'NONE', #2036, 0.09999999999998898659 ) ;
#151930 = CARTESIAN_POINT ( 'NONE',  ( -18.44085059012131822, 11.51401249349495437, -76.25969468087851055 ) ) ;
#151931 = EDGE_LOOP ( 'NONE', ( #137265, #226640, #111297, #53716 ) ) ;
#151932 = CARTESIAN_POINT ( 'NONE',  ( -21.05000000000000071, 76.10000000001170406, -76.06376443622556849 ) ) ;
#151934 = ORIENTED_EDGE ( 'NONE', *, *, #148172, .F. ) ;
#151933 =( GEOMETRIC_REPRESENTATION_CONTEXT ( 3 ) GLOBAL_UNCERTAINTY_ASSIGNED_CONTEXT ( ( #146884 ) ) GLOBAL_UNIT_ASSIGNED_CONTEXT ( ( #123024, #78729, #222079 ) ) REPRESENTATION_CONTEXT ( 'NONE', 'WORKASPACE' ) );
#151935 = DIRECTION ( 'NONE',  ( 0.000000000000000000, -0.4999999999999689138, -0.8660254037844565822 ) ) ;
#151936 = EDGE_CURVE ( 'NONE', #35199, #118789, #99533, .T. ) ;
#151937 = FACE_OUTER_BOUND ( 'NONE', #188398, .T. ) ;
#151938 = VERTEX_POINT ( 'NONE', #201090 ) ;
#151939 = CARTESIAN_POINT ( 'NONE',  ( -21.04999999999999361, 30.88834551968416164, -252.0800683362990355 ) ) ;
#151940 =( NAMED_UNIT ( * ) SI_UNIT ( $, .STERADIAN. ) SOLID_ANGLE_UNIT ( ) );
#151941 = AXIS2_PLACEMENT_3D ( 'NONE', #20719, #220189, #136783 ) ;
#151942 = EDGE_LOOP ( 'NONE', ( #129661, #95175, #248849, #161388 ) ) ;
#151943 = AXIS2_PLACEMENT_3D ( 'NONE', #36366, #76740, #55870 ) ;
#151944 = ORIENTED_EDGE ( 'NONE', *, *, #115513, .T. ) ;
#151945 = CIRCLE ( 'NONE', #122727, 7.900000000000007461 ) ;
#151946 = CARTESIAN_POINT ( 'NONE',  ( -23.25000000000000000, 74.00000000001151079, -49.24772940728643533 ) ) ;
#151947 = CARTESIAN_POINT ( 'NONE',  ( 21.04999999999999716, 10.54375127550677149, -41.05638780866501492 ) ) ;
#151948 = DIRECTION ( 'NONE',  ( 0.000000000000000000, 0.000000000000000000, -1.000000000000000000 ) ) ;
#151949 = DIRECTION ( 'NONE',  ( 0.000000000000000000, 0.000000000000000000, 1.000000000000000000 ) ) ;
#151950 = CARTESIAN_POINT ( 'NONE',  ( -18.59999999999999787, 3.132039894996829776, -190.2813437854022993 ) ) ;
#151952 = CARTESIAN_POINT ( 'NONE',  ( 18.49999999999999289, 64.35000000001245724, -181.7731074845244450 ) ) ;
#151951 = DIRECTION ( 'NONE',  ( 0.000000000000000000, 0.7397360091702755991, -0.6728971962616832059 ) ) ;
#151953 = LINE ( 'NONE', #72410, #174394 ) ;
#151955 = VERTEX_POINT ( 'NONE', #138520 ) ;
#151954 = FACE_OUTER_BOUND ( 'NONE', #231752, .T. ) ;
#151957 = CARTESIAN_POINT ( 'NONE',  ( -18.40000000000000213, 11.75000000001113953, -191.7499999999999716 ) ) ;
#151956 = DIRECTION ( 'NONE',  ( 0.000000000000000000, -6.982962677686266711E-15, 1.000000000000000000 ) ) ;
#151958 = DIRECTION ( 'NONE',  ( 1.000000000000000000, 0.000000000000000000, 0.000000000000000000 ) ) ;
#151959 = ORIENTED_EDGE ( 'NONE', *, *, #202958, .T. ) ;
#151960 = CARTESIAN_POINT ( 'NONE',  ( -23.25000000000000000, 64.35000000001180354, -81.77310748452438816 ) ) ;
#151961 = CIRCLE ( 'NONE', #47854, 0.09999999999999095723 ) ;
#151962 = CARTESIAN_POINT ( 'NONE',  ( -23.15000000000000213, 70.80971041069356886, -215.3055740759912453 ) ) ;
#151963 = DIRECTION ( 'NONE',  ( 0.000000000000000000, -0.2128009952263485993, 0.9770955615653341697 ) ) ;
#151964 = AXIS2_PLACEMENT_3D ( 'NONE', #111960, #51941, #114508 ) ;
#151965 = VERTEX_POINT ( 'NONE', #81125 ) ;
#151966 = AXIS2_PLACEMENT_3D ( 'NONE', #246676, #68049, #191883 ) ;
#151967 = CARTESIAN_POINT ( 'NONE',  ( -16.85312841634288006, 61.03918102309979332, -220.8126985114581942 ) ) ;
#151968 = CIRCLE ( 'NONE', #5594, 1.749999999999999778 ) ;
#151969 = FACE_OUTER_BOUND ( 'NONE', #65779, .T. ) ;
#151970 = EDGE_CURVE ( 'NONE', #153027, #236989, #245329, .T. ) ;
#151971 = CARTESIAN_POINT ( 'NONE',  ( 12.60053434924909865, 66.61046543766512684, -87.34829818013440672 ) ) ;
#151972 = ORIENTED_EDGE ( 'NONE', *, *, #111141, .F. ) ;
#151973 = VERTEX_POINT ( 'NONE', #78567 ) ;
#151974 = TOROIDAL_SURFACE ( 'NONE', #243517, 0.6000000000000009770, 0.1000000000000000056 ) ;
#151975 = CARTESIAN_POINT ( 'NONE',  ( -18.50000000000000000, -1.866714910046153308, -145.7526752462820241 ) ) ;
#151976 = TOROIDAL_SURFACE ( 'NONE', #60354, 0.4000000000000003553, 0.1000000000000000056 ) ;
#151977 = DIRECTION ( 'NONE',  ( 0.000000000000000000, 0.2617529984165152257, 0.9651348961777124202 ) ) ;
#151978 = LINE ( 'NONE', #131097, #223941 ) ;
#151979 = DIRECTION ( 'NONE',  ( 1.000000000000000000, 0.000000000000000000, 0.000000000000000000 ) ) ;
#151980 = ORIENTED_EDGE ( 'NONE', *, *, #179030, .T. ) ;
#151981 = VECTOR ( 'NONE', #29018, 1000.000000000000000 ) ;
#151982 = AXIS2_PLACEMENT_3D ( 'NONE', #182221, #42701, #122246 ) ;
#151983 = ADVANCED_FACE ( 'NONE', ( #137258 ), #216794, .F. ) ;
#151984 = CARTESIAN_POINT ( 'NONE',  ( 18.49999999999999289, 6.450000000000001066, -21.15000000000000213 ) ) ;
#151985 = DIRECTION ( 'NONE',  ( -0.000000000000000000, 0.8127272543710918340, -0.5826443254700303109 ) ) ;
#151986 = ADVANCED_FACE ( 'NONE', ( #119002 ), #82962, .T. ) ;
#151987 = DIRECTION ( 'NONE',  ( 0.000000000000000000, -0.9126074666063769270, -0.4088369013363280513 ) ) ;
#151988 = CARTESIAN_POINT ( 'NONE',  ( 20.12500000000000000, 11.25287472715600146, -206.8511660127314826 ) ) ;
#151989 = EDGE_LOOP ( 'NONE', ( #207113, #124833, #192326, #42496 ) ) ;
#151990 = CARTESIAN_POINT ( 'NONE',  ( -18.46907102845854354, -9.473727364752949853, -207.6760347387364618 ) ) ;
#151991 = ADVANCED_FACE ( 'NONE', ( #99400 ), #153791, .F. ) ;
#151993 = ORIENTED_EDGE ( 'NONE', *, *, #131190, .T. ) ;
#151992 = DIRECTION ( 'NONE',  ( 0.000000000000000000, 0.000000000000000000, 1.000000000000000000 ) ) ;
#151994 = DIRECTION ( 'NONE',  ( 0.000000000000000000, 0.9229812358755983270, -0.3848449534832869001 ) ) ;
#151995 = DIRECTION ( 'NONE',  ( 0.000000000000000000, -7.056502275159894776E-15, 1.000000000000000000 ) ) ;
#151996 = DIRECTION ( 'NONE',  ( -0.000000000000000000, 0.9887567792719327286, 0.1495327102803745423 ) ) ;
#151997 = DIRECTION ( 'NONE',  ( 6.938893903907991995E-14, 0.000000000000000000, 1.000000000000000000 ) ) ;
#151998 = LINE ( 'NONE', #249786, #150418 ) ;
#151999 = EDGE_CURVE ( 'NONE', #88201, #60723, #313, .T. ) ;
#152000 = ORIENTED_EDGE ( 'NONE', *, *, #131163, .T. ) ;
#152001 = FACE_OUTER_BOUND ( 'NONE', #84570, .T. ) ;
#152002 = ADVANCED_FACE ( 'NONE', ( #38187 ), #56428, .T. ) ;
#152003 = LINE ( 'NONE', #150690, #63426 ) ;
#152004 = DIRECTION ( 'NONE',  ( 0.000000000000000000, -0.9770955615653316162, -0.2128009952263604232 ) ) ;
#152005 = ORIENTED_EDGE ( 'NONE', *, *, #85585, .T. ) ;
#152006 = CARTESIAN_POINT ( 'NONE',  ( 18.59999999999999432, 42.92545512184477730, -254.1955779480491344 ) ) ;
#152007 = AXIS2_PLACEMENT_3D ( 'NONE', #117099, #139193, #237042 ) ;
#152008 = DIRECTION ( 'NONE',  ( -1.000000000000000000, 0.000000000000000000, 0.000000000000000000 ) ) ;
#152010 = VECTOR ( 'NONE', #204359, 1000.000000000000000 ) ;
#152009 = DIRECTION ( 'NONE',  ( 0.000000000000000000, 0.000000000000000000, -1.000000000000000000 ) ) ;
#152011 = EDGE_CURVE ( 'NONE', #188501, #203019, #16383, .T. ) ;
#152012 = CIRCLE ( 'NONE', #93527, 0.09999999999998898659 ) ;
#152013 = DIRECTION ( 'NONE',  ( -1.000000000000000000, 0.000000000000000000, 0.000000000000000000 ) ) ;
#152014 = LINE ( 'NONE', #213223, #30202 ) ;
#152015 = ORIENTED_EDGE ( 'NONE', *, *, #237175, .T. ) ;
#152016 = ORIENTED_EDGE ( 'NONE', *, *, #111945, .T. ) ;
#152017 = CYLINDRICAL_SURFACE ( 'NONE', #10005, 0.09999999999998898659 ) ;
#152018 = CIRCLE ( 'NONE', #97786, 12.97500000000000675 ) ;
#152019 = DIRECTION ( 'NONE',  ( 1.000000000000000000, -0.000000000000000000, -0.000000000000000000 ) ) ;
#152020 = EDGE_CURVE ( 'NONE', #2253, #215594, #139820, .T. ) ;
#152021 = LINE ( 'NONE', #112866, #157926 ) ;
#152023 = CIRCLE ( 'NONE', #164480, 0.1000000000000118433 ) ;
#152022 = CARTESIAN_POINT ( 'NONE',  ( -20.94999999999999929, 87.75000000001266187, -200.6231074845242688 ) ) ;
#152024 = AXIS2_PLACEMENT_3D ( 'NONE', #202581, #223408, #244254 ) ;
#152025 = CARTESIAN_POINT ( 'NONE',  ( -16.94445028196808778, 9.992063609708889516, -79.60733017841850767 ) ) ;
#152026 = ORIENTED_EDGE ( 'NONE', *, *, #253632, .T. ) ;
#152027 = LINE ( 'NONE', #93304, #202742 ) ;
#152028 = VERTEX_POINT ( 'NONE', #120316 ) ;
#152029 = DIRECTION ( 'NONE',  ( 0.000000000000000000, -7.026728003956686545E-15, 1.000000000000000000 ) ) ;
#152030 = DIRECTION ( 'NONE',  ( 1.000000000000000000, 0.000000000000000000, 0.000000000000000000 ) ) ;
#152032 = AXIS2_PLACEMENT_3D ( 'NONE', #248338, #30598, #69719 ) ;
#152031 = DIRECTION ( 'NONE',  ( 0.000000000000000000, 0.4721928772777346239, 0.8814952561688430555 ) ) ;
#152033 = CARTESIAN_POINT ( 'NONE',  ( -22.48660254037843487, 11.65000000000000036, 0.04999999999998061551 ) ) ;
#152034 = DIRECTION ( 'NONE',  ( -0.000000000000000000, 1.000000000000000000, 6.982962677686266711E-15 ) ) ;
#152035 = CARTESIAN_POINT ( 'NONE',  ( 18.52326479938722059, 85.64236444492716771, -62.80835007111859625 ) ) ;
#152036 = DIRECTION ( 'NONE',  ( 0.000000000000000000, 0.9126074666064696306, 0.4088369013361213278 ) ) ;
#152037 = ORIENTED_EDGE ( 'NONE', *, *, #231044, .F. ) ;
#152038 = CARTESIAN_POINT ( 'NONE',  ( -16.93226657140833069, 22.93862264524221573, -230.8577296051770418 ) ) ;
#152039 = DIRECTION ( 'NONE',  ( 0.000000000000000000, 6.982962677686266711E-15, -1.000000000000000000 ) ) ;
#152040 = DIRECTION ( 'NONE',  ( 0.000000000000000000, -6.982962677686266711E-15, 1.000000000000000000 ) ) ;
#152041 = DIRECTION ( 'NONE',  ( 1.000000000000000000, 0.000000000000000000, 0.000000000000000000 ) ) ;
#152042 = LINE ( 'NONE', #100681, #216325 ) ;
#152043 = CIRCLE ( 'NONE', #239516, 0.09999999999999939493 ) ;
#152044 = EDGE_CURVE ( 'NONE', #148706, #120086, #49686, .T. ) ;
#152045 = AXIS2_PLACEMENT_3D ( 'NONE', #36601, #116111, #173558 ) ;
#152046 = VERTEX_POINT ( 'NONE', #98105 ) ;
#152047 = DIRECTION ( 'NONE',  ( -1.000000000000000000, -0.000000000000000000, -0.000000000000000000 ) ) ;
#152048 = DIRECTION ( 'NONE',  ( 1.000000000000000000, 0.000000000000000000, -0.000000000000000000 ) ) ;
#152049 = ORIENTED_EDGE ( 'NONE', *, *, #57006, .F. ) ;
#152050 = EDGE_CURVE ( 'NONE', #195479, #186480, #87262, .T. ) ;
#152051 = ORIENTED_EDGE ( 'NONE', *, *, #42764, .T. ) ;
#152052 = DIRECTION ( 'NONE',  ( 0.000000000000000000, -0.9908441862701596881, 0.1350103645451904977 ) ) ;
#152053 = LINE ( 'NONE', #52919, #169052 ) ;
#152054 = EDGE_CURVE ( 'NONE', #20503, #182622, #220661, .T. ) ;
#152055 = ORIENTED_EDGE ( 'NONE', *, *, #13960, .F. ) ;
#152057 = EDGE_CURVE ( 'NONE', #58353, #75872, #223016, .T. ) ;
#152056 = DIRECTION ( 'NONE',  ( 0.000000000000000000, 0.2617529984165030132, 0.9651348961777157509 ) ) ;
#152058 = CARTESIAN_POINT ( 'NONE',  ( 20.95512820512820440, 8.876151316299273120, -42.05862899514095687 ) ) ;
#152059 = ORIENTED_EDGE ( 'NONE', *, *, #221796, .T. ) ;
#152060 = CIRCLE ( 'NONE', #172931, 0.09999999999999742428 ) ;
#152061 = CARTESIAN_POINT ( 'NONE',  ( 18.58719872626880232, -9.566644397587491966, -174.3224781963970429 ) ) ;
#152062 = CIRCLE ( 'NONE', #18761, 0.09999999999999967248 ) ;
#152063 = ORIENTED_EDGE ( 'NONE', *, *, #79553, .T. ) ;
#152064 = CYLINDRICAL_SURFACE ( 'NONE', #26887, 0.09999999999999939493 ) ;
#152065 = ADVANCED_FACE ( 'NONE', ( #77281 ), #158162, .T. ) ;
#152066 = CARTESIAN_POINT ( 'NONE',  ( 20.94999999999999574, -11.41227409414968719, -2.900000000000003464 ) ) ;
#152068 = ORIENTED_EDGE ( 'NONE', *, *, #199479, .F. ) ;
#152067 = CARTESIAN_POINT ( 'NONE',  ( 15.48841904831874849, 8.561580951681223794, -20.85000000000000497 ) ) ;
#152069 = DIRECTION ( 'NONE',  ( 0.000000000000000000, 0.000000000000000000, 1.000000000000000000 ) ) ;
#152071 = UNCERTAINTY_MEASURE_WITH_UNIT (LENGTH_MEASURE( 1.000000000000000082E-05 ), #358, 'distance_accuracy_value', 'NONE');
#152070 = CARTESIAN_POINT ( 'NONE',  ( 18.59999999999999076, 69.55000000001159322, -59.50608031408435039 ) ) ;
#152072 = ADVANCED_FACE ( 'NONE', ( #257156 ), #27629, .F. ) ;
#152073 = CARTESIAN_POINT ( 'NONE',  ( 23.14999999999999503, 53.24180694658302571, -234.8354225850497130 ) ) ;
#152074 = DIRECTION ( 'NONE',  ( 1.000000000000000000, 0.000000000000000000, 0.000000000000000000 ) ) ;
#152075 = DIRECTION ( 'NONE',  ( 1.000000000000000000, 0.000000000000000000, 0.000000000000000000 ) ) ;
#152076 = LINE ( 'NONE', #206892, #188714 ) ;
#152077 = DIRECTION ( 'NONE',  ( 0.000000000000000000, 0.01283462868040226822, 0.9999176327611370985 ) ) ;
#152079 = ORIENTED_EDGE ( 'NONE', *, *, #168388, .T. ) ;
#152078 = CARTESIAN_POINT ( 'NONE',  ( 21.30000000000002558, 76.00000000001216449, -140.5731074845242858 ) ) ;
#152081 = ORIENTED_EDGE ( 'NONE', *, *, #40930, .F. ) ;
#152080 = PRODUCT_DEFINITION ( 'UNKNOWN', '', #132161, #240885 ) ;
#152083 = CARTESIAN_POINT ( 'NONE',  ( 20.94999999999999929, 65.61821452928792553, -97.51526212064020172 ) ) ;
#152082 = DIRECTION ( 'NONE',  ( 1.000000000000000000, 2.952720810173289112E-16, -0.000000000000000000 ) ) ;
#152085 = EDGE_LOOP ( 'NONE', ( #193886, #149845 ) ) ;
#152084 = DIRECTION ( 'NONE',  ( 1.000000000000000000, -2.952720810173289112E-16, -2.061873921506763405E-30 ) ) ;
#152086 = EDGE_LOOP ( 'NONE', ( #253761, #10390, #118091 ) ) ;
#152087 = DIRECTION ( 'NONE',  ( 0.000000000000000000, 0.000000000000000000, 1.000000000000000000 ) ) ;
#152088 = FACE_OUTER_BOUND ( 'NONE', #57813, .T. ) ;
#152089 = VECTOR ( 'NONE', #203116, 1000.000000000000227 ) ;
#152090 = AXIS2_PLACEMENT_3D ( 'NONE', #57767, #198569, #96869 ) ;
#152092 = ADVANCED_FACE ( 'NONE', ( #23774 ), #253857, .T. ) ;
#152091 = CARTESIAN_POINT ( 'NONE',  ( 20.27550659511089037, 13.44185616693653529, -219.4112591824391529 ) ) ;
#152093 = DIRECTION ( 'NONE',  ( -0.000000000000000000, -0.8660254037844420383, 0.4999999999999943379 ) ) ;
#152094 = EDGE_CURVE ( 'NONE', #21586, #27420, #257911, .T. ) ;
#152095 = EDGE_CURVE ( 'NONE', #112449, #75197, #207527, .T. ) ;
#152096 = FACE_OUTER_BOUND ( 'NONE', #43428, .T. ) ;
#152097 = CARTESIAN_POINT ( 'NONE',  ( -16.87683809663752399, 66.15000000001201386, -116.4254715027206686 ) ) ;
#152098 = DIRECTION ( 'NONE',  ( -1.000000000000000000, 0.000000000000000000, 0.000000000000000000 ) ) ;
#152099 = ORIENTED_EDGE ( 'NONE', *, *, #251396, .T. ) ;
#152100 = EDGE_LOOP ( 'NONE', ( #87366, #116755, #166726, #92100, #238354, #36829, #171579, #39699, #156738, #176793, #176448, #30322, #22231, #109845 ) ) ;
#152101 = CARTESIAN_POINT ( 'NONE',  ( 23.24999999999999645, 36.65892442174935439, -249.5511627012433848 ) ) ;
#152102 = AXIS2_PLACEMENT_3D ( 'NONE', #167868, #11334, #145691 ) ;
#152103 = AXIS2_PLACEMENT_3D ( 'NONE', #220387, #24772, #200816 ) ;
#152104 = VERTEX_POINT ( 'NONE', #227062 ) ;
#152105 = DIRECTION ( 'NONE',  ( 0.000000000000000000, -1.000000000000000000, 0.000000000000000000 ) ) ;
#152106 = EDGE_LOOP ( 'NONE', ( #221659, #55500, #1611, #255066 ) ) ;
#152107 = CARTESIAN_POINT ( 'NONE',  ( 20.90000000000000213, 7.800000000000000711, -1.212568896937008089 ) ) ;
#152108 = CIRCLE ( 'NONE', #18797, 0.09999999999999939493 ) ;
#152109 = B_SPLINE_CURVE_WITH_KNOTS ( 'NONE', 3,
 ( #216240, #15516, #235811, #20643, #80562, #155030, #117165, #196681, #79291, #256607 ),
 .UNSPECIFIED., .F., .F.,
 ( 4, 3, 3, 4 ),
 ( 0.000000000000000000, 4.874959354404207151E-05, 9.785140065121151641E-05, 0.0001360444631936073986 ),
 .UNSPECIFIED. ) ;
#152110 = DIRECTION ( 'NONE',  ( 0.000000000000000000, 0.9229812358756199764, -0.3848449534832346086 ) ) ;
#152111 = COLOUR_RGB ( '', 0.08235294, 0.09019608, 0.10196078) ;
#152112 = DIRECTION ( 'NONE',  ( 1.000000000000000000, 0.000000000000000000, 0.000000000000000000 ) ) ;
#152113 = VERTEX_POINT ( 'NONE', #64155 ) ;
#152114 = DIRECTION ( 'NONE',  ( 1.476360405086644309E-16, 1.000000000000000000, 0.000000000000000000 ) ) ;
#152115 = ORIENTED_EDGE ( 'NONE', *, *, #232126, .T. ) ;
#152116 = CARTESIAN_POINT ( 'NONE',  ( 21.14999999999999858, 36.69980811187836878, -249.6424234479061113 ) ) ;
#152117 = EDGE_CURVE ( 'NONE', #57260, #242049, #212199, .T. ) ;
#152118 = CARTESIAN_POINT ( 'NONE',  ( 18.51565452909304099, 9.054758213346417506, -245.3745873853864055 ) ) ;
#152119 = ORIENTED_EDGE ( 'NONE', *, *, #115761, .T. ) ;
#152120 = CARTESIAN_POINT ( 'NONE',  ( -20.94999999999999929, -1.851028230129704522, -45.15391326942249606 ) ) ;
#152121 = ORIENTED_EDGE ( 'NONE', *, *, #249238, .F. ) ;
#152124 = VERTEX_POINT ( 'NONE', #146239 ) ;
#152123 = DIRECTION ( 'NONE',  ( 0.000000000000000000, 0.9910827722268055195, 0.1332476588733540468 ) ) ;
#152122 = CYLINDRICAL_SURFACE ( 'NONE', #220022, 0.09999999999998898659 ) ;
#152126 = ORIENTED_EDGE ( 'NONE', *, *, #57373, .F. ) ;
#152125 = AXIS2_PLACEMENT_3D ( 'NONE', #216242, #37643, #238382 ) ;
#152127 = TOROIDAL_SURFACE ( 'NONE', #39702, 11.70000000000000639, 0.1000000000000000056 ) ;
#152128 = ORIENTED_EDGE ( 'NONE', *, *, #71226, .T. ) ;
#152129 = AXIS2_PLACEMENT_3D ( 'NONE', #253674, #154624, #149478 ) ;
#152130 = EDGE_CURVE ( 'NONE', #60425, #212130, #70741, .T. ) ;
#152131 = DIRECTION ( 'NONE',  ( -0.000000000000000000, -0.2128009952263603677, 0.9770955615653313941 ) ) ;
#152132 = EDGE_LOOP ( 'NONE', ( #79333, #8905, #47309 ) ) ;
#152133 = LINE ( 'NONE', #110407, #105942 ) ;
#152134 = DIRECTION ( 'NONE',  ( 1.073024830501117725E-15, -0.000000000000000000, -1.000000000000000000 ) ) ;
#152135 = CARTESIAN_POINT ( 'NONE',  ( 11.60000000000000142, -8.350000000000004974, 15.00000000000000355 ) ) ;
#152136 = AXIS2_PLACEMENT_3D ( 'NONE', #115156, #177730, #113869 ) ;
#152137 = EDGE_CURVE ( 'NONE', #7658, #3601, #178908, .T. ) ;
#152138 = CIRCLE ( 'NONE', #18836, 2.000000000000001776 ) ;
#152139 = AXIS2_PLACEMENT_3D ( 'NONE', #149286, #230084, #11038 ) ;
#152140 = CARTESIAN_POINT ( 'NONE',  ( -23.15000000000000213, 64.35000000001146248, -43.03791325517835276 ) ) ;
#152141 = ORIENTED_EDGE ( 'NONE', *, *, #136340, .F. ) ;
#152142 = ADVANCED_FACE ( 'NONE', ( #245365 ), #65427, .T. ) ;
#152143 = CARTESIAN_POINT ( 'NONE',  ( 20.94999999999999929, -1.162701749926853712, -74.90000000000004832 ) ) ;
#152144 = LINE ( 'NONE', #231673, #186357 ) ;
#152145 = CARTESIAN_POINT ( 'NONE',  ( 21.08621493067296271, 6.349294291182824956, -33.44380516052389396 ) ) ;
#152146 = ORIENTED_EDGE ( 'NONE', *, *, #128945, .T. ) ;
#152147 = CARTESIAN_POINT ( 'NONE',  ( -21.07928932188134041, 0.09889514565439468108, 6.328516656393293083 ) ) ;
#152148 = VERTEX_POINT ( 'NONE', #126692 ) ;
#152149 = CARTESIAN_POINT ( 'NONE',  ( -21.17356465864818560, 33.94277835663822174, -243.7301031769779343 ) ) ;
#152150 = ORIENTED_EDGE ( 'NONE', *, *, #89091, .F. ) ;
#152151 = EDGE_CURVE ( 'NONE', #88024, #195816, #45594, .T. ) ;
#152152 = AXIS2_PLACEMENT_3D ( 'NONE', #124253, #222025, #104634 ) ;
#152153 = EDGE_CURVE ( 'NONE', #129607, #10810, #233052, .T. ) ;
#152154 = AXIS2_PLACEMENT_3D ( 'NONE', #95530, #250750, #211646 ) ;
#152155 = CARTESIAN_POINT ( 'NONE',  ( 20.94999999999999929, 70.50000000001253397, -182.4283735034374843 ) ) ;
#152156 = LINE ( 'NONE', #53014, #247757 ) ;
#152158 = ORIENTED_EDGE ( 'NONE', *, *, #229824, .T. ) ;
#152157 = CARTESIAN_POINT ( 'NONE',  ( -18.50000000000000000, 3.912899247244609580, -78.48182297301100618 ) ) ;
#152159 = CARTESIAN_POINT ( 'NONE',  ( 21.00000000000000000, 66.25000000001151079, -48.37310748452438958 ) ) ;
#152160 = ORIENTED_EDGE ( 'NONE', *, *, #138834, .F. ) ;
#152161 = AXIS2_PLACEMENT_3D ( 'NONE', #161327, #24388, #240854 ) ;
#152162 = AXIS2_PLACEMENT_3D ( 'NONE', #188324, #129635, #50090 ) ;
#152163 = DIRECTION ( 'NONE',  ( 0.000000000000000000, 0.2128009952263603677, -0.9770955615653313941 ) ) ;
#152164 = CARTESIAN_POINT ( 'NONE',  ( 20.95512820512820440, 10.62384868371188062, -21.25000000000000000 ) ) ;
#152165 = ORIENTED_EDGE ( 'NONE', *, *, #120056, .F. ) ;
#152166 = CARTESIAN_POINT ( 'NONE',  ( 18.39999999999999858, 85.40000000001222702, -148.2731074845242460 ) ) ;
#152167 = CARTESIAN_POINT ( 'NONE',  ( 21.14999999999999858, 23.38726701055792745, -229.1122755113798348 ) ) ;
#152168 = VERTEX_POINT ( 'NONE', #104524 ) ;
#152169 = DIRECTION ( 'NONE',  ( -1.000000000000000000, -0.000000000000000000, -0.000000000000000000 ) ) ;
#152170 = EDGE_CURVE ( 'NONE', #164707, #16838, #83668, .T. ) ;
#152171 = ADVANCED_FACE ( 'NONE', ( #184090 ), #62862, .T. ) ;
#152172 = ORIENTED_EDGE ( 'NONE', *, *, #32517, .F. ) ;
#152173 = CARTESIAN_POINT ( 'NONE',  ( 12.25000000000000000, 9.350000000011140955, -117.2500000000000284 ) ) ;
#152174 = CARTESIAN_POINT ( 'NONE',  ( 23.14999999999999858, 76.00000000001243450, -168.0231074845243597 ) ) ;
#152175 = EDGE_CURVE ( 'NONE', #192091, #76825, #145530, .T. ) ;
#152178 = ORIENTED_EDGE ( 'NONE', *, *, #125615, .F. ) ;
#152177 = EDGE_LOOP ( 'NONE', ( #63640, #166704, #207039, #31870 ) ) ;
#152176 = DIRECTION ( 'NONE',  ( 0.000000000000000000, -7.109473446599835262E-15, 1.000000000000000000 ) ) ;
#152179 = VECTOR ( 'NONE', #187998, 1000.000000000000000 ) ;
#152180 = LINE ( 'NONE', #8793, #41290 ) ;
#152181 = CARTESIAN_POINT ( 'NONE',  ( -22.43310005002225438, 0.005636942152031573783, -155.8503378728655662 ) ) ;
#152182 = EDGE_CURVE ( 'NONE', #97170, #173551, #162311, .T. ) ;
#152183 = AXIS2_PLACEMENT_3D ( 'NONE', #61993, #137646, #36020 ) ;
#152184 = DIRECTION ( 'NONE',  ( 0.000000000000000000, -6.467318590049456648E-15, 1.000000000000000000 ) ) ;
#152186 = DIRECTION ( 'NONE',  ( -1.000000000000000000, -0.000000000000000000, -0.000000000000000000 ) ) ;
#152185 = CARTESIAN_POINT ( 'NONE',  ( 21.00000000000000000, 9.750000000011153745, -88.25000000000005684 ) ) ;
#152187 = DIRECTION ( 'NONE',  ( 0.000000000000000000, 0.8814952561688430555, -0.4721928772777346239 ) ) ;
#152188 = VECTOR ( 'NONE', #14203, 1000.000000000000000 ) ;
#152190 = EDGE_CURVE ( 'NONE', #128152, #60123, #45866, .T. ) ;
#152189 = DIRECTION ( 'NONE',  ( 0.000000000000000000, 0.000000000000000000, 1.000000000000000000 ) ) ;
#152191 = DIRECTION ( 'NONE',  ( 0.000000000000000000, 0.2128009952263485993, -0.9770955615653341697 ) ) ;
#152192 = CARTESIAN_POINT ( 'NONE',  ( -21.05000000000000071, -11.64999999998884483, -103.5000000000000426 ) ) ;
#152193 = ORIENTED_EDGE ( 'NONE', *, *, #230123, .T. ) ;
#152194 = ORIENTED_EDGE ( 'NONE', *, *, #43189, .F. ) ;
#152195 = CARTESIAN_POINT ( 'NONE',  ( -23.25000000000000000, 4.350000000011156054, -121.8500000000000227 ) ) ;
#152197 = VERTEX_POINT ( 'NONE', #2872 ) ;
#152196 = FACE_OUTER_BOUND ( 'NONE', #101095, .T. ) ;
#152198 = ORIENTED_EDGE ( 'NONE', *, *, #188614, .F. ) ;
#152199 = CARTESIAN_POINT ( 'NONE',  ( -16.77828822508139694, 12.41303647063107718, -211.2560303524380174 ) ) ;
#152200 =( BOUNDED_CURVE ( )  B_SPLINE_CURVE ( 3, ( #6664, #165772, #187894, #50904 ),
 .UNSPECIFIED., .F., .F. ) 
 B_SPLINE_CURVE_WITH_KNOTS ( ( 4, 4 ),
 ( 5.731445031868799056, 5.983100554402348337 ),
 .UNSPECIFIED. ) 
 CURVE ( )  GEOMETRIC_REPRESENTATION_ITEM ( )  RATIONAL_B_SPLINE_CURVE ( ( 1.000000000000000000, 0.9947294176030464508, 0.9947294176030464508, 1.000000000000000000 ) ) 
 REPRESENTATION_ITEM ( '' )  );
#152201 = ORIENTED_EDGE ( 'NONE', *, *, #83837, .T. ) ;
#152202 = CARTESIAN_POINT ( 'NONE',  ( 21.07016717456946964, 34.07469055596557439, -243.7826248964179854 ) ) ;
#152203 = EDGE_CURVE ( 'NONE', #82821, #252796, #99720, .T. ) ;
#152204 = CIRCLE ( 'NONE', #106363, 0.1000000000000028644 ) ;
#152205 = EDGE_CURVE ( 'NONE', #189995, #3592, #33153, .T. ) ;
#152206 = CIRCLE ( 'NONE', #122968, 2.000000000000001776 ) ;
#152207 = ORIENTED_EDGE ( 'NONE', *, *, #195767, .T. ) ;
#152208 = VECTOR ( 'NONE', #126287, 1000.000000000000000 ) ;
#152209 = CARTESIAN_POINT ( 'NONE',  ( 18.54999999999999716, 66.05000000001156479, -56.87310748452444642 ) ) ;
#152211 = ORIENTED_EDGE ( 'NONE', *, *, #29435, .T. ) ;
#152210 = ORIENTED_EDGE ( 'NONE', *, *, #62846, .F. ) ;
#152212 = EDGE_LOOP ( 'NONE', ( #224472, #35543, #184774, #204430 ) ) ;
#152213 = EDGE_LOOP ( 'NONE', ( #255001, #166095, #193945, #19853 ) ) ;
#152214 = ORIENTED_EDGE ( 'NONE', *, *, #168839, .F. ) ;
#152215 = DIRECTION ( 'NONE',  ( -0.000000000000000000, 1.156482317317873105E-15, 1.000000000000000000 ) ) ;
#152216 = FACE_OUTER_BOUND ( 'NONE', #28560, .T. ) ;
#152217 = PLANE ( 'NONE',  #52034 ) ;
#152219 = ORIENTED_EDGE ( 'NONE', *, *, #55800, .T. ) ;
#152218 = CARTESIAN_POINT ( 'NONE',  ( -21.45000000000000284, 10.16011026985487398, -211.4267369781599939 ) ) ;
#152220 = AXIS2_PLACEMENT_3D ( 'NONE', #158273, #197343, #123929 ) ;
#152221 = FACE_OUTER_BOUND ( 'NONE', #249258, .T. ) ;
#152222 = LINE ( 'NONE', #153526, #257493 ) ;
#152224 = ORIENTED_EDGE ( 'NONE', *, *, #40076, .F. ) ;
#152223 = CARTESIAN_POINT ( 'NONE',  ( 20.94999999999999574, 77.36087058720436005, -161.9501095574333931 ) ) ;
#152225 = CARTESIAN_POINT ( 'NONE',  ( -22.39999999999999858, 11.48087284840413425, -198.4995883060917947 ) ) ;
#152226 = ORIENTED_EDGE ( 'NONE', *, *, #170645, .F. ) ;
#152227 = CARTESIAN_POINT ( 'NONE',  ( 20.99142135623731065, 11.60000000001116049, -127.0717967697245570 ) ) ;
#152228 = ORIENTED_EDGE ( 'NONE', *, *, #214597, .T. ) ;
#152229 = FACE_OUTER_BOUND ( 'NONE', #155202, .T. ) ;
#152230 = DIRECTION ( 'NONE',  ( 0.000000000000000000, 0.000000000000000000, -1.000000000000000000 ) ) ;
#152231 = ORIENTED_EDGE ( 'NONE', *, *, #60314, .T. ) ;
#152233 = CARTESIAN_POINT ( 'NONE',  ( 20.85000000000000142, 77.73670573947995877, -158.5056848969006182 ) ) ;
#152232 = CARTESIAN_POINT ( 'NONE',  ( -23.15000000000000213, 6.857177884343597540, -212.0437362999421680 ) ) ;
#152234 = B_SPLINE_CURVE_WITH_KNOTS ( 'NONE', 3,
 ( #248647, #49161, #28359, #70038, #167860, #109123, #50423, #209523, #30922, #110417, #189966, #236773, #253765, #214647, #157277, #174301, #56831, #34771, #78964 ),
 .UNSPECIFIED., .F., .F.,
 ( 4, 3, 3, 3, 3, 3, 4 ),
 ( -2.000416914663624153E-06, 0.000000000000000000, 4.714008503747321038E-05, 9.979203887777386673E-05, 0.0001372215519229492986, 0.0001635031576221004674, 0.0001900083748504117793 ),
 .UNSPECIFIED. ) ;
#152235 = DIRECTION ( 'NONE',  ( 0.000000000000000000, -0.9910465087640861759, 0.1335171055202901691 ) ) ;
#152236 = AXIS2_PLACEMENT_3D ( 'NONE', #14329, #93829, #153864 ) ;
#152237 = EDGE_CURVE ( 'NONE', #25987, #213658, #58030, .T. ) ;
#152238 = DIRECTION ( 'NONE',  ( -1.000000000000000000, 0.000000000000000000, 0.000000000000000000 ) ) ;
#152239 = CIRCLE ( 'NONE', #218823, 0.1000000000000124678 ) ;
#152240 = VERTEX_POINT ( 'NONE', #250477 ) ;
#152241 = ORIENTED_EDGE ( 'NONE', *, *, #166583, .T. ) ;
#152242 = LINE ( 'NONE', #192630, #34710 ) ;
#152243 = DIRECTION ( 'NONE',  ( 4.336808689942127388E-15, 0.8496786552930133407, 0.5273008465188128158 ) ) ;
#152244 = VERTEX_POINT ( 'NONE', #11902 ) ;
#152245 = CARTESIAN_POINT ( 'NONE',  ( -22.59080734064477980, 55.88289069467541736, -232.8092063914161542 ) ) ;
#152246 = ORIENTED_EDGE ( 'NONE', *, *, #54345, .F. ) ;
#152247 = CARTESIAN_POINT ( 'NONE',  ( -22.50047199487879368, 0.04490605193106571302, -55.24995258108270946 ) ) ;
#152248 = DIRECTION ( 'NONE',  ( 1.186688945009010077E-16, 1.000000000000000000, 6.982962677686266711E-15 ) ) ;
#152249 = CARTESIAN_POINT ( 'NONE',  ( 22.39999999999999503, -0.1008583690875579364, -155.7504328765105868 ) ) ;
#152250 = ORIENTED_EDGE ( 'NONE', *, *, #88603, .F. ) ;
#152251 = CARTESIAN_POINT ( 'NONE',  ( -16.79139129368504157, 66.05505583755092402, -190.8528628516986316 ) ) ;
#152252 = PRESENTATION_STYLE_ASSIGNMENT (( #229205 ) ) ;
#152253 = ADVANCED_FACE ( 'NONE', ( #232231 ), #49857, .T. ) ;
#152254 = ORIENTED_EDGE ( 'NONE', *, *, #221556, .T. ) ;
#152255 = ORIENTED_EDGE ( 'NONE', *, *, #250499, .F. ) ;
#152256 = EDGE_LOOP ( 'NONE', ( #105317, #238337, #30615, #106035 ) ) ;
#152257 = DIRECTION ( 'NONE',  ( -0.000000000000000000, -0.7397890806274223241, -0.6728388485993012091 ) ) ;
#152258 = CARTESIAN_POINT ( 'NONE',  ( 12.93225390519044993, 66.58234804117054750, -54.16432009208397602 ) ) ;
#152259 = CIRCLE ( 'NONE', #10766, 0.1000000000000124678 ) ;
#152260 = FACE_OUTER_BOUND ( 'NONE', #246632, .T. ) ;
#152261 = DIRECTION ( 'NONE',  ( 0.000000000000000000, 1.224646799142185182E-16, 1.000000000000000000 ) ) ;
#152262 = CARTESIAN_POINT ( 'NONE',  ( -17.22361732159831860, 31.52054061960090436, -235.0627536016827719 ) ) ;
#152264 = CARTESIAN_POINT ( 'NONE',  ( -20.64999999999999858, 1.115600667400684642E-11, -113.4750000000000369 ) ) ;
#152263 = CARTESIAN_POINT ( 'NONE',  ( -18.50000000000000000, 1.115600667400684642E-11, -134.0000000000000284 ) ) ;
#152266 = EDGE_LOOP ( 'NONE', ( #217455, #36459, #35470, #163928 ) ) ;
#152265 = DIRECTION ( 'NONE',  ( 1.000000000000000000, 0.000000000000000000, 0.000000000000000000 ) ) ;
#152267 = CYLINDRICAL_SURFACE ( 'NONE', #253980, 0.1000000000000028644 ) ;
#152268 = ORIENTED_EDGE ( 'NONE', *, *, #69677, .F. ) ;
#152269 = ORIENTED_EDGE ( 'NONE', *, *, #47376, .F. ) ;
#152270 = EDGE_LOOP ( 'NONE', ( #159711, #43820, #1164, #189348 ) ) ;
#152271 = CARTESIAN_POINT ( 'NONE',  ( -23.25000000000000000, 76.00000000001185185, -95.12310748452429721 ) ) ;
#152272 = CYLINDRICAL_SURFACE ( 'NONE', #18632, 0.1000000000000013933 ) ;
#152273 = CARTESIAN_POINT ( 'NONE',  ( -16.92563707711778065, 66.03100930561473092, -48.64234918500041971 ) ) ;
#152274 = DIRECTION ( 'NONE',  ( 0.000000000000000000, 0.8814952561688429444, -0.4721928772777347350 ) ) ;
#152275 = AXIS2_PLACEMENT_3D ( 'NONE', #102392, #144105, #146664 ) ;
#152276 = AXIS2_PLACEMENT_3D ( 'NONE', #48045, #224108, #8928 ) ;
#152277 = CARTESIAN_POINT ( 'NONE',  ( 23.50000000000005684, 76.00000000001119815, -36.02310748452479316 ) ) ;
#152278 = ORIENTED_EDGE ( 'NONE', *, *, #213642, .F. ) ;
#152279 = ORIENTED_EDGE ( 'NONE', *, *, #77036, .F. ) ;
#152280 = DIRECTION ( 'NONE',  ( 0.000000000000000000, 0.000000000000000000, -1.000000000000000000 ) ) ;
#152281 = ORIENTED_EDGE ( 'NONE', *, *, #215831, .F. ) ;
#152282 = DIRECTION ( 'NONE',  ( 0.000000000000000000, 0.3738317757009225195, 0.9274965247785541544 ) ) ;
#152283 = CARTESIAN_POINT ( 'NONE',  ( 21.10000000000000142, -11.65000000000000036, 12.09999999999999609 ) ) ;
#152284 = ORIENTED_EDGE ( 'NONE', *, *, #83205, .T. ) ;
#152285 = CARTESIAN_POINT ( 'NONE',  ( 20.94999999999999929, 76.00000000001213607, -136.5231074845243313 ) ) ;
#152286 = CARTESIAN_POINT ( 'NONE',  ( -20.85000000106584750, 11.75000000001115197, -60.15550465647356049 ) ) ;
#152287 = CARTESIAN_POINT ( 'NONE',  ( -21.05000000000000071, 6.119053122312926973, -199.6316501170689719 ) ) ;
#152288 = CARTESIAN_POINT ( 'NONE',  ( 23.14999999999999503, 11.65000000001116298, -59.98519422934606382 ) ) ;
#152289 = ORIENTED_EDGE ( 'NONE', *, *, #23133, .T. ) ;
#152290 = CYLINDRICAL_SURFACE ( 'NONE', #116889, 0.1000000000000076245 ) ;
#152291 = CARTESIAN_POINT ( 'NONE',  ( 22.50497660315937765, 76.07871793023727491, -81.27290298941976232 ) ) ;
#152292 = SPHERICAL_SURFACE ( 'NONE', #187503, 0.1000000000000000056 ) ;
#152293 = DIRECTION ( 'NONE',  ( -0.000000000000000000, -6.982962677686266711E-15, 1.000000000000000000 ) ) ;
#152294 = FACE_OUTER_BOUND ( 'NONE', #25528, .T. ) ;
#152295 = ADVANCED_FACE ( 'NONE', ( #249213 ), #203797, .T. ) ;
#152296 = AXIS2_PLACEMENT_3D ( 'NONE', #71026, #127118, #224917 ) ;
#152297 = CARTESIAN_POINT ( 'NONE',  ( -21.00250684356852560, 57.72708596625226818, -226.0092949377465459 ) ) ;
#152298 = CIRCLE ( 'NONE', #110573, 4.100000000000006750 ) ;
#152299 = VECTOR ( 'NONE', #126293, 1000.000000000000000 ) ;
#152300 = CIRCLE ( 'NONE', #81493, 4.099999999999992539 ) ;
#152301 = ORIENTED_EDGE ( 'NONE', *, *, #165471, .F. ) ;
#152302 =( BOUNDED_CURVE ( )  B_SPLINE_CURVE ( 3, ( #196962, #108774, #149211, #195723 ),
 .UNSPECIFIED., .F., .T. ) 
 B_SPLINE_CURVE_WITH_KNOTS ( ( 4, 4 ),
 ( 4.712388980384690562, 6.283185307179586232 ),
 .UNSPECIFIED. ) 
 CURVE ( )  GEOMETRIC_REPRESENTATION_ITEM ( )  RATIONAL_B_SPLINE_CURVE ( ( 1.000000000000000000, 0.8047378541243652705, 0.8047378541243652705, 1.000000000000000000 ) ) 
 REPRESENTATION_ITEM ( '' )  );
#152303 = STYLED_ITEM ( 'NONE', ( #38701 ), #228621 ) ;
#152304 = EDGE_CURVE ( 'NONE', #156269, #25377, #13170, .T. ) ;
#152305 = CYLINDRICAL_SURFACE ( 'NONE', #124573, 0.1000000000000028644 ) ;
#152306 = ORIENTED_EDGE ( 'NONE', *, *, #169233, .F. ) ;
#152307 = DIRECTION ( 'NONE',  ( 0.000000000000000000, -0.4999999999999943379, -0.8660254037844420383 ) ) ;
#152308 = DIRECTION ( 'NONE',  ( 0.000000000000000000, -0.9968797965484670343, -0.07893460099023182075 ) ) ;
#152309 = EDGE_CURVE ( 'NONE', #186437, #26532, #149844, .T. ) ;
#152310 = CARTESIAN_POINT ( 'NONE',  ( -16.83199318825828072, 66.06935387203064636, -82.29552229631519822 ) ) ;
#152311 = DIRECTION ( 'NONE',  ( -1.836970198721029934E-16, -0.9651348961777157509, 0.2617529984165031243 ) ) ;
#152312 = DIRECTION ( 'NONE',  ( -2.940209281316621509E-16, 1.000000000000000000, 0.000000000000000000 ) ) ;
#152313 = FACE_OUTER_BOUND ( 'NONE', #199399, .T. ) ;
#152314 = ORIENTED_EDGE ( 'NONE', *, *, #97773, .F. ) ;
#152315 = FACE_OUTER_BOUND ( 'NONE', #92274, .T. ) ;
#152316 = FACE_OUTER_BOUND ( 'NONE', #247291, .T. ) ;
#152317 = CARTESIAN_POINT ( 'NONE',  ( -33.72168855820451938, 9.950000000011156587, -121.3500000000000938 ) ) ;
#152318 = CARTESIAN_POINT ( 'NONE',  ( -23.25000000000000000, 77.85161776048096272, -124.9199177649206689 ) ) ;
#152319 = ADVANCED_FACE ( 'NONE', ( #150126 ), #208801, .T. ) ;
#152320 = AXIS2_PLACEMENT_3D ( 'NONE', #60701, #200236, #140235 ) ;
#152321 = CARTESIAN_POINT ( 'NONE',  ( -18.50000000000000000, 77.13501884592227498, -128.8061306010920362 ) ) ;
#152322 = TOROIDAL_SURFACE ( 'NONE', #131440, 11.70000000000000639, 0.1000000000000000056 ) ;
#152323 = ORIENTED_EDGE ( 'NONE', *, *, #116492, .F. ) ;
#152324 = ORIENTED_EDGE ( 'NONE', *, *, #178797, .T. ) ;
#152325 = DIRECTION ( 'NONE',  ( -1.000000000000000000, 0.000000000000000000, -0.000000000000000000 ) ) ;
#152326 = CARTESIAN_POINT ( 'NONE',  ( 21.05000000000000071, 40.18490544642472173, -251.4399342103543233 ) ) ;
#152327 = CARTESIAN_POINT ( 'NONE',  ( 23.14999999999999858, 67.23127455305835554, -235.8551265064784559 ) ) ;
#152328 = CARTESIAN_POINT ( 'NONE',  ( 20.94999999999999929, 67.12338541492479749, -94.63802700567968884 ) ) ;
#152329 = CIRCLE ( 'NONE', #235480, 0.09999999999998898659 ) ;
#152330 = ADVANCED_FACE ( 'NONE', ( #109679 ), #224637, .T. ) ;
#152331 = VERTEX_POINT ( 'NONE', #93968 ) ;
#152332 = CARTESIAN_POINT ( 'NONE',  ( 18.59999999999999787, -9.749999999999994671, 30.00000000000000000 ) ) ;
#152333 = AXIS2_PLACEMENT_3D ( 'NONE', #52282, #229663, #211387 ) ;
#152334 = CONTEXT_DEPENDENT_SHAPE_REPRESENTATION ( #122458, #183007 ) ;
#152335 = VECTOR ( 'NONE', #186714, 1000.000000000000000 ) ;
#152336 = AXIS2_PLACEMENT_3D ( 'NONE', #212793, #191965, #249355 ) ;
#152337 = CARTESIAN_POINT ( 'NONE',  ( 21.05000000000000071, 76.00000000001237765, -170.0231074845243597 ) ) ;
#152338 = ORIENTED_EDGE ( 'NONE', *, *, #246538, .T. ) ;
#152339 = DIRECTION ( 'NONE',  ( 1.000000000000000000, 0.000000000000000000, 0.000000000000000000 ) ) ;
#152340 = DIRECTION ( 'NONE',  ( 0.000000000000000000, 1.000000000000000000, 0.000000000000000000 ) ) ;
#152341 = ORIENTED_EDGE ( 'NONE', *, *, #189999, .T. ) ;
#152344 = ORIENTED_EDGE ( 'NONE', *, *, #80419, .T. ) ;
#152343 = CIRCLE ( 'NONE', #39909, 0.1000000000000028644 ) ;
#152342 = CARTESIAN_POINT ( 'NONE',  ( -18.40000000000000213, 64.52683809664910086, -56.87310748452440379 ) ) ;
#152345 = ORIENTED_EDGE ( 'NONE', *, *, #119400, .T. ) ;
#152346 = CARTESIAN_POINT ( 'NONE',  ( -20.85000000000000142, -1.263275465206102233, -74.90186466674640542 ) ) ;
#152347 = AXIS2_PLACEMENT_3D ( 'NONE', #162940, #217736, #121268 ) ;
#152348 = FACE_OUTER_BOUND ( 'NONE', #41694, .T. ) ;
#152349 = DIRECTION ( 'NONE',  ( 0.000000000000000000, 0.000000000000000000, 1.000000000000000000 ) ) ;
#152350 = VECTOR ( 'NONE', #133061, 1000.000000000000114 ) ;
#152351 = DIRECTION ( 'NONE',  ( 0.000000000000000000, 0.000000000000000000, 1.000000000000000000 ) ) ;
#152352 = LINE ( 'NONE', #250140, #94454 ) ;
#152353 = DIRECTION ( 'NONE',  ( 0.000000000000000000, 1.000000000000000000, 0.000000000000000000 ) ) ;
#152354 = DIRECTION ( 'NONE',  ( 0.000000000000000000, -6.982962677686266711E-15, 1.000000000000000000 ) ) ;
#152356 = CARTESIAN_POINT ( 'NONE',  ( -20.54999999999999716, 23.49882452903949925, -253.1653563615082305 ) ) ;
#152355 = CARTESIAN_POINT ( 'NONE',  ( 20.95545211741311320, 65.41358668846794444, -95.43696062493610555 ) ) ;
#152357 = DIRECTION ( 'NONE',  ( -4.408576920032447972E-17, -0.1350103645451946055, 0.9908441862701591329 ) ) ;
#152358 = DIRECTION ( 'NONE',  ( 3.265361837132813093E-16, 1.000000000000000000, 6.982962677686266711E-15 ) ) ;
#152359 = CARTESIAN_POINT ( 'NONE',  ( -21.14999999999999858, 64.35000000001268461, -203.4231074845244507 ) ) ;
#152360 = DIRECTION ( 'NONE',  ( -0.000000000000000000, 0.1350103645451876666, -0.9908441862701600211 ) ) ;
#152361 = EDGE_LOOP ( 'NONE', ( #222716, #100190, #7898, #189362 ) ) ;
#152362 = CARTESIAN_POINT ( 'NONE',  ( -18.46919391072058758, -9.670724388277745831, -40.17380353179954255 ) ) ;
#152363 = DIRECTION ( 'NONE',  ( -1.000000000000000000, -0.000000000000000000, -0.000000000000000000 ) ) ;
#152364 = EDGE_CURVE ( 'NONE', #237399, #70987, #183156, .T. ) ;
#152365 = DIRECTION ( 'NONE',  ( -1.000000000000000000, -0.000000000000000000, -0.000000000000000000 ) ) ;
#152366 = FACE_OUTER_BOUND ( 'NONE', #177115, .T. ) ;
#152367 = DIRECTION ( 'NONE',  ( 1.000000000000000000, 0.000000000000000000, 0.000000000000000000 ) ) ;
#152368 = EDGE_CURVE ( 'NONE', #40380, #204366, #133084, .T. ) ;
#152369 = VERTEX_POINT ( 'NONE', #73167 ) ;
#152370 = AXIS2_PLACEMENT_3D ( 'NONE', #255615, #140864, #178737 ) ;
#152371 = SPHERICAL_SURFACE ( 'NONE', #151239, 0.1000000000000000056 ) ;
#152372 = ORIENTED_EDGE ( 'NONE', *, *, #83020, .F. ) ;
#152375 = ADVANCED_FACE ( 'NONE', ( #71868 ), #151407, .T. ) ;
#152374 = AXIS2_PLACEMENT_3D ( 'NONE', #123655, #238457, #164062 ) ;
#152373 = DIRECTION ( 'NONE',  ( 0.000000000000000000, 0.000000000000000000, -1.000000000000000000 ) ) ;
#152376 = DIRECTION ( 'NONE',  ( 0.000000000000000000, 0.000000000000000000, 1.000000000000000000 ) ) ;
#152377 = AXIS2_PLACEMENT_3D ( 'NONE', #135072, #252454, #115521 ) ;
#152378 = CIRCLE ( 'NONE', #202420, 0.1000000000000002554 ) ;
#152379 = ORIENTED_EDGE ( 'NONE', *, *, #251499, .F. ) ;
#152380 = DIRECTION ( 'NONE',  ( 0.000000000000000000, 0.9126074666063769270, 0.4088369013363280513 ) ) ;
#152381 = EDGE_CURVE ( 'NONE', #199264, #55215, #34046, .T. ) ;
#152382 = ORIENTED_EDGE ( 'NONE', *, *, #136249, .F. ) ;
#152384 = AXIS2_PLACEMENT_3D ( 'NONE', #40633, #21053, #254466 ) ;
#152383 = CARTESIAN_POINT ( 'NONE',  ( -16.87036670365549895, 9.989418819301647545, -12.52043988269794639 ) ) ;
#152386 = CIRCLE ( 'NONE', #73286, 0.1000000000000028644 ) ;
#152385 = DIRECTION ( 'NONE',  ( 0.000000000000000000, 0.6728388485993177515, -0.7397890806274072251 ) ) ;
#152388 = CARTESIAN_POINT ( 'NONE',  ( 20.94999999999999574, 0.000000000000000000, 0.000000000000000000 ) ) ;
#152387 = UNCERTAINTY_MEASURE_WITH_UNIT (LENGTH_MEASURE( 1.000000000000000082E-05 ), #172512, 'distance_accuracy_value', 'NONE');
#152389 = ADVANCED_FACE ( 'NONE', ( #193093 ), #53951, .T. ) ;
#152390 = LINE ( 'NONE', #154954, #33534 ) ;
#152391 = ADVANCED_FACE ( 'NONE', ( #173573 ), #233511, .T. ) ;
#152392 = CARTESIAN_POINT ( 'NONE',  ( 21.05000000000000071, -11.48912529306489994, -131.0000000000000284 ) ) ;
#152393 = DIRECTION ( 'NONE',  ( 0.000000000000000000, -0.1298341882520022694, -0.9915357197604853789 ) ) ;
#152394 = AXIS2_PLACEMENT_3D ( 'NONE', #149098, #206487, #129520 ) ;
#152395 = CARTESIAN_POINT ( 'NONE',  ( -23.25000000000000000, 4.150000000011156764, -121.6500000000000341 ) ) ;
#152396 = LINE ( 'NONE', #92379, #12210 ) ;
#152398 = ORIENTED_EDGE ( 'NONE', *, *, #229001, .T. ) ;
#152397 = DIRECTION ( 'NONE',  ( 1.000000000000000000, 0.000000000000000000, 0.000000000000000000 ) ) ;
#152399 = FACE_OUTER_BOUND ( 'NONE', #187096, .T. ) ;
#152400 = EDGE_LOOP ( 'NONE', ( #200122, #49179, #192473, #77153 ) ) ;
#152402 = ORIENTED_EDGE ( 'NONE', *, *, #185409, .T. ) ;
#152401 = CARTESIAN_POINT ( 'NONE',  ( -21.05000000000000071, -11.29603075032412995, -70.04789915966391334 ) ) ;
#152403 = ORIENTED_EDGE ( 'NONE', *, *, #17368, .T. ) ;
#152404 = DIRECTION ( 'NONE',  ( -0.000000000000000000, -0.000000000000000000, -1.000000000000000000 ) ) ;
#152405 = CARTESIAN_POINT ( 'NONE',  ( 20.85000000000000142, 77.75000000001134026, -24.40415744590205804 ) ) ;
#152406 = ADVANCED_FACE ( 'NONE', ( #187955 ), #9307, .T. ) ;
#152407 = CARTESIAN_POINT ( 'NONE',  ( 22.40736611211992368, 76.00000000001173817, -81.17267829206912211 ) ) ;
#152408 = CARTESIAN_POINT ( 'NONE',  ( 21.05000000000000071, 86.32947205150912851, -209.3293116780858156 ) ) ;
#152410 = DIRECTION ( 'NONE',  ( -0.000000000000000000, -0.9126074666063770380, -0.4088369013363281068 ) ) ;
#152409 = VECTOR ( 'NONE', #166616, 1000.000000000000000 ) ;
#152411 = EDGE_CURVE ( 'NONE', #116858, #57931, #8182, .T. ) ;
#152412 = ADVANCED_FACE ( 'NONE', ( #15762 ), #79528, .F. ) ;
#152413 = CARTESIAN_POINT ( 'NONE',  ( -16.87036670365549540, 12.42497885867826568, -211.1079079717509046 ) ) ;
#152414 = DIRECTION ( 'NONE',  ( 1.441126678808781001E-14, -0.9876197685951241256, -0.1568667991644932258 ) ) ;
#152415 = ORIENTED_EDGE ( 'NONE', *, *, #74318, .T. ) ;
#152416 = ORIENTED_EDGE ( 'NONE', *, *, #111278, .T. ) ;
#152417 = DIRECTION ( 'NONE',  ( -1.000000000000000000, 0.000000000000000000, -0.000000000000000000 ) ) ;
#152418 = VECTOR ( 'NONE', #170894, 1000.000000000000000 ) ;
#152419 = VECTOR ( 'NONE', #4971, 1000.000000000000114 ) ;
#152420 = VERTEX_POINT ( 'NONE', #219046 ) ;
#152421 = VECTOR ( 'NONE', #235116, 1000.000000000000000 ) ;
#152423 = PLANE ( 'NONE',  #234047 ) ;
#152422 = CIRCLE ( 'NONE', #35884, 0.1000000000000028644 ) ;
#152424 = ORIENTED_EDGE ( 'NONE', *, *, #6445, .F. ) ;
#152425 = CARTESIAN_POINT ( 'NONE',  ( 18.33683296300432986, -9.511149971132869752, -40.40570741271005062 ) ) ;
#152426 = ADVANCED_FACE ( 'NONE', ( #95262 ), #119996, .T. ) ;
#152427 = CARTESIAN_POINT ( 'NONE',  ( 23.14999999999999858, 1.115600667400684642E-11, -33.50000000000000000 ) ) ;
#152428 = DIRECTION ( 'NONE',  ( 0.000000000000000000, 0.8700118002898322711, -0.4930308989875231140 ) ) ;
#152429 = EDGE_CURVE ( 'NONE', #57698, #186207, #174821, .T. ) ;
#152430 = CARTESIAN_POINT ( 'NONE',  ( 21.14999999999999858, 60.91865828504416669, -234.1430899377568267 ) ) ;
#152431 = CARTESIAN_POINT ( 'NONE',  ( -20.94999999999999929, 76.00000000001213607, -136.5231074845243313 ) ) ;
#152432 = ORIENTED_EDGE ( 'NONE', *, *, #243975, .F. ) ;
#152433 = CARTESIAN_POINT ( 'NONE',  ( -18.49372193242257012, -9.442484523346656999, -207.7647812600339989 ) ) ;
#152434 = CARTESIAN_POINT ( 'NONE',  ( 23.24999999999999289, 4.150000000011154988, -67.00000000000004263 ) ) ;
#152435 = EDGE_CURVE ( 'NONE', #18582, #136324, #95810, .T. ) ;
#152436 = DIRECTION ( 'NONE',  ( 0.000000000000000000, 0.000000000000000000, -1.000000000000000000 ) ) ;
#152437 = AXIS2_PLACEMENT_3D ( 'NONE', #222462, #234685, #114740 ) ;
#152438 = DIRECTION ( 'NONE',  ( 0.000000000000000000, 0.000000000000000000, 1.000000000000000000 ) ) ;
#152439 = ORIENTED_EDGE ( 'NONE', *, *, #163402, .T. ) ;
#152440 = VECTOR ( 'NONE', #215108, 1000.000000000000000 ) ;
#152442 = DIRECTION ( 'NONE',  ( -1.000000000000000000, -2.952720810173289112E-16, 0.000000000000000000 ) ) ;
#152441 = CARTESIAN_POINT ( 'NONE',  ( -21.05000000000000071, 1.250000000011155299, -41.50000000000000000 ) ) ;
#152443 = VERTEX_POINT ( 'NONE', #237349 ) ;
#152446 = EDGE_LOOP ( 'NONE', ( #90905, #53117, #23804, #231382 ) ) ;
#152445 = CARTESIAN_POINT ( 'NONE',  ( 21.05000000000000071, 69.19063053712525857, -247.5666987377248631 ) ) ;
#152444 = FACE_OUTER_BOUND ( 'NONE', #204114, .T. ) ;
#152447 = CARTESIAN_POINT ( 'NONE',  ( -23.25000000000000000, 6.933893972137497030, -104.2856458343736250 ) ) ;
#152448 = DIRECTION ( 'NONE',  ( 1.000000000000000000, -0.000000000000000000, -0.000000000000000000 ) ) ;
#152449 = AXIS2_PLACEMENT_3D ( 'NONE', #218389, #136273, #176736 ) ;
#152450 = VERTEX_POINT ( 'NONE', #17028 ) ;
#152451 = DIRECTION ( 'NONE',  ( 1.000000000000000000, 0.000000000000000000, 0.000000000000000000 ) ) ;
#152452 = CARTESIAN_POINT ( 'NONE',  ( 23.25000000000000000, -8.596261682231833845, -42.95012751715027832 ) ) ;
#152453 = CARTESIAN_POINT ( 'NONE',  ( 20.85000000000000142, 6.846123162363745074, -104.2377262668499043 ) ) ;
#152455 = EDGE_LOOP ( 'NONE', ( #91842, #185749 ) ) ;
#152454 = PLANE ( 'NONE',  #189192 ) ;
#152456 = EDGE_CURVE ( 'NONE', #25147, #134587, #233238, .T. ) ;
#152457 = ORIENTED_EDGE ( 'NONE', *, *, #125913, .T. ) ;
#152458 = EDGE_CURVE ( 'NONE', #138430, #199092, #75020, .T. ) ;
#152459 = CARTESIAN_POINT ( 'NONE',  ( -21.04999999999999716, 78.33723480602354527, -231.5810597241785729 ) ) ;
#152460 = CARTESIAN_POINT ( 'NONE',  ( 22.10000000000000497, 11.99999999999999822, 12.00000000000000000 ) ) ;
#152461 = AXIS2_PLACEMENT_3D ( 'NONE', #182965, #146365, #83801 ) ;
#152462 = DIRECTION ( 'NONE',  ( 0.000000000000000000, 0.9752329468386375932, 0.2211802418852714114 ) ) ;
#152463 = ORIENTED_EDGE ( 'NONE', *, *, #20164, .T. ) ;
#152464 = CARTESIAN_POINT ( 'NONE',  ( -21.65000000000000213, 7.249999999999983125, -12.65000000000000213 ) ) ;
#152465 = EDGE_CURVE ( 'NONE', #135871, #114955, #129176, .T. ) ;
#152466 = EDGE_CURVE ( 'NONE', #103588, #219544, #62530, .T. ) ;
#152467 = CARTESIAN_POINT ( 'NONE',  ( -22.39999999999999858, 0.1000000000111554016, -59.20922040162664501 ) ) ;
#152468 = CARTESIAN_POINT ( 'NONE',  ( 18.60000000000000142, -9.321008403350125704, -141.2359382490778899 ) ) ;
#152469 = ORIENTED_EDGE ( 'NONE', *, *, #115052, .F. ) ;
#152470 = CARTESIAN_POINT ( 'NONE',  ( 20.21494484322227692, 60.43554925037637560, -225.3705126911073648 ) ) ;
#152471 = EDGE_CURVE ( 'NONE', #140343, #180772, #76977, .T. ) ;
#152472 = FACE_OUTER_BOUND ( 'NONE', #24870, .T. ) ;
#152473 = ORIENTED_EDGE ( 'NONE', *, *, #159107, .F. ) ;
#152474 = CIRCLE ( 'NONE', #185760, 0.1000000000000055844 ) ;
#152475 = DIRECTION ( 'NONE',  ( 0.000000000000000000, 0.000000000000000000, -1.000000000000000000 ) ) ;
#152476 = COLOUR_RGB ( '', 0.08235294, 0.09019608, 0.10196078) ;
#152477 = AXIS2_PLACEMENT_3D ( 'NONE', #122149, #102537, #41351 ) ;
#152478 = AXIS2_PLACEMENT_3D ( 'NONE', #66205, #244825, #221396 ) ;
#152479 = ADVANCED_FACE ( 'NONE', ( #195678 ), #117395, .F. ) ;
#152480 = VERTEX_POINT ( 'NONE', #136952 ) ;
#152481 = ORIENTED_EDGE ( 'NONE', *, *, #215097, .T. ) ;
#152482 = EDGE_CURVE ( 'NONE', #207656, #49547, #162494, .T. ) ;
#152483 = MECHANICAL_DESIGN_GEOMETRIC_PRESENTATION_REPRESENTATION (  '', ( #160686 ), #48212 ) ;
#152484 = CARTESIAN_POINT ( 'NONE',  ( -20.64999999999999858, 68.75000000001185185, -90.77310748452435973 ) ) ;
#152485 = ORIENTED_EDGE ( 'NONE', *, *, #117136, .F. ) ;
#152487 = ORIENTED_EDGE ( 'NONE', *, *, #245743, .T. ) ;
#152486 = DIRECTION ( 'NONE',  ( 0.000000000000000000, -6.467318590049456648E-15, 1.000000000000000000 ) ) ;
#152488 = ADVANCED_FACE ( 'NONE', ( #177401 ), #158234, .T. ) ;
#152489 = ORIENTED_EDGE ( 'NONE', *, *, #35201, .T. ) ;
#152492 = VERTEX_POINT ( 'NONE', #199521 ) ;
#152491 = EDGE_LOOP ( 'NONE', ( #251387, #56846, #397, #56812 ) ) ;
#152490 = DIRECTION ( 'NONE',  ( -1.000000000000000000, -0.000000000000000000, -0.000000000000000000 ) ) ;
#152493 = PLANE ( 'NONE',  #77345 ) ;
#152494 = ORIENTED_EDGE ( 'NONE', *, *, #11081, .F. ) ;
#152495 = DIRECTION ( 'NONE',  ( 2.933373889701419960E-15, -0.8164989248600479366, 0.5773469543544730298 ) ) ;
#152496 = CARTESIAN_POINT ( 'NONE',  ( -20.54999999999999716, 23.94791789707936758, -237.8074276425068661 ) ) ;
#152497 = EDGE_CURVE ( 'NONE', #176243, #57243, #50048, .T. ) ;
#152498 = ADVANCED_FACE ( 'NONE', ( #179948 ), #1278, .T. ) ;
#152499 = AXIS2_PLACEMENT_3D ( 'NONE', #211359, #191819, #173560 ) ;
#152500 = CARTESIAN_POINT ( 'NONE',  ( -18.50000000000000000, 76.00000000001213607, -136.5231074845243313 ) ) ;
#152501 = DIRECTION ( 'NONE',  ( -1.000000000000000000, 0.000000000000000000, 0.000000000000000000 ) ) ;
#152502 = DIRECTION ( 'NONE',  ( 0.000000000000000000, 0.8660254037844378194, 0.5000000000000016653 ) ) ;
#152504 = VERTEX_POINT ( 'NONE', #35332 ) ;
#152503 = CIRCLE ( 'NONE', #173369, 11.74999999999999645 ) ;
#152505 = ORIENTED_EDGE ( 'NONE', *, *, #182181, .T. ) ;
#152506 = ORIENTED_EDGE ( 'NONE', *, *, #86643, .F. ) ;
#152507 = EDGE_CURVE ( 'NONE', #127256, #206286, #208278, .T. ) ;
#152508 = FACE_OUTER_BOUND ( 'NONE', #19511, .T. ) ;
#152510 = ORIENTED_EDGE ( 'NONE', *, *, #113093, .F. ) ;
#152509 = CARTESIAN_POINT ( 'NONE',  ( -18.59999999999999787, 0.000000000000000000, -33.50000000000000000 ) ) ;
#152512 = DIRECTION ( 'NONE',  ( -3.265361837132813093E-16, 1.000000000000000000, 0.000000000000000000 ) ) ;
#152511 = AXIS2_PLACEMENT_3D ( 'NONE', #13178, #190546, #250484 ) ;
#152513 = VERTEX_POINT ( 'NONE', #3866 ) ;
#152514 = EDGE_LOOP ( 'NONE', ( #120131, #57796, #10278, #212390 ) ) ;
#152515 = EDGE_CURVE ( 'NONE', #225500, #4224, #127657, .T. ) ;
#152516 = CYLINDRICAL_SURFACE ( 'NONE', #187849, 0.09999999999999939493 ) ;
#152517 = CIRCLE ( 'NONE', #177463, 0.1999999999999987899 ) ;
#152518 = AXIS2_PLACEMENT_3D ( 'NONE', #63980, #183925, #84785 ) ;
#152519 = EDGE_CURVE ( 'NONE', #187777, #38637, #27323, .T. ) ;
#152520 = VERTEX_POINT ( 'NONE', #203355 ) ;
#152521 = FACE_OUTER_BOUND ( 'NONE', #172413, .T. ) ;
#152522 = CARTESIAN_POINT ( 'NONE',  ( -16.97683809663752186, 66.05000000001210481, -127.2731074845243597 ) ) ;
#152525 = VERTEX_POINT ( 'NONE', #87233 ) ;
#152524 = ORIENTED_EDGE ( 'NONE', *, *, #227097, .T. ) ;
#152523 = CIRCLE ( 'NONE', #131638, 0.5000000000000004441 ) ;
#152526 = ORIENTED_EDGE ( 'NONE', *, *, #30056, .F. ) ;
#152527 = CARTESIAN_POINT ( 'NONE',  ( 18.59999999999999432, 77.83585931145526615, -58.01866831572577610 ) ) ;
#152528 = CIRCLE ( 'NONE', #40096, 0.09999999999999939493 ) ;
#152529 = VERTEX_POINT ( 'NONE', #66410 ) ;
#152530 = AXIS2_PLACEMENT_3D ( 'NONE', #58315, #38789, #19218 ) ;
#152531 = ORIENTED_EDGE ( 'NONE', *, *, #219729, .F. ) ;
#152532 = DIRECTION ( 'NONE',  ( -1.000000000000000000, 0.000000000000000000, 0.000000000000000000 ) ) ;
#152534 = VERTEX_POINT ( 'NONE', #243760 ) ;
#152533 = DIRECTION ( 'NONE',  ( 0.000000000000000000, -0.2128009952263485993, 0.9770955615653341697 ) ) ;
#152535 = EDGE_CURVE ( 'NONE', #184016, #23909, #120809, .T. ) ;
#152536 = DIRECTION ( 'NONE',  ( 0.000000000000000000, -0.2617529984165152257, -0.9651348961777124202 ) ) ;
#152537 = AXIS2_PLACEMENT_3D ( 'NONE', #133848, #36051, #191290 ) ;
#152539 = CARTESIAN_POINT ( 'NONE',  ( -20.64999999999999858, 7.128833340093095217, -233.7327013124392749 ) ) ;
#152538 = DIRECTION ( 'NONE',  ( 0.000000000000000000, 0.1568667991644863147, 0.9876197685951252359 ) ) ;
#152540 = CARTESIAN_POINT ( 'NONE',  ( 21.05000000000000071, 62.99095723518624368, -207.1734234082435080 ) ) ;
#152541 = DIRECTION ( 'NONE',  ( 1.000000000000000000, -1.646408749285562060E-14, -1.073024830501232702E-15 ) ) ;
#152542 = ORIENTED_EDGE ( 'NONE', *, *, #247247, .F. ) ;
#152543 = VERTEX_POINT ( 'NONE', #41730 ) ;
#152544 = CARTESIAN_POINT ( 'NONE',  ( 18.52326479938722059, 85.64236444492735245, -96.30835007111858204 ) ) ;
#152545 = EDGE_CURVE ( 'NONE', #92740, #86390, #89744, .T. ) ;
#152546 = CARTESIAN_POINT ( 'NONE',  ( 23.15000000000000213, 84.66355140188075268, -59.99900636645695329 ) ) ;
#152547 = DIRECTION ( 'NONE',  ( -1.000000000000000000, 1.560919790631901733E-14, -5.345137975828415463E-15 ) ) ;
#152548 = AXIS2_PLACEMENT_3D ( 'NONE', #126810, #189359, #169832 ) ;
#152549 = VERTEX_POINT ( 'NONE', #46820 ) ;
#152550 = CARTESIAN_POINT ( 'NONE',  ( -16.94445028196807002, 30.26380394232451465, -234.7901145182196956 ) ) ;
#152551 = DIRECTION ( 'NONE',  ( 0.000000000000000000, 0.000000000000000000, -1.000000000000000000 ) ) ;
#152552 = DIRECTION ( 'NONE',  ( -0.7071067811865475727, 0.7071067811865475727, 4.937700262164531476E-15 ) ) ;
#152553 = VERTEX_POINT ( 'NONE', #186368 ) ;
#152554 = ORIENTED_EDGE ( 'NONE', *, *, #232314, .F. ) ;
#152555 = CARTESIAN_POINT ( 'NONE',  ( -20.64999999999999858, -7.079251802663312887, -212.6676826711374417 ) ) ;
#152556 = EDGE_CURVE ( 'NONE', #131991, #135464, #245885, .T. ) ;
#152557 = DIRECTION ( 'NONE',  ( 0.000000000000000000, 0.8814952561688430555, -0.4721928772777346239 ) ) ;
#152558 = ORIENTED_EDGE ( 'NONE', *, *, #253155, .F. ) ;
#152559 = DIRECTION ( 'NONE',  ( 1.000000000000000000, -0.000000000000000000, -0.000000000000000000 ) ) ;
#152561 = EDGE_LOOP ( 'NONE', ( #56373, #25838, #106897, #142485 ) ) ;
#152560 = APPLICATION_CONTEXT ( 'automotive_design' ) ;
#152562 = CARTESIAN_POINT ( 'NONE',  ( 18.50000000000000355, -9.399999999988841282, -140.8820418481727188 ) ) ;
#152564 = CARTESIAN_POINT ( 'NONE',  ( -21.65000000000000213, 68.29142135624888965, -57.17310748452437963 ) ) ;
#152563 = LINE ( 'NONE', #234630, #24068 ) ;
#152565 = AXIS2_PLACEMENT_3D ( 'NONE', #134110, #192831, #72908 ) ;
#152566 = CARTESIAN_POINT ( 'NONE',  ( 20.94999999999999929, 5.850000000000001421, -23.36750277572207679 ) ) ;
#152567 = AXIS2_PLACEMENT_3D ( 'NONE', #123789, #7701, #246302 ) ;
#152568 = CARTESIAN_POINT ( 'NONE',  ( 20.73486653747088582, 7.250000000011182166, -188.3499999999999659 ) ) ;
#152569 = VECTOR ( 'NONE', #111813, 1000.000000000000000 ) ;
#152570 = CIRCLE ( 'NONE', #177511, 0.1999999999999987899 ) ;
#152572 = ORIENTED_EDGE ( 'NONE', *, *, #34208, .T. ) ;
#152571 = DIRECTION ( 'NONE',  ( 0.7071067811865476838, -0.2890913453342132122, 0.6453109281988448354 ) ) ;
#152573 = ADVANCED_FACE ( 'NONE', ( #224186 ), #183329, .F. ) ;
#152574 = VECTOR ( 'NONE', #191957, 1000.000000000000000 ) ;
#152576 = ORIENTED_EDGE ( 'NONE', *, *, #196291, .F. ) ;
#152575 = ORIENTED_EDGE ( 'NONE', *, *, #193660, .T. ) ;
#152577 = ORIENTED_EDGE ( 'NONE', *, *, #199555, .F. ) ;
#152578 = CARTESIAN_POINT ( 'NONE',  ( -22.94999999999999929, 6.322468214605804882, 12.11686199900910488 ) ) ;
#152579 = DIRECTION ( 'NONE',  ( 0.000000000000000000, 0.2617529984165152257, 0.9651348961777124202 ) ) ;
#152580 = AXIS2_PLACEMENT_3D ( 'NONE', #33263, #112766, #55318 ) ;
#152582 = FACE_OUTER_BOUND ( 'NONE', #110328, .T. ) ;
#152581 = LINE ( 'NONE', #110847, #220409 ) ;
#152583 = DIRECTION ( 'NONE',  ( 0.000000000000000000, 0.000000000000000000, -1.000000000000000000 ) ) ;
#152584 = VERTEX_POINT ( 'NONE', #22167 ) ;
#152585 = DIRECTION ( 'NONE',  ( 0.000000000000000000, -1.000000000000000000, -6.860497997771531562E-15 ) ) ;
#152586 = TOROIDAL_SURFACE ( 'NONE', #85877, 3.899999999999999467, 0.1000000000000000056 ) ;
#152587 = ORIENTED_EDGE ( 'NONE', *, *, #228009, .F. ) ;
#152588 = ORIENTED_EDGE ( 'NONE', *, *, #72815, .F. ) ;
#152589 = CARTESIAN_POINT ( 'NONE',  ( -21.05000000000000071, 69.45934304831041572, -69.42310748452437963 ) ) ;
#152590 = CIRCLE ( 'NONE', #19267, 0.1999999999999987899 ) ;
#152591 = CARTESIAN_POINT ( 'NONE',  ( -22.42253884134832020, 0.001932351146464885046, -88.85039430265160831 ) ) ;
#152592 = CARTESIAN_POINT ( 'NONE',  ( -21.05000000000000071, 1.622572661696384477, -230.6714771550894056 ) ) ;
#152593 = LINE ( 'NONE', #194283, #193132 ) ;
#152594 = DIRECTION ( 'NONE',  ( -0.000000000000000000, 0.09425075112713271475, 0.9955484899852801162 ) ) ;
#152595 = EDGE_LOOP ( 'NONE', ( #38018, #33186, #12699, #12119 ) ) ;
#152596 = EDGE_LOOP ( 'NONE', ( #188468, #203883, #5649, #214369 ) ) ;
#152597 = CARTESIAN_POINT ( 'NONE',  ( -23.25000000000000000, 76.00000000001213607, -136.5231074845242745 ) ) ;
#152598 = DIRECTION ( 'NONE',  ( 0.7071359030027593029, 0.000000000000000000, -0.7070776581709197206 ) ) ;
#152599 = CIRCLE ( 'NONE', #106752, 12.77499999999999503 ) ;
#152600 = DIRECTION ( 'NONE',  ( 0.000000000000000000, 0.000000000000000000, -1.000000000000000000 ) ) ;
#152601 = CARTESIAN_POINT ( 'NONE',  ( -18.59999999999999787, 18.26942912180536638, -237.6183358664095238 ) ) ;
#152602 = LINE ( 'NONE', #212558, #152440 ) ;
#152603 = CARTESIAN_POINT ( 'NONE',  ( 23.40000000000005542, 74.16448838626247664, -47.52760213295649550 ) ) ;
#152604 = CARTESIAN_POINT ( 'NONE',  ( -21.05000000000000071, 74.26374286841418382, -57.95445515550683524 ) ) ;
#152605 = CARTESIAN_POINT ( 'NONE',  ( -17.11825945287481332, 66.05000000001224691, -149.2731074845244450 ) ) ;
#152607 = DIRECTION ( 'NONE',  ( -1.073024830501117725E-15, 6.982962677686266711E-15, -1.000000000000000000 ) ) ;
#152606 = LINE ( 'NONE', #133022, #236937 ) ;
#152609 = ADVANCED_FACE ( 'NONE', ( #142081 ), #224824, .T. ) ;
#152608 = LINE ( 'NONE', #212564, #12533 ) ;
#152610 = CARTESIAN_POINT ( 'NONE',  ( -20.85000000000000142, 11.75000000001115552, -134.0000000000000284 ) ) ;
#152611 = CARTESIAN_POINT ( 'NONE',  ( 23.14999999999998437, -11.75000000000000000, 3.469446951953614189E-15 ) ) ;
#152612 = CARTESIAN_POINT ( 'NONE',  ( 20.85882249326303040, 10.33248238083634796, -139.5948465439131780 ) ) ;
#152615 = VERTEX_POINT ( 'NONE', #122545 ) ;
#152614 = CIRCLE ( 'NONE', #73502, 0.1000000000000028644 ) ;
#152613 = DIRECTION ( 'NONE',  ( 0.000000000000000000, 0.000000000000000000, -1.000000000000000000 ) ) ;
#152616 = CIRCLE ( 'NONE', #198359, 0.1000000000000073330 ) ;
#152617 = CIRCLE ( 'NONE', #2714, 0.09999999999998898659 ) ;
#152618 = ADVANCED_FACE ( 'NONE', ( #222900 ), #43002, .F. ) ;
#152619 = DIRECTION ( 'NONE',  ( 0.000000000000000000, 0.000000000000000000, -1.000000000000000000 ) ) ;
#152620 = ADVANCED_FACE ( 'NONE', ( #105495 ), #6425, .F. ) ;
#152621 = FACE_OUTER_BOUND ( 'NONE', #173388, .T. ) ;
#152622 = CARTESIAN_POINT ( 'NONE',  ( 21.07928932188134397, 0.09889514566555242248, -60.67148334360673800 ) ) ;
#152623 = VECTOR ( 'NONE', #129804, 1000.000000000000000 ) ;
#152624 = CARTESIAN_POINT ( 'NONE',  ( 15.74999999999999645, 9.350000000011139178, -83.75000000000004263 ) ) ;
#152625 = CARTESIAN_POINT ( 'NONE',  ( 21.04142135623731136, 6.223900101154154818, 12.00000000000000000 ) ) ;
#152626 = AXIS2_PLACEMENT_3D ( 'NONE', #66616, #173476, #133018 ) ;
#152627 = CIRCLE ( 'NONE', #11126, 0.09999999999999868716 ) ;
#152628 = EDGE_CURVE ( 'NONE', #155749, #249694, #165522, .T. ) ;
#152629 = CARTESIAN_POINT ( 'NONE',  ( 20.94999999999999929, -11.48912529306489994, -97.40000000000004832 ) ) ;
#152630 = CARTESIAN_POINT ( 'NONE',  ( 21.10000000000000142, 0.000000000000000000, 0.000000000000000000 ) ) ;
#152631 = DIRECTION ( 'NONE',  ( 1.000000000000000000, -0.000000000000000000, -0.000000000000000000 ) ) ;
#152632 = ADVANCED_FACE ( 'NONE', ( #82088 ), #79828, .F. ) ;
#152633 = VECTOR ( 'NONE', #200789, 1000.000000000000000 ) ;
#152635 = ORIENTED_EDGE ( 'NONE', *, *, #133098, .T. ) ;
#152634 = ADVANCED_FACE ( 'NONE', ( #230627, #53267, #207218 ), #51953, .F. ) ;
#152636 = CARTESIAN_POINT ( 'NONE',  ( -23.25000000000000000, 11.65000000001115588, -112.6500000000000483 ) ) ;
#152638 = ORIENTED_EDGE ( 'NONE', *, *, #24891, .F. ) ;
#152637 = FACE_OUTER_BOUND ( 'NONE', #114929, .T. ) ;
#152639 = LINE ( 'NONE', #110908, #63214 ) ;
#152640 = ADVANCED_FACE ( 'NONE', ( #12878 ), #228053, .T. ) ;
#152641 = DIRECTION ( 'NONE',  ( 1.000000000000000000, 0.000000000000000000, 0.000000000000000000 ) ) ;
#152642 = ORIENTED_EDGE ( 'NONE', *, *, #231288, .T. ) ;
#152643 = CARTESIAN_POINT ( 'NONE',  ( -16.80891096016297226, 66.05000000001261640, -190.8907702917946096 ) ) ;
#152644 = APPLICATION_PROTOCOL_DEFINITION ( 'draft international standard', 'automotive_design', 1998, #242380 ) ;
#152645 = CYLINDRICAL_SURFACE ( 'NONE', #215039, 0.09999999999999939493 ) ;
#152647 = EDGE_CURVE ( 'NONE', #98041, #248715, #99898, .T. ) ;
#152646 = DIRECTION ( 'NONE',  ( 1.000000000000000000, -0.000000000000000000, 0.000000000000000000 ) ) ;
#152648 = ORIENTED_EDGE ( 'NONE', *, *, #118369, .F. ) ;
#152649 = DIRECTION ( 'NONE',  ( 0.000000000000000000, 6.997203936713175802E-15, -1.000000000000000000 ) ) ;
#152650 = DIRECTION ( 'NONE',  ( 0.000000000000000000, 0.000000000000000000, -1.000000000000000000 ) ) ;
#152651 = AXIS2_PLACEMENT_3D ( 'NONE', #126523, #22311, #160541 ) ;
#152652 = CYLINDRICAL_SURFACE ( 'NONE', #3555, 11.80000000000000959 ) ;
#152653 = EDGE_LOOP ( 'NONE', ( #208663, #51033, #56987, #14403 ) ) ;
#152654 = ORIENTED_EDGE ( 'NONE', *, *, #152657, .T. ) ;
#152655 = AXIS2_PLACEMENT_3D ( 'NONE', #138741, #179224, #81343 ) ;
#152656 = LINE ( 'NONE', #93929, #46459 ) ;
#152657 = EDGE_CURVE ( 'NONE', #104063, #63323, #25124, .T. ) ;
#152658 = CYLINDRICAL_SURFACE ( 'NONE', #182063, 0.5000000000000004441 ) ;
#152659 = CARTESIAN_POINT ( 'NONE',  ( -21.14999999999999858, -0.09999999998884338825, -27.25000000000000355 ) ) ;
#152660 = DIRECTION ( 'NONE',  ( 0.000000000000000000, 0.8814952561688437216, -0.4721928772777334582 ) ) ;
#152663 = LINE ( 'NONE', #130488, #232697 ) ;
#152662 = AXIS2_PLACEMENT_3D ( 'NONE', #223167, #44555, #53531 ) ;
#152661 = CARTESIAN_POINT ( 'NONE',  ( 23.15000000000000213, -11.64999999998884483, -67.00000000000004263 ) ) ;
#152664 = CARTESIAN_POINT ( 'NONE',  ( -21.08134388332232589, 75.92418108250545572, -176.3577880650423140 ) ) ;
#152665 = CARTESIAN_POINT ( 'NONE',  ( 23.14999999999999503, 11.65000000001116298, -155.3500000000000227 ) ) ;
#152666 = CARTESIAN_POINT ( 'NONE',  ( -20.94999999999999929, 40.18490544642472173, -251.4399342103543233 ) ) ;
#152667 = CARTESIAN_POINT ( 'NONE',  ( -18.50000000000000355, 47.07326788871597500, -255.0992659944397758 ) ) ;
#152668 = AXIS2_PLACEMENT_3D ( 'NONE', #125685, #243061, #226037 ) ;
#152669 = ORIENTED_EDGE ( 'NONE', *, *, #7426, .T. ) ;
#152670 = AXIS2_PLACEMENT_3D ( 'NONE', #163715, #181997, #244518 ) ;
#152672 = ORIENTED_EDGE ( 'NONE', *, *, #34128, .T. ) ;
#152671 = DIRECTION ( 'NONE',  ( 0.000000000000000000, -1.000000000000000000, 0.000000000000000000 ) ) ;
#152673 = CARTESIAN_POINT ( 'NONE',  ( -18.59999999999999787, 9.250000000000001776, -12.34999999999999964 ) ) ;
#152674 = LINE ( 'NONE', #69268, #224148 ) ;
#152676 = CARTESIAN_POINT ( 'NONE',  ( -21.14999999999999858, 11.75000000001115552, -167.5999999999999659 ) ) ;
#152675 = DIRECTION ( 'NONE',  ( 1.000000000000000000, -0.000000000000000000, -0.000000000000000000 ) ) ;
#152677 =( GEOMETRIC_REPRESENTATION_CONTEXT ( 3 ) GLOBAL_UNCERTAINTY_ASSIGNED_CONTEXT ( ( #136626 ) ) GLOBAL_UNIT_ASSIGNED_CONTEXT ( ( #169937, #26540, #9518 ) ) REPRESENTATION_CONTEXT ( 'NONE', 'WORKASPACE' ) );
#152678 = EDGE_CURVE ( 'NONE', #231071, #250167, #251456, .T. ) ;
#152679 = ORIENTED_EDGE ( 'NONE', *, *, #176150, .F. ) ;
#152680 = CYLINDRICAL_SURFACE ( 'NONE', #68359, 0.09999999999999939493 ) ;
#152681 = DIRECTION ( 'NONE',  ( -0.000000000000000000, -0.1332476588733589318, -0.9910827722268049644 ) ) ;
#152682 = CARTESIAN_POINT ( 'NONE',  ( 22.48970261584622321, 11.65000000001115588, -133.9446305117826341 ) ) ;
#152683 = CARTESIAN_POINT ( 'NONE',  ( 12.48201962039795987, 12.91318972656261188, -216.2290661304645596 ) ) ;
#152684 = ORIENTED_EDGE ( 'NONE', *, *, #53676, .T. ) ;
#152685 = VERTEX_POINT ( 'NONE', #70291 ) ;
#152686 = DIRECTION ( 'NONE',  ( 0.000000000000000000, -1.000000000000000000, 0.000000000000000000 ) ) ;
#152687 = ORIENTED_EDGE ( 'NONE', *, *, #82999, .F. ) ;
#152688 = EDGE_CURVE ( 'NONE', #81117, #11734, #72858, .T. ) ;
#152689 = DIRECTION ( 'NONE',  ( -1.000000000000000000, -0.000000000000000000, -0.000000000000000000 ) ) ;
#152690 = EDGE_CURVE ( 'NONE', #120381, #174683, #54723, .T. ) ;
#152691 = DIRECTION ( 'NONE',  ( 1.000000000000000000, 0.000000000000000000, 0.000000000000000000 ) ) ;
#152692 = CIRCLE ( 'NONE', #156780, 0.09999999999999939493 ) ;
#152693 = DIRECTION ( 'NONE',  ( 0.000000000000000000, -0.4088369013363280513, 0.9126074666063769270 ) ) ;
#152694 = TOROIDAL_SURFACE ( 'NONE', #40259, 12.77499999999999858, 0.1000000000000000056 ) ;
#152696 = ORIENTED_EDGE ( 'NONE', *, *, #236392, .F. ) ;
#152695 = AXIS2_PLACEMENT_3D ( 'NONE', #212363, #131520, #113239 ) ;
#152697 = CARTESIAN_POINT ( 'NONE',  ( -20.85000000000000142, 69.06610602788553877, -99.23746165015076315 ) ) ;
#152698 = EDGE_CURVE ( 'NONE', #97226, #118710, #212382, .T. ) ;
#152699 = TOROIDAL_SURFACE ( 'NONE', #27800, 0.4000000000000009104, 0.1000000000000000056 ) ;
#152700 = DIRECTION ( 'NONE',  ( 1.000000000000000000, 0.000000000000000000, 0.000000000000000000 ) ) ;
#152701 = AXIS2_PLACEMENT_3D ( 'NONE', #12379, #90589, #91882 ) ;
#152702 = DIRECTION ( 'NONE',  ( 1.000000000000000000, 0.000000000000000000, 0.000000000000000000 ) ) ;
#152703 = EDGE_CURVE ( 'NONE', #236288, #181403, #4235, .T. ) ;
#152704 = CARTESIAN_POINT ( 'NONE',  ( 21.12642695952774119, 75.90109671682282055, -142.8987674065594717 ) ) ;
#152705 = EDGE_CURVE ( 'NONE', #152450, #180362, #208508, .T. ) ;
#152706 = DIRECTION ( 'NONE',  ( 1.000000000000000000, 2.885090398161910739E-16, 6.283419270304611573E-17 ) ) ;
#152708 = DIRECTION ( 'NONE',  ( -1.000000000000000000, -0.000000000000000000, -0.000000000000000000 ) ) ;
#152707 = CARTESIAN_POINT ( 'NONE',  ( -20.90000000000000213, 1.212568896937007645, -8.000000000000000000 ) ) ;
#152709 = CARTESIAN_POINT ( 'NONE',  ( -16.85697194749129224, 66.09145628588855459, -149.4581117521382509 ) ) ;
#152710 = EDGE_LOOP ( 'NONE', ( #22312, #10367, #12627, #80628 ) ) ;
#152712 = DIRECTION ( 'NONE',  ( 0.000000000000000000, -1.000000000000000000, 0.000000000000000000 ) ) ;
#152711 = CYLINDRICAL_SURFACE ( 'NONE', #15985, 1.749999999999998002 ) ;
#152713 = VERTEX_POINT ( 'NONE', #9000 ) ;
#152715 = ORIENTED_EDGE ( 'NONE', *, *, #56463, .T. ) ;
#152714 = CARTESIAN_POINT ( 'NONE',  ( 19.99999999999998934, 62.39550153362034735, -208.7959266050682459 ) ) ;
#152716 = CIRCLE ( 'NONE', #169474, 0.3999999999999952482 ) ;
#152717 = ORIENTED_EDGE ( 'NONE', *, *, #153644, .F. ) ;
#152718 = FACE_OUTER_BOUND ( 'NONE', #215790, .T. ) ;
#152719 = AXIS2_PLACEMENT_3D ( 'NONE', #39693, #35828, #234003 ) ;
#152720 = AXIS2_PLACEMENT_3D ( 'NONE', #98396, #174177, #58009 ) ;
#152721 = DIRECTION ( 'NONE',  ( 0.000000000000000000, 0.000000000000000000, -1.000000000000000000 ) ) ;
#152722 = EDGE_CURVE ( 'NONE', #170796, #153564, #141623, .T. ) ;
#152723 = CARTESIAN_POINT ( 'NONE',  ( 21.05000000000000071, 65.57661458509919328, -129.0310555606542664 ) ) ;
#152724 = ORIENTED_EDGE ( 'NONE', *, *, #195482, .T. ) ;
#152725 = CARTESIAN_POINT ( 'NONE',  ( 21.06277459767431637, 8.872862438279403463, -112.7039991923567044 ) ) ;
#152726 = CARTESIAN_POINT ( 'NONE',  ( -21.05000000000000071, 67.23127455305841238, -235.8551265064783991 ) ) ;
#152727 = VERTEX_POINT ( 'NONE', #89804 ) ;
#152728 = CARTESIAN_POINT ( 'NONE',  ( 20.94999999999999929, 28.50120599808395028, -258.2149742250584268 ) ) ;
#152729 = CIRCLE ( 'NONE', #223406, 0.1000000000000001860 ) ;
#152730 = CARTESIAN_POINT ( 'NONE',  ( 21.14999999999999858, 6.540656951701244282, 0.000000000000000000 ) ) ;
#152731 = EDGE_LOOP ( 'NONE', ( #154276, #138693, #2273, #150333 ) ) ;
#152732 = PLANE ( 'NONE',  #156017 ) ;
#152733 = ORIENTED_EDGE ( 'NONE', *, *, #15585, .F. ) ;
#152734 = CARTESIAN_POINT ( 'NONE',  ( -23.15000000000000213, 85.00000000001197975, -112.9170766071766820 ) ) ;
#152735 = ORIENTED_EDGE ( 'NONE', *, *, #189918, .F. ) ;
#152736 = CARTESIAN_POINT ( 'NONE',  ( -23.15000000000000213, -4.259020970815408091, -226.0869574510824123 ) ) ;
#152737 = EDGE_CURVE ( 'NONE', #26629, #18391, #248907, .T. ) ;
#152738 = FACE_OUTER_BOUND ( 'NONE', #89962, .T. ) ;
#152739 = DIRECTION ( 'NONE',  ( 0.000000000000000000, 1.000000000000000000, 6.982962677686266711E-15 ) ) ;
#152740 = EDGE_CURVE ( 'NONE', #110576, #172081, #250184, .T. ) ;
#152741 = DIRECTION ( 'NONE',  ( 1.000000000000000000, 0.000000000000000000, 0.000000000000000000 ) ) ;
#152742 = AXIS2_PLACEMENT_3D ( 'NONE', #238040, #196349, #195099 ) ;
#152743 = AXIS2_PLACEMENT_3D ( 'NONE', #116840, #196367, #17717 ) ;
#152744 = AXIS2_PLACEMENT_3D ( 'NONE', #205109, #201272, #217296 ) ;
#152745 = CIRCLE ( 'NONE', #111203, 7.791421356237338003 ) ;
#152746 = EDGE_CURVE ( 'NONE', #52759, #2978, #151084, .T. ) ;
#152747 = CARTESIAN_POINT ( 'NONE',  ( -22.14074124539699895, 0.09905289585522827900, -26.10992214895623675 ) ) ;
#152748 = DIRECTION ( 'NONE',  ( -6.938893903907224433E-15, 1.000000000000000000, 0.000000000000000000 ) ) ;
#152749 = DIRECTION ( 'NONE',  ( 0.000000000000000000, 0.000000000000000000, -1.000000000000000000 ) ) ;
#152750 = ORIENTED_EDGE ( 'NONE', *, *, #108172, .T. ) ;
#152751 = DIRECTION ( 'NONE',  ( 1.000000000000000000, 0.000000000000000000, 0.000000000000000000 ) ) ;
#152752 = ORIENTED_EDGE ( 'NONE', *, *, #23112, .F. ) ;
#152755 = ORIENTED_EDGE ( 'NONE', *, *, #173553, .F. ) ;
#152754 = DIRECTION ( 'NONE',  ( 0.000000000000000000, -0.000000000000000000, -1.000000000000000000 ) ) ;
#152753 = DIRECTION ( 'NONE',  ( 0.000000000000000000, -0.9770955615653315052, -0.2128009952263603954 ) ) ;
#152756 = VECTOR ( 'NONE', #158932, 1000.000000000000114 ) ;
#152757 = VERTEX_POINT ( 'NONE', #137911 ) ;
#152758 = DIRECTION ( 'NONE',  ( -1.000000000000000000, -0.000000000000000000, -0.000000000000000000 ) ) ;
#152759 = DIRECTION ( 'NONE',  ( 0.000000000000000000, -0.8814952561688398358, 0.4721928772777406746 ) ) ;
#152760 = DIRECTION ( 'NONE',  ( 2.952720810173289112E-16, -1.000000000000000000, 0.000000000000000000 ) ) ;
#152761 = LINE ( 'NONE', #109728, #245606 ) ;
#152762 = VERTEX_POINT ( 'NONE', #254014 ) ;
#152764 = ORIENTED_EDGE ( 'NONE', *, *, #119331, .F. ) ;
#152763 = CARTESIAN_POINT ( 'NONE',  ( 21.14999999999998082, -11.48087284838115885, -203.5004116939112464 ) ) ;
#152765 = AXIS2_PLACEMENT_3D ( 'NONE', #168640, #164734, #6934 ) ;
#152767 = CYLINDRICAL_SURFACE ( 'NONE', #88315, 0.1000000000000000472 ) ;
#152766 = DIRECTION ( 'NONE',  ( 1.000000000000000000, 0.000000000000000000, 0.000000000000000000 ) ) ;
#152768 = AXIS2_PLACEMENT_3D ( 'NONE', #46137, #106089, #185658 ) ;
#152770 = VERTEX_POINT ( 'NONE', #58361 ) ;
#152769 = CARTESIAN_POINT ( 'NONE',  ( -16.90987985657661952, 9.957807518190886498, -54.36928708888363815 ) ) ;
#152771 = AXIS2_PLACEMENT_3D ( 'NONE', #25963, #88463, #168078 ) ;
#152772 = VERTEX_POINT ( 'NONE', #20572 ) ;
#152773 = EDGE_CURVE ( 'NONE', #241027, #68027, #66630, .T. ) ;
#152774 = DIRECTION ( 'NONE',  ( 0.000000000000000000, 0.000000000000000000, -1.000000000000000000 ) ) ;
#152775 = CARTESIAN_POINT ( 'NONE',  ( -18.59999999999999787, 11.65000000001115232, -134.0000000000000284 ) ) ;
#152776 = ORIENTED_EDGE ( 'NONE', *, *, #237255, .T. ) ;
#152777 = CYLINDRICAL_SURFACE ( 'NONE', #143357, 0.1000000000000054040 ) ;
#152778 = VERTEX_POINT ( 'NONE', #154956 ) ;
#152779 = AXIS2_PLACEMENT_3D ( 'NONE', #208951, #131980, #49870 ) ;
#152780 = EDGE_CURVE ( 'NONE', #97301, #112762, #170727, .T. ) ;
#152781 = DIRECTION ( 'NONE',  ( -0.000000000000000000, 0.9651348961777157509, -0.2617529984165031243 ) ) ;
#152782 = DIRECTION ( 'NONE',  ( 0.000000000000000000, 1.000000000000000000, 0.000000000000000000 ) ) ;
#152783 = ORIENTED_EDGE ( 'NONE', *, *, #111592, .T. ) ;
#152784 = FACE_OUTER_BOUND ( 'NONE', #79379, .T. ) ;
#152785 = EDGE_CURVE ( 'NONE', #113902, #156829, #97485, .T. ) ;
#152786 = EDGE_CURVE ( 'NONE', #171580, #12386, #54539, .T. ) ;
#152787 = AXIS2_PLACEMENT_3D ( 'NONE', #65349, #203582, #245288 ) ;
#152788 = CIRCLE ( 'NONE', #240260, 0.09999999999999939493 ) ;
#152789 = CARTESIAN_POINT ( 'NONE',  ( 21.08035267497491105, 6.169086428650065734, -199.5718117947534438 ) ) ;
#152790 = AXIS2_PLACEMENT_3D ( 'NONE', #256214, #116776, #17663 ) ;
#152791 = AXIS2_PLACEMENT_3D ( 'NONE', #194911, #16282, #254805 ) ;
#152792 = EDGE_CURVE ( 'NONE', #103483, #3738, #74142, .T. ) ;
#152793 = ORIENTED_EDGE ( 'NONE', *, *, #29307, .F. ) ;
#152794 = ORIENTED_EDGE ( 'NONE', *, *, #222483, .F. ) ;
#152797 = ADVANCED_FACE ( 'NONE', ( #199193 ), #35022, .F. ) ;
#152796 = EDGE_CURVE ( 'NONE', #140862, #19748, #29251, .T. ) ;
#152795 = CARTESIAN_POINT ( 'NONE',  ( 20.97250901189795158, 18.90193937995545781, -227.9863388870093104 ) ) ;
#152798 = ORIENTED_EDGE ( 'NONE', *, *, #79443, .T. ) ;
#152799 = CARTESIAN_POINT ( 'NONE',  ( 19.75857864376268935, 64.25000000001148237, -44.67310748452440095 ) ) ;
#152800 = ORIENTED_EDGE ( 'NONE', *, *, #54959, .T. ) ;
#152802 = VERTEX_POINT ( 'NONE', #114519 ) ;
#152801 = DIRECTION ( 'NONE',  ( -1.000000000000000000, 0.000000000000000000, 0.000000000000000000 ) ) ;
#152803 = EDGE_LOOP ( 'NONE', ( #1243, #229335, #117795, #161615 ) ) ;
#152804 = DIRECTION ( 'NONE',  ( -1.000000000000000000, -0.000000000000000000, -0.000000000000000000 ) ) ;
#152805 = ORIENTED_EDGE ( 'NONE', *, *, #221632, .T. ) ;
#152808 = ORIENTED_EDGE ( 'NONE', *, *, #36215, .T. ) ;
#152807 = ORIENTED_EDGE ( 'NONE', *, *, #250499, .T. ) ;
#152806 = CARTESIAN_POINT ( 'NONE',  ( -16.93339986808596720, 65.99489607144565184, -56.95711381271154039 ) ) ;
#152809 = VECTOR ( 'NONE', #176357, 1000.000000000000114 ) ;
#152810 = CIRCLE ( 'NONE', #202655, 0.4000000000000033529 ) ;
#152811 = VECTOR ( 'NONE', #108167, 1000.000000000000000 ) ;
#152812 = EDGE_LOOP ( 'NONE', ( #13382, #111116, #101776 ) ) ;
#152813 = EDGE_CURVE ( 'NONE', #8019, #148058, #65294, .T. ) ;
#152814 = EDGE_CURVE ( 'NONE', #9830, #79879, #158806, .T. ) ;
#152815 = TOROIDAL_SURFACE ( 'NONE', #127853, 0.2000000000000000111, 0.1000000000000000056 ) ;
#152816 = PLANE ( 'NONE',  #71813 ) ;
#152817 = ORIENTED_EDGE ( 'NONE', *, *, #178890, .F. ) ;
#152818 = EDGE_CURVE ( 'NONE', #84132, #28041, #237034, .T. ) ;
#152819 = DIRECTION ( 'NONE',  ( 1.000000000000000000, 0.000000000000000000, 0.000000000000000000 ) ) ;
#152821 = ORIENTED_EDGE ( 'NONE', *, *, #111492, .F. ) ;
#152820 = DIRECTION ( 'NONE',  ( 0.000000000000000000, -1.000000000000000000, -6.352154140967427193E-15 ) ) ;
#152822 = DIRECTION ( 'NONE',  ( 1.000000000000000000, 0.000000000000000000, 0.000000000000000000 ) ) ;
#152823 = ORIENTED_EDGE ( 'NONE', *, *, #147088, .F. ) ;
#152824 = VERTEX_POINT ( 'NONE', #40147 ) ;
#152826 = ADVANCED_FACE ( 'NONE', ( #85616 ), #64803, .T. ) ;
#152825 = DIRECTION ( 'NONE',  ( -0.000000000000000000, -6.982962677686266711E-15, 1.000000000000000000 ) ) ;
#152827 = FACE_OUTER_BOUND ( 'NONE', #123542, .T. ) ;
#152829 = EDGE_LOOP ( 'NONE', ( #29469, #146945, #221468, #13306 ) ) ;
#152828 = B_SPLINE_CURVE_WITH_KNOTS ( 'NONE', 3,
 ( #75109, #192460, #248575, #114200, #90770, #13822, #9967 ),
 .UNSPECIFIED., .F., .F.,
 ( 4, 3, 4 ),
 ( 0.000000000000000000, 1.860045280646151707E-05, 5.251155757305330614E-05 ),
 .UNSPECIFIED. ) ;
#152830 = ADVANCED_FACE ( 'NONE', ( #184744 ), #242155, .F. ) ;
#152832 = VERTEX_POINT ( 'NONE', #239607 ) ;
#152831 = CARTESIAN_POINT ( 'NONE',  ( -16.77683809663752257, 63.08610022504904435, -213.1421742787362064 ) ) ;
#152833 = DIRECTION ( 'NONE',  ( -1.000000000000000000, 3.265361837132813093E-16, 2.280189983783949500E-30 ) ) ;
#152834 = AXIS2_PLACEMENT_3D ( 'NONE', #201898, #23288, #3686 ) ;
#152836 = ORIENTED_EDGE ( 'NONE', *, *, #235684, .T. ) ;
#152835 = EDGE_LOOP ( 'NONE', ( #35444, #60191, #7193, #229054 ) ) ;
#152837 = ORIENTED_EDGE ( 'NONE', *, *, #39739, .F. ) ;
#152838 = DIRECTION ( 'NONE',  ( -1.000000000000000000, -0.000000000000000000, -0.000000000000000000 ) ) ;
#152839 = ORIENTED_EDGE ( 'NONE', *, *, #30883, .T. ) ;
#152840 = VERTEX_POINT ( 'NONE', #63511 ) ;
#152841 = LINE ( 'NONE', #234919, #100780 ) ;
#152842 = EDGE_LOOP ( 'NONE', ( #244479, #251058, #176523, #143785 ) ) ;
#152843 = EDGE_CURVE ( 'NONE', #166926, #71198, #71096, .T. ) ;
#152844 = CARTESIAN_POINT ( 'NONE',  ( 21.05000000000000071, 8.826429739528350638, -41.91405471294370244 ) ) ;
#152845 = CIRCLE ( 'NONE', #173708, 0.5000000000000013323 ) ;
#152846 = FACE_OUTER_BOUND ( 'NONE', #167864, .T. ) ;
#152847 = ORIENTED_EDGE ( 'NONE', *, *, #180995, .T. ) ;
#152848 = ORIENTED_EDGE ( 'NONE', *, *, #174193, .F. ) ;
#152849 = VECTOR ( 'NONE', #5076, 1000.000000000000114 ) ;
#152850 = ADVANCED_FACE ( 'NONE', ( #244713 ), #24429, .T. ) ;
#152851 = DIRECTION ( 'NONE',  ( 0.000000000000000000, 0.2617529984165033463, 0.9651348961777157509 ) ) ;
#152852 = EDGE_LOOP ( 'NONE', ( #23642, #150196, #159238, #120302 ) ) ;
#152854 = B_SPLINE_CURVE_WITH_KNOTS ( 'NONE', 3,
 ( #227770, #89535, #248621, #70013, #149551, #236745, #18986, #215889, #254972, #98484 ),
 .UNSPECIFIED., .F., .F.,
 ( 4, 3, 3, 4 ),
 ( 0.000000000000000000, 1.004626015991589319E-05, 1.831183478183387304E-05, 2.062343583996250457E-05 ),
 .UNSPECIFIED. ) ;
#152853 = VECTOR ( 'NONE', #139644, 1000.000000000000000 ) ;
#152855 = CIRCLE ( 'NONE', #11168, 11.70000000000000284 ) ;
#152856 = CARTESIAN_POINT ( 'NONE',  ( 21.05000000000000071, 60.94483358488582070, -234.0465764481390636 ) ) ;
#152857 = VECTOR ( 'NONE', #142217, 1000.000000000000000 ) ;
#152858 = ORIENTED_EDGE ( 'NONE', *, *, #88771, .T. ) ;
#152859 = ORIENTED_EDGE ( 'NONE', *, *, #175814, .T. ) ;
#152860 = DIRECTION ( 'NONE',  ( -1.000000000000000000, -0.000000000000000000, 0.000000000000000000 ) ) ;
#152861 = EDGE_CURVE ( 'NONE', #107215, #196105, #120993, .T. ) ;
#152862 = TOROIDAL_SURFACE ( 'NONE', #206990, 0.4000000000000015210, 0.1000000000000000056 ) ;
#152864 = VERTEX_POINT ( 'NONE', #143042 ) ;
#152863 = CARTESIAN_POINT ( 'NONE',  ( -16.84419801905645997, 9.950000000011140600, -121.3305101537780075 ) ) ;
#152865 = FACE_OUTER_BOUND ( 'NONE', #127163, .T. ) ;
#152866 = CARTESIAN_POINT ( 'NONE',  ( -16.87036670365548474, 30.33914847462230568, -234.8334748671511818 ) ) ;
#152867 = CARTESIAN_POINT ( 'NONE',  ( 20.95575313997065336, 65.38544669673724741, -128.9018167825795445 ) ) ;
#152868 = CARTESIAN_POINT ( 'NONE',  ( -21.37071067811865532, 67.92928932189333580, -115.3731074845243540 ) ) ;
#152869 = CARTESIAN_POINT ( 'NONE',  ( -11.59999999999994458, 63.75000000001119815, -21.02310748452479316 ) ) ;
#152870 = CARTESIAN_POINT ( 'NONE',  ( -16.88815647973233780, 66.04916738069655935, -157.3758904211984202 ) ) ;
#152871 = LINE ( 'NONE', #56282, #24809 ) ;
#152872 = CARTESIAN_POINT ( 'NONE',  ( 21.95218792049437795, 10.44204081626609160, -227.3378460360148381 ) ) ;
#152873 = CARTESIAN_POINT ( 'NONE',  ( 18.47135592147670025, 38.07830107212508608, -261.0558283097952312 ) ) ;
#152874 = CARTESIAN_POINT ( 'NONE',  ( 23.24999999999999645, 1.115600667400684642E-11, -167.4999999999999716 ) ) ;
#152875 = CYLINDRICAL_SURFACE ( 'NONE', #88891, 0.1000000000000028644 ) ;
#152876 = AXIS2_PLACEMENT_3D ( 'NONE', #254271, #95217, #16985 ) ;
#152877 = ORIENTED_EDGE ( 'NONE', *, *, #199032, .F. ) ;
#152878 = AXIS2_PLACEMENT_3D ( 'NONE', #30931, #248659, #129973 ) ;
#152881 = ORIENTED_EDGE ( 'NONE', *, *, #202136, .F. ) ;
#152880 = ORIENTED_EDGE ( 'NONE', *, *, #112158, .T. ) ;
#152879 = AXIS2_PLACEMENT_3D ( 'NONE', #38024, #155416, #137096 ) ;
#152882 = ORIENTED_EDGE ( 'NONE', *, *, #21642, .T. ) ;
#152883 = DIRECTION ( 'NONE',  ( -0.000000000000000000, 0.9910827722268049644, 0.1332476588733589318 ) ) ;
#152884 = LINE ( 'NONE', #211543, #169468 ) ;
#152885 = CIRCLE ( 'NONE', #173751, 0.2000000000000057288 ) ;
#152887 = DIRECTION ( 'NONE',  ( 0.000000000000000000, 0.000000000000000000, -1.000000000000000000 ) ) ;
#152886 = CARTESIAN_POINT ( 'NONE',  ( -18.50000000000000000, 52.91185528119410719, -244.1460391050142960 ) ) ;
#152888 = EDGE_LOOP ( 'NONE', ( #103070, #60924, #163195, #56061, #43366, #233447, #256330, #5537, #26931, #195308, #11755, #27762, #137915, #203129 ) ) ;
#152889 = ORIENTED_EDGE ( 'NONE', *, *, #105550, .F. ) ;
#152890 =( LENGTH_UNIT ( ) NAMED_UNIT ( * ) SI_UNIT ( .MILLI., .METRE. ) );
#152891 = CARTESIAN_POINT ( 'NONE',  ( -21.44999999999999929, 21.48591740176965814, -233.0852932139783036 ) ) ;
#152892 = DIRECTION ( 'NONE',  ( 0.000000000000000000, 0.8660254037844411501, 0.4999999999999956701 ) ) ;
#152893 = DIRECTION ( 'NONE',  ( -1.000000000000000000, 0.000000000000000000, 0.000000000000000000 ) ) ;
#152894 = VERTEX_POINT ( 'NONE', #222575 ) ;
#152895 = EDGE_LOOP ( 'NONE', ( #106374, #82179, #218817, #80947 ) ) ;
#152896 = CIRCLE ( 'NONE', #23894, 0.09999999999999939493 ) ;
#152897 = CARTESIAN_POINT ( 'NONE',  ( -23.25000000000000000, 78.57160958314655375, -238.9307242378722833 ) ) ;
#152898 = AXIS2_PLACEMENT_3D ( 'NONE', #201650, #41327, #161260 ) ;
#152899 = DIRECTION ( 'NONE',  ( 1.000000000000000000, 0.000000000000000000, 0.000000000000000000 ) ) ;
#152900 = FACE_OUTER_BOUND ( 'NONE', #59372, .T. ) ;
#152901 = ORIENTED_EDGE ( 'NONE', *, *, #229902, .T. ) ;
#152902 = PLANE ( 'NONE',  #231842 ) ;
#152903 = CARTESIAN_POINT ( 'NONE',  ( -20.95000000000000284, 64.35000000001176090, -76.53791325517833855 ) ) ;
#152904 = CARTESIAN_POINT ( 'NONE',  ( -20.00857864376270001, 66.85000000001150511, -48.27310748452438816 ) ) ;
#152905 = ORIENTED_EDGE ( 'NONE', *, *, #249208, .F. ) ;
#152906 = CARTESIAN_POINT ( 'NONE',  ( 20.94999999999999929, 84.66355140188093742, -79.04720860259155302 ) ) ;
#152907 = FACE_OUTER_BOUND ( 'NONE', #203425, .T. ) ;
#152908 = CARTESIAN_POINT ( 'NONE',  ( -22.39999999999999858, 11.75000000001115552, -134.0000000000000284 ) ) ;
#152910 = DIRECTION ( 'NONE',  ( 0.000000000000000000, 0.9126074666063660468, 0.4088369013363524762 ) ) ;
#152909 = DIRECTION ( 'NONE',  ( 0.000000000000000000, 6.938893903907270030E-14, 1.000000000000000000 ) ) ;
#152912 = EDGE_CURVE ( 'NONE', #199005, #47571, #43963, .T. ) ;
#152911 = CARTESIAN_POINT ( 'NONE',  ( 21.05000000000000071, 36.65892442174472876, -249.5511627012454596 ) ) ;
#152913 = AXIS2_PLACEMENT_3D ( 'NONE', #71055, #34499, #113997 ) ;
#152914 = CARTESIAN_POINT ( 'NONE',  ( -20.94999999999999929, 77.16270174995064224, -195.6231074845243540 ) ) ;
#152915 = CARTESIAN_POINT ( 'NONE',  ( 23.14999999999999858, 1.115600667400684642E-11, -134.0000000000000284 ) ) ;
#152916 = CARTESIAN_POINT ( 'NONE',  ( 22.16821283564876666, 7.558973340791918183, -33.50000000000000000 ) ) ;
#152917 = B_SPLINE_CURVE_WITH_KNOTS ( 'NONE', 3,
 ( #218119, #237711, #100720, #77330, #16116, #257215, #136011 ),
 .UNSPECIFIED., .F., .F.,
 ( 4, 3, 4 ),
 ( 0.000000000000000000, 3.357501770814779694E-05, 5.199112466348563400E-05 ),
 .UNSPECIFIED. ) ;
#152918 = ORIENTED_EDGE ( 'NONE', *, *, #94430, .F. ) ;
#152919 = VECTOR ( 'NONE', #6213, 1000.000000000000000 ) ;
#152920 = ORIENTED_EDGE ( 'NONE', *, *, #129038, .F. ) ;
#152921 = CARTESIAN_POINT ( 'NONE',  ( 21.14999999999999858, 8.786607556611267356, -112.8500000000000369 ) ) ;
#152922 = CARTESIAN_POINT ( 'NONE',  ( -23.15000000000000213, -8.999999999988844479, -124.6060308773475924 ) ) ;
#152923 = ORIENTED_EDGE ( 'NONE', *, *, #197415, .T. ) ;
#152924 = DIRECTION ( 'NONE',  ( 0.000000000000000000, 0.000000000000000000, 1.000000000000000000 ) ) ;
#152925 = AXIS2_PLACEMENT_3D ( 'NONE', #85357, #223599, #202773 ) ;
#152926 = ADVANCED_FACE ( 'NONE', ( #160085 ), #200476, .F. ) ;
#152927 = EDGE_CURVE ( 'NONE', #232805, #13912, #178111, .T. ) ;
#152928 = CIRCLE ( 'NONE', #240379, 0.09999999999998898659 ) ;
#152929 = EDGE_LOOP ( 'NONE', ( #248111, #182194, #29991, #248755, #89680 ) ) ;
#152930 = CIRCLE ( 'NONE', #86231, 0.09999999999999939493 ) ;
#152931 = CIRCLE ( 'NONE', #207068, 0.1999999999999999833 ) ;
#152932 = ORIENTED_EDGE ( 'NONE', *, *, #229554, .F. ) ;
#152933 = CARTESIAN_POINT ( 'NONE',  ( 22.42357213249528769, 7.672932386371071445, -66.90091303599848516 ) ) ;
#152934 = ORIENTED_EDGE ( 'NONE', *, *, #240631, .T. ) ;
#152935 = AXIS2_PLACEMENT_3D ( 'NONE', #21016, #97923, #100489 ) ;
#152936 = CYLINDRICAL_SURFACE ( 'NONE', #113868, 12.87499999999999822 ) ;
#152937 = CARTESIAN_POINT ( 'NONE',  ( 20.94999999999999574, 0.000000000000000000, 0.000000000000000000 ) ) ;
#152938 = CARTESIAN_POINT ( 'NONE',  ( -18.59999999999999787, 74.16465844978745281, -91.46795619196133487 ) ) ;
#152939 = EDGE_CURVE ( 'NONE', #175419, #13038, #81769, .T. ) ;
#152940 =( BOUNDED_CURVE ( )  B_SPLINE_CURVE ( 3, ( #256457, #214827, #19202, #156173 ),
 .UNSPECIFIED., .F., .F. ) 
 B_SPLINE_CURVE_WITH_KNOTS ( ( 4, 4 ),
 ( 0.5235987755982449698, 1.570796326794896558 ),
 .UNSPECIFIED. ) 
 CURVE ( )  GEOMETRIC_REPRESENTATION_ITEM ( )  RATIONAL_B_SPLINE_CURVE ( ( 1.000000000000000000, 0.9106836025229499976, 0.9106836025229499976, 1.000000000000000000 ) ) 
 REPRESENTATION_ITEM ( '' )  );
#152941 = CARTESIAN_POINT ( 'NONE',  ( -20.85000000000000142, 65.66751761918648356, -63.92826094061121722 ) ) ;
#152942 = EDGE_CURVE ( 'NONE', #208701, #204082, #58595, .T. ) ;
#152943 = CYLINDRICAL_SURFACE ( 'NONE', #141040, 0.1000000000000088596 ) ;
#152945 = ORIENTED_EDGE ( 'NONE', *, *, #158933, .T. ) ;
#152944 = CARTESIAN_POINT ( 'NONE',  ( -16.97683809663752186, 29.54312324717475136, -234.4517840742876729 ) ) ;
#152947 = CARTESIAN_POINT ( 'NONE',  ( 19.90621891164687440, 11.75000000001116263, -192.3284452778769662 ) ) ;
#152946 = CARTESIAN_POINT ( 'NONE',  ( 23.14999999999998437, 67.23127455305841238, -235.8551265064783991 ) ) ;
#152948 = CARTESIAN_POINT ( 'NONE',  ( -18.59999999999999787, 64.35000000001171827, -69.52310748452438816 ) ) ;
#152949 = CARTESIAN_POINT ( 'NONE',  ( 13.76927104934457624, 66.54401276639930529, -121.5115763176265347 ) ) ;
#152951 = EDGE_CURVE ( 'NONE', #212023, #227433, #237497, .T. ) ;
#152950 = FACE_OUTER_BOUND ( 'NONE', #171725, .T. ) ;
#152952 = CARTESIAN_POINT ( 'NONE',  ( 18.49999999999998934, 64.35000000001147669, -44.77310748452440237 ) ) ;
#152954 = ORIENTED_EDGE ( 'NONE', *, *, #87426, .T. ) ;
#152953 = AXIS2_PLACEMENT_3D ( 'NONE', #187816, #148685, #112135 ) ;
#152955 = CIRCLE ( 'NONE', #173822, 11.64999999999999680 ) ;
#152956 =( LENGTH_UNIT ( ) NAMED_UNIT ( * ) SI_UNIT ( .MILLI., .METRE. ) );
#152957 = CARTESIAN_POINT ( 'NONE',  ( 18.39999999999998082, 64.52683809664912928, -60.27310748452440947 ) ) ;
#152958 = EDGE_CURVE ( 'NONE', #69378, #136580, #179250, .T. ) ;
#152959 = ORIENTED_EDGE ( 'NONE', *, *, #232770, .T. ) ;
#152960 = CARTESIAN_POINT ( 'NONE',  ( -16.77683809663752257, 52.34166666667924517, -186.7731074845245303 ) ) ;
#152961 = ORIENTED_EDGE ( 'NONE', *, *, #75333, .T. ) ;
#152962 = AXIS2_PLACEMENT_3D ( 'NONE', #159716, #61896, #241808 ) ;
#152963 = CARTESIAN_POINT ( 'NONE',  ( -23.15000000000000213, 7.958757221477368304, -237.5433740025449083 ) ) ;
#152964 = EDGE_CURVE ( 'NONE', #56940, #242287, #204735, .T. ) ;
#152965 = DIRECTION ( 'NONE',  ( 1.000000000000000000, -0.000000000000000000, -0.000000000000000000 ) ) ;
#152966 = DIRECTION ( 'NONE',  ( -7.304098846218132695E-16, 0.9770955615653315052, 0.2128009952263603954 ) ) ;
#152967 = EDGE_LOOP ( 'NONE', ( #162040, #10812, #145940 ) ) ;
#152968 = VERTEX_POINT ( 'NONE', #182201 ) ;
#152969 = ADVANCED_FACE ( 'NONE', ( #165196 ), #166796, .F. ) ;
#152970 = DIRECTION ( 'NONE',  ( 0.000000000000000000, 0.000000000000000000, -1.000000000000000000 ) ) ;
#152971 = DIRECTION ( 'NONE',  ( 1.000000000000000000, -0.000000000000000000, -0.000000000000000000 ) ) ;
#152972 = FACE_OUTER_BOUND ( 'NONE', #87535, .T. ) ;
#152974 = CARTESIAN_POINT ( 'NONE',  ( 18.79999999999999361, -11.75000000000000000, 30.00000000000000000 ) ) ;
#152973 = FACE_OUTER_BOUND ( 'NONE', #184884, .T. ) ;
#152975 = CIRCLE ( 'NONE', #148860, 2.000000000000001776 ) ;
#152976 = DIRECTION ( 'NONE',  ( 1.000000000000000000, -0.000000000000000000, -0.000000000000000000 ) ) ;
#152978 = AXIS2_PLACEMENT_3D ( 'NONE', #68058, #128043, #48491 ) ;
#152977 = LINE ( 'NONE', #124099, #206033 ) ;
#152979 = CIRCLE ( 'NONE', #232073, 0.09999999999998898659 ) ;
#152980 = CARTESIAN_POINT ( 'NONE',  ( 21.04999999999999716, 30.92067721666403912, -252.0498334655604253 ) ) ;
#152981 = ORIENTED_EDGE ( 'NONE', *, *, #111678, .T. ) ;
#152982 = CARTESIAN_POINT ( 'NONE',  ( 21.72449340488910607, 10.28395627750226815, -121.3500000000000227 ) ) ;
#152984 = ORIENTED_EDGE ( 'NONE', *, *, #145450, .T. ) ;
#152983 = DIRECTION ( 'NONE',  ( 0.000000000000000000, 0.2128009952263604510, -0.9770955615653315052 ) ) ;
#152985 = CARTESIAN_POINT ( 'NONE',  ( 22.00411653962159164, 68.74655713164219151, -170.1221455902930302 ) ) ;
#152986 = FACE_OUTER_BOUND ( 'NONE', #11571, .T. ) ;
#152988 = DIRECTION ( 'NONE',  ( 1.000000000000000000, 0.000000000000000000, 0.000000000000000000 ) ) ;
#152987 = CARTESIAN_POINT ( 'NONE',  ( -23.25000000000000000, 76.10085836911093793, -148.2726746080136877 ) ) ;
#152989 = CARTESIAN_POINT ( 'NONE',  ( -20.00857864376270001, 9.150000000011157653, -45.85000000000000142 ) ) ;
#152991 = ORIENTED_EDGE ( 'NONE', *, *, #119453, .T. ) ;
#152990 = CARTESIAN_POINT ( 'NONE',  ( -15.70407651835961360, 62.46590406472956403, -217.6831045281099932 ) ) ;
#152992 = DIRECTION ( 'NONE',  ( -1.000000000000000000, -0.000000000000000000, -0.000000000000000000 ) ) ;
#152993 = CARTESIAN_POINT ( 'NONE',  ( -20.54999999999999716, 76.00000000001142553, -36.02310748452432421 ) ) ;
#152994 = CARTESIAN_POINT ( 'NONE',  ( 22.39999999999999858, 7.591056067193225232, -199.2444047917219052 ) ) ;
#152995 = DIRECTION ( 'NONE',  ( -1.836970198721029934E-16, -1.000000000000000000, -6.982962677686266711E-15 ) ) ;
#152996 = CARTESIAN_POINT ( 'NONE',  ( 21.04999999999999716, 65.31569084252720359, -162.4964106941976070 ) ) ;
#152997 = ORIENTED_EDGE ( 'NONE', *, *, #191309, .F. ) ;
#152998 = CARTESIAN_POINT ( 'NONE',  ( 21.05000000000000071, 8.776282895303632259, -109.0586289951409924 ) ) ;
#152999 = ORIENTED_EDGE ( 'NONE', *, *, #217799, .F. ) ;
#153000 = TOROIDAL_SURFACE ( 'NONE', #77927, 2.100000000000002309, 0.1000000000000000056 ) ;
#153002 = AXIS2_PLACEMENT_3D ( 'NONE', #51916, #132787, #12841 ) ;
#153001 = DIRECTION ( 'NONE',  ( 1.000000000000000000, 0.000000000000000000, 0.000000000000000000 ) ) ;
#153003 = ORIENTED_EDGE ( 'NONE', *, *, #238942, .T. ) ;
#153004 = CARTESIAN_POINT ( 'NONE',  ( 19.97071067811864609, 11.72071067812981404, -121.8500000000000369 ) ) ;
#153005 = ORIENTED_EDGE ( 'NONE', *, *, #206007, .T. ) ;
#153006 = EDGE_CURVE ( 'NONE', #8700, #164965, #133443, .T. ) ;
#153008 = CARTESIAN_POINT ( 'NONE',  ( -15.55912972643740488, 12.75457250812873689, -219.6632863702431848 ) ) ;
#153007 = AXIS2_PLACEMENT_3D ( 'NONE', #102310, #24124, #181895 ) ;
#153010 = EDGE_CURVE ( 'NONE', #231849, #203482, #8690, .T. ) ;
#153009 = FACE_OUTER_BOUND ( 'NONE', #198513, .T. ) ;
#153011 = DIRECTION ( 'NONE',  ( -0.000000000000000000, 0.9910827722268049644, 0.1332476588733589040 ) ) ;
#153012 = ORIENTED_EDGE ( 'NONE', *, *, #13618, .F. ) ;
#153013 = EDGE_CURVE ( 'NONE', #189305, #72671, #50211, .T. ) ;
#153015 = EDGE_CURVE ( 'NONE', #125024, #139303, #183506, .T. ) ;
#153014 =( BOUNDED_SURFACE ( )  B_SPLINE_SURFACE ( 3, 2, ( 
 ( #161152, #201544, #141575 ),
 ( #119462, #22944, #79005 ),
 ( #157320, #80283, #158601 ),
 ( #122017, #238097, #17757 ),
 ( #102414, #196408, #239403 ),
 ( #180717, #138973, #2048 ) ),
 .UNSPECIFIED., .F., .F., .F. ) 
 B_SPLINE_SURFACE_WITH_KNOTS ( ( 4, 2, 4 ),
 ( 3, 3 ),
 ( 0.0001792624049599484879, 0.0003686986002124686881, 0.0005581347954649888612 ),
 ( 0.000000000000000000, 1.000000000000000000 ),
 .UNSPECIFIED. ) 
 GEOMETRIC_REPRESENTATION_ITEM ( )  RATIONAL_B_SPLINE_SURFACE ( (
 ( 1.000000000000000000, 0.9238795325112671986, 1.000000000000000000),
 ( 1.000000000000000000, 0.9229318695239959736, 1.000000000000000000),
 ( 1.000000000000000000, 0.8926288119229054407, 1.000000000000000000),
 ( 1.000000000000000000, 0.8123777807272675178, 1.000000000000000000),
 ( 1.000000000000000000, 0.7629087100930393994, 1.000000000000000000),
 ( 1.000000000000000000, 0.7071067811865352493, 1.000000000000000000) ) ) 
 REPRESENTATION_ITEM ( '' )  SURFACE ( )  );
#153016 = CYLINDRICAL_SURFACE ( 'NONE', #142480, 0.09999999999998898659 ) ;
#153017 = DIRECTION ( 'NONE',  ( -0.000000000000000000, 1.000000000000000000, 0.000000000000000000 ) ) ;
#153018 = ADVANCED_FACE ( 'NONE', ( #131194 ), #32129, .T. ) ;
#153019 = CARTESIAN_POINT ( 'NONE',  ( -21.59780538579341069, 6.669199007058423057, -199.4462207020707751 ) ) ;
#153020 = DIRECTION ( 'NONE',  ( 1.000000000000000000, 0.000000000000000000, 0.000000000000000000 ) ) ;
#153021 = CARTESIAN_POINT ( 'NONE',  ( 21.14999999999999858, 6.540656951712400691, -167.5999999999999659 ) ) ;
#153022 = EDGE_CURVE ( 'NONE', #178117, #193731, #122085, .T. ) ;
#153023 = AXIS2_PLACEMENT_3D ( 'NONE', #216954, #473, #117864 ) ;
#153024 = ORIENTED_EDGE ( 'NONE', *, *, #28237, .F. ) ;
#153026 = EDGE_CURVE ( 'NONE', #1847, #14385, #54309, .T. ) ;
#153025 = CARTESIAN_POINT ( 'NONE',  ( 18.79999999999999716, 3.362550747017865493, 28.82623795144604983 ) ) ;
#153027 = VERTEX_POINT ( 'NONE', #171653 ) ;
#153029 = ORIENTED_EDGE ( 'NONE', *, *, #1985, .T. ) ;
#153028 = CARTESIAN_POINT ( 'NONE',  ( 21.13920837816993270, 67.21675294989194072, -90.77310748452437394 ) ) ;
#153030 = ORIENTED_EDGE ( 'NONE', *, *, #212325, .F. ) ;
#153031 = CARTESIAN_POINT ( 'NONE',  ( 18.42555734704285086, 85.49715836194937424, -196.4832769867893205 ) ) ;
#153032 = DIRECTION ( 'NONE',  ( -3.265361837132813586E-16, 0.9770955615653315052, 0.2128009952263600901 ) ) ;
#153033 = CARTESIAN_POINT ( 'NONE',  ( -2.995603634470891112E-16, 69.35000000001151932, -48.27310748452436684 ) ) ;
#153034 = ADVANCED_FACE ( 'NONE', ( #187342 ), #129905, .T. ) ;
#153035 = CARTESIAN_POINT ( 'NONE',  ( -22.40000000000000213, 76.00000000001173817, -81.27354037698292188 ) ) ;
#153036 = ORIENTED_EDGE ( 'NONE', *, *, #53738, .F. ) ;
#153037 = CARTESIAN_POINT ( 'NONE',  ( 21.14999999999999858, 56.01362831242965967, -232.7091905853083347 ) ) ;
#153038 = AXIS2_PLACEMENT_3D ( 'NONE', #142957, #63436, #42602 ) ;
#153039 = CARTESIAN_POINT ( 'NONE',  ( 18.58719872626880587, -9.566644397587481308, -140.8224781963970713 ) ) ;
#153040 = VERTEX_POINT ( 'NONE', #30848 ) ;
#153041 = EDGE_CURVE ( 'NONE', #206239, #86183, #204150, .T. ) ;
#153043 = EDGE_LOOP ( 'NONE', ( #176841, #55388, #163343, #99269 ) ) ;
#153042 = FACE_OUTER_BOUND ( 'NONE', #126008, .T. ) ;
#153044 = CARTESIAN_POINT ( 'NONE',  ( 23.14999999999999858, 1.115600667400684642E-11, -134.0000000000000000 ) ) ;
#153045 = LINE ( 'NONE', #214265, #202291 ) ;
#153046 = CIRCLE ( 'NONE', #186324, 0.09999999999999939493 ) ;
#153047 = EDGE_CURVE ( 'NONE', #166383, #103596, #148196, .T. ) ;
#153048 = CARTESIAN_POINT ( 'NONE',  ( 20.95512820512820440, 44.11820694106860685, -236.4833523840364933 ) ) ;
#153049 = AXIS2_PLACEMENT_3D ( 'NONE', #72552, #112950, #213313 ) ;
#153050 = ORIENTED_EDGE ( 'NONE', *, *, #95569, .F. ) ;
#153051 = AXIS2_PLACEMENT_3D ( 'NONE', #107939, #88347, #153537 ) ;
#153052 = ORIENTED_EDGE ( 'NONE', *, *, #114664, .F. ) ;
#153053 =( BOUNDED_CURVE ( )  B_SPLINE_CURVE ( 3, ( #115609, #195179, #232584, #76042 ),
 .UNSPECIFIED., .F., .F. ) 
 B_SPLINE_CURVE_WITH_KNOTS ( ( 4, 4 ),
 ( 2.589852378279006828, 2.850972632318391042 ),
 .UNSPECIFIED. ) 
 CURVE ( )  GEOMETRIC_REPRESENTATION_ITEM ( )  RATIONAL_B_SPLINE_CURVE ( ( 1.000000000000000000, 0.9943260843901261525, 0.9943260843901261525, 1.000000000000000000 ) ) 
 REPRESENTATION_ITEM ( '' )  );
#153054 = ORIENTED_EDGE ( 'NONE', *, *, #187207, .F. ) ;
#153055 = DIRECTION ( 'NONE',  ( 0.000000000000000000, -1.000000000000000000, 0.000000000000000000 ) ) ;
#153056 = EDGE_CURVE ( 'NONE', #210631, #207046, #216820, .T. ) ;
#153057 = CYLINDRICAL_SURFACE ( 'NONE', #67096, 0.09999999999999939493 ) ;
#153059 = ORIENTED_EDGE ( 'NONE', *, *, #232248, .F. ) ;
#153058 = VECTOR ( 'NONE', #115942, 1000.000000000000000 ) ;
#153060 = DIRECTION ( 'NONE',  ( 1.000000000000000000, -0.000000000000000000, -0.000000000000000000 ) ) ;
#153061 = AXIS2_PLACEMENT_3D ( 'NONE', #206774, #188485, #145504 ) ;
#153062 = EDGE_CURVE ( 'NONE', #92271, #122419, #250152, .T. ) ;
#153063 = CARTESIAN_POINT ( 'NONE',  ( -22.60000000000094289, -2.401771312553118598, -189.4980873520050011 ) ) ;
#153064 = EDGE_CURVE ( 'NONE', #178566, #55514, #104372, .T. ) ;
#153065 = CARTESIAN_POINT ( 'NONE',  ( -22.39999999999999858, 1.619487989037824871, -230.7814958294534335 ) ) ;
#153066 = VECTOR ( 'NONE', #149776, 1000.000000000000000 ) ;
#153067 = AXIS2_PLACEMENT_3D ( 'NONE', #241923, #142804, #31908 ) ;
#153068 = ORIENTED_EDGE ( 'NONE', *, *, #236442, .T. ) ;
#153069 = CARTESIAN_POINT ( 'NONE',  ( 20.94999999999999929, -4.735542975717121905, -233.2463119243910796 ) ) ;
#153070 = VECTOR ( 'NONE', #67824, 1000.000000000000000 ) ;
#153071 = CIRCLE ( 'NONE', #241104, 0.1000000000000052097 ) ;
#153072 = ORIENTED_EDGE ( 'NONE', *, *, #132397, .T. ) ;
#153073 = CIRCLE ( 'NONE', #223739, 0.1000000000000072220 ) ;
#153074 = DIRECTION ( 'NONE',  ( -0.000000000000000000, 1.000000000000000000, -0.000000000000000000 ) ) ;
#153076 = ORIENTED_EDGE ( 'NONE', *, *, #35424, .F. ) ;
#153075 = CARTESIAN_POINT ( 'NONE',  ( 21.05000000000000071, 10.72371710471867701, -146.1500000000000341 ) ) ;
#153077 = CARTESIAN_POINT ( 'NONE',  ( 21.14999999999999858, 1.115600667400684642E-11, -88.85042919245522341 ) ) ;
#153079 = CIRCLE ( 'NONE', #169827, 1.899999999999999023 ) ;
#153078 = DIRECTION ( 'NONE',  ( 1.000000000000000000, 0.000000000000000000, 0.000000000000000000 ) ) ;
#153080 = CARTESIAN_POINT ( 'NONE',  ( 23.14999999999999858, 76.00000000001143974, -38.02310748452432421 ) ) ;
#153081 = CARTESIAN_POINT ( 'NONE',  ( -16.88815647973234135, 22.97600747097644813, -230.9330153782701984 ) ) ;
#153082 = CARTESIAN_POINT ( 'NONE',  ( 21.14999999999999858, 6.540656951712400691, -33.50000000000000000 ) ) ;
#153083 = FACE_OUTER_BOUND ( 'NONE', #23840, .T. ) ;
#153084 = CARTESIAN_POINT ( 'NONE',  ( 21.14999999999999858, 23.34004772283015683, -229.2004250369967338 ) ) ;
#153086 = ORIENTED_EDGE ( 'NONE', *, *, #31191, .F. ) ;
#153085 = FACE_OUTER_BOUND ( 'NONE', #87338, .T. ) ;
#153087 = AXIS2_PLACEMENT_3D ( 'NONE', #78110, #53427, #73031 ) ;
#153088 = AXIS2_PLACEMENT_3D ( 'NONE', #197197, #235058, #176382 ) ;
#153089 = CIRCLE ( 'NONE', #219664, 0.09999999999999939493 ) ;
#153090 = CARTESIAN_POINT ( 'NONE',  ( -20.54999999999999716, 4.350000000011156054, -155.1500000000000057 ) ) ;
#153091 = CARTESIAN_POINT ( 'NONE',  ( -18.58744394320951443, 85.56638515456009486, -62.70025943064806739 ) ) ;
#153092 = DIRECTION ( 'NONE',  ( 1.000000000000000000, 0.000000000000000000, 0.000000000000000000 ) ) ;
#153093 = ORIENTED_EDGE ( 'NONE', *, *, #52623, .T. ) ;
#153094 = LINE ( 'NONE', #128686, #170775 ) ;
#153095 = AXIS2_PLACEMENT_3D ( 'NONE', #183667, #205779, #226615 ) ;
#153096 = ADVANCED_FACE ( 'NONE', ( #9971 ), #89492, .F. ) ;
#153097 = DIRECTION ( 'NONE',  ( -1.000000000000000000, 0.000000000000000000, 0.000000000000000000 ) ) ;
#153098 = AXIS2_PLACEMENT_3D ( 'NONE', #254469, #75865, #97966 ) ;
#153099 = CARTESIAN_POINT ( 'NONE',  ( -20.85000000000000142, 62.88396779178383156, -206.9948552354529170 ) ) ;
#153100 = EDGE_CURVE ( 'NONE', #88353, #220738, #125079, .T. ) ;
#153102 = ORIENTED_EDGE ( 'NONE', *, *, #56707, .F. ) ;
#153101 = CIRCLE ( 'NONE', #157374, 11.80000000000000426 ) ;
#153103 = DIRECTION ( 'NONE',  ( 1.000000000000000000, 0.000000000000000000, 0.000000000000000000 ) ) ;
#153105 = FACE_OUTER_BOUND ( 'NONE', #11064, .T. ) ;
#153104 = AXIS2_PLACEMENT_3D ( 'NONE', #142544, #3028, #203812 ) ;
#153106 = EDGE_CURVE ( 'NONE', #95552, #198561, #62712, .T. ) ;
#153107 = VERTEX_POINT ( 'NONE', #135026 ) ;
#153109 = EDGE_CURVE ( 'NONE', #240937, #157687, #178052, .T. ) ;
#153108 = CARTESIAN_POINT ( 'NONE',  ( 18.59999999999999076, 65.79142135624952914, -148.6731074845244223 ) ) ;
#153110 = ORIENTED_EDGE ( 'NONE', *, *, #208866, .T. ) ;
#153112 = VERTEX_POINT ( 'NONE', #13826 ) ;
#153111 = CARTESIAN_POINT ( 'NONE',  ( 21.11833042828123652, 6.445644693866283248, -133.9928994909406299 ) ) ;
#153113 = CIRCLE ( 'NONE', #173968, 0.09999999999999939493 ) ;
#153114 = CARTESIAN_POINT ( 'NONE',  ( -23.15000000000000213, 76.00000000001190870, -103.0231074845243029 ) ) ;
#153115 = VERTEX_POINT ( 'NONE', #154648 ) ;
#153116 = DIRECTION ( 'NONE',  ( 0.000000000000000000, -1.000000000000000000, -6.982962677686266711E-15 ) ) ;
#153117 = AXIS2_PLACEMENT_3D ( 'NONE', #178578, #256744, #237239 ) ;
#153118 = CIRCLE ( 'NONE', #173973, 0.09999999999999939493 ) ;
#153119 = ORIENTED_EDGE ( 'NONE', *, *, #141896, .T. ) ;
#153121 = EDGE_LOOP ( 'NONE', ( #234539, #153774, #87616, #168116 ) ) ;
#153120 = ORIENTED_EDGE ( 'NONE', *, *, #113904, .T. ) ;
#153122 = DIRECTION ( 'NONE',  ( 0.000000000000000000, -0.2128009952263678062, 0.9770955615653298398 ) ) ;
#153123 = CIRCLE ( 'NONE', #132811, 0.1999999999999945155 ) ;
#153125 = VERTEX_POINT ( 'NONE', #153380 ) ;
#153124 = DIRECTION ( 'NONE',  ( 1.186688945009009831E-16, 0.9651348961777157509, -0.2617529984165031243 ) ) ;
#153126 = DIRECTION ( 'NONE',  ( 1.000000000000000000, -0.000000000000000000, -0.000000000000000000 ) ) ;
#153127 = VERTEX_POINT ( 'NONE', #172943 ) ;
#153128 = EDGE_CURVE ( 'NONE', #13038, #238989, #213293, .T. ) ;
#153129 = VERTEX_POINT ( 'NONE', #196301 ) ;
#153130 = CARTESIAN_POINT ( 'NONE',  ( 23.15000000000000213, 85.00000000001179501, -79.41707660717668205 ) ) ;
#153131 = CARTESIAN_POINT ( 'NONE',  ( 21.17356465864818915, 75.90108875899782959, -75.94591061076604888 ) ) ;
#153132 = CARTESIAN_POINT ( 'NONE',  ( -23.15000000000000213, 36.65892442174935439, -249.5511627012433848 ) ) ;
#153133 = ORIENTED_EDGE ( 'NONE', *, *, #256490, .F. ) ;
#153134 = CARTESIAN_POINT ( 'NONE',  ( -2.995603634470829482E-16, 12.37888392014804495, -249.8746333190754569 ) ) ;
#153135 = CARTESIAN_POINT ( 'NONE',  ( 20.95512820512820440, 67.12384868372417657, -157.8731074845244109 ) ) ;
#153136 = DIRECTION ( 'NONE',  ( 0.7071067811865474617, 0.7071067811865474617, 2.044391222244499837E-16 ) ) ;
#153137 = AXIS2_PLACEMENT_3D ( 'NONE', #228698, #89156, #56110 ) ;
#153138 = EDGE_LOOP ( 'NONE', ( #42126, #156247, #41628, #154051 ) ) ;
#153139 = FACE_OUTER_BOUND ( 'NONE', #128637, .T. ) ;
#153141 = EDGE_CURVE ( 'NONE', #255363, #89629, #241757, .T. ) ;
#153140 = DIRECTION ( 'NONE',  ( 0.000000000000000000, 0.9999631594459056361, -0.008583690987128059571 ) ) ;
#153142 = CARTESIAN_POINT ( 'NONE',  ( -23.15000000000000213, 76.00000000001142553, -36.02310748452432421 ) ) ;
#153143 = ORIENTED_EDGE ( 'NONE', *, *, #158346, .T. ) ;
#153144 = ADVANCED_FACE ( 'NONE', ( #234144 ), #229314, .T. ) ;
#153145 = VERTEX_POINT ( 'NONE', #237993 ) ;
#153146 = DIRECTION ( 'NONE',  ( 0.000000000000000000, 0.4721928772777351790, 0.8814952561688427224 ) ) ;
#153148 = EDGE_LOOP ( 'NONE', ( #225784, #119482, #174164 ) ) ;
#153147 = AXIS2_PLACEMENT_3D ( 'NONE', #225776, #86262, #64165 ) ;
#153149 = CARTESIAN_POINT ( 'NONE',  ( -13.77178122865954002, 24.82620238936339874, -232.4854380501665787 ) ) ;
#153150 = ORIENTED_EDGE ( 'NONE', *, *, #105378, .T. ) ;
#153151 = ORIENTED_EDGE ( 'NONE', *, *, #72904, .F. ) ;
#153152 = CARTESIAN_POINT ( 'NONE',  ( -22.48660254037843487, 11.37252324248628632, -198.4720136275361710 ) ) ;
#153153 = CARTESIAN_POINT ( 'NONE',  ( -20.15000000000000568, 9.291421356248463326, -79.25000000000004263 ) ) ;
#153154 = ORIENTED_EDGE ( 'NONE', *, *, #61637, .T. ) ;
#153155 = VERTEX_POINT ( 'NONE', #15117 ) ;
#153156 = EDGE_CURVE ( 'NONE', #197965, #11636, #116866, .T. ) ;
#153157 = PLANE ( 'NONE',  #10482 ) ;
#153158 = DIRECTION ( 'NONE',  ( 0.000000000000000000, -0.9908441862701596881, 0.1350103645451904977 ) ) ;
#153159 = EDGE_CURVE ( 'NONE', #194376, #183157, #115481, .T. ) ;
#153160 = ORIENTED_EDGE ( 'NONE', *, *, #39474, .T. ) ;
#153161 = B_SPLINE_CURVE_WITH_KNOTS ( 'NONE', 3,
 ( #134333, #184368, #85242, #157817 ),
 .UNSPECIFIED., .F., .F.,
 ( 4, 4 ),
 ( 3.469446951953614189E-18, 0.0001058379652594569419 ),
 .UNSPECIFIED. ) ;
#153162 = ADVANCED_FACE ( 'NONE', ( #232898 ), #54220, .F. ) ;
#153163 = CIRCLE ( 'NONE', #240598, 0.5000000000000004441 ) ;
#153164 = AXIS2_PLACEMENT_3D ( 'NONE', #117948, #77511, #194944 ) ;
#153165 = AXIS2_PLACEMENT_3D ( 'NONE', #110571, #130130, #195273 ) ;
#153166 = ORIENTED_EDGE ( 'NONE', *, *, #237101, .T. ) ;
#153167 = LINE ( 'NONE', #190991, #39074 ) ;
#153168 = CYLINDRICAL_SURFACE ( 'NONE', #13895, 7.899999999999995914 ) ;
#153169 = EDGE_CURVE ( 'NONE', #253301, #226312, #137687, .T. ) ;
#153170 = DIRECTION ( 'NONE',  ( -1.000000000000000000, -0.000000000000000000, -0.000000000000000000 ) ) ;
#153172 = ORIENTED_EDGE ( 'NONE', *, *, #521, .T. ) ;
#153171 = CARTESIAN_POINT ( 'NONE',  ( 21.00000000000000000, 66.25000000001229239, -157.6731074845244223 ) ) ;
#153173 = FACE_OUTER_BOUND ( 'NONE', #165575, .T. ) ;
#153174 = DIRECTION ( 'NONE',  ( 1.000000000000000000, 0.000000000000000000, 0.000000000000000000 ) ) ;
#153175 = DIRECTION ( 'NONE',  ( 0.000000000000000000, 0.1335171055202901413, -0.9910465087640860649 ) ) ;
#153176 = EDGE_CURVE ( 'NONE', #160025, #245624, #25305, .T. ) ;
#153179 = CARTESIAN_POINT ( 'NONE',  ( -40.23850191057533010, 65.27857539272349641, -29.97167177764265489 ) ) ;
#153178 = AXIS2_PLACEMENT_3D ( 'NONE', #169445, #91147, #131558 ) ;
#153177 = CARTESIAN_POINT ( 'NONE',  ( -22.59999999999999787, 76.00000000001267608, -203.5231074845243597 ) ) ;
#153180 = LINE ( 'NONE', #14926, #253018 ) ;
#153181 = DIRECTION ( 'NONE',  ( -0.000000000000000000, 6.982962677686266711E-15, -1.000000000000000000 ) ) ;
#153182 = VECTOR ( 'NONE', #183757, 1000.000000000000000 ) ;
#153183 = DIRECTION ( 'NONE',  ( 1.000000000000000000, -0.000000000000000000, -0.000000000000000000 ) ) ;
#153184 = EDGE_LOOP ( 'NONE', ( #114333, #64273, #121220 ) ) ;
#153185 = AXIS2_PLACEMENT_3D ( 'NONE', #235877, #157684, #1099 ) ;
#153187 = ORIENTED_EDGE ( 'NONE', *, *, #39113, .T. ) ;
#153186 = LINE ( 'NONE', #237817, #111494 ) ;
#153188 = DIRECTION ( 'NONE',  ( 1.000000000000000000, 0.000000000000000000, 0.000000000000000000 ) ) ;
#153189 = DIRECTION ( 'NONE',  ( -1.000000000000000000, 0.000000000000000000, 0.000000000000000000 ) ) ;
#153190 = ORIENTED_EDGE ( 'NONE', *, *, #157964, .F. ) ;
#153191 =( NAMED_UNIT ( * ) PLANE_ANGLE_UNIT ( ) SI_UNIT ( $, .RADIAN. ) );
#153192 = CARTESIAN_POINT ( 'NONE',  ( -23.15000000000000213, 71.65000000001151648, -48.17310748452435121 ) ) ;
#153193 = AXIS2_PLACEMENT_3D ( 'NONE', #212540, #230823, #251646 ) ;
#153194 = ORIENTED_EDGE ( 'NONE', *, *, #124755, .T. ) ;
#153195 = EDGE_LOOP ( 'NONE', ( #47658, #160073, #27923, #231300 ) ) ;
#153196 = AXIS2_PLACEMENT_3D ( 'NONE', #156670, #214044, #111086 ) ;
#153197 = CARTESIAN_POINT ( 'NONE',  ( 20.73486653747090003, 65.69159657275403674, -213.8343546826533554 ) ) ;
#153198 = DIRECTION ( 'NONE',  ( 0.000000000000000000, -0.9770955615653357240, -0.2128009952263406890 ) ) ;
#153199 = LINE ( 'NONE', #208020, #16168 ) ;
#153201 = ORIENTED_EDGE ( 'NONE', *, *, #222822, .T. ) ;
#153200 = CARTESIAN_POINT ( 'NONE',  ( 18.59999999999997655, 76.00000000001185185, -95.12310748452429721 ) ) ;
#153203 = ORIENTED_EDGE ( 'NONE', *, *, #104562, .F. ) ;
#153202 = DIRECTION ( 'NONE',  ( 0.000000000000000000, 0.000000000000000000, -1.000000000000000000 ) ) ;
#153204 = CARTESIAN_POINT ( 'NONE',  ( -21.05000000000000782, 10.12198123692519403, -228.1806781248011191 ) ) ;
#153205 = FACE_OUTER_BOUND ( 'NONE', #167368, .T. ) ;
#153206 = CARTESIAN_POINT ( 'NONE',  ( -20.90000000000000213, 6.726092018229619107, 9.512212474619550662 ) ) ;
#153207 = CARTESIAN_POINT ( 'NONE',  ( 20.85000000000000142, -1.835859311432481045, -145.6044391687985637 ) ) ;
#153208 = CIRCLE ( 'NONE', #111481, 0.1000000000000028644 ) ;
#153210 = CARTESIAN_POINT ( 'NONE',  ( 21.05000000000000071, 10.72371710471867701, -179.6499999999999773 ) ) ;
#153209 = CARTESIAN_POINT ( 'NONE',  ( -16.85722902420155123, 9.950000000011138823, -154.7344525262302284 ) ) ;
#153212 = ADVANCED_FACE ( 'NONE', ( #34691 ), #170917, .F. ) ;
#153211 = CARTESIAN_POINT ( 'NONE',  ( 20.73486653747088937, 7.750000000011182166, -146.6500000000000341 ) ) ;
#153213 = DIRECTION ( 'NONE',  ( -1.000000000000000000, -0.000000000000000000, -0.000000000000000000 ) ) ;
#153214 = CARTESIAN_POINT ( 'NONE',  ( 20.85000000000000142, -1.835859311443637010, -45.00443916879852679 ) ) ;
#153215 = CIRCLE ( 'NONE', #40792, 0.1000000000000002692 ) ;
#153216 = AXIS2_PLACEMENT_3D ( 'NONE', #90615, #167627, #250973 ) ;
#153217 = CARTESIAN_POINT ( 'NONE',  ( 21.04999999999999716, 1.443015084894189615, -230.7069270091447208 ) ) ;
#153218 = LINE ( 'NONE', #30695, #242714 ) ;
#153219 = CIRCLE ( 'NONE', #53233, 0.09999999999998898659 ) ;
#153220 = EDGE_LOOP ( 'NONE', ( #55252, #96039, #151271, #207037, #202715 ) ) ;
#153221 = CARTESIAN_POINT ( 'NONE',  ( -17.22767730082996707, 10.34924421247852422, -78.35757130942955939 ) ) ;
#153222 = CIRCLE ( 'NONE', #49122, 4.149999999999999467 ) ;
#153223 = ORIENTED_EDGE ( 'NONE', *, *, #227537, .F. ) ;
#153224 = ORIENTED_EDGE ( 'NONE', *, *, #139109, .F. ) ;
#153226 = FACE_OUTER_BOUND ( 'NONE', #170623, .T. ) ;
#153225 = AXIS2_PLACEMENT_3D ( 'NONE', #60512, #97043, #141352 ) ;
#153227 = EDGE_CURVE ( 'NONE', #12989, #209609, #191743, .T. ) ;
#153228 = LINE ( 'NONE', #91924, #169289 ) ;
#153229 = ADVANCED_FACE ( 'NONE', ( #158499, #215850 ), #16413, .T. ) ;
#153230 = ADVANCED_FACE ( 'NONE', ( #137597 ), #59329, .T. ) ;
#153231 = ORIENTED_EDGE ( 'NONE', *, *, #207916, .T. ) ;
#153232 = DIRECTION ( 'NONE',  ( 0.000000000000000000, 6.982962677686266711E-15, -1.000000000000000000 ) ) ;
#153233 = AXIS2_PLACEMENT_3D ( 'NONE', #74766, #39486, #17330 ) ;
#153234 = ORIENTED_EDGE ( 'NONE', *, *, #199001, .T. ) ;
#153235 = TOROIDAL_SURFACE ( 'NONE', #57505, 0.2000000000000000111, 0.1000000000000000056 ) ;
#153236 = ORIENTED_EDGE ( 'NONE', *, *, #97919, .T. ) ;
#153238 = DIRECTION ( 'NONE',  ( 0.000000000000000000, 0.1332476588733448597, 0.9910827722268067408 ) ) ;
#153237 = VECTOR ( 'NONE', #102765, 1000.000000000000000 ) ;
#153239 = CARTESIAN_POINT ( 'NONE',  ( 21.05000000000000071, 10.60832956796514104, -41.09168501329539680 ) ) ;
#153240 = DIRECTION ( 'NONE',  ( 1.000000000000000000, 0.000000000000000000, -0.000000000000000000 ) ) ;
#153241 = AXIS2_PLACEMENT_3D ( 'NONE', #224615, #103371, #108530 ) ;
#153242 = CYLINDRICAL_SURFACE ( 'NONE', #86404, 10.00000000000000178 ) ;
#153243 = CARTESIAN_POINT ( 'NONE',  ( 18.39999999999997371, 11.47316190337362940, -124.7500000000000426 ) ) ;
#153244 = AXIS2_PLACEMENT_3D ( 'NONE', #85985, #70345, #207272 ) ;
#153245 = EDGE_CURVE ( 'NONE', #99302, #20693, #155927, .T. ) ;
#153247 = CARTESIAN_POINT ( 'NONE',  ( -21.14999999999999858, -0.09999999998884338825, -161.2499999999999716 ) ) ;
#153246 = CARTESIAN_POINT ( 'NONE',  ( -21.05000000000000071, 5.900000000011162093, -190.7809002353436085 ) ) ;
#153248 = CARTESIAN_POINT ( 'NONE',  ( 18.52928932304149967, 10.27928932305266407, -58.17625343280370487 ) ) ;
#153250 = ORIENTED_EDGE ( 'NONE', *, *, #192850, .F. ) ;
#153249 = CARTESIAN_POINT ( 'NONE',  ( -18.59999999999999787, 13.56015509305096778, -219.7948714774209691 ) ) ;
#153252 = CARTESIAN_POINT ( 'NONE',  ( -20.94999999999999929, 65.70729864261056719, -164.5657455973725121 ) ) ;
#153251 = DIRECTION ( 'NONE',  ( 1.000000000000000000, 0.000000000000000000, 0.000000000000000000 ) ) ;
#153253 = AXIS2_PLACEMENT_3D ( 'NONE', #234192, #236760, #254984 ) ;
#153254 = PLANE ( 'NONE',  #7427 ) ;
#153255 = ORIENTED_EDGE ( 'NONE', *, *, #32037, .F. ) ;
#153256 = CARTESIAN_POINT ( 'NONE',  ( 23.24999999999999289, 11.38316329224760892, -198.5208684056144079 ) ) ;
#153257 = CARTESIAN_POINT ( 'NONE',  ( 23.04999999999999716, 8.822561741666397950, -9.250000000000001776 ) ) ;
#153258 = ORIENTED_EDGE ( 'NONE', *, *, #73687, .T. ) ;
#153259 = CARTESIAN_POINT ( 'NONE',  ( -16.87683809663752399, 61.23280479334025017, -220.3417702668379832 ) ) ;
#153260 = AXIS2_PLACEMENT_3D ( 'NONE', #180444, #140004, #81300 ) ;
#153261 = DIRECTION ( 'NONE',  ( 1.000000000000000000, -0.000000000000000000, -0.000000000000000000 ) ) ;
#153262 = CARTESIAN_POINT ( 'NONE',  ( 20.94999999999999929, 69.45000000001157048, -57.27310748452437394 ) ) ;
#153263 = VECTOR ( 'NONE', #90919, 1000.000000000000227 ) ;
#153265 = ORIENTED_EDGE ( 'NONE', *, *, #130343, .F. ) ;
#153264 = CIRCLE ( 'NONE', #219847, 4.300000000000024691 ) ;
#153266 = VERTEX_POINT ( 'NONE', #98445 ) ;
#153267 = CARTESIAN_POINT ( 'NONE',  ( -18.59999999999999787, 77.16270174994961906, -61.42310748452431568 ) ) ;
#153268 = EDGE_CURVE ( 'NONE', #16439, #215983, #75391, .T. ) ;
#153269 = EDGE_CURVE ( 'NONE', #249539, #215142, #21231, .T. ) ;
#153270 = DIRECTION ( 'NONE',  ( -1.000000000000000000, -1.794895427898103559E-16, -3.909090864890002444E-17 ) ) ;
#153271 = DIRECTION ( 'NONE',  ( -1.000000000000000000, 0.000000000000000000, 0.000000000000000000 ) ) ;
#153272 = DIRECTION ( 'NONE',  ( 1.000000000000000000, -2.808674667590276147E-16, -1.035613708381807261E-15 ) ) ;
#153273 = ORIENTED_EDGE ( 'NONE', *, *, #105381, .F. ) ;
#153274 = CYLINDRICAL_SURFACE ( 'NONE', #200279, 0.1000000000000028644 ) ;
#153275 = COLOUR_RGB ( '', 0.66274510, 0.83137255, 0.94901961) ;
#153276 = LINE ( 'NONE', #11162, #166550 ) ;
#153277 = AXIS2_PLACEMENT_3D ( 'NONE', #60478, #200015, #39679 ) ;
#153278 = EDGE_CURVE ( 'NONE', #231047, #202321, #249686, .T. ) ;
#153279 = CARTESIAN_POINT ( 'NONE',  ( 23.14999999999999858, 9.960715529987961503, -220.4198853720552904 ) ) ;
#153280 = CYLINDRICAL_SURFACE ( 'NONE', #170101, 0.1000000000000024342 ) ;
#153281 = CIRCLE ( 'NONE', #24266, 3.899999999999999467 ) ;
#153282 = DIRECTION ( 'NONE',  ( -0.000000000000000000, -6.982962677686266711E-15, 1.000000000000000000 ) ) ;
#153283 = CIRCLE ( 'NONE', #61661, 0.1000000000000033223 ) ;
#153285 = ORIENTED_EDGE ( 'NONE', *, *, #70913, .T. ) ;
#153284 = CARTESIAN_POINT ( 'NONE',  ( -20.64999999999999858, 20.02211948220868365, -235.8179285081017156 ) ) ;
#153286 = DIRECTION ( 'NONE',  ( -1.000000000000000000, 0.000000000000000000, 0.000000000000000000 ) ) ;
#153287 = CARTESIAN_POINT ( 'NONE',  ( 23.24999999999999289, 6.450000000011156587, -179.8499999999999943 ) ) ;
#153288 = DIRECTION ( 'NONE',  ( 0.000000000000000000, 1.000000000000000000, 0.000000000000000000 ) ) ;
#153289 = CARTESIAN_POINT ( 'NONE',  ( -22.39999999999999858, -0.1008583690875579364, -122.2504328765106294 ) ) ;
#153290 = FACE_OUTER_BOUND ( 'NONE', #231052, .T. ) ;
#153292 = ORIENTED_EDGE ( 'NONE', *, *, #228617, .T. ) ;
#153291 = DIRECTION ( 'NONE',  ( 0.000000000000000000, -1.000000000000000000, 0.000000000000000000 ) ) ;
#153293 = DIRECTION ( 'NONE',  ( -1.000000000000000000, 0.000000000000000000, -0.000000000000000000 ) ) ;
#153294 = AXIS2_PLACEMENT_3D ( 'NONE', #219804, #137685, #78988 ) ;
#153295 = CARTESIAN_POINT ( 'NONE',  ( 21.05000000000000071, -1.162701749926853712, -74.90000000000004832 ) ) ;
#153296 = DIRECTION ( 'NONE',  ( -1.000000000000000000, -2.952720810173289112E-16, 0.000000000000000000 ) ) ;
#153297 = ORIENTED_EDGE ( 'NONE', *, *, #188089, .F. ) ;
#153298 = DIRECTION ( 'NONE',  ( -1.000000000000000000, 0.000000000000000000, -0.000000000000000000 ) ) ;
#153299 = DIRECTION ( 'NONE',  ( 0.000000000000000000, 1.000000000000000000, 0.000000000000000000 ) ) ;
#153300 = CYLINDRICAL_SURFACE ( 'NONE', #192266, 0.09999999999999939493 ) ;
#153301 = CIRCLE ( 'NONE', #40862, 0.09999999999998898659 ) ;
#153302 = CIRCLE ( 'NONE', #74190, 0.1000000000000033362 ) ;
#153303 = AXIS2_PLACEMENT_3D ( 'NONE', #134730, #215564, #38233 ) ;
#153304 = CARTESIAN_POINT ( 'NONE',  ( -20.85000000000000142, 7.804459559388684298, -245.4620200072988325 ) ) ;
#153305 = VECTOR ( 'NONE', #89311, 1000.000000000000000 ) ;
#153306 = DIRECTION ( 'NONE',  ( 0.000000000000000000, 0.000000000000000000, -1.000000000000000000 ) ) ;
#153307 = ORIENTED_EDGE ( 'NONE', *, *, #231423, .F. ) ;
#153308 = ORIENTED_EDGE ( 'NONE', *, *, #169002, .F. ) ;
#153309 = EDGE_CURVE ( 'NONE', #103813, #81484, #200173, .T. ) ;
#153310 = CARTESIAN_POINT ( 'NONE',  ( -22.50000000000000000, 7.790779598384560245, -33.39999999999999858 ) ) ;
#153312 = EDGE_CURVE ( 'NONE', #133183, #145174, #220996, .T. ) ;
#153311 = DIRECTION ( 'NONE',  ( 0.000000000000000000, 0.000000000000000000, 1.000000000000000000 ) ) ;
#153313 = CARTESIAN_POINT ( 'NONE',  ( -21.03571358705564975, 38.08373427723915228, -236.0376694442006169 ) ) ;
#153314 = CARTESIAN_POINT ( 'NONE',  ( 21.05000000000000071, 30.48950451747912993, -239.6099224343151946 ) ) ;
#153315 = EDGE_CURVE ( 'NONE', #68524, #32954, #112776, .T. ) ;
#153316 = ADVANCED_FACE ( 'NONE', ( #646 ), #42066, .T. ) ;
#153317 = CARTESIAN_POINT ( 'NONE',  ( -21.37071067811865532, 65.00420125700266283, -213.2334772433522687 ) ) ;
#153318 = AXIS2_PLACEMENT_3D ( 'NONE', #118696, #79524, #198206 ) ;
#153319 = CARTESIAN_POINT ( 'NONE',  ( -20.65000000000000568, 5.649999999999983480, -20.85000000000000142 ) ) ;
#153320 = ADVANCED_FACE ( 'NONE', ( #84013 ), #39835, .T. ) ;
#153321 = CARTESIAN_POINT ( 'NONE',  ( -22.50000000000000000, 59.68594599439717285, -233.9123800762197902 ) ) ;
#153322 = CIRCLE ( 'NONE', #186624, 11.74999999999999289 ) ;
#153323 = CARTESIAN_POINT ( 'NONE',  ( -23.25000000000000000, 77.16412189325360771, -162.1082593989527254 ) ) ;
#153324 = EDGE_CURVE ( 'NONE', #20493, #54257, #165504, .T. ) ;
#153326 = EDGE_CURVE ( 'NONE', #155807, #148843, #56461, .T. ) ;
#153325 = ADVANCED_FACE ( 'NONE', ( #80178 ), #216988, .T. ) ;
#153327 = VERTEX_POINT ( 'NONE', #42376 ) ;
#153328 = FACE_BOUND ( 'NONE', #144157, .T. ) ;
#153329 = ORIENTED_EDGE ( 'NONE', *, *, #201726, .T. ) ;
#153330 = CARTESIAN_POINT ( 'NONE',  ( -16.87242674293849731, 9.950000000011138823, -154.8510902463723937 ) ) ;
#153331 = CARTESIAN_POINT ( 'NONE',  ( 22.39999999999999503, 75.90000000001199965, -109.2731074845243171 ) ) ;
#153332 = DIRECTION ( 'NONE',  ( 2.694716079187273439E-16, 1.000000000000000000, 6.467318590049456648E-15 ) ) ;
#153335 = EDGE_CURVE ( 'NONE', #24291, #197777, #33716, .T. ) ;
#153334 = ORIENTED_EDGE ( 'NONE', *, *, #44171, .F. ) ;
#153333 = CYLINDRICAL_SURFACE ( 'NONE', #195256, 0.1000000000000028644 ) ;
#153336 = B_SPLINE_CURVE_WITH_KNOTS ( 'NONE', 3,
 ( #163324, #242848, #167201, #229712, #188024, #30241 ),
 .UNSPECIFIED., .F., .F.,
 ( 4, 2, 4 ),
 ( 0.000000000000000000, 0.0001497467027049249823, 0.0002994934054098499646 ),
 .UNSPECIFIED. ) ;
#153337 = DIRECTION ( 'NONE',  ( 0.000000000000000000, 6.982962677686266711E-15, -1.000000000000000000 ) ) ;
#153338 = LINE ( 'NONE', #172905, #185273 ) ;
#153339 = CYLINDRICAL_SURFACE ( 'NONE', #37237, 0.1999999999999987899 ) ;
#153340 = DIRECTION ( 'NONE',  ( 1.000000000000000000, 0.000000000000000000, 0.000000000000000000 ) ) ;
#153341 = VERTEX_POINT ( 'NONE', #82744 ) ;
#153342 = CARTESIAN_POINT ( 'NONE',  ( -20.54999999999999716, 9.350000000011156942, -79.25000000000004263 ) ) ;
#153343 = EDGE_CURVE ( 'NONE', #7325, #103845, #129530, .T. ) ;
#153344 = CARTESIAN_POINT ( 'NONE',  ( 18.52928932304156717, 65.72071067697063995, -145.3468540517212944 ) ) ;
#153345 = DIRECTION ( 'NONE',  ( 0.000000000000000000, -0.000000000000000000, -1.000000000000000000 ) ) ;
#153346 = CARTESIAN_POINT ( 'NONE',  ( -18.49346865148307018, 85.44307379853742646, -162.8379112292089985 ) ) ;
#153347 = AXIS2_PLACEMENT_3D ( 'NONE', #55097, #16034, #38154 ) ;
#153348 = VECTOR ( 'NONE', #53824, 1000.000000000000000 ) ;
#153349 = CIRCLE ( 'NONE', #240796, 0.5000000000000004441 ) ;
#153350 = EDGE_CURVE ( 'NONE', #223063, #203104, #229491, .T. ) ;
#153351 = AXIS2_PLACEMENT_3D ( 'NONE', #252321, #55382, #54125 ) ;
#153352 = ADVANCED_FACE ( 'NONE', ( #123200 ), #117058, .F. ) ;
#153353 = CARTESIAN_POINT ( 'NONE',  ( 20.85000000000000142, 80.73028107938317532, -192.7673210925340186 ) ) ;
#153354 = ORIENTED_EDGE ( 'NONE', *, *, #155654, .T. ) ;
#153355 = DIRECTION ( 'NONE',  ( 0.000000000000000000, -6.454785026890510900E-15, 1.000000000000000000 ) ) ;
#153357 = ADVANCED_FACE ( 'NONE', ( #24121 ), #133611, .F. ) ;
#153356 = CARTESIAN_POINT ( 'NONE',  ( 20.85000000000000142, 76.00000000001185185, -95.12310748452429721 ) ) ;
#153358 = ORIENTED_EDGE ( 'NONE', *, *, #198016, .F. ) ;
#153359 = ORIENTED_EDGE ( 'NONE', *, *, #154187, .T. ) ;
#153360 = CARTESIAN_POINT ( 'NONE',  ( -20.54999999999999716, 9.350000000011156942, -88.15000000000004832 ) ) ;
#153361 = LINE ( 'NONE', #232874, #193977 ) ;
#153362 = EDGE_CURVE ( 'NONE', #62638, #252199, #12844, .T. ) ;
#153363 = ORIENTED_EDGE ( 'NONE', *, *, #121271, .F. ) ;
#153364 = AXIS2_PLACEMENT_3D ( 'NONE', #198776, #60545, #18858 ) ;
#153365 = CARTESIAN_POINT ( 'NONE',  ( 18.37172112093885801, -9.570961652231641636, -174.3167344534841448 ) ) ;
#153366 = DIRECTION ( 'NONE',  ( -0.000000000000000000, -0.000000000000000000, -1.000000000000000000 ) ) ;
#153367 = ADVANCED_FACE ( 'NONE', ( #91461 ), #92721, .T. ) ;
#153368 = ORIENTED_EDGE ( 'NONE', *, *, #57373, .T. ) ;
#153369 =( BOUNDED_SURFACE ( )  B_SPLINE_SURFACE ( 3, 2, ( 
 ( #55486, #95920, #230304 ),
 ( #15125, #52948, #212050 ),
 ( #111645, #112937, #17667 ),
 ( #37268, #73838, #252423 ) ),
 .UNSPECIFIED., .F., .F., .T. ) 
 B_SPLINE_SURFACE_WITH_KNOTS ( ( 4, 4 ),
 ( 3, 3 ),
 ( 0.0002700421466196717673, 0.0004789321604330994782 ),
 ( 0.000000000000000000, 1.000000000000000000 ),
 .UNSPECIFIED. ) 
 GEOMETRIC_REPRESENTATION_ITEM ( )  RATIONAL_B_SPLINE_SURFACE ( (
 ( 1.000000000000000000, 0.7071067811865475727, 1.000000000000000000),
 ( 1.000000000000000000, 0.7163411249511767442, 1.000000000000000000),
 ( 1.000000000000000000, 0.7221957104841900676, 1.000000000000000000),
 ( 1.000000000000000000, 0.7250110520819876836, 1.000000000000000000) ) ) 
 REPRESENTATION_ITEM ( '' )  SURFACE ( )  );
#153370 = EDGE_LOOP ( 'NONE', ( #3619, #1677, #143732, #239583 ) ) ;
#153371 = CARTESIAN_POINT ( 'NONE',  ( 23.15000000000000213, -11.64999999998883595, -21.75000000000000355 ) ) ;
#153372 = EDGE_CURVE ( 'NONE', #44201, #71370, #52302, .T. ) ;
#153373 = FACE_OUTER_BOUND ( 'NONE', #37495, .T. ) ;
#153375 = EDGE_LOOP ( 'NONE', ( #211139, #122708, #256282, #155091 ) ) ;
#153374 = CARTESIAN_POINT ( 'NONE',  ( 20.94999999999999929, 6.550000000011156231, -45.65000000000000568 ) ) ;
#153376 = LINE ( 'NONE', #55470, #215704 ) ;
#153377 = CARTESIAN_POINT ( 'NONE',  ( -21.44999999999999929, 7.250000000011155521, -88.25000000000005684 ) ) ;
#153378 = CARTESIAN_POINT ( 'NONE',  ( -20.89878130938411616, 65.67252876774553272, -130.9457041994994881 ) ) ;
#153379 = CARTESIAN_POINT ( 'NONE',  ( 20.73486653747088582, 7.250000000011182166, -76.25000000000004263 ) ) ;
#153380 = CARTESIAN_POINT ( 'NONE',  ( -20.54999999999999716, 68.37653524343949130, -222.4633752038642172 ) ) ;
#153381 = CARTESIAN_POINT ( 'NONE',  ( 20.94999999999999929, 5.499999999999998224, -21.09473398108690390 ) ) ;
#153382 = FACE_OUTER_BOUND ( 'NONE', #242708, .T. ) ;
#153384 = ORIENTED_EDGE ( 'NONE', *, *, #193660, .F. ) ;
#153383 = FACE_OUTER_BOUND ( 'NONE', #141376, .T. ) ;
#153385 = ORIENTED_EDGE ( 'NONE', *, *, #211791, .T. ) ;
#153387 = CARTESIAN_POINT ( 'NONE',  ( -16.82055514392346396, 51.59440680927360745, -231.9574250574065957 ) ) ;
#153386 = CARTESIAN_POINT ( 'NONE',  ( 20.94999999999999929, 14.05000000001115623, -161.9863049292391111 ) ) ;
#153388 = EDGE_LOOP ( 'NONE', ( #203212, #108219, #149177, #32824 ) ) ;
#153389 = CIRCLE ( 'NONE', #157478, 0.2000000000000057288 ) ;
#153390 = ORIENTED_EDGE ( 'NONE', *, *, #90164, .F. ) ;
#153391 = FACE_OUTER_BOUND ( 'NONE', #232904, .T. ) ;
#153393 = CARTESIAN_POINT ( 'NONE',  ( 23.25000000000000000, -8.999999999988844479, -143.8939691226524644 ) ) ;
#153392 = AXIS2_PLACEMENT_3D ( 'NONE', #249331, #150236, #229750 ) ;
#153394 = VECTOR ( 'NONE', #147176, 1000.000000000000000 ) ;
#153395 = DIRECTION ( 'NONE',  ( -1.000000000000000000, 0.000000000000000000, 0.000000000000000000 ) ) ;
#153396 = DIRECTION ( 'NONE',  ( 1.000000000000000000, 0.000000000000000000, 0.000000000000000000 ) ) ;
#153398 = CARTESIAN_POINT ( 'NONE',  ( -21.05000000000000071, 76.10000000001272724, -210.0637644362255969 ) ) ;
#153397 = CIRCLE ( 'NONE', #128416, 0.09999999999999939493 ) ;
#153399 = CYLINDRICAL_SURFACE ( 'NONE', #202875, 0.09999999999999939493 ) ;
#153400 = CARTESIAN_POINT ( 'NONE',  ( -18.59999999999999787, 11.65000000001115232, -73.91480577065404134 ) ) ;
#153402 = ORIENTED_EDGE ( 'NONE', *, *, #61233, .F. ) ;
#153401 = EDGE_CURVE ( 'NONE', #246455, #9598, #14513, .T. ) ;
#153403 = ORIENTED_EDGE ( 'NONE', *, *, #33293, .T. ) ;
#153404 = CARTESIAN_POINT ( 'NONE',  ( 21.05000000000000071, 30.90801580390118630, -252.0203440857215469 ) ) ;
#153405 = VECTOR ( 'NONE', #62934, 1000.000000000000000 ) ;
#153406 = CIRCLE ( 'NONE', #57667, 0.1000000000000028644 ) ;
#153407 = EDGE_CURVE ( 'NONE', #72763, #93820, #25482, .T. ) ;
#153408 = EDGE_LOOP ( 'NONE', ( #254362, #57230, #69863, #164750, #190340 ) ) ;
#153409 = CARTESIAN_POINT ( 'NONE',  ( -22.50000000000000000, 1.115600667400684642E-11, -127.7500000000000284 ) ) ;
#153410 = ORIENTED_EDGE ( 'NONE', *, *, #131227, .T. ) ;
#153412 = CARTESIAN_POINT ( 'NONE',  ( 20.94999999999999574, -1.249999999988843369, -175.4999999999999716 ) ) ;
#153411 = AXIS2_PLACEMENT_3D ( 'NONE', #201437, #142736, #239291 ) ;
#153413 = TOROIDAL_SURFACE ( 'NONE', #215707, 0.2000000000000000111, 0.1000000000000000056 ) ;
#153414 = DIRECTION ( 'NONE',  ( 0.000000000000000000, 0.000000000000000000, -1.000000000000000000 ) ) ;
#153415 = EDGE_CURVE ( 'NONE', #50939, #209214, #226119, .T. ) ;
#153417 = EDGE_CURVE ( 'NONE', #178795, #127037, #204334, .T. ) ;
#153416 = DIRECTION ( 'NONE',  ( 1.000000000000000000, 0.000000000000000000, -0.000000000000000000 ) ) ;
#153418 = ORIENTED_EDGE ( 'NONE', *, *, #42097, .T. ) ;
#153419 = CARTESIAN_POINT ( 'NONE',  ( -23.15000000000000213, 86.27712145182582049, -209.5223386573213702 ) ) ;
#153420 = ORIENTED_EDGE ( 'NONE', *, *, #184211, .T. ) ;
#153421 = AXIS2_PLACEMENT_3D ( 'NONE', #96480, #151365, #76935 ) ;
#153422 = FACE_BOUND ( 'NONE', #91633, .T. ) ;
#153423 = CARTESIAN_POINT ( 'NONE',  ( 23.14999999999999858, 30.38404434817536526, -239.4399867032566078 ) ) ;
#153424 = ORIENTED_EDGE ( 'NONE', *, *, #168538, .F. ) ;
#153425 = CARTESIAN_POINT ( 'NONE',  ( 23.24999999999999645, 5.000000000011153745, -188.5947339810868755 ) ) ;
#153426 = CIRCLE ( 'NONE', #40980, 0.09999999999999939493 ) ;
#153427 = ORIENTED_EDGE ( 'NONE', *, *, #126729, .T. ) ;
#153430 = VERTEX_POINT ( 'NONE', #193133 ) ;
#153429 = LINE ( 'NONE', #231653, #155453 ) ;
#153428 = CARTESIAN_POINT ( 'NONE',  ( 22.50000000000000000, 55.96169194136206215, -232.9023299069559130 ) ) ;
#153431 = CARTESIAN_POINT ( 'NONE',  ( -21.05000000000000426, -0.02103547652895681672, -27.19554417805234792 ) ) ;
#153432 = CIRCLE ( 'NONE', #257366, 0.09999999999998898659 ) ;
#153433 = ORIENTED_EDGE ( 'NONE', *, *, #225038, .F. ) ;
#153434 = EDGE_CURVE ( 'NONE', #206366, #7452, #133151, .T. ) ;
#153435 = AXIS2_PLACEMENT_3D ( 'NONE', #69480, #49889, #89003 ) ;
#153436 = EDGE_LOOP ( 'NONE', ( #63922, #432, #152224, #150835 ) ) ;
#153437 = VECTOR ( 'NONE', #93069, 1000.000000000000000 ) ;
#153438 = AXIS2_PLACEMENT_3D ( 'NONE', #130386, #190393, #249081 ) ;
#153439 = AXIS2_PLACEMENT_3D ( 'NONE', #4850, #243490, #205635 ) ;
#153440 = DIRECTION ( 'NONE',  ( 0.000000000000000000, 0.000000000000000000, -1.000000000000000000 ) ) ;
#153441 = EDGE_LOOP ( 'NONE', ( #23949, #95435, #83488, #170057 ) ) ;
#153443 = AXIS2_PLACEMENT_3D ( 'NONE', #64597, #223664, #162446 ) ;
#153442 = CARTESIAN_POINT ( 'NONE',  ( -20.85000000000000142, 64.25000000001176659, -76.36470817442145176 ) ) ;
#153444 = CARTESIAN_POINT ( 'NONE',  ( 21.05000000000000071, 69.74218538953552127, -69.62089777583315708 ) ) ;
#153445 = DIRECTION ( 'NONE',  ( -0.000000000000000000, 0.8127272543710951647, -0.5826443254700256480 ) ) ;
#153446 = CARTESIAN_POINT ( 'NONE',  ( 23.24999999999999289, 4.150000000011154988, -134.0000000000000000 ) ) ;
#153447 = DIRECTION ( 'NONE',  ( 0.000000000000000000, 6.982962677686266711E-15, -1.000000000000000000 ) ) ;
#153448 = ORIENTED_EDGE ( 'NONE', *, *, #182700, .T. ) ;
#153449 = CARTESIAN_POINT ( 'NONE',  ( -16.93226657140833069, 44.05016941585932244, -235.2828622548803708 ) ) ;
#153450 = DIRECTION ( 'NONE',  ( 0.000000000000000000, -0.1350103645451974088, 0.9908441862701587999 ) ) ;
#153451 = CARTESIAN_POINT ( 'NONE',  ( -21.05000000000000071, 4.184122562697131897, -245.3714803909117279 ) ) ;
#153452 = ORIENTED_EDGE ( 'NONE', *, *, #181470, .T. ) ;
#153453 = ADVANCED_FACE ( 'NONE', ( #154047 ), #233548, .F. ) ;
#153454 = LINE ( 'NONE', #97233, #80237 ) ;
#153456 = ORIENTED_EDGE ( 'NONE', *, *, #186875, .T. ) ;
#153455 = CIRCLE ( 'NONE', #24243, 4.099999999999999645 ) ;
#153458 = CIRCLE ( 'NONE', #41010, 0.09999999999999939493 ) ;
#153457 = DIRECTION ( 'NONE',  ( -1.000000000000000000, -0.000000000000000000, 0.000000000000000000 ) ) ;
#153459 = EDGE_LOOP ( 'NONE', ( #27129, #137313, #138604, #80004 ) ) ;
#153460 = FACE_OUTER_BOUND ( 'NONE', #87411, .T. ) ;
#153461 = CARTESIAN_POINT ( 'NONE',  ( -21.05000000000000071, -1.835341550213255957, -112.1551512925630050 ) ) ;
#153463 = ORIENTED_EDGE ( 'NONE', *, *, #101116, .T. ) ;
#153462 = CYLINDRICAL_SURFACE ( 'NONE', #227841, 0.1000000000000028644 ) ;
#153464 = CARTESIAN_POINT ( 'NONE',  ( 23.24999999999999645, -2.099999999988846344, -200.9999999999999432 ) ) ;
#153465 = ORIENTED_EDGE ( 'NONE', *, *, #248744, .F. ) ;
#153466 = EDGE_CURVE ( 'NONE', #242536, #17057, #251806, .T. ) ;
#153467 = CARTESIAN_POINT ( 'NONE',  ( -21.05315837413033009, 36.17631400068042780, -235.9630178772233648 ) ) ;
#153468 = AXIS2_PLACEMENT_3D ( 'NONE', #141342, #177917, #217011 ) ;
#153469 = CARTESIAN_POINT ( 'NONE',  ( -16.96982749440708460, 9.950000000011137047, -113.6247784088119062 ) ) ;
#153470 = EDGE_CURVE ( 'NONE', #185697, #222817, #196157, .T. ) ;
#153471 = ORIENTED_EDGE ( 'NONE', *, *, #214068, .T. ) ;
#153472 = DIRECTION ( 'NONE',  ( -1.000000000000000000, 0.000000000000000000, 0.000000000000000000 ) ) ;
#153473 = DIRECTION ( 'NONE',  ( 1.000000000000000000, 3.265361837132813093E-16, -0.000000000000000000 ) ) ;
#153474 = AXIS2_PLACEMENT_3D ( 'NONE', #216763, #19873, #79800 ) ;
#153475 = EDGE_LOOP ( 'NONE', ( #249059, #51365, #147520, #240368, #166462 ) ) ;
#153476 = CARTESIAN_POINT ( 'NONE',  ( -16.93226657140833069, 9.999543822735571297, -146.5787131109736379 ) ) ;
#153477 = ORIENTED_EDGE ( 'NONE', *, *, #56707, .T. ) ;
#153478 = CIRCLE ( 'NONE', #3573, 0.1999999999999987899 ) ;
#153479 = EDGE_CURVE ( 'NONE', #67087, #190151, #19052, .T. ) ;
#153480 = DIRECTION ( 'NONE',  ( 0.000000000000000000, 0.000000000000000000, -1.000000000000000000 ) ) ;
#153481 = DIRECTION ( 'NONE',  ( 0.000000000000000000, 0.000000000000000000, -1.000000000000000000 ) ) ;
#153482 = EDGE_CURVE ( 'NONE', #20141, #208598, #254352, .T. ) ;
#153483 = TOROIDAL_SURFACE ( 'NONE', #240923, 11.70000000000000462, 0.1000000000000000056 ) ;
#153484 = ADVANCED_FACE ( 'NONE', ( #7094 ), #125753, .F. ) ;
#153486 = ORIENTED_EDGE ( 'NONE', *, *, #17538, .T. ) ;
#153485 = CARTESIAN_POINT ( 'NONE',  ( -20.94999999999999929, 76.00000000001244871, -170.0231074845243597 ) ) ;
#153487 = CARTESIAN_POINT ( 'NONE',  ( -20.54999999999999716, -8.999999999988846255, -143.8939691226524644 ) ) ;
#153488 = AXIS2_PLACEMENT_3D ( 'NONE', #141363, #22731, #102202 ) ;
#153489 = DIRECTION ( 'NONE',  ( 0.000000000000000000, 0.000000000000000000, -1.000000000000000000 ) ) ;
#153490 = AXIS2_PLACEMENT_3D ( 'NONE', #178921, #217981, #120235 ) ;
#153491 = CARTESIAN_POINT ( 'NONE',  ( -16.93353400591625757, 10.00461239617294140, -20.93268447020540890 ) ) ;
#153492 = EDGE_CURVE ( 'NONE', #147319, #223586, #46218, .T. ) ;
#153493 = AXIS2_PLACEMENT_3D ( 'NONE', #21596, #204058, #85366 ) ;
#153495 = CARTESIAN_POINT ( 'NONE',  ( -15.51798037960204546, 66.62334006147798959, -51.89491493630710295 ) ) ;
#153494 = FACE_OUTER_BOUND ( 'NONE', #185510, .T. ) ;
#153496 = CARTESIAN_POINT ( 'NONE',  ( -0.8999999999999438449, 67.72071067812984779, -6.052396806406134644 ) ) ;
#153497 = FACE_OUTER_BOUND ( 'NONE', #173866, .T. ) ;
#153498 = PLANE ( 'NONE',  #68453 ) ;
#153499 = AXIS2_PLACEMENT_3D ( 'NONE', #175907, #54637, #115916 ) ;
#153500 = DIRECTION ( 'NONE',  ( -1.000000000000000000, 0.000000000000000000, -0.000000000000000000 ) ) ;
#153501 = ORIENTED_EDGE ( 'NONE', *, *, #40981, .F. ) ;
#153502 = EDGE_LOOP ( 'NONE', ( #127581, #194105, #172603, #69324, #119688, #52056, #209164, #171034, #205922, #239840, #49659, #19248, #74642, #199223, #84144, #191655, #211776, #141169 ) ) ;
#153503 = CARTESIAN_POINT ( 'NONE',  ( -20.64999999999999858, 7.250000000011155521, -112.7500000000000284 ) ) ;
#153505 = EDGE_LOOP ( 'NONE', ( #237377, #204117, #6128, #5747 ) ) ;
#153504 = DIRECTION ( 'NONE',  ( 1.000000000000000000, 0.000000000000000000, 0.000000000000000000 ) ) ;
#153506 = VERTEX_POINT ( 'NONE', #79569 ) ;
#153507 = EDGE_CURVE ( 'NONE', #32310, #190202, #87800, .T. ) ;
#153508 = CARTESIAN_POINT ( 'NONE',  ( 18.50000000000000000, -9.399999999988843058, -140.8820418481727188 ) ) ;
#153509 = ORIENTED_EDGE ( 'NONE', *, *, #91939, .T. ) ;
#153510 = DIRECTION ( 'NONE',  ( 1.000000000000000000, 0.000000000000000000, 0.000000000000000000 ) ) ;
#153511 = TOROIDAL_SURFACE ( 'NONE', #245040, 11.70000000000000639, 0.1000000000000000056 ) ;
#153512 = ORIENTED_EDGE ( 'NONE', *, *, #251385, .F. ) ;
#153513 = CARTESIAN_POINT ( 'NONE',  ( 0.000000000000000000, 0.000000000000000000, 0.000000000000000000 ) ) ;
#153514 = CARTESIAN_POINT ( 'NONE',  ( 20.04142135623730070, 51.38014393322265505, -230.1906178717505611 ) ) ;
#153516 = ORIENTED_EDGE ( 'NONE', *, *, #21908, .T. ) ;
#153515 = VERTEX_POINT ( 'NONE', #195719 ) ;
#153517 = ORIENTED_EDGE ( 'NONE', *, *, #106129, .F. ) ;
#153518 = ORIENTED_EDGE ( 'NONE', *, *, #73530, .F. ) ;
#153519 = EDGE_LOOP ( 'NONE', ( #254443, #119610, #234457, #144765 ) ) ;
#153520 = CARTESIAN_POINT ( 'NONE',  ( -22.47071067811865319, 1.115600667400684642E-11, -167.4999999999999716 ) ) ;
#153521 = CARTESIAN_POINT ( 'NONE',  ( -18.50000000000000000, 102.4393534156131977, -151.8815988770167280 ) ) ;
#153522 = DIRECTION ( 'NONE',  ( -4.408576920032448588E-17, -0.1350103645451807555, -0.9908441862701609093 ) ) ;
#153524 = ORIENTED_EDGE ( 'NONE', *, *, #175669, .T. ) ;
#153523 = DIRECTION ( 'NONE',  ( 0.000000000000000000, 0.9770955615653313941, 0.2128009952263606452 ) ) ;
#153525 = CARTESIAN_POINT ( 'NONE',  ( -21.14999999999999858, 11.40444339177023814, -198.6185779617709670 ) ) ;
#153526 = CARTESIAN_POINT ( 'NONE',  ( -20.09999999999999787, 3.461118860469513336, 28.84309995045515507 ) ) ;
#153528 = EDGE_LOOP ( 'NONE', ( #19897, #27792, #185592, #57131 ) ) ;
#153527 = CARTESIAN_POINT ( 'NONE',  ( -16.89268316805466341, 60.93619025550653134, -221.0468289635910537 ) ) ;
#153529 = CYLINDRICAL_SURFACE ( 'NONE', #241540, 0.09999999999999939493 ) ;
#153530 = ORIENTED_EDGE ( 'NONE', *, *, #190122, .T. ) ;
#153532 = EDGE_LOOP ( 'NONE', ( #40772, #136548, #210761, #152817 ) ) ;
#153531 = CARTESIAN_POINT ( 'NONE',  ( 21.07199075132371746, 8.774944999127242795, -112.7135321616128891 ) ) ;
#153533 = LINE ( 'NONE', #73980, #231053 ) ;
#153534 = CARTESIAN_POINT ( 'NONE',  ( -16.92973740335373734, 9.992503814478400415, -113.0939409647979943 ) ) ;
#153535 = ORIENTED_EDGE ( 'NONE', *, *, #241203, .T. ) ;
#153536 = CIRCLE ( 'NONE', #128544, 0.1000000000000028644 ) ;
#153539 = CARTESIAN_POINT ( 'NONE',  ( -18.39999999999999858, -9.499999999988849808, -140.6001893912220737 ) ) ;
#153538 = CIRCLE ( 'NONE', #253426, 11.75000000000000000 ) ;
#153537 = DIRECTION ( 'NONE',  ( 0.000000000000000000, -7.086529944415894657E-15, 1.000000000000000000 ) ) ;
#153540 = TOROIDAL_SURFACE ( 'NONE', #195212, 0.2000000000000000111, 0.1000000000000000056 ) ;
#153541 = CARTESIAN_POINT ( 'NONE',  ( 23.24999999999999645, 65.08943781962308606, -222.1672656287770451 ) ) ;
#153542 = ADVANCED_FACE ( 'NONE', ( #198247 ), #234817, .F. ) ;
#153543 = PLANE ( 'NONE',  #184689 ) ;
#153544 = DIRECTION ( 'NONE',  ( 0.000000000000000000, 1.000000000000000000, 0.000000000000000000 ) ) ;
#153545 = VERTEX_POINT ( 'NONE', #135697 ) ;
#153546 = VERTEX_POINT ( 'NONE', #181285 ) ;
#153547 = CARTESIAN_POINT ( 'NONE',  ( -17.11825945287481332, 10.04999999999998295, -20.75000000000000000 ) ) ;
#153548 = LINE ( 'NONE', #133923, #61128 ) ;
#153549 = ORIENTED_EDGE ( 'NONE', *, *, #144761, .T. ) ;
#153550 = CARTESIAN_POINT ( 'NONE',  ( -22.57320508075687115, 55.89093952297024970, -232.7795287750844579 ) ) ;
#153551 = ORIENTED_EDGE ( 'NONE', *, *, #76329, .T. ) ;
#153552 = DIRECTION ( 'NONE',  ( -1.000000000000000000, 0.000000000000000000, 0.000000000000000000 ) ) ;
#153553 = EDGE_CURVE ( 'NONE', #56965, #47601, #121193, .T. ) ;
#153554 = CARTESIAN_POINT ( 'NONE',  ( -20.94999999999999929, 56.27731819600170837, -227.9967441372480721 ) ) ;
#153555 = EDGE_CURVE ( 'NONE', #80932, #238808, #8720, .T. ) ;
#153557 = EDGE_CURVE ( 'NONE', #161523, #173295, #39209, .T. ) ;
#153556 = CIRCLE ( 'NONE', #107710, 0.09999999999998898659 ) ;
#153558 = ORIENTED_EDGE ( 'NONE', *, *, #22618, .T. ) ;
#153559 = CIRCLE ( 'NONE', #186842, 0.1000000000000028644 ) ;
#153560 = FACE_OUTER_BOUND ( 'NONE', #227463, .T. ) ;
#153561 = VERTEX_POINT ( 'NONE', #17072 ) ;
#153562 = AXIS2_PLACEMENT_3D ( 'NONE', #133591, #253530, #254778 ) ;
#153563 = ORIENTED_EDGE ( 'NONE', *, *, #161878, .T. ) ;
#153564 = VERTEX_POINT ( 'NONE', #116168 ) ;
#153565 = FACE_OUTER_BOUND ( 'NONE', #245008, .T. ) ;
#153566 = CARTESIAN_POINT ( 'NONE',  ( -23.25000000000000000, -4.356730526971941408, -226.1082375506050539 ) ) ;
#153567 = DIRECTION ( 'NONE',  ( -1.000000000000000000, 0.000000000000000000, 0.000000000000000000 ) ) ;
#153568 = DIRECTION ( 'NONE',  ( 1.186688945009009831E-16, -1.000000000000000000, 0.000000000000000000 ) ) ;
#153569 = CARTESIAN_POINT ( 'NONE',  ( 12.48201962039795809, 66.62334006147848697, -118.8949149363070319 ) ) ;
#153570 = ADVANCED_FACE ( 'NONE', ( #56157 ), #60009, .T. ) ;
#153572 = DIRECTION ( 'NONE',  ( -1.000000000000000000, 0.000000000000000000, 0.000000000000000000 ) ) ;
#153571 = DIRECTION ( 'NONE',  ( 1.000000000000000000, -0.000000000000000000, -0.000000000000000000 ) ) ;
#153574 = VERTEX_POINT ( 'NONE', #217792 ) ;
#153573 = DIRECTION ( 'NONE',  ( 0.000000000000000000, 0.9893560106964510714, -0.1455152366551481502 ) ) ;
#153575 = LINE ( 'NONE', #93542, #29184 ) ;
#153576 = ORIENTED_EDGE ( 'NONE', *, *, #240373, .T. ) ;
#153577 = CARTESIAN_POINT ( 'NONE',  ( -12.84409460144753901, 9.410682294279110849, -149.4311434419483362 ) ) ;
#153578 = EDGE_LOOP ( 'NONE', ( #234590, #162530, #256280, #8936 ) ) ;
#153579 = ORIENTED_EDGE ( 'NONE', *, *, #27146, .T. ) ;
#153580 = CYLINDRICAL_SURFACE ( 'NONE', #8802, 0.09999999999999867328 ) ;
#153581 = CARTESIAN_POINT ( 'NONE',  ( -16.93772744219066340, 9.993541108763512426, -46.09806197196969890 ) ) ;
#153582 = DIRECTION ( 'NONE',  ( -4.408576920032448588E-17, 0.1350103645451876666, 0.9908441862701600211 ) ) ;
#153583 = DIRECTION ( 'NONE',  ( -1.000000000000000000, 0.000000000000000000, 0.000000000000000000 ) ) ;
#153584 = CIRCLE ( 'NONE', #45188, 11.70000000000000284 ) ;
#153585 = AXIS2_PLACEMENT_3D ( 'NONE', #151527, #253157, #137070 ) ;
#153586 = VECTOR ( 'NONE', #146846, 1000.000000000000000 ) ;
#153587 = CARTESIAN_POINT ( 'NONE',  ( 20.90851465518105812, 18.40294846151842023, -236.9778203247716419 ) ) ;
#153588 = ORIENTED_EDGE ( 'NONE', *, *, #92437, .F. ) ;
#153589 = ORIENTED_EDGE ( 'NONE', *, *, #115871, .T. ) ;
#153590 = DIRECTION ( 'NONE',  ( 0.000000000000000000, 0.8814952561694257005, -0.4721928772766468829 ) ) ;
#153592 = ORIENTED_EDGE ( 'NONE', *, *, #181940, .F. ) ;
#153591 = EDGE_CURVE ( 'NONE', #56745, #246680, #254391, .T. ) ;
#153593 = DIRECTION ( 'NONE',  ( 0.000000000000000000, 0.000000000000000000, -1.000000000000000000 ) ) ;
#153594 = ORIENTED_EDGE ( 'NONE', *, *, #88674, .F. ) ;
#153595 = ADVANCED_FACE ( 'NONE', ( #216530 ), #36649, .T. ) ;
#153597 = CARTESIAN_POINT ( 'NONE',  ( 20.99999999999999645, 9.750000000011137757, -79.65000000000004832 ) ) ;
#153596 = VECTOR ( 'NONE', #109653, 1000.000000000000000 ) ;
#153598 = CARTESIAN_POINT ( 'NONE',  ( 20.04142135623730070, 11.75000000001115907, -21.75000000000000355 ) ) ;
#153599 = CARTESIAN_POINT ( 'NONE',  ( 16.87683809663750267, 66.05000000001261640, -190.8731074845244393 ) ) ;
#153600 = CARTESIAN_POINT ( 'NONE',  ( 20.94999999999999929, 10.29270135740183179, -38.95736188715193293 ) ) ;
#153601 = EDGE_LOOP ( 'NONE', ( #218454, #60077, #197113, #94145 ) ) ;
#153602 = DIRECTION ( 'NONE',  ( -1.020425574104004196E-15, -6.982962677686266711E-15, 1.000000000000000000 ) ) ;
#153603 = CARTESIAN_POINT ( 'NONE',  ( -20.94999999999999929, 7.661991824395936845, -241.5144583139544636 ) ) ;
#153604 = EDGE_CURVE ( 'NONE', #95393, #91550, #91914, .T. ) ;
#153605 = CIRCLE ( 'NONE', #141083, 0.9000000000000014655 ) ;
#153606 = DIRECTION ( 'NONE',  ( 0.000000000000000000, 0.7397360091702777085, -0.6728971962616808744 ) ) ;
#153607 = AXIS2_PLACEMENT_3D ( 'NONE', #109580, #209990, #86145 ) ;
#153608 = AXIS2_PLACEMENT_3D ( 'NONE', #149855, #211095, #229385 ) ;
#153609 = ORIENTED_EDGE ( 'NONE', *, *, #206248, .T. ) ;
#153610 = CARTESIAN_POINT ( 'NONE',  ( 20.94999999999999929, 76.00000000001189449, -101.1231074845242972 ) ) ;
#153611 = VERTEX_POINT ( 'NONE', #117441 ) ;
#153612 = LINE ( 'NONE', #71481, #26672 ) ;
#153613 = CARTESIAN_POINT ( 'NONE',  ( 20.27550659511088682, 9.216043722508844738, -9.250000000000001776 ) ) ;
#153614 = CARTESIAN_POINT ( 'NONE',  ( -18.59999999999999787, 72.08710075277861051, -125.0412845115133678 ) ) ;
#153616 = VECTOR ( 'NONE', #25241, 1000.000000000000000 ) ;
#153615 = DIRECTION ( 'NONE',  ( 0.000000000000000000, 0.9994937237965558774, 0.03181660087586650476 ) ) ;
#153617 = DIRECTION ( 'NONE',  ( 0.000000000000000000, 0.000000000000000000, -1.000000000000000000 ) ) ;
#153618 = DIRECTION ( 'NONE',  ( 0.000000000000000000, 0.9126074666063660468, 0.4088369013363524762 ) ) ;
#153619 = CIRCLE ( 'NONE', #45414, 0.09999999999999993616 ) ;
#153620 = ORIENTED_EDGE ( 'NONE', *, *, #20276, .F. ) ;
#153621 = EDGE_CURVE ( 'NONE', #111659, #182617, #175342, .T. ) ;
#153622 = CARTESIAN_POINT ( 'NONE',  ( -16.93388492042257454, 66.01145817749633693, -149.1225623613382538 ) ) ;
#153623 = CARTESIAN_POINT ( 'NONE',  ( -16.88328101497759448, 66.04964716579294759, -82.17192796959510304 ) ) ;
#153624 = CARTESIAN_POINT ( 'NONE',  ( 22.40000000000000213, 10.80758397488569855, -226.8651660546161395 ) ) ;
#153625 = CARTESIAN_POINT ( 'NONE',  ( 20.94999999999999929, 8.788681102860177674, -241.3540466926497174 ) ) ;
#153626 = AXIS2_PLACEMENT_3D ( 'NONE', #115798, #96221, #74136 ) ;
#153627 = CARTESIAN_POINT ( 'NONE',  ( 21.05000000000000071, 67.12338541492522381, -161.6380270056797599 ) ) ;
#153628 = AXIS2_PLACEMENT_3D ( 'NONE', #40653, #236234, #120185 ) ;
#153629 = CIRCLE ( 'NONE', #141119, 11.74999999999999467 ) ;
#153631 = ORIENTED_EDGE ( 'NONE', *, *, #215891, .F. ) ;
#153630 = AXIS2_PLACEMENT_3D ( 'NONE', #70470, #165701, #50836 ) ;
#153632 = ORIENTED_EDGE ( 'NONE', *, *, #37964, .F. ) ;
#153633 = DIRECTION ( 'NONE',  ( -1.000000000000000000, 0.000000000000000000, -0.000000000000000000 ) ) ;
#153634 = CIRCLE ( 'NONE', #174483, 0.1000000000000024342 ) ;
#153635 = CARTESIAN_POINT ( 'NONE',  ( -20.85000000000000142, 64.25000000001190870, -103.0231074845243882 ) ) ;
#153637 = ADVANCED_FACE ( 'NONE', ( #97837 ), #19631, .T. ) ;
#153636 = DIRECTION ( 'NONE',  ( 0.000000000000000000, 0.000000000000000000, 1.000000000000000000 ) ) ;
#153638 = SURFACE_STYLE_FILL_AREA ( #206175 ) ;
#153639 = CARTESIAN_POINT ( 'NONE',  ( -20.94999999999999929, 18.18127959618848521, -237.5711165786817389 ) ) ;
#153640 = AXIS2_PLACEMENT_3D ( 'NONE', #47283, #167290, #149000 ) ;
#153641 = ORIENTED_EDGE ( 'NONE', *, *, #58654, .F. ) ;
#153642 = CARTESIAN_POINT ( 'NONE',  ( -19.89999999999999858, 4.631764625546179737, 22.00000000000000355 ) ) ;
#153643 = EDGE_CURVE ( 'NONE', #25415, #131827, #162876, .T. ) ;
#153644 = EDGE_CURVE ( 'NONE', #171759, #232638, #237388, .T. ) ;
#153645 = CARTESIAN_POINT ( 'NONE',  ( 23.14999999999999503, 11.65000000001116298, -146.1500000000000341 ) ) ;
#153646 = ORIENTED_EDGE ( 'NONE', *, *, #237163, .T. ) ;
#153647 = DIRECTION ( 'NONE',  ( 0.000000000000000000, 0.000000000000000000, 1.000000000000000000 ) ) ;
#153648 = PRODUCT_DEFINITION_SHAPE ( 'NONE', 'NONE',  #121752 ) ;
#153649 = FACE_OUTER_BOUND ( 'NONE', #26039, .T. ) ;
#153650 = CIRCLE ( 'NONE', #186939, 11.79999999999999716 ) ;
#153651 = CIRCLE ( 'NONE', #228442, 0.6000000000000033085 ) ;
#153652 = EDGE_CURVE ( 'NONE', #136022, #228701, #238666, .T. ) ;
#153653 = EDGE_CURVE ( 'NONE', #171995, #103813, #183875, .T. ) ;
#153654 = ORIENTED_EDGE ( 'NONE', *, *, #188288, .F. ) ;
#153655 = CARTESIAN_POINT ( 'NONE',  ( 18.49999999999999645, 76.00000000001126921, -203.5231074845248997 ) ) ;
#153656 = VERTEX_POINT ( 'NONE', #123870 ) ;
#153657 = CARTESIAN_POINT ( 'NONE',  ( -16.97683809663754673, 9.950000000011137047, -154.2284708321106166 ) ) ;
#153658 = DIRECTION ( 'NONE',  ( -0.7071067811865487940, -0.7071067811865463515, -4.937700262164522799E-15 ) ) ;
#153659 = DIRECTION ( 'NONE',  ( -1.000000000000000000, 2.849773892568378313E-16, -7.728835255496647986E-17 ) ) ;
#153660 = B_SPLINE_CURVE_WITH_KNOTS ( 'NONE', 3,
 ( #55278, #134823, #175300, #157008, #216941, #257308, #254751, #38335, #154456, #155735 ),
 .UNSPECIFIED., .F., .F.,
 ( 4, 3, 3, 4 ),
 ( 0.000000000000000000, 4.874959354402336225E-05, 9.785140065120830446E-05, 0.0001360444631935979931 ),
 .UNSPECIFIED. ) ;
#153661 = CARTESIAN_POINT ( 'NONE',  ( -20.85000000000000142, 7.661991824395936845, -241.5144583139544636 ) ) ;
#153663 = TOROIDAL_SURFACE ( 'NONE', #45460, 0.2000000000000000111, 0.1000000000000000056 ) ;
#153662 = DIRECTION ( 'NONE',  ( -0.000000000000000000, -1.000000000000000000, -6.982962677686266711E-15 ) ) ;
#153664 = CARTESIAN_POINT ( 'NONE',  ( 20.94999999999999929, 76.00000000001213607, -136.5231074845243313 ) ) ;
#153665 = DIRECTION ( 'NONE',  ( 0.000000000000000000, 0.000000000000000000, -1.000000000000000000 ) ) ;
#153666 = DIRECTION ( 'NONE',  ( 0.000000000000000000, -0.7960711469212456981, 0.6052030477777622375 ) ) ;
#153667 = AXIS2_PLACEMENT_3D ( 'NONE', #193131, #71903, #212693 ) ;
#153669 = CARTESIAN_POINT ( 'NONE',  ( 18.50000000000000000, -9.499999999988842703, -207.6001893912220169 ) ) ;
#153668 = CARTESIAN_POINT ( 'NONE',  ( -18.59999999999999787, 85.50000000001156764, -57.37310748452425457 ) ) ;
#153670 = EDGE_CURVE ( 'NONE', #200730, #62499, #46865, .T. ) ;
#153671 = DIRECTION ( 'NONE',  ( 1.000000000000000000, 0.000000000000000000, -0.000000000000000000 ) ) ;
#153672 = CIRCLE ( 'NONE', #257592, 4.300000000000025580 ) ;
#153673 = CYLINDRICAL_SURFACE ( 'NONE', #189646, 11.80000000000000426 ) ;
#153674 = DIRECTION ( 'NONE',  ( 1.000000000000000000, 0.000000000000000000, 0.000000000000000000 ) ) ;
#153675 = ORIENTED_EDGE ( 'NONE', *, *, #28609, .F. ) ;
#153676 = CARTESIAN_POINT ( 'NONE',  ( -20.99551997958347016, 11.75000000001097078, -93.65165913768963435 ) ) ;
#153677 = EDGE_CURVE ( 'NONE', #116470, #97927, #5157, .T. ) ;
#153678 = DIRECTION ( 'NONE',  ( 0.000000000000000000, -1.000000000000000000, 0.000000000000000000 ) ) ;
#153679 = CARTESIAN_POINT ( 'NONE',  ( 18.49999999999999289, 7.021664781911246322, -171.3335654018973173 ) ) ;
#153680 = VERTEX_POINT ( 'NONE', #243800 ) ;
#153681 = CARTESIAN_POINT ( 'NONE',  ( 23.24999999999999289, 5.950000000011163692, -190.6942976949651438 ) ) ;
#153683 = EDGE_CURVE ( 'NONE', #140456, #237761, #203400, .T. ) ;
#153682 = FACE_OUTER_BOUND ( 'NONE', #41474, .T. ) ;
#153684 = DIRECTION ( 'NONE',  ( 1.000000000000000000, 0.000000000000000000, 0.000000000000000000 ) ) ;
#153685 = ORIENTED_EDGE ( 'NONE', *, *, #45784, .T. ) ;
#153686 = ADVANCED_FACE ( 'NONE', ( #6465 ), #245085, .F. ) ;
#153687 = AXIS2_PLACEMENT_3D ( 'NONE', #149091, #66963, #147799 ) ;
#153688 = AXIS2_PLACEMENT_3D ( 'NONE', #62494, #80741, #166428 ) ;
#153689 = EDGE_CURVE ( 'NONE', #132861, #145347, #21404, .T. ) ;
#153690 = DIRECTION ( 'NONE',  ( 0.000000000000000000, 0.2128009952263603122, -0.9770955615653315052 ) ) ;
#153691 = ORIENTED_EDGE ( 'NONE', *, *, #182937, .T. ) ;
#153692 = CARTESIAN_POINT ( 'NONE',  ( 21.05000000000000071, -1.249999999988843369, -141.9000000000000341 ) ) ;
#153693 = DIRECTION ( 'NONE',  ( -1.000000000000000000, -0.000000000000000000, -0.000000000000000000 ) ) ;
#153694 = EDGE_CURVE ( 'NONE', #106082, #86886, #17295, .T. ) ;
#153695 = VERTEX_POINT ( 'NONE', #24788 ) ;
#153696 = CARTESIAN_POINT ( 'NONE',  ( 20.94999999999999929, -7.079251802663310222, -212.6676826711374417 ) ) ;
#153697 = ORIENTED_EDGE ( 'NONE', *, *, #211687, .T. ) ;
#153698 = ADVANCED_FACE ( 'NONE', ( #23510 ), #102989, .F. ) ;
#153699 = CARTESIAN_POINT ( 'NONE',  ( -20.94999999999999929, 87.65000000001192859, -100.1231074845242262 ) ) ;
#153700 = EDGE_CURVE ( 'NONE', #100104, #36544, #121622, .T. ) ;
#153701 = DIRECTION ( 'NONE',  ( 1.000000000000000000, -2.952720810173289112E-16, -2.061873921506763405E-30 ) ) ;
#153703 = DIRECTION ( 'NONE',  ( 0.000000000000000000, 1.000000000000000000, 0.000000000000000000 ) ) ;
#153702 = VECTOR ( 'NONE', #11257, 1000.000000000000000 ) ;
#153704 = DIRECTION ( 'NONE',  ( 0.000000000000000000, 0.000000000000000000, -1.000000000000000000 ) ) ;
#153705 = FACE_OUTER_BOUND ( 'NONE', #176436, .T. ) ;
#153706 = CARTESIAN_POINT ( 'NONE',  ( -15.70407651835960650, 47.70130725485975631, -234.3525798712488779 ) ) ;
#153707 = CARTESIAN_POINT ( 'NONE',  ( -20.65000000000000568, 5.650000000011139001, -143.2500000000000284 ) ) ;
#153708 = DIRECTION ( 'NONE',  ( 1.000000000000000000, 0.000000000000000000, 0.000000000000000000 ) ) ;
#153710 = ORIENTED_EDGE ( 'NONE', *, *, #238528, .F. ) ;
#153709 = CARTESIAN_POINT ( 'NONE',  ( 21.05000000000000071, 69.70076908992504627, -103.1215449845243626 ) ) ;
#153712 = FACE_OUTER_BOUND ( 'NONE', #223498, .T. ) ;
#153711 = FACE_OUTER_BOUND ( 'NONE', #161793, .T. ) ;
#153713 = ORIENTED_EDGE ( 'NONE', *, *, #124593, .F. ) ;
#153715 = EDGE_LOOP ( 'NONE', ( #126608, #252384, #155978, #216814 ) ) ;
#153714 = CARTESIAN_POINT ( 'NONE',  ( 20.94999999999999929, 85.00000000001159606, -59.62913836187181715 ) ) ;
#153716 = ORIENTED_EDGE ( 'NONE', *, *, #241530, .F. ) ;
#153717 = DIRECTION ( 'NONE',  ( -1.186688945009010077E-16, 1.000000000000000000, 0.000000000000000000 ) ) ;
#153718 = LINE ( 'NONE', #118393, #76159 ) ;
#153719 = CARTESIAN_POINT ( 'NONE',  ( 21.05000000000000071, 62.82351852614505106, -207.2177435922979214 ) ) ;
#153720 = CARTESIAN_POINT ( 'NONE',  ( 18.59999999999999787, -9.321008403361304318, -7.235938249077860540 ) ) ;
#153721 = DIRECTION ( 'NONE',  ( 0.000000000000000000, 0.000000000000000000, -1.000000000000000000 ) ) ;
#153722 = CARTESIAN_POINT ( 'NONE',  ( -23.15000000000000213, 11.75000000001115552, -121.8500000000000369 ) ) ;
#153723 = DIRECTION ( 'NONE',  ( 1.000000000000000000, 0.000000000000000000, 0.000000000000000000 ) ) ;
#153725 = ORIENTED_EDGE ( 'NONE', *, *, #237385, .F. ) ;
#153724 = ADVANCED_FACE ( 'NONE', ( #147264 ), #237854, .T. ) ;
#153726 = VERTEX_POINT ( 'NONE', #85977 ) ;
#153727 = CIRCLE ( 'NONE', #74601, 0.09999999999998898659 ) ;
#153728 = CARTESIAN_POINT ( 'NONE',  ( -23.15000000000000213, -8.999999999988846255, -177.3939691226524076 ) ) ;
#153729 = AXIS2_PLACEMENT_3D ( 'NONE', #175437, #154597, #30792 ) ;
#153730 = AXIS2_PLACEMENT_3D ( 'NONE', #206719, #230132, #47621 ) ;
#153731 = ADVANCED_FACE ( 'NONE', ( #183828 ), #163003, .T. ) ;
#153732 = EDGE_LOOP ( 'NONE', ( #135016, #32177, #114384, #180076 ) ) ;
#153733 = CARTESIAN_POINT ( 'NONE',  ( -18.50000000000000000, 64.25000000001173817, -81.27310748452440237 ) ) ;
#153734 = ORIENTED_EDGE ( 'NONE', *, *, #63460, .F. ) ;
#153735 = CARTESIAN_POINT ( 'NONE',  ( 18.50000000000000355, -9.421074344987191651, -40.32447205943020663 ) ) ;
#153736 = CIRCLE ( 'NONE', #162068, 0.1000000000000000472 ) ;
#153737 = LINE ( 'NONE', #54569, #238383 ) ;
#153738 = CYLINDRICAL_SURFACE ( 'NONE', #188757, 0.09999999999999939493 ) ;
#153739 = CARTESIAN_POINT ( 'NONE',  ( 21.05000000000000071, 11.43341603104965110, -245.8667934851861787 ) ) ;
#153740 = CARTESIAN_POINT ( 'NONE',  ( 21.59780538579341780, 75.90102133041474985, -210.3701980144676043 ) ) ;
#153741 = ORIENTED_EDGE ( 'NONE', *, *, #69694, .T. ) ;
#153742 = CARTESIAN_POINT ( 'NONE',  ( -18.46919391072053074, -9.670724388266537019, -207.6738035317995639 ) ) ;
#153744 = DIRECTION ( 'NONE',  ( -1.000000000000000000, 0.000000000000000000, -0.000000000000000000 ) ) ;
#153743 = CIRCLE ( 'NONE', #95425, 12.77500000000000924 ) ;
#153745 = AXIS2_PLACEMENT_3D ( 'NONE', #246534, #148741, #228275 ) ;
#153746 = CARTESIAN_POINT ( 'NONE',  ( 21.14999999999999858, 9.997527148596393687, -228.1702915402975407 ) ) ;
#153748 = CIRCLE ( 'NONE', #195230, 0.1000000000000053069 ) ;
#153747 = FACE_OUTER_BOUND ( 'NONE', #80643, .T. ) ;
#153749 = CARTESIAN_POINT ( 'NONE',  ( 20.95000000000000284, 11.60000000001116227, -160.5717967697245285 ) ) ;
#153750 = EDGE_CURVE ( 'NONE', #58852, #119168, #65154, .T. ) ;
#153751 = ORIENTED_EDGE ( 'NONE', *, *, #89824, .T. ) ;
#153753 = CARTESIAN_POINT ( 'NONE',  ( -18.59999994787167310, 85.52363768977302527, -29.14065794975181589 ) ) ;
#153752 = CARTESIAN_POINT ( 'NONE',  ( -21.05000000000000071, 36.65892442174472876, -249.5511627012454596 ) ) ;
#153754 = ORIENTED_EDGE ( 'NONE', *, *, #223064, .F. ) ;
#153757 = EDGE_LOOP ( 'NONE', ( #212545, #140227, #147251 ) ) ;
#153756 = DIRECTION ( 'NONE',  ( 0.000000000000000000, 0.000000000000000000, -1.000000000000000000 ) ) ;
#153755 = CARTESIAN_POINT ( 'NONE',  ( 20.94999999999999574, 87.75000000001190870, -99.92310748452422331 ) ) ;
#153758 = CIRCLE ( 'NONE', #41295, 0.09999999999999080458 ) ;
#153759 = SPHERICAL_SURFACE ( 'NONE', #189397, 0.1000000000000000056 ) ;
#153760 = CARTESIAN_POINT ( 'NONE',  ( -16.97683809663752186, 9.850000000011137402, -147.4023640181965220 ) ) ;
#153761 = ORIENTED_EDGE ( 'NONE', *, *, #192089, .F. ) ;
#153762 = DIRECTION ( 'NONE',  ( 1.000000000000000000, 0.000000000000000000, 0.000000000000000000 ) ) ;
#153764 = CARTESIAN_POINT ( 'NONE',  ( 23.40000000000005187, 76.00000000001119815, -36.02310748452479316 ) ) ;
#153763 =( BOUNDED_CURVE ( )  B_SPLINE_CURVE ( 3, ( #98886, #139308, #40265, #20692 ),
 .UNSPECIFIED., .F., .F. ) 
 B_SPLINE_CURVE_WITH_KNOTS ( ( 4, 4 ),
 ( 4.712388980384690562, 6.283185307179586232 ),
 .UNSPECIFIED. ) 
 CURVE ( )  GEOMETRIC_REPRESENTATION_ITEM ( )  RATIONAL_B_SPLINE_CURVE ( ( 1.000000000000000000, 0.8047378541243652705, 0.8047378541243652705, 1.000000000000000000 ) ) 
 REPRESENTATION_ITEM ( '' )  );
#153765 = CARTESIAN_POINT ( 'NONE',  ( -22.49510344025093644, -3.108862830562444834, -228.1724956784199208 ) ) ;
#153767 = VERTEX_POINT ( 'NONE', #125151 ) ;
#153766 = PLANE ( 'NONE',  #97569 ) ;
#153768 = ORIENTED_EDGE ( 'NONE', *, *, #25153, .T. ) ;
#153769 = DIRECTION ( 'NONE',  ( 0.000000000000000000, 0.000000000000000000, 1.000000000000000000 ) ) ;
#153770 = DIRECTION ( 'NONE',  ( 0.000000000000000000, 0.9876197685951252359, -0.1568667991644863424 ) ) ;
#153771 = CIRCLE ( 'NONE', #224439, 1.749999999999998002 ) ;
#153772 = AXIS2_PLACEMENT_3D ( 'NONE', #179942, #160395, #239917 ) ;
#153773 = LINE ( 'NONE', #169475, #92566 ) ;
#153774 = ORIENTED_EDGE ( 'NONE', *, *, #101873, .T. ) ;
#153775 = DIRECTION ( 'NONE',  ( 1.000000000000000000, 0.000000000000000000, 0.000000000000000000 ) ) ;
#153776 = CARTESIAN_POINT ( 'NONE',  ( 23.15000000000000213, -6.688413578037176066, -212.5825622730469036 ) ) ;
#153777 = DIRECTION ( 'NONE',  ( 0.000000000000000000, -1.000000000000000000, 6.308085367188393199E-16 ) ) ;
#153778 = AXIS2_PLACEMENT_3D ( 'NONE', #40943, #199996, #21374 ) ;
#153779 = ORIENTED_EDGE ( 'NONE', *, *, #168813, .F. ) ;
#153780 = CARTESIAN_POINT ( 'NONE',  ( 20.21567752745037794, 59.45201827013453055, -225.5779475914478382 ) ) ;
#153781 = FACE_OUTER_BOUND ( 'NONE', #72399, .T. ) ;
#153782 = EDGE_CURVE ( 'NONE', #212682, #211698, #25042, .T. ) ;
#153783 = EDGE_LOOP ( 'NONE', ( #196092, #109237, #28197, #77112 ) ) ;
#153785 = VECTOR ( 'NONE', #203894, 1000.000000000000000 ) ;
#153784 = DIRECTION ( 'NONE',  ( 0.000000000000000000, -1.000000000000000000, -6.982962677686265922E-15 ) ) ;
#153786 = CARTESIAN_POINT ( 'NONE',  ( -21.05000000000000071, 85.51932773110434027, -96.05013110796491560 ) ) ;
#153787 = DIRECTION ( 'NONE',  ( 0.000000000000000000, 0.9126074666063660468, 0.4088369013363524762 ) ) ;
#153788 = AXIS2_PLACEMENT_3D ( 'NONE', #175138, #169998, #91696 ) ;
#153789 = ORIENTED_EDGE ( 'NONE', *, *, #222391, .T. ) ;
#153790 = VERTEX_POINT ( 'NONE', #204658 ) ;
#153791 = TOROIDAL_SURFACE ( 'NONE', #187072, 0.9750000000000019762, 0.1000000000000000056 ) ;
#153792 = EDGE_CURVE ( 'NONE', #139556, #166926, #225493, .T. ) ;
#153793 = DIRECTION ( 'NONE',  ( 0.000000000000000000, 6.982962677686266711E-15, -1.000000000000000000 ) ) ;
#153794 = EDGE_LOOP ( 'NONE', ( #101166, #62116, #114348, #1187 ) ) ;
#153796 = ORIENTED_EDGE ( 'NONE', *, *, #179175, .F. ) ;
#153795 = DIRECTION ( 'NONE',  ( -0.000000000000000000, -0.1298341882519953583, -0.9915357197604862671 ) ) ;
#153797 = EDGE_CURVE ( 'NONE', #91963, #183616, #83869, .T. ) ;
#153798 = CIRCLE ( 'NONE', #28904, 0.1000000000000000472 ) ;
#153799 = AXIS2_PLACEMENT_3D ( 'NONE', #251090, #192426, #202375 ) ;
#153802 = ORIENTED_EDGE ( 'NONE', *, *, #201979, .T. ) ;
#153801 = ORIENTED_EDGE ( 'NONE', *, *, #27334, .F. ) ;
#153800 = CARTESIAN_POINT ( 'NONE',  ( -20.94999999999999929, 8.001317420522642720, -237.7387931148579980 ) ) ;
#153803 = CARTESIAN_POINT ( 'NONE',  ( -20.94999999999999929, 11.65000000001115588, -40.51480577065400013 ) ) ;
#153804 = ADVANCED_FACE ( 'NONE', ( #172013 ), #72902, .T. ) ;
#153805 = DIRECTION ( 'NONE',  ( 0.000000000000000000, 2.851451713636794872E-13, 1.000000000000000000 ) ) ;
#153806 = CARTESIAN_POINT ( 'NONE',  ( 21.11701782572533048, 10.72160911601861244, -112.7450374295112567 ) ) ;
#153807 = CARTESIAN_POINT ( 'NONE',  ( -18.59999999999999787, 43.35377423437995503, -245.1717807829448930 ) ) ;
#153808 = CIRCLE ( 'NONE', #41355, 0.09999999999999489853 ) ;
#153809 = DIRECTION ( 'NONE',  ( 0.000000000000000000, 0.000000000000000000, -1.000000000000000000 ) ) ;
#153810 = CARTESIAN_POINT ( 'NONE',  ( 20.94999999999999929, 55.99424519013661694, -234.9720658648265896 ) ) ;
#153811 = ORIENTED_EDGE ( 'NONE', *, *, #177148, .F. ) ;
#153812 = CIRCLE ( 'NONE', #41357, 0.09999999999998898659 ) ;
#153813 = ORIENTED_EDGE ( 'NONE', *, *, #3416, .F. ) ;
#153814 = AXIS2_PLACEMENT_3D ( 'NONE', #84472, #164072, #124943 ) ;
#153815 = VERTEX_POINT ( 'NONE', #132857 ) ;
#153816 = FACE_OUTER_BOUND ( 'NONE', #228511, .T. ) ;
#153817 = ORIENTED_EDGE ( 'NONE', *, *, #14613, .F. ) ;
#153818 = DIRECTION ( 'NONE',  ( 1.000000000000000000, -2.952720810173289112E-16, -2.061873921506763405E-30 ) ) ;
#153819 = ORIENTED_EDGE ( 'NONE', *, *, #74007, .T. ) ;
#153820 = CIRCLE ( 'NONE', #257759, 11.70000000000000639 ) ;
#153821 = ADVANCED_FACE ( 'NONE', ( #148562 ), #228105, .F. ) ;
#153822 = VERTEX_POINT ( 'NONE', #114566 ) ;
#153823 = DIRECTION ( 'NONE',  ( 2.952720810173288619E-16, -0.4721928772777346239, -0.8814952561688430555 ) ) ;
#153824 = ORIENTED_EDGE ( 'NONE', *, *, #211331, .T. ) ;
#153825 = CARTESIAN_POINT ( 'NONE',  ( -22.50000000000000000, 7.128833340093095217, -233.7327013124392749 ) ) ;
#153826 = DIRECTION ( 'NONE',  ( -1.000000000000000000, 0.000000000000000000, 0.000000000000000000 ) ) ;
#153827 = TOROIDAL_SURFACE ( 'NONE', #195316, 12.97499999999999609, 0.1000000000000000056 ) ;
#153829 = VERTEX_POINT ( 'NONE', #251494 ) ;
#153828 = EDGE_LOOP ( 'NONE', ( #167248, #10959, #82358, #202888 ) ) ;
#153830 = EDGE_LOOP ( 'NONE', ( #79912, #123262, #234529, #191529 ) ) ;
#153831 = CARTESIAN_POINT ( 'NONE',  ( 21.05000000000000071, 8.776282895292474961, -8.488000721584361585 ) ) ;
#153832 = VERTEX_POINT ( 'NONE', #231965 ) ;
#153833 = ORIENTED_EDGE ( 'NONE', *, *, #24142, .F. ) ;
#153834 = CARTESIAN_POINT ( 'NONE',  ( -20.54999999999999716, 76.00000000001165290, -69.52310748452431710 ) ) ;
#153836 = ORIENTED_EDGE ( 'NONE', *, *, #227569, .F. ) ;
#153835 = DIRECTION ( 'NONE',  ( 0.000000000000000000, 0.000000000000000000, 1.000000000000000000 ) ) ;
#153837 = DIRECTION ( 'NONE',  ( -0.000000000000000000, 6.982962677686266711E-15, -1.000000000000000000 ) ) ;
#153839 = LINE ( 'NONE', #55940, #252738 ) ;
#153838 = CYLINDRICAL_SURFACE ( 'NONE', #148944, 0.1000000000000028644 ) ;
#153840 = DIRECTION ( 'NONE',  ( 0.000000000000000000, 0.000000000000000000, -1.000000000000000000 ) ) ;
#153841 = DIRECTION ( 'NONE',  ( -1.000000000000000000, -0.000000000000000000, 0.000000000000000000 ) ) ;
#153842 = DIRECTION ( 'NONE',  ( 2.952720810173289112E-16, 1.000000000000000000, 6.982962677686266711E-15 ) ) ;
#153843 = ORIENTED_EDGE ( 'NONE', *, *, #229330, .F. ) ;
#153844 = CIRCLE ( 'NONE', #28946, 2.000000000000002665 ) ;
#153845 = ORIENTED_EDGE ( 'NONE', *, *, #52722, .T. ) ;
#153846 = DIRECTION ( 'NONE',  ( -1.000000000000000000, 0.000000000000000000, -0.000000000000000000 ) ) ;
#153847 = DIRECTION ( 'NONE',  ( -1.000000000000000000, -0.000000000000000000, -0.000000000000000000 ) ) ;
#153848 = CARTESIAN_POINT ( 'NONE',  ( 21.05000000000000071, 36.65892442174935439, -249.5511627012433848 ) ) ;
#153849 = AXIS2_PLACEMENT_3D ( 'NONE', #222547, #84279, #221265 ) ;
#153850 = ORIENTED_EDGE ( 'NONE', *, *, #46487, .T. ) ;
#153851 = CARTESIAN_POINT ( 'NONE',  ( -16.98495255085916611, 30.24612551772337810, -234.7653289254189417 ) ) ;
#153852 = AXIS2_PLACEMENT_3D ( 'NONE', #154212, #95465, #211574 ) ;
#153853 = EDGE_CURVE ( 'NONE', #118873, #6716, #38145, .T. ) ;
#153854 = FACE_OUTER_BOUND ( 'NONE', #236660, .T. ) ;
#153855 = CARTESIAN_POINT ( 'NONE',  ( -23.25000000000000000, 1.115600667400684642E-11, -67.00000000000004263 ) ) ;
#153856 = ORIENTED_EDGE ( 'NONE', *, *, #62005, .T. ) ;
#153857 = ORIENTED_EDGE ( 'NONE', *, *, #160485, .T. ) ;
#153858 =( BOUNDED_SURFACE ( )  B_SPLINE_SURFACE ( 3, 2, ( 
 ( #199793, #180221, #21164 ),
 ( #61548, #103213, #197193 ),
 ( #101920, #138480, #122817 ),
 ( #62824, #1553, #43269 ) ),
 .UNSPECIFIED., .F., .F., .F. ) 
 B_SPLINE_SURFACE_WITH_KNOTS ( ( 4, 4 ),
 ( 3, 3 ),
 ( 3.239053990300444497E-18, 0.0003124336600439674345 ),
 ( 0.000000000000000000, 1.000000000000000000 ),
 .UNSPECIFIED. ) 
 GEOMETRIC_REPRESENTATION_ITEM ( )  RATIONAL_B_SPLINE_SURFACE ( (
 ( 1.000000000000000000, 0.7071067811865475727, 1.000000000000000000),
 ( 1.000000000000000000, 0.7089187706049921989, 1.000000000000000000),
 ( 1.000000000000000000, 0.7039288185051796320, 1.000000000000000000),
 ( 1.000000000000000000, 0.7040654476015839602, 1.000000000000000000) ) ) 
 REPRESENTATION_ITEM ( '' )  SURFACE ( )  );
#153859 = CARTESIAN_POINT ( 'NONE',  ( -21.44999999999999929, 7.150000000011155876, -179.8499999999999943 ) ) ;
#153860 = DIRECTION ( 'NONE',  ( 0.000000000000000000, 0.000000000000000000, -1.000000000000000000 ) ) ;
#153861 = ORIENTED_EDGE ( 'NONE', *, *, #171635, .F. ) ;
#153862 = CARTESIAN_POINT ( 'NONE',  ( 20.85000000000000142, -1.263275465206102233, -141.9018646667464338 ) ) ;
#153863 = ORIENTED_EDGE ( 'NONE', *, *, #134117, .F. ) ;
#153864 = DIRECTION ( 'NONE',  ( 0.000000000000000000, 1.224646799142185182E-16, 1.000000000000000000 ) ) ;
#153866 = EDGE_CURVE ( 'NONE', #106114, #39467, #87981, .T. ) ;
#153865 = DIRECTION ( 'NONE',  ( 0.000000000000000000, -0.4721928772777346239, -0.8814952561688430555 ) ) ;
#153868 = PLANE ( 'NONE',  #257558 ) ;
#153867 = DIRECTION ( 'NONE',  ( 0.000000000000000000, 0.000000000000000000, 1.000000000000000000 ) ) ;
#153869 = CIRCLE ( 'NONE', #45477, 12.87499999999999822 ) ;
#153870 = CARTESIAN_POINT ( 'NONE',  ( 18.50211644919735221, 65.69792220476372790, -164.5335554128461979 ) ) ;
#153871 = CARTESIAN_POINT ( 'NONE',  ( 21.05933563467872105, 65.27547528793053289, -90.82945973556843455 ) ) ;
#153872 = AXIS2_PLACEMENT_3D ( 'NONE', #127787, #63954, #86044 ) ;
#153873 = ADVANCED_FACE ( 'NONE', ( #131557 ), #29916, .F. ) ;
#153874 = EDGE_CURVE ( 'NONE', #2636, #246153, #33903, .T. ) ;
#153875 = LINE ( 'NONE', #209957, #206560 ) ;
#153876 = AXIS2_PLACEMENT_3D ( 'NONE', #207584, #228430, #125470 ) ;
#153878 = ORIENTED_EDGE ( 'NONE', *, *, #95887, .F. ) ;
#153877 = ORIENTED_EDGE ( 'NONE', *, *, #163455, .F. ) ;
#153879 = VERTEX_POINT ( 'NONE', #70337 ) ;
#153880 = SPHERICAL_SURFACE ( 'NONE', #254291, 0.1000000000000000056 ) ;
#153881 = CARTESIAN_POINT ( 'NONE',  ( 23.24999999999999645, 71.22429906543214884, -57.67433938047838637 ) ) ;
#153882 = EDGE_CURVE ( 'NONE', #19574, #29111, #192827, .T. ) ;
#153883 = DIRECTION ( 'NONE',  ( 1.000000000000000000, -0.000000000000000000, -0.000000000000000000 ) ) ;
#153884 = EDGE_CURVE ( 'NONE', #16612, #184466, #129704, .T. ) ;
#153886 = CARTESIAN_POINT ( 'NONE',  ( -13.12432614554023402, 66.56923500458954379, -87.79257008977393184 ) ) ;
#153885 = CARTESIAN_POINT ( 'NONE',  ( -18.50000000000000000, 77.68707439010402993, -182.8376804510660065 ) ) ;
#153887 = DIRECTION ( 'NONE',  ( -3.469446951953515108E-14, -1.000000000000000000, 0.000000000000000000 ) ) ;
#153888 = ORIENTED_EDGE ( 'NONE', *, *, #170689, .F. ) ;
#153889 = EDGE_CURVE ( 'NONE', #174500, #241398, #252773, .T. ) ;
#153890 = DIRECTION ( 'NONE',  ( 0.000000000000000000, 0.000000000000000000, -1.000000000000000000 ) ) ;
#153891 = VERTEX_POINT ( 'NONE', #248952 ) ;
#153892 = VERTEX_POINT ( 'NONE', #229388 ) ;
#153893 = CARTESIAN_POINT ( 'NONE',  ( -21.04999999999999716, 69.55922910634974698, -69.50551029751636634 ) ) ;
#153894 = CARTESIAN_POINT ( 'NONE',  ( -22.47886152344871036, 0.03750093887284931121, -88.85001135695209484 ) ) ;
#153895 = DIRECTION ( 'NONE',  ( 1.000000000000000000, 0.000000000000000000, 0.000000000000000000 ) ) ;
#153896 = VECTOR ( 'NONE', #187664, 1000.000000000000000 ) ;
#153897 = CARTESIAN_POINT ( 'NONE',  ( 21.00000000000000000, 9.750000000011153745, -155.1500000000000057 ) ) ;
#153898 = CARTESIAN_POINT ( 'NONE',  ( -23.15000000000000213, 76.00000000001197975, -107.0731074845243143 ) ) ;
#153899 = ORIENTED_EDGE ( 'NONE', *, *, #68217, .T. ) ;
#153900 = VERTEX_POINT ( 'NONE', #50705 ) ;
#153901 = CARTESIAN_POINT ( 'NONE',  ( -20.54999999999999716, 76.00000000001213607, -136.5231074845243313 ) ) ;
#153902 = EDGE_CURVE ( 'NONE', #127248, #139087, #242122, .T. ) ;
#153903 = DIRECTION ( 'NONE',  ( 0.000000000000000000, 0.000000000000000000, -1.000000000000000000 ) ) ;
#153904 = EDGE_CURVE ( 'NONE', #88487, #216022, #138066, .T. ) ;
#153905 = CARTESIAN_POINT ( 'NONE',  ( 18.54999999999999716, 8.750000000011182166, -42.75000000000000000 ) ) ;
#153906 = CARTESIAN_POINT ( 'NONE',  ( -20.64999999999999858, 4.350000000011156054, -45.85000000000000142 ) ) ;
#153907 = ADVANCED_FACE ( 'NONE', ( #153747 ), #54580, .T. ) ;
#153908 = LINE ( 'NONE', #151304, #175286 ) ;
#153909 = CARTESIAN_POINT ( 'NONE',  ( -15.75000000000000355, 66.65000000001204228, -119.7731074845243739 ) ) ;
#153910 = CARTESIAN_POINT ( 'NONE',  ( -21.05000000000000071, 11.65000000000000036, -0.1000000000000028644 ) ) ;
#153912 = DIRECTION ( 'NONE',  ( 0.000000000000000000, -7.056502275159890832E-15, 1.000000000000000000 ) ) ;
#153911 = CARTESIAN_POINT ( 'NONE',  ( -22.43310005002225438, 0.005636942140875567109, 11.64966212713439830 ) ) ;
#153913 = CARTESIAN_POINT ( 'NONE',  ( -23.15000000000000213, 19.93396995659179893, -235.7707092203739307 ) ) ;
#153914 = DIRECTION ( 'NONE',  ( 0.000000000000000000, 0.000000000000000000, -1.000000000000000000 ) ) ;
#153915 = AXIS2_PLACEMENT_3D ( 'NONE', #167447, #246942, #141426 ) ;
#153916 = CIRCLE ( 'NONE', #137279, 0.09999999999998898659 ) ;
#153917 = DIRECTION ( 'NONE',  ( 1.000000000000000000, 0.000000000000000000, 0.000000000000000000 ) ) ;
#153918 = CARTESIAN_POINT ( 'NONE',  ( 20.86777300164945004, 10.33200063080771969, -139.5931674956643462 ) ) ;
#153919 = CIRCLE ( 'NONE', #41447, 0.09999999999998898659 ) ;
#153920 = VECTOR ( 'NONE', #229528, 999.9999999999998863 ) ;
#153922 = EDGE_LOOP ( 'NONE', ( #194363, #64207, #119048, #212755 ) ) ;
#153921 = CARTESIAN_POINT ( 'NONE',  ( 18.59999999999999432, -9.480686695267811714, -140.9411151687579036 ) ) ;
#153923 = AXIS2_PLACEMENT_3D ( 'NONE', #172218, #76905, #212591 ) ;
#153924 = EDGE_CURVE ( 'NONE', #109830, #3891, #130260, .T. ) ;
#153925 = EDGE_CURVE ( 'NONE', #95684, #90874, #238024, .T. ) ;
#153926 = DIRECTION ( 'NONE',  ( 0.000000000000000000, -7.026728003956683390E-15, 1.000000000000000000 ) ) ;
#153927 = AXIS2_PLACEMENT_3D ( 'NONE', #115585, #197681, #234241 ) ;
#153928 = CIRCLE ( 'NONE', #103950, 0.09999999999999939493 ) ;
#153929 = EDGE_CURVE ( 'NONE', #76475, #160738, #258007, .T. ) ;
#153931 = VECTOR ( 'NONE', #229038, 1000.000000000000000 ) ;
#153930 = DIRECTION ( 'NONE',  ( -2.561896900575096011E-15, 0.5907332058517336115, -0.8068669527896984439 ) ) ;
#153932 = CARTESIAN_POINT ( 'NONE',  ( 12.33938619321247998, 9.360723793997191677, -84.31392719460676233 ) ) ;
#153933 = DIRECTION ( 'NONE',  ( 1.000000000000000000, 0.000000000000000000, 0.000000000000000000 ) ) ;
#153934 = DIRECTION ( 'NONE',  ( 0.000000000000000000, -1.000000000000000000, 0.000000000000000000 ) ) ;
#153935 = DIRECTION ( 'NONE',  ( 1.000000000000000000, 0.000000000000000000, 0.000000000000000000 ) ) ;
#153936 = CYLINDRICAL_SURFACE ( 'NONE', #236319, 1.749999999999998002 ) ;
#153937 = VERTEX_POINT ( 'NONE', #247653 ) ;
#153938 = CARTESIAN_POINT ( 'NONE',  ( -21.44999999999999929, 9.593045456726526865, -211.4478935133083439 ) ) ;
#153939 = ORIENTED_EDGE ( 'NONE', *, *, #210439, .T. ) ;
#153940 = FACE_OUTER_BOUND ( 'NONE', #3218, .T. ) ;
#153941 = CARTESIAN_POINT ( 'NONE',  ( -21.78635804494510708, 68.96433851485919320, -170.1221125500320852 ) ) ;
#153942 = CARTESIAN_POINT ( 'NONE',  ( -22.59999985501179154, 31.79527822860976016, -238.8549629533907250 ) ) ;
#153943 = ORIENTED_EDGE ( 'NONE', *, *, #98770, .F. ) ;
#153944 = DIRECTION ( 'NONE',  ( 1.000000000000000000, 2.952720810173289112E-16, -0.000000000000000000 ) ) ;
#153945 = EDGE_CURVE ( 'NONE', #125534, #99579, #212916, .T. ) ;
#153946 = APPLICATION_PROTOCOL_DEFINITION ( 'draft international standard', 'automotive_design', 1998, #125842 ) ;
#153947 = CARTESIAN_POINT ( 'NONE',  ( -22.50000000000000000, 0.000000000000000000, 0.000000000000000000 ) ) ;
#153948 = DIRECTION ( 'NONE',  ( 1.000000000000000000, 0.000000000000000000, 0.000000000000000000 ) ) ;
#153949 = VERTEX_POINT ( 'NONE', #94993 ) ;
#153951 = EDGE_CURVE ( 'NONE', #151179, #10849, #168290, .T. ) ;
#153950 = DIRECTION ( 'NONE',  ( -1.000000000000000000, 0.000000000000000000, 0.000000000000000000 ) ) ;
#153952 = CARTESIAN_POINT ( 'NONE',  ( 20.94999999999999929, 10.72371710471867701, -175.1649135690875880 ) ) ;
#153953 = AXIS2_PLACEMENT_3D ( 'NONE', #108102, #204612, #83365 ) ;
#153954 = ADVANCED_FACE ( 'NONE', ( #256582 ), #237079, .T. ) ;
#153955 = EDGE_CURVE ( 'NONE', #208289, #240530, #60993, .T. ) ;
#153956 = CARTESIAN_POINT ( 'NONE',  ( 20.95443524775735256, 8.878554263883970066, -176.0337222756001267 ) ) ;
#153957 = ORIENTED_EDGE ( 'NONE', *, *, #59158, .F. ) ;
#153958 = VECTOR ( 'NONE', #151602, 1000.000000000000000 ) ;
#153959 = EDGE_LOOP ( 'NONE', ( #138227, #105514, #232068, #12665 ) ) ;
#153960 = EDGE_CURVE ( 'NONE', #139652, #120723, #118424, .T. ) ;
#153961 = DIRECTION ( 'NONE',  ( 0.000000000000000000, -0.2128009952263604232, 0.9770955615653316162 ) ) ;
#153962 = LINE ( 'NONE', #176070, #107026 ) ;
#153963 = CARTESIAN_POINT ( 'NONE',  ( 23.24999999999999645, 72.10000000001170406, -69.52310748452433131 ) ) ;
#153964 = DIRECTION ( 'NONE',  ( 1.000000000000000000, -0.000000000000000000, 0.000000000000000000 ) ) ;
#153966 = CARTESIAN_POINT ( 'NONE',  ( 20.94999999999999929, -8.999999999988842703, -124.1060308773475924 ) ) ;
#153965 = DIRECTION ( 'NONE',  ( 0.000000000000000000, -6.982962677686266711E-15, 1.000000000000000000 ) ) ;
#153967 = DIRECTION ( 'NONE',  ( 0.000000000000000000, -0.5000000000000004441, -0.8660254037844384856 ) ) ;
#153968 = FACE_OUTER_BOUND ( 'NONE', #12471, .T. ) ;
#153969 = DIRECTION ( 'NONE',  ( 0.000000000000000000, 6.308085367182471812E-16, 1.000000000000000000 ) ) ;
#153970 = CARTESIAN_POINT ( 'NONE',  ( -21.45000000000000284, 68.29142135624960019, -157.6731074845243938 ) ) ;
#153971 = VERTEX_POINT ( 'NONE', #234498 ) ;
#153972 = EDGE_CURVE ( 'NONE', #237661, #21030, #79616, .T. ) ;
#153973 = ORIENTED_EDGE ( 'NONE', *, *, #61995, .F. ) ;
#153974 = CARTESIAN_POINT ( 'NONE',  ( 18.52928932188133970, 65.72071067813064360, -115.1731074845243796 ) ) ;
#153976 = ADVANCED_FACE ( 'NONE', ( #58406 ), #137955, .T. ) ;
#153975 = AXIS2_PLACEMENT_3D ( 'NONE', #3, #19591, #238628 ) ;
#153977 = CARTESIAN_POINT ( 'NONE',  ( -16.91256925476569606, 66.01426884188406063, -149.0554649955191735 ) ) ;
#153979 = DIRECTION ( 'NONE',  ( 0.000000000000000000, 0.000000000000000000, -1.000000000000000000 ) ) ;
#153978 = DIRECTION ( 'NONE',  ( -2.952720810173289112E-16, -1.000000000000000000, -6.982962677686266711E-15 ) ) ;
#153980 = AXIS2_PLACEMENT_3D ( 'NONE', #35858, #95789, #175381 ) ;
#153981 = CARTESIAN_POINT ( 'NONE',  ( -18.40000000000000213, 64.25000000001222134, -145.7731074845244450 ) ) ;
#153983 = EDGE_CURVE ( 'NONE', #253379, #14829, #112959, .T. ) ;
#153982 = CARTESIAN_POINT ( 'NONE',  ( -21.14999999999994174, 74.25000000001119815, -47.64205752314703801 ) ) ;
#153984 = CARTESIAN_POINT ( 'NONE',  ( 12.26145404764308111, 12.75065881068273654, -215.6014281960218852 ) ) ;
#153985 = ORIENTED_EDGE ( 'NONE', *, *, #132931, .T. ) ;
#153986 = AXIS2_PLACEMENT_3D ( 'NONE', #136854, #152607, #194297 ) ;
#153987 = ORIENTED_EDGE ( 'NONE', *, *, #91706, .T. ) ;
#153988 = DIRECTION ( 'NONE',  ( 0.000000000000000000, 0.000000000000000000, 1.000000000000000000 ) ) ;
#153989 = ORIENTED_EDGE ( 'NONE', *, *, #144943, .F. ) ;
#153990 = DIRECTION ( 'NONE',  ( 0.000000000000000000, 6.982962677686266711E-15, -1.000000000000000000 ) ) ;
#153991 = EDGE_CURVE ( 'NONE', #70808, #165685, #8914, .T. ) ;
#153992 = AXIS2_PLACEMENT_3D ( 'NONE', #97037, #193623, #176644 ) ;
#153993 = CARTESIAN_POINT ( 'NONE',  ( 18.69999999999999929, -11.65000000000000036, 0.000000000000000000 ) ) ;
#153994 = CIRCLE ( 'NONE', #257933, 0.09999999999999939493 ) ;
#153996 = CIRCLE ( 'NONE', #58241, 0.09999999999998898659 ) ;
#153995 = FACE_OUTER_BOUND ( 'NONE', #173874, .T. ) ;
#153997 = AXIS2_PLACEMENT_3D ( 'NONE', #97317, #176924, #253848 ) ;
#153998 = AXIS2_PLACEMENT_3D ( 'NONE', #58373, #157552, #36297 ) ;
#153999 = EDGE_CURVE ( 'NONE', #195524, #102524, #115848, .T. ) ;
#154000 = EDGE_LOOP ( 'NONE', ( #105660, #111777, #115434, #84285, #184892 ) ) ;
#154001 = DIRECTION ( 'NONE',  ( -1.000000000000000000, 0.000000000000000000, 0.000000000000000000 ) ) ;
#154002 = B_SPLINE_CURVE_WITH_KNOTS ( 'NONE', 3,
 ( #149544, #213324, #93384, #11294, #36002, #169117, #34731, #154680, #174263, #115514 ),
 .UNSPECIFIED., .F., .F.,
 ( 4, 3, 3, 4 ),
 ( 1.894194122894209342E-15, 3.877043166999333273E-05, 7.336897548476464001E-05, 7.659383120239687261E-05 ),
 .UNSPECIFIED. ) ;
#154003 = CIRCLE ( 'NONE', #204004, 0.09999999999998898659 ) ;
#154004 = EDGE_CURVE ( 'NONE', #60346, #98150, #225537, .T. ) ;
#154005 = CARTESIAN_POINT ( 'NONE',  ( -20.54999999999999716, 61.88149656937975607, -248.1136133839584090 ) ) ;
#154006 = ADVANCED_FACE ( 'NONE', ( #136676 ), #37611, .T. ) ;
#154007 = DIRECTION ( 'NONE',  ( 0.000000000000000000, 6.982962677686266711E-15, -1.000000000000000000 ) ) ;
#154008 = CARTESIAN_POINT ( 'NONE',  ( -21.14999999999999858, -0.09999999998884338825, -155.8504291924551808 ) ) ;
#154009 = CARTESIAN_POINT ( 'NONE',  ( -23.25000000000000000, 77.16412189325360771, -162.1082593989527254 ) ) ;
#154010 = DIRECTION ( 'NONE',  ( 0.000000000000000000, -7.026728003956695223E-15, 1.000000000000000000 ) ) ;
#154011 = DIRECTION ( 'NONE',  ( 0.000000000000000000, 0.000000000000000000, -1.000000000000000000 ) ) ;
#154013 = ORIENTED_EDGE ( 'NONE', *, *, #96157, .T. ) ;
#154012 = B_SPLINE_CURVE_WITH_KNOTS ( 'NONE', 3,
 ( #33253, #11091, #73655, #28106, #107611, #51462, #227558, #250958, #192298, #171480 ),
 .UNSPECIFIED., .F., .F.,
 ( 4, 3, 3, 4 ),
 ( 0.000000000000000000, 0.0002000000000008536833, 0.001000000000082972495, 0.001967863649483305062 ),
 .UNSPECIFIED. ) ;
#154015 = CARTESIAN_POINT ( 'NONE',  ( -20.85000000000000142, 6.846123162363745074, -204.7377262668498190 ) ) ;
#154014 = CARTESIAN_POINT ( 'NONE',  ( -23.25000000000000000, -0.09999999998884338825, -122.3504291924552234 ) ) ;
#154016 = VERTEX_POINT ( 'NONE', #18021 ) ;
#154018 = VERTEX_POINT ( 'NONE', #97527 ) ;
#154017 = CARTESIAN_POINT ( 'NONE',  ( -23.25000000000000355, 11.75000000001113953, -121.3500000000000369 ) ) ;
#154019 = ORIENTED_EDGE ( 'NONE', *, *, #256033, .F. ) ;
#154020 = DIRECTION ( 'NONE',  ( -1.000000000000000000, 0.000000000000000000, 0.000000000000000000 ) ) ;
#154021 = PLANE ( 'NONE',  #88433 ) ;
#154022 = DIRECTION ( 'NONE',  ( 1.000000000000000000, 0.000000000000000000, 0.000000000000000000 ) ) ;
#154023 = CARTESIAN_POINT ( 'NONE',  ( 22.50000000000000000, 1.115600667400684642E-11, -167.4999999999999716 ) ) ;
#154024 = VERTEX_POINT ( 'NONE', #19310 ) ;
#154025 = EDGE_CURVE ( 'NONE', #188047, #89128, #92465, .T. ) ;
#154026 = SURFACE_STYLE_FILL_AREA ( #236072 ) ;
#154027 = DIRECTION ( 'NONE',  ( 0.000000000000000000, 0.000000000000000000, -1.000000000000000000 ) ) ;
#154028 = EDGE_LOOP ( 'NONE', ( #208202, #225644, #176298, #242795 ) ) ;
#154029 = CIRCLE ( 'NONE', #104057, 0.2000000000000057288 ) ;
#154030 = CARTESIAN_POINT ( 'NONE',  ( 21.05000000000000071, -3.444512620907433487, -226.2123967847655308 ) ) ;
#154031 = AXIS2_PLACEMENT_3D ( 'NONE', #10786, #254190, #36476 ) ;
#154032 = CARTESIAN_POINT ( 'NONE',  ( -23.15000000000000213, -4.660452010345190743, -233.2299579127752054 ) ) ;
#154033 = VERTEX_POINT ( 'NONE', #220082 ) ;
#154034 = VERTEX_POINT ( 'NONE', #199245 ) ;
#154035 = FACE_OUTER_BOUND ( 'NONE', #251463, .T. ) ;
#154036 = CIRCLE ( 'NONE', #179136, 0.1000000000000028644 ) ;
#154037 = ORIENTED_EDGE ( 'NONE', *, *, #94659, .T. ) ;
#154038 = DIRECTION ( 'NONE',  ( 1.000000000000000000, -2.849773892568378313E-16, 7.728835255496647986E-17 ) ) ;
#154039 = ORIENTED_EDGE ( 'NONE', *, *, #52959, .T. ) ;
#154040 = LINE ( 'NONE', #56150, #159428 ) ;
#154041 = EDGE_CURVE ( 'NONE', #231547, #85475, #192263, .T. ) ;
#154042 = CARTESIAN_POINT ( 'NONE',  ( 18.39999999999999503, 23.82801463864234037, -229.3483719500187306 ) ) ;
#154043 = CYLINDRICAL_SURFACE ( 'NONE', #18462, 0.09999999999999939493 ) ;
#154044 = DIRECTION ( 'NONE',  ( 0.000000000000000000, 0.1350103645451974088, -0.9908441862701587999 ) ) ;
#154045 = CIRCLE ( 'NONE', #4146, 0.1000000000000000472 ) ;
#154046 = TOROIDAL_SURFACE ( 'NONE', #141507, 0.2000000000000000111, 0.1000000000000000056 ) ;
#154047 = FACE_OUTER_BOUND ( 'NONE', #66846, .T. ) ;
#154048 = DIRECTION ( 'NONE',  ( 1.000000000000000000, -7.304098846218134667E-16, -4.639676173203993355E-30 ) ) ;
#154050 = ADVANCED_FACE ( 'NONE', ( #15483 ), #200514, .F. ) ;
#154049 = CARTESIAN_POINT ( 'NONE',  ( -21.05000000000000071, 11.65000000001115588, -160.4851942293460638 ) ) ;
#154051 = ORIENTED_EDGE ( 'NONE', *, *, #91639, .F. ) ;
#154054 = CARTESIAN_POINT ( 'NONE',  ( 23.24999999999999645, 3.900000000011155432, -200.9999999999999432 ) ) ;
#154053 = CARTESIAN_POINT ( 'NONE',  ( -20.65000000000000568, 5.650000000011139001, -121.3500000000000369 ) ) ;
#154052 = CIRCLE ( 'NONE', #199818, 1.749999999999999778 ) ;
#154055 = VERTEX_POINT ( 'NONE', #44005 ) ;
#154058 = VERTEX_POINT ( 'NONE', #183524 ) ;
#154057 = DIRECTION ( 'NONE',  ( 0.000000000000000000, -0.9770955615653313941, -0.2128009952263603677 ) ) ;
#154056 = DIRECTION ( 'NONE',  ( 1.000000000000000000, 0.000000000000000000, -0.000000000000000000 ) ) ;
#154059 = ORIENTED_EDGE ( 'NONE', *, *, #178934, .T. ) ;
#154060 = CARTESIAN_POINT ( 'NONE',  ( 23.14999999999999503, 64.35000000001254250, -182.1731074845244507 ) ) ;
#154061 = CARTESIAN_POINT ( 'NONE',  ( -21.09610168723072832, 6.378955715224779333, 0.03358950689149174662 ) ) ;
#154062 = DIRECTION ( 'NONE',  ( 1.000000000000000000, 3.265361837132813093E-16, -0.000000000000000000 ) ) ;
#154063 = DIRECTION ( 'NONE',  ( 0.000000000000000000, -1.000000000000000000, 0.000000000000000000 ) ) ;
#154064 = ORIENTED_EDGE ( 'NONE', *, *, #136452, .T. ) ;
#154066 = ORIENTED_EDGE ( 'NONE', *, *, #180666, .T. ) ;
#154065 = DIRECTION ( 'NONE',  ( 0.000000000000000000, 0.000000000000000000, 1.000000000000000000 ) ) ;
#154068 = PLANE ( 'NONE',  #188309 ) ;
#154067 = CARTESIAN_POINT ( 'NONE',  ( 18.39999999999999858, 85.60000000001240039, -163.4229180933022576 ) ) ;
#154070 = ORIENTED_EDGE ( 'NONE', *, *, #244905, .F. ) ;
#154069 = CARTESIAN_POINT ( 'NONE',  ( -21.14999999999994174, 85.92654454508293327, -48.30233646433089234 ) ) ;
#154071 = AXIS2_PLACEMENT_3D ( 'NONE', #201749, #206893, #145616 ) ;
#154072 = AXIS2_PLACEMENT_3D ( 'NONE', #257208, #156910, #197285 ) ;
#154073 = VERTEX_POINT ( 'NONE', #102665 ) ;
#154074 = CARTESIAN_POINT ( 'NONE',  ( 20.95568717954149562, 11.97698268079552797, -206.1722622973479702 ) ) ;
#154075 = CARTESIAN_POINT ( 'NONE',  ( 20.95512820512820085, 67.12384868372377866, -94.46447848938342418 ) ) ;
#154076 = ORIENTED_EDGE ( 'NONE', *, *, #218792, .F. ) ;
#154077 = DIRECTION ( 'NONE',  ( 1.000000000000000000, 0.000000000000000000, 0.000000000000000000 ) ) ;
#154078 = ORIENTED_EDGE ( 'NONE', *, *, #55122, .F. ) ;
#154079 = CARTESIAN_POINT ( 'NONE',  ( -18.42637059832563651, -9.496945461878544492, -107.1090773097998721 ) ) ;
#154080 = DIRECTION ( 'NONE',  ( 0.000000000000000000, -1.000000000000000000, -1.897661533703519897E-16 ) ) ;
#154081 = ORIENTED_EDGE ( 'NONE', *, *, #184782, .T. ) ;
#154082 = CARTESIAN_POINT ( 'NONE',  ( 20.94999999999999574, 87.48912529308817909, -133.4231074845242233 ) ) ;
#154083 = EDGE_CURVE ( 'NONE', #232002, #149532, #162680, .T. ) ;
#154084 = AXIS2_PLACEMENT_3D ( 'NONE', #39503, #60298, #135976 ) ;
#154085 = CIRCLE ( 'NONE', #174942, 11.64999999999998614 ) ;
#154086 = AXIS2_PLACEMENT_3D ( 'NONE', #12208, #170022, #33080 ) ;
#154087 = AXIS2_PLACEMENT_3D ( 'NONE', #111839, #87115, #131385 ) ;
#154088 = CARTESIAN_POINT ( 'NONE',  ( 18.59999999999999787, 77.83534155023670564, -158.4679561919613491 ) ) ;
#154089 = ORIENTED_EDGE ( 'NONE', *, *, #84168, .T. ) ;
#154090 = AXIS2_PLACEMENT_3D ( 'NONE', #55714, #114452, #15371 ) ;
#154091 = ORIENTED_EDGE ( 'NONE', *, *, #121225, .T. ) ;
#154092 = DIRECTION ( 'NONE',  ( 1.000000000000000000, 0.000000000000000000, 0.000000000000000000 ) ) ;
#154093 = ORIENTED_EDGE ( 'NONE', *, *, #165763, .F. ) ;
#154094 = EDGE_CURVE ( 'NONE', #34485, #204479, #250688, .T. ) ;
#154095 = ORIENTED_EDGE ( 'NONE', *, *, #252443, .F. ) ;
#154097 = ORIENTED_EDGE ( 'NONE', *, *, #134512, .T. ) ;
#154096 = DIRECTION ( 'NONE',  ( -1.000000000000000000, 2.952720810173289112E-16, 2.061873921506763405E-30 ) ) ;
#154098 = APPLICATION_CONTEXT ( 'automotive_design' ) ;
#154099 = EDGE_CURVE ( 'NONE', #84465, #19709, #46480, .T. ) ;
#154100 = ORIENTED_EDGE ( 'NONE', *, *, #168038, .T. ) ;
#154101 = DIRECTION ( 'NONE',  ( -1.000000000000000000, 0.000000000000000000, -0.000000000000000000 ) ) ;
#154102 = AXIS2_PLACEMENT_3D ( 'NONE', #145524, #45149, #146798 ) ;
#154103 = ORIENTED_EDGE ( 'NONE', *, *, #106269, .T. ) ;
#154106 = EDGE_LOOP ( 'NONE', ( #139822, #238227, #204812, #241670 ) ) ;
#154105 = VERTEX_POINT ( 'NONE', #204350 ) ;
#154104 = DIRECTION ( 'NONE',  ( -1.000000000000000000, -2.952720810173289112E-16, 0.000000000000000000 ) ) ;
#154107 = AXIS2_PLACEMENT_3D ( 'NONE', #139551, #60015, #102994 ) ;
#154109 = ADVANCED_FACE ( 'NONE', ( #163963 ), #146936, .F. ) ;
#154108 = ORIENTED_EDGE ( 'NONE', *, *, #53445, .F. ) ;
#154110 = AXIS2_PLACEMENT_3D ( 'NONE', #43847, #4691, #50238 ) ;
#154111 = ADVANCED_BREP_SHAPE_REPRESENTATION ( '', ( #196328, #2425 ), #81157 ) ;
#154112 = B_SPLINE_CURVE_WITH_KNOTS ( 'NONE', 3,
 ( #117827, #231376, #202505, #64281, #142514, #219488, #141250, #222036, #434, #23900 ),
 .UNSPECIFIED., .F., .F.,
 ( 4, 2, 2, 2, 4 ),
 ( 0.000000000000000000, 0.0003916577441626962618, 0.0005874866162440451787, 0.0006854010522846982513, 0.0007833154883253513239 ),
 .UNSPECIFIED. ) ;
#154113 = DIRECTION ( 'NONE',  ( 1.000000000000000000, 7.136802563874199107E-16, 1.554319503706929991E-16 ) ) ;
#154114 = ORIENTED_EDGE ( 'NONE', *, *, #251411, .F. ) ;
#154115 = CARTESIAN_POINT ( 'NONE',  ( 21.05000000000000071, 76.00000000001267608, -203.5231074845243597 ) ) ;
#154117 = ORIENTED_EDGE ( 'NONE', *, *, #205397, .T. ) ;
#154116 = DIRECTION ( 'NONE',  ( 0.000000000000000000, 0.000000000000000000, 1.000000000000000000 ) ) ;
#154118 = DIRECTION ( 'NONE',  ( 0.000000000000000000, 0.8660254037844377084, 0.5000000000000015543 ) ) ;
#154119 = ORIENTED_EDGE ( 'NONE', *, *, #50288, .F. ) ;
#154120 = EDGE_CURVE ( 'NONE', #164364, #236786, #150737, .T. ) ;
#154121 = VERTEX_POINT ( 'NONE', #101356 ) ;
#154122 = DIRECTION ( 'NONE',  ( 0.000000000000000000, 0.3634403228828347321, -0.9316174814283063599 ) ) ;
#154123 = DIRECTION ( 'NONE',  ( 0.000000000000000000, 0.2128009952263403282, -0.9770955615653358350 ) ) ;
#154124 = ADVANCED_FACE ( 'NONE', ( #203073 ), #142353, .F. ) ;
#154125 = ORIENTED_EDGE ( 'NONE', *, *, #193634, .T. ) ;
#154126 = ORIENTED_EDGE ( 'NONE', *, *, #231421, .F. ) ;
#154127 = DIRECTION ( 'NONE',  ( 0.000000000000000000, 0.000000000000000000, -1.000000000000000000 ) ) ;
#154129 = VERTEX_POINT ( 'NONE', #23187 ) ;
#154128 = ORIENTED_EDGE ( 'NONE', *, *, #196554, .F. ) ;
#154130 = VERTEX_POINT ( 'NONE', #141813 ) ;
#154131 = CARTESIAN_POINT ( 'NONE',  ( -21.05000000000000071, 0.09779029131994770863, -27.24218538952388613 ) ) ;
#154132 = ORIENTED_EDGE ( 'NONE', *, *, #62343, .F. ) ;
#154133 = ORIENTED_EDGE ( 'NONE', *, *, #107424, .T. ) ;
#154134 = LINE ( 'NONE', #96644, #130025 ) ;
#154135 = AXIS2_PLACEMENT_3D ( 'NONE', #235934, #95149, #217637 ) ;
#154136 = ORIENTED_EDGE ( 'NONE', *, *, #142255, .F. ) ;
#154137 = CARTESIAN_POINT ( 'NONE',  ( -16.93255653858138388, 12.44682876851034870, -211.1657874719333563 ) ) ;
#154138 = CARTESIAN_POINT ( 'NONE',  ( -23.25000000000000000, 84.59626168225506149, -127.0729799673739677 ) ) ;
#154139 = EDGE_CURVE ( 'NONE', #52403, #22426, #50752, .T. ) ;
#154140 = ORIENTED_EDGE ( 'NONE', *, *, #13479, .T. ) ;
#154141 = EDGE_LOOP ( 'NONE', ( #48215, #178004, #66467, #237490 ) ) ;
#154142 = CARTESIAN_POINT ( 'NONE',  ( 18.79999999999999716, 1.410778198689825125, -7.973296578895943121 ) ) ;
#154144 = ORIENTED_EDGE ( 'NONE', *, *, #202456, .T. ) ;
#154143 = AXIS2_PLACEMENT_3D ( 'NONE', #101615, #2541, #82059 ) ;
#154145 = VECTOR ( 'NONE', #100055, 1000.000000000000000 ) ;
#154146 = ADVANCED_FACE ( 'NONE', ( #126092 ), #81808, .F. ) ;
#154147 = CARTESIAN_POINT ( 'NONE',  ( -18.41353343127311248, 85.50000000001190870, -95.99103808782456326 ) ) ;
#154148 = VERTEX_POINT ( 'NONE', #205630 ) ;
#154149 = ORIENTED_EDGE ( 'NONE', *, *, #214054, .T. ) ;
#154150 = AXIS2_PLACEMENT_3D ( 'NONE', #227308, #66954, #90360 ) ;
#154151 = DIRECTION ( 'NONE',  ( 0.000000000000000000, -0.2617529984165152257, -0.9651348961777124202 ) ) ;
#154153 = ORIENTED_EDGE ( 'NONE', *, *, #75895, .T. ) ;
#154152 = CARTESIAN_POINT ( 'NONE',  ( 18.43473516226089259, 85.49494228277045238, -162.9772088011748110 ) ) ;
#154154 = DIRECTION ( 'NONE',  ( 0.000000000000000000, -0.8814952561688430555, 0.4721928772777346239 ) ) ;
#154155 = CARTESIAN_POINT ( 'NONE',  ( -16.91256925476569251, 30.32690185447398790, -234.8310981037861609 ) ) ;
#154156 = AXIS2_PLACEMENT_3D ( 'NONE', #179230, #230529, #12779 ) ;
#154157 = DIRECTION ( 'NONE',  ( 0.000000000000000000, 0.000000000000000000, 1.000000000000000000 ) ) ;
#154159 = EDGE_CURVE ( 'NONE', #157238, #189017, #63557, .T. ) ;
#154158 = SPHERICAL_SURFACE ( 'NONE', #28830, 0.1000000000000000056 ) ;
#154160 = CARTESIAN_POINT ( 'NONE',  ( 18.59999999999999432, -3.616484641954614165, -226.0163245033746477 ) ) ;
#154161 = CYLINDRICAL_SURFACE ( 'NONE', #15008, 0.09999999999999939493 ) ;
#154162 = CARTESIAN_POINT ( 'NONE',  ( -21.05000000000000071, 44.55458850188623643, -247.3966190010231969 ) ) ;
#154163 = CARTESIAN_POINT ( 'NONE',  ( 22.37643362114956247, 10.64233729798123029, -226.9638180893018955 ) ) ;
#154164 = CARTESIAN_POINT ( 'NONE',  ( -21.17356465864818560, 69.57719687376993534, -69.62201872553823989 ) ) ;
#154165 = CARTESIAN_POINT ( 'NONE',  ( -21.64999999999999858, 10.05000000001113847, -46.25000000000000711 ) ) ;
#154166 = DIRECTION ( 'NONE',  ( 0.000000000000000000, 0.000000000000000000, -1.000000000000000000 ) ) ;
#154167 = ADVANCED_FACE ( 'NONE', ( #223907 ), #240932, .T. ) ;
#154168 = EDGE_LOOP ( 'NONE', ( #138344, #35258, #67412, #78431 ) ) ;
#154169 = EDGE_CURVE ( 'NONE', #238440, #113568, #25851, .T. ) ;
#154170 = AXIS2_PLACEMENT_3D ( 'NONE', #250711, #189471, #249452 ) ;
#154171 = CIRCLE ( 'NONE', #95835, 0.09999999999999939493 ) ;
#154172 = AXIS2_PLACEMENT_3D ( 'NONE', #162180, #241693, #63043 ) ;
#154173 = AXIS2_PLACEMENT_3D ( 'NONE', #257056, #141027, #57607 ) ;
#154175 = ORIENTED_EDGE ( 'NONE', *, *, #113249, .F. ) ;
#154174 = ORIENTED_EDGE ( 'NONE', *, *, #163258, .T. ) ;
#154176 = ORIENTED_EDGE ( 'NONE', *, *, #240821, .T. ) ;
#154177 = AXIS2_PLACEMENT_3D ( 'NONE', #166043, #100854, #120500 ) ;
#154178 = CARTESIAN_POINT ( 'NONE',  ( -21.08198257630413508, 0.07264332379574613141, -94.16340326598496802 ) ) ;
#154179 = EDGE_CURVE ( 'NONE', #37930, #73948, #13201, .T. ) ;
#154180 = DIRECTION ( 'NONE',  ( 0.000000000000000000, 0.9651348961777379554, -0.2617529984164210233 ) ) ;
#154182 = LINE ( 'NONE', #233682, #57092 ) ;
#154181 = DIRECTION ( 'NONE',  ( 1.000000000000000000, 0.000000000000000000, 0.000000000000000000 ) ) ;
#154183 = VERTEX_POINT ( 'NONE', #105212 ) ;
#154184 = ORIENTED_EDGE ( 'NONE', *, *, #214867, .T. ) ;
#154185 = EDGE_CURVE ( 'NONE', #125531, #8374, #113144, .T. ) ;
#154186 = FILL_AREA_STYLE_COLOUR ( '', #152111 ) ;
#154187 = EDGE_CURVE ( 'NONE', #72316, #28626, #158962, .T. ) ;
#154188 = DIRECTION ( 'NONE',  ( 0.000000000000000000, 0.000000000000000000, -1.000000000000000000 ) ) ;
#154189 = DIRECTION ( 'NONE',  ( 0.000000000000000000, 0.000000000000000000, 1.000000000000000000 ) ) ;
#154190 = LINE ( 'NONE', #255766, #216436 ) ;
#154191 = EDGE_LOOP ( 'NONE', ( #101846, #40863, #187023, #111901 ) ) ;
#154192 = ORIENTED_EDGE ( 'NONE', *, *, #14460, .F. ) ;
#154193 = DIRECTION ( 'NONE',  ( -0.000000000000000000, -0.000000000000000000, 1.000000000000000000 ) ) ;
#154194 = EDGE_CURVE ( 'NONE', #31293, #68386, #200631, .T. ) ;
#154195 = VERTEX_POINT ( 'NONE', #110391 ) ;
#154196 = CARTESIAN_POINT ( 'NONE',  ( 20.85000000000000142, 36.46860332481993794, -249.8166405164294588 ) ) ;
#154198 = EDGE_LOOP ( 'NONE', ( #246654, #153741, #192958, #128001, #94915, #51355, #78402, #239269, #88057, #140243, #236873, #43661 ) ) ;
#154197 = DIRECTION ( 'NONE',  ( 1.000000000000000000, -0.000000000000000000, -0.000000000000000000 ) ) ;
#154199 = DIRECTION ( 'NONE',  ( -1.000000000000000000, 0.000000000000000000, -0.000000000000000000 ) ) ;
#154200 = EDGE_CURVE ( 'NONE', #198561, #95552, #138247, .T. ) ;
#154201 = CARTESIAN_POINT ( 'NONE',  ( 0.9000000000000535350, 67.75000000001118394, -14.06452884076210630 ) ) ;
#154202 = EDGE_CURVE ( 'NONE', #207317, #148869, #17456, .T. ) ;
#154203 = B_SPLINE_CURVE_WITH_KNOTS ( 'NONE', 3,
 ( #14484, #215223, #116137, #93979, #90119, #169722, #70611 ),
 .UNSPECIFIED., .F., .F.,
 ( 4, 3, 4 ),
 ( 0.000000000000000000, 3.882884552234470657E-05, 5.798605692158509758E-05 ),
 .UNSPECIFIED. ) ;
#154204 = LINE ( 'NONE', #35529, #29362 ) ;
#154205 = ORIENTED_EDGE ( 'NONE', *, *, #140202, .F. ) ;
#154206 = CYLINDRICAL_SURFACE ( 'NONE', #73759, 0.09999999999999939493 ) ;
#154207 = CARTESIAN_POINT ( 'NONE',  ( -18.40000000000000213, 11.47316190337362762, -180.0499999999999545 ) ) ;
#154208 = TOROIDAL_SURFACE ( 'NONE', #58448, 12.77499999999999858, 0.1000000000000000056 ) ;
#154209 = FACE_OUTER_BOUND ( 'NONE', #46300, .T. ) ;
#154211 = DIRECTION ( 'NONE',  ( 0.000000000000000000, 0.000000000000000000, -1.000000000000000000 ) ) ;
#154210 = DIRECTION ( 'NONE',  ( -0.000000000000000000, -6.982962677686266711E-15, 1.000000000000000000 ) ) ;
#154212 = CARTESIAN_POINT ( 'NONE',  ( -20.64999999999999858, 71.65000000001180069, -81.87310748452433984 ) ) ;
#154213 = VECTOR ( 'NONE', #209872, 1000.000000000000000 ) ;
#154214 = DIRECTION ( 'NONE',  ( -0.000000000000000000, 6.982962677686266711E-15, -1.000000000000000000 ) ) ;
#154215 = CARTESIAN_POINT ( 'NONE',  ( -22.48660254037843487, 11.65000000000000036, 0.04999999999998061551 ) ) ;
#154216 = CARTESIAN_POINT ( 'NONE',  ( -23.15000000000000213, -9.499999999988848032, -43.39396912265245021 ) ) ;
#154218 = ORIENTED_EDGE ( 'NONE', *, *, #149206, .F. ) ;
#154217 = VECTOR ( 'NONE', #147960, 1000.000000000000000 ) ;
#154219 = EDGE_LOOP ( 'NONE', ( #235564, #256617, #86557, #72582 ) ) ;
#154220 = DIRECTION ( 'NONE',  ( 0.9880948137434723000, 0.1538461538461484146, -0.000000000000000000 ) ) ;
#154221 = ADVANCED_FACE ( 'NONE', ( #231646 ), #44824, .F. ) ;
#154222 = ORIENTED_EDGE ( 'NONE', *, *, #111554, .T. ) ;
#154223 = ADVANCED_FACE ( 'NONE', ( #206934 ), #251168, .T. ) ;
#154224 = DIRECTION ( 'NONE',  ( 0.000000000000000000, 0.8636236514130390951, -0.5041370733441546959 ) ) ;
#154225 = AXIS2_PLACEMENT_3D ( 'NONE', #107418, #85252, #70896 ) ;
#154226 = VERTEX_POINT ( 'NONE', #109100 ) ;
#154227 = TOROIDAL_SURFACE ( 'NONE', #25199, 0.2000000000000000111, 0.1000000000000000056 ) ;
#154228 = EDGE_CURVE ( 'NONE', #179110, #185777, #184051, .T. ) ;
#154229 = ORIENTED_EDGE ( 'NONE', *, *, #67990, .F. ) ;
#154230 = CARTESIAN_POINT ( 'NONE',  ( -21.45000000000000284, 7.708578643773852157, -121.6500000000000341 ) ) ;
#154231 = TOROIDAL_SURFACE ( 'NONE', #66707, 0.2000000000000000111, 0.1000000000000000056 ) ;
#154232 = ORIENTED_EDGE ( 'NONE', *, *, #237753, .T. ) ;
#154233 = VECTOR ( 'NONE', #136714, 1000.000000000000000 ) ;
#154234 = CARTESIAN_POINT ( 'NONE',  ( 20.12500000000000355, 66.74195072709531473, -195.1597686473820090 ) ) ;
#154235 = CARTESIAN_POINT ( 'NONE',  ( -12.30589683808040391, 9.356746017089404788, -50.70335972136417979 ) ) ;
#154236 = LINE ( 'NONE', #94199, #198544 ) ;
#154237 = CARTESIAN_POINT ( 'NONE',  ( 21.05000000000000071, 1.162701749949165642, -74.90000000000004832 ) ) ;
#154238 = CARTESIAN_POINT ( 'NONE',  ( 21.14999999999999858, 76.10000000001241460, -176.5637644362255969 ) ) ;
#154240 = EDGE_LOOP ( 'NONE', ( #58500, #187522, #2447, #101430 ) ) ;
#154239 = DIRECTION ( 'NONE',  ( 1.000000000000000000, 0.000000000000000000, 0.000000000000000000 ) ) ;
#154242 = FACE_OUTER_BOUND ( 'NONE', #219523, .T. ) ;
#154241 = CARTESIAN_POINT ( 'NONE',  ( 21.05000000000000071, 6.412126976762839270, -199.7058512474018244 ) ) ;
#154243 = CARTESIAN_POINT ( 'NONE',  ( -16.86578989773640913, 9.984809801269951990, -154.9646648866222449 ) ) ;
#154244 = CARTESIAN_POINT ( 'NONE',  ( 22.39999999999999503, 64.35000000001213039, -136.6231074845243825 ) ) ;
#154245 = DIRECTION ( 'NONE',  ( 0.000000000000000000, 0.000000000000000000, 1.000000000000000000 ) ) ;
#154246 = CARTESIAN_POINT ( 'NONE',  ( 20.94999999999999574, 76.00000000001213607, -136.5231074845242745 ) ) ;
#154247 = ORIENTED_EDGE ( 'NONE', *, *, #157854, .T. ) ;
#154248 = EDGE_CURVE ( 'NONE', #19770, #139998, #34076, .T. ) ;
#154249 = DIRECTION ( 'NONE',  ( 1.000000000000000000, 0.000000000000000000, 0.000000000000000000 ) ) ;
#154250 = VECTOR ( 'NONE', #200298, 1000.000000000000000 ) ;
#154251 = VERTEX_POINT ( 'NONE', #10015 ) ;
#154252 = EDGE_CURVE ( 'NONE', #186873, #144175, #217353, .T. ) ;
#154253 = CARTESIAN_POINT ( 'NONE',  ( 18.39999999999999858, 85.50000000001161027, -62.49103808782458458 ) ) ;
#154254 = ORIENTED_EDGE ( 'NONE', *, *, #178070, .T. ) ;
#154255 = CARTESIAN_POINT ( 'NONE',  ( 18.59999999999999432, 1.162701749949165642, -41.60000000000000142 ) ) ;
#154256 = DIRECTION ( 'NONE',  ( 1.000000000000000000, -2.952720810173289112E-16, -2.061873921506763405E-30 ) ) ;
#154257 = EDGE_CURVE ( 'NONE', #243362, #213681, #252457, .T. ) ;
#154258 = LINE ( 'NONE', #195924, #16072 ) ;
#154259 = ORIENTED_EDGE ( 'NONE', *, *, #107824, .F. ) ;
#154260 = ORIENTED_EDGE ( 'NONE', *, *, #151485, .T. ) ;
#154261 = ADVANCED_FACE ( 'NONE', ( #129939 ), #61578, .T. ) ;
#154262 = DIRECTION ( 'NONE',  ( 1.000000000000000000, 0.000000000000000000, 0.000000000000000000 ) ) ;
#154263 = DIRECTION ( 'NONE',  ( 0.000000000000000000, -1.000000000000000000, 0.000000000000000000 ) ) ;
#154264 = AXIS2_PLACEMENT_3D ( 'NONE', #216504, #194407, #155288 ) ;
#154265 = FACE_OUTER_BOUND ( 'NONE', #225968, .T. ) ;
#154267 = CARTESIAN_POINT ( 'NONE',  ( 18.50000000000000000, -9.499999999999998224, -7.032069396699667685 ) ) ;
#154266 = AXIS2_PLACEMENT_3D ( 'NONE', #200988, #130430, #228265 ) ;
#154268 = ADVANCED_FACE ( 'NONE', ( #133803 ), #246419, .T. ) ;
#154269 = VECTOR ( 'NONE', #200306, 1000.000000000000000 ) ;
#154272 = CARTESIAN_POINT ( 'NONE',  ( -23.15000000000000213, 5.900000000011162093, -190.7809002353436085 ) ) ;
#154271 = AXIS2_PLACEMENT_3D ( 'NONE', #198750, #39714, #219590 ) ;
#154270 = CARTESIAN_POINT ( 'NONE',  ( -23.15000000000000213, 85.00000000001197975, -112.4170766071766678 ) ) ;
#154273 = FACE_OUTER_BOUND ( 'NONE', #72934, .T. ) ;
#154274 = CARTESIAN_POINT ( 'NONE',  ( 12.33938619321247820, 9.360723793997193454, -50.81392719460670548 ) ) ;
#154275 = FACE_OUTER_BOUND ( 'NONE', #149945, .T. ) ;
#154276 = ORIENTED_EDGE ( 'NONE', *, *, #205141, .T. ) ;
#154277 = CARTESIAN_POINT ( 'NONE',  ( 23.14999999999999858, 1.115600667400684642E-11, -104.5000000000000568 ) ) ;
#154278 = EDGE_CURVE ( 'NONE', #257618, #63374, #163222, .T. ) ;
#154279 = VERTEX_POINT ( 'NONE', #118098 ) ;
#154280 = AXIS2_PLACEMENT_3D ( 'NONE', #152989, #91692, #211659 ) ;
#154281 = CARTESIAN_POINT ( 'NONE',  ( 22.59066674512251183, 11.75000000000000000, 0.03050412363060323040 ) ) ;
#154283 = EDGE_CURVE ( 'NONE', #10718, #100827, #196362, .T. ) ;
#154282 = EDGE_CURVE ( 'NONE', #254425, #92348, #104900, .T. ) ;
#154284 = CARTESIAN_POINT ( 'NONE',  ( 23.15000000000000213, -11.74999999998883560, -130.9000000000000341 ) ) ;
#154286 = CARTESIAN_POINT ( 'NONE',  ( -23.39999999999994529, 83.90000000001120384, -34.86056257560453986 ) ) ;
#154285 = DIRECTION ( 'NONE',  ( 0.000000000000000000, -0.4088369013363281068, 0.9126074666063770380 ) ) ;
#154288 = VERTEX_POINT ( 'NONE', #115522 ) ;
#154287 = CARTESIAN_POINT ( 'NONE',  ( 23.24999999999999289, -0.1830918614494220220, -222.4987906021368360 ) ) ;
#154289 = CARTESIAN_POINT ( 'NONE',  ( -20.94999999999999929, 77.83534155023598089, -57.96795619196132776 ) ) ;
#154290 = CARTESIAN_POINT ( 'NONE',  ( -16.94226253665224746, 51.34806072463185700, -232.0677850682404255 ) ) ;
#154291 = CARTESIAN_POINT ( 'NONE',  ( -23.25000000000000000, -1.835859311432481045, -78.50443916879852679 ) ) ;
#154292 = CYLINDRICAL_SURFACE ( 'NONE', #70184, 0.1000000000000028644 ) ;
#154293 = LINE ( 'NONE', #215493, #211685 ) ;
#154294 = ORIENTED_EDGE ( 'NONE', *, *, #59065, .T. ) ;
#154295 = CARTESIAN_POINT ( 'NONE',  ( -18.59999999999999787, 7.675662554762638479, -241.7139905447625381 ) ) ;
#154297 = ORIENTED_EDGE ( 'NONE', *, *, #163530, .F. ) ;
#154296 = AXIS2_PLACEMENT_3D ( 'NONE', #27573, #70543, #107055 ) ;
#154298 = CIRCLE ( 'NONE', #137466, 0.5000000000000004441 ) ;
#154299 = CARTESIAN_POINT ( 'NONE',  ( -20.94999999999999929, 1.360870587192041681, -8.072997927090961312 ) ) ;
#154300 = ORIENTED_EDGE ( 'NONE', *, *, #28789, .T. ) ;
#154301 = CARTESIAN_POINT ( 'NONE',  ( -20.94403535211772294, 46.37740828070795374, -243.0652246697500800 ) ) ;
#154302 = ADVANCED_FACE ( 'NONE', ( #137640 ), #256251, .F. ) ;
#154303 = ADVANCED_FACE ( 'NONE', ( #174274 ), #236746, .T. ) ;
#154304 = VERTEX_POINT ( 'NONE', #215890 ) ;
#154305 = DIRECTION ( 'NONE',  ( 1.000000000000000000, 0.000000000000000000, 0.000000000000000000 ) ) ;
#154306 = CARTESIAN_POINT ( 'NONE',  ( -20.65000000000000568, 7.250000000011138646, -121.3500000000000369 ) ) ;
#154307 = EDGE_CURVE ( 'NONE', #209179, #182327, #254973, .T. ) ;
#154308 = DIRECTION ( 'NONE',  ( 0.000000000000000000, -1.000000000000000000, 0.000000000000000000 ) ) ;
#154309 = VERTEX_POINT ( 'NONE', #37300 ) ;
#154310 = EDGE_CURVE ( 'NONE', #162722, #27378, #18987, .T. ) ;
#154311 = CARTESIAN_POINT ( 'NONE',  ( -16.89935556175729658, 9.949999999999981526, -13.13967636288533036 ) ) ;
#154312 = EDGE_CURVE ( 'NONE', #135166, #241512, #209003, .T. ) ;
#154313 = LINE ( 'NONE', #57710, #211670 ) ;
#154314 = DIRECTION ( 'NONE',  ( -1.000000000000000000, -0.000000000000000000, -0.000000000000000000 ) ) ;
#154315 = CARTESIAN_POINT ( 'NONE',  ( 18.59999999999999076, 69.35000000001222986, -148.7731074845244166 ) ) ;
#154317 = DIRECTION ( 'NONE',  ( -1.000000000000000000, 0.000000000000000000, 0.000000000000000000 ) ) ;
#154316 = AXIS2_PLACEMENT_3D ( 'NONE', #84006, #243132, #64505 ) ;
#154318 = ORIENTED_EDGE ( 'NONE', *, *, #137613, .T. ) ;
#154319 = DIRECTION ( 'NONE',  ( -1.000000000000000000, 0.000000000000000000, 0.000000000000000000 ) ) ;
#154320 = EDGE_LOOP ( 'NONE', ( #136658, #218269, #110761, #164671 ) ) ;
#154322 = EDGE_LOOP ( 'NONE', ( #245179, #154144, #759, #191499 ) ) ;
#154321 = FACE_OUTER_BOUND ( 'NONE', #134298, .T. ) ;
#154323 = ORIENTED_EDGE ( 'NONE', *, *, #32733, .T. ) ;
#154324 = CARTESIAN_POINT ( 'NONE',  ( 23.14999999999999858, 1.115600667400684642E-11, -67.00000000000000000 ) ) ;
#154325 = LINE ( 'NONE', #69616, #96620 ) ;
#154326 = DIRECTION ( 'NONE',  ( -1.000000000000000000, 0.000000000000000000, 0.000000000000000000 ) ) ;
#154327 = LINE ( 'NONE', #233822, #195756 ) ;
#154328 = CIRCLE ( 'NONE', #132, 0.1999999999999987899 ) ;
#154329 = ORIENTED_EDGE ( 'NONE', *, *, #21758, .T. ) ;
#154330 = EDGE_CURVE ( 'NONE', #88245, #75640, #242310, .T. ) ;
#154331 = CARTESIAN_POINT ( 'NONE',  ( -17.11825945287481332, 9.949999999999983302, -20.75000000000000000 ) ) ;
#154332 = DIRECTION ( 'NONE',  ( 1.000000000000000000, 0.000000000000000000, 0.000000000000000000 ) ) ;
#154333 = ORIENTED_EDGE ( 'NONE', *, *, #178167, .F. ) ;
#154335 = ORIENTED_EDGE ( 'NONE', *, *, #119416, .F. ) ;
#154334 = DIRECTION ( 'NONE',  ( 0.000000000000000000, -0.9126074666063769270, -0.4088369013363280513 ) ) ;
#154336 = CARTESIAN_POINT ( 'NONE',  ( 11.60000000000000320, -12.24999999999999822, 15.00000000000000355 ) ) ;
#154337 = CARTESIAN_POINT ( 'NONE',  ( -20.85000000000000142, 10.33248238083635151, -106.0948465439132065 ) ) ;
#154338 = EDGE_CURVE ( 'NONE', #219800, #137417, #84040, .T. ) ;
#154339 = FACE_OUTER_BOUND ( 'NONE', #47944, .T. ) ;
#154340 = CIRCLE ( 'NONE', #54308, 0.09999999999999520384 ) ;
#154341 = ORIENTED_EDGE ( 'NONE', *, *, #22995, .F. ) ;
#154342 = AXIS2_PLACEMENT_3D ( 'NONE', #83047, #62246, #221294 ) ;
#154343 = ORIENTED_EDGE ( 'NONE', *, *, #171769, .F. ) ;
#154344 = CARTESIAN_POINT ( 'NONE',  ( -18.59999999999999787, 43.48442877397276618, -245.2193771921251084 ) ) ;
#154345 = ORIENTED_EDGE ( 'NONE', *, *, #121745, .F. ) ;
#154346 = LINE ( 'NONE', #33113, #146082 ) ;
#154347 = TOROIDAL_SURFACE ( 'NONE', #166801, 0.2000000000000000111, 0.1000000000000000056 ) ;
#154348 = EDGE_CURVE ( 'NONE', #119515, #69522, #130057, .T. ) ;
#154349 = CYLINDRICAL_SURFACE ( 'NONE', #101422, 0.1000000000000028644 ) ;
#154350 = AXIS2_PLACEMENT_3D ( 'NONE', #31722, #190795, #91660 ) ;
#154351 = CIRCLE ( 'NONE', #41897, 12.87500000000000000 ) ;
#154352 = FACE_OUTER_BOUND ( 'NONE', #17644, .T. ) ;
#154353 = AXIS2_PLACEMENT_3D ( 'NONE', #246250, #204542, #225377 ) ;
#154354 = CIRCLE ( 'NONE', #37622, 0.2000000000000057288 ) ;
#154355 = VERTEX_POINT ( 'NONE', #15159 ) ;
#154357 = DIRECTION ( 'NONE',  ( 1.000000000000000000, 0.000000000000000000, 0.000000000000000000 ) ) ;
#154356 = AXIS2_PLACEMENT_3D ( 'NONE', #179839, #72062, #112472 ) ;
#154358 = AXIS2_PLACEMENT_3D ( 'NONE', #72764, #92280, #91003 ) ;
#154359 = ORIENTED_EDGE ( 'NONE', *, *, #238012, .T. ) ;
#154360 = DIRECTION ( 'NONE',  ( 0.000000000000000000, 0.000000000000000000, 1.000000000000000000 ) ) ;
#154361 = DIRECTION ( 'NONE',  ( 0.7071067811865474617, 0.7071067811865474617, 0.000000000000000000 ) ) ;
#154363 = ORIENTED_EDGE ( 'NONE', *, *, #65366, .F. ) ;
#154362 = CARTESIAN_POINT ( 'NONE',  ( -18.59999999999999787, 11.64494613601372386, -211.0010114233329830 ) ) ;
#154364 = CARTESIAN_POINT ( 'NONE',  ( 20.94999999999999574, 77.25000000001159606, -61.52310748452431710 ) ) ;
#154365 = DIRECTION ( 'NONE',  ( -1.000000000000000000, 0.000000000000000000, -0.000000000000000000 ) ) ;
#154366 = CARTESIAN_POINT ( 'NONE',  ( -23.25000000000000000, 11.65000000001115588, -193.9851942293460070 ) ) ;
#154367 = CARTESIAN_POINT ( 'NONE',  ( 21.05000000000000426, 6.344359042054589892, -33.48514436510635051 ) ) ;
#154368 = DIRECTION ( 'NONE',  ( 2.952720810173289112E-16, 1.000000000000000000, -6.088138035986627436E-46 ) ) ;
#154369 = CYLINDRICAL_SURFACE ( 'NONE', #144747, 0.09999999999998898659 ) ;
#154370 = VECTOR ( 'NONE', #72306, 1000.000000000000000 ) ;
#154372 = ORIENTED_EDGE ( 'NONE', *, *, #169271, .T. ) ;
#154371 = CARTESIAN_POINT ( 'NONE',  ( -23.25000000000000000, 87.75000000001192291, -106.1231074845242262 ) ) ;
#154373 = DIRECTION ( 'NONE',  ( 0.000000000000000000, 0.000000000000000000, 1.000000000000000000 ) ) ;
#154374 = DIRECTION ( 'NONE',  ( 0.000000000000000000, -7.272083257015735086E-15, 1.000000000000000000 ) ) ;
#154375 = CYLINDRICAL_SURFACE ( 'NONE', #64054, 0.09999999999999811817 ) ;
#154376 = ORIENTED_EDGE ( 'NONE', *, *, #117319, .T. ) ;
#154377 = FACE_OUTER_BOUND ( 'NONE', #253167, .T. ) ;
#154378 = CIRCLE ( 'NONE', #133487, 4.299999999999970512 ) ;
#154379 = EDGE_CURVE ( 'NONE', #56792, #239682, #109212, .T. ) ;
#154380 = DIRECTION ( 'NONE',  ( 1.000000000000000000, 0.000000000000000000, 0.000000000000000000 ) ) ;
#154381 = DIRECTION ( 'NONE',  ( -1.000000000000000000, -0.000000000000000000, -0.000000000000000000 ) ) ;
#154382 = VERTEX_POINT ( 'NONE', #33040 ) ;
#154383 = AXIS2_PLACEMENT_3D ( 'NONE', #197347, #16178, #20027 ) ;
#154384 = DIRECTION ( 'NONE',  ( 0.000000000000000000, 0.9770955615653313941, 0.2128009952263606452 ) ) ;
#154385 = CARTESIAN_POINT ( 'NONE',  ( 18.54999999999999716, 8.750000000011182166, -176.7499999999999716 ) ) ;
#154387 = ORIENTED_EDGE ( 'NONE', *, *, #37072, .T. ) ;
#154386 = AXIS2_PLACEMENT_3D ( 'NONE', #187530, #145797, #8871 ) ;
#154388 = CARTESIAN_POINT ( 'NONE',  ( 18.49999999999999645, -1.362429037182155023, -175.3888812479212334 ) ) ;
#154389 = EDGE_LOOP ( 'NONE', ( #76811, #114016, #71748, #163397 ) ) ;
#154390 = EDGE_CURVE ( 'NONE', #137324, #79014, #167512, .T. ) ;
#154392 = EDGE_LOOP ( 'NONE', ( #72599, #38298, #25390, #54121 ) ) ;
#154391 = FACE_OUTER_BOUND ( 'NONE', #173966, .T. ) ;
#154394 = ADVANCED_FACE ( 'NONE', ( #73430 ), #133381, .F. ) ;
#154393 = CARTESIAN_POINT ( 'NONE',  ( 18.79999999999999716, -1.467286812112899463, 33.00000000000000000 ) ) ;
#154395 = ORIENTED_EDGE ( 'NONE', *, *, #146269, .F. ) ;
#154396 = AXIS2_PLACEMENT_3D ( 'NONE', #126838, #111127, #30323 ) ;
#154397 = LINE ( 'NONE', #77367, #72383 ) ;
#154398 = ORIENTED_EDGE ( 'NONE', *, *, #78451, .F. ) ;
#154400 = VERTEX_POINT ( 'NONE', #249482 ) ;
#154399 = ORIENTED_EDGE ( 'NONE', *, *, #124785, .T. ) ;
#154401 = DIRECTION ( 'NONE',  ( 1.000000000000000000, -2.283407518332345398E-16, 1.048447799332034305E-15 ) ) ;
#154403 = ORIENTED_EDGE ( 'NONE', *, *, #214169, .F. ) ;
#154402 = FACE_OUTER_BOUND ( 'NONE', #178104, .T. ) ;
#154404 = CARTESIAN_POINT ( 'NONE',  ( -16.94389599337535657, 14.20826918932317895, -219.2876906590868487 ) ) ;
#154405 = AXIS2_PLACEMENT_3D ( 'NONE', #251653, #117284, #75611 ) ;
#154407 = EDGE_CURVE ( 'NONE', #40931, #113635, #59296, .T. ) ;
#154406 = ORIENTED_EDGE ( 'NONE', *, *, #221160, .F. ) ;
#154408 = VECTOR ( 'NONE', #111761, 1000.000000000000000 ) ;
#154409 = EDGE_CURVE ( 'NONE', #246837, #131784, #150923, .T. ) ;
#154410 = EDGE_CURVE ( 'NONE', #249890, #246507, #230023, .T. ) ;
#154411 = ORIENTED_EDGE ( 'NONE', *, *, #122264, .T. ) ;
#154412 = CARTESIAN_POINT ( 'NONE',  ( -21.44999999999999929, 7.150000000011155876, -121.7500000000000426 ) ) ;
#154413 = CARTESIAN_POINT ( 'NONE',  ( 21.00000000000000000, 9.750000000011153745, -54.65000000000000568 ) ) ;
#154414 = DIRECTION ( 'NONE',  ( -1.000000000000000000, -3.265361837132813093E-16, 0.000000000000000000 ) ) ;
#154415 = ORIENTED_EDGE ( 'NONE', *, *, #164724, .T. ) ;
#154416 = EDGE_CURVE ( 'NONE', #71915, #183810, #38501, .T. ) ;
#154417 = FACE_OUTER_BOUND ( 'NONE', #30809, .T. ) ;
#154418 = CARTESIAN_POINT ( 'NONE',  ( -21.05000000000000071, 74.83729825007408465, -128.4231074845243086 ) ) ;
#154419 = DIRECTION ( 'NONE',  ( 0.000000000000000000, 0.000000000000000000, 1.000000000000000000 ) ) ;
#154420 = ORIENTED_EDGE ( 'NONE', *, *, #43528, .T. ) ;
#154421 = DIRECTION ( 'NONE',  ( 0.000000000000000000, 1.000000000000000000, 1.321694076934707365E-14 ) ) ;
#154422 = CARTESIAN_POINT ( 'NONE',  ( -18.39999999999999858, 37.99112772578904895, -261.0419300540664835 ) ) ;
#154423 = EDGE_CURVE ( 'NONE', #105294, #110925, #117609, .T. ) ;
#154424 = VECTOR ( 'NONE', #64856, 1000.000000000000000 ) ;
#154425 = ORIENTED_EDGE ( 'NONE', *, *, #42073, .T. ) ;
#154426 = DIRECTION ( 'NONE',  ( -1.000000000000000000, -2.885090398161910739E-16, -6.283419270304611573E-17 ) ) ;
#154427 = ORIENTED_EDGE ( 'NONE', *, *, #220343, .F. ) ;
#154428 = VERTEX_POINT ( 'NONE', #74726 ) ;
#154429 = EDGE_CURVE ( 'NONE', #19166, #206017, #253307, .T. ) ;
#154430 = CARTESIAN_POINT ( 'NONE',  ( -12.29659703204451482, 25.90497867185234071, -233.1769111789295437 ) ) ;
#154431 = EDGE_LOOP ( 'NONE', ( #199958, #191688, #216020, #257824 ) ) ;
#154432 = ORIENTED_EDGE ( 'NONE', *, *, #6884, .F. ) ;
#154433 = DIRECTION ( 'NONE',  ( 0.000000000000000000, 0.000000000000000000, -1.000000000000000000 ) ) ;
#154434 = CARTESIAN_POINT ( 'NONE',  ( -16.93262454970419384, 10.00202046794151478, -188.4270762262372898 ) ) ;
#154435 = EDGE_LOOP ( 'NONE', ( #149488, #122616, #189334, #74258, #68691, #22191, #228757 ) ) ;
#154436 = EDGE_CURVE ( 'NONE', #256383, #208604, #9565, .T. ) ;
#154437 = ORIENTED_EDGE ( 'NONE', *, *, #146211, .F. ) ;
#154438 = FACE_OUTER_BOUND ( 'NONE', #253786, .T. ) ;
#154439 = FACE_OUTER_BOUND ( 'NONE', #183963, .T. ) ;
#154440 = EDGE_CURVE ( 'NONE', #238954, #114550, #190813, .T. ) ;
#154441 = ORIENTED_EDGE ( 'NONE', *, *, #2888, .T. ) ;
#154442 = CIRCLE ( 'NONE', #41991, 0.09999999999999939493 ) ;
#154443 = CIRCLE ( 'NONE', #183634, 0.09999999999999939493 ) ;
#154444 = AXIS2_PLACEMENT_3D ( 'NONE', #191443, #179564, #76584 ) ;
#154445 = ORIENTED_EDGE ( 'NONE', *, *, #249011, .F. ) ;
#154446 = TOROIDAL_SURFACE ( 'NONE', #171214, 0.6000000000000009770, 0.1000000000000000056 ) ;
#154447 = CARTESIAN_POINT ( 'NONE',  ( -20.64999999999999858, 44.91518204311810081, -238.0177672736398620 ) ) ;
#154448 = ADVANCED_FACE ( 'NONE', ( #152973 ), #10865, .T. ) ;
#154449 = DIRECTION ( 'NONE',  ( 1.000000000000000000, 0.000000000000000000, 0.000000000000000000 ) ) ;
#154450 = DIRECTION ( 'NONE',  ( 1.000000000000000000, 0.000000000000000000, 0.000000000000000000 ) ) ;
#154451 = DIRECTION ( 'NONE',  ( -1.000000000000000000, -0.000000000000000000, -0.000000000000000000 ) ) ;
#154452 = CARTESIAN_POINT ( 'NONE',  ( -22.10000000000000142, -1.467286812112899463, 32.89999999999999858 ) ) ;
#154453 = AXIS2_PLACEMENT_3D ( 'NONE', #93921, #173520, #114776 ) ;
#154454 = DIRECTION ( 'NONE',  ( 0.000000000000000000, 0.000000000000000000, -1.000000000000000000 ) ) ;
#154455 = CARTESIAN_POINT ( 'NONE',  ( -20.54999999999999716, 85.00000000001261924, -193.6291383618718385 ) ) ;
#154457 = DIRECTION ( 'NONE',  ( -1.000000000000000000, 0.000000000000000000, -0.000000000000000000 ) ) ;
#154456 = CARTESIAN_POINT ( 'NONE',  ( -16.88495309932522304, 9.954627058472855339, -12.63454867381191526 ) ) ;
#154458 = FACE_OUTER_BOUND ( 'NONE', #45634, .T. ) ;
#154459 = CARTESIAN_POINT ( 'NONE',  ( -16.89935556175777265, 23.40971485048315159, -231.1662851018464835 ) ) ;
#154460 = CARTESIAN_POINT ( 'NONE',  ( 23.24999999999999289, 21.17283678855157802, -243.7231193059830048 ) ) ;
#154461 = FACE_OUTER_BOUND ( 'NONE', #144691, .T. ) ;
#154462 = ORIENTED_EDGE ( 'NONE', *, *, #95592, .F. ) ;
#154463 = EDGE_CURVE ( 'NONE', #229965, #84708, #150382, .T. ) ;
#154464 =( BOUNDED_CURVE ( )  B_SPLINE_CURVE ( 3, ( #187692, #7758, #226788, #6456 ),
 .UNSPECIFIED., .F., .F. ) 
 B_SPLINE_CURVE_WITH_KNOTS ( ( 4, 4 ),
 ( 3.141592653589778461, 4.712388980384686121 ),
 .UNSPECIFIED. ) 
 CURVE ( )  GEOMETRIC_REPRESENTATION_ITEM ( )  RATIONAL_B_SPLINE_CURVE ( ( 1.000000000000000000, 0.8047378541243622729, 0.8047378541243622729, 1.000000000000000000 ) ) 
 REPRESENTATION_ITEM ( '' )  );
#154466 = VERTEX_POINT ( 'NONE', #154270 ) ;
#154465 = DIRECTION ( 'NONE',  ( 1.000000000000000000, 0.000000000000000000, 0.000000000000000000 ) ) ;
#154467 = CIRCLE ( 'NONE', #79404, 0.09999999999999939493 ) ;
#154468 = ADVANCED_FACE ( 'NONE', ( #129524 ), #30437, .T. ) ;
#154469 = CARTESIAN_POINT ( 'NONE',  ( -20.64999999999999858, 1.925233644870967487, -188.2697564668738153 ) ) ;
#154470 = DIRECTION ( 'NONE',  ( 1.000000000000000000, 0.000000000000000000, 0.000000000000000000 ) ) ;
#154471 = ORIENTED_EDGE ( 'NONE', *, *, #119533, .F. ) ;
#154472 = AXIS2_PLACEMENT_3D ( 'NONE', #7313, #228937, #29488 ) ;
#154473 = ADVANCED_FACE ( 'NONE', ( #209057 ), #246588, .T. ) ;
#154474 = EDGE_CURVE ( 'NONE', #101205, #53590, #192621, .T. ) ;
#154475 = DIRECTION ( 'NONE',  ( 1.000000000000000000, -0.000000000000000000, 0.000000000000000000 ) ) ;
#154476 = VECTOR ( 'NONE', #240924, 1000.000000000000000 ) ;
#154477 = EDGE_CURVE ( 'NONE', #129700, #216121, #132088, .T. ) ;
#154478 = LINE ( 'NONE', #119172, #207909 ) ;
#154479 = ADVANCED_FACE ( 'NONE', ( #13435 ), #242498, .F. ) ;
#154480 = ORIENTED_EDGE ( 'NONE', *, *, #148424, .T. ) ;
#154481 = DIRECTION ( 'NONE',  ( -1.020425574104004196E-15, 6.982962677686266711E-15, -1.000000000000000000 ) ) ;
#154482 = FACE_OUTER_BOUND ( 'NONE', #185007, .T. ) ;
#154483 = EDGE_CURVE ( 'NONE', #64792, #246608, #13557, .T. ) ;
#154484 = CIRCLE ( 'NONE', #162857, 0.09999999999998898659 ) ;
#154485 = CARTESIAN_POINT ( 'NONE',  ( -18.59999999999999787, 74.75000000001189449, -95.02310748452431710 ) ) ;
#154487 = ORIENTED_EDGE ( 'NONE', *, *, #12403, .T. ) ;
#154486 = DIRECTION ( 'NONE',  ( 0.000000000000000000, 0.000000000000000000, -1.000000000000000000 ) ) ;
#154488 = DIRECTION ( 'NONE',  ( 1.000000000000000000, 0.000000000000000000, 0.000000000000000000 ) ) ;
#154490 = ORIENTED_EDGE ( 'NONE', *, *, #119647, .T. ) ;
#154489 = DIRECTION ( 'NONE',  ( -1.000000000000000000, 0.000000000000000000, 0.000000000000000000 ) ) ;
#154491 = LINE ( 'NONE', #34528, #191575 ) ;
#154492 = DIRECTION ( 'NONE',  ( -1.000000000000000000, -1.646408749285562691E-14, 0.000000000000000000 ) ) ;
#154493 = DIRECTION ( 'NONE',  ( 0.000000000000000000, 0.9371753822965326330, -0.3488585713686107592 ) ) ;
#154494 = DIRECTION ( 'NONE',  ( 0.000000000000000000, 0.8700118002898322711, -0.4930308989875231140 ) ) ;
#154496 = DIRECTION ( 'NONE',  ( 0.000000000000000000, 1.000000000000000000, 6.982962677686266711E-15 ) ) ;
#154495 = CARTESIAN_POINT ( 'NONE',  ( -16.84981964351507600, 9.917318234109812281, -154.6303983859796460 ) ) ;
#154497 = DIRECTION ( 'NONE',  ( -3.469446951953995998E-14, 0.000000000000000000, 1.000000000000000000 ) ) ;
#154498 = CARTESIAN_POINT ( 'NONE',  ( -21.05000000000000071, 64.36312671090826143, -163.2013482711997199 ) ) ;
#154499 = CARTESIAN_POINT ( 'NONE',  ( 21.22070241538126467, 0.09891903054618129965, -161.0300537271303654 ) ) ;
#154500 = DIRECTION ( 'NONE',  ( 1.000000000000000000, 0.000000000000000000, 0.000000000000000000 ) ) ;
#154501 = DIRECTION ( 'NONE',  ( 0.000000000000000000, -0.5378121776619179117, 0.8430646840892729310 ) ) ;
#154502 = VECTOR ( 'NONE', #99753, 1000.000000000000000 ) ;
#154503 = VERTEX_POINT ( 'NONE', #238513 ) ;
#154504 = EDGE_CURVE ( 'NONE', #8134, #114896, #79969, .T. ) ;
#154505 = DIRECTION ( 'NONE',  ( 1.000000000000000000, 2.952720810173289112E-16, -0.000000000000000000 ) ) ;
#154506 = ORIENTED_EDGE ( 'NONE', *, *, #78938, .F. ) ;
#154507 = AXIS2_PLACEMENT_3D ( 'NONE', #233454, #194331, #232162 ) ;
#154508 = ORIENTED_EDGE ( 'NONE', *, *, #119171, .F. ) ;
#154509 = DIRECTION ( 'NONE',  ( 0.000000000000000000, 6.938893903907270030E-14, 1.000000000000000000 ) ) ;
#154510 = CARTESIAN_POINT ( 'NONE',  ( 23.14999999999999858, 1.115600667400684642E-11, -167.4999999999999716 ) ) ;
#154511 = EDGE_CURVE ( 'NONE', #236784, #21148, #105089, .T. ) ;
#154512 = ORIENTED_EDGE ( 'NONE', *, *, #121139, .F. ) ;
#154513 = EDGE_CURVE ( 'NONE', #252270, #156138, #205060, .T. ) ;
#154514 = CIRCLE ( 'NONE', #83702, 0.1000000000000021844 ) ;
#154515 = ORIENTED_EDGE ( 'NONE', *, *, #140643, .T. ) ;
#154516 = FACE_OUTER_BOUND ( 'NONE', #47575, .T. ) ;
#154517 = FILL_AREA_STYLE ('',( #253569 ) ) ;
#154519 = ORIENTED_EDGE ( 'NONE', *, *, #212877, .F. ) ;
#154518 = CIRCLE ( 'NONE', #200277, 0.09999999999998898659 ) ;
#154520 = CIRCLE ( 'NONE', #254415, 4.000000000000003553 ) ;
#154521 = VECTOR ( 'NONE', #42581, 1000.000000000000000 ) ;
#154522 = ORIENTED_EDGE ( 'NONE', *, *, #204406, .T. ) ;
#154523 = AXIS2_PLACEMENT_3D ( 'NONE', #15012, #117931, #98331 ) ;
#154524 = AXIS2_PLACEMENT_3D ( 'NONE', #109326, #152357, #91068 ) ;
#154525 = DIRECTION ( 'NONE',  ( -1.000000000000000000, -0.000000000000000000, 0.000000000000000000 ) ) ;
#154526 = FACE_OUTER_BOUND ( 'NONE', #156958, .T. ) ;
#154527 = DIRECTION ( 'NONE',  ( -1.000000000000000000, -0.000000000000000000, -0.000000000000000000 ) ) ;
#154528 = CARTESIAN_POINT ( 'NONE',  ( 23.24999999999999645, 3.900000000011155432, -167.5000000000000284 ) ) ;
#154529 = CARTESIAN_POINT ( 'NONE',  ( 14.45204356427542081, 9.450668889167527453, -15.05554649020734814 ) ) ;
#154531 = PLANE ( 'NONE',  #45855 ) ;
#154530 = DIRECTION ( 'NONE',  ( 1.000000000000000000, 0.000000000000000000, 0.000000000000000000 ) ) ;
#154532 = DIRECTION ( 'NONE',  ( 0.000000000000000000, 7.147358527629759053E-15, -1.000000000000000000 ) ) ;
#154534 = EDGE_LOOP ( 'NONE', ( #10438, #66378, #183492, #196445 ) ) ;
#154533 = FACE_OUTER_BOUND ( 'NONE', #144933, .T. ) ;
#154536 = LINE ( 'NONE', #215734, #158520 ) ;
#154535 = CARTESIAN_POINT ( 'NONE',  ( -16.27683809663750480, 9.349999999999978328, -9.250000000000001776 ) ) ;
#154537 = DIRECTION ( 'NONE',  ( 0.000000000000000000, -0.2128009952262926163, 0.9770955615653463822 ) ) ;
#154538 =( BOUNDED_SURFACE ( )  B_SPLINE_SURFACE ( 3, 2, ( 
 ( #197040, #61396, #217878 ),
 ( #39294, #118820, #220486 ),
 ( #99215, #140948, #121412 ),
 ( #186489, #147352, #242588 ),
 ( #26136, #142212, #207342 ),
 ( #163088, #204743, #63969 ) ),
 .UNSPECIFIED., .F., .F., .F. ) 
 B_SPLINE_SURFACE_WITH_KNOTS ( ( 4, 2, 4 ),
 ( 3, 3 ),
 ( 0.0001792624049599519573, 0.0003686986002124681460, 0.0005581347954649843075 ),
 ( 0.000000000000000000, 1.000000000000000000 ),
 .UNSPECIFIED. ) 
 GEOMETRIC_REPRESENTATION_ITEM ( )  RATIONAL_B_SPLINE_SURFACE ( (
 ( 1.000000000000000000, 0.9238795325112673096, 1.000000000000000000),
 ( 1.000000000000000000, 0.9229318695242666459, 1.000000000000000000),
 ( 1.000000000000000000, 0.8926288119225271878, 1.000000000000000000),
 ( 1.000000000000000000, 0.8123777807276841845, 1.000000000000000000),
 ( 1.000000000000000000, 0.7629087100927172127, 1.000000000000000000),
 ( 1.000000000000000000, 0.7071067811865352493, 1.000000000000000000) ) ) 
 REPRESENTATION_ITEM ( '' )  SURFACE ( )  );
#154539 = EDGE_LOOP ( 'NONE', ( #243884, #56512, #256136, #136051, #81597 ) ) ;
#154540 = CARTESIAN_POINT ( 'NONE',  ( 21.13920837816993270, 8.783247050131068434, -146.2500000000000284 ) ) ;
#154541 = CARTESIAN_POINT ( 'NONE',  ( -21.05000000000000071, 77.85102823015316176, -158.3691942151018566 ) ) ;
#154542 = ORIENTED_EDGE ( 'NONE', *, *, #108323, .T. ) ;
#154543 = DIRECTION ( 'NONE',  ( 1.000000000000000000, 0.000000000000000000, 0.000000000000000000 ) ) ;
#154544 = DIRECTION ( 'NONE',  ( 0.000000000000000000, -8.338584948901395817E-15, 1.000000000000000000 ) ) ;
#154545 = DIRECTION ( 'NONE',  ( 0.000000000000000000, -0.8660254037844445918, -0.4999999999999897304 ) ) ;
#154546 = ORIENTED_EDGE ( 'NONE', *, *, #23437, .F. ) ;
#154547 = ORIENTED_EDGE ( 'NONE', *, *, #196238, .F. ) ;
#154548 = DIRECTION ( 'NONE',  ( 0.000000000000000000, 0.9908441862701605762, -0.1350103645451835310 ) ) ;
#154549 = CARTESIAN_POINT ( 'NONE',  ( -18.54260524012582323, -0.8405054967425236168, -242.3671242014665097 ) ) ;
#154550 = CARTESIAN_POINT ( 'NONE',  ( -18.59999999999999787, 7.021664781911246322, -104.3335654018973315 ) ) ;
#154551 = DIRECTION ( 'NONE',  ( -0.7071067811865456854, -0.7071067811865493491, -4.937700262164544098E-15 ) ) ;
#154552 = ORIENTED_EDGE ( 'NONE', *, *, #59474, .F. ) ;
#154553 = AXIS2_PLACEMENT_3D ( 'NONE', #170774, #112048, #232000 ) ;
#154554 = CARTESIAN_POINT ( 'NONE',  ( 12.93225390519045881, 46.82518482938920101, -234.6773041598981990 ) ) ;
#154555 = EDGE_CURVE ( 'NONE', #71706, #206437, #250857, .T. ) ;
#154556 = LINE ( 'NONE', #71155, #166749 ) ;
#154557 = CARTESIAN_POINT ( 'NONE',  ( 21.93642651522410603, 7.327166239336949438, -167.4999999999999716 ) ) ;
#154558 = EDGE_CURVE ( 'NONE', #248454, #233399, #42588, .T. ) ;
#154559 = DIRECTION ( 'NONE',  ( 0.000000000000000000, 1.000000000000000000, 2.891205793294679805E-16 ) ) ;
#154560 =( BOUNDED_SURFACE ( )  B_SPLINE_SURFACE ( 3, 2, ( 
 ( #158871, #218803, #256602 ),
 ( #55863, #96284, #177158 ),
 ( #40211, #97554, #238375 ),
 ( #137977, #36359, #100124 ) ),
 .UNSPECIFIED., .F., .F., .F. ) 
 B_SPLINE_SURFACE_WITH_KNOTS ( ( 4, 4 ),
 ( 3, 3 ),
 ( 0.0008258556059633777964, 0.0009616864997632713560 ),
 ( 0.000000000000000000, 1.000000000000000000 ),
 .UNSPECIFIED. ) 
 GEOMETRIC_REPRESENTATION_ITEM ( )  RATIONAL_B_SPLINE_SURFACE ( (
 ( 1.000000000000000000, 0.9152888060719425178, 1.000000000000000000),
 ( 1.000000000000000000, 0.9327727094138110742, 1.000000000000000000),
 ( 1.000000000000000000, 0.9369023509258611604, 1.000000000000000000),
 ( 1.000000000000000000, 0.9246339933864502481, 1.000000000000000000) ) ) 
 REPRESENTATION_ITEM ( '' )  SURFACE ( )  );
#154561 = EDGE_CURVE ( 'NONE', #196062, #214056, #16916, .T. ) ;
#154562 = TOROIDAL_SURFACE ( 'NONE', #150461, 11.70000000000000462, 0.1000000000000000056 ) ;
#154564 = VERTEX_POINT ( 'NONE', #18189 ) ;
#154563 = DIRECTION ( 'NONE',  ( -1.000000000000000000, -0.000000000000000000, -0.000000000000000000 ) ) ;
#154565 = CARTESIAN_POINT ( 'NONE',  ( 23.04999999999999716, 8.822561741677553471, -180.1499999999999773 ) ) ;
#154566 = EDGE_CURVE ( 'NONE', #125623, #44063, #113321, .T. ) ;
#154567 = DIRECTION ( 'NONE',  ( -1.000000000000000000, 0.000000000000000000, -0.000000000000000000 ) ) ;
#154568 = CARTESIAN_POINT ( 'NONE',  ( 20.94999999999999929, -1.835341550213257733, -78.55515129256302487 ) ) ;
#154569 = DIRECTION ( 'NONE',  ( -1.000000000000000000, 0.000000000000000000, 0.000000000000000000 ) ) ;
#154570 = CARTESIAN_POINT ( 'NONE',  ( 21.05000000000000071, 10.62950747927176387, -175.1279793999966898 ) ) ;
#154572 = VERTEX_POINT ( 'NONE', #222448 ) ;
#154571 = CARTESIAN_POINT ( 'NONE',  ( -23.25000000000000000, 76.00000000001195133, -103.0231074845243171 ) ) ;
#154573 = DIRECTION ( 'NONE',  ( -1.000000000000000000, 0.000000000000000000, 0.000000000000000000 ) ) ;
#154574 = DIRECTION ( 'NONE',  ( -1.000000000000000000, 0.000000000000000000, 0.000000000000000000 ) ) ;
#154575 = CARTESIAN_POINT ( 'NONE',  ( -18.34374000495060386, 11.47316190336247033, -9.249999999999998224 ) ) ;
#154576 = VERTEX_POINT ( 'NONE', #144206 ) ;
#154577 = LINE ( 'NONE', #77542, #88612 ) ;
#154578 = PLANE ( 'NONE',  #2595 ) ;
#154579 = LINE ( 'NONE', #257432, #4778 ) ;
#154580 = FACE_OUTER_BOUND ( 'NONE', #139501, .T. ) ;
#154582 = CIRCLE ( 'NONE', #216891, 0.1000000000000028644 ) ;
#154581 = CARTESIAN_POINT ( 'NONE',  ( -18.43473496883401808, 78.23946247294885836, -231.5402422415359069 ) ) ;
#154584 = AXIS2_PLACEMENT_3D ( 'NONE', #166339, #171477, #134849 ) ;
#154583 = CYLINDRICAL_SURFACE ( 'NONE', #50996, 0.09999999999999817368 ) ;
#154585 = EDGE_CURVE ( 'NONE', #142261, #47050, #145502, .T. ) ;
#154586 = EDGE_CURVE ( 'NONE', #54863, #109286, #864, .T. ) ;
#154587 = VERTEX_POINT ( 'NONE', #258031 ) ;
#154588 = ORIENTED_EDGE ( 'NONE', *, *, #36224, .T. ) ;
#154589 = CARTESIAN_POINT ( 'NONE',  ( -21.05000000000000071, 64.35000000001146248, -43.03791325517834565 ) ) ;
#154590 = CYLINDRICAL_SURFACE ( 'NONE', #37485, 0.1000000000000028644 ) ;
#154591 = CARTESIAN_POINT ( 'NONE',  ( -23.25000000000000000, 87.65000000001163016, -66.42310748452423752 ) ) ;
#154592 = CARTESIAN_POINT ( 'NONE',  ( -21.07928932188134041, 6.328516656404449492, -133.9011048543456184 ) ) ;
#154593 = DIRECTION ( 'NONE',  ( 1.000000000000000000, 0.000000000000000000, 0.000000000000000000 ) ) ;
#154594 = CARTESIAN_POINT ( 'NONE',  ( -23.25000000000000000, 69.01799029515495931, -32.32695536626808774 ) ) ;
#154595 = ADVANCED_FACE ( 'NONE', ( #45128 ), #124674, .F. ) ;
#154596 = TOROIDAL_SURFACE ( 'NONE', #83785, 0.4000000000000003553, 0.1000000000000000056 ) ;
#154597 = DIRECTION ( 'NONE',  ( 1.000000000000000000, 0.000000000000000000, 0.000000000000000000 ) ) ;
#154598 = ADVANCED_FACE ( 'NONE', ( #97692 ), #28094, .T. ) ;
#154599 = CARTESIAN_POINT ( 'NONE',  ( -22.39999999999999858, 31.80471377451587500, -238.9601694054148027 ) ) ;
#154600 = ORIENTED_EDGE ( 'NONE', *, *, #238048, .T. ) ;
#154601 = LINE ( 'NONE', #55429, #102183 ) ;
#154602 = VERTEX_POINT ( 'NONE', #5981 ) ;
#154603 = VERTEX_POINT ( 'NONE', #129792 ) ;
#154604 = DIRECTION ( 'NONE',  ( 1.000000000000000000, 0.000000000000000000, 0.000000000000000000 ) ) ;
#154605 = DIRECTION ( 'NONE',  ( 0.000000000000000000, 0.000000000000000000, 1.000000000000000000 ) ) ;
#154606 = CARTESIAN_POINT ( 'NONE',  ( -18.39999999999999858, 64.52683809665015247, -194.1971614177164724 ) ) ;
#154608 = ORIENTED_EDGE ( 'NONE', *, *, #234512, .F. ) ;
#154607 = CARTESIAN_POINT ( 'NONE',  ( -20.94999999999999929, -11.48912529306490349, -103.6000000000000369 ) ) ;
#154609 = EDGE_CURVE ( 'NONE', #253301, #111732, #171805, .T. ) ;
#154610 = CARTESIAN_POINT ( 'NONE',  ( -23.25000000000000000, 79.19526988099229925, -196.1889237952725296 ) ) ;
#154611 = DIRECTION ( 'NONE',  ( 0.000000000000000000, 0.000000000000000000, -1.000000000000000000 ) ) ;
#154612 = CARTESIAN_POINT ( 'NONE',  ( 18.50000000000000355, 85.40000000001165859, -62.64106563635154856 ) ) ;
#154613 = EDGE_LOOP ( 'NONE', ( #68675, #129087, #230362, #94828 ) ) ;
#154614 = CARTESIAN_POINT ( 'NONE',  ( -12.60829076262180948, 9.389529397477893724, -151.8171079128937606 ) ) ;
#154615 = CIRCLE ( 'NONE', #12573, 0.09999999999999939493 ) ;
#154616 = LINE ( 'NONE', #16377, #192452 ) ;
#154617 = AXIS2_PLACEMENT_3D ( 'NONE', #85369, #68421, #187103 ) ;
#154618 = CIRCLE ( 'NONE', #96298, 0.09999999999998898659 ) ;
#154619 = DIRECTION ( 'NONE',  ( 4.026293107431335996E-15, 0.8700118002898393765, -0.4930308989875104575 ) ) ;
#154620 = CARTESIAN_POINT ( 'NONE',  ( -18.50000000000001066, 85.42130820975189920, -162.7807442704735479 ) ) ;
#154621 = CIRCLE ( 'NONE', #242062, 0.1000000000000070832 ) ;
#154622 = ADVANCED_FACE ( 'NONE', ( #210617 ), #116427, .T. ) ;
#154623 = ORIENTED_EDGE ( 'NONE', *, *, #83826, .T. ) ;
#154624 = DIRECTION ( 'NONE',  ( 1.000000000000000000, 0.000000000000000000, 0.000000000000000000 ) ) ;
#154625 = DIRECTION ( 'NONE',  ( 0.000000000000000000, 0.000000000000000000, -1.000000000000000000 ) ) ;
#154626 = VERTEX_POINT ( 'NONE', #187227 ) ;
#154627 = CARTESIAN_POINT ( 'NONE',  ( 21.09813707148777340, 6.385062105747659977, -133.9686485004704934 ) ) ;
#154628 = EDGE_CURVE ( 'NONE', #121241, #158368, #21757, .T. ) ;
#154629 = DIRECTION ( 'NONE',  ( -0.000000000000000000, -0.1350103645451928291, -0.9908441862701594660 ) ) ;
#154630 = CARTESIAN_POINT ( 'NONE',  ( 21.05000000000000071, 36.02367271998545561, -235.8812521208699309 ) ) ;
#154631 = AXIS2_PLACEMENT_3D ( 'NONE', #185015, #5060, #84578 ) ;
#154632 = EDGE_CURVE ( 'NONE', #74222, #40972, #88349, .T. ) ;
#154633 = EDGE_LOOP ( 'NONE', ( #122320, #80337, #91667, #198297 ) ) ;
#154634 = CARTESIAN_POINT ( 'NONE',  ( 18.44206774312976194, -9.491027357528897923, -174.1262275046982779 ) ) ;
#154635 = CARTESIAN_POINT ( 'NONE',  ( 21.05000000000000071, 60.94483358488582070, -234.0465764481390636 ) ) ;
#154636 = ORIENTED_EDGE ( 'NONE', *, *, #51725, .F. ) ;
#154637 = ORIENTED_EDGE ( 'NONE', *, *, #141510, .T. ) ;
#154638 = CARTESIAN_POINT ( 'NONE',  ( -23.25000000000000000, 4.250000000011156409, -155.1500000000000057 ) ) ;
#154639 = LINE ( 'NONE', #254927, #58702 ) ;
#154640 = VECTOR ( 'NONE', #118666, 1000.000000000000000 ) ;
#154642 = ORIENTED_EDGE ( 'NONE', *, *, #128011, .T. ) ;
#154641 = FACE_OUTER_BOUND ( 'NONE', #234106, .T. ) ;
#154643 = DIRECTION ( 'NONE',  ( 1.000000000000000000, -1.875376730785737719E-16, -1.309568571767809260E-30 ) ) ;
#154645 = CARTESIAN_POINT ( 'NONE',  ( -17.11825945287482753, 9.950000000011138823, -113.2500000000000284 ) ) ;
#154644 = UNCERTAINTY_MEASURE_WITH_UNIT (LENGTH_MEASURE( 1.000000000000000082E-05 ), #152890, 'distance_accuracy_value', 'NONE');
#154646 = CARTESIAN_POINT ( 'NONE',  ( -20.54999999999999361, 61.57587952878036930, -212.2000740415318774 ) ) ;
#154647 = CARTESIAN_POINT ( 'NONE',  ( -18.38639463286148867, 11.48019957384713230, -76.25000000000004263 ) ) ;
#154648 = CARTESIAN_POINT ( 'NONE',  ( -23.15000000000000213, -11.75000000000000000, -30.39999999999999503 ) ) ;
#154649 = AXIS2_PLACEMENT_3D ( 'NONE', #214209, #233776, #152983 ) ;
#154650 = LINE ( 'NONE', #58061, #217923 ) ;
#154651 = DIRECTION ( 'NONE',  ( 0.000000000000000000, 0.5273008465187821736, -0.8496786552930323255 ) ) ;
#154653 = ORIENTED_EDGE ( 'NONE', *, *, #215664, .T. ) ;
#154652 = CARTESIAN_POINT ( 'NONE',  ( 18.59999999999999076, 68.87972903831379767, -32.36354444268504693 ) ) ;
#154654 = ORIENTED_EDGE ( 'NONE', *, *, #241766, .T. ) ;
#154656 = CARTESIAN_POINT ( 'NONE',  ( -16.77180007708460963, 51.63199159464676313, -231.9405875366200860 ) ) ;
#154655 = CARTESIAN_POINT ( 'NONE',  ( -21.14999999999999858, 55.91711482281189660, -232.6830152854666949 ) ) ;
#154658 = ORIENTED_EDGE ( 'NONE', *, *, #138648, .T. ) ;
#154657 = DIRECTION ( 'NONE',  ( 1.000000000000000000, -0.000000000000000000, -0.000000000000000000 ) ) ;
#154659 = CIRCLE ( 'NONE', #63029, 0.1000000000000000472 ) ;
#154660 = EDGE_LOOP ( 'NONE', ( #93232, #86579, #91589, #155083 ) ) ;
#154661 = CARTESIAN_POINT ( 'NONE',  ( -18.53317502108577486, 10.32263460347359540, -106.0605957968672470 ) ) ;
#154662 = LINE ( 'NONE', #17673, #51371 ) ;
#154663 = CIRCLE ( 'NONE', #42209, 0.09999999999998898659 ) ;
#154664 = CARTESIAN_POINT ( 'NONE',  ( 18.59999999999999787, -11.74999999998883737, -158.8500000000000227 ) ) ;
#154665 = AXIS2_PLACEMENT_3D ( 'NONE', #194316, #58607, #119920 ) ;
#154666 = CARTESIAN_POINT ( 'NONE',  ( 19.97071067695831559, 11.72071067696947644, -58.17625343280366934 ) ) ;
#154667 = CARTESIAN_POINT ( 'NONE',  ( -18.50000000000000000, 67.49463558145298236, -195.5618716440587548 ) ) ;
#154668 = CARTESIAN_POINT ( 'NONE',  ( 21.05000000000000071, 11.65000000000000746, 0.000000000000000000 ) ) ;
#154669 = AXIS2_PLACEMENT_3D ( 'NONE', #172771, #78737, #14949 ) ;
#154670 = DIRECTION ( 'NONE',  ( -0.000000000000000000, 1.000000000000000000, 0.000000000000000000 ) ) ;
#154671 = VERTEX_POINT ( 'NONE', #9849 ) ;
#154672 = ORIENTED_EDGE ( 'NONE', *, *, #170446, .T. ) ;
#154673 = EDGE_CURVE ( 'NONE', #156346, #30659, #168972, .T. ) ;
#154674 = CARTESIAN_POINT ( 'NONE',  ( -16.81744102076749314, 12.41403342719998726, -211.2428889513006993 ) ) ;
#154675 = AXIS2_PLACEMENT_3D ( 'NONE', #179966, #236071, #1295 ) ;
#154676 = VERTEX_POINT ( 'NONE', #50241 ) ;
#154677 = DIRECTION ( 'NONE',  ( 1.000000000000000000, -0.000000000000000000, -0.000000000000000000 ) ) ;
#154678 = DIRECTION ( 'NONE',  ( -0.000000000000000000, 0.2128009952263603677, -0.9770955615653313941 ) ) ;
#154679 = VECTOR ( 'NONE', #117985, 1000.000000000000000 ) ;
#154680 = CARTESIAN_POINT ( 'NONE',  ( -16.94333152886235894, 9.990342011461637028, -79.60796846894562862 ) ) ;
#154681 = ORIENTED_EDGE ( 'NONE', *, *, #201402, .T. ) ;
#154682 = EDGE_CURVE ( 'NONE', #196464, #105159, #209324, .T. ) ;
#154683 = DIRECTION ( 'NONE',  ( 0.000000000000000000, 0.000000000000000000, -1.000000000000000000 ) ) ;
#154684 = EDGE_LOOP ( 'NONE', ( #33818, #173268, #146323, #138369 ) ) ;
#154686 = CIRCLE ( 'NONE', #17131, 0.09999999999999939493 ) ;
#154685 = DIRECTION ( 'NONE',  ( 3.616040088954497272E-32, -1.224646799147352961E-16, 1.000000000000000000 ) ) ;
#154687 = EDGE_LOOP ( 'NONE', ( #131667, #68115, #22563, #194416 ) ) ;
#154688 = EDGE_CURVE ( 'NONE', #27378, #191238, #256463, .T. ) ;
#154689 = CARTESIAN_POINT ( 'NONE',  ( 20.94999999999999929, 87.65000000001144542, -38.92310748452424463 ) ) ;
#154690 = DIRECTION ( 'NONE',  ( 0.000000000000000000, 0.000000000000000000, 1.000000000000000000 ) ) ;
#154691 = ORIENTED_EDGE ( 'NONE', *, *, #99609, .F. ) ;
#154692 = CARTESIAN_POINT ( 'NONE',  ( 20.12500000000000000, 9.749999999999998224, -21.15000000000000213 ) ) ;
#154693 = ORIENTED_EDGE ( 'NONE', *, *, #7851, .F. ) ;
#154695 = ORIENTED_EDGE ( 'NONE', *, *, #207240, .F. ) ;
#154694 = FACE_OUTER_BOUND ( 'NONE', #28312, .T. ) ;
#154696 = AXIS2_PLACEMENT_3D ( 'NONE', #23452, #5099, #84626 ) ;
#154697 = CARTESIAN_POINT ( 'NONE',  ( -20.96077737575335576, 64.37609936600659921, -42.88231552741780206 ) ) ;
#154698 = AXIS2_PLACEMENT_3D ( 'NONE', #122599, #92425, #250229 ) ;
#154700 = EDGE_LOOP ( 'NONE', ( #227377, #183611, #149679, #187491, #99490, #209917, #77661, #61968, #175348, #89185, #139378, #142426 ) ) ;
#154699 = CIRCLE ( 'NONE', #88176, 0.09999999999999939493 ) ;
#154701 = VERTEX_POINT ( 'NONE', #26877 ) ;
#154702 = EDGE_CURVE ( 'NONE', #1482, #125207, #7272, .T. ) ;
#154703 = PLANE ( 'NONE',  #99020 ) ;
#154704 = ADVANCED_FACE ( 'NONE', ( #17534 ), #34569, .T. ) ;
#154705 = ORIENTED_EDGE ( 'NONE', *, *, #69694, .F. ) ;
#154706 = LINE ( 'NONE', #175548, #10109 ) ;
#154707 = CARTESIAN_POINT ( 'NONE',  ( 21.04999999999999716, 69.55891531154045992, -69.50538805121503572 ) ) ;
#154708 = DIRECTION ( 'NONE',  ( 1.186688945009010077E-16, 1.000000000000000000, 6.982962677686266711E-15 ) ) ;
#154709 = CARTESIAN_POINT ( 'NONE',  ( -20.54999999999999716, 78.98983215084128062, -228.7927651294584450 ) ) ;
#154710 = CARTESIAN_POINT ( 'NONE',  ( -21.11101077989000174, 0.01528526892543676310, -60.57631526527391941 ) ) ;
#154711 = ORIENTED_EDGE ( 'NONE', *, *, #172877, .F. ) ;
#154712 = DIRECTION ( 'NONE',  ( -0.000000000000000000, -0.000000000000000000, -1.000000000000000000 ) ) ;
#154713 = CARTESIAN_POINT ( 'NONE',  ( -21.05000000000000071, 38.08698097766499302, -236.1457910985472779 ) ) ;
#154714 = CARTESIAN_POINT ( 'NONE',  ( -21.05000000000000071, -1.360870587180885716, -41.57299792709095954 ) ) ;
#154715 = ORIENTED_EDGE ( 'NONE', *, *, #68118, .F. ) ;
#154716 = LINE ( 'NONE', #37325, #63718 ) ;
#154717 = ORIENTED_EDGE ( 'NONE', *, *, #65637, .F. ) ;
#154718 = CARTESIAN_POINT ( 'NONE',  ( -20.64999999999999858, 2.499999999999998668, -20.27537807723789953 ) ) ;
#154719 = ORIENTED_EDGE ( 'NONE', *, *, #75800, .T. ) ;
#154720 = EDGE_CURVE ( 'NONE', #9387, #17853, #188331, .T. ) ;
#154721 = DIRECTION ( 'NONE',  ( -1.000000000000000000, 1.335000415235278971E-16, -2.979993593738921214E-16 ) ) ;
#154722 = DIRECTION ( 'NONE',  ( -0.7071067811865127117, -0.7071067811865821007, 0.000000000000000000 ) ) ;
#154724 = ORIENTED_EDGE ( 'NONE', *, *, #38740, .T. ) ;
#154723 = DIRECTION ( 'NONE',  ( 1.000000000000000000, 0.000000000000000000, 0.000000000000000000 ) ) ;
#154725 = CARTESIAN_POINT ( 'NONE',  ( -18.43473496883421348, 8.856286808022053592, -245.4294671909037504 ) ) ;
#154726 = ORIENTED_EDGE ( 'NONE', *, *, #41117, .T. ) ;
#154727 = AXIS2_PLACEMENT_3D ( 'NONE', #217214, #97243, #20343 ) ;
#154728 = CARTESIAN_POINT ( 'NONE',  ( -21.02374657821557946, 36.02918351771350558, -236.0543695115171943 ) ) ;
#154729 = LINE ( 'NONE', #32210, #52084 ) ;
#154731 = EDGE_CURVE ( 'NONE', #94704, #143019, #233646, .T. ) ;
#154730 = EDGE_LOOP ( 'NONE', ( #58564, #179119, #81896, #238773 ) ) ;
#154732 = CARTESIAN_POINT ( 'NONE',  ( 18.54999999999999716, 66.05000000001200533, -115.6731074845243228 ) ) ;
#154733 = CARTESIAN_POINT ( 'NONE',  ( -20.54999999999999716, 85.50000000001179501, -79.41707660717668205 ) ) ;
#154734 = ORIENTED_EDGE ( 'NONE', *, *, #178207, .F. ) ;
#154735 = CARTESIAN_POINT ( 'NONE',  ( 21.07928932188134397, 10.02993822722305062, -228.1074463178676979 ) ) ;
#154736 = VERTEX_POINT ( 'NONE', #115362 ) ;
#154738 = CARTESIAN_POINT ( 'NONE',  ( 15.31784899511109899, 9.396630376328872103, -118.4070573928183165 ) ) ;
#154737 = CIRCLE ( 'NONE', #192158, 0.1000000000000028644 ) ;
#154739 = LINE ( 'NONE', #200259, #30696 ) ;
#154741 = ORIENTED_EDGE ( 'NONE', *, *, #179901, .F. ) ;
#154740 = FACE_OUTER_BOUND ( 'NONE', #6958, .T. ) ;
#154742 = CARTESIAN_POINT ( 'NONE',  ( -18.59999999999999787, 42.98415524044398950, -233.9519173640448173 ) ) ;
#154743 = CARTESIAN_POINT ( 'NONE',  ( -20.94999999999999929, 70.17424292862648372, -198.1782849070719124 ) ) ;
#154744 = CARTESIAN_POINT ( 'NONE',  ( -16.94107738177414291, 10.01423928513661998, -20.94999999999999929 ) ) ;
#154746 = CARTESIAN_POINT ( 'NONE',  ( 23.40000000000005542, 87.50449464844290048, -34.18759587077607165 ) ) ;
#154745 = FACE_OUTER_BOUND ( 'NONE', #70778, .T. ) ;
#154747 = DIRECTION ( 'NONE',  ( -1.000000000000000000, 0.000000000000000000, 0.000000000000000000 ) ) ;
#154748 = DIRECTION ( 'NONE',  ( 1.000000000000000000, 0.000000000000000000, 0.000000000000000000 ) ) ;
#154749 = AXIS2_PLACEMENT_3D ( 'NONE', #88737, #249143, #169634 ) ;
#154750 = CARTESIAN_POINT ( 'NONE',  ( 18.57071067811864040, 65.82071067813089371, -148.7731074845244450 ) ) ;
#154751 = VECTOR ( 'NONE', #104696, 1000.000000000000000 ) ;
#154752 = DIRECTION ( 'NONE',  ( -7.304098846218134667E-16, 1.000000000000000000, 6.982962677686266711E-15 ) ) ;
#154754 = VERTEX_POINT ( 'NONE', #77494 ) ;
#154753 = CIRCLE ( 'NONE', #79702, 0.09999999999998898659 ) ;
#154755 = ORIENTED_EDGE ( 'NONE', *, *, #227876, .T. ) ;
#154756 = EDGE_CURVE ( 'NONE', #136422, #97734, #38402, .T. ) ;
#154757 = DIRECTION ( 'NONE',  ( 0.000000000000000000, 0.9126074666063770380, 0.4088369013363281068 ) ) ;
#154758 = EDGE_CURVE ( 'NONE', #224002, #126102, #117922, .T. ) ;
#154760 = ORIENTED_EDGE ( 'NONE', *, *, #230159, .F. ) ;
#154759 = CARTESIAN_POINT ( 'NONE',  ( -20.94999999999994600, 65.35000000001120668, -4.623107484524796362 ) ) ;
#154761 = ORIENTED_EDGE ( 'NONE', *, *, #7650, .F. ) ;
#154762 = CARTESIAN_POINT ( 'NONE',  ( -18.38204789744325396, 64.52049896284744079, -179.2731074845244450 ) ) ;
#154763 = ORIENTED_EDGE ( 'NONE', *, *, #29750, .F. ) ;
#154764 = EDGE_CURVE ( 'NONE', #103887, #52039, #137858, .T. ) ;
#154765 = EDGE_CURVE ( 'NONE', #71756, #208687, #154663, .T. ) ;
#154766 = ORIENTED_EDGE ( 'NONE', *, *, #71734, .F. ) ;
#154767 = AXIS2_PLACEMENT_3D ( 'NONE', #105446, #186315, #187611 ) ;
#154768 = ADVANCED_FACE ( 'NONE', ( #133647 ), #213176, .F. ) ;
#154769 = SURFACE_STYLE_USAGE ( .BOTH. , #97293 ) ;
#154770 = DIRECTION ( 'NONE',  ( -1.000000000000000000, 0.000000000000000000, 0.000000000000000000 ) ) ;
#154771 = EDGE_CURVE ( 'NONE', #16494, #255303, #57940, .T. ) ;
#154773 = ORIENTED_EDGE ( 'NONE', *, *, #195603, .T. ) ;
#154772 = ORIENTED_EDGE ( 'NONE', *, *, #30824, .F. ) ;
#154774 = ORIENTED_EDGE ( 'NONE', *, *, #186153, .T. ) ;
#154776 = ADVANCED_FACE ( 'NONE', ( #136178 ), #187967, .T. ) ;
#154775 = EDGE_CURVE ( 'NONE', #155129, #84120, #203220, .T. ) ;
#154777 = ORIENTED_EDGE ( 'NONE', *, *, #188022, .T. ) ;
#154778 = ORIENTED_EDGE ( 'NONE', *, *, #10687, .T. ) ;
#154779 = CARTESIAN_POINT ( 'NONE',  ( 21.05000000000000071, 8.826429739528350638, -142.4140547129437095 ) ) ;
#154780 = DIRECTION ( 'NONE',  ( 0.000000000000000000, 6.982962677686266711E-15, -1.000000000000000000 ) ) ;
#154782 = ORIENTED_EDGE ( 'NONE', *, *, #239702, .F. ) ;
#154781 = DIRECTION ( 'NONE',  ( 5.850181106597693140E-15, -0.1686199900910279881, 0.9856811345164833149 ) ) ;
#154783 = CARTESIAN_POINT ( 'NONE',  ( -21.07016717456946964, 34.07469055596557439, -243.7826248964179854 ) ) ;
#154784 = DIRECTION ( 'NONE',  ( 1.000000000000000000, 0.000000000000000000, -0.000000000000000000 ) ) ;
#154786 = ORIENTED_EDGE ( 'NONE', *, *, #115285, .F. ) ;
#154785 = CYLINDRICAL_SURFACE ( 'NONE', #222320, 0.5000000000000004441 ) ;
#154787 = LINE ( 'NONE', #118200, #87580 ) ;
#154788 = ORIENTED_EDGE ( 'NONE', *, *, #20234, .F. ) ;
#154789 = LINE ( 'NONE', #110494, #86868 ) ;
#154791 = ORIENTED_EDGE ( 'NONE', *, *, #256043, .F. ) ;
#154790 = DIRECTION ( 'NONE',  ( 0.000000000000000000, 0.000000000000000000, 1.000000000000000000 ) ) ;
#154792 = LINE ( 'NONE', #252566, #35249 ) ;
#154794 = ADVANCED_FACE ( 'NONE', ( #174108 ), #50556, .T. ) ;
#154793 = CARTESIAN_POINT ( 'NONE',  ( -23.15000000000000213, 4.250000000011156409, -45.85000000000000142 ) ) ;
#154795 = CIRCLE ( 'NONE', #4887, 0.09999999999998969435 ) ;
#154796 = AXIS2_PLACEMENT_3D ( 'NONE', #207739, #126900, #29129 ) ;
#154797 = CIRCLE ( 'NONE', #133911, 0.3999999999999975797 ) ;
#154798 = ORIENTED_EDGE ( 'NONE', *, *, #113718, .F. ) ;
#154800 = DIRECTION ( 'NONE',  ( 1.000000000000000000, 0.000000000000000000, 0.000000000000000000 ) ) ;
#154799 = DIRECTION ( 'NONE',  ( 1.000000000000000000, 0.000000000000000000, 0.000000000000000000 ) ) ;
#154801 = EDGE_CURVE ( 'NONE', #2421, #117589, #257381, .T. ) ;
#154802 = EDGE_CURVE ( 'NONE', #110925, #207616, #28117, .T. ) ;
#154803 = CARTESIAN_POINT ( 'NONE',  ( -22.39999999999999858, 11.65000000001115588, -100.4000000000000483 ) ) ;
#154804 = CARTESIAN_POINT ( 'NONE',  ( -18.50000000000000000, -1.164121893230052995, -74.71484808557160306 ) ) ;
#154805 = DIRECTION ( 'NONE',  ( 1.000000000000000000, -0.000000000000000000, -0.000000000000000000 ) ) ;
#154806 = EDGE_LOOP ( 'NONE', ( #106245, #242557, #197974, #31365 ) ) ;
#154807 = ORIENTED_EDGE ( 'NONE', *, *, #77197, .F. ) ;
#154808 = ADVANCED_FACE ( 'NONE', ( #112807 ), #13696, .F. ) ;
#154809 = CARTESIAN_POINT ( 'NONE',  ( -21.14999999999999858, -11.75000000000000000, 3.469446951953614189E-15 ) ) ;
#154810 = CARTESIAN_POINT ( 'NONE',  ( 20.94999999999999574, 77.83534155023646406, -124.9679561919613064 ) ) ;
#154811 = ORIENTED_EDGE ( 'NONE', *, *, #238648, .T. ) ;
#154812 = DIRECTION ( 'NONE',  ( 0.000000000000000000, -6.547589603894034005E-15, 1.000000000000000000 ) ) ;
#154813 = ORIENTED_EDGE ( 'NONE', *, *, #130679, .F. ) ;
#154814 = DIRECTION ( 'NONE',  ( 0.000000000000000000, 7.116814260417668513E-15, -1.000000000000000000 ) ) ;
#154815 = CYLINDRICAL_SURFACE ( 'NONE', #200157, 4.000000000000000000 ) ;
#154816 = EDGE_CURVE ( 'NONE', #77397, #251500, #65497, .T. ) ;
#154817 = AXIS2_PLACEMENT_3D ( 'NONE', #109000, #43908, #247230 ) ;
#154818 = EDGE_LOOP ( 'NONE', ( #202144, #151373, #184972 ) ) ;
#154819 = CARTESIAN_POINT ( 'NONE',  ( -16.81930730667007623, 66.06300193113855812, -190.7963397539862740 ) ) ;
#154820 = ORIENTED_EDGE ( 'NONE', *, *, #54179, .F. ) ;
#154821 = EDGE_LOOP ( 'NONE', ( #225828, #98031, #156610, #54356 ) ) ;
#154822 = ORIENTED_EDGE ( 'NONE', *, *, #94695, .F. ) ;
#154823 = DIRECTION ( 'NONE',  ( -1.000000000000000000, -0.000000000000000000, -0.000000000000000000 ) ) ;
#154824 = DIRECTION ( 'NONE',  ( 1.000000000000000000, -0.000000000000000000, 0.000000000000000000 ) ) ;
#154825 = CARTESIAN_POINT ( 'NONE',  ( 20.46382478191414833, 8.901379558713770734, -142.5457280948831169 ) ) ;
#154826 = DIRECTION ( 'NONE',  ( -1.000000000000000000, -0.000000000000000000, -0.000000000000000000 ) ) ;
#154827 = DIRECTION ( 'NONE',  ( 0.000000000000000000, -1.000000000000000000, 0.000000000000000000 ) ) ;
#154828 = CIRCLE ( 'NONE', #175662, 0.4000000000000045186 ) ;
#154830 = DIRECTION ( 'NONE',  ( 0.000000000000000000, -6.688090509790097607E-15, 1.000000000000000000 ) ) ;
#154829 = DIRECTION ( 'NONE',  ( 1.000000000000000000, 0.000000000000000000, 0.000000000000000000 ) ) ;
#154832 = ORIENTED_EDGE ( 'NONE', *, *, #240178, .F. ) ;
#154831 = CARTESIAN_POINT ( 'NONE',  ( -18.59999999999999787, 64.25000000001170974, -69.52310748452438816 ) ) ;
#154833 = CARTESIAN_POINT ( 'NONE',  ( -20.54999999999999716, 46.10080905699345521, -240.6643289267983334 ) ) ;
#154834 = ORIENTED_EDGE ( 'NONE', *, *, #28388, .F. ) ;
#154835 = CARTESIAN_POINT ( 'NONE',  ( -16.86757978335471719, 22.93962380547342050, -230.8967158438207719 ) ) ;
#154836 = ORIENTED_EDGE ( 'NONE', *, *, #128945, .F. ) ;
#154837 = ORIENTED_EDGE ( 'NONE', *, *, #238410, .F. ) ;
#154838 = CARTESIAN_POINT ( 'NONE',  ( -16.94107738177414291, 65.98576071487489969, -48.57310748452439952 ) ) ;
#154839 = TOROIDAL_SURFACE ( 'NONE', #163196, 0.2000000000000000111, 0.1000000000000000056 ) ;
#154840 = CARTESIAN_POINT ( 'NONE',  ( -21.09107601085575467, 6.363877975371003970, -133.9606928352826003 ) ) ;
#154841 = CARTESIAN_POINT ( 'NONE',  ( 23.14999999999998437, -3.957237024328102759, -201.8618440306682658 ) ) ;
#154842 = CARTESIAN_POINT ( 'NONE',  ( 0.8999999999999993561, -9.650000000000003908, 28.60000000000000142 ) ) ;
#154843 = VECTOR ( 'NONE', #247870, 1000.000000000000000 ) ;
#154844 = B_SPLINE_CURVE_WITH_KNOTS ( 'NONE', 3,
 ( #109189, #30990, #27140, #106613, #186185, #149639, #8828, #128781, #7538, #88326 ),
 .UNSPECIFIED., .F., .F.,
 ( 4, 3, 3, 4 ),
 ( 0.000000000000000000, 1.004626015990974373E-05, 1.831183478182685622E-05, 2.062343583996223352E-05 ),
 .UNSPECIFIED. ) ;
#154845 = CARTESIAN_POINT ( 'NONE',  ( 20.85882249326303040, 18.41524492703433324, -237.0006385043383546 ) ) ;
#154846 = ORIENTED_EDGE ( 'NONE', *, *, #145336, .F. ) ;
#154847 = EDGE_LOOP ( 'NONE', ( #154822, #10999, #225837, #161839 ) ) ;
#154848 = CIRCLE ( 'NONE', #50740, 0.09999999999999939493 ) ;
#154849 = ORIENTED_EDGE ( 'NONE', *, *, #230053, .T. ) ;
#154850 = CARTESIAN_POINT ( 'NONE',  ( -18.59999999999999787, 74.36282728704190959, -158.4409541190523498 ) ) ;
#154851 = DIRECTION ( 'NONE',  ( 0.000000000000000000, 1.000000000000000000, 6.982962677686266711E-15 ) ) ;
#154852 = ORIENTED_EDGE ( 'NONE', *, *, #234052, .T. ) ;
#154853 = CARTESIAN_POINT ( 'NONE',  ( -20.94999999999999929, -11.48912529306489994, -164.5000000000000000 ) ) ;
#154854 = DIRECTION ( 'NONE',  ( 0.000000000000000000, 1.000000000000000000, 6.982962677686266711E-15 ) ) ;
#154855 = CARTESIAN_POINT ( 'NONE',  ( -22.50000000000000000, 64.35042919246686210, -69.62310748452439668 ) ) ;
#154856 = CARTESIAN_POINT ( 'NONE',  ( 21.05000000000000071, 81.91411460262999356, -215.0718681741873013 ) ) ;
#154857 = ORIENTED_EDGE ( 'NONE', *, *, #16129, .T. ) ;
#154858 = CIRCLE ( 'NONE', #29957, 0.09999999999999939493 ) ;
#154860 = VECTOR ( 'NONE', #104753, 1000.000000000000000 ) ;
#154859 = CARTESIAN_POINT ( 'NONE',  ( -16.27683809663751191, 66.65000000001263913, -194.2731074845244450 ) ) ;
#154861 = ADVANCED_FACE ( 'NONE', ( #220875 ), #63087, .T. ) ;
#154862 = CARTESIAN_POINT ( 'NONE',  ( -12.25000000000000178, 66.15000000001185754, -86.27310748452437394 ) ) ;
#154863 = VECTOR ( 'NONE', #203044, 1000.000000000000000 ) ;
#154864 = FACE_OUTER_BOUND ( 'NONE', #241031, .T. ) ;
#154865 = EDGE_CURVE ( 'NONE', #121176, #184585, #71267, .T. ) ;
#154866 = AXIS2_PLACEMENT_3D ( 'NONE', #40188, #179681, #119708 ) ;
#154867 = ORIENTED_EDGE ( 'NONE', *, *, #191514, .T. ) ;
#154868 = AXIS2_PLACEMENT_3D ( 'NONE', #135265, #156160, #17890 ) ;
#154869 = ADVANCED_FACE ( 'NONE', ( #184317 ), #162226, .F. ) ;
#154870 = CARTESIAN_POINT ( 'NONE',  ( 21.09793522318410552, 10.72462451021277730, -12.23929087097709356 ) ) ;
#154871 = ADVANCED_FACE ( 'NONE', ( #179222 ), #78312, .T. ) ;
#154872 = VERTEX_POINT ( 'NONE', #61822 ) ;
#154873 = CARTESIAN_POINT ( 'NONE',  ( -21.45000000000000284, 68.29142135624888965, -57.17310748452437963 ) ) ;
#154874 = AXIS2_PLACEMENT_3D ( 'NONE', #188014, #115844, #57124 ) ;
#154875 = CARTESIAN_POINT ( 'NONE',  ( -16.93234230245722216, 14.22041164560202375, -219.3109751335834687 ) ) ;
#154876 = CARTESIAN_POINT ( 'NONE',  ( 18.59999999999999076, 6.649999999999999467, -21.15000000000000213 ) ) ;
#154877 = CARTESIAN_POINT ( 'NONE',  ( 18.59999999999998366, 68.97833521811159585, -65.68954208262705663 ) ) ;
#154878 = DIRECTION ( 'NONE',  ( 1.000000000000000000, 0.000000000000000000, -0.000000000000000000 ) ) ;
#154879 = CARTESIAN_POINT ( 'NONE',  ( 5.899999999999995914, -11.65000000000000036, 10.10000000000000142 ) ) ;
#154880 = ORIENTED_EDGE ( 'NONE', *, *, #98015, .T. ) ;
#154881 = CARTESIAN_POINT ( 'NONE',  ( 20.94999999999999929, 1.115600667400684642E-11, -134.0000000000000000 ) ) ;
#154882 = CARTESIAN_POINT ( 'NONE',  ( -16.89081410710458542, 66.04868147016469493, -82.16870156468802122 ) ) ;
#154883 = LINE ( 'NONE', #16644, #226689 ) ;
#154884 = CARTESIAN_POINT ( 'NONE',  ( 23.24999999999999645, 40.29670989715187090, -235.0462836312595130 ) ) ;
#154885 = B_SPLINE_CURVE_WITH_KNOTS ( 'NONE', 3,
 ( #138554, #139852, #197274, #233840, #173912, #135995, #215548, #18639, #77314, #39524, #36956, #98135, #177744, #120349, #156898, #74806, #116466, #55159, #196007, #17364, #257195, #158197, #57749, #175196, #78601, #134715, #214278, #194736, #237690, #254647 ),
 .UNSPECIFIED., .F., .F.,
 ( 4, 2, 2, 2, 2, 2, 2, 2, 2, 2, 2, 2, 2, 2, 4 ),
 ( 0.000000000000000000, 0.0003422764154113329101, 0.0006845528308226658202, 0.001026829246233998839, 0.001369105661645331640, 0.002053658492468003749, 0.002738211323290675424, 0.003080487738702009093, 0.003422764154113342328, 0.003765040569524676431, 0.004107316984936010100, 0.004449593400347342902, 0.004791869815758676571, 0.005134146231170010240, 0.005476422646581343909 ),
 .UNSPECIFIED. ) ;
#154886 = VECTOR ( 'NONE', #119327, 1000.000000000000000 ) ;
#154887 = AXIS2_PLACEMENT_3D ( 'NONE', #108052, #247556, #148465 ) ;
#154888 = DIRECTION ( 'NONE',  ( 0.000000000000000000, 6.982962677686266711E-15, -1.000000000000000000 ) ) ;
#154889 = AXIS2_PLACEMENT_3D ( 'NONE', #25653, #184712, #119629 ) ;
#154890 = EDGE_CURVE ( 'NONE', #104833, #95993, #484, .T. ) ;
#154891 = VECTOR ( 'NONE', #18184, 1000.000000000000000 ) ;
#154892 = EDGE_CURVE ( 'NONE', #164555, #75163, #43547, .T. ) ;
#154893 = VERTEX_POINT ( 'NONE', #198749 ) ;
#154894 = ORIENTED_EDGE ( 'NONE', *, *, #139169, .F. ) ;
#154895 = DIRECTION ( 'NONE',  ( 0.000000000000000000, -0.9126074666063769270, -0.4088369013363280513 ) ) ;
#154896 = CARTESIAN_POINT ( 'NONE',  ( -21.10000000000000142, 6.322468214605803993, 12.11686199900910488 ) ) ;
#154897 = DIRECTION ( 'NONE',  ( 1.000000000000000000, -1.207181226542539700E-16, 2.694675058168174199E-16 ) ) ;
#154898 = CARTESIAN_POINT ( 'NONE',  ( -18.59999999999999787, 15.90518444080775851, -219.2841490888777116 ) ) ;
#154899 = EDGE_LOOP ( 'NONE', ( #219756, #55430, #58465, #110782 ) ) ;
#154900 = LINE ( 'NONE', #210998, #92995 ) ;
#154901 = DIRECTION ( 'NONE',  ( 0.000000000000000000, 1.000000000000000000, 0.000000000000000000 ) ) ;
#154902 = ORIENTED_EDGE ( 'NONE', *, *, #171016, .T. ) ;
#154903 = FACE_OUTER_BOUND ( 'NONE', #67235, .T. ) ;
#154904 = EDGE_CURVE ( 'NONE', #212207, #100678, #127884, .T. ) ;
#154905 = DIRECTION ( 'NONE',  ( 0.000000000000000000, 0.000000000000000000, -1.000000000000000000 ) ) ;
#154906 = EDGE_CURVE ( 'NONE', #242104, #148843, #46281, .T. ) ;
#154907 = AXIS2_PLACEMENT_3D ( 'NONE', #26197, #207407, #109554 ) ;
#154908 = VERTEX_POINT ( 'NONE', #210327 ) ;
#154909 = CARTESIAN_POINT ( 'NONE',  ( -18.38639463286148867, 64.51980042617665845, -194.2731074845244450 ) ) ;
#154910 = ORIENTED_EDGE ( 'NONE', *, *, #254176, .F. ) ;
#154911 = DIRECTION ( 'NONE',  ( 0.000000000000000000, 0.8814952561688446098, -0.4721928772777316263 ) ) ;
#154912 = CARTESIAN_POINT ( 'NONE',  ( 23.24999999999999645, 7.525330762710603416, -212.0571253909869256 ) ) ;
#154913 = DIRECTION ( 'NONE',  ( 1.000000000000000000, 0.000000000000000000, 0.000000000000000000 ) ) ;
#154914 = EDGE_CURVE ( 'NONE', #14603, #194502, #33878, .T. ) ;
#154915 = CARTESIAN_POINT ( 'NONE',  ( 21.78635804494511419, 75.90099493450475165, -177.0587689696775442 ) ) ;
#154916 = DIRECTION ( 'NONE',  ( 1.000000000000000000, -7.304098846218134667E-16, -0.000000000000000000 ) ) ;
#154917 = DIRECTION ( 'NONE',  ( 1.000000000000000000, -0.000000000000000000, 0.000000000000000000 ) ) ;
#154918 = DIRECTION ( 'NONE',  ( 0.000000000000000000, 0.07893460099012303277, -0.9968797965484756940 ) ) ;
#154919 = DIRECTION ( 'NONE',  ( 0.000000000000000000, -1.000000000000000000, 0.000000000000000000 ) ) ;
#154920 = EDGE_CURVE ( 'NONE', #695, #148919, #87774, .T. ) ;
#154922 = LINE ( 'NONE', #118343, #20683 ) ;
#154921 = CARTESIAN_POINT ( 'NONE',  ( 18.57071067811864040, 10.17928932189250091, -155.2500000000000284 ) ) ;
#154923 = DIRECTION ( 'NONE',  ( -0.000000000000000000, 1.000000000000000000, 6.352154140967427193E-15 ) ) ;
#154924 = DIRECTION ( 'NONE',  ( 0.000000000000000000, -7.056502275159890832E-15, 1.000000000000000000 ) ) ;
#154925 = DIRECTION ( 'NONE',  ( -1.000000000000000000, 0.000000000000000000, 0.000000000000000000 ) ) ;
#154926 = DIRECTION ( 'NONE',  ( 0.000000000000000000, -0.9770955615653315052, -0.2128009952263605897 ) ) ;
#154927 = ADVANCED_FACE ( 'NONE', ( #26558 ), #186481, .T. ) ;
#154928 = ORIENTED_EDGE ( 'NONE', *, *, #112760, .F. ) ;
#154929 = CARTESIAN_POINT ( 'NONE',  ( 21.05000012384952868, 10.62872029888669978, -79.17797733003580163 ) ) ;
#154930 = CARTESIAN_POINT ( 'NONE',  ( -21.05000000000000071, 18.62343931468261360, -223.9512205031617498 ) ) ;
#154931 = CIRCLE ( 'NONE', #175768, 0.1000000000000000472 ) ;
#154932 = ORIENTED_EDGE ( 'NONE', *, *, #101087, .T. ) ;
#154933 = CARTESIAN_POINT ( 'NONE',  ( -20.94999999999999929, 5.850000000011108092, -177.6324972242779268 ) ) ;
#154934 = DIRECTION ( 'NONE',  ( 1.000000000000000000, 0.000000000000000000, 0.000000000000000000 ) ) ;
#154935 = CARTESIAN_POINT ( 'NONE',  ( -20.64999999999999858, 71.75000000001223555, -148.8731074845244109 ) ) ;
#154936 = EDGE_CURVE ( 'NONE', #189647, #172354, #79601, .T. ) ;
#154937 =( BOUNDED_CURVE ( )  B_SPLINE_CURVE ( 3, ( #132394, #71156, #112830, #131104 ),
 .UNSPECIFIED., .F., .F. ) 
 B_SPLINE_CURVE_WITH_KNOTS ( ( 4, 4 ),
 ( 3.192897208853993085, 4.712388980384689674 ),
 .UNSPECIFIED. ) 
 CURVE ( )  GEOMETRIC_REPRESENTATION_ITEM ( )  RATIONAL_B_SPLINE_CURVE ( ( 1.000000000000000000, 0.8166740347213228279, 0.8166740347213228279, 1.000000000000000000 ) ) 
 REPRESENTATION_ITEM ( '' )  );
#154938 = ORIENTED_EDGE ( 'NONE', *, *, #181279, .F. ) ;
#154939 = CYLINDRICAL_SURFACE ( 'NONE', #163697, 0.1000000000000028644 ) ;
#154940 = EDGE_CURVE ( 'NONE', #189515, #102738, #63034, .T. ) ;
#154941 = EDGE_LOOP ( 'NONE', ( #253367, #211650, #167957, #86330 ) ) ;
#154942 = CARTESIAN_POINT ( 'NONE',  ( -23.15000000000000213, -11.64999999998884483, -97.40000000000004832 ) ) ;
#154943 = DIRECTION ( 'NONE',  ( -1.000000000000000000, 0.000000000000000000, 0.000000000000000000 ) ) ;
#154944 = AXIS2_PLACEMENT_3D ( 'NONE', #172207, #52188, #148753 ) ;
#154945 = VECTOR ( 'NONE', #7049, 1000.000000000000000 ) ;
#154946 = ORIENTED_EDGE ( 'NONE', *, *, #175517, .T. ) ;
#154947 = CARTESIAN_POINT ( 'NONE',  ( 21.05000000000000071, 67.22371710472020823, -203.5231074845244166 ) ) ;
#154948 = EDGE_CURVE ( 'NONE', #32589, #104317, #25465, .T. ) ;
#154949 = VERTEX_POINT ( 'NONE', #48661 ) ;
#154950 = PLANE ( 'NONE',  #208257 ) ;
#154951 = CYLINDRICAL_SURFACE ( 'NONE', #95305, 0.1000000000000124678 ) ;
#154953 = CARTESIAN_POINT ( 'NONE',  ( 21.13736287352038445, 8.046642376395153562, -109.7500000000000426 ) ) ;
#154952 = PRODUCT_DEFINITION_CONTEXT ( 'detailed design', #202408, 'design' ) ;
#154954 = CARTESIAN_POINT ( 'NONE',  ( -17.01825945287481545, 30.11817903451004952, -234.7598257170722889 ) ) ;
#154955 = DIRECTION ( 'NONE',  ( 0.000000000000000000, 0.000000000000000000, -1.000000000000000000 ) ) ;
#154956 = CARTESIAN_POINT ( 'NONE',  ( -21.14999999999999858, 64.25000000001190870, -96.23924182154622997 ) ) ;
#154957 = VECTOR ( 'NONE', #132607, 1000.000000000000000 ) ;
#154958 = CARTESIAN_POINT ( 'NONE',  ( 18.49999999999998934, 10.25000000001115552, -58.15000000000000568 ) ) ;
#154959 = CARTESIAN_POINT ( 'NONE',  ( -21.05000000000000071, 13.71992543034163958, -238.5823796952984992 ) ) ;
#154961 = ORIENTED_EDGE ( 'NONE', *, *, #188775, .F. ) ;
#154960 = CARTESIAN_POINT ( 'NONE',  ( 18.50000000000000355, -0.5913595841389387431, -242.4574432119242999 ) ) ;
#154962 = VERTEX_POINT ( 'NONE', #65659 ) ;
#154964 = CYLINDRICAL_SURFACE ( 'NONE', #43648, 0.1000000000000008105 ) ;
#154963 = DIRECTION ( 'NONE',  ( -1.000000000000000000, 0.000000000000000000, 0.000000000000000000 ) ) ;
#154965 = VERTEX_POINT ( 'NONE', #169952 ) ;
#154967 = VERTEX_POINT ( 'NONE', #185616 ) ;
#154966 = CARTESIAN_POINT ( 'NONE',  ( -20.54999999999999716, 85.00000000001197975, -112.9170766071766820 ) ) ;
#154968 = ORIENTED_EDGE ( 'NONE', *, *, #43702, .F. ) ;
#154969 = DIRECTION ( 'NONE',  ( 0.000000000000000000, 0.8814952561688429444, -0.4721928772777345684 ) ) ;
#154970 = CARTESIAN_POINT ( 'NONE',  ( -20.54999999999999716, -6.688413578037177842, -212.5825622730469036 ) ) ;
#154971 = DIRECTION ( 'NONE',  ( 1.000000000000000000, 7.304098846218133681E-16, -4.607487905232622991E-31 ) ) ;
#154972 = DIRECTION ( 'NONE',  ( 0.000000000000000000, 0.8814952561688444987, -0.4721928772777320149 ) ) ;
#154973 = CYLINDRICAL_SURFACE ( 'NONE', #52510, 0.09999999999998898659 ) ;
#154974 = DIRECTION ( 'NONE',  ( 0.000000000000000000, 0.9126074666063844765, 0.4088369013363114535 ) ) ;
#154975 = CARTESIAN_POINT ( 'NONE',  ( -21.05000000000000071, 75.90220970870321082, -109.2809220950004203 ) ) ;
#154976 = AXIS2_PLACEMENT_3D ( 'NONE', #27357, #143403, #164269 ) ;
#154977 = VECTOR ( 'NONE', #64442, 1000.000000000000000 ) ;
#154979 = AXIS2_PLACEMENT_3D ( 'NONE', #4438, #576, #64433 ) ;
#154978 = LINE ( 'NONE', #79237, #185280 ) ;
#154980 = EDGE_LOOP ( 'NONE', ( #165788, #158376, #241809, #209177 ) ) ;
#154981 = ORIENTED_EDGE ( 'NONE', *, *, #190710, .F. ) ;
#154982 = DIRECTION ( 'NONE',  ( -0.000000000000000000, -6.982962677686266711E-15, 1.000000000000000000 ) ) ;
#154983 = EDGE_LOOP ( 'NONE', ( #28419, #2427, #109465, #121891 ) ) ;
#154984 = CARTESIAN_POINT ( 'NONE',  ( 20.95392731769792150, 8.883061479199918509, -142.5222279795713121 ) ) ;
#154985 = ORIENTED_EDGE ( 'NONE', *, *, #57035, .F. ) ;
#154986 = CARTESIAN_POINT ( 'NONE',  ( 18.48413544395645047, -9.664304033627754364, -40.18310499303830596 ) ) ;
#154987 = CARTESIAN_POINT ( 'NONE',  ( -20.94999999999999929, 11.60000000001115517, -60.07179676972450011 ) ) ;
#154988 = DIRECTION ( 'NONE',  ( 0.000000000000000000, 0.4930308989874729320, 0.8700118002898605818 ) ) ;
#154989 = EDGE_CURVE ( 'NONE', #81393, #221732, #207769, .T. ) ;
#154991 = VERTEX_POINT ( 'NONE', #125638 ) ;
#154990 = CARTESIAN_POINT ( 'NONE',  ( 18.52351027002948314, -9.642162904684017377, -207.7150469505097021 ) ) ;
#154992 = DIRECTION ( 'NONE',  ( 1.000000000000000000, 0.000000000000000000, 0.000000000000000000 ) ) ;
#154993 = ORIENTED_EDGE ( 'NONE', *, *, #131688, .T. ) ;
#154994 = CARTESIAN_POINT ( 'NONE',  ( 20.85000000000000142, -1.149570369564537842, -141.8159124845019790 ) ) ;
#154995 = AXIS2_PLACEMENT_3D ( 'NONE', #51572, #172891, #249817 ) ;
#154996 = ADVANCED_FACE ( 'NONE', ( #29156 ), #146467, .T. ) ;
#154997 = DIRECTION ( 'NONE',  ( -0.000000000000000000, -6.982962677686266711E-15, 1.000000000000000000 ) ) ;
#154998 = ADVANCED_FACE ( 'NONE', ( #107351, #108643, #9534 ), #168673, .F. ) ;
#154999 = DIRECTION ( 'NONE',  ( 0.000000000000000000, -0.9910827722268055195, 0.1332476588733540468 ) ) ;
#155000 = DIRECTION ( 'NONE',  ( 0.000000000000000000, -0.2128009952263602289, 0.9770955615653315052 ) ) ;
#155001 = ORIENTED_EDGE ( 'NONE', *, *, #44968, .T. ) ;
#155003 = CARTESIAN_POINT ( 'NONE',  ( -23.15000000000000213, -11.64999999998884483, -88.75000000000004263 ) ) ;
#155002 = CARTESIAN_POINT ( 'NONE',  ( -17.05016517655894148, 60.94529903456965059, -221.0198211075746713 ) ) ;
#155005 = ORIENTED_EDGE ( 'NONE', *, *, #29941, .F. ) ;
#155004 = B_SPLINE_CURVE_WITH_KNOTS ( 'NONE', 3,
 ( #113745, #15974, #109887, #172498, #10808, #228579, #52476, #69515 ),
 .UNSPECIFIED., .F., .F.,
 ( 4, 2, 2, 4 ),
 ( 0.000000000000000000, 6.534141206309662642E-05, 0.0001306828241261932528, 0.0002613656482524241275 ),
 .UNSPECIFIED. ) ;
#155008 = ORIENTED_EDGE ( 'NONE', *, *, #189412, .F. ) ;
#155007 = DIRECTION ( 'NONE',  ( 1.000000000000000000, 0.000000000000000000, 0.000000000000000000 ) ) ;
#155006 = CARTESIAN_POINT ( 'NONE',  ( -20.64999999999999858, 85.00000000001159606, -59.62913836187181715 ) ) ;
#155010 = B_SPLINE_CURVE_WITH_KNOTS ( 'NONE', 3,
 ( #64840, #223904, #124834, #247330, #66132, #128690, #109097, #70012, #146934, #149549 ),
 .UNSPECIFIED., .F., .F.,
 ( 4, 2, 2, 2, 4 ),
 ( 5.259846352425386116E-16, 9.930191194500792909E-05, 0.0001986038238894898575, 0.0003972076477784336566, 0.0007944152955563403909 ),
 .UNSPECIFIED. ) ;
#155009 = TOROIDAL_SURFACE ( 'NONE', #130006, 12.77500000000000036, 0.1000000000000000056 ) ;
#155011 = DIRECTION ( 'NONE',  ( 2.952720810173289112E-16, 0.9651348961777146407, -0.2617529984165072321 ) ) ;
#155012 = CARTESIAN_POINT ( 'NONE',  ( 21.05000000000000071, 76.10000000001194564, -103.0231074845243171 ) ) ;
#155013 = ORIENTED_EDGE ( 'NONE', *, *, #229771, .F. ) ;
#155014 = DIRECTION ( 'NONE',  ( -1.000000000000000000, 0.000000000000000000, 0.000000000000000000 ) ) ;
#155015 = ADVANCED_FACE ( 'NONE', ( #38111 ), #71506, .T. ) ;
#155016 = AXIS2_PLACEMENT_3D ( 'NONE', #6541, #83481, #44405 ) ;
#155017 = DIRECTION ( 'NONE',  ( 1.000000000000000000, 0.000000000000000000, 0.000000000000000000 ) ) ;
#155018 = DIRECTION ( 'NONE',  ( 0.000000000000000000, 0.000000000000000000, -1.000000000000000000 ) ) ;
#155020 = VERTEX_POINT ( 'NONE', #36847 ) ;
#155019 = FACE_OUTER_BOUND ( 'NONE', #15277, .T. ) ;
#155021 = VECTOR ( 'NONE', #192991, 1000.000000000000000 ) ;
#155022 = LINE ( 'NONE', #135414, #18493 ) ;
#155023 = VECTOR ( 'NONE', #112337, 1000.000000000000000 ) ;
#155024 = ORIENTED_EDGE ( 'NONE', *, *, #55192, .F. ) ;
#155025 = AXIS2_PLACEMENT_3D ( 'NONE', #117353, #258091, #216439 ) ;
#155026 = AXIS2_PLACEMENT_3D ( 'NONE', #4289, #205049, #26452 ) ;
#155027 = DIRECTION ( 'NONE',  ( 0.000000000000000000, 1.000000000000000000, 0.000000000000000000 ) ) ;
#155028 = DIRECTION ( 'NONE',  ( -1.000000000000000000, -0.000000000000000000, -0.000000000000000000 ) ) ;
#155029 = DIRECTION ( 'NONE',  ( -0.000000000000000000, 0.2599159095383575813, -0.9656312546561697241 ) ) ;
#155030 = CARTESIAN_POINT ( 'NONE',  ( -16.86757978335472075, 66.03434962097800565, -157.4251028313569236 ) ) ;
#155032 = ORIENTED_EDGE ( 'NONE', *, *, #123537, .T. ) ;
#155031 = VECTOR ( 'NONE', #207147, 1000.000000000000000 ) ;
#155033 = LINE ( 'NONE', #53336, #222628 ) ;
#155034 = EDGE_CURVE ( 'NONE', #205485, #255544, #236289, .T. ) ;
#155035 = DIRECTION ( 'NONE',  ( 0.000000000000000000, -0.9770955615653320603, -0.2128009952263585081 ) ) ;
#155036 = CARTESIAN_POINT ( 'NONE',  ( -17.04295772865462766, 10.02489942527107303, -46.14999999999999858 ) ) ;
#155037 = EDGE_CURVE ( 'NONE', #33291, #238448, #255810, .T. ) ;
#155038 = VERTEX_POINT ( 'NONE', #190785 ) ;
#155039 = DIRECTION ( 'NONE',  ( -1.000000000000000000, 0.000000000000000000, -0.000000000000000000 ) ) ;
#155040 = B_SPLINE_CURVE_WITH_KNOTS ( 'NONE', 3,
 ( #30857, #12572, #131201, #189903 ),
 .UNSPECIFIED., .F., .F.,
 ( 4, 4 ),
 ( 0.000000000000000000, 7.713889350930169559E-05 ),
 .UNSPECIFIED. ) ;
#155041 = AXIS2_PLACEMENT_3D ( 'NONE', #141647, #242029, #221172 ) ;
#155042 = CARTESIAN_POINT ( 'NONE',  ( 20.95512820512820440, 52.42293488718664207, -232.7629365818759481 ) ) ;
#155043 = VECTOR ( 'NONE', #221835, 1000.000000000000000 ) ;
#155045 = EDGE_CURVE ( 'NONE', #203005, #75879, #4585, .T. ) ;
#155044 = ORIENTED_EDGE ( 'NONE', *, *, #80581, .F. ) ;
#155046 = CIRCLE ( 'NONE', #13554, 0.09999999999999986677 ) ;
#155047 = CIRCLE ( 'NONE', #109209, 0.09999999999999939493 ) ;
#155048 = CARTESIAN_POINT ( 'NONE',  ( 21.05000000000000071, 82.09643798151613225, -215.4278993322501208 ) ) ;
#155049 = CARTESIAN_POINT ( 'NONE',  ( -23.25000000000000000, 1.115600667400684642E-11, -67.00000000000000000 ) ) ;
#155051 = FACE_OUTER_BOUND ( 'NONE', #257773, .T. ) ;
#155050 = AXIS2_PLACEMENT_3D ( 'NONE', #238037, #135073, #257546 ) ;
#155052 = ORIENTED_EDGE ( 'NONE', *, *, #206142, .T. ) ;
#155053 = ORIENTED_EDGE ( 'NONE', *, *, #91503, .F. ) ;
#155054 = AXIS2_PLACEMENT_3D ( 'NONE', #209374, #13747, #251056 ) ;
#155055 = CARTESIAN_POINT ( 'NONE',  ( -21.05000000000000071, 77.26178616857734482, -161.9366085209788650 ) ) ;
#155056 = VERTEX_POINT ( 'NONE', #137190 ) ;
#155058 = ORIENTED_EDGE ( 'NONE', *, *, #255004, .T. ) ;
#155057 = DIRECTION ( 'NONE',  ( 1.000000000000000000, 0.000000000000000000, 0.000000000000000000 ) ) ;
#155059 = AXIS2_PLACEMENT_3D ( 'NONE', #83086, #81806, #80529 ) ;
#155063 = EDGE_CURVE ( 'NONE', #184107, #2240, #250307, .T. ) ;
#155062 = ORIENTED_EDGE ( 'NONE', *, *, #218642, .F. ) ;
#155061 = ORIENTED_EDGE ( 'NONE', *, *, #5973, .T. ) ;
#155060 = CARTESIAN_POINT ( 'NONE',  ( -21.08884785362073089, 0.04978309506672475016, 6.357193367425618469 ) ) ;
#155064 = CARTESIAN_POINT ( 'NONE',  ( 20.94999999999999929, 87.65000000001214175, -136.5231074845242745 ) ) ;
#155065 = CARTESIAN_POINT ( 'NONE',  ( -16.84981964351492678, 12.42883166081041502, -211.4644154259821676 ) ) ;
#155066 = CARTESIAN_POINT ( 'NONE',  ( -21.05000000000000071, -1.835341550213255957, -112.0551512925630107 ) ) ;
#155067 = CIRCLE ( 'NONE', #230049, 0.09999999999999939493 ) ;
#155068 = CARTESIAN_POINT ( 'NONE',  ( 20.95429693346638800, 65.45669512011706104, -195.9622249462115064 ) ) ;
#155069 = VECTOR ( 'NONE', #210424, 1000.000000000000000 ) ;
#155070 = DIRECTION ( 'NONE',  ( 0.000000000000000000, -0.1350103645451876666, -0.9908441862701600211 ) ) ;
#155072 = CARTESIAN_POINT ( 'NONE',  ( -22.39999999999999858, 25.97741635855165399, -254.4468634167653249 ) ) ;
#155071 = TOROIDAL_SURFACE ( 'NONE', #225755, 0.2000000000000000111, 0.1000000000000000056 ) ;
#155073 = ORIENTED_EDGE ( 'NONE', *, *, #175938, .F. ) ;
#155074 = EDGE_LOOP ( 'NONE', ( #116525, #187813, #150929, #58238 ) ) ;
#155075 = ORIENTED_EDGE ( 'NONE', *, *, #251254, .F. ) ;
#155076 = ADVANCED_FACE ( 'NONE', ( #77208 ), #208810, .F. ) ;
#155077 = CARTESIAN_POINT ( 'NONE',  ( -21.05000000000000071, 74.25000000001156764, -57.85359592662268824 ) ) ;
#155079 = ORIENTED_EDGE ( 'NONE', *, *, #68831, .T. ) ;
#155078 = CARTESIAN_POINT ( 'NONE',  ( 23.40000000000005542, 87.50449464844290048, -37.85861909827351468 ) ) ;
#155080 = DIRECTION ( 'NONE',  ( 1.000000000000000000, 7.166229603267616255E-16, 4.447280054184918885E-16 ) ) ;
#155081 = ORIENTED_EDGE ( 'NONE', *, *, #238215, .F. ) ;
#155082 = CARTESIAN_POINT ( 'NONE',  ( 23.40000000000005542, 64.35000000001120668, -3.123107484524795474 ) ) ;
#155083 = ORIENTED_EDGE ( 'NONE', *, *, #78011, .F. ) ;
#155084 = DIRECTION ( 'NONE',  ( 2.694716079187273439E-16, -0.9770955615653316162, -0.2128009952263598958 ) ) ;
#155085 = EDGE_CURVE ( 'NONE', #253877, #105957, #171254, .T. ) ;
#155086 = EDGE_CURVE ( 'NONE', #104231, #119881, #171237, .T. ) ;
#155087 = VERTEX_POINT ( 'NONE', #133352 ) ;
#155088 = CARTESIAN_POINT ( 'NONE',  ( -20.54999999999999716, 2.500000000000000444, -13.22462192276210224 ) ) ;
#155089 = DIRECTION ( 'NONE',  ( -1.000000000000000000, -0.000000000000000000, 0.000000000000000000 ) ) ;
#155090 = EDGE_CURVE ( 'NONE', #248567, #110678, #242102, .T. ) ;
#155092 = EDGE_LOOP ( 'NONE', ( #139493, #110481, #70972, #216291 ) ) ;
#155091 = ORIENTED_EDGE ( 'NONE', *, *, #48882, .T. ) ;
#155093 = EDGE_LOOP ( 'NONE', ( #18741, #934, #165073, #9796 ) ) ;
#155095 = EDGE_CURVE ( 'NONE', #51335, #235216, #8892, .T. ) ;
#155094 = DIRECTION ( 'NONE',  ( 1.000000000000000000, -7.304098846218134667E-16, 4.607487905232622991E-31 ) ) ;
#155096 = ORIENTED_EDGE ( 'NONE', *, *, #41161, .F. ) ;
#155097 = EDGE_LOOP ( 'NONE', ( #211195, #221022, #137770, #141114 ) ) ;
#155098 = LINE ( 'NONE', #234595, #5495 ) ;
#155100 = ORIENTED_EDGE ( 'NONE', *, *, #46227, .T. ) ;
#155099 = CARTESIAN_POINT ( 'NONE',  ( 18.44206774312972641, -9.491027357528919239, -107.1262275046983206 ) ) ;
#155101 = LINE ( 'NONE', #82860, #123254 ) ;
#155102 = ADVANCED_FACE ( 'NONE', ( #72102 ), #196316, .F. ) ;
#155104 = DIRECTION ( 'NONE',  ( 0.000000000000000000, 0.000000000000000000, -1.000000000000000000 ) ) ;
#155103 = CARTESIAN_POINT ( 'NONE',  ( -21.44999999999999929, 68.65000000001150227, -48.37310748452437537 ) ) ;
#155105 = DIRECTION ( 'NONE',  ( -0.7071067811865463515, -0.7071067811865487940, -4.937700262164540154E-15 ) ) ;
#155106 = DIRECTION ( 'NONE',  ( 0.000000000000000000, 0.000000000000000000, 1.000000000000000000 ) ) ;
#155107 = DIRECTION ( 'NONE',  ( 1.158076286952576634E-15, -0.1335171055202867274, -0.9910465087640865089 ) ) ;
#155108 = ORIENTED_EDGE ( 'NONE', *, *, #219278, .T. ) ;
#155109 = ORIENTED_EDGE ( 'NONE', *, *, #18514, .F. ) ;
#155110 = CARTESIAN_POINT ( 'NONE',  ( -2.995603634470829482E-16, 53.24180694658302571, -234.8354225850497130 ) ) ;
#155111 = CARTESIAN_POINT ( 'NONE',  ( 0.9000000000000554223, 63.75000000001118394, -10.02310748452479139 ) ) ;
#155113 = ADVANCED_FACE ( 'NONE', ( #112511 ), #58748, .F. ) ;
#155112 = CARTESIAN_POINT ( 'NONE',  ( 18.59999999999999787, 77.36242903720570041, -162.1342262366031548 ) ) ;
#155114 = VERTEX_POINT ( 'NONE', #113772 ) ;
#155116 = B_SPLINE_CURVE_WITH_KNOTS ( 'NONE', 3,
 ( #187620, #29841, #50635, #130179, #171931, #88472, #27282, #168084 ),
 .UNSPECIFIED., .F., .F.,
 ( 4, 2, 2, 4 ),
 ( 0.000000000000000000, 0.0001881495939909207983, 0.0002822243909863812110, 0.0003762991879818415966 ),
 .UNSPECIFIED. ) ;
#155115 = CARTESIAN_POINT ( 'NONE',  ( 22.94999999999999929, 0.000000000000000000, 0.000000000000000000 ) ) ;
#155117 = EDGE_CURVE ( 'NONE', #83513, #45115, #146250, .T. ) ;
#155118 = EDGE_CURVE ( 'NONE', #156798, #127092, #87962, .T. ) ;
#155119 = AXIS2_PLACEMENT_3D ( 'NONE', #192397, #93284, #153306 ) ;
#155120 = LINE ( 'NONE', #234617, #217821 ) ;
#155121 = DIRECTION ( 'NONE',  ( 1.000000000000000000, -0.000000000000000000, -0.000000000000000000 ) ) ;
#155122 = EDGE_LOOP ( 'NONE', ( #156481, #124142, #63810, #249093, #73066 ) ) ;
#155123 = ORIENTED_EDGE ( 'NONE', *, *, #26669, .F. ) ;
#155124 = EDGE_CURVE ( 'NONE', #63728, #13549, #18536, .T. ) ;
#155125 = FACE_OUTER_BOUND ( 'NONE', #111383, .T. ) ;
#155126 = LINE ( 'NONE', #221450, #160755 ) ;
#155127 = ORIENTED_EDGE ( 'NONE', *, *, #214473, .F. ) ;
#155128 = DIRECTION ( 'NONE',  ( 0.000000000000000000, 0.000000000000000000, -1.000000000000000000 ) ) ;
#155129 = VERTEX_POINT ( 'NONE', #22406 ) ;
#155130 = DIRECTION ( 'NONE',  ( 0.000000000000000000, -7.487053152578134969E-15, 1.000000000000000000 ) ) ;
#155131 = CARTESIAN_POINT ( 'NONE',  ( -17.29158576265544056, 10.36474766602906783, -145.4172417552078400 ) ) ;
#155133 = CARTESIAN_POINT ( 'NONE',  ( -17.22361732159831860, 65.65484434140907410, -47.39389201039153221 ) ) ;
#155132 = DIRECTION ( 'NONE',  ( 1.000000000000000000, -0.000000000000000000, -0.000000000000000000 ) ) ;
#155134 = EDGE_CURVE ( 'NONE', #166775, #39025, #40706, .T. ) ;
#155136 = ADVANCED_FACE ( 'NONE', ( #160641 ), #62796, .T. ) ;
#155135 = CARTESIAN_POINT ( 'NONE',  ( -23.15000000000000213, 76.00000000001270450, -207.6731074845243370 ) ) ;
#155137 = LINE ( 'NONE', #234634, #224486 ) ;
#155138 = EDGE_CURVE ( 'NONE', #128766, #86886, #82323, .T. ) ;
#155139 = AXIS2_PLACEMENT_3D ( 'NONE', #126291, #27240, #166751 ) ;
#155140 = LINE ( 'NONE', #54713, #135803 ) ;
#155141 = AXIS2_PLACEMENT_3D ( 'NONE', #182852, #162002, #241515 ) ;
#155143 = ORIENTED_EDGE ( 'NONE', *, *, #55570, .T. ) ;
#155142 = ORIENTED_EDGE ( 'NONE', *, *, #120706, .T. ) ;
#155144 = ORIENTED_EDGE ( 'NONE', *, *, #71112, .F. ) ;
#155145 = AXIS2_PLACEMENT_3D ( 'NONE', #203218, #44161, #220235 ) ;
#155146 = DIRECTION ( 'NONE',  ( 0.000000000000000000, 0.2617529984165027912, 0.9651348961777157509 ) ) ;
#155147 = CARTESIAN_POINT ( 'NONE',  ( -23.25000000000000000, -8.596261682242989366, -24.04987248284972168 ) ) ;
#155148 = FACE_OUTER_BOUND ( 'NONE', #70712, .T. ) ;
#155149 = DIRECTION ( 'NONE',  ( -1.000000000000000000, 0.000000000000000000, 0.000000000000000000 ) ) ;
#155150 = EDGE_CURVE ( 'NONE', #129552, #238489, #17440, .T. ) ;
#155152 = CARTESIAN_POINT ( 'NONE',  ( -15.74999999999999645, 66.65000000001187175, -86.50158811269930936 ) ) ;
#155151 = DIRECTION ( 'NONE',  ( 0.000000000000000000, -1.000000000000000000, -6.982962677686266711E-15 ) ) ;
#155153 = CARTESIAN_POINT ( 'NONE',  ( 15.74999999999999645, 26.30888228346803714, -233.3999513616626587 ) ) ;
#155154 = EDGE_LOOP ( 'NONE', ( #76180, #246440, #96782, #42355 ) ) ;
#155155 = CARTESIAN_POINT ( 'NONE',  ( 20.46382478191414833, 10.59862044130854031, -74.67781446934550615 ) ) ;
#155156 = VERTEX_POINT ( 'NONE', #61517 ) ;
#155157 = ORIENTED_EDGE ( 'NONE', *, *, #201218, .F. ) ;
#155158 = CARTESIAN_POINT ( 'NONE',  ( -11.59999999999994458, 64.35000000001120668, -23.62310748452479103 ) ) ;
#155160 = AXIS2_PLACEMENT_3D ( 'NONE', #1750, #239103, #42192 ) ;
#155159 = DIRECTION ( 'NONE',  ( 1.000000000000000000, 0.000000000000000000, 0.000000000000000000 ) ) ;
#155161 = CIRCLE ( 'NONE', #217636, 0.1999999999999945155 ) ;
#155162 = CARTESIAN_POINT ( 'NONE',  ( 21.07016717457012689, 76.00000000001273293, -209.8440483226252979 ) ) ;
#155163 = DIRECTION ( 'NONE',  ( 0.000000000000000000, 0.3565161741896938907, -0.9342891509276685102 ) ) ;
#155164 = CARTESIAN_POINT ( 'NONE',  ( -21.04999999999994387, 83.80000000001119531, -37.18565239344504647 ) ) ;
#155165 = ORIENTED_EDGE ( 'NONE', *, *, #53357, .F. ) ;
#155166 = ORIENTED_EDGE ( 'NONE', *, *, #188771, .T. ) ;
#155167 = DIRECTION ( 'NONE',  ( -1.000000000000000000, 0.000000000000000000, 0.000000000000000000 ) ) ;
#155168 = AXIS2_PLACEMENT_3D ( 'NONE', #165552, #207251, #222932 ) ;
#155169 = DIRECTION ( 'NONE',  ( 0.000000000000000000, 0.000000000000000000, 1.000000000000000000 ) ) ;
#155170 = CARTESIAN_POINT ( 'NONE',  ( -20.64999999999999858, 7.150000000011155876, -155.1500000000000057 ) ) ;
#155171 = CARTESIAN_POINT ( 'NONE',  ( -23.15000000000000213, 76.00000000001168132, -73.67310748452432279 ) ) ;
#155172 = DIRECTION ( 'NONE',  ( -1.000000000000000000, -0.000000000000000000, -0.000000000000000000 ) ) ;
#155173 = CARTESIAN_POINT ( 'NONE',  ( -21.05000000000000071, 13.71992543034163958, -238.5823796952984992 ) ) ;
#155174 = DIRECTION ( 'NONE',  ( 1.000000000000000000, -0.000000000000000000, 0.000000000000000000 ) ) ;
#155175 = AXIS2_PLACEMENT_3D ( 'NONE', #210650, #8604, #32041 ) ;
#155178 = DIRECTION ( 'NONE',  ( 1.000000000000000000, 0.000000000000000000, 0.000000000000000000 ) ) ;
#155177 = AXIS2_PLACEMENT_3D ( 'NONE', #23172, #42708, #243470 ) ;
#155176 = CARTESIAN_POINT ( 'NONE',  ( 23.14999999999998437, 7.128833340093095217, -233.7327013124392749 ) ) ;
#155180 = DIRECTION ( 'NONE',  ( 1.000000000000000000, 0.000000000000000000, 0.000000000000000000 ) ) ;
#155179 = CIRCLE ( 'NONE', #200925, 0.09999999999998898659 ) ;
#155181 = CIRCLE ( 'NONE', #42702, 12.77500000000000924 ) ;
#155182 = DIRECTION ( 'NONE',  ( 1.000000000000000000, 0.000000000000000000, 0.000000000000000000 ) ) ;
#155183 = ADVANCED_FACE ( 'NONE', ( #177639 ), #81049, .T. ) ;
#155184 = FACE_OUTER_BOUND ( 'NONE', #215014, .T. ) ;
#155185 = CARTESIAN_POINT ( 'NONE',  ( 21.12757541349815682, 69.52661942876123646, -203.5282687003341380 ) ) ;
#155187 = ORIENTED_EDGE ( 'NONE', *, *, #176667, .T. ) ;
#155186 = DIRECTION ( 'NONE',  ( -1.000000000000000000, 2.952720810173289112E-16, 2.061873921506763405E-30 ) ) ;
#155188 = EDGE_CURVE ( 'NONE', #57171, #64755, #233923, .T. ) ;
#155189 = CARTESIAN_POINT ( 'NONE',  ( 20.95017935633852346, 10.47548927963648069, -41.07743979739048967 ) ) ;
#155190 = ORIENTED_EDGE ( 'NONE', *, *, #187950, .T. ) ;
#155191 = DIRECTION ( 'NONE',  ( 0.000000000000000000, 0.2128009952263603677, -0.9770955615653313941 ) ) ;
#155192 = EDGE_LOOP ( 'NONE', ( #106524, #170145, #127330, #6233 ) ) ;
#155193 = CARTESIAN_POINT ( 'NONE',  ( 22.49231231312462853, 11.64998490368843953, -100.4389471123986652 ) ) ;
#155194 = EDGE_CURVE ( 'NONE', #221934, #143978, #98098, .T. ) ;
#155195 = CARTESIAN_POINT ( 'NONE',  ( 14.88075390448864965, 9.431689550535256927, -85.27929003223610493 ) ) ;
#155197 = AXIS2_PLACEMENT_3D ( 'NONE', #56460, #132171, #112612 ) ;
#155196 = DIRECTION ( 'NONE',  ( 2.715809747126116508E-16, -1.000000000000000000, 0.000000000000000000 ) ) ;
#155198 = VECTOR ( 'NONE', #254166, 999.9999999999998863 ) ;
#155199 = CARTESIAN_POINT ( 'NONE',  ( -20.65000000000000568, 7.250000000011138646, -121.3500000000000369 ) ) ;
#155200 = CARTESIAN_POINT ( 'NONE',  ( -21.05000000000000071, 77.16270174994961906, -61.62310748452431142 ) ) ;
#155201 = FACE_OUTER_BOUND ( 'NONE', #156413, .T. ) ;
#155202 = EDGE_LOOP ( 'NONE', ( #150919, #92824, #91237, #84555 ) ) ;
#155203 = DIRECTION ( 'NONE',  ( 0.000000000000000000, 0.000000000000000000, -1.000000000000000000 ) ) ;
#155205 = ORIENTED_EDGE ( 'NONE', *, *, #160082, .F. ) ;
#155204 = CARTESIAN_POINT ( 'NONE',  ( -20.64999999999999858, 6.757359537351773859, -220.2789794402637824 ) ) ;
#155206 = DIRECTION ( 'NONE',  ( 0.000000000000000000, 0.000000000000000000, -1.000000000000000000 ) ) ;
#155207 = CIRCLE ( 'NONE', #5293, 4.049999999999994493 ) ;
#155208 = DIRECTION ( 'NONE',  ( -0.000000000000000000, -1.000000000000000000, 0.000000000000000000 ) ) ;
#155209 = CARTESIAN_POINT ( 'NONE',  ( 23.14999999999998437, 76.00000000001213607, -136.5231074845242745 ) ) ;
#155210 = ORIENTED_EDGE ( 'NONE', *, *, #29398, .T. ) ;
#155211 = DIRECTION ( 'NONE',  ( 1.000000000000000000, -0.000000000000000000, -0.000000000000000000 ) ) ;
#155212 = TOROIDAL_SURFACE ( 'NONE', #200966, 0.2000000000000000111, 0.1000000000000000056 ) ;
#155213 = PRODUCT_CONTEXT ( 'NONE', #25723, 'mechanical' ) ;
#155214 = DIRECTION ( 'NONE',  ( 0.000000000000000000, 0.000000000000000000, -1.000000000000000000 ) ) ;
#155216 = AXIS2_PLACEMENT_3D ( 'NONE', #72922, #188989, #70356 ) ;
#155215 = DIRECTION ( 'NONE',  ( -1.000000000000000000, -0.000000000000000000, -0.000000000000000000 ) ) ;
#155217 = ORIENTED_EDGE ( 'NONE', *, *, #247552, .T. ) ;
#155218 = AXIS2_PLACEMENT_3D ( 'NONE', #38956, #2361, #20681 ) ;
#155219 = DIRECTION ( 'NONE',  ( -0.000000000000000000, -0.8814952561688430555, 0.4721928772777344019 ) ) ;
#155220 = CIRCLE ( 'NONE', #213421, 0.4999999999999944489 ) ;
#155221 = AXIS2_PLACEMENT_3D ( 'NONE', #255184, #200408, #21785 ) ;
#155222 = CIRCLE ( 'NONE', #250843, 12.97499999999999964 ) ;
#155223 = DIRECTION ( 'NONE',  ( 1.000000000000000000, 0.000000000000000000, 0.000000000000000000 ) ) ;
#155224 = ORIENTED_EDGE ( 'NONE', *, *, #165580, .T. ) ;
#155225 = ORIENTED_EDGE ( 'NONE', *, *, #51093, .F. ) ;
#155227 = AXIS2_PLACEMENT_3D ( 'NONE', #177919, #16288, #257370 ) ;
#155226 = DIRECTION ( 'NONE',  ( -8.673617379884087537E-15, -1.000000000000000000, 0.000000000000000000 ) ) ;
#155228 = EDGE_CURVE ( 'NONE', #112457, #168131, #213069, .T. ) ;
#155230 = AXIS2_PLACEMENT_3D ( 'NONE', #34611, #8938, #174145 ) ;
#155229 = DIRECTION ( 'NONE',  ( 0.000000000000000000, -1.000000000000000000, -2.891205793294679805E-16 ) ) ;
#155231 = SPHERICAL_SURFACE ( 'NONE', #52580, 0.1000000000000000056 ) ;
#155232 = LINE ( 'NONE', #237307, #28535 ) ;
#155233 = ADVANCED_FACE ( 'NONE', ( #220591 ), #217146, .T. ) ;
#155235 = CARTESIAN_POINT ( 'NONE',  ( -20.64999999999999858, 6.780748427709700543, -212.1627259556213403 ) ) ;
#155234 = CARTESIAN_POINT ( 'NONE',  ( -18.59999999999999787, 11.64999999999999680, -12.14999999999999858 ) ) ;
#155236 = AXIS2_PLACEMENT_3D ( 'NONE', #45007, #60697, #221062 ) ;
#155237 = CARTESIAN_POINT ( 'NONE',  ( 20.92356734117541706, 65.68026841930851845, -30.47257401318895376 ) ) ;
#155238 = FACE_OUTER_BOUND ( 'NONE', #181627, .T. ) ;
#155239 = DIRECTION ( 'NONE',  ( 4.408576920032447355E-17, 0.1350103645451807555, 0.9908441862701610203 ) ) ;
#155240 = DIRECTION ( 'NONE',  ( -0.000000000000000000, 7.272083257015735086E-15, -1.000000000000000000 ) ) ;
#155241 = VERTEX_POINT ( 'NONE', #23702 ) ;
#155242 = VERTEX_POINT ( 'NONE', #242704 ) ;
#155243 = CARTESIAN_POINT ( 'NONE',  ( -18.50000000000000000, 76.00000000001170974, -69.52310748452431710 ) ) ;
#155244 = VECTOR ( 'NONE', #198301, 1000.000000000000000 ) ;
#155245 = CARTESIAN_POINT ( 'NONE',  ( -16.94107738177413225, 65.98576071487563866, -149.0731074845244564 ) ) ;
#155246 = PLANE ( 'NONE',  #133877 ) ;
#155247 = AXIS2_PLACEMENT_3D ( 'NONE', #111267, #112558, #168719 ) ;
#155248 = ADVANCED_FACE ( 'NONE', ( #79758 ), #121512, .T. ) ;
#155249 = DIRECTION ( 'NONE',  ( -1.652117596168391700E-15, -1.000000000000000000, 0.000000000000000000 ) ) ;
#155250 = CARTESIAN_POINT ( 'NONE',  ( 21.30000000000002558, 0.000000000000000000, 4.049999999999998934 ) ) ;
#155251 = DIRECTION ( 'NONE',  ( -0.000000000000000000, 0.4791956752371485107, 0.8777080977375185666 ) ) ;
#155252 = EDGE_CURVE ( 'NONE', #187394, #231082, #219291, .T. ) ;
#155253 = ORIENTED_EDGE ( 'NONE', *, *, #216858, .F. ) ;
#155254 = ADVANCED_FACE ( 'NONE', ( #120240 ), #21129, .F. ) ;
#155255 = ORIENTED_EDGE ( 'NONE', *, *, #193982, .F. ) ;
#155256 = FACE_OUTER_BOUND ( 'NONE', #123156, .T. ) ;
#155257 = ADVANCED_FACE ( 'NONE', ( #64076 ), #117408, .T. ) ;
#155258 = VERTEX_POINT ( 'NONE', #9234 ) ;
#155259 = DIRECTION ( 'NONE',  ( 1.000000000000000000, 0.000000000000000000, 0.000000000000000000 ) ) ;
#155260 = VECTOR ( 'NONE', #35920, 1000.000000000000114 ) ;
#155261 = DIRECTION ( 'NONE',  ( 0.000000000000000000, 0.000000000000000000, 1.000000000000000000 ) ) ;
#155262 = AXIS2_PLACEMENT_3D ( 'NONE', #158701, #180809, #161249 ) ;
#155263 = FACE_OUTER_BOUND ( 'NONE', #240600, .T. ) ;
#155264 = ORIENTED_EDGE ( 'NONE', *, *, #136249, .T. ) ;
#155265 = CARTESIAN_POINT ( 'NONE',  ( 20.99142135623731065, 36.02918351690956200, -236.0543695120160805 ) ) ;
#155266 = EDGE_CURVE ( 'NONE', #250869, #43729, #133959, .T. ) ;
#155267 =( BOUNDED_SURFACE ( )  B_SPLINE_SURFACE ( 3, 2, ( 
 ( #39633, #239087, #450 ),
 ( #119142, #122999, #182974 ),
 ( #142532, #21345, #78699 ),
 ( #1735, #158299, #220798 ),
 ( #60428, #160848, #121722 ),
 ( #180399, #257301, #218204 ) ),
 .UNSPECIFIED., .F., .F., .F. ) 
 B_SPLINE_SURFACE_WITH_KNOTS ( ( 4, 2, 4 ),
 ( 3, 3 ),
 ( 0.0001792624049599534481, 0.0003686986002124527503, 0.0005581347954649519983 ),
 ( 0.000000000000000000, 1.000000000000000000 ),
 .UNSPECIFIED. ) 
 GEOMETRIC_REPRESENTATION_ITEM ( )  RATIONAL_B_SPLINE_SURFACE ( (
 ( 1.000000000000000000, 0.9238795325112854062, 1.000000000000000000),
 ( 1.000000000000000000, 0.9229318695247270554, 1.000000000000000000),
 ( 1.000000000000000000, 0.8926288119218640515, 1.000000000000000000),
 ( 1.000000000000000000, 0.8123777807284088270, 1.000000000000000000),
 ( 1.000000000000000000, 0.7629087100922027354, 1.000000000000000000),
 ( 1.000000000000000000, 0.7071067811865475727, 1.000000000000000000) ) ) 
 REPRESENTATION_ITEM ( '' )  SURFACE ( )  );
#155268 = ORIENTED_EDGE ( 'NONE', *, *, #113023, .T. ) ;
#155269 = B_SPLINE_CURVE_WITH_KNOTS ( 'NONE', 3,
 ( #135822, #34205, #237518, #198378, #177575, #255739, #257019, #77142, #78425, #236218, #54990, #57568, #19763, #134532 ),
 .UNSPECIFIED., .F., .F.,
 ( 4, 2, 2, 2, 2, 2, 4 ),
 ( 0.000000000000000000, 0.0003823333598417659224, 0.0005735000397626485854, 0.0006690833797230926003, 0.0007168750497033104336, 0.0007407708846934199466, 0.0007646667196835293511 ),
 .UNSPECIFIED. ) ;
#155270 = CARTESIAN_POINT ( 'NONE',  ( -21.14999999999999858, 87.65000000001269598, -203.5231074845243029 ) ) ;
#155271 = DIRECTION ( 'NONE',  ( 1.000000000000000000, 0.000000000000000000, 0.000000000000000000 ) ) ;
#155272 = FACE_OUTER_BOUND ( 'NONE', #241256, .T. ) ;
#155273 = FACE_OUTER_BOUND ( 'NONE', #75150, .T. ) ;
#155275 = DIRECTION ( 'NONE',  ( -1.000000000000000000, 0.000000000000000000, 0.000000000000000000 ) ) ;
#155274 = DIRECTION ( 'NONE',  ( 0.000000000000000000, 0.4999999999999608646, 0.8660254037844612451 ) ) ;
#155276 = CARTESIAN_POINT ( 'NONE',  ( -23.15000000000000213, 76.00000000001213607, -136.5231074845243313 ) ) ;
#155277 = EDGE_LOOP ( 'NONE', ( #243097, #198196, #34077, #10649 ) ) ;
#155278 = CIRCLE ( 'NONE', #205099, 0.1000000000000028644 ) ;
#155280 = CARTESIAN_POINT ( 'NONE',  ( 23.24999999999999645, -2.099999999988846344, -134.0000000000000284 ) ) ;
#155279 = CARTESIAN_POINT ( 'NONE',  ( 18.59999999999999076, 14.73746888278883560, -235.8584165281851028 ) ) ;
#155281 = ORIENTED_EDGE ( 'NONE', *, *, #12066, .T. ) ;
#155283 = VERTEX_POINT ( 'NONE', #88753 ) ;
#155282 = DIRECTION ( 'NONE',  ( -4.801466763864313332E-15, -0.2605042016806672911, -0.9654727137038716656 ) ) ;
#155284 = VERTEX_POINT ( 'NONE', #185311 ) ;
#155285 = DIRECTION ( 'NONE',  ( -1.000000000000000000, -0.000000000000000000, -0.000000000000000000 ) ) ;
#155286 = LINE ( 'NONE', #136964, #30215 ) ;
#155287 = DIRECTION ( 'NONE',  ( 0.000000000000000000, -6.467318590049456648E-15, 1.000000000000000000 ) ) ;
#155288 = DIRECTION ( 'NONE',  ( 0.000000000000000000, 0.000000000000000000, -1.000000000000000000 ) ) ;
#155289 = AXIS2_PLACEMENT_3D ( 'NONE', #204894, #103220, #181517 ) ;
#155290 = ORIENTED_EDGE ( 'NONE', *, *, #246313, .T. ) ;
#155291 = DIRECTION ( 'NONE',  ( 2.827886303505249259E-16, 0.8660254037844377084, 0.5000000000000016653 ) ) ;
#155292 = SURFACE_SIDE_STYLE ('',( #154026 ) ) ;
#155293 = DIRECTION ( 'NONE',  ( -1.000000000000000000, 0.000000000000000000, -0.000000000000000000 ) ) ;
#155294 = ORIENTED_EDGE ( 'NONE', *, *, #239869, .F. ) ;
#155295 = FACE_OUTER_BOUND ( 'NONE', #126486, .T. ) ;
#155296 = CARTESIAN_POINT ( 'NONE',  ( 22.39999999999999503, 1.115600667400684642E-11, -159.7499999999999432 ) ) ;
#155297 = EDGE_LOOP ( 'NONE', ( #184808, #31063, #169523, #183664 ) ) ;
#155298 = VERTEX_POINT ( 'NONE', #144882 ) ;
#155299 = FACE_OUTER_BOUND ( 'NONE', #148468, .T. ) ;
#155300 = EDGE_CURVE ( 'NONE', #130026, #3373, #121530, .T. ) ;
#155301 = TOROIDAL_SURFACE ( 'NONE', #92711, 0.2000000000000000111, 0.1000000000000000056 ) ;
#155302 = ORIENTED_EDGE ( 'NONE', *, *, #193313, .F. ) ;
#155303 = DIRECTION ( 'NONE',  ( 1.000000000000000000, 0.000000000000000000, 0.000000000000000000 ) ) ;
#155304 = ORIENTED_EDGE ( 'NONE', *, *, #17060, .F. ) ;
#155305 = CARTESIAN_POINT ( 'NONE',  ( 20.94999999999999929, 40.18490544642472173, -251.4399342103543233 ) ) ;
#155306 = DIRECTION ( 'NONE',  ( -3.265361837132812600E-16, 0.4721928772777346239, 0.8814952561688430555 ) ) ;
#155307 = FACE_OUTER_BOUND ( 'NONE', #77165, .T. ) ;
#155308 = EDGE_CURVE ( 'NONE', #94115, #17720, #129853, .T. ) ;
#155309 = CARTESIAN_POINT ( 'NONE',  ( -16.87304349924914604, 63.08462258781068499, -213.0868426661930641 ) ) ;
#155310 = EDGE_CURVE ( 'NONE', #253481, #9372, #658, .T. ) ;
#155311 = EDGE_CURVE ( 'NONE', #208387, #159529, #7970, .T. ) ;
#155313 = AXIS2_PLACEMENT_3D ( 'NONE', #205516, #105104, #69894 ) ;
#155312 = DIRECTION ( 'NONE',  ( -0.000000000000000000, 0.8814952561688430555, -0.4721928772777346239 ) ) ;
#155314 = CARTESIAN_POINT ( 'NONE',  ( 18.47135592147657235, -9.471088613254476485, -73.68359493984345931 ) ) ;
#155315 = CARTESIAN_POINT ( 'NONE',  ( -21.45000000000000284, 52.90028168070691095, -233.8284721206281915 ) ) ;
#155316 = ORIENTED_EDGE ( 'NONE', *, *, #54675, .F. ) ;
#155318 = DIRECTION ( 'NONE',  ( 0.000000000000000000, 0.4088369013363280513, -0.9126074666063769270 ) ) ;
#155317 = CARTESIAN_POINT ( 'NONE',  ( 21.05000012384647690, 22.88246860595696219, -230.1138889447267957 ) ) ;
#155320 = ORIENTED_EDGE ( 'NONE', *, *, #215104, .T. ) ;
#155319 = AXIS2_PLACEMENT_3D ( 'NONE', #156257, #218742, #255266 ) ;
#155323 = ORIENTED_EDGE ( 'NONE', *, *, #203527, .T. ) ;
#155322 = CARTESIAN_POINT ( 'NONE',  ( -18.46856557590793813, 85.47421590779813982, -62.42112124364197001 ) ) ;
#155321 = LINE ( 'NONE', #113592, #132180 ) ;
#155324 = ORIENTED_EDGE ( 'NONE', *, *, #229300, .T. ) ;
#155325 = DIRECTION ( 'NONE',  ( -0.000000000000000000, -0.000000000000000000, 1.000000000000000000 ) ) ;
#155326 = CARTESIAN_POINT ( 'NONE',  ( 21.07928932188134041, 0.09889514566578908039, -60.67148334360133788 ) ) ;
#155328 = DIRECTION ( 'NONE',  ( 1.000000000000000000, 0.000000000000000000, 0.000000000000000000 ) ) ;
#155327 = AXIS2_PLACEMENT_3D ( 'NONE', #240766, #24297, #2126 ) ;
#155329 = CARTESIAN_POINT ( 'NONE',  ( -28.12018973533754362, 11.62642356364895413, -347.0000000000001137 ) ) ;
#155330 = ORIENTED_EDGE ( 'NONE', *, *, #198067, .T. ) ;
#155332 = EDGE_LOOP ( 'NONE', ( #151137, #39945, #245688, #101047 ) ) ;
#155331 = CARTESIAN_POINT ( 'NONE',  ( -20.94999999999994600, 65.27857539272349641, -29.97167177764265844 ) ) ;
#155333 = ADVANCED_FACE ( 'NONE', ( #204853 ), #183858, .T. ) ;
#155334 = EDGE_CURVE ( 'NONE', #70064, #136730, #188136, .T. ) ;
#155336 = CARTESIAN_POINT ( 'NONE',  ( 20.95539060131842746, 10.62386215765564579, -7.653733813656191209 ) ) ;
#155335 = DIRECTION ( 'NONE',  ( 0.000000000000000000, 0.000000000000000000, -1.000000000000000000 ) ) ;
#155338 = ORIENTED_EDGE ( 'NONE', *, *, #75007, .T. ) ;
#155337 = DIRECTION ( 'NONE',  ( 0.000000000000000000, 0.000000000000000000, 1.000000000000000000 ) ) ;
#155339 = AXIS2_PLACEMENT_3D ( 'NONE', #80653, #61110, #122378 ) ;
#155340 = CIRCLE ( 'NONE', #167795, 11.74999999999999289 ) ;
#155341 = PRODUCT_DEFINITION ( 'UNKNOWN', '', #82056, #14157 ) ;
#155342 = ORIENTED_EDGE ( 'NONE', *, *, #89318, .F. ) ;
#155343 = DIRECTION ( 'NONE',  ( 1.000000000000000000, -0.000000000000000000, -0.000000000000000000 ) ) ;
#155344 = CARTESIAN_POINT ( 'NONE',  ( -16.89318236219975944, 44.13017269538578091, -235.2996277017026046 ) ) ;
#155345 = VERTEX_POINT ( 'NONE', #87477 ) ;
#155346 = DIRECTION ( 'NONE',  ( -0.000000000000000000, 0.2128009952263604232, -0.9770955615653316162 ) ) ;
#155347 = ORIENTED_EDGE ( 'NONE', *, *, #30394, .F. ) ;
#155348 = EDGE_CURVE ( 'NONE', #159949, #70015, #179772, .T. ) ;
#155349 = VECTOR ( 'NONE', #190059, 1000.000000000000000 ) ;
#155351 = EDGE_CURVE ( 'NONE', #223143, #80694, #126619, .T. ) ;
#155350 = DIRECTION ( 'NONE',  ( -0.000000000000000000, -0.000000000000000000, -1.000000000000000000 ) ) ;
#155352 = EDGE_CURVE ( 'NONE', #143703, #203901, #229823, .T. ) ;
#155353 = ORIENTED_EDGE ( 'NONE', *, *, #20925, .F. ) ;
#155354 = CYLINDRICAL_SURFACE ( 'NONE', #25369, 0.09999999999999108213 ) ;
#155355 = AXIS2_PLACEMENT_3D ( 'NONE', #112541, #14743, #151691 ) ;
#155356 = TOROIDAL_SURFACE ( 'NONE', #113798, 0.2000000000000000111, 0.1000000000000000056 ) ;
#155357 = CIRCLE ( 'NONE', #226191, 0.1000000000000000472 ) ;
#155358 = CIRCLE ( 'NONE', #234414, 2.100000000000004530 ) ;
#155359 = DIRECTION ( 'NONE',  ( -1.000000000000000000, 0.000000000000000000, 0.000000000000000000 ) ) ;
#155360 = ORIENTED_EDGE ( 'NONE', *, *, #43026, .T. ) ;
#155361 = VERTEX_POINT ( 'NONE', #65356 ) ;
#155362 = CARTESIAN_POINT ( 'NONE',  ( -18.43634282235122157, -9.679787199916759732, -73.66065188545398712 ) ) ;
#155363 =( BOUNDED_SURFACE ( )  B_SPLINE_SURFACE ( 3, 2, ( 
 ( #230213, #52847, #114105 ),
 ( #33338, #132403, #51540 ),
 ( #131108, #35887, #110258 ),
 ( #111555, #90693, #115393 ) ),
 .UNSPECIFIED., .F., .F., .T. ) 
 B_SPLINE_SURFACE_WITH_KNOTS ( ( 4, 4 ),
 ( 3, 3 ),
 ( 5.727910411845712702, 5.983100554402349225 ),
 ( 0.000000000000000000, 1.000000000000000000 ),
 .UNSPECIFIED. ) 
 GEOMETRIC_REPRESENTATION_ITEM ( )  RATIONAL_B_SPLINE_SURFACE ( (
 ( 1.000000000000000000, 0.8946697475932141597, 1.000000000000000000),
 ( 1.000000000000000000, 0.9035312726220691149, 1.000000000000000000),
 ( 1.000000000000000000, 0.9104333467450248518, 1.000000000000000000),
 ( 1.000000000000000000, 0.9152888060719485130, 1.000000000000000000) ) ) 
 REPRESENTATION_ITEM ( '' )  SURFACE ( )  );
#155364 = ORIENTED_EDGE ( 'NONE', *, *, #15054, .F. ) ;
#155365 = ORIENTED_EDGE ( 'NONE', *, *, #132076, .F. ) ;
#155367 = EDGE_LOOP ( 'NONE', ( #48523, #66802, #20709, #69386 ) ) ;
#155366 = CARTESIAN_POINT ( 'NONE',  ( 23.24999999999999645, 71.00000000001253397, -182.4283735034374843 ) ) ;
#155368 = VERTEX_POINT ( 'NONE', #124067 ) ;
#155369 = DIRECTION ( 'NONE',  ( 0.000000000000000000, 7.056502275159890043E-15, -1.000000000000000000 ) ) ;
#155370 = ORIENTED_EDGE ( 'NONE', *, *, #11374, .F. ) ;
#155374 = EDGE_CURVE ( 'NONE', #16906, #175179, #12402, .T. ) ;
#155373 = ORIENTED_EDGE ( 'NONE', *, *, #76422, .T. ) ;
#155372 = EDGE_LOOP ( 'NONE', ( #186144, #130048, #87295, #205316 ) ) ;
#155371 = DIRECTION ( 'NONE',  ( -0.000000000000000000, -1.000000000000000000, 6.308085367188393199E-16 ) ) ;
#155375 = CIRCLE ( 'NONE', #151267, 11.74999999999999645 ) ;
#155377 = ORIENTED_EDGE ( 'NONE', *, *, #166940, .T. ) ;
#155376 = B_SPLINE_CURVE_WITH_KNOTS ( 'NONE', 3,
 ( #99003, #254237, #212578, #33974, #155193, #242387, #159038 ),
 .UNSPECIFIED., .F., .F.,
 ( 4, 3, 4 ),
 ( 0.000000000000000000, 3.357501770813415632E-05, 5.199112466348475308E-05 ),
 .UNSPECIFIED. ) ;
#155378 = DIRECTION ( 'NONE',  ( -1.000000000000000000, -0.000000000000000000, 0.000000000000000000 ) ) ;
#155379 = CARTESIAN_POINT ( 'NONE',  ( 18.52928932188133970, 65.72071067813116940, -178.7731074845244450 ) ) ;
#155380 = DIRECTION ( 'NONE',  ( 0.000000000000000000, -0.8814952561688430555, 0.4721928772777346239 ) ) ;
#155381 = ORIENTED_EDGE ( 'NONE', *, *, #115851, .F. ) ;
#155382 = AXIS2_PLACEMENT_3D ( 'NONE', #120726, #181966, #58129 ) ;
#155383 = ADVANCED_FACE ( 'NONE', ( #243989 ), #28857, .F. ) ;
#155384 = CARTESIAN_POINT ( 'NONE',  ( 18.49999999999998934, 69.45000000001230944, -160.0060803140843859 ) ) ;
#155385 = AXIS2_PLACEMENT_3D ( 'NONE', #195831, #250626, #133264 ) ;
#155387 = ORIENTED_EDGE ( 'NONE', *, *, #43207, .F. ) ;
#155386 = LINE ( 'NONE', #232345, #99158 ) ;
#155388 = CARTESIAN_POINT ( 'NONE',  ( 16.87683809663750267, 12.41403342719998371, -211.2428889513006993 ) ) ;
#155389 = ORIENTED_EDGE ( 'NONE', *, *, #31842, .T. ) ;
#155390 = VERTEX_POINT ( 'NONE', #184017 ) ;
#155391 = AXIS2_PLACEMENT_3D ( 'NONE', #195614, #96460, #136893 ) ;
#155392 = EDGE_CURVE ( 'NONE', #154603, #106161, #246553, .T. ) ;
#155393 = CARTESIAN_POINT ( 'NONE',  ( -21.05000000000000071, 0.5663372425336981042, -209.0641885820623997 ) ) ;
#155394 = FILL_AREA_STYLE ('',( #75823 ) ) ;
#155395 = AXIS2_PLACEMENT_3D ( 'NONE', #63265, #179392, #80229 ) ;
#155396 = VECTOR ( 'NONE', #250920, 1000.000000000000000 ) ;
#155397 = EDGE_CURVE ( 'NONE', #79959, #243325, #138043, .T. ) ;
#155398 = ORIENTED_EDGE ( 'NONE', *, *, #8624, .F. ) ;
#155399 = VERTEX_POINT ( 'NONE', #207457 ) ;
#155400 = FACE_OUTER_BOUND ( 'NONE', #47456, .T. ) ;
#155401 = DIRECTION ( 'NONE',  ( -1.000000000000000000, 0.000000000000000000, 0.000000000000000000 ) ) ;
#155402 = VECTOR ( 'NONE', #187073, 1000.000000000000000 ) ;
#155403 = EDGE_CURVE ( 'NONE', #30013, #159618, #249155, .T. ) ;
#155405 = VERTEX_POINT ( 'NONE', #130467 ) ;
#155404 = ORIENTED_EDGE ( 'NONE', *, *, #965, .T. ) ;
#155406 = ORIENTED_EDGE ( 'NONE', *, *, #254388, .T. ) ;
#155408 = EDGE_CURVE ( 'NONE', #134698, #28383, #104698, .T. ) ;
#155407 = CARTESIAN_POINT ( 'NONE',  ( -20.64999999999999858, 1.115600667400684642E-11, -100.5000000000000284 ) ) ;
#155409 = ORIENTED_EDGE ( 'NONE', *, *, #221045, .F. ) ;
#155410 = EDGE_LOOP ( 'NONE', ( #117622, #138499, #107734, #228553, #158936 ) ) ;
#155411 = CARTESIAN_POINT ( 'NONE',  ( 20.95224633520496127, 18.81837940936716791, -229.8973978886525913 ) ) ;
#155412 = B_SPLINE_CURVE_WITH_KNOTS ( 'NONE', 3,
 ( #143966, #65724, #67010, #203948, #164836, #22772, #100942, #142669, #185678, #145247 ),
 .UNSPECIFIED., .F., .F.,
 ( 4, 3, 3, 4 ),
 ( 0.000000000000000000, 0.0002000000000002897355, 0.001000000000045110204, 0.001967863649472100917 ),
 .UNSPECIFIED. ) ;
#155413 = ORIENTED_EDGE ( 'NONE', *, *, #147461, .T. ) ;
#155414 = DIRECTION ( 'NONE',  ( 0.000000000000000000, -1.000000000000000000, -6.982962677686265922E-15 ) ) ;
#155415 = AXIS2_PLACEMENT_3D ( 'NONE', #180183, #101881, #1513 ) ;
#155417 = DIRECTION ( 'NONE',  ( 1.000000000000000000, -3.965082230804126670E-15, 0.000000000000000000 ) ) ;
#155416 = DIRECTION ( 'NONE',  ( 1.000000000000000000, 0.000000000000000000, 0.000000000000000000 ) ) ;
#155419 = ORIENTED_EDGE ( 'NONE', *, *, #91997, .F. ) ;
#155418 = VECTOR ( 'NONE', #112949, 1000.000000000000000 ) ;
#155420 = ORIENTED_EDGE ( 'NONE', *, *, #136196, .T. ) ;
#155421 = DIRECTION ( 'NONE',  ( 0.000000000000000000, 0.000000000000000000, -1.000000000000000000 ) ) ;
#155422 = VERTEX_POINT ( 'NONE', #35262 ) ;
#155423 = ADVANCED_FACE ( 'NONE', ( #251703 ), #33987, .F. ) ;
#155424 = EDGE_CURVE ( 'NONE', #212362, #42512, #95199, .T. ) ;
#155425 = CIRCLE ( 'NONE', #101164, 0.09999999999999939493 ) ;
#155426 = AXIS2_PLACEMENT_3D ( 'NONE', #203633, #221885, #125391 ) ;
#155427 = AXIS2_PLACEMENT_3D ( 'NONE', #179379, #80215, #229405 ) ;
#155428 = AXIS2_PLACEMENT_3D ( 'NONE', #91664, #126942, #248173 ) ;
#155429 = DIRECTION ( 'NONE',  ( 1.000000000000000000, 0.000000000000000000, 0.000000000000000000 ) ) ;
#155430 = ORIENTED_EDGE ( 'NONE', *, *, #173357, .T. ) ;
#155431 = ORIENTED_EDGE ( 'NONE', *, *, #155037, .F. ) ;
#155432 = ADVANCED_FACE ( 'NONE', ( #16962 ), #31410, .F. ) ;
#155433 = DIRECTION ( 'NONE',  ( -1.000000000000000000, -0.000000000000000000, 0.000000000000000000 ) ) ;
#155435 = EDGE_LOOP ( 'NONE', ( #214602, #84208, #82779, #25177 ) ) ;
#155434 = CARTESIAN_POINT ( 'NONE',  ( 18.49999999999997868, 85.32100840337365355, -162.7871692354464130 ) ) ;
#155436 = FACE_OUTER_BOUND ( 'NONE', #26018, .T. ) ;
#155437 = CARTESIAN_POINT ( 'NONE',  ( -18.37013991200266005, 33.97311679673139651, -235.0667207747197267 ) ) ;
#155438 = VERTEX_POINT ( 'NONE', #74390 ) ;
#155439 = DIRECTION ( 'NONE',  ( 0.000000000000000000, -7.429790795770644761E-15, 1.000000000000000000 ) ) ;
#155440 = FACE_OUTER_BOUND ( 'NONE', #174957, .T. ) ;
#155441 = CARTESIAN_POINT ( 'NONE',  ( 18.59999999999999787, 76.00000000001195133, -103.0231074845243171 ) ) ;
#155442 = DIRECTION ( 'NONE',  ( 0.000000000000000000, -7.272083257015735086E-15, 1.000000000000000000 ) ) ;
#155443 = DIRECTION ( 'NONE',  ( -1.000000000000000000, -0.000000000000000000, -0.000000000000000000 ) ) ;
#155444 = LINE ( 'NONE', #175017, #19988 ) ;
#155446 = EDGE_CURVE ( 'NONE', #86798, #24027, #229583, .T. ) ;
#155445 = CARTESIAN_POINT ( 'NONE',  ( -21.40925344232282512, 69.34148114062121238, -69.62205767314401328 ) ) ;
#155447 = CARTESIAN_POINT ( 'NONE',  ( -20.94999999999999929, 5.900000000011102586, -144.2190997646564483 ) ) ;
#155448 = CYLINDRICAL_SURFACE ( 'NONE', #159836, 11.74999999999999645 ) ;
#155449 = EDGE_CURVE ( 'NONE', #248851, #120967, #254722, .T. ) ;
#155450 = AXIS2_PLACEMENT_3D ( 'NONE', #84703, #224245, #185131 ) ;
#155452 = ORIENTED_EDGE ( 'NONE', *, *, #159960, .T. ) ;
#155451 = CIRCLE ( 'NONE', #126160, 0.09999999999999939493 ) ;
#155453 = VECTOR ( 'NONE', #13876, 1000.000000000000000 ) ;
#155454 = VECTOR ( 'NONE', #243539, 1000.000000000000000 ) ;
#155455 = EDGE_CURVE ( 'NONE', #125245, #117081, #142332, .T. ) ;
#155457 = ORIENTED_EDGE ( 'NONE', *, *, #251890, .F. ) ;
#155456 = ORIENTED_EDGE ( 'NONE', *, *, #203929, .F. ) ;
#155458 = EDGE_LOOP ( 'NONE', ( #23853, #93975, #137052, #114532 ) ) ;
#155459 = CARTESIAN_POINT ( 'NONE',  ( -21.08376601933334271, 0.06377601094103638180, -94.15805272872430010 ) ) ;
#155460 = DIRECTION ( 'NONE',  ( 0.000000000000000000, 0.000000000000000000, 1.000000000000000000 ) ) ;
#155462 = CARTESIAN_POINT ( 'NONE',  ( 20.94999999999999929, 53.86595165227826243, -236.3638196928718855 ) ) ;
#155461 = DIRECTION ( 'NONE',  ( 0.000000000000000000, 0.000000000000000000, 1.000000000000000000 ) ) ;
#155463 = EDGE_CURVE ( 'NONE', #181967, #51363, #152639, .T. ) ;
#155464 = EDGE_LOOP ( 'NONE', ( #109602, #142160, #76132, #120705 ) ) ;
#155465 = DIRECTION ( 'NONE',  ( -1.000000000000000000, 0.000000000000000000, -0.000000000000000000 ) ) ;
#155466 =( NAMED_UNIT ( * ) PLANE_ANGLE_UNIT ( ) SI_UNIT ( $, .RADIAN. ) );
#155467 = CARTESIAN_POINT ( 'NONE',  ( 23.24999999999999289, 71.85000000001166143, -69.52310748452434552 ) ) ;
#155468 = CARTESIAN_POINT ( 'NONE',  ( -16.87383368123029825, 9.950000000011138823, -180.1499999999999773 ) ) ;
#155469 = DIRECTION ( 'NONE',  ( -0.000000000000000000, -0.000000000000000000, 1.000000000000000000 ) ) ;
#155470 = VERTEX_POINT ( 'NONE', #193026 ) ;
#155471 = VERTEX_POINT ( 'NONE', #230880 ) ;
#155472 = CARTESIAN_POINT ( 'NONE',  ( -20.54999999999999716, 73.50000000001223555, -149.7477294072864709 ) ) ;
#155473 = CARTESIAN_POINT ( 'NONE',  ( 23.25000000000000000, 85.00000000001179501, -79.41707660717668205 ) ) ;
#155474 = VECTOR ( 'NONE', #76305, 1000.000000000000000 ) ;
#155475 = EDGE_LOOP ( 'NONE', ( #28223, #97140, #193412, #48755, #181040, #96510, #253878, #246157, #125029, #100921 ) ) ;
#155476 = FACE_BOUND ( 'NONE', #249321, .T. ) ;
#155477 = DIRECTION ( 'NONE',  ( 0.000000000000000000, 0.2128009952263603677, -0.9770955615653313941 ) ) ;
#155478 = DIRECTION ( 'NONE',  ( -1.000000000000000000, 0.000000000000000000, 0.000000000000000000 ) ) ;
#155479 = DIRECTION ( 'NONE',  ( 0.000000000000000000, 0.000000000000000000, -1.000000000000000000 ) ) ;
#155480 = DIRECTION ( 'NONE',  ( 0.000000000000000000, -6.982962677686266711E-15, 1.000000000000000000 ) ) ;
#155481 = ORIENTED_EDGE ( 'NONE', *, *, #224159, .T. ) ;
#155482 = FACE_OUTER_BOUND ( 'NONE', #68164, .T. ) ;
#155483 = DIRECTION ( 'NONE',  ( 1.000000000000000000, 0.000000000000000000, 0.000000000000000000 ) ) ;
#155484 = DIRECTION ( 'NONE',  ( 0.000000000000000000, 0.000000000000000000, 1.000000000000000000 ) ) ;
#155486 = DIRECTION ( 'NONE',  ( -1.652117596168391700E-15, 1.000000000000000000, 6.982962677686266711E-15 ) ) ;
#155485 = CARTESIAN_POINT ( 'NONE',  ( -20.94999999999999929, 74.16465844978715438, -57.96795619196135618 ) ) ;
#155487 = DIRECTION ( 'NONE',  ( -1.000000000000000000, 0.000000000000000000, 0.000000000000000000 ) ) ;
#155488 = DIRECTION ( 'NONE',  ( 0.000000000000000000, -0.9651348961777379554, 0.2617529984164210233 ) ) ;
#155489 = DIRECTION ( 'NONE',  ( -1.000000000000000000, 0.000000000000000000, 0.000000000000000000 ) ) ;
#155490 = CARTESIAN_POINT ( 'NONE',  ( 22.43288208788031568, 75.99510014512664213, -114.6727593282433872 ) ) ;
#155491 = VECTOR ( 'NONE', #127711, 1000.000000000000000 ) ;
#155492 = ORIENTED_EDGE ( 'NONE', *, *, #38029, .F. ) ;
#155493 = ADVANCED_FACE ( 'NONE', ( #153940 ), #254249, .T. ) ;
#155494 = VECTOR ( 'NONE', #92674, 1000.000000000000000 ) ;
#155495 = VERTEX_POINT ( 'NONE', #131753 ) ;
#155496 = PLANE ( 'NONE',  #144554 ) ;
#155497 = EDGE_LOOP ( 'NONE', ( #191474, #6179, #16063, #98865 ) ) ;
#155498 = DIRECTION ( 'NONE',  ( 0.000000000000000000, -0.000000000000000000, 1.000000000000000000 ) ) ;
#155499 = ORIENTED_EDGE ( 'NONE', *, *, #145017, .T. ) ;
#155500 = SURFACE_STYLE_USAGE ( .BOTH. , #254530 ) ;
#155501 = VECTOR ( 'NONE', #160697, 1000.000000000000000 ) ;
#155502 = ADVANCED_FACE ( 'NONE', ( #52202 ), #53505, .F. ) ;
#155503 = ORIENTED_EDGE ( 'NONE', *, *, #233898, .F. ) ;
#155504 = AXIS2_PLACEMENT_3D ( 'NONE', #234158, #231612, #195065 ) ;
#155505 = CARTESIAN_POINT ( 'NONE',  ( 18.46921299892754575, -7.804820308205004942, -209.8501601876789948 ) ) ;
#155506 = CARTESIAN_POINT ( 'NONE',  ( -13.54036565897074951, 9.451541661396669625, -51.95387549883059819 ) ) ;
#155507 = CARTESIAN_POINT ( 'NONE',  ( 18.59999999999996945, 65.66751761918692409, -130.9282609406112670 ) ) ;
#155508 = CIRCLE ( 'NONE', #188782, 0.1000000000000089567 ) ;
#155509 = CARTESIAN_POINT ( 'NONE',  ( 21.05000000000000071, 76.00000000001195133, -103.0231074845243171 ) ) ;
#155511 = ORIENTED_EDGE ( 'NONE', *, *, #76829, .T. ) ;
#155510 = DIRECTION ( 'NONE',  ( 0.000000000000000000, -6.982962677686266711E-15, 1.000000000000000000 ) ) ;
#155513 = CARTESIAN_POINT ( 'NONE',  ( 19.83283456528359423, 11.75000000001116263, -192.3499999994177472 ) ) ;
#155512 = CARTESIAN_POINT ( 'NONE',  ( 21.04999999999999716, 6.195883767078806059, -199.6353987068638105 ) ) ;
#155514 = CARTESIAN_POINT ( 'NONE',  ( -21.05000000000000071, -0.09999999999999939493, 11.65000000000000036 ) ) ;
#155515 = CARTESIAN_POINT ( 'NONE',  ( 21.05000000000000071, 64.40000000001194280, -109.9513107147998880 ) ) ;
#155516 = CARTESIAN_POINT ( 'NONE',  ( 18.79999999999999716, 1.885425182446133885, -11.49641995933507843 ) ) ;
#155517 = CARTESIAN_POINT ( 'NONE',  ( -21.55000000000000426, 7.708578643773852157, -112.8500000000000369 ) ) ;
#155518 = ORIENTED_EDGE ( 'NONE', *, *, #204047, .T. ) ;
#155520 = DIRECTION ( 'NONE',  ( 2.879366945564059217E-14, 0.9875055080513762684, -0.1575844902526679081 ) ) ;
#155519 = AXIS2_PLACEMENT_3D ( 'NONE', #143796, #242902, #220779 ) ;
#155521 = AXIS2_PLACEMENT_3D ( 'NONE', #186694, #150139, #28937 ) ;
#155522 = ORIENTED_EDGE ( 'NONE', *, *, #168222, .T. ) ;
#155523 = DIRECTION ( 'NONE',  ( 0.000000000000000000, 0.000000000000000000, -1.000000000000000000 ) ) ;
#155524 = ORIENTED_EDGE ( 'NONE', *, *, #28374, .F. ) ;
#155525 = DIRECTION ( 'NONE',  ( 0.000000000000000000, 0.000000000000000000, 1.000000000000000000 ) ) ;
#155526 = AXIS2_PLACEMENT_3D ( 'NONE', #150621, #248440, #193603 ) ;
#155527 = DIRECTION ( 'NONE',  ( 1.000000000000000000, 0.000000000000000000, 0.000000000000000000 ) ) ;
#155528 = DIRECTION ( 'NONE',  ( 1.000000000000000000, 0.000000000000000000, 0.000000000000000000 ) ) ;
#155529 = EDGE_LOOP ( 'NONE', ( #221424, #220285, #203858, #27521 ) ) ;
#155530 = EDGE_LOOP ( 'NONE', ( #59633, #251490, #3657, #116813 ) ) ;
#155531 = AXIS2_PLACEMENT_3D ( 'NONE', #118963, #19866, #99360 ) ;
#155532 = AXIS2_PLACEMENT_3D ( 'NONE', #157927, #100437, #18366 ) ;
#155533 = AXIS2_PLACEMENT_3D ( 'NONE', #192154, #73499, #146869 ) ;
#155534 = CIRCLE ( 'NONE', #209477, 0.09999999999998898659 ) ;
#155535 = DIRECTION ( 'NONE',  ( -0.000000000000000000, -0.000000000000000000, -1.000000000000000000 ) ) ;
#155536 = DIRECTION ( 'NONE',  ( 2.715809747126116508E-16, -1.000000000000000000, 4.345295595401786413E-15 ) ) ;
#155537 = CARTESIAN_POINT ( 'NONE',  ( -16.87401514999228880, 63.06741435278433272, -213.1951636644405710 ) ) ;
#155538 = FACE_OUTER_BOUND ( 'NONE', #36985, .T. ) ;
#155539 = EDGE_CURVE ( 'NONE', #42440, #242161, #212594, .T. ) ;
#155541 = DIRECTION ( 'NONE',  ( 1.000000000000000000, 0.000000000000000000, 0.000000000000000000 ) ) ;
#155540 = CARTESIAN_POINT ( 'NONE',  ( -21.93340585900934414, 76.00000000001219291, -143.8472545066296391 ) ) ;
#155542 = CARTESIAN_POINT ( 'NONE',  ( 21.05000000000000071, -3.770473190032740174, -225.9805569534692324 ) ) ;
#155543 = CARTESIAN_POINT ( 'NONE',  ( 13.22461703343584816, 9.436662931810237964, -51.82303673229489505 ) ) ;
#155544 = SPHERICAL_SURFACE ( 'NONE', #9556, 0.1000000000000000056 ) ;
#155545 = ORIENTED_EDGE ( 'NONE', *, *, #36171, .F. ) ;
#155546 = CARTESIAN_POINT ( 'NONE',  ( 20.94999999999999574, 74.25000000001259082, -191.8535959266227451 ) ) ;
#155548 = ORIENTED_EDGE ( 'NONE', *, *, #24403, .T. ) ;
#155547 = DIRECTION ( 'NONE',  ( 0.000000000000000000, -1.000000000000000000, 0.000000000000000000 ) ) ;
#155549 = CARTESIAN_POINT ( 'NONE',  ( 23.24999999999999645, 78.10000000001245724, -170.0231074845243313 ) ) ;
#155550 = CARTESIAN_POINT ( 'NONE',  ( 22.49806830649814060, 11.36657099087203093, -198.4452018475131183 ) ) ;
#155552 = LINE ( 'NONE', #176387, #190927 ) ;
#155551 = DIRECTION ( 'NONE',  ( -1.000000000000000000, 0.000000000000000000, 0.000000000000000000 ) ) ;
#155553 = ADVANCED_FACE ( 'NONE', ( #173511 ), #4754, .T. ) ;
#155555 = ORIENTED_EDGE ( 'NONE', *, *, #22990, .F. ) ;
#155554 = CARTESIAN_POINT ( 'NONE',  ( 21.07094088545303734, 69.67983277809565834, -136.6220011870765632 ) ) ;
#155557 = DIRECTION ( 'NONE',  ( 1.000000000000000000, 0.000000000000000000, -0.000000000000000000 ) ) ;
#155556 = CARTESIAN_POINT ( 'NONE',  ( 20.94999999999999929, 9.863005973831429074, -220.4411654715779321 ) ) ;
#155558 = FACE_OUTER_BOUND ( 'NONE', #109806, .T. ) ;
#155559 = LINE ( 'NONE', #195953, #226092 ) ;
#155560 = DIRECTION ( 'NONE',  ( -2.978066053179066765E-16, 0.9770955615653311721, 0.2128009952263619775 ) ) ;
#155561 = CARTESIAN_POINT ( 'NONE',  ( -20.64999999999999858, -3.664072692419557242, -226.4691047342518857 ) ) ;
#155562 = EDGE_CURVE ( 'NONE', #53558, #256577, #11839, .T. ) ;
#155563 = ORIENTED_EDGE ( 'NONE', *, *, #183702, .F. ) ;
#155564 = CYLINDRICAL_SURFACE ( 'NONE', #238667, 0.1000000000000028644 ) ;
#155565 = ORIENTED_EDGE ( 'NONE', *, *, #22329, .F. ) ;
#155566 = CIRCLE ( 'NONE', #209694, 0.09999999999999108213 ) ;
#155567 = AXIS2_PLACEMENT_3D ( 'NONE', #203546, #204808, #44485 ) ;
#155568 = CARTESIAN_POINT ( 'NONE',  ( -18.41418431465368144, -9.500000000000223821, -40.10018939122146264 ) ) ;
#155569 = EDGE_CURVE ( 'NONE', #212622, #167295, #16655, .T. ) ;
#155570 = ORIENTED_EDGE ( 'NONE', *, *, #68389, .T. ) ;
#155571 = DIRECTION ( 'NONE',  ( -1.000000000000000000, 3.265361837132813093E-16, 2.280189983783949500E-30 ) ) ;
#155572 = AXIS2_PLACEMENT_3D ( 'NONE', #121591, #240236, #103247 ) ;
#155573 = ORIENTED_EDGE ( 'NONE', *, *, #47501, .T. ) ;
#155574 = DIRECTION ( 'NONE',  ( -1.000000000000000000, -0.000000000000000000, -0.000000000000000000 ) ) ;
#155575 = CARTESIAN_POINT ( 'NONE',  ( 20.94999999999999929, 1.115600667400684642E-11, -67.00000000000000000 ) ) ;
#155576 = AXIS2_PLACEMENT_3D ( 'NONE', #197358, #57832, #199953 ) ;
#155577 = TOROIDAL_SURFACE ( 'NONE', #72342, 0.2000000000000000111, 0.1000000000000000056 ) ;
#155578 = DIRECTION ( 'NONE',  ( -0.000000000000000000, 1.000000000000000000, 6.982962677686266711E-15 ) ) ;
#155579 = EDGE_LOOP ( 'NONE', ( #247297, #61694, #16160, #126496 ) ) ;
#155580 = ADVANCED_FACE ( 'NONE', ( #191767 ), #195608, .F. ) ;
#155581 = VECTOR ( 'NONE', #148463, 1000.000000000000000 ) ;
#155582 = CARTESIAN_POINT ( 'NONE',  ( -18.42637059832563651, -9.496945461878544492, -174.1090773097998579 ) ) ;
#155584 = AXIS2_PLACEMENT_3D ( 'NONE', #37018, #173986, #155688 ) ;
#155583 = DIRECTION ( 'NONE',  ( 0.000000000000000000, -6.982962677686266711E-15, 1.000000000000000000 ) ) ;
#155585 = DIRECTION ( 'NONE',  ( 0.000000000000000000, 0.000000000000000000, -1.000000000000000000 ) ) ;
#155586 = CIRCLE ( 'NONE', #21707, 11.70000000000000284 ) ;
#155588 = CIRCLE ( 'NONE', #30664, 0.1000000000000028644 ) ;
#155587 = B_SPLINE_CURVE_WITH_KNOTS ( 'NONE', 3,
 ( #69225, #228283, #49631, #138137, #116045, #78168, #177323 ),
 .UNSPECIFIED., .F., .F.,
 ( 4, 3, 4 ),
 ( 0.000000000000000000, 3.882884552233767958E-05, 5.798605692157499417E-05 ),
 .UNSPECIFIED. ) ;
#155589 = CARTESIAN_POINT ( 'NONE',  ( -16.87331047859651179, 60.93935776605891164, -221.0417277355860790 ) ) ;
#155590 = FACE_OUTER_BOUND ( 'NONE', #236346, .T. ) ;
#155591 = VERTEX_POINT ( 'NONE', #121221 ) ;
#155592 = DIRECTION ( 'NONE',  ( -1.000000000000000000, 0.000000000000000000, 0.000000000000000000 ) ) ;
#155593 = ORIENTED_EDGE ( 'NONE', *, *, #26444, .F. ) ;
#155595 = ORIENTED_EDGE ( 'NONE', *, *, #251627, .F. ) ;
#155594 = DIRECTION ( 'NONE',  ( 0.000000000000000000, -0.008583690987162452199, 0.9999631594459053030 ) ) ;
#155596 = CIRCLE ( 'NONE', #226243, 0.1999999999999996503 ) ;
#155597 = VERTEX_POINT ( 'NONE', #117331 ) ;
#155598 = CARTESIAN_POINT ( 'NONE',  ( 21.00023020733503287, 1.115539681028482333E-11, -60.60913075473168021 ) ) ;
#155599 = DIRECTION ( 'NONE',  ( 0.000000000000000000, 0.5859227990963362664, 0.8103668758649469339 ) ) ;
#155600 = SPHERICAL_SURFACE ( 'NONE', #1531, 0.1000000000000000056 ) ;
#155601 = FACE_OUTER_BOUND ( 'NONE', #37218, .T. ) ;
#155602 = ORIENTED_EDGE ( 'NONE', *, *, #95597, .T. ) ;
#155603 = DIRECTION ( 'NONE',  ( -0.000000000000000000, 0.9770955615653313941, 0.2128009952263603954 ) ) ;
#155605 = DIRECTION ( 'NONE',  ( 0.000000000000000000, 0.000000000000000000, -1.000000000000000000 ) ) ;
#155604 = AXIS2_PLACEMENT_3D ( 'NONE', #257083, #78480, #158084 ) ;
#155606 = ORIENTED_EDGE ( 'NONE', *, *, #254879, .T. ) ;
#155607 = ADVANCED_FACE ( 'NONE', ( #239854 ), #847, .F. ) ;
#155609 = ORIENTED_EDGE ( 'NONE', *, *, #1103, .T. ) ;
#155608 = CARTESIAN_POINT ( 'NONE',  ( 23.14999999999999858, 70.50000000001180922, -81.92837350343744163 ) ) ;
#155610 = CARTESIAN_POINT ( 'NONE',  ( -18.50000000000000000, 64.25000000001165290, -69.42310748452440805 ) ) ;
#155611 = CIRCLE ( 'NONE', #147184, 0.5000000000000004441 ) ;
#155612 = CARTESIAN_POINT ( 'NONE',  ( -16.80070461187915498, 9.950000000011140600, -79.64696382916137907 ) ) ;
#155613 = EDGE_LOOP ( 'NONE', ( #216586, #150025, #132973, #78377 ) ) ;
#155614 = AXIS2_PLACEMENT_3D ( 'NONE', #4606, #84102, #26786 ) ;
#155615 = VECTOR ( 'NONE', #89233, 1000.000000000000000 ) ;
#155616 = EDGE_CURVE ( 'NONE', #64893, #5474, #200799, .T. ) ;
#155617 = AXIS2_PLACEMENT_3D ( 'NONE', #60229, #244000, #241454 ) ;
#155618 = CARTESIAN_POINT ( 'NONE',  ( -20.64999999999999858, -9.499999999988848032, -76.89396912265249284 ) ) ;
#155619 = ORIENTED_EDGE ( 'NONE', *, *, #247931, .F. ) ;
#155620 = CARTESIAN_POINT ( 'NONE',  ( -20.94999999999999929, -1.835341550213255957, -179.1551512925629197 ) ) ;
#155621 = DIRECTION ( 'NONE',  ( -1.000000000000000000, -0.000000000000000000, 0.000000000000000000 ) ) ;
#155622 = EDGE_CURVE ( 'NONE', #34485, #168568, #204870, .T. ) ;
#155623 = CARTESIAN_POINT ( 'NONE',  ( -18.40000000000000213, 67.17743825834509153, -45.27310748452438816 ) ) ;
#155624 = ADVANCED_FACE ( 'NONE', ( #177339 ), #119934, .F. ) ;
#155625 = AXIS2_PLACEMENT_3D ( 'NONE', #83104, #122281, #201804 ) ;
#155626 = AXIS2_PLACEMENT_3D ( 'NONE', #176769, #197586, #77620 ) ;
#155627 = AXIS2_PLACEMENT_3D ( 'NONE', #239615, #163927, #238314 ) ;
#155628 = CIRCLE ( 'NONE', #180544, 0.09999999999999939493 ) ;
#155629 = ORIENTED_EDGE ( 'NONE', *, *, #71997, .F. ) ;
#155630 = LINE ( 'NONE', #153069, #131995 ) ;
#155631 = EDGE_LOOP ( 'NONE', ( #188242, #256012, #191116, #134566 ) ) ;
#155632 = CARTESIAN_POINT ( 'NONE',  ( -17.11825945287481687, 9.950000000011138823, -188.2499999999999716 ) ) ;
#155633 = DIRECTION ( 'NONE',  ( -4.336808689941752679E-15, 0.8660254037844482555, 0.4999999999999837907 ) ) ;
#155636 = ADVANCED_FACE ( 'NONE', ( #79469 ), #102874, .F. ) ;
#155635 = VERTEX_POINT ( 'NONE', #217681 ) ;
#155634 = CARTESIAN_POINT ( 'NONE',  ( 21.06089410995830491, 10.72529553213474429, -146.2023807310431778 ) ) ;
#155637 = FACE_OUTER_BOUND ( 'NONE', #250373, .T. ) ;
#155638 = CARTESIAN_POINT ( 'NONE',  ( 20.94999999999999929, -11.29603075032412640, -97.45210084033617193 ) ) ;
#155639 = FACE_OUTER_BOUND ( 'NONE', #155579, .T. ) ;
#155640 = CARTESIAN_POINT ( 'NONE',  ( -18.59999999999999787, 1.340746217944851715, -157.2271374945787841 ) ) ;
#155641 = CARTESIAN_POINT ( 'NONE',  ( 21.05000000000000071, 6.257814610487288043, -33.40220970869120976 ) ) ;
#155642 = EDGE_CURVE ( 'NONE', #237787, #56976, #159130, .T. ) ;
#155643 = DIRECTION ( 'NONE',  ( -1.000000000000000000, 2.952720810173289112E-16, 2.061873921506763405E-30 ) ) ;
#155644 = ADVANCED_FACE ( 'NONE', ( #159052 ), #178617, .F. ) ;
#155645 = LINE ( 'NONE', #173937, #252914 ) ;
#155647 = ORIENTED_EDGE ( 'NONE', *, *, #142084, .T. ) ;
#155646 = CARTESIAN_POINT ( 'NONE',  ( 18.69999999999999929, 1.410778198689825125, -7.973296578895943121 ) ) ;
#155649 = EDGE_CURVE ( 'NONE', #246982, #3356, #40401, .T. ) ;
#155648 = CARTESIAN_POINT ( 'NONE',  ( -18.39999999999999858, -9.682403433476396870, -40.15684337741279109 ) ) ;
#155650 = AXIS2_PLACEMENT_3D ( 'NONE', #220679, #100686, #184105 ) ;
#155652 = EDGE_CURVE ( 'NONE', #82258, #237661, #179962, .T. ) ;
#155651 = CYLINDRICAL_SURFACE ( 'NONE', #107558, 0.09999999999999939493 ) ;
#155653 = CARTESIAN_POINT ( 'NONE',  ( -21.05000000000000071, -11.64999999998884306, -131.1000000000000227 ) ) ;
#155654 = EDGE_CURVE ( 'NONE', #56627, #216065, #9252, .T. ) ;
#155655 = VERTEX_POINT ( 'NONE', #82015 ) ;
#155656 = FACE_OUTER_BOUND ( 'NONE', #166557, .T. ) ;
#155657 = DIRECTION ( 'NONE',  ( 0.000000000000000000, 0.000000000000000000, 1.000000000000000000 ) ) ;
#155658 = CARTESIAN_POINT ( 'NONE',  ( -18.50000000000000355, 85.40000000001157332, -62.22584772486096938 ) ) ;
#155659 = ORIENTED_EDGE ( 'NONE', *, *, #179608, .T. ) ;
#155660 = CIRCLE ( 'NONE', #247195, 0.2000000000000005107 ) ;
#155661 = CARTESIAN_POINT ( 'NONE',  ( -20.54999999999999716, 7.128833340094563376, -233.7327013124401276 ) ) ;
#155662 = AXIS2_PLACEMENT_3D ( 'NONE', #221587, #2552, #143353 ) ;
#155663 = CARTESIAN_POINT ( 'NONE',  ( -23.15000000000000213, 71.65000000001187175, -90.87310748452432563 ) ) ;
#155664 = ORIENTED_EDGE ( 'NONE', *, *, #93583, .T. ) ;
#155665 = DIRECTION ( 'NONE',  ( -1.000000000000000000, 0.000000000000000000, -0.000000000000000000 ) ) ;
#155666 = ADVANCED_FACE ( 'NONE', ( #101579 ), #18234, .F. ) ;
#155667 = VERTEX_POINT ( 'NONE', #218986 ) ;
#155668 = ADVANCED_FACE ( 'NONE', ( #20819 ), #57332, .T. ) ;
#155669 = FACE_OUTER_BOUND ( 'NONE', #210929, .T. ) ;
#155671 = EDGE_LOOP ( 'NONE', ( #250056, #64342, #171219, #169717 ) ) ;
#155670 = LINE ( 'NONE', #73562, #68103 ) ;
#155672 = CARTESIAN_POINT ( 'NONE',  ( -23.25000000000000000, 74.08971962618026907, -123.8917396293253717 ) ) ;
#155673 = ORIENTED_EDGE ( 'NONE', *, *, #113320, .T. ) ;
#155674 = DIRECTION ( 'NONE',  ( 0.000000000000000000, -0.000000000000000000, 1.000000000000000000 ) ) ;
#155675 = ORIENTED_EDGE ( 'NONE', *, *, #128557, .F. ) ;
#155678 = EDGE_CURVE ( 'NONE', #182258, #172675, #88322, .T. ) ;
#155677 = ORIENTED_EDGE ( 'NONE', *, *, #98572, .T. ) ;
#155676 = ORIENTED_EDGE ( 'NONE', *, *, #214708, .T. ) ;
#155680 = CARTESIAN_POINT ( 'NONE',  ( 20.94999999999999574, 10.62357026049396680, -107.9919452032305855 ) ) ;
#155679 = CIRCLE ( 'NONE', #143146, 0.9750000000000036415 ) ;
#155681 = ORIENTED_EDGE ( 'NONE', *, *, #209416, .T. ) ;
#155682 = DIRECTION ( 'NONE',  ( -1.000000000000000000, 0.000000000000000000, 0.000000000000000000 ) ) ;
#155683 = EDGE_LOOP ( 'NONE', ( #220477, #125168, #4232, #79769 ) ) ;
#155684 = CIRCLE ( 'NONE', #176513, 0.1000000000000014488 ) ;
#155685 = AXIS2_PLACEMENT_3D ( 'NONE', #226453, #189929, #73865 ) ;
#155686 = ORIENTED_EDGE ( 'NONE', *, *, #145169, .T. ) ;
#155687 = CARTESIAN_POINT ( 'NONE',  ( -21.65000000000000213, 9.949999999999985079, -12.75000000000000178 ) ) ;
#155688 = DIRECTION ( 'NONE',  ( 1.000000000000000000, 0.000000000000000000, 0.000000000000000000 ) ) ;
#155689 = LINE ( 'NONE', #196075, #136576 ) ;
#155690 = VERTEX_POINT ( 'NONE', #122477 ) ;
#155691 = DIRECTION ( 'NONE',  ( -0.000000000000000000, 1.000000000000000000, 0.000000000000000000 ) ) ;
#155692 = CARTESIAN_POINT ( 'NONE',  ( 18.59999999999999076, 11.75000000000000355, -24.85000000000000142 ) ) ;
#155693 = CONICAL_SURFACE ( 'NONE', #255563, 4.049999999999998046, 0.7853981633974604915 ) ;
#155695 = ORIENTED_EDGE ( 'NONE', *, *, #22513, .F. ) ;
#155694 = EDGE_CURVE ( 'NONE', #127618, #132550, #184034, .T. ) ;
#155696 = DIRECTION ( 'NONE',  ( 0.000000000000000000, -0.9126074666063769270, -0.4088369013363280513 ) ) ;
#155697 = DIRECTION ( 'NONE',  ( 0.000000000000000000, -0.8814952561688430555, 0.4721928772777346239 ) ) ;
#155698 = DIRECTION ( 'NONE',  ( 0.000000000000000000, 0.4999999999999543698, 0.8660254037844650199 ) ) ;
#155699 = CIRCLE ( 'NONE', #39169, 0.09999999999999939493 ) ;
#155700 = EDGE_CURVE ( 'NONE', #62294, #60194, #175870, .T. ) ;
#155701 = ORIENTED_EDGE ( 'NONE', *, *, #209888, .T. ) ;
#155702 = DIRECTION ( 'NONE',  ( 0.000000000000000000, 0.000000000000000000, 1.000000000000000000 ) ) ;
#155703 = ORIENTED_EDGE ( 'NONE', *, *, #232165, .F. ) ;
#155704 = ORIENTED_EDGE ( 'NONE', *, *, #138522, .T. ) ;
#155705 = DIRECTION ( 'NONE',  ( -1.000000000000000000, 0.000000000000000000, 0.000000000000000000 ) ) ;
#155707 = VERTEX_POINT ( 'NONE', #45493 ) ;
#155706 = CIRCLE ( 'NONE', #30796, 0.8750000000000007772 ) ;
#155708 = VERTEX_POINT ( 'NONE', #68932 ) ;
#155710 = EDGE_CURVE ( 'NONE', #227674, #100958, #168052, .T. ) ;
#155709 = FACE_OUTER_BOUND ( 'NONE', #35683, .T. ) ;
#155711 = DIRECTION ( 'NONE',  ( 1.000000000000000000, 0.000000000000000000, 0.000000000000000000 ) ) ;
#155712 = EDGE_LOOP ( 'NONE', ( #223217, #174882, #35006 ) ) ;
#155713 = EDGE_LOOP ( 'NONE', ( #244982, #223835, #180387, #54844 ) ) ;
#155714 = CARTESIAN_POINT ( 'NONE',  ( -18.50000000000000000, 1.148907358139439339E-11, -201.0000000000015064 ) ) ;
#155715 = AXIS2_PLACEMENT_3D ( 'NONE', #142151, #101711, #82151 ) ;
#155716 = ADVANCED_FACE ( 'NONE', ( #165457 ), #85871, .T. ) ;
#155717 = AXIS2_PLACEMENT_3D ( 'NONE', #196944, #75737, #93989 ) ;
#155718 = DIRECTION ( 'NONE',  ( 0.000000000000000000, 0.000000000000000000, -1.000000000000000000 ) ) ;
#155719 = AXIS2_PLACEMENT_3D ( 'NONE', #229919, #185655, #109961 ) ;
#155720 = ORIENTED_EDGE ( 'NONE', *, *, #191929, .F. ) ;
#155721 = ADVANCED_FACE ( 'NONE', ( #67619 ), #169766, .T. ) ;
#155722 = ORIENTED_EDGE ( 'NONE', *, *, #144120, .F. ) ;
#155723 = EDGE_CURVE ( 'NONE', #53634, #123588, #205851, .T. ) ;
#155726 = EDGE_CURVE ( 'NONE', #239043, #247011, #105427, .T. ) ;
#155725 = EDGE_CURVE ( 'NONE', #115637, #241027, #238191, .T. ) ;
#155724 = DIRECTION ( 'NONE',  ( 0.000000000000000000, 5.329070518200686707E-15, 1.000000000000000000 ) ) ;
#155727 = DIRECTION ( 'NONE',  ( 0.000000000000000000, 5.880418562633242623E-15, -1.000000000000000000 ) ) ;
#155728 = EDGE_CURVE ( 'NONE', #224530, #56955, #127603, .T. ) ;
#155729 = DIRECTION ( 'NONE',  ( -1.000000000000000000, 2.952720810173289112E-16, 2.061873921506763405E-30 ) ) ;
#155730 = DIRECTION ( 'NONE',  ( -1.000000000000000000, -0.000000000000000000, -0.000000000000000000 ) ) ;
#155731 = FACE_OUTER_BOUND ( 'NONE', #252213, .T. ) ;
#155732 = DIRECTION ( 'NONE',  ( 1.000000000000000000, 2.952720810173289112E-16, -0.000000000000000000 ) ) ;
#155733 = CARTESIAN_POINT ( 'NONE',  ( -21.06715728752538297, 11.74999999999999467, -7.014805770654001904 ) ) ;
#155734 = CIRCLE ( 'NONE', #105601, 0.1000000000000028644 ) ;
#155736 = DIRECTION ( 'NONE',  ( -1.000000000000000000, 0.000000000000000000, -0.000000000000000000 ) ) ;
#155735 = CARTESIAN_POINT ( 'NONE',  ( -16.89268316805466341, 9.951721813242185632, -12.64424752145445296 ) ) ;
#155737 = DIRECTION ( 'NONE',  ( 4.408576920032447355E-17, -0.1350103645451876666, 0.9908441862701600211 ) ) ;
#155738 = DIRECTION ( 'NONE',  ( -0.000000000000000000, -0.000000000000000000, -1.000000000000000000 ) ) ;
#155739 = CARTESIAN_POINT ( 'NONE',  ( 21.14999999999999858, 76.10000000001245724, -181.6726782920691505 ) ) ;
#155741 = CARTESIAN_POINT ( 'NONE',  ( 18.49999999999998934, 15.26077403838592339, -222.9041953915167369 ) ) ;
#155740 = CIRCLE ( 'NONE', #247267, 0.1999999999999987899 ) ;
#155742 = EDGE_CURVE ( 'NONE', #131459, #297, #8939, .T. ) ;
#155743 = EDGE_CURVE ( 'NONE', #223565, #59699, #250661, .T. ) ;
#155744 = VERTEX_POINT ( 'NONE', #46763 ) ;
#155745 = AXIS2_PLACEMENT_3D ( 'NONE', #230942, #50968, #130524 ) ;
#155746 = EDGE_CURVE ( 'NONE', #22920, #18391, #209155, .T. ) ;
#155747 = CIRCLE ( 'NONE', #251569, 0.09999999999999939493 ) ;
#155749 = VERTEX_POINT ( 'NONE', #185008 ) ;
#155748 = CARTESIAN_POINT ( 'NONE',  ( -23.15000000000000213, -8.999999999988844479, -90.60603087734760663 ) ) ;
#155750 = EDGE_CURVE ( 'NONE', #18100, #97476, #96702, .T. ) ;
#155751 = CIRCLE ( 'NONE', #51626, 0.1000000000000072220 ) ;
#155752 = CARTESIAN_POINT ( 'NONE',  ( -22.47120815636973745, 64.15397383650149266, -247.0913167448723868 ) ) ;
#155753 = EDGE_CURVE ( 'NONE', #151091, #146114, #87170, .T. ) ;
#155754 = EDGE_LOOP ( 'NONE', ( #67813, #72441, #214711, #161684, #53856, #209814, #54718, #206340, #143458, #236098, #193477, #164151 ) ) ;
#155755 = CIRCLE ( 'NONE', #105812, 0.1000000000000124678 ) ;
#155756 = CARTESIAN_POINT ( 'NONE',  ( 20.94788355080263997, 10.30207779525983547, -206.4895520716781903 ) ) ;
#155757 = CIRCLE ( 'NONE', #214003, 0.09999999999999939493 ) ;
#155758 = CARTESIAN_POINT ( 'NONE',  ( -16.92209698673480744, 9.950000000011138823, -54.28936443294811198 ) ) ;
#155759 = EDGE_LOOP ( 'NONE', ( #169439, #233515, #92004, #180702 ) ) ;
#155760 = CARTESIAN_POINT ( 'NONE',  ( 21.15000000000005542, 82.64476912853859858, -26.37791261425322986 ) ) ;
#155761 = CARTESIAN_POINT ( 'NONE',  ( -20.64999999999999858, 63.53703427598990316, -222.1606900896233583 ) ) ;
#155762 = EDGE_CURVE ( 'NONE', #203870, #171566, #17605, .T. ) ;
#155763 = CARTESIAN_POINT ( 'NONE',  ( -23.25000000000000000, 1.115600667400684642E-11, -200.9999999999999432 ) ) ;
#155765 = EDGE_LOOP ( 'NONE', ( #255732, #235426, #217260, #183916, #185505 ) ) ;
#155764 = CARTESIAN_POINT ( 'NONE',  ( 18.39999999999997371, 11.47316190337362940, -91.25000000000005684 ) ) ;
#155766 = CIRCLE ( 'NONE', #43329, 0.1000000000000124678 ) ;
#155768 = ORIENTED_EDGE ( 'NONE', *, *, #17054, .T. ) ;
#155767 = DIRECTION ( 'NONE',  ( 1.000000000000000000, 0.000000000000000000, 0.000000000000000000 ) ) ;
#155769 = CARTESIAN_POINT ( 'NONE',  ( -21.05000000000000071, 10.30543449102040476, -228.0143625250146329 ) ) ;
#155770 = CARTESIAN_POINT ( 'NONE',  ( -21.65000000000000213, 7.750000000011155521, -79.35000000000005116 ) ) ;
#155771 = LINE ( 'NONE', #56599, #207412 ) ;
#155772 = CARTESIAN_POINT ( 'NONE',  ( -22.49806830649814060, 55.96728299348496449, -232.8804964729971232 ) ) ;
#155773 = ADVANCED_FACE ( 'NONE', ( #143304 ), #227985, .T. ) ;
#155774 = AXIS2_PLACEMENT_3D ( 'NONE', #61058, #117196, #36398 ) ;
#155776 = CARTESIAN_POINT ( 'NONE',  ( -20.54999999999999716, 2.000000000011154189, -188.1753780772378946 ) ) ;
#155775 = CARTESIAN_POINT ( 'NONE',  ( 18.47654891039377034, 8.940911883994163034, -245.4411313438577054 ) ) ;
#155777 = CARTESIAN_POINT ( 'NONE',  ( -20.64999999999999858, 47.57365439703043108, -242.5355162900727919 ) ) ;
#155778 = CARTESIAN_POINT ( 'NONE',  ( -21.05000000000000071, 64.35000000001234355, -163.2392418215462726 ) ) ;
#155779 = DIRECTION ( 'NONE',  ( 0.000000000000000000, 0.8814952561688438326, -0.4721928772777331251 ) ) ;
#155780 = CARTESIAN_POINT ( 'NONE',  ( 21.05000000000000071, 1.658775325992685845, -230.6916041481568982 ) ) ;
#155781 = VECTOR ( 'NONE', #23606, 1000.000000000000000 ) ;
#155783 = ORIENTED_EDGE ( 'NONE', *, *, #66930, .T. ) ;
#155782 = AXIS2_PLACEMENT_3D ( 'NONE', #49812, #26419, #71958 ) ;
#155784 = CYLINDRICAL_SURFACE ( 'NONE', #93122, 11.80000000000000959 ) ;
#155785 = CIRCLE ( 'NONE', #251435, 0.1000000000000028644 ) ;
#155786 = ORIENTED_EDGE ( 'NONE', *, *, #43192, .F. ) ;
#155787 = EDGE_LOOP ( 'NONE', ( #217565, #193113, #144730, #18140 ) ) ;
#155788 = EDGE_CURVE ( 'NONE', #189474, #61020, #79949, .T. ) ;
#155789 = FACE_OUTER_BOUND ( 'NONE', #54367, .T. ) ;
#155790 = ORIENTED_EDGE ( 'NONE', *, *, #220263, .T. ) ;
#155791 = ORIENTED_EDGE ( 'NONE', *, *, #216778, .T. ) ;
#155792 = CARTESIAN_POINT ( 'NONE',  ( 18.59999999999999076, 54.95667902235472013, -229.8578999281555753 ) ) ;
#155793 = TOROIDAL_SURFACE ( 'NONE', #247340, 0.2000000000000000111, 0.1000000000000000056 ) ;
#155794 = ADVANCED_FACE ( 'NONE', ( #170633 ), #250115, .F. ) ;
#155795 = ORIENTED_EDGE ( 'NONE', *, *, #10687, .F. ) ;
#155796 = AXIS2_PLACEMENT_3D ( 'NONE', #208200, #247295, #126058 ) ;
#155797 = VECTOR ( 'NONE', #113988, 1000.000000000000000 ) ;
#155798 = VERTEX_POINT ( 'NONE', #252662 ) ;
#155799 = DIRECTION ( 'NONE',  ( 0.000000000000000000, 1.000000000000000000, 0.000000000000000000 ) ) ;
#155800 = CARTESIAN_POINT ( 'NONE',  ( 21.05000000000000071, 85.50000000001222134, -146.4170766071767389 ) ) ;
#155801 = FACE_OUTER_BOUND ( 'NONE', #69487, .T. ) ;
#155802 = FACE_OUTER_BOUND ( 'NONE', #79704, .T. ) ;
#155803 = DIRECTION ( 'NONE',  ( 1.000000000000000000, 0.000000000000000000, 0.000000000000000000 ) ) ;
#155804 = CARTESIAN_POINT ( 'NONE',  ( -18.50000000000000000, 64.35000000001174669, -81.27310748452440237 ) ) ;
#155805 = CARTESIAN_POINT ( 'NONE',  ( -21.05000000000000071, 76.10000000001276987, -215.1726782920691505 ) ) ;
#155807 = VERTEX_POINT ( 'NONE', #214825 ) ;
#155806 = DIRECTION ( 'NONE',  ( 1.000000000000000000, 0.000000000000000000, 0.000000000000000000 ) ) ;
#155808 = DIRECTION ( 'NONE',  ( 0.000000000000000000, 7.026728003956695223E-15, -1.000000000000000000 ) ) ;
#155809 = DIRECTION ( 'NONE',  ( 0.000000000000000000, -1.387778780781406043E-13, -1.000000000000000000 ) ) ;
#155810 = ORIENTED_EDGE ( 'NONE', *, *, #176937, .T. ) ;
#155811 = CARTESIAN_POINT ( 'NONE',  ( 21.05000000000000071, 87.65000000001172964, -72.42310748452422331 ) ) ;
#155812 = CYLINDRICAL_SURFACE ( 'NONE', #187436, 0.09999999999999939493 ) ;
#155813 = VERTEX_POINT ( 'NONE', #93605 ) ;
#155814 = CARTESIAN_POINT ( 'NONE',  ( -23.15000000000000213, 64.35000000001156195, -57.37310748452439668 ) ) ;
#155815 = CARTESIAN_POINT ( 'NONE',  ( -18.50000000000000000, 11.75000000001115197, -121.8500000000000369 ) ) ;
#155816 = CARTESIAN_POINT ( 'NONE',  ( 22.57320508075688892, 64.25000000001163869, -69.52310748452440237 ) ) ;
#155817 = ORIENTED_EDGE ( 'NONE', *, *, #102853, .F. ) ;
#155818 = ORIENTED_EDGE ( 'NONE', *, *, #225859, .T. ) ;
#155819 = AXIS2_PLACEMENT_3D ( 'NONE', #36628, #156578, #237365 ) ;
#155820 = FACE_OUTER_BOUND ( 'NONE', #77227, .T. ) ;
#155821 = CARTESIAN_POINT ( 'NONE',  ( -22.45305610364635740, -0.1008583690875579086, -55.25043287651066493 ) ) ;
#155822 = CARTESIAN_POINT ( 'NONE',  ( -20.64999999999999858, 71.65000000001228386, -157.6731074845243938 ) ) ;
#155823 = FACE_OUTER_BOUND ( 'NONE', #49308, .T. ) ;
#155824 = ORIENTED_EDGE ( 'NONE', *, *, #214699, .F. ) ;
#155825 = CARTESIAN_POINT ( 'NONE',  ( 15.70340296795548163, 47.69902910524211137, -234.3535107520372947 ) ) ;
#155826 = EDGE_CURVE ( 'NONE', #156548, #30013, #191461, .T. ) ;
#155827 = CARTESIAN_POINT ( 'NONE',  ( 22.39999999999999503, 7.790779598384535376, -167.4999999999999716 ) ) ;
#155828 = CARTESIAN_POINT ( 'NONE',  ( 18.49999999999999289, 65.70729864261004138, -97.56574559737244101 ) ) ;
#155829 = AXIS2_PLACEMENT_3D ( 'NONE', #117482, #255651, #39248 ) ;
#155830 = CIRCLE ( 'NONE', #43383, 0.09999999999999939493 ) ;
#155831 = DIRECTION ( 'NONE',  ( 1.000000000000000000, 0.000000000000000000, -0.000000000000000000 ) ) ;
#155832 = AXIS2_PLACEMENT_3D ( 'NONE', #130413, #204803, #26200 ) ;
#155833 = AXIS2_PLACEMENT_3D ( 'NONE', #70135, #113085, #90943 ) ;
#155835 = ORIENTED_EDGE ( 'NONE', *, *, #114162, .T. ) ;
#155834 = DIRECTION ( 'NONE',  ( -1.000000000000000000, 0.000000000000000000, 0.000000000000000000 ) ) ;
#155836 = DIRECTION ( 'NONE',  ( 0.000000000000000000, -0.7092521942343630315, -0.7049548389604409770 ) ) ;
#155837 = CARTESIAN_POINT ( 'NONE',  ( -16.89155683852331791, 66.05000000001187743, -89.74573563498417172 ) ) ;
#155838 = SPHERICAL_SURFACE ( 'NONE', #66923, 0.1000000000000000056 ) ;
#155839 = CARTESIAN_POINT ( 'NONE',  ( -18.59999999999999787, 74.16465844978765176, -124.9679561919613207 ) ) ;
#155840 = EDGE_CURVE ( 'NONE', #154676, #47981, #42567, .T. ) ;
#155841 = DIRECTION ( 'NONE',  ( 0.000000000000000000, 6.982962677686266711E-15, -1.000000000000000000 ) ) ;
#155843 = ORIENTED_EDGE ( 'NONE', *, *, #18120, .F. ) ;
#155842 = PLANE ( 'NONE',  #127612 ) ;
#155844 = CARTESIAN_POINT ( 'NONE',  ( -18.50000000000000000, 0.6770221356676882074, -212.8807256103264649 ) ) ;
#155845 = DIRECTION ( 'NONE',  ( 0.000000000000000000, 0.000000000000000000, -1.000000000000000000 ) ) ;
#155846 = CARTESIAN_POINT ( 'NONE',  ( -23.25000000000000000, 76.00000000001162448, -65.47310748452431994 ) ) ;
#155847 = EDGE_CURVE ( 'NONE', #44396, #137285, #196682, .T. ) ;
#155848 = VERTEX_POINT ( 'NONE', #153635 ) ;
#155849 = CARTESIAN_POINT ( 'NONE',  ( -22.39999999999999858, 76.10000000001174669, -81.17267829206912211 ) ) ;
#155850 = CARTESIAN_POINT ( 'NONE',  ( -21.44999999999999929, 45.00644278977874535, -237.9768835835062077 ) ) ;
#155851 = FACE_OUTER_BOUND ( 'NONE', #1557, .T. ) ;
#155852 = DIRECTION ( 'NONE',  ( 0.000000000000000000, 0.2617529984164915779, 0.9651348961777189706 ) ) ;
#155853 = CIRCLE ( 'NONE', #210007, 4.049999999999974953 ) ;
#155854 = LINE ( 'NONE', #100937, #234048 ) ;
#155855 = EDGE_CURVE ( 'NONE', #78078, #23345, #221615, .T. ) ;
#155856 = VECTOR ( 'NONE', #202944, 1000.000000000000000 ) ;
#155857 = DIRECTION ( 'NONE',  ( 0.000000000000000000, 0.9770955615653317272, 0.2128009952263598126 ) ) ;
#155859 = ORIENTED_EDGE ( 'NONE', *, *, #26730, .T. ) ;
#155858 = AXIS2_PLACEMENT_3D ( 'NONE', #10671, #221023, #204985 ) ;
#155860 = ORIENTED_EDGE ( 'NONE', *, *, #5272, .T. ) ;
#155861 = TOROIDAL_SURFACE ( 'NONE', #243301, 0.4000000000000012990, 0.1000000000000000056 ) ;
#155862 = EDGE_CURVE ( 'NONE', #194241, #79556, #213243, .T. ) ;
#155863 = CARTESIAN_POINT ( 'NONE',  ( 22.00356870067119175, -1.543709994167115740, -193.9119119857884073 ) ) ;
#155865 = DIRECTION ( 'NONE',  ( 1.000000000000000000, 0.000000000000000000, 0.000000000000000000 ) ) ;
#155864 = VECTOR ( 'NONE', #159385, 1000.000000000000000 ) ;
#155866 = ADVANCED_FACE ( 'NONE', ( #171898 ), #5124, .T. ) ;
#155867 = FACE_OUTER_BOUND ( 'NONE', #254798, .T. ) ;
#155868 = CARTESIAN_POINT ( 'NONE',  ( -20.00857864376270001, 9.350000000011156942, -188.7499999999999716 ) ) ;
#155869 = EDGE_CURVE ( 'NONE', #206400, #73136, #234270, .T. ) ;
#155870 = DIRECTION ( 'NONE',  ( 0.000000000000000000, 0.9908441862701782288, -0.1350103645450542456 ) ) ;
#155871 = VECTOR ( 'NONE', #32982, 1000.000000000000000 ) ;
#155872 = AXIS2_PLACEMENT_3D ( 'NONE', #196916, #200773, #139502 ) ;
#155873 = CARTESIAN_POINT ( 'NONE',  ( 20.58091095332355280, 10.60340429618756275, -207.3066863033071456 ) ) ;
#155874 = TOROIDAL_SURFACE ( 'NONE', #47684, 12.97499999999999609, 0.1000000000000000056 ) ;
#155875 = ADVANCED_FACE ( 'NONE', ( #233147 ), #132754, .T. ) ;
#155876 = CARTESIAN_POINT ( 'NONE',  ( -16.77779411503079032, 9.946101446924121348, -12.66305741761983406 ) ) ;
#155877 = AXIS2_PLACEMENT_3D ( 'NONE', #203728, #223272, #99461 ) ;
#155878 = DIRECTION ( 'NONE',  ( 1.000000000000000000, -0.000000000000000000, 0.000000000000000000 ) ) ;
#155879 = ORIENTED_EDGE ( 'NONE', *, *, #51935, .F. ) ;
#155880 = DIRECTION ( 'NONE',  ( 1.000000000000000000, 0.000000000000000000, 0.000000000000000000 ) ) ;
#155881 = CIRCLE ( 'NONE', #68566, 0.1000000000000016986 ) ;
#155882 = ORIENTED_EDGE ( 'NONE', *, *, #135621, .F. ) ;
#155883 = ORIENTED_EDGE ( 'NONE', *, *, #132597, .T. ) ;
#155884 = CARTESIAN_POINT ( 'NONE',  ( 21.07928932188134397, 75.90110485435802445, -176.3516241409176644 ) ) ;
#155885 = CARTESIAN_POINT ( 'NONE',  ( -17.11825945287482753, 65.95000000001188312, -90.37310748452438247 ) ) ;
#155886 = DIRECTION ( 'NONE',  ( 0.000000000000000000, 0.000000000000000000, 1.000000000000000000 ) ) ;
#155887 = ORIENTED_EDGE ( 'NONE', *, *, #44573, .F. ) ;
#155889 = AXIS2_PLACEMENT_3D ( 'NONE', #129958, #127417, #28354 ) ;
#155888 = LINE ( 'NONE', #17614, #140612 ) ;
#155890 = CARTESIAN_POINT ( 'NONE',  ( -21.05000000000000071, 5.850000000011105428, -177.6324972242779268 ) ) ;
#155891 = CARTESIAN_POINT ( 'NONE',  ( -16.80117486205003630, 30.20515730058129833, -234.8068064003087159 ) ) ;
#155892 = AXIS2_PLACEMENT_3D ( 'NONE', #123849, #144668, #104250 ) ;
#155893 = ORIENTED_EDGE ( 'NONE', *, *, #68626, .F. ) ;
#155894 = EDGE_CURVE ( 'NONE', #23148, #116019, #63592, .T. ) ;
#155896 = CARTESIAN_POINT ( 'NONE',  ( -12.42749937872396515, 9.370689921613767126, -151.5264651266610656 ) ) ;
#155895 = AXIS2_PLACEMENT_3D ( 'NONE', #128908, #29831, #109314 ) ;
#155898 = VERTEX_POINT ( 'NONE', #91041 ) ;
#155897 = CARTESIAN_POINT ( 'NONE',  ( 21.14999999999999858, 76.00000000001156764, -57.37310748452432563 ) ) ;
#155899 = LINE ( 'NONE', #51594, #214955 ) ;
#155900 = CARTESIAN_POINT ( 'NONE',  ( -18.45037301276615693, 85.49020044755471304, -163.0104333481092453 ) ) ;
#155901 = EDGE_LOOP ( 'NONE', ( #227206, #251895, #228587, #133227 ) ) ;
#155902 = CARTESIAN_POINT ( 'NONE',  ( 21.03670563405601968, 65.37517631068435264, -191.1975605983152775 ) ) ;
#155904 = EDGE_CURVE ( 'NONE', #128410, #34141, #188499, .T. ) ;
#155903 = CARTESIAN_POINT ( 'NONE',  ( -1.739115166359751801E-14, 64.35000000001149090, -44.67310748452440095 ) ) ;
#155905 = EDGE_LOOP ( 'NONE', ( #125909, #143656, #118791, #129305 ) ) ;
#155906 = DIRECTION ( 'NONE',  ( 0.000000000000000000, 0.000000000000000000, -1.000000000000000000 ) ) ;
#155907 = AXIS2_PLACEMENT_3D ( 'NONE', #73173, #152712, #133119 ) ;
#155908 = ORIENTED_EDGE ( 'NONE', *, *, #107045, .F. ) ;
#155909 = CARTESIAN_POINT ( 'NONE',  ( -18.59999999999999787, 42.15997144203495139, -239.2817429668763793 ) ) ;
#155910 = CIRCLE ( 'NONE', #43463, 11.75000000000001066 ) ;
#155912 = ORIENTED_EDGE ( 'NONE', *, *, #48179, .T. ) ;
#155911 = AXIS2_PLACEMENT_3D ( 'NONE', #944, #41418, #238302 ) ;
#155913 = EDGE_CURVE ( 'NONE', #78593, #194417, #134008, .T. ) ;
#155914 = CIRCLE ( 'NONE', #218222, 4.150000000000001243 ) ;
#155915 = AXIS2_PLACEMENT_3D ( 'NONE', #252585, #231765, #229196 ) ;
#155916 = VERTEX_POINT ( 'NONE', #213539 ) ;
#155917 = CARTESIAN_POINT ( 'NONE',  ( 20.94999999999999574, 69.65000000001231228, -160.1792853948412869 ) ) ;
#155918 = DIRECTION ( 'NONE',  ( 0.000000000000000000, -2.428612866367527723E-14, -1.000000000000000000 ) ) ;
#155921 = ADVANCED_FACE ( 'NONE', ( #253943 ), #43303, .T. ) ;
#155920 = VERTEX_POINT ( 'NONE', #114453 ) ;
#155919 = DIRECTION ( 'NONE',  ( -0.000000000000000000, 0.1298341882520022694, 0.9915357197604853789 ) ) ;
#155922 = CARTESIAN_POINT ( 'NONE',  ( -20.64999999999999858, 1.115600667400684642E-11, -135.9000000000000625 ) ) ;
#155924 = AXIS2_PLACEMENT_3D ( 'NONE', #218358, #39779, #119292 ) ;
#155923 = FACE_OUTER_BOUND ( 'NONE', #46952, .T. ) ;
#155925 = FACE_OUTER_BOUND ( 'NONE', #13610, .T. ) ;
#155926 = LINE ( 'NONE', #235418, #6032 ) ;
#155927 = LINE ( 'NONE', #112926, #150388 ) ;
#155928 = VECTOR ( 'NONE', #193581, 1000.000000000000000 ) ;
#155929 = EDGE_CURVE ( 'NONE', #79905, #164965, #221791, .T. ) ;
#155930 = SPHERICAL_SURFACE ( 'NONE', #151332, 0.1000000000000000056 ) ;
#155931 = DIRECTION ( 'NONE',  ( 0.000000000000000000, 0.000000000000000000, 1.000000000000000000 ) ) ;
#155932 = EDGE_CURVE ( 'NONE', #97404, #98428, #19201, .T. ) ;
#155934 = ORIENTED_EDGE ( 'NONE', *, *, #249011, .T. ) ;
#155933 = FACE_OUTER_BOUND ( 'NONE', #175105, .T. ) ;
#155936 = VERTEX_POINT ( 'NONE', #197828 ) ;
#155935 = CARTESIAN_POINT ( 'NONE',  ( -18.59999999999999787, 16.44800918141279311, -240.8068063186265135 ) ) ;
#155938 = CARTESIAN_POINT ( 'NONE',  ( -16.97683809663752186, 50.93224991157929793, -232.2540631895259082 ) ) ;
#155937 = CARTESIAN_POINT ( 'NONE',  ( -16.89318236219976299, 60.93653333852449805, -221.0462766641838357 ) ) ;
#155939 = AXIS2_PLACEMENT_3D ( 'NONE', #121778, #4364, #240423 ) ;
#155941 = VERTEX_POINT ( 'NONE', #80416 ) ;
#155940 = CARTESIAN_POINT ( 'NONE',  ( -20.54999999999999716, 71.65000000001155911, -57.17310748452435121 ) ) ;
#155942 = VERTEX_POINT ( 'NONE', #119607 ) ;
#155943 = CARTESIAN_POINT ( 'NONE',  ( 18.59999999999999076, 74.75000000001206502, -128.5231074845243029 ) ) ;
#155944 = DIRECTION ( 'NONE',  ( 0.000000000000000000, 0.2617529984164856383, 0.9651348961777204138 ) ) ;
#155945 = AXIS2_PLACEMENT_3D ( 'NONE', #54293, #230375, #115557 ) ;
#155947 = EDGE_CURVE ( 'NONE', #113546, #149556, #151099, .T. ) ;
#155946 = DIRECTION ( 'NONE',  ( 0.000000000000000000, 1.776356839400306474E-15, 1.000000000000000000 ) ) ;
#155948 = CARTESIAN_POINT ( 'NONE',  ( 19.97071067811865674, 11.72071067812981937, -58.15000000000000568 ) ) ;
#155949 = CARTESIAN_POINT ( 'NONE',  ( 21.15000000000005187, 83.90000000001120384, -34.77310748452479316 ) ) ;
#155950 = AXIS2_PLACEMENT_3D ( 'NONE', #41026, #137511, #235336 ) ;
#155951 = CARTESIAN_POINT ( 'NONE',  ( 21.14999999999999503, -11.64999999998883595, -155.7499999999999716 ) ) ;
#155952 = AXIS2_PLACEMENT_3D ( 'NONE', #21645, #239405, #42474 ) ;
#155953 = ORIENTED_EDGE ( 'NONE', *, *, #30268, .T. ) ;
#155954 = VERTEX_POINT ( 'NONE', #240825 ) ;
#155955 = DIRECTION ( 'NONE',  ( 0.000000000000000000, 0.000000000000000000, 1.000000000000000000 ) ) ;
#155956 = ORIENTED_EDGE ( 'NONE', *, *, #80620, .T. ) ;
#155957 = DIRECTION ( 'NONE',  ( 0.000000000000000000, 0.000000000000000000, -1.000000000000000000 ) ) ;
#155959 = AXIS2_PLACEMENT_3D ( 'NONE', #15583, #191661, #37711 ) ;
#155958 = CARTESIAN_POINT ( 'NONE',  ( -16.91049119928364775, 51.64781119986088243, -231.9335005483882810 ) ) ;
#155960 = VECTOR ( 'NONE', #214702, 1000.000000000000114 ) ;
#155961 = DIRECTION ( 'NONE',  ( -1.000000000000000000, -0.000000000000000000, -0.000000000000000000 ) ) ;
#155962 = CARTESIAN_POINT ( 'NONE',  ( -18.50000000000000000, -1.835341550224411922, -11.55515129256297868 ) ) ;
#155963 = ORIENTED_EDGE ( 'NONE', *, *, #80897, .F. ) ;
#155964 = CARTESIAN_POINT ( 'NONE',  ( -14.45422546970484312, 66.54939790392351995, -118.0792115214276947 ) ) ;
#155965 = ADVANCED_FACE ( 'NONE', ( #117020 ), #109377, .T. ) ;
#155966 = ORIENTED_EDGE ( 'NONE', *, *, #125705, .F. ) ;
#155967 = EDGE_CURVE ( 'NONE', #223991, #106564, #217382, .T. ) ;
#155968 = CYLINDRICAL_SURFACE ( 'NONE', #83841, 11.74999999999999645 ) ;
#155969 = ORIENTED_EDGE ( 'NONE', *, *, #22070, .T. ) ;
#155970 = FACE_OUTER_BOUND ( 'NONE', #120510, .T. ) ;
#155971 = DIRECTION ( 'NONE',  ( 0.000000000000000000, -7.272083257015735086E-15, 1.000000000000000000 ) ) ;
#155972 = DIRECTION ( 'NONE',  ( -1.000000000000000000, 0.000000000000000000, 0.000000000000000000 ) ) ;
#155973 = EDGE_LOOP ( 'NONE', ( #76699, #9752, #250848, #137571 ) ) ;
#155974 = DIRECTION ( 'NONE',  ( 0.000000000000000000, 1.000000000000000000, 0.000000000000000000 ) ) ;
#155976 = ORIENTED_EDGE ( 'NONE', *, *, #90985, .F. ) ;
#155975 = FACE_OUTER_BOUND ( 'NONE', #102547, .T. ) ;
#155977 = CARTESIAN_POINT ( 'NONE',  ( 23.40000000000005542, 66.40137734081807253, -35.02137779515522453 ) ) ;
#155978 = ORIENTED_EDGE ( 'NONE', *, *, #104546, .F. ) ;
#155979 = ORIENTED_EDGE ( 'NONE', *, *, #133816, .T. ) ;
#155980 = AXIS2_PLACEMENT_3D ( 'NONE', #111891, #193998, #113159 ) ;
#155982 = CARTESIAN_POINT ( 'NONE',  ( -21.14999999999994174, 83.98667523412385094, -34.76145429838185663 ) ) ;
#155981 =( BOUNDED_SURFACE ( )  B_SPLINE_SURFACE ( 3, 2, ( 
 ( #223463, #200070, #164797 ),
 ( #100914, #244311, #205183 ),
 ( #1837, #106068, #81365 ),
 ( #240474, #42284, #30432 ) ),
 .UNSPECIFIED., .F., .F., .F. ) 
 B_SPLINE_SURFACE_WITH_KNOTS ( ( 4, 4 ),
 ( 3, 3 ),
 ( 3.658908243880847788, 4.712388980384689674 ),
 ( 0.000000000000000000, 1.000000000000000000 ),
 .UNSPECIFIED. ) 
 GEOMETRIC_REPRESENTATION_ITEM ( )  RATIONAL_B_SPLINE_SURFACE ( (
 ( 1.000000000000000000, 0.8984936768950640973, 1.000000000000000000),
 ( 1.000000000000000000, 0.8646876308616019413, 1.000000000000000000),
 ( 1.000000000000000000, 0.7953136715913022847, 1.000000000000000000),
 ( 1.000000000000000000, 0.7071067811865475727, 1.000000000000000000) ) ) 
 REPRESENTATION_ITEM ( '' )  SURFACE ( )  );
#155983 = ORIENTED_EDGE ( 'NONE', *, *, #243211, .T. ) ;
#155984 = DIRECTION ( 'NONE',  ( 1.000000000000000000, 0.000000000000000000, 0.000000000000000000 ) ) ;
#155985 = CARTESIAN_POINT ( 'NONE',  ( 21.09096482362065217, 69.63645563460735843, -69.56255576329859025 ) ) ;
#155986 = CARTESIAN_POINT ( 'NONE',  ( 22.48660254037844197, 11.65000000001116298, -100.4500000000000455 ) ) ;
#155987 = CARTESIAN_POINT ( 'NONE',  ( 18.49999999999998934, 67.49462292596862767, -195.5612049585272700 ) ) ;
#155988 = CARTESIAN_POINT ( 'NONE',  ( -18.59999999999999787, 76.00000000001136868, -28.12310748452432208 ) ) ;
#155989 = VERTEX_POINT ( 'NONE', #98693 ) ;
#155990 = DIRECTION ( 'NONE',  ( -1.000000000000000000, 0.000000000000000000, 0.000000000000000000 ) ) ;
#155991 = DIRECTION ( 'NONE',  ( -0.000000000000000000, -0.2606175937107957918, 0.9654421110809259243 ) ) ;
#155992 = DIRECTION ( 'NONE',  ( 1.073024830501117725E-15, 0.000000000000000000, 1.000000000000000000 ) ) ;
#155993 = EDGE_CURVE ( 'NONE', #225819, #33564, #140419, .T. ) ;
#155994 = ORIENTED_EDGE ( 'NONE', *, *, #159691, .F. ) ;
#155995 = CARTESIAN_POINT ( 'NONE',  ( -21.44999999999999929, 7.250000000011155521, -45.85000000000000142 ) ) ;
#155996 = VERTEX_POINT ( 'NONE', #76601 ) ;
#155997 = DIRECTION ( 'NONE',  ( -1.000000000000000000, 0.000000000000000000, 0.000000000000000000 ) ) ;
#155998 = ORIENTED_EDGE ( 'NONE', *, *, #166110, .F. ) ;
#155999 = AXIS2_PLACEMENT_3D ( 'NONE', #187050, #206584, #244420 ) ;
#156000 = CYLINDRICAL_SURFACE ( 'NONE', #93366, 12.87499999999999822 ) ;
#156001 = CARTESIAN_POINT ( 'NONE',  ( -21.37071067811865532, 67.92928932189285263, -48.37310748452437537 ) ) ;
#156004 = VERTEX_POINT ( 'NONE', #178303 ) ;
#156003 = ADVANCED_FACE ( 'NONE', ( #16650 ), #216107, .T. ) ;
#156002 = DIRECTION ( 'NONE',  ( 1.000000000000000000, 0.000000000000000000, 0.000000000000000000 ) ) ;
#156005 = DIRECTION ( 'NONE',  ( 0.000000000000000000, -0.2617529984165031243, -0.9651348961777157509 ) ) ;
#156006 = EDGE_LOOP ( 'NONE', ( #25537, #45101, #240168, #140779 ) ) ;
#156007 = CARTESIAN_POINT ( 'NONE',  ( -18.59999999999999787, 36.65892442174935439, -249.5511627012433848 ) ) ;
#156008 = ADVANCED_FACE ( 'NONE', ( #58304 ), #96149, .F. ) ;
#156009 = CARTESIAN_POINT ( 'NONE',  ( 23.14999999999999858, 1.115600667400684642E-11, -67.00000000000000000 ) ) ;
#156010 = ORIENTED_EDGE ( 'NONE', *, *, #198342, .F. ) ;
#156011 = CARTESIAN_POINT ( 'NONE',  ( 21.05000000000000071, 8.299331953467152800, -209.2670685529822663 ) ) ;
#156013 = EDGE_CURVE ( 'NONE', #197068, #230546, #184209, .T. ) ;
#156012 = CARTESIAN_POINT ( 'NONE',  ( -20.85000000000000142, 11.75000000001115197, -194.2161343370218560 ) ) ;
#156014 = ORIENTED_EDGE ( 'NONE', *, *, #164606, .T. ) ;
#156016 = CARTESIAN_POINT ( 'NONE',  ( 21.11833042828145324, 10.16616178894255107, -228.0475432820529136 ) ) ;
#156015 = CIRCLE ( 'NONE', #114292, 0.09999999999999939493 ) ;
#156017 = AXIS2_PLACEMENT_3D ( 'NONE', #191860, #92710, #11927 ) ;
#156018 = ORIENTED_EDGE ( 'NONE', *, *, #182744, .F. ) ;
#156019 = VECTOR ( 'NONE', #161563, 1000.000000000000000 ) ;
#156020 = CIRCLE ( 'NONE', #181148, 2.000000000000002665 ) ;
#156021 = EDGE_CURVE ( 'NONE', #150811, #147068, #96879, .T. ) ;
#156023 = EDGE_CURVE ( 'NONE', #169719, #62507, #180852, .T. ) ;
#156022 = CARTESIAN_POINT ( 'NONE',  ( 18.57071067811864040, 30.66719544722269220, -234.7938047061825841 ) ) ;
#156025 = VERTEX_POINT ( 'NONE', #42615 ) ;
#156024 = CYLINDRICAL_SURFACE ( 'NONE', #105484, 0.1000000000000000472 ) ;
#156026 = LINE ( 'NONE', #213393, #41463 ) ;
#156027 = DIRECTION ( 'NONE',  ( 1.875376730785737719E-16, -1.000000000000000000, 0.000000000000000000 ) ) ;
#156028 = FACE_OUTER_BOUND ( 'NONE', #245162, .T. ) ;
#156029 = VECTOR ( 'NONE', #93702, 1000.000000000000000 ) ;
#156031 = CARTESIAN_POINT ( 'NONE',  ( -22.48479450179659977, 75.95300841882557563, -181.6731059307759608 ) ) ;
#156030 = CARTESIAN_POINT ( 'NONE',  ( -17.04761207306819770, 63.01194694731475465, -213.1076103415853993 ) ) ;
#156032 = CARTESIAN_POINT ( 'NONE',  ( 22.48660254037844197, 64.35000000001237197, -170.0731074845244279 ) ) ;
#156033 = CARTESIAN_POINT ( 'NONE',  ( -18.40000000000000213, 5.650000000011139001, -54.35000000000000142 ) ) ;
#156034 = CARTESIAN_POINT ( 'NONE',  ( -23.25000000000000355, 70.35000000001181775, -82.17310748452435121 ) ) ;
#156035 = CIRCLE ( 'NONE', #226740, 1.500000000000001332 ) ;
#156036 = CARTESIAN_POINT ( 'NONE',  ( -21.33487959338958362, 69.27444184810096317, -136.5231074845243313 ) ) ;
#156037 = EDGE_CURVE ( 'NONE', #125487, #72763, #9428, .T. ) ;
#156038 = ADVANCED_FACE ( 'NONE', ( #889 ), #120902, .T. ) ;
#156039 = CIRCLE ( 'NONE', #27054, 0.1000000000000078465 ) ;
#156040 = EDGE_LOOP ( 'NONE', ( #147297, #176105, #154811, #73929, #99813, #58063, #119065, #86538, #82196, #109902 ) ) ;
#156041 = ORIENTED_EDGE ( 'NONE', *, *, #252797, .F. ) ;
#156042 = VECTOR ( 'NONE', #146666, 1000.000000000000000 ) ;
#156043 = DIRECTION ( 'NONE',  ( -1.000000000000000000, -7.136802563874199107E-16, -1.554319503706929991E-16 ) ) ;
#156044 = AXIS2_PLACEMENT_3D ( 'NONE', #139482, #42977, #181213 ) ;
#156046 = ORIENTED_EDGE ( 'NONE', *, *, #226378, .T. ) ;
#156045 = CARTESIAN_POINT ( 'NONE',  ( -23.15000000000000213, 87.75000000001192291, -106.1231074845242262 ) ) ;
#156047 = EDGE_LOOP ( 'NONE', ( #122053, #117693, #178767, #53747 ) ) ;
#156048 = EDGE_CURVE ( 'NONE', #177022, #104140, #141706, .T. ) ;
#156049 = LINE ( 'NONE', #235544, #139537 ) ;
#156050 = ORIENTED_EDGE ( 'NONE', *, *, #126357, .T. ) ;
#156051 = CARTESIAN_POINT ( 'NONE',  ( 20.94999999999999574, 8.926614585087095932, -8.471683019223121391 ) ) ;
#156052 =( BOUNDED_SURFACE ( )  B_SPLINE_SURFACE ( 3, 2, ( 
 ( #166357, #149352, #245861 ),
 ( #223708, #8534, #228868 ),
 ( #50206, #67218, #184594 ),
 ( #146728, #88036, #226264 ),
 ( #5937, #85459, #247127 ),
 ( #47630, #127200, #107623 ) ),
 .UNSPECIFIED., .F., .F., .F. ) 
 B_SPLINE_SURFACE_WITH_KNOTS ( ( 4, 2, 4 ),
 ( 3, 3 ),
 ( 3.141592653589793116, 3.926990816987241395, 4.712388980384689674 ),
 ( 0.000000000000000000, 1.000000000000000000 ),
 .UNSPECIFIED. ) 
 GEOMETRIC_REPRESENTATION_ITEM ( )  RATIONAL_B_SPLINE_SURFACE ( (
 ( 1.000000000000000000, 0.9238795325112820755, 1.000000000000000000),
 ( 1.000000000000000000, 0.9240297172248476132, 1.000000000000000000),
 ( 1.000000000000000000, 0.9038128468032942120, 1.000000000000000000),
 ( 1.000000000000000000, 0.8282379607655763198, 1.000000000000000000),
 ( 1.000000000000000000, 0.7727932973486544288, 1.000000000000000000),
 ( 1.000000000000000000, 0.7071067811865475727, 1.000000000000000000) ) ) 
 REPRESENTATION_ITEM ( '' )  SURFACE ( )  );
#156053 = AXIS2_PLACEMENT_3D ( 'NONE', #156217, #230604, #151064 ) ;
#156054 = CIRCLE ( 'NONE', #214302, 0.09999999999999949207 ) ;
#156055 = EDGE_CURVE ( 'NONE', #226018, #242431, #142687, .T. ) ;
#156056 = ORIENTED_EDGE ( 'NONE', *, *, #235817, .F. ) ;
#156057 = AXIS2_PLACEMENT_3D ( 'NONE', #91771, #34390, #231298 ) ;
#156058 =( NAMED_UNIT ( * ) SI_UNIT ( $, .STERADIAN. ) SOLID_ANGLE_UNIT ( ) );
#156059 = DIRECTION ( 'NONE',  ( 0.000000000000000000, 0.000000000000000000, 1.000000000000000000 ) ) ;
#156060 = ADVANCED_FACE ( 'NONE', ( #67307 ), #3477, .F. ) ;
#156061 = AXIS2_PLACEMENT_3D ( 'NONE', #220720, #42107, #182895 ) ;
#156063 = VERTEX_POINT ( 'NONE', #106411 ) ;
#156062 = VERTEX_POINT ( 'NONE', #86853 ) ;
#156064 = VERTEX_POINT ( 'NONE', #103849 ) ;
#156065 = ORIENTED_EDGE ( 'NONE', *, *, #69135, .T. ) ;
#156066 = ORIENTED_EDGE ( 'NONE', *, *, #140428, .T. ) ;
#156067 = DIRECTION ( 'NONE',  ( 0.000000000000000000, -0.8660254037844411501, -0.4999999999999956701 ) ) ;
#156068 = CYLINDRICAL_SURFACE ( 'NONE', #125978, 0.09999999999999939493 ) ;
#156070 = ORIENTED_EDGE ( 'NONE', *, *, #234699, .T. ) ;
#156069 = CARTESIAN_POINT ( 'NONE',  ( 23.14999999999999503, 13.96869538424789070, -210.3925794786331949 ) ) ;
#156071 = DIRECTION ( 'NONE',  ( 0.000000000000000000, 0.000000000000000000, -1.000000000000000000 ) ) ;
#156072 = EDGE_CURVE ( 'NONE', #39363, #123093, #176062, .T. ) ;
#156073 = CARTESIAN_POINT ( 'NONE',  ( -18.50000000000000000, 7.128833340093095217, -233.7327013124392749 ) ) ;
#156075 = ORIENTED_EDGE ( 'NONE', *, *, #1970, .T. ) ;
#156074 = DIRECTION ( 'NONE',  ( 1.000000000000000000, 0.000000000000000000, 0.000000000000000000 ) ) ;
#156076 = CARTESIAN_POINT ( 'NONE',  ( 19.97071067811864609, 54.36283943849028333, -228.7769250045207912 ) ) ;
#156077 = ORIENTED_EDGE ( 'NONE', *, *, #126553, .F. ) ;
#156078 = CIRCLE ( 'NONE', #130916, 0.09999999999999939493 ) ;
#156079 = CARTESIAN_POINT ( 'NONE',  ( 20.95512820512820440, 8.876151316299271343, -176.0586289951409071 ) ) ;
#156080 = AXIS2_PLACEMENT_3D ( 'NONE', #19289, #115824, #38867 ) ;
#156082 = ORIENTED_EDGE ( 'NONE', *, *, #21750, .F. ) ;
#156081 = DIRECTION ( 'NONE',  ( 1.000000000000000000, 0.000000000000000000, 0.000000000000000000 ) ) ;
#156083 = DIRECTION ( 'NONE',  ( 0.000000000000000000, 0.000000000000000000, 1.000000000000000000 ) ) ;
#156084 = CARTESIAN_POINT ( 'NONE',  ( -16.90202395485750841, 9.965944544562109542, -113.0969862787403457 ) ) ;
#156085 = DIRECTION ( 'NONE',  ( -1.000000000000000000, 0.000000000000000000, -0.000000000000000000 ) ) ;
#156087 = EDGE_CURVE ( 'NONE', #73216, #154893, #166452, .T. ) ;
#156086 = ORIENTED_EDGE ( 'NONE', *, *, #30875, .F. ) ;
#156089 = CARTESIAN_POINT ( 'NONE',  ( 20.94999999999999929, 9.006788119787323410, -211.5755741104441654 ) ) ;
#156088 = CARTESIAN_POINT ( 'NONE',  ( -16.77431908686106610, 9.945805754529134290, -46.16416078234976084 ) ) ;
#156090 = DIRECTION ( 'NONE',  ( 0.000000000000000000, 0.000000000000000000, -1.000000000000000000 ) ) ;
#156091 = CYLINDRICAL_SURFACE ( 'NONE', #47301, 0.1000000000000013933 ) ;
#156092 = DIRECTION ( 'NONE',  ( 0.7070776581708965169, 0.000000000000000000, 0.7071359030027827286 ) ) ;
#156093 = ORIENTED_EDGE ( 'NONE', *, *, #237427, .F. ) ;
#156094 = ORIENTED_EDGE ( 'NONE', *, *, #209631, .T. ) ;
#156095 =( BOUNDED_SURFACE ( )  B_SPLINE_SURFACE ( 3, 2, ( 
 ( #104265, #203396, #145970 ),
 ( #221646, #45602, #27364 ),
 ( #62600, #125148, #182561 ),
 ( #243797, #43040, #181281 ),
 ( #246370, #183822, #225489 ),
 ( #143410, #126412, #3905 ) ),
 .UNSPECIFIED., .F., .F., .F. ) 
 B_SPLINE_SURFACE_WITH_KNOTS ( ( 4, 2, 4 ),
 ( 3, 3 ),
 ( 0.0001342700090130150253, 0.0002909192928057470397, 0.0004475685765984790000 ),
 ( 0.000000000000000000, 1.000000000000000000 ),
 .UNSPECIFIED. ) 
 GEOMETRIC_REPRESENTATION_ITEM ( )  RATIONAL_B_SPLINE_SURFACE ( (
 ( 1.000000000000000000, 0.7250110520819876836, 1.000000000000000000),
 ( 1.000000000000000000, 0.7257599279136393022, 1.000000000000000000),
 ( 1.000000000000000000, 0.7137594617280778042, 1.000000000000000000),
 ( 1.000000000000000000, 0.6959270178813201646, 1.000000000000000000),
 ( 1.000000000000000000, 0.6919879549336147573, 1.000000000000000000),
 ( 1.000000000000000000, 0.7071067811865475727, 1.000000000000000000) ) ) 
 REPRESENTATION_ITEM ( '' )  SURFACE ( )  );
#156096 = CARTESIAN_POINT ( 'NONE',  ( -20.85000000000000142, -1.164121893230052995, -141.7148480855716457 ) ) ;
#156097 = CARTESIAN_POINT ( 'NONE',  ( -23.15000000000000213, 11.65000000001115588, -146.1500000000000341 ) ) ;
#156098 = VERTEX_POINT ( 'NONE', #144255 ) ;
#156099 = DIRECTION ( 'NONE',  ( 0.000000000000000000, -0.9910465087640866200, -0.1335171055202867274 ) ) ;
#156100 = ORIENTED_EDGE ( 'NONE', *, *, #95501, .F. ) ;
#156101 = EDGE_CURVE ( 'NONE', #192851, #164178, #88523, .T. ) ;
#156102 = DIRECTION ( 'NONE',  ( -0.000000000000000000, 0.9770955615653313941, 0.2128009952263603677 ) ) ;
#156103 = DIRECTION ( 'NONE',  ( 0.000000000000000000, 0.9126074666063545004, 0.4088369013363783999 ) ) ;
#156104 = CIRCLE ( 'NONE', #127033, 0.09999999999999939493 ) ;
#156105 = VERTEX_POINT ( 'NONE', #184681 ) ;
#156106 = DIRECTION ( 'NONE',  ( -1.000000000000000000, 0.000000000000000000, 0.000000000000000000 ) ) ;
#156107 = SURFACE_STYLE_FILL_AREA ( #16583 ) ;
#156108 = AXIS2_PLACEMENT_3D ( 'NONE', #84012, #3225, #180604 ) ;
#156109 = ORIENTED_EDGE ( 'NONE', *, *, #14510, .F. ) ;
#156110 = VERTEX_POINT ( 'NONE', #223806 ) ;
#156111 = ORIENTED_EDGE ( 'NONE', *, *, #89306, .T. ) ;
#156112 = LINE ( 'NONE', #174413, #237567 ) ;
#156113 = CARTESIAN_POINT ( 'NONE',  ( 13.12220780326572012, 66.56936653093875123, -54.29134168970031737 ) ) ;
#156114 = VECTOR ( 'NONE', #129767, 1000.000000000000000 ) ;
#156115 = DIRECTION ( 'NONE',  ( -1.000000000000000000, 0.000000000000000000, -0.000000000000000000 ) ) ;
#156116 = CARTESIAN_POINT ( 'NONE',  ( 20.94999999999999929, 69.35000000001186038, -90.87310748452435405 ) ) ;
#156117 = CARTESIAN_POINT ( 'NONE',  ( 12.25000000000000000, 66.65000000001205649, -119.6588398769083312 ) ) ;
#156119 = CARTESIAN_POINT ( 'NONE',  ( -16.87683809663752399, 9.849999999999988987, -20.09763598180369826 ) ) ;
#156118 = CYLINDRICAL_SURFACE ( 'NONE', #199580, 0.09999999999999939493 ) ;
#156121 = EDGE_LOOP ( 'NONE', ( #76521, #223302, #24412 ) ) ;
#156120 = DIRECTION ( 'NONE',  ( 1.000000000000000000, 0.000000000000000000, 0.000000000000000000 ) ) ;
#156122 = CARTESIAN_POINT ( 'NONE',  ( -16.86422026484316916, 9.970447360871810716, -79.58221322567304412 ) ) ;
#156123 = ORIENTED_EDGE ( 'NONE', *, *, #130147, .T. ) ;
#156124 = CARTESIAN_POINT ( 'NONE',  ( -16.86337532320261801, 22.90501630980172720, -230.8619360331160237 ) ) ;
#156125 = ORIENTED_EDGE ( 'NONE', *, *, #102492, .F. ) ;
#156126 = ORIENTED_EDGE ( 'NONE', *, *, #221851, .F. ) ;
#156127 = CARTESIAN_POINT ( 'NONE',  ( -16.93353400591625757, 65.99538760383858005, -48.59042301431898636 ) ) ;
#156128 = AXIS2_PLACEMENT_3D ( 'NONE', #223390, #44775, #125589 ) ;
#156129 = CARTESIAN_POINT ( 'NONE',  ( -21.05000000000000071, 6.299230910103442049, -133.9015624999997556 ) ) ;
#156130 = DIRECTION ( 'NONE',  ( 1.000000000000000000, 0.000000000000000000, 0.000000000000000000 ) ) ;
#156131 = VERTEX_POINT ( 'NONE', #64740 ) ;
#156132 = CIRCLE ( 'NONE', #76391, 0.1000000000000105804 ) ;
#156133 = AXIS2_PLACEMENT_3D ( 'NONE', #180451, #160904, #1791 ) ;
#156134 = CARTESIAN_POINT ( 'NONE',  ( -17.01825945287482966, 65.95000000001262208, -190.8731074845244393 ) ) ;
#156135 = VERTEX_POINT ( 'NONE', #43901 ) ;
#156136 = VERTEX_POINT ( 'NONE', #183419 ) ;
#156137 = CARTESIAN_POINT ( 'NONE',  ( -20.94999999999999929, 38.23914636435922176, -236.1324109481172968 ) ) ;
#156138 = VERTEX_POINT ( 'NONE', #63451 ) ;
#156139 = CARTESIAN_POINT ( 'NONE',  ( -16.93970660449832621, 60.85312929741117927, -221.1195901196794580 ) ) ;
#156140 = SPHERICAL_SURFACE ( 'NONE', #236158, 0.1000000000000000056 ) ;
#156141 = VERTEX_POINT ( 'NONE', #167726 ) ;
#156142 = DIRECTION ( 'NONE',  ( 0.000000000000000000, -0.8660254037844377084, -0.5000000000000016653 ) ) ;
#156143 = AXIS2_PLACEMENT_3D ( 'NONE', #176384, #237626, #214212 ) ;
#156144 = DIRECTION ( 'NONE',  ( 1.073024830501117725E-15, 0.2617529984165031243, 0.9651348961777157509 ) ) ;
#156145 = FACE_OUTER_BOUND ( 'NONE', #33924, .T. ) ;
#156146 = ORIENTED_EDGE ( 'NONE', *, *, #180835, .T. ) ;
#156147 = FACE_OUTER_BOUND ( 'NONE', #242044, .T. ) ;
#156149 = ADVANCED_FACE ( 'NONE', ( #247224 ), #217520, .F. ) ;
#156148 = DIRECTION ( 'NONE',  ( 1.000000000000000000, 3.265361837132813093E-16, -0.000000000000000000 ) ) ;
#156150 = DIRECTION ( 'NONE',  ( 0.000000000000000000, -0.8660254037844377084, -0.5000000000000016653 ) ) ;
#156151 = VECTOR ( 'NONE', #177568, 1000.000000000000000 ) ;
#156152 = ORIENTED_EDGE ( 'NONE', *, *, #41161, .T. ) ;
#156153 = CIRCLE ( 'NONE', #68642, 0.09999999999999971412 ) ;
#156154 = DIRECTION ( 'NONE',  ( 1.000000000000000000, 0.000000000000000000, 0.000000000000000000 ) ) ;
#156155 = ORIENTED_EDGE ( 'NONE', *, *, #20520, .T. ) ;
#156156 = CARTESIAN_POINT ( 'NONE',  ( 23.25000000000000000, 6.550000000011156231, -79.35000000000005116 ) ) ;
#156157 = DIRECTION ( 'NONE',  ( 2.952720810173289112E-16, 1.000000000000000000, 6.982962677686266711E-15 ) ) ;
#156158 = CARTESIAN_POINT ( 'NONE',  ( -18.59999999999999787, 68.59681812508419796, -224.1344059333694361 ) ) ;
#156159 = CYLINDRICAL_SURFACE ( 'NONE', #131511, 0.09999999999999939493 ) ;
#156160 = DIRECTION ( 'NONE',  ( 0.000000000000000000, 1.000000000000000000, 6.982962677686266711E-15 ) ) ;
#156161 = CARTESIAN_POINT ( 'NONE',  ( -20.64999999999999858, 76.00000000001126921, -203.5231074845248997 ) ) ;
#156162 = ADVANCED_FACE ( 'NONE', ( #68606 ), #6039, .F. ) ;
#156163 = VERTEX_POINT ( 'NONE', #162584 ) ;
#156164 = CARTESIAN_POINT ( 'NONE',  ( -23.15000000000000213, 87.41227409416185878, -139.5231074845243029 ) ) ;
#156165 = CYLINDRICAL_SURFACE ( 'NONE', #93978, 0.09999999999999939493 ) ;
#156166 = DIRECTION ( 'NONE',  ( 0.000000000000000000, 1.224646799142185182E-16, 1.000000000000000000 ) ) ;
#156167 = VECTOR ( 'NONE', #200308, 1000.000000000000000 ) ;
#156168 = CARTESIAN_POINT ( 'NONE',  ( 20.97250901189795513, 65.37543196630971920, -61.85856176755740421 ) ) ;
#156169 = ORIENTED_EDGE ( 'NONE', *, *, #85563, .T. ) ;
#156170 = VERTEX_POINT ( 'NONE', #82988 ) ;
#156171 = CARTESIAN_POINT ( 'NONE',  ( 18.79999999999999716, -1.901609089591594470, -11.59510167572422112 ) ) ;
#156172 = DIRECTION ( 'NONE',  ( -1.000000000000000000, -2.952720810173289112E-16, 0.000000000000000000 ) ) ;
#156174 = ADVANCED_FACE ( 'NONE', ( #122161 ), #84249, .F. ) ;
#156173 = CARTESIAN_POINT ( 'NONE',  ( -17.11825945287482753, 66.05000000001261640, -190.7731074845244166 ) ) ;
#156176 = CARTESIAN_POINT ( 'NONE',  ( 21.04999999999999716, 58.88961039665833397, -225.7941988232044821 ) ) ;
#156175 = AXIS2_PLACEMENT_3D ( 'NONE', #212619, #216447, #78219 ) ;
#156177 = DIRECTION ( 'NONE',  ( -0.000000000000000000, 0.9579639084728068799, 0.2868887416116283617 ) ) ;
#156178 = EDGE_CURVE ( 'NONE', #152331, #50174, #213426, .T. ) ;
#156179 = ORIENTED_EDGE ( 'NONE', *, *, #117492, .T. ) ;
#156180 = FACE_OUTER_BOUND ( 'NONE', #180309, .T. ) ;
#156181 = ADVANCED_FACE ( 'NONE', ( #205526 ), #66027, .T. ) ;
#156182 = CONTEXT_DEPENDENT_SHAPE_REPRESENTATION ( #85848, #99568 ) ;
#156183 = DIRECTION ( 'NONE',  ( 0.7071359030027473125, 0.1504668293610846030, -0.6908824414808292236 ) ) ;
#156184 = VERTEX_POINT ( 'NONE', #25625 ) ;
#156185 = DIRECTION ( 'NONE',  ( -0.000000000000000000, -0.4088369013363281623, 0.9126074666063771490 ) ) ;
#156186 = ADVANCED_FACE ( 'NONE', ( #23079 ), #226361, .F. ) ;
#156187 = CARTESIAN_POINT ( 'NONE',  ( 23.24999999999999289, 69.35000000001200249, -115.3731074845243398 ) ) ;
#156188 = AXIS2_PLACEMENT_3D ( 'NONE', #242235, #126133, #225223 ) ;
#156189 = AXIS2_PLACEMENT_3D ( 'NONE', #81175, #197289, #158214 ) ;
#156190 = EDGE_CURVE ( 'NONE', #98368, #256387, #165132, .T. ) ;
#156191 = ORIENTED_EDGE ( 'NONE', *, *, #131571, .F. ) ;
#156192 = DIRECTION ( 'NONE',  ( 0.000000000000000000, -1.000000000000000000, 0.000000000000000000 ) ) ;
#156193 = ORIENTED_EDGE ( 'NONE', *, *, #13932, .F. ) ;
#156194 = CARTESIAN_POINT ( 'NONE',  ( -21.09096482362064506, 75.96055172123749344, -75.88665184992862578 ) ) ;
#156195 = CARTESIAN_POINT ( 'NONE',  ( -21.05000000000000071, 70.10000000001177511, -79.74220724918072278 ) ) ;
#156196 = CARTESIAN_POINT ( 'NONE',  ( -23.15000000000000213, 70.12557831835937350, -215.6322690948981915 ) ) ;
#156197 = DIRECTION ( 'NONE',  ( -1.000000000000000000, -3.265361837132813093E-16, 0.000000000000000000 ) ) ;
#156198 = CARTESIAN_POINT ( 'NONE',  ( 20.95512820512820440, 65.37615131630018084, -124.3731074845243825 ) ) ;
#156199 = CARTESIAN_POINT ( 'NONE',  ( 23.14999999999998792, 11.65000000001115588, -100.5000000000000284 ) ) ;
#156200 = FACE_OUTER_BOUND ( 'NONE', #54416, .T. ) ;
#156201 = DIRECTION ( 'NONE',  ( -1.000000000000000000, 0.000000000000000000, 0.000000000000000000 ) ) ;
#156202 = EDGE_CURVE ( 'NONE', #249634, #116906, #105068, .T. ) ;
#156203 = DIRECTION ( 'NONE',  ( 0.000000000000000000, 0.000000000000000000, -1.000000000000000000 ) ) ;
#156204 = CARTESIAN_POINT ( 'NONE',  ( -18.50000000000000000, 11.65000000001115232, -134.1000000000000227 ) ) ;
#156205 = CARTESIAN_POINT ( 'NONE',  ( 21.11345278033269324, 22.11771856871110487, -231.6856372840668428 ) ) ;
#156206 = CARTESIAN_POINT ( 'NONE',  ( -22.59999999999999787, 75.89914163091351895, -148.2726746080136877 ) ) ;
#156208 = CARTESIAN_POINT ( 'NONE',  ( 18.59117750673696179, 10.33248238083634796, -206.5948465439131496 ) ) ;
#156207 = AXIS2_PLACEMENT_3D ( 'NONE', #106556, #249945, #71328 ) ;
#156209 = VECTOR ( 'NONE', #157566, 1000.000000000000000 ) ;
#156210 = CARTESIAN_POINT ( 'NONE',  ( 21.04999999999999716, 10.72371711693665652, -79.17623960113832027 ) ) ;
#156212 = FACE_OUTER_BOUND ( 'NONE', #136165, .T. ) ;
#156211 = AXIS2_PLACEMENT_3D ( 'NONE', #208078, #185924, #222453 ) ;
#156213 = CIRCLE ( 'NONE', #160490, 0.1999999999999996503 ) ;
#156214 = ORIENTED_EDGE ( 'NONE', *, *, #79383, .T. ) ;
#156215 = CARTESIAN_POINT ( 'NONE',  ( -21.05000000000000071, 77.16270174994990327, -95.02310748452430289 ) ) ;
#156216 = DIRECTION ( 'NONE',  ( 0.000000000000000000, 0.000000000000000000, 1.000000000000000000 ) ) ;
#156217 = CARTESIAN_POINT ( 'NONE',  ( -23.15000000000000213, -4.831324760611774849, -117.4696969421987802 ) ) ;
#156218 = ORIENTED_EDGE ( 'NONE', *, *, #15148, .F. ) ;
#156219 = LINE ( 'NONE', #235715, #76384 ) ;
#156220 = DIRECTION ( 'NONE',  ( 1.000000000000000000, 0.000000000000000000, 0.000000000000000000 ) ) ;
#156221 = VERTEX_POINT ( 'NONE', #88124 ) ;
#156222 = DIRECTION ( 'NONE',  ( -0.000000000000000000, -1.000000000000000000, 0.000000000000000000 ) ) ;
#156223 = CARTESIAN_POINT ( 'NONE',  ( 20.85000000000000142, 67.23127455305835554, -235.8551265064784559 ) ) ;
#156224 = AXIS2_PLACEMENT_3D ( 'NONE', #148273, #49166, #247360 ) ;
#156225 = AXIS2_PLACEMENT_3D ( 'NONE', #71688, #11710, #168246 ) ;
#156226 = EDGE_CURVE ( 'NONE', #13123, #111385, #78537, .T. ) ;
#156228 = EDGE_CURVE ( 'NONE', #15384, #211799, #192594, .T. ) ;
#156227 = VECTOR ( 'NONE', #226397, 1000.000000000000114 ) ;
#156229 = ORIENTED_EDGE ( 'NONE', *, *, #18461, .T. ) ;
#156230 = DIRECTION ( 'NONE',  ( 0.000000000000000000, 0.000000000000000000, 1.000000000000000000 ) ) ;
#156231 = ORIENTED_EDGE ( 'NONE', *, *, #165682, .F. ) ;
#156232 = EDGE_CURVE ( 'NONE', #5184, #82775, #30783, .T. ) ;
#156234 = ADVANCED_FACE ( 'NONE', ( #77251 ), #149443, .F. ) ;
#156233 = CARTESIAN_POINT ( 'NONE',  ( 21.05000000000000071, -0.02138556593762391128, 6.304961112684640767 ) ) ;
#156235 = CARTESIAN_POINT ( 'NONE',  ( 21.06277459767465032, 67.12713756174342450, -124.3191082921676980 ) ) ;
#156237 = AXIS2_PLACEMENT_3D ( 'NONE', #6758, #240253, #82414 ) ;
#156236 = CARTESIAN_POINT ( 'NONE',  ( -15.75000000000000355, 9.349999999999983658, -16.75000000000000355 ) ) ;
#156239 = CARTESIAN_POINT ( 'NONE',  ( -18.59999999999999787, 70.10000000001267040, -193.3040077198679967 ) ) ;
#156238 = AXIS2_PLACEMENT_3D ( 'NONE', #163294, #61617, #221942 ) ;
#156240 = VECTOR ( 'NONE', #94414, 1000.000000000000000 ) ;
#156241 = CARTESIAN_POINT ( 'NONE',  ( 18.50000000000000000, -10.35479209692539548, -27.25654098307376216 ) ) ;
#156242 = CARTESIAN_POINT ( 'NONE',  ( -13.43673303185028800, 46.56726880910646571, -234.7610735323249571 ) ) ;
#156243 = ADVANCED_FACE ( 'NONE', ( #137234 ), #257133, .F. ) ;
#156244 = DIRECTION ( 'NONE',  ( 1.000000000000000000, 0.000000000000000000, 0.000000000000000000 ) ) ;
#156245 = DIRECTION ( 'NONE',  ( 0.000000000000000000, 0.000000000000000000, 1.000000000000000000 ) ) ;
#156247 = ORIENTED_EDGE ( 'NONE', *, *, #144151, .T. ) ;
#156246 = CARTESIAN_POINT ( 'NONE',  ( -18.47653818581420282, -9.465280387751807467, -40.62596081613983046 ) ) ;
#156248 = EDGE_LOOP ( 'NONE', ( #247405, #6982, #136057, #187293 ) ) ;
#156250 = CARTESIAN_POINT ( 'NONE',  ( -20.95613430942403355, 64.25000000001159606, -62.66594483630497336 ) ) ;
#156249 = DIRECTION ( 'NONE',  ( 0.000000000000000000, 6.308085367182471812E-16, 1.000000000000000000 ) ) ;
#156252 = EDGE_LOOP ( 'NONE', ( #220579, #172716, #115015, #35052 ) ) ;
#156251 = CYLINDRICAL_SURFACE ( 'NONE', #156784, 0.09999999999999939493 ) ;
#156253 = EDGE_CURVE ( 'NONE', #56702, #991, #46834, .T. ) ;
#156254 = ORIENTED_EDGE ( 'NONE', *, *, #180755, .T. ) ;
#156255 = PLANE ( 'NONE',  #108166 ) ;
#156256 = EDGE_CURVE ( 'NONE', #185953, #112792, #218355, .T. ) ;
#156257 = CARTESIAN_POINT ( 'NONE',  ( 20.73486653747088937, 7.750000000011182166, -46.15000000000000568 ) ) ;
#156258 = VECTOR ( 'NONE', #240349, 1000.000000000000000 ) ;
#156259 = VECTOR ( 'NONE', #136266, 1000.000000000000000 ) ;
#156260 = ADVANCED_FACE ( 'NONE', ( #177682 ), #251698, .T. ) ;
#156261 = CARTESIAN_POINT ( 'NONE',  ( 18.49999999999999645, 36.65892442174935439, -249.5511627012433848 ) ) ;
#156262 = DIRECTION ( 'NONE',  ( 0.000000000000000000, 0.000000000000000000, 1.000000000000000000 ) ) ;
#156263 = AXIS2_PLACEMENT_3D ( 'NONE', #120712, #42429, #157272 ) ;
#156264 = CARTESIAN_POINT ( 'NONE',  ( -23.15000000000000213, 76.00000000001170974, -69.52310748452431710 ) ) ;
#156265 = AXIS2_PLACEMENT_3D ( 'NONE', #47812, #227748, #127378 ) ;
#156266 = DIRECTION ( 'NONE',  ( 1.000000000000000000, -7.304098846218134667E-16, -5.100424963727256530E-30 ) ) ;
#156267 = ADVANCED_FACE ( 'NONE', ( #216768 ), #98076, .T. ) ;
#156268 = CARTESIAN_POINT ( 'NONE',  ( 5.899999999999995914, -11.34999999999999964, 10.10000000000000142 ) ) ;
#156269 = VERTEX_POINT ( 'NONE', #188543 ) ;
#156270 = ORIENTED_EDGE ( 'NONE', *, *, #115887, .F. ) ;
#156271 = LINE ( 'NONE', #113261, #156401 ) ;
#156272 = EDGE_CURVE ( 'NONE', #20618, #223936, #108992, .T. ) ;
#156273 = EDGE_CURVE ( 'NONE', #180198, #196244, #89433, .T. ) ;
#156274 = VERTEX_POINT ( 'NONE', #176390 ) ;
#156275 = CARTESIAN_POINT ( 'NONE',  ( 20.95512820512820440, 8.876151316299271343, -142.5586289951409640 ) ) ;
#156276 = EDGE_LOOP ( 'NONE', ( #239127, #31303, #158372, #253798 ) ) ;
#156277 = CARTESIAN_POINT ( 'NONE',  ( -22.48970261584618058, 64.35000000001214460, -136.5784769727417824 ) ) ;
#156278 = EDGE_CURVE ( 'NONE', #236113, #82258, #254591, .T. ) ;
#156279 = DIRECTION ( 'NONE',  ( -1.000000000000000000, 0.000000000000000000, 0.000000000000000000 ) ) ;
#156280 = DIRECTION ( 'NONE',  ( 0.000000000000000000, 0.000000000000000000, 1.000000000000000000 ) ) ;
#156282 = EDGE_LOOP ( 'NONE', ( #180292, #160444, #249121, #237020 ) ) ;
#156281 = DIRECTION ( 'NONE',  ( -0.000000000000000000, -6.982962677686266711E-15, 1.000000000000000000 ) ) ;
#156283 = EDGE_CURVE ( 'NONE', #16503, #214669, #69907, .T. ) ;
#156284 = DIRECTION ( 'NONE',  ( -1.000000000000000000, -1.040834085586090568E-13, 0.000000000000000000 ) ) ;
#156285 = EDGE_LOOP ( 'NONE', ( #80526, #138490, #50185, #63996 ) ) ;
#156286 = ADVANCED_FACE ( 'NONE', ( #129841 ), #110280, .F. ) ;
#156287 = CARTESIAN_POINT ( 'NONE',  ( -20.54999999999999716, 68.59518897103603763, -214.2073844195901131 ) ) ;
#156288 = AXIS2_PLACEMENT_3D ( 'NONE', #124182, #246667, #25095 ) ;
#156289 = DIRECTION ( 'NONE',  ( -2.602085213965226419E-14, -0.000000000000000000, -1.000000000000000000 ) ) ;
#156290 = CARTESIAN_POINT ( 'NONE',  ( -22.47071067811865319, 29.57301391503005661, -252.6169816238249552 ) ) ;
#156291 = VECTOR ( 'NONE', #161099, 1000.000000000000000 ) ;
#156292 = DIRECTION ( 'NONE',  ( -0.000000000000000000, -0.000000000000000000, 1.000000000000000000 ) ) ;
#156293 = DIRECTION ( 'NONE',  ( 1.000000000000000000, 0.000000000000000000, 0.000000000000000000 ) ) ;
#156294 = TOROIDAL_SURFACE ( 'NONE', #10524, 11.65000000000000036, 0.1000000000000000056 ) ;
#156295 = VERTEX_POINT ( 'NONE', #71186 ) ;
#156296 = CYLINDRICAL_SURFACE ( 'NONE', #131681, 4.049999999999987388 ) ;
#156297 = ORIENTED_EDGE ( 'NONE', *, *, #84739, .F. ) ;
#156300 = ORIENTED_EDGE ( 'NONE', *, *, #66638, .F. ) ;
#156299 = DIRECTION ( 'NONE',  ( 1.000000000000000000, 0.000000000000000000, 0.000000000000000000 ) ) ;
#156298 = DIRECTION ( 'NONE',  ( 1.000000000000000000, -7.304098846218134667E-16, -4.217023435051626718E-16 ) ) ;
#156301 = CARTESIAN_POINT ( 'NONE',  ( -20.64999999999999858, 76.00000000001205080, -123.5481074845242802 ) ) ;
#156302 = VECTOR ( 'NONE', #57786, 1000.000000000000114 ) ;
#156303 = SPHERICAL_SURFACE ( 'NONE', #212659, 0.1000000000000000056 ) ;
#156304 = CIRCLE ( 'NONE', #43841, 0.1000000000000028644 ) ;
#156305 = ORIENTED_EDGE ( 'NONE', *, *, #50157, .F. ) ;
#156306 = CARTESIAN_POINT ( 'NONE',  ( -20.15000000000000568, 9.291421356248463326, -54.65000000000000568 ) ) ;
#156307 = CARTESIAN_POINT ( 'NONE',  ( 23.15000000000000213, -5.658827671433157569, -233.3450493518450344 ) ) ;
#156308 = FACE_OUTER_BOUND ( 'NONE', #157621, .T. ) ;
#156309 = UNCERTAINTY_MEASURE_WITH_UNIT (LENGTH_MEASURE( 1.000000000000000082E-05 ), #60655, 'distance_accuracy_value', 'NONE');
#156311 = VERTEX_POINT ( 'NONE', #249808 ) ;
#156310 = LINE ( 'NONE', #117156, #151793 ) ;
#156312 = AXIS2_PLACEMENT_3D ( 'NONE', #69497, #149032, #134561 ) ;
#156313 = DIRECTION ( 'NONE',  ( -1.000000000000000000, -0.000000000000000000, 0.000000000000000000 ) ) ;
#156314 = AXIS2_PLACEMENT_3D ( 'NONE', #108026, #70205, #153615 ) ;
#156315 = ORIENTED_EDGE ( 'NONE', *, *, #193568, .T. ) ;
#156316 = CARTESIAN_POINT ( 'NONE',  ( -21.05000000000000071, 87.29603075034721371, -106.0710066441880883 ) ) ;
#156317 = CARTESIAN_POINT ( 'NONE',  ( 18.50000000000000355, -9.421456145484233602, -74.24198208401919885 ) ) ;
#156318 = CARTESIAN_POINT ( 'NONE',  ( -23.39999999999994529, 64.35000000001120668, -3.123107484524795474 ) ) ;
#156319 = ORIENTED_EDGE ( 'NONE', *, *, #68840, .F. ) ;
#156320 = CARTESIAN_POINT ( 'NONE',  ( 20.85000000000000142, 1.115600667400684642E-11, -200.9999999999999432 ) ) ;
#156321 = ORIENTED_EDGE ( 'NONE', *, *, #237608, .T. ) ;
#156322 = CARTESIAN_POINT ( 'NONE',  ( -18.50000000000000000, 64.35000000001230092, -157.8731074845244393 ) ) ;
#156323 = CARTESIAN_POINT ( 'NONE',  ( 23.25000000000000000, -11.74999999998883560, -146.1500000000000341 ) ) ;
#156324 = DIRECTION ( 'NONE',  ( -7.304098846218134667E-16, -0.4088369013363281068, 0.9126074666063770380 ) ) ;
#156325 = AXIS2_PLACEMENT_3D ( 'NONE', #193064, #36583, #253014 ) ;
#156326 = ORIENTED_EDGE ( 'NONE', *, *, #80074, .F. ) ;
#156327 = CARTESIAN_POINT ( 'NONE',  ( 21.12769345151713196, 22.98650045582965618, -230.0668730597805052 ) ) ;
#156328 = DIRECTION ( 'NONE',  ( 0.000000000000000000, 0.000000000000000000, 1.000000000000000000 ) ) ;
#156329 = ADVANCED_FACE ( 'NONE', ( #194681 ), #235067, .F. ) ;
#156330 = ORIENTED_EDGE ( 'NONE', *, *, #194990, .T. ) ;
#156331 = CARTESIAN_POINT ( 'NONE',  ( -21.05000000000000071, 76.00000000001213607, -136.5231074845243313 ) ) ;
#156333 = EDGE_CURVE ( 'NONE', #16525, #38380, #114322, .T. ) ;
#156332 = CARTESIAN_POINT ( 'NONE',  ( -21.05000000000000071, 4.898587196589414801E-16, -37.50000000000000000 ) ) ;
#156334 = PLANE ( 'NONE',  #3020 ) ;
#156335 = VECTOR ( 'NONE', #136802, 1000.000000000000000 ) ;
#156336 = AXIS2_PLACEMENT_3D ( 'NONE', #29249, #10937, #9635 ) ;
#156337 = VERTEX_POINT ( 'NONE', #142366 ) ;
#156338 = EDGE_CURVE ( 'NONE', #242014, #200486, #1873, .T. ) ;
#156339 = CARTESIAN_POINT ( 'NONE',  ( -18.59999999999999787, -1.835859311432481045, -112.0044391687985694 ) ) ;
#156340 = EDGE_LOOP ( 'NONE', ( #154149, #115172, #250667, #156946 ) ) ;
#156343 = ADVANCED_FACE ( 'NONE', ( #218033 ), #36478, .F. ) ;
#156342 = VERTEX_POINT ( 'NONE', #139788 ) ;
#156341 = CARTESIAN_POINT ( 'NONE',  ( 18.59999999999998721, 14.70949956575304185, -235.9560995168023112 ) ) ;
#156346 = VERTEX_POINT ( 'NONE', #58951 ) ;
#156345 = ORIENTED_EDGE ( 'NONE', *, *, #89850, .T. ) ;
#156344 = DIRECTION ( 'NONE',  ( 0.000000000000000000, 0.000000000000000000, 1.000000000000000000 ) ) ;
#156347 = CARTESIAN_POINT ( 'NONE',  ( -21.05000000000000071, 28.63831050940605394, -258.0693639473472558 ) ) ;
#156348 = CARTESIAN_POINT ( 'NONE',  ( -23.15000000000000213, 54.18213181965657554, -236.9344197582443883 ) ) ;
#156349 = DIRECTION ( 'NONE',  ( 1.000000000000000000, -0.000000000000000000, -0.000000000000000000 ) ) ;
#156350 = CARTESIAN_POINT ( 'NONE',  ( -16.85697194749127803, 12.43417586606322445, -211.5301872951059750 ) ) ;
#156351 = CARTESIAN_POINT ( 'NONE',  ( 21.07189867249812210, 10.72498027010430377, -112.7124514422767732 ) ) ;
#156352 = CIRCLE ( 'NONE', #2178, 0.2000000000000005107 ) ;
#156353 = CARTESIAN_POINT ( 'NONE',  ( 20.95000000000000284, 11.60000000001116227, -127.0717967697245143 ) ) ;
#156354 = CARTESIAN_POINT ( 'NONE',  ( 23.24999999999999645, 71.22429906543244726, -91.17433938047835795 ) ) ;
#156355 = DIRECTION ( 'NONE',  ( 1.000000000000000000, 0.000000000000000000, 0.000000000000000000 ) ) ;
#156357 = EDGE_CURVE ( 'NONE', #76270, #185168, #43281, .T. ) ;
#156356 = EDGE_LOOP ( 'NONE', ( #184453, #257593, #13155, #110064 ) ) ;
#156358 = ORIENTED_EDGE ( 'NONE', *, *, #169580, .F. ) ;
#156359 = ORIENTED_EDGE ( 'NONE', *, *, #27545, .T. ) ;
#156360 = DIRECTION ( 'NONE',  ( 0.000000000000000000, -0.9947597004326491632, 0.1022405907413782566 ) ) ;
#156361 = CIRCLE ( 'NONE', #118754, 0.1000000000000002554 ) ;
#156363 = VERTEX_POINT ( 'NONE', #83642 ) ;
#156362 = LINE ( 'NONE', #235851, #74463 ) ;
#156364 = CARTESIAN_POINT ( 'NONE',  ( -16.87683809663752399, 66.15000000001205649, -123.1207434663280651 ) ) ;
#156365 = EDGE_LOOP ( 'NONE', ( #32867, #189368, #18832, #89654 ) ) ;
#156366 = DIRECTION ( 'NONE',  ( 0.000000000000000000, 0.8700118002898356018, -0.4930308989875170078 ) ) ;
#156367 = ORIENTED_EDGE ( 'NONE', *, *, #103222, .F. ) ;
#156368 = CARTESIAN_POINT ( 'NONE',  ( 20.94999999999999929, -1.835341550213257733, -179.0551512925629538 ) ) ;
#156369 = EDGE_CURVE ( 'NONE', #175321, #133719, #43409, .T. ) ;
#156370 = ORIENTED_EDGE ( 'NONE', *, *, #134717, .T. ) ;
#156371 = CARTESIAN_POINT ( 'NONE',  ( 20.94999999999999574, 43.97124485275623584, -258.7804622366496119 ) ) ;
#156372 = DIRECTION ( 'NONE',  ( -1.000000000000000000, 0.000000000000000000, 0.000000000000000000 ) ) ;
#156373 = EDGE_CURVE ( 'NONE', #79099, #131441, #189161, .T. ) ;
#156376 = VERTEX_POINT ( 'NONE', #202347 ) ;
#156375 = ORIENTED_EDGE ( 'NONE', *, *, #221105, .F. ) ;
#156374 = TOROIDAL_SURFACE ( 'NONE', #247919, 0.2000000000000000111, 0.1000000000000000056 ) ;
#156377 = AXIS2_PLACEMENT_3D ( 'NONE', #63752, #106714, #62485 ) ;
#156378 = VERTEX_POINT ( 'NONE', #62836 ) ;
#156379 = CARTESIAN_POINT ( 'NONE',  ( 18.59999999999999076, 5.950000000011100632, -110.8057023050348988 ) ) ;
#156380 = ORIENTED_EDGE ( 'NONE', *, *, #33022, .F. ) ;
#156381 = ORIENTED_EDGE ( 'NONE', *, *, #116727, .F. ) ;
#156382 = DIRECTION ( 'NONE',  ( 0.000000000000000000, -0.000000000000000000, 1.000000000000000000 ) ) ;
#156384 = ORIENTED_EDGE ( 'NONE', *, *, #213375, .T. ) ;
#156383 = CARTESIAN_POINT ( 'NONE',  ( 18.59999999999999432, 5.699452464321598910, 12.54227395656983290 ) ) ;
#156386 = CARTESIAN_POINT ( 'NONE',  ( -23.15000000000000213, 76.00000000001244871, -170.0231074845243597 ) ) ;
#156385 = DIRECTION ( 'NONE',  ( 0.7071359030027680737, 0.7070776581709111719, 0.000000000000000000 ) ) ;
#156387 = ADVANCED_FACE ( 'NONE', ( #21177 ), #221882, .T. ) ;
#156388 = DIRECTION ( 'NONE',  ( 1.000000000000000000, 0.000000000000000000, 0.000000000000000000 ) ) ;
#156389 = CARTESIAN_POINT ( 'NONE',  ( 18.50000000000000000, -9.419209763398098900, -74.24776946275900968 ) ) ;
#156390 = DIRECTION ( 'NONE',  ( 0.000000000000000000, -7.272083257015735086E-15, 1.000000000000000000 ) ) ;
#156391 = ORIENTED_EDGE ( 'NONE', *, *, #54037, .T. ) ;
#156392 = EDGE_CURVE ( 'NONE', #210485, #229898, #143651, .T. ) ;
#156393 = EDGE_LOOP ( 'NONE', ( #198525, #96234, #171068, #188092 ) ) ;
#156394 = CARTESIAN_POINT ( 'NONE',  ( 18.43466021071412797, 85.49419069046841457, -96.40604592439639475 ) ) ;
#156395 = CARTESIAN_POINT ( 'NONE',  ( 21.14999999999999858, 11.65000000001115943, -100.6000000000000369 ) ) ;
#156396 = DIRECTION ( 'NONE',  ( -1.000000000000000000, -0.000000000000000000, -0.000000000000000000 ) ) ;
#156397 = AXIS2_PLACEMENT_3D ( 'NONE', #164963, #90550, #65858 ) ;
#156399 = ADVANCED_FACE ( 'NONE', ( #79805 ), #238913, .T. ) ;
#156398 = VERTEX_POINT ( 'NONE', #287 ) ;
#156400 = CARTESIAN_POINT ( 'NONE',  ( -23.15000000000000213, 1.115600667400684642E-11, -171.5499999999999829 ) ) ;
#156401 = VECTOR ( 'NONE', #256560, 1000.000000000000000 ) ;
#156402 = AXIS2_PLACEMENT_3D ( 'NONE', #56356, #65040, #198453 ) ;
#156403 = AXIS2_PLACEMENT_3D ( 'NONE', #65220, #121392, #63949 ) ;
#156404 = CARTESIAN_POINT ( 'NONE',  ( 0.8999999999999993561, -8.250000000000005329, 28.60000000000000142 ) ) ;
#156405 = CARTESIAN_POINT ( 'NONE',  ( -13.88555196119802915, 12.43281162335558321, -213.6438014222476909 ) ) ;
#156406 = ORIENTED_EDGE ( 'NONE', *, *, #188411, .T. ) ;
#156407 = VERTEX_POINT ( 'NONE', #247890 ) ;
#156408 =( GEOMETRIC_REPRESENTATION_CONTEXT ( 3 ) GLOBAL_UNCERTAINTY_ASSIGNED_CONTEXT ( ( #68666 ) ) GLOBAL_UNIT_ASSIGNED_CONTEXT ( ( #32308, #49267, #230480 ) ) REPRESENTATION_CONTEXT ( 'NONE', 'WORKASPACE' ) );
#156409 = DIRECTION ( 'NONE',  ( 0.000000000000000000, 0.000000000000000000, 1.000000000000000000 ) ) ;
#156410 = DIRECTION ( 'NONE',  ( 1.301042606982683418E-14, -0.8660254037844330455, 0.5000000000000096589 ) ) ;
#156411 = ORIENTED_EDGE ( 'NONE', *, *, #158627, .T. ) ;
#156412 = DIRECTION ( 'NONE',  ( 0.7071359030027766224, -0.7070776581709024011, 0.000000000000000000 ) ) ;
#156413 = EDGE_LOOP ( 'NONE', ( #42835, #193510, #168510, #78761, #30973, #149125, #136455 ) ) ;
#156414 = ADVANCED_FACE ( 'NONE', ( #246600 ), #47663, .T. ) ;
#156415 = CYLINDRICAL_SURFACE ( 'NONE', #127263, 0.09999999999999939493 ) ;
#156416 = CARTESIAN_POINT ( 'NONE',  ( -20.64999999999999858, 85.50000000001179501, -79.41707660717668205 ) ) ;
#156418 = CARTESIAN_POINT ( 'NONE',  ( -22.49999999999999645, 55.86495732666937641, -232.8769840133978164 ) ) ;
#156417 = DIRECTION ( 'NONE',  ( 0.000000000000000000, -1.000000000000000000, 0.000000000000000000 ) ) ;
#156419 = DIRECTION ( 'NONE',  ( 0.000000000000000000, -0.4088369013363281623, 0.9126074666063771490 ) ) ;
#156421 = EDGE_CURVE ( 'NONE', #140349, #89932, #87515, .T. ) ;
#156420 = CARTESIAN_POINT ( 'NONE',  ( -21.05000000000000071, 5.900000000011102586, -144.2190997646564483 ) ) ;
#156422 = CARTESIAN_POINT ( 'NONE',  ( 21.05000000000000071, 79.33069327855442054, -236.1318330389568985 ) ) ;
#156423 = AXIS2_PLACEMENT_3D ( 'NONE', #187412, #203108, #27073 ) ;
#156424 =( BOUNDED_CURVE ( )  B_SPLINE_CURVE ( 3, ( #121351, #143434, #46888, #44353 ),
 .UNSPECIFIED., .F., .T. ) 
 B_SPLINE_CURVE_WITH_KNOTS ( ( 4, 4 ),
 ( 0.5235987755983111391, 1.570796326794896558 ),
 .UNSPECIFIED. ) 
 CURVE ( )  GEOMETRIC_REPRESENTATION_ITEM ( )  RATIONAL_B_SPLINE_CURVE ( ( 1.000000000000000000, 0.9106836025229610998, 0.9106836025229610998, 1.000000000000000000 ) ) 
 REPRESENTATION_ITEM ( '' )  );
#156425 = AXIS2_PLACEMENT_3D ( 'NONE', #205720, #131324, #207019 ) ;
#156427 = VERTEX_POINT ( 'NONE', #206201 ) ;
#156426 = ORIENTED_EDGE ( 'NONE', *, *, #198285, .F. ) ;
#156428 = ORIENTED_EDGE ( 'NONE', *, *, #256308, .F. ) ;
#156429 = AXIS2_PLACEMENT_3D ( 'NONE', #46860, #164275, #85973 ) ;
#156430 = CARTESIAN_POINT ( 'NONE',  ( -18.59999999999999787, -9.849999999999994316, 30.09999999999999076 ) ) ;
#156431 = CARTESIAN_POINT ( 'NONE',  ( -16.78055652883087134, 60.94529327262787177, -221.0321558084000912 ) ) ;
#156432 = CARTESIAN_POINT ( 'NONE',  ( 23.24999999999999645, 1.115600667400684642E-11, -33.50000000000000000 ) ) ;
#156433 = AXIS2_PLACEMENT_3D ( 'NONE', #146246, #244065, #184097 ) ;
#156434 = CYLINDRICAL_SURFACE ( 'NONE', #61927, 11.80000000000000426 ) ;
#156436 = CARTESIAN_POINT ( 'NONE',  ( 5.900000000000059863, 64.25000000001119815, -25.92310748452479174 ) ) ;
#156435 = CARTESIAN_POINT ( 'NONE',  ( 20.30466543256828160, 9.304236939255389416, -8.253662651392039251 ) ) ;
#156437 = CARTESIAN_POINT ( 'NONE',  ( -16.81931177881021711, 66.06300394050762748, -48.74988960590717113 ) ) ;
#156438 = VERTEX_POINT ( 'NONE', #45839 ) ;
#156439 = AXIS2_PLACEMENT_3D ( 'NONE', #19611, #203375, #99106 ) ;
#156440 = CARTESIAN_POINT ( 'NONE',  ( 22.00356870143104260, 68.74575763753909996, -69.52310748452437394 ) ) ;
#156441 = CIRCLE ( 'NONE', #139814, 10.00000000000000178 ) ;
#156442 = AXIS2_PLACEMENT_3D ( 'NONE', #165667, #143506, #241345 ) ;
#156443 = ORIENTED_EDGE ( 'NONE', *, *, #74980, .F. ) ;
#156444 = ORIENTED_EDGE ( 'NONE', *, *, #198683, .T. ) ;
#156445 = CARTESIAN_POINT ( 'NONE',  ( -21.05000000000000071, 69.69503888732667463, -69.50172191858641213 ) ) ;
#156446 = DIRECTION ( 'NONE',  ( 0.000000000000000000, -0.8814952561688410571, 0.4721928772777385097 ) ) ;
#156447 = CARTESIAN_POINT ( 'NONE',  ( -20.85000000000000142, -1.164121893230052995, -141.9148480855716343 ) ) ;
#156448 = DIRECTION ( 'NONE',  ( 0.000000000000000000, -0.2128009952263485993, 0.9770955615653341697 ) ) ;
#156449 = CIRCLE ( 'NONE', #223216, 0.2000000000000052014 ) ;
#156450 = CARTESIAN_POINT ( 'NONE',  ( -21.05000000000000071, 77.26178616857691850, -94.93660852097882241 ) ) ;
#156451 = ORIENTED_EDGE ( 'NONE', *, *, #60134, .T. ) ;
#156452 = EDGE_LOOP ( 'NONE', ( #204483, #238238, #25778, #19373 ) ) ;
#156453 = CIRCLE ( 'NONE', #181377, 0.2000000000000048683 ) ;
#156454 = CARTESIAN_POINT ( 'NONE',  ( 21.14999999999999858, 30.90801580390627734, -252.0203440857197279 ) ) ;
#156455 = LINE ( 'NONE', #136843, #215431 ) ;
#156456 = EDGE_LOOP ( 'NONE', ( #41661, #177117, #164053, #150341 ) ) ;
#156457 = CARTESIAN_POINT ( 'NONE',  ( 18.39999999999999503, 16.64129698264336099, -222.1941556740511032 ) ) ;
#156458 = LINE ( 'NONE', #37778, #215136 ) ;
#156459 = AXIS2_PLACEMENT_3D ( 'NONE', #81734, #202995, #145585 ) ;
#156460 = CARTESIAN_POINT ( 'NONE',  ( -16.97683809663754673, 9.950000000011137047, -187.7284708321105029 ) ) ;
#156461 = VECTOR ( 'NONE', #125773, 1000.000000000000000 ) ;
#156462 = DIRECTION ( 'NONE',  ( -1.000000000000000000, 0.000000000000000000, -0.000000000000000000 ) ) ;
#156463 = CARTESIAN_POINT ( 'NONE',  ( -18.50000000000000000, 30.36376046184471988, -235.5720385971402493 ) ) ;
#156465 = DIRECTION ( 'NONE',  ( 0.000000000000000000, -0.8814952561688430555, 0.4721928772777346239 ) ) ;
#156464 = CARTESIAN_POINT ( 'NONE',  ( -22.50000000000000000, 0.09999999999999939493, 11.64957080754479968 ) ) ;
#156466 = FACE_OUTER_BOUND ( 'NONE', #83126, .T. ) ;
#156467 = CARTESIAN_POINT ( 'NONE',  ( -18.59999999999999787, -1.835859311432481045, -78.50443916879852679 ) ) ;
#156468 = DIRECTION ( 'NONE',  ( 1.000000000000000000, 0.000000000000000000, 0.000000000000000000 ) ) ;
#156469 = DIRECTION ( 'NONE',  ( 0.000000000000000000, 0.9770955615653548199, 0.2128009952262535920 ) ) ;
#156471 = ORIENTED_EDGE ( 'NONE', *, *, #175404, .T. ) ;
#156470 = PLANE ( 'NONE',  #19679 ) ;
#156472 = DIRECTION ( 'NONE',  ( 0.000000000000000000, 4.336808689941893885E-15, 1.000000000000000000 ) ) ;
#156473 = EDGE_CURVE ( 'NONE', #183612, #244854, #165813, .T. ) ;
#156474 = EDGE_LOOP ( 'NONE', ( #41740, #65635, #177497, #36640, #41284 ) ) ;
#156476 = CIRCLE ( 'NONE', #173044, 0.1000000000000124678 ) ;
#156475 = CARTESIAN_POINT ( 'NONE',  ( -22.42357213249529124, 0.09908696401271366305, -92.82706761364009651 ) ) ;
#156478 = EDGE_CURVE ( 'NONE', #94366, #162266, #67770, .T. ) ;
#156477 = DIRECTION ( 'NONE',  ( 0.000000000000000000, 0.000000000000000000, 1.000000000000000000 ) ) ;
#156479 = EDGE_CURVE ( 'NONE', #185233, #50777, #180789, .T. ) ;
#156481 = ORIENTED_EDGE ( 'NONE', *, *, #233943, .F. ) ;
#156480 = AXIS2_PLACEMENT_3D ( 'NONE', #98197, #37011, #116528 ) ;
#156482 = CARTESIAN_POINT ( 'NONE',  ( 20.95512820512820440, 10.49413282287806481, -207.4737445703522383 ) ) ;
#156483 = VECTOR ( 'NONE', #191246, 1000.000000000000000 ) ;
#156484 = DIRECTION ( 'NONE',  ( 0.000000000000000000, 0.9126074666063770380, 0.4088369013363281068 ) ) ;
#156485 = CARTESIAN_POINT ( 'NONE',  ( 20.94999999999999574, 1.835341550235569663, -45.05515129256298223 ) ) ;
#156486 = DIRECTION ( 'NONE',  ( 0.000000000000000000, 6.982962677686266711E-15, -1.000000000000000000 ) ) ;
#156487 = CYLINDRICAL_SURFACE ( 'NONE', #165548, 0.1000000000000106914 ) ;
#156488 = FACE_OUTER_BOUND ( 'NONE', #92518, .T. ) ;
#156489 = CIRCLE ( 'NONE', #98144, 0.09999999999999609201 ) ;
#156490 = ORIENTED_EDGE ( 'NONE', *, *, #201969, .F. ) ;
#156491 = FACE_OUTER_BOUND ( 'NONE', #163905, .T. ) ;
#156493 = ORIENTED_EDGE ( 'NONE', *, *, #27547, .T. ) ;
#156492 = CYLINDRICAL_SURFACE ( 'NONE', #188510, 0.09999999999999520384 ) ;
#156494 = DIRECTION ( 'NONE',  ( 0.000000000000000000, 0.000000000000000000, -1.000000000000000000 ) ) ;
#156495 = EDGE_CURVE ( 'NONE', #251548, #16273, #243305, .T. ) ;
#156496 = CARTESIAN_POINT ( 'NONE',  ( 20.97224591636398827, 22.94420667656951807, -230.1510067393869576 ) ) ;
#156497 = CARTESIAN_POINT ( 'NONE',  ( 23.24999999999999645, 11.74999999999998224, -20.84999999999999432 ) ) ;
#156498 = AXIS2_PLACEMENT_3D ( 'NONE', #200945, #65286, #224356 ) ;
#156499 = ORIENTED_EDGE ( 'NONE', *, *, #99618, .F. ) ;
#156500 = CARTESIAN_POINT ( 'NONE',  ( 18.49999999999999289, 70.08587962373171365, -198.1273832143211848 ) ) ;
#156501 = CIRCLE ( 'NONE', #119056, 0.09999999999999939493 ) ;
#156502 = APPLICATION_PROTOCOL_DEFINITION ( 'draft international standard', 'automotive_design', 1998, #10884 ) ;
#156503 = LINE ( 'NONE', #14415, #152350 ) ;
#156504 = DIRECTION ( 'NONE',  ( 0.000000000000000000, 0.000000000000000000, 1.000000000000000000 ) ) ;
#156505 = TOROIDAL_SURFACE ( 'NONE', #44032, 0.2000000000000000111, 0.1000000000000000056 ) ;
#156506 = ORIENTED_EDGE ( 'NONE', *, *, #116425, .F. ) ;
#156507 = CARTESIAN_POINT ( 'NONE',  ( 18.59999999999999787, -1.835341550213255957, -112.1551512925630050 ) ) ;
#156508 = DIRECTION ( 'NONE',  ( 1.000000000000000000, 0.000000000000000000, 0.000000000000000000 ) ) ;
#156509 = EDGE_CURVE ( 'NONE', #60290, #97714, #208779, .T. ) ;
#156510 = ORIENTED_EDGE ( 'NONE', *, *, #237508, .T. ) ;
#156511 = EDGE_CURVE ( 'NONE', #133646, #19150, #143359, .T. ) ;
#156512 = CIRCLE ( 'NONE', #81425, 0.09999999999999939493 ) ;
#156513 = ORIENTED_EDGE ( 'NONE', *, *, #4237, .F. ) ;
#156514 = CARTESIAN_POINT ( 'NONE',  ( -20.54999999999999716, 68.75000000001223555, -148.7731074845244166 ) ) ;
#156515 = FACE_OUTER_BOUND ( 'NONE', #175799, .T. ) ;
#156516 = FACE_OUTER_BOUND ( 'NONE', #257960, .T. ) ;
#156517 = DIRECTION ( 'NONE',  ( 0.000000000000000000, -1.000000000000000000, -6.982962677686265922E-15 ) ) ;
#156518 = FACE_OUTER_BOUND ( 'NONE', #159547, .T. ) ;
#156519 = EDGE_CURVE ( 'NONE', #213499, #158981, #72653, .T. ) ;
#156520 = FACE_OUTER_BOUND ( 'NONE', #87323, .T. ) ;
#156521 = FACE_OUTER_BOUND ( 'NONE', #81354, .T. ) ;
#156522 = CARTESIAN_POINT ( 'NONE',  ( -18.50000000000000000, -1.736257131597395809, -11.56865232901749785 ) ) ;
#156523 = DIRECTION ( 'NONE',  ( 0.000000000000000000, 0.000000000000000000, -1.000000000000000000 ) ) ;
#156524 = LINE ( 'NONE', #78222, #123930 ) ;
#156525 = AXIS2_PLACEMENT_3D ( 'NONE', #142910, #2125, #200347 ) ;
#156526 = VERTEX_POINT ( 'NONE', #189212 ) ;
#156527 = VECTOR ( 'NONE', #115981, 1000.000000000000114 ) ;
#156528 = ORIENTED_EDGE ( 'NONE', *, *, #231237, .T. ) ;
#156529 = AXIS2_PLACEMENT_3D ( 'NONE', #199851, #23794, #103271 ) ;
#156531 = CARTESIAN_POINT ( 'NONE',  ( 18.59999999999999076, 10.49142135623730709, -24.75000000000000000 ) ) ;
#156530 = AXIS2_PLACEMENT_3D ( 'NONE', #193966, #154851, #17868 ) ;
#156532 = CARTESIAN_POINT ( 'NONE',  ( -17.73285935862685392, 65.14201819622533662, -146.7645456747499111 ) ) ;
#156534 = DIRECTION ( 'NONE',  ( 0.000000000000000000, 0.000000000000000000, -1.000000000000000000 ) ) ;
#156533 = CARTESIAN_POINT ( 'NONE',  ( 21.08376601933332495, 69.65805272873599563, -69.58688349545435869 ) ) ;
#156535 = FACE_OUTER_BOUND ( 'NONE', #99920, .T. ) ;
#156536 = DIRECTION ( 'NONE',  ( -0.5932847527679310229, 0.8049926720990042694, -6.366092712777067056E-16 ) ) ;
#156537 = DIRECTION ( 'NONE',  ( -1.000000000000000000, 0.000000000000000000, 0.000000000000000000 ) ) ;
#156538 = EDGE_LOOP ( 'NONE', ( #117488, #131357, #14453 ) ) ;
#156539 = ORIENTED_EDGE ( 'NONE', *, *, #129234, .F. ) ;
#156540 = CARTESIAN_POINT ( 'NONE',  ( -18.59999999999999787, -1.162701749926853712, -108.5000000000000426 ) ) ;
#156541 = ORIENTED_EDGE ( 'NONE', *, *, #76642, .T. ) ;
#156542 = CARTESIAN_POINT ( 'NONE',  ( -20.00857864376270001, 66.65000000001205649, -124.1731074845243654 ) ) ;
#156543 = AXIS2_PLACEMENT_3D ( 'NONE', #9494, #186877, #32967 ) ;
#156544 = DIRECTION ( 'NONE',  ( 0.000000000000000000, 0.000000000000000000, -1.000000000000000000 ) ) ;
#156545 = EDGE_CURVE ( 'NONE', #39695, #109372, #164227, .T. ) ;
#156546 = VECTOR ( 'NONE', #223827, 1000.000000000000000 ) ;
#156547 = EDGE_CURVE ( 'NONE', #159476, #8211, #147462, .T. ) ;
#156548 = VERTEX_POINT ( 'NONE', #90086 ) ;
#156549 = DIRECTION ( 'NONE',  ( 0.000000000000000000, -0.3343365196859449662, 0.9424537609900497381 ) ) ;
#156550 = ORIENTED_EDGE ( 'NONE', *, *, #172920, .F. ) ;
#156551 = ADVANCED_FACE ( 'NONE', ( #147510 ), #48398, .F. ) ;
#156553 = EDGE_CURVE ( 'NONE', #171102, #221915, #1697, .T. ) ;
#156552 = DIRECTION ( 'NONE',  ( 0.000000000000000000, 6.982962677686266711E-15, -1.000000000000000000 ) ) ;
#156554 = CARTESIAN_POINT ( 'NONE',  ( 20.94999999999999929, 56.27731819600170837, -227.9967441372480437 ) ) ;
#156555 = CARTESIAN_POINT ( 'NONE',  ( -20.54999999999999716, -8.999999999988846255, -143.8939691226524644 ) ) ;
#156556 = DIRECTION ( 'NONE',  ( 1.000000000000000000, 0.000000000000000000, 0.000000000000000000 ) ) ;
#156557 = DIRECTION ( 'NONE',  ( 0.000000000000000000, 6.982962677686266711E-15, -1.000000000000000000 ) ) ;
#156559 = CYLINDRICAL_SURFACE ( 'NONE', #16951, 0.09999999999999939493 ) ;
#156558 = DIRECTION ( 'NONE',  ( 0.000000000000000000, 1.000000000000000000, 0.000000000000000000 ) ) ;
#156560 = CARTESIAN_POINT ( 'NONE',  ( -20.85000000000000142, 87.75000000001190870, -103.0231074845242176 ) ) ;
#156561 = ORIENTED_EDGE ( 'NONE', *, *, #11332, .F. ) ;
#156563 = CARTESIAN_POINT ( 'NONE',  ( -16.83794479845802883, 66.07364258066050411, -115.8266627803021009 ) ) ;
#156562 = LINE ( 'NONE', #151411, #78476 ) ;
#156564 = ORIENTED_EDGE ( 'NONE', *, *, #118586, .F. ) ;
#156566 = VERTEX_POINT ( 'NONE', #144921 ) ;
#156565 = DIRECTION ( 'NONE',  ( 0.000000000000000000, 0.000000000000000000, -1.000000000000000000 ) ) ;
#156567 = EDGE_CURVE ( 'NONE', #155954, #229799, #9281, .T. ) ;
#156568 = AXIS2_PLACEMENT_3D ( 'NONE', #5567, #245500, #205055 ) ;
#156569 = ORIENTED_EDGE ( 'NONE', *, *, #135583, .T. ) ;
#156570 = DIRECTION ( 'NONE',  ( 0.000000000000000000, 0.000000000000000000, -1.000000000000000000 ) ) ;
#156572 = EDGE_CURVE ( 'NONE', #46944, #241842, #230875, .T. ) ;
#156571 = EDGE_CURVE ( 'NONE', #16272, #190824, #85064, .T. ) ;
#156573 = FACE_OUTER_BOUND ( 'NONE', #217002, .T. ) ;
#156574 = CARTESIAN_POINT ( 'NONE',  ( -21.04999999999999716, -9.599999999988844124, -40.53206939669966857 ) ) ;
#156575 = LINE ( 'NONE', #256866, #263 ) ;
#156576 = EDGE_LOOP ( 'NONE', ( #177057, #171128, #22602, #4017 ) ) ;
#156577 = PLANE ( 'NONE',  #100450 ) ;
#156578 = DIRECTION ( 'NONE',  ( 0.000000000000000000, 0.1298341882520022972, 0.9915357197604853789 ) ) ;
#156580 = ADVANCED_FACE ( 'NONE', ( #134343 ), #36587, .T. ) ;
#156579 = CARTESIAN_POINT ( 'NONE',  ( 22.49544290803804003, 64.25012976215469962, -203.5884194437818451 ) ) ;
#156581 = ORIENTED_EDGE ( 'NONE', *, *, #98314, .T. ) ;
#156582 = FACE_OUTER_BOUND ( 'NONE', #123158, .T. ) ;
#156583 = ADVANCED_FACE ( 'NONE', ( #156535 ), #236029, .F. ) ;
#156585 = VECTOR ( 'NONE', #178960, 1000.000000000000000 ) ;
#156584 = CARTESIAN_POINT ( 'NONE',  ( 20.94999999999999929, 87.39257802171759693, -106.0970570643561501 ) ) ;
#156586 = EDGE_LOOP ( 'NONE', ( #97596, #96085 ) ) ;
#156587 = ORIENTED_EDGE ( 'NONE', *, *, #122134, .T. ) ;
#156588 = FACE_OUTER_BOUND ( 'NONE', #75705, .T. ) ;
#156589 = ADVANCED_FACE ( 'NONE', ( #117373 ), #234749, .F. ) ;
#156590 = EDGE_CURVE ( 'NONE', #245594, #228258, #196899, .T. ) ;
#156591 = VECTOR ( 'NONE', #66337, 1000.000000000000000 ) ;
#156592 = CIRCLE ( 'NONE', #131598, 0.1000000000000028644 ) ;
#156593 = VERTEX_POINT ( 'NONE', #131794 ) ;
#156594 = LINE ( 'NONE', #134396, #138355 ) ;
#156595 = ORIENTED_EDGE ( 'NONE', *, *, #95248, .T. ) ;
#156596 = CARTESIAN_POINT ( 'NONE',  ( 20.89192007715128341, 10.32898536001801304, -173.0826683222764757 ) ) ;
#156597 = ADVANCED_FACE ( 'NONE', ( #91395 ), #152680, .T. ) ;
#156598 = LINE ( 'NONE', #236089, #35633 ) ;
#156599 = CARTESIAN_POINT ( 'NONE',  ( 20.94999999999999929, 60.83337574417770810, -225.3422414619148810 ) ) ;
#156600 = CARTESIAN_POINT ( 'NONE',  ( -16.86578989773640558, 63.08215007703680755, -213.0078429336296608 ) ) ;
#156601 = ADVANCED_FACE ( 'NONE', ( #114805 ), #92664, .T. ) ;
#156602 = EDGE_CURVE ( 'NONE', #127404, #167594, #13146, .T. ) ;
#156603 = CARTESIAN_POINT ( 'NONE',  ( 23.15000000000000213, 87.75000000001259082, -191.3731074845242688 ) ) ;
#156604 = CARTESIAN_POINT ( 'NONE',  ( 18.49362639424889210, -9.442604367877116545, -73.76444093351176434 ) ) ;
#156605 = FACE_BOUND ( 'NONE', #251107, .T. ) ;
#156606 = ORIENTED_EDGE ( 'NONE', *, *, #22050, .F. ) ;
#156608 = DIRECTION ( 'NONE',  ( -6.938893903907222067E-15, -1.000000000000000000, -7.272083257015735086E-15 ) ) ;
#156607 = CARTESIAN_POINT ( 'NONE',  ( 21.04999999999999716, 22.85780672939456792, -230.1006782354234872 ) ) ;
#156609 = AXIS2_PLACEMENT_3D ( 'NONE', #19023, #178124, #99812 ) ;
#156610 = ORIENTED_EDGE ( 'NONE', *, *, #63052, .F. ) ;
#156613 = ORIENTED_EDGE ( 'NONE', *, *, #137398, .F. ) ;
#156612 = DIRECTION ( 'NONE',  ( 0.000000000000000000, -6.982962677686266711E-15, 1.000000000000000000 ) ) ;
#156611 = CYLINDRICAL_SURFACE ( 'NONE', #94753, 0.09999999999999939493 ) ;
#156614 = EDGE_LOOP ( 'NONE', ( #49, #50030, #100485, #253953 ) ) ;
#156615 = DIRECTION ( 'NONE',  ( -1.000000000000000000, 0.000000000000000000, 0.000000000000000000 ) ) ;
#156616 = CIRCLE ( 'NONE', #235664, 0.09999999999999939493 ) ;
#156617 = CYLINDRICAL_SURFACE ( 'NONE', #126424, 0.09999999999999939493 ) ;
#156618 = DIRECTION ( 'NONE',  ( 1.000000000000000000, -0.000000000000000000, -0.000000000000000000 ) ) ;
#156619 = CARTESIAN_POINT ( 'NONE',  ( -20.94999999999999929, -11.74999999998884448, -63.89999999999999858 ) ) ;
#156620 = VERTEX_POINT ( 'NONE', #170977 ) ;
#156621 = CARTESIAN_POINT ( 'NONE',  ( -20.54999999999999716, -8.663551401858001100, -124.4758988819327215 ) ) ;
#156622 = AXIS2_PLACEMENT_3D ( 'NONE', #236061, #251777, #52271 ) ;
#156623 = ADVANCED_FACE ( 'NONE', ( #32741 ), #136929, .F. ) ;
#156624 = DIRECTION ( 'NONE',  ( 0.000000000000000000, 0.000000000000000000, 1.000000000000000000 ) ) ;
#156625 = VECTOR ( 'NONE', #100073, 1000.000000000000000 ) ;
#156627 = DIRECTION ( 'NONE',  ( 0.000000000000000000, 0.2128009952263601456, -0.9770955615653316162 ) ) ;
#156626 = DIRECTION ( 'NONE',  ( 0.000000000000000000, 1.000000000000000000, 0.000000000000000000 ) ) ;
#156628 = AXIS2_PLACEMENT_3D ( 'NONE', #87372, #246463, #226897 ) ;
#156630 = VERTEX_POINT ( 'NONE', #37858 ) ;
#156629 = CARTESIAN_POINT ( 'NONE',  ( 20.95000000000005258, 67.65000000001118963, -25.49719488170504533 ) ) ;
#156631 = ORIENTED_EDGE ( 'NONE', *, *, #254488, .F. ) ;
#156632 = CARTESIAN_POINT ( 'NONE',  ( 22.48660254037844197, 11.65000000001115588, -167.4499999999999602 ) ) ;
#156633 = AXIS2_PLACEMENT_3D ( 'NONE', #83150, #46610, #63626 ) ;
#156634 = CARTESIAN_POINT ( 'NONE',  ( -16.90202395485720288, 44.08058226997761153, -235.3060544617264327 ) ) ;
#156635 = ORIENTED_EDGE ( 'NONE', *, *, #256631, .T. ) ;
#156636 = DIRECTION ( 'NONE',  ( 1.000000000000000000, 0.000000000000000000, -0.000000000000000000 ) ) ;
#156637 = ORIENTED_EDGE ( 'NONE', *, *, #176789, .T. ) ;
#156638 = TOROIDAL_SURFACE ( 'NONE', #44182, 12.77500000000000036, 0.1000000000000000056 ) ;
#156639 = DIRECTION ( 'NONE',  ( 0.000000000000000000, -0.9667078373770112698, -0.2558827019434132821 ) ) ;
#156640 = CARTESIAN_POINT ( 'NONE',  ( 21.15000000000005187, 79.88763423575340994, -7.282924647898262549 ) ) ;
#156641 = CARTESIAN_POINT ( 'NONE',  ( 19.75857864376268935, 11.65000000001115943, -125.2500000000000284 ) ) ;
#156643 = ORIENTED_EDGE ( 'NONE', *, *, #28276, .F. ) ;
#156642 = VECTOR ( 'NONE', #33992, 1000.000000000000114 ) ;
#156644 = DIRECTION ( 'NONE',  ( 0.7071067811865475727, -0.6824534298470373850, 0.1850873201762210096 ) ) ;
#156645 = EDGE_CURVE ( 'NONE', #27482, #168945, #57375, .T. ) ;
#156647 = EDGE_CURVE ( 'NONE', #225791, #254838, #250456, .T. ) ;
#156646 = CARTESIAN_POINT ( 'NONE',  ( -18.59999999999999787, 6.933893972137497030, -137.7856458343736108 ) ) ;
#156648 = EDGE_LOOP ( 'NONE', ( #59157, #219691, #10777, #228826 ) ) ;
#156649 = ORIENTED_EDGE ( 'NONE', *, *, #42974, .T. ) ;
#156650 = ORIENTED_EDGE ( 'NONE', *, *, #3102, .F. ) ;
#156651 = ADVANCED_FACE ( 'NONE', ( #133088 ), #17003, .T. ) ;
#156652 = VERTEX_POINT ( 'NONE', #176090 ) ;
#156655 = EDGE_CURVE ( 'NONE', #3373, #36418, #15734, .T. ) ;
#156654 = ORIENTED_EDGE ( 'NONE', *, *, #217708, .T. ) ;
#156653 = CARTESIAN_POINT ( 'NONE',  ( 21.78635804494511419, 75.90099493450432533, -110.0587689696774873 ) ) ;
#156656 = VERTEX_POINT ( 'NONE', #253021 ) ;
#156657 = AXIS2_PLACEMENT_3D ( 'NONE', #254063, #38894, #118429 ) ;
#156658 = VECTOR ( 'NONE', #180987, 1000.000000000000000 ) ;
#156661 = ORIENTED_EDGE ( 'NONE', *, *, #124243, .F. ) ;
#156660 = VERTEX_POINT ( 'NONE', #255540 ) ;
#156659 = CARTESIAN_POINT ( 'NONE',  ( 23.24999999999999645, 1.115600667400684642E-11, -100.5000000000000426 ) ) ;
#156662 = CIRCLE ( 'NONE', #94071, 11.90000000000000213 ) ;
#156663 = EDGE_LOOP ( 'NONE', ( #217387, #46208, #88684 ) ) ;
#156664 = CYLINDRICAL_SURFACE ( 'NONE', #89718, 0.09999999999999609201 ) ;
#156665 = FACE_OUTER_BOUND ( 'NONE', #38750, .T. ) ;
#156666 = AXIS2_PLACEMENT_3D ( 'NONE', #92160, #128732, #251218 ) ;
#156667 = CARTESIAN_POINT ( 'NONE',  ( -16.83558968593873928, 14.15638303188477742, -219.2430492119315204 ) ) ;
#156668 = EDGE_LOOP ( 'NONE', ( #18111, #39661, #112379, #230016 ) ) ;
#156669 = CARTESIAN_POINT ( 'NONE',  ( -23.15000000000000213, 1.115600667400684642E-11, -134.0000000000000284 ) ) ;
#156671 = VERTEX_POINT ( 'NONE', #113519 ) ;
#156670 = CARTESIAN_POINT ( 'NONE',  ( 20.85000000000000142, -11.64999999998883595, -67.00000000000000000 ) ) ;
#156672 = CARTESIAN_POINT ( 'NONE',  ( -18.59999999999999787, -1.736705739456431807, -145.5174225876237699 ) ) ;
#156674 = ORIENTED_EDGE ( 'NONE', *, *, #182569, .F. ) ;
#156673 = DIRECTION ( 'NONE',  ( 9.044546369203339308E-15, -0.7397360091702694929, -0.6728971962616898672 ) ) ;
#156675 = CIRCLE ( 'NONE', #189959, 0.1000000000000028644 ) ;
#156676 = ORIENTED_EDGE ( 'NONE', *, *, #18492, .T. ) ;
#156677 = AXIS2_PLACEMENT_3D ( 'NONE', #103528, #183101, #4436 ) ;
#156678 = DIRECTION ( 'NONE',  ( 0.7071067811865474617, -0.7071067811865474617, -4.937700262164531476E-15 ) ) ;
#156679 = DIRECTION ( 'NONE',  ( 0.000000000000000000, -1.265107689135680095E-16, 1.000000000000000000 ) ) ;
#156680 = EDGE_LOOP ( 'NONE', ( #85665, #2373, #185892 ) ) ;
#156681 = ORIENTED_EDGE ( 'NONE', *, *, #151923, .F. ) ;
#156682 = DIRECTION ( 'NONE',  ( 1.000000000000000000, 0.000000000000000000, 0.000000000000000000 ) ) ;
#156683 = ADVANCED_FACE ( 'NONE', ( #53547 ), #147847, .T. ) ;
#156685 = ORIENTED_EDGE ( 'NONE', *, *, #131242, .T. ) ;
#156684 = EDGE_LOOP ( 'NONE', ( #207744, #18105, #91514, #166707, #195012 ) ) ;
#156686 = ORIENTED_EDGE ( 'NONE', *, *, #65177, .T. ) ;
#156687 = SPHERICAL_SURFACE ( 'NONE', #140923, 0.1000000000000000056 ) ;
#156688 = ORIENTED_EDGE ( 'NONE', *, *, #34729, .T. ) ;
#156689 = EDGE_LOOP ( 'NONE', ( #173010, #42041, #82302, #163382 ) ) ;
#156690 = CARTESIAN_POINT ( 'NONE',  ( -18.59999999999999787, 57.79742415652444265, -226.1319837253768981 ) ) ;
#156691 = CIRCLE ( 'NONE', #81593, 0.1000000000000054040 ) ;
#156692 = ORIENTED_EDGE ( 'NONE', *, *, #125289, .F. ) ;
#156693 = CARTESIAN_POINT ( 'NONE',  ( -16.93339986808596720, 12.44999860098303657, -211.1490805700459248 ) ) ;
#156695 = CARTESIAN_POINT ( 'NONE',  ( 21.00000000000000000, 9.750000000011153745, -146.3500000000000227 ) ) ;
#156694 = CARTESIAN_POINT ( 'NONE',  ( 23.24999999999999645, -2.099999999988846344, -100.5000000000000426 ) ) ;
#156696 = EDGE_CURVE ( 'NONE', #952, #174802, #168543, .T. ) ;
#156697 = ORIENTED_EDGE ( 'NONE', *, *, #70009, .T. ) ;
#156698 = ADVANCED_FACE ( 'NONE', ( #237323 ), #221576, .T. ) ;
#156699 = ORIENTED_EDGE ( 'NONE', *, *, #101950, .T. ) ;
#156700 = CARTESIAN_POINT ( 'NONE',  ( -18.50000000000000000, 66.65000000001150227, -48.37310748452438958 ) ) ;
#156701 = ORIENTED_EDGE ( 'NONE', *, *, #111257, .F. ) ;
#156702 = AXIS2_PLACEMENT_3D ( 'NONE', #151950, #117916, #132355 ) ;
#156703 = CIRCLE ( 'NONE', #10942, 0.09999999999999939493 ) ;
#156704 = EDGE_CURVE ( 'NONE', #194806, #167959, #10290, .T. ) ;
#156705 = DIRECTION ( 'NONE',  ( -1.000000000000000000, 0.000000000000000000, -0.000000000000000000 ) ) ;
#156706 = ORIENTED_EDGE ( 'NONE', *, *, #66169, .T. ) ;
#156707 = ORIENTED_EDGE ( 'NONE', *, *, #34208, .F. ) ;
#156708 = DIRECTION ( 'NONE',  ( 0.000000000000000000, 6.982962677686266711E-15, -1.000000000000000000 ) ) ;
#156711 = ADVANCED_FACE ( 'NONE', ( #222876 ), #177379, .F. ) ;
#156710 = VERTEX_POINT ( 'NONE', #78231 ) ;
#156709 = DIRECTION ( 'NONE',  ( 0.000000000000000000, -0.2128009952263604232, 0.9770955615653316162 ) ) ;
#156712 = CARTESIAN_POINT ( 'NONE',  ( 18.59999999999996945, 10.33248238083634440, -206.5948465439131496 ) ) ;
#156713 = DIRECTION ( 'NONE',  ( 0.000000000000000000, 0.9893560106964510714, -0.1455152366551481502 ) ) ;
#156714 = VERTEX_POINT ( 'NONE', #256819 ) ;
#156715 = EDGE_CURVE ( 'NONE', #13140, #24943, #138190, .T. ) ;
#156716 = CARTESIAN_POINT ( 'NONE',  ( 18.59999999999998721, 56.14960075277838314, -100.7428044267230973 ) ) ;
#156717 = CARTESIAN_POINT ( 'NONE',  ( -20.94999999999999929, 5.849999999999949019, -10.13249722427797117 ) ) ;
#156718 = CARTESIAN_POINT ( 'NONE',  ( 18.49999999999999645, 16.56538529403860238, -240.6448716151659823 ) ) ;
#156719 = CARTESIAN_POINT ( 'NONE',  ( -20.94999999999999929, 87.65000000001266756, -200.6231074845242688 ) ) ;
#156720 = DIRECTION ( 'NONE',  ( 0.7071067811865475727, -0.2890913453342130457, 0.6453109281988449464 ) ) ;
#156721 = CARTESIAN_POINT ( 'NONE',  ( -16.97683809663752186, 62.88879881541066652, -213.8537543555185607 ) ) ;
#156722 = CARTESIAN_POINT ( 'NONE',  ( -21.12642695952773764, 69.62434007797649826, -69.62201076771371788 ) ) ;
#156724 = EDGE_CURVE ( 'NONE', #247553, #80054, #255919, .T. ) ;
#156723 = CARTESIAN_POINT ( 'NONE',  ( 18.60000000000000142, -9.321008403350125704, -74.23593824907794669 ) ) ;
#156725 = CARTESIAN_POINT ( 'NONE',  ( -20.85000000000000142, 68.97833521811131163, -32.18954208262707795 ) ) ;
#156726 = CIRCLE ( 'NONE', #202481, 0.09999999999999938105 ) ;
#156727 = CIRCLE ( 'NONE', #123371, 3.999999999999999112 ) ;
#156728 = ORIENTED_EDGE ( 'NONE', *, *, #59591, .T. ) ;
#156730 = ORIENTED_EDGE ( 'NONE', *, *, #116118, .T. ) ;
#156729 = ORIENTED_EDGE ( 'NONE', *, *, #130520, .F. ) ;
#156731 = VECTOR ( 'NONE', #206555, 1000.000000000000000 ) ;
#156732 = ORIENTED_EDGE ( 'NONE', *, *, #103815, .T. ) ;
#156734 = EDGE_CURVE ( 'NONE', #196891, #40351, #6162, .T. ) ;
#156733 = CARTESIAN_POINT ( 'NONE',  ( 21.14999999999999858, 76.00000000001271871, -210.0637644362255969 ) ) ;
#156735 = CARTESIAN_POINT ( 'NONE',  ( -23.15000000000000213, 2.000000000011154189, -87.27537807723794572 ) ) ;
#156737 = DIRECTION ( 'NONE',  ( 0.000000000000000000, 0.000000000000000000, -1.000000000000000000 ) ) ;
#156736 = DIRECTION ( 'NONE',  ( 2.694716079187273439E-16, 1.000000000000000000, 6.467318590049456648E-15 ) ) ;
#156738 = ORIENTED_EDGE ( 'NONE', *, *, #224783, .F. ) ;
#156739 = CARTESIAN_POINT ( 'NONE',  ( 20.94999999999999929, 1.115600667400684642E-11, -136.0000000000000284 ) ) ;
#156740 =( LENGTH_UNIT ( ) NAMED_UNIT ( * ) SI_UNIT ( .MILLI., .METRE. ) );
#156741 = CARTESIAN_POINT ( 'NONE',  ( 20.94999999999999929, 6.511710453938116316, -230.8991241839006534 ) ) ;
#156742 = CARTESIAN_POINT ( 'NONE',  ( -20.90000000000000213, -11.75000000000000000, -15.00000000000000000 ) ) ;
#156743 = CARTESIAN_POINT ( 'NONE',  ( 18.59999999999999432, -1.162701749926853712, -108.6000000000000227 ) ) ;
#156744 = EDGE_LOOP ( 'NONE', ( #112387, #208262, #176529, #193851 ) ) ;
#156745 = CIRCLE ( 'NONE', #119299, 0.1000000000000028644 ) ;
#156746 = CARTESIAN_POINT ( 'NONE',  ( 20.85000000000000142, -1.835859311443637010, -45.00443916879852679 ) ) ;
#156747 = ORIENTED_EDGE ( 'NONE', *, *, #190900, .T. ) ;
#156748 = CARTESIAN_POINT ( 'NONE',  ( -20.54999999999999716, -7.176961358819843539, -212.6889627706600834 ) ) ;
#156749 = CARTESIAN_POINT ( 'NONE',  ( 18.48197441911733208, 77.41062428956240637, -241.7243103415940766 ) ) ;
#156750 = CARTESIAN_POINT ( 'NONE',  ( 21.05000000000000071, -11.64999999998883595, -197.8999999999999773 ) ) ;
#156751 = CARTESIAN_POINT ( 'NONE',  ( 21.13736287352038445, 61.88639443390047745, -224.8213959476306911 ) ) ;
#156752 = DIRECTION ( 'NONE',  ( 0.000000000000000000, 0.000000000000000000, -1.000000000000000000 ) ) ;
#156753 = CARTESIAN_POINT ( 'NONE',  ( -23.15000000000000213, 7.554435330547284444, -235.6868924355707691 ) ) ;
#156754 = ORIENTED_EDGE ( 'NONE', *, *, #192949, .T. ) ;
#156755 = CARTESIAN_POINT ( 'NONE',  ( -21.04999999999994387, 77.83551161375991967, -47.52760213295649550 ) ) ;
#156756 = CYLINDRICAL_SURFACE ( 'NONE', #22632, 0.09999999999999939493 ) ;
#156757 = FACE_OUTER_BOUND ( 'NONE', #8104, .T. ) ;
#156759 = FACE_OUTER_BOUND ( 'NONE', #127931, .T. ) ;
#156758 = CARTESIAN_POINT ( 'NONE',  ( -21.44999999999999929, 65.89281126173843006, -213.4744760240239145 ) ) ;
#156760 = CARTESIAN_POINT ( 'NONE',  ( 20.94999999999999929, 1.115625160336667635E-11, -65.00000000000000000 ) ) ;
#156761 = DIRECTION ( 'NONE',  ( 0.000000000000000000, 0.000000000000000000, -1.000000000000000000 ) ) ;
#156762 = FACE_OUTER_BOUND ( 'NONE', #2662, .T. ) ;
#156763 = CARTESIAN_POINT ( 'NONE',  ( 22.46250603428203618, 75.97885582387323211, -114.6729705818644049 ) ) ;
#156764 = AXIS2_PLACEMENT_3D ( 'NONE', #159689, #222190, #179270 ) ;
#156765 = EDGE_LOOP ( 'NONE', ( #24197, #192388, #141684, #178438 ) ) ;
#156766 = AXIS2_PLACEMENT_3D ( 'NONE', #123306, #202829, #24218 ) ;
#156767 = ADVANCED_FACE ( 'NONE', ( #44263 ), #219025, .F. ) ;
#156769 = ORIENTED_EDGE ( 'NONE', *, *, #83205, .F. ) ;
#156768 =( GEOMETRIC_REPRESENTATION_CONTEXT ( 3 ) GLOBAL_UNCERTAINTY_ASSIGNED_CONTEXT ( ( #79213 ) ) GLOBAL_UNIT_ASSIGNED_CONTEXT ( ( #209015, #150340, #109897 ) ) REPRESENTATION_CONTEXT ( 'NONE', 'WORKASPACE' ) );
#156770 = LINE ( 'NONE', #115049, #202816 ) ;
#156771 = ORIENTED_EDGE ( 'NONE', *, *, #237569, .F. ) ;
#156772 = EDGE_CURVE ( 'NONE', #7959, #30904, #198185, .T. ) ;
#156773 = LINE ( 'NONE', #38097, #51373 ) ;
#156774 = EDGE_CURVE ( 'NONE', #248466, #19155, #62535, .T. ) ;
#156775 = ADVANCED_FACE ( 'NONE', ( #238600, #61248, #200759 ), #122519, .T. ) ;
#156776 = FACE_OUTER_BOUND ( 'NONE', #164832, .T. ) ;
#156777 = CIRCLE ( 'NONE', #44336, 0.09999999999999062417 ) ;
#156778 = VERTEX_POINT ( 'NONE', #202044 ) ;
#156779 = DIRECTION ( 'NONE',  ( -0.000000000000000000, 0.01283462868039629209, -0.9999176327611372095 ) ) ;
#156780 = AXIS2_PLACEMENT_3D ( 'NONE', #90506, #108791, #85350 ) ;
#156781 = CARTESIAN_POINT ( 'NONE',  ( -12.33960340485503870, 9.360749169926263491, -50.81457014060730160 ) ) ;
#156782 = LINE ( 'NONE', #133346, #157048 ) ;
#156783 = CARTESIAN_POINT ( 'NONE',  ( 18.39999999999999858, -9.499999999988842703, -40.53206939669966857 ) ) ;
#156786 = ORIENTED_EDGE ( 'NONE', *, *, #135584, .T. ) ;
#156785 = DIRECTION ( 'NONE',  ( 0.000000000000000000, 1.000000000000000000, 0.000000000000000000 ) ) ;
#156784 = AXIS2_PLACEMENT_3D ( 'NONE', #125741, #255262, #197901 ) ;
#156788 = CARTESIAN_POINT ( 'NONE',  ( 19.80993210785717196, 11.75000000000834177, -192.2671177488814749 ) ) ;
#156787 = DIRECTION ( 'NONE',  ( 1.000000000000000000, 0.000000000000000000, 0.000000000000000000 ) ) ;
#156789 = EDGE_CURVE ( 'NONE', #84395, #217417, #247599, .T. ) ;
#156790 = DIRECTION ( 'NONE',  ( 1.000000000000000000, -0.000000000000000000, -0.000000000000000000 ) ) ;
#156791 =( BOUNDED_SURFACE ( )  B_SPLINE_SURFACE ( 3, 2, ( 
 ( #9116, #88618, #202176 ),
 ( #168226, #5226, #204726 ),
 ( #6532, #7838, #126485 ),
 ( #225562, #247718, #243859 ),
 ( #223005, #23582, #65224 ),
 ( #103053, #44400, #164345 ),
 ( #104332, #105609, #46928 ),
 ( #183897, #185180, #224298 ),
 ( #206029, #45670, #27431 ),
 ( #50776, #254121, #95058 ) ),
 .UNSPECIFIED., .F., .F., .F. ) 
 B_SPLINE_SURFACE_WITH_KNOTS ( ( 4, 2, 2, 2, 4 ),
 ( 3, 3 ),
 ( 0.0001836757140119138357, 0.0004000170051583584025, 0.0005081876507315807130, 0.0005622729735181917869, 0.0006163582963048029693 ),
 ( 0.000000000000000000, 1.000000000000000000 ),
 .UNSPECIFIED. ) 
 GEOMETRIC_REPRESENTATION_ITEM ( )  RATIONAL_B_SPLINE_SURFACE ( (
 ( 1.000000000000000000, 0.7071067811865933139, 1.000000000000000000),
 ( 1.000000000000000000, 0.6461995200037486953, 1.000000000000000000),
 ( 1.000000000000000000, 0.5776453529538307929, 1.000000000000000000),
 ( 1.000000000000000000, 0.4585233068357276176, 1.000000000000000000),
 ( 1.000000000000000000, 0.4154092989952298254, 1.000000000000000000),
 ( 1.000000000000000000, 0.3550093145831299535, 1.000000000000000000),
 ( 1.000000000000000000, 0.3354498651682248367, 1.000000000000000000),
 ( 1.000000000000000000, 0.3060347992260692429, 1.000000000000000000),
 ( 1.000000000000000000, 0.2963555829624867632, 1.000000000000000000),
 ( 1.000000000000000000, 0.2966190024559665073, 1.000000000000000000) ) ) 
 REPRESENTATION_ITEM ( '' )  SURFACE ( )  );
#156792 = DIRECTION ( 'NONE',  ( 0.000000000000000000, -1.000000000000000000, -6.352154140967427193E-15 ) ) ;
#156793 = VECTOR ( 'NONE', #60647, 1000.000000000000227 ) ;
#156794 = FACE_OUTER_BOUND ( 'NONE', #99552, .T. ) ;
#156796 = ADVANCED_FACE ( 'NONE', ( #23438 ), #121266, .T. ) ;
#156795 = SPHERICAL_SURFACE ( 'NONE', #241585, 0.1000000000000000056 ) ;
#156798 = VERTEX_POINT ( 'NONE', #241185 ) ;
#156797 = VECTOR ( 'NONE', #206702, 1000.000000000000000 ) ;
#156799 = DIRECTION ( 'NONE',  ( 1.000000000000000000, 0.000000000000000000, 0.000000000000000000 ) ) ;
#156800 = PLANE ( 'NONE',  #212576 ) ;
#156801 = ORIENTED_EDGE ( 'NONE', *, *, #249567, .T. ) ;
#156802 = CARTESIAN_POINT ( 'NONE',  ( -16.88593481969334320, 66.04943990992822478, -182.6712352275799276 ) ) ;
#156803 = ORIENTED_EDGE ( 'NONE', *, *, #140788, .T. ) ;
#156804 = AXIS2_PLACEMENT_3D ( 'NONE', #19055, #214682, #36069 ) ;
#156805 = DIRECTION ( 'NONE',  ( 0.000000000000000000, -0.9770955615653315052, -0.2128009952263603954 ) ) ;
#156806 = AXIS2_PLACEMENT_3D ( 'NONE', #247142, #170243, #213158 ) ;
#156807 = CIRCLE ( 'NONE', #123646, 0.09999999999999939493 ) ;
#156808 = EDGE_CURVE ( 'NONE', #143581, #11117, #210201, .T. ) ;
#156809 = DIRECTION ( 'NONE',  ( 2.715809747126117987E-16, 1.000000000000000000, 6.517943393102682774E-15 ) ) ;
#156810 = DIRECTION ( 'NONE',  ( 0.000000000000000000, -0.9594490217226104845, -0.2818822000686205809 ) ) ;
#156811 = ADVANCED_FACE ( 'NONE', ( #83343 ), #162938, .F. ) ;
#156812 = ORIENTED_EDGE ( 'NONE', *, *, #249128, .T. ) ;
#156813 = EDGE_CURVE ( 'NONE', #170648, #52565, #18270, .T. ) ;
#156814 = AXIS2_PLACEMENT_3D ( 'NONE', #213374, #34785, #76434 ) ;
#156815 = ORIENTED_EDGE ( 'NONE', *, *, #86285, .F. ) ;
#156816 = CARTESIAN_POINT ( 'NONE',  ( 21.13461538461538325, 8.885417037985616773, -112.8500000000000369 ) ) ;
#156817 = FACE_OUTER_BOUND ( 'NONE', #179887, .T. ) ;
#156818 = CARTESIAN_POINT ( 'NONE',  ( 21.07928932188134397, -1.250084634896337255, -194.7953894783290423 ) ) ;
#156819 = LINE ( 'NONE', #176374, #182002 ) ;
#156820 = AXIS2_PLACEMENT_3D ( 'NONE', #233004, #251240, #191321 ) ;
#156821 = EDGE_CURVE ( 'NONE', #231797, #243814, #180974, .T. ) ;
#156823 = LINE ( 'NONE', #40729, #211845 ) ;
#156822 = CARTESIAN_POINT ( 'NONE',  ( -20.00857864376270001, 9.150000000011157653, -88.25000000000005684 ) ) ;
#156824 = CARTESIAN_POINT ( 'NONE',  ( -18.40000000000000213, 58.56629890316250453, -223.9209570932885356 ) ) ;
#156825 = CARTESIAN_POINT ( 'NONE',  ( 21.05000000000000071, 65.27628289530434813, -90.87310748452438247 ) ) ;
#156826 = DIRECTION ( 'NONE',  ( -1.000000000000000000, 0.000000000000000000, 0.000000000000000000 ) ) ;
#156827 = ORIENTED_EDGE ( 'NONE', *, *, #101487, .F. ) ;
#156828 = DIRECTION ( 'NONE',  ( 6.938893903906363786E-14, -0.2617529984165152257, -0.9651348961777124202 ) ) ;
#156829 = VERTEX_POINT ( 'NONE', #228026 ) ;
#156830 = CARTESIAN_POINT ( 'NONE',  ( 22.59999999999999432, 11.74956712348939192, 0.1008583690987083364 ) ) ;
#156831 = DIRECTION ( 'NONE',  ( 1.000000000000000000, -0.000000000000000000, -0.000000000000000000 ) ) ;
#156833 = CARTESIAN_POINT ( 'NONE',  ( -20.64999999999999858, 1.115600667400684642E-11, -67.00000000000000000 ) ) ;
#156832 = CARTESIAN_POINT ( 'NONE',  ( 23.14999999999999503, 11.65000000001116298, -45.75000000000000711 ) ) ;
#156834 = EDGE_LOOP ( 'NONE', ( #162332, #256391, #127636, #241335 ) ) ;
#156836 = DIRECTION ( 'NONE',  ( -1.000000000000000000, 0.000000000000000000, 0.000000000000000000 ) ) ;
#156835 = CARTESIAN_POINT ( 'NONE',  ( 18.59999999999999076, 10.20857864377385127, -155.3500000000000227 ) ) ;
#156837 = LINE ( 'NONE', #199805, #87070 ) ;
#156838 = CARTESIAN_POINT ( 'NONE',  ( 23.14999999999999503, 64.25000000001244871, -181.7731074845244450 ) ) ;
#156839 = DIRECTION ( 'NONE',  ( 1.000000000000000000, 0.000000000000000000, 0.000000000000000000 ) ) ;
#156840 = DIRECTION ( 'NONE',  ( 1.836970198721029934E-16, 0.9651348961777157509, -0.2617529984165031243 ) ) ;
#156841 = ORIENTED_EDGE ( 'NONE', *, *, #64497, .F. ) ;
#156842 = CARTESIAN_POINT ( 'NONE',  ( -22.48970261584618058, 31.84544391280713072, -238.9419228052725543 ) ) ;
#156843 = AXIS2_PLACEMENT_3D ( 'NONE', #167839, #148242, #227776 ) ;
#156844 = EDGE_LOOP ( 'NONE', ( #242620, #71992, #24975, #252516 ) ) ;
#156845 = EDGE_CURVE ( 'NONE', #228584, #89549, #40111, .T. ) ;
#156846 = AXIS2_PLACEMENT_3D ( 'NONE', #35528, #36809, #94163 ) ;
#156847 = VECTOR ( 'NONE', #138605, 1000.000000000000000 ) ;
#156848 = DIRECTION ( 'NONE',  ( 0.000000000000000000, 0.2617529984165046231, 0.9651348961777154178 ) ) ;
#156849 = ORIENTED_EDGE ( 'NONE', *, *, #42375, .F. ) ;
#156850 = CARTESIAN_POINT ( 'NONE',  ( -20.85882249326303040, 46.46967969402478360, -243.0849751855955674 ) ) ;
#156851 = VERTEX_POINT ( 'NONE', #128934 ) ;
#156852 = AXIS2_PLACEMENT_3D ( 'NONE', #162427, #21624, #167260 ) ;
#156853 = LINE ( 'NONE', #137251, #226664 ) ;
#156854 = ADVANCED_FACE ( 'NONE', ( #245015 ), #70266, .T. ) ;
#156855 = DIRECTION ( 'NONE',  ( -0.000000000000000000, 0.9126074666063770380, 0.4088369013363281068 ) ) ;
#156856 = VERTEX_POINT ( 'NONE', #248877 ) ;
#156857 = VECTOR ( 'NONE', #173779, 1000.000000000000000 ) ;
#156858 = EDGE_CURVE ( 'NONE', #218618, #218857, #135148, .T. ) ;
#156860 = AXIS2_PLACEMENT_3D ( 'NONE', #154571, #176687, #94549 ) ;
#156859 = CARTESIAN_POINT ( 'NONE',  ( -18.41418431465367789, -9.499999999989068300, -174.1001893912213916 ) ) ;
#156861 = CARTESIAN_POINT ( 'NONE',  ( 21.05000000000000071, 67.23127455305835554, -235.8551265064784559 ) ) ;
#156862 = VECTOR ( 'NONE', #198166, 1000.000000000000227 ) ;
#156863 = DIRECTION ( 'NONE',  ( -1.000000000000000000, -2.952720810173289112E-16, 0.000000000000000000 ) ) ;
#156864 = DIRECTION ( 'NONE',  ( 0.000000000000000000, -0.4721928772777346239, -0.8814952561688430555 ) ) ;
#156865 = DIRECTION ( 'NONE',  ( 0.000000000000000000, 0.4721928772777346239, 0.8814952561688430555 ) ) ;
#156866 = ORIENTED_EDGE ( 'NONE', *, *, #36347, .T. ) ;
#156867 = DIRECTION ( 'NONE',  ( 0.000000000000000000, 0.8741572761215442577, -0.4856429311786202851 ) ) ;
#156868 = ORIENTED_EDGE ( 'NONE', *, *, #94855, .F. ) ;
#156870 = VERTEX_POINT ( 'NONE', #147201 ) ;
#156869 = DIRECTION ( 'NONE',  ( 1.000000000000000000, 7.304098846218134667E-16, 5.100424963727256530E-30 ) ) ;
#156871 = ADVANCED_FACE ( 'NONE', ( #89781 ), #246307, .T. ) ;
#156872 = VERTEX_POINT ( 'NONE', #50645 ) ;
#156873 = CARTESIAN_POINT ( 'NONE',  ( 21.53752568622135044, 0.09897446127761702628, -60.21319212545145660 ) ) ;
#156874 = EDGE_CURVE ( 'NONE', #58429, #217887, #48093, .T. ) ;
#156875 = CARTESIAN_POINT ( 'NONE',  ( 14.77516762759922209, 66.56332574816974557, -188.3462455535252502 ) ) ;
#156876 = CARTESIAN_POINT ( 'NONE',  ( 20.85000000000000142, 77.83585931145546510, -91.41866831572575336 ) ) ;
#156877 = DIRECTION ( 'NONE',  ( -1.000000000000000000, 0.000000000000000000, 0.000000000000000000 ) ) ;
#156879 = ORIENTED_EDGE ( 'NONE', *, *, #210933, .T. ) ;
#156878 = AXIS2_PLACEMENT_3D ( 'NONE', #236813, #77727, #41223 ) ;
#156880 = CARTESIAN_POINT ( 'NONE',  ( -23.39999999999994529, 83.80000000001119531, -37.18565239344504647 ) ) ;
#156881 = DIRECTION ( 'NONE',  ( 0.000000000000000000, 0.000000000000000000, 1.000000000000000000 ) ) ;
#156882 = ORIENTED_EDGE ( 'NONE', *, *, #210005, .F. ) ;
#156884 = ORIENTED_EDGE ( 'NONE', *, *, #119025, .T. ) ;
#156883 = CARTESIAN_POINT ( 'NONE',  ( -16.91256925476570672, 66.01426884188381905, -115.5554649955190882 ) ) ;
#156885 = FACE_OUTER_BOUND ( 'NONE', #208143, .T. ) ;
#156886 = EDGE_CURVE ( 'NONE', #132493, #28102, #28597, .T. ) ;
#156887 = CARTESIAN_POINT ( 'NONE',  ( 22.39999999999999503, 7.790779598384535376, -100.5000000000000284 ) ) ;
#156888 = AXIS2_PLACEMENT_3D ( 'NONE', #25269, #202605, #140038 ) ;
#156889 = ORIENTED_EDGE ( 'NONE', *, *, #87612, .F. ) ;
#156890 = VECTOR ( 'NONE', #30705, 1000.000000000000000 ) ;
#156891 = CIRCLE ( 'NONE', #52780, 0.5000000000000004441 ) ;
#156892 = ADVANCED_FACE ( 'NONE', ( #27292 ), #67661, .F. ) ;
#156893 = CARTESIAN_POINT ( 'NONE',  ( 21.04386569057533762, 64.25000000001236344, -109.8802701327437319 ) ) ;
#156894 = ORIENTED_EDGE ( 'NONE', *, *, #106254, .F. ) ;
#156895 = DIRECTION ( 'NONE',  ( 1.000000000000000000, 0.000000000000000000, 0.000000000000000000 ) ) ;
#156896 = EDGE_CURVE ( 'NONE', #227165, #146767, #169378, .T. ) ;
#156897 = DIRECTION ( 'NONE',  ( 0.000000000000000000, 0.4999999999999956701, -0.8660254037844411501 ) ) ;
#156898 = CARTESIAN_POINT ( 'NONE',  ( 13.77030915526558275, 66.54399267394222761, -51.03447399037763432 ) ) ;
#156899 = DIRECTION ( 'NONE',  ( -1.000000000000000000, -1.594516344651357984E-15, 4.324467345337419894E-16 ) ) ;
#156900 = ADVANCED_FACE ( 'NONE', ( #24720, #164213 ), #243736, .F. ) ;
#156901 = CIRCLE ( 'NONE', #165237, 0.1000000000000028644 ) ;
#156902 = ADVANCED_FACE ( 'NONE', ( #15411 ), #97726, .F. ) ;
#156903 = AXIS2_PLACEMENT_3D ( 'NONE', #11478, #90994, #48012 ) ;
#156904 = AXIS2_PLACEMENT_3D ( 'NONE', #77029, #34103, #177456 ) ;
#156905 = ORIENTED_EDGE ( 'NONE', *, *, #42406, .T. ) ;
#156906 = CARTESIAN_POINT ( 'NONE',  ( 21.05000000000000071, 67.22371710471912820, -60.96447848938343839 ) ) ;
#156907 = AXIS2_PLACEMENT_3D ( 'NONE', #168771, #93023, #209117 ) ;
#156908 = ORIENTED_EDGE ( 'NONE', *, *, #219086, .T. ) ;
#156909 = DIRECTION ( 'NONE',  ( 0.000000000000000000, -0.9908441862701791170, 0.1350103645450472789 ) ) ;
#156910 = DIRECTION ( 'NONE',  ( -1.000000000000000000, -0.000000000000000000, -0.000000000000000000 ) ) ;
#156912 = ORIENTED_EDGE ( 'NONE', *, *, #198020, .T. ) ;
#156911 = LINE ( 'NONE', #214291, #54286 ) ;
#156914 = ADVANCED_FACE ( 'NONE', ( #175770 ), #234425, .F. ) ;
#156913 = DIRECTION ( 'NONE',  ( -1.000000000000000000, 0.000000000000000000, 0.000000000000000000 ) ) ;
#156915 = DIRECTION ( 'NONE',  ( 0.000000000000000000, 0.000000000000000000, -1.000000000000000000 ) ) ;
#156916 = LINE ( 'NONE', #59027, #101968 ) ;
#156917 = CARTESIAN_POINT ( 'NONE',  ( -20.85000000000000497, 64.25000000001148237, -42.94225473048309993 ) ) ;
#156918 = CARTESIAN_POINT ( 'NONE',  ( -17.11825945287482753, 12.43531352672262003, -211.3405985074572300 ) ) ;
#156919 = EDGE_CURVE ( 'NONE', #32896, #111115, #192759, .T. ) ;
#156920 = LINE ( 'NONE', #117756, #84819 ) ;
#156921 = DIRECTION ( 'NONE',  ( 0.000000000000000000, 2.168404344971247498E-15, 1.000000000000000000 ) ) ;
#156923 = ORIENTED_EDGE ( 'NONE', *, *, #174541, .F. ) ;
#156922 = CARTESIAN_POINT ( 'NONE',  ( -20.54999999999999716, 5.256951610580939516, -213.3897168960460533 ) ) ;
#156924 = AXIS2_PLACEMENT_3D ( 'NONE', #37715, #254150, #255394 ) ;
#156925 = CARTESIAN_POINT ( 'NONE',  ( 21.05000000000000071, 71.00000000001199396, -115.4283735034374274 ) ) ;
#156926 = CARTESIAN_POINT ( 'NONE',  ( -18.50000000000000000, 85.48068669529064323, -62.58199231576639932 ) ) ;
#156927 = CARTESIAN_POINT ( 'NONE',  ( -18.41799967126735282, 85.50000000001263345, -196.4910376712677476 ) ) ;
#156928 = VECTOR ( 'NONE', #1523, 1000.000000000000227 ) ;
#156929 = ORIENTED_EDGE ( 'NONE', *, *, #47286, .F. ) ;
#156930 = CARTESIAN_POINT ( 'NONE',  ( -20.94999999999999929, -11.64999999998884483, -198.0999999999999659 ) ) ;
#156931 = CARTESIAN_POINT ( 'NONE',  ( -18.46093223321764754, 85.48068296828618884, -62.43855697059758114 ) ) ;
#156932 = CIRCLE ( 'NONE', #148544, 0.1000000000000028644 ) ;
#156933 = ORIENTED_EDGE ( 'NONE', *, *, #223728, .F. ) ;
#156934 = AXIS2_PLACEMENT_3D ( 'NONE', #23615, #50812, #7883 ) ;
#156935 = CIRCLE ( 'NONE', #86157, 1.999999999999994893 ) ;
#156937 = EDGE_CURVE ( 'NONE', #54007, #247013, #243500, .T. ) ;
#156936 = CARTESIAN_POINT ( 'NONE',  ( -40.23850191057533010, 64.35000000001119247, -6.123107484524794586 ) ) ;
#156938 = CYLINDRICAL_SURFACE ( 'NONE', #84775, 0.09999999999999810429 ) ;
#156939 = AXIS2_PLACEMENT_3D ( 'NONE', #9241, #142325, #64082 ) ;
#156940 = ORIENTED_EDGE ( 'NONE', *, *, #204020, .F. ) ;
#156941 = DIRECTION ( 'NONE',  ( 0.000000000000000000, 0.9126074666063770380, 0.4088369013363281068 ) ) ;
#156942 = EDGE_LOOP ( 'NONE', ( #139349, #150310, #49842, #192867 ) ) ;
#156943 = CARTESIAN_POINT ( 'NONE',  ( -23.25000000000000000, 55.89093952297024970, -232.7795287750844579 ) ) ;
#156944 = CIRCLE ( 'NONE', #86160, 0.1000000000000003525 ) ;
#156946 = ORIENTED_EDGE ( 'NONE', *, *, #223149, .F. ) ;
#156945 = CARTESIAN_POINT ( 'NONE',  ( 21.05000000000000071, 6.257814610487288043, -133.9022097086912311 ) ) ;
#156947 = DIRECTION ( 'NONE',  ( 1.000000000000000000, 0.000000000000000000, 0.000000000000000000 ) ) ;
#156948 = EDGE_LOOP ( 'NONE', ( #139283, #190630, #142455 ) ) ;
#156949 = CARTESIAN_POINT ( 'NONE',  ( 23.15000000000000213, 85.00000000001261924, -193.6291383618718385 ) ) ;
#156950 = VERTEX_POINT ( 'NONE', #235709 ) ;
#156952 = ORIENTED_EDGE ( 'NONE', *, *, #132290, .T. ) ;
#156951 = ORIENTED_EDGE ( 'NONE', *, *, #106231, .T. ) ;
#156953 = CARTESIAN_POINT ( 'NONE',  ( 23.14999999999999858, 37.65052946403260137, -247.7000226632887916 ) ) ;
#156954 = ORIENTED_EDGE ( 'NONE', *, *, #127293, .T. ) ;
#156955 = EDGE_CURVE ( 'NONE', #44654, #202405, #226941, .T. ) ;
#156956 = DIRECTION ( 'NONE',  ( 0.000000000000000000, -6.982962677686266711E-15, 1.000000000000000000 ) ) ;
#156958 = EDGE_LOOP ( 'NONE', ( #113209, #76469, #7158, #130659, #232490, #66792, #17168, #121927, #130480, #107035 ) ) ;
#156957 = AXIS2_PLACEMENT_3D ( 'NONE', #62813, #223159, #163212 ) ;
#156959 = AXIS2_PLACEMENT_3D ( 'NONE', #179079, #216876, #117786 ) ;
#156960 = VECTOR ( 'NONE', #254509, 1000.000000000000000 ) ;
#156961 = VERTEX_POINT ( 'NONE', #212332 ) ;
#156962 = AXIS2_PLACEMENT_3D ( 'NONE', #33756, #134076, #72869 ) ;
#156963 = DIRECTION ( 'NONE',  ( -1.020425574104004196E-15, -1.210927747993693964E-31, 1.000000000000000000 ) ) ;
#156964 = DIRECTION ( 'NONE',  ( -1.000000000000000000, 0.000000000000000000, 0.000000000000000000 ) ) ;
#156965 = CARTESIAN_POINT ( 'NONE',  ( -21.05000000000000071, 74.73821383144760944, -195.4366085209788935 ) ) ;
#156966 = DIRECTION ( 'NONE',  ( 0.000000000000000000, -0.4999999999999478195, 0.8660254037844686836 ) ) ;
#156967 = ORIENTED_EDGE ( 'NONE', *, *, #5027, .F. ) ;
#156968 = CIRCLE ( 'NONE', #107042, 0.09999999999999646672 ) ;
#156969 = DIRECTION ( 'NONE',  ( 0.000000000000000000, 7.026728003956683390E-15, -1.000000000000000000 ) ) ;
#156970 = AXIS2_PLACEMENT_3D ( 'NONE', #21074, #78437, #56298 ) ;
#156971 = FACE_OUTER_BOUND ( 'NONE', #126884, .T. ) ;
#156972 = DIRECTION ( 'NONE',  ( 1.186688945009010077E-16, 1.000000000000000000, 6.982962677686266711E-15 ) ) ;
#156973 = EDGE_LOOP ( 'NONE', ( #27412, #131668, #78129, #254185 ) ) ;
#156974 = DIRECTION ( 'NONE',  ( 1.000000000000000000, 0.000000000000000000, 0.000000000000000000 ) ) ;
#156975 = DIRECTION ( 'NONE',  ( 1.000000000000000000, 0.000000000000000000, 0.000000000000000000 ) ) ;
#156976 = FACE_OUTER_BOUND ( 'NONE', #152653, .T. ) ;
#156977 = ORIENTED_EDGE ( 'NONE', *, *, #206290, .F. ) ;
#156978 = CARTESIAN_POINT ( 'NONE',  ( -16.90257928357874562, 66.04589317890649625, -90.38682205441068618 ) ) ;
#156979 = ORIENTED_EDGE ( 'NONE', *, *, #32969, .T. ) ;
#156980 = ORIENTED_EDGE ( 'NONE', *, *, #178345, .F. ) ;
#156981 = TOROIDAL_SURFACE ( 'NONE', #44539, 0.4000000000000005773, 0.1000000000000000056 ) ;
#156982 = VECTOR ( 'NONE', #150335, 1000.000000000000114 ) ;
#156983 = DIRECTION ( 'NONE',  ( 1.000000000000000000, 0.000000000000000000, 0.000000000000000000 ) ) ;
#156984 = ORIENTED_EDGE ( 'NONE', *, *, #245641, .F. ) ;
#156985 = EDGE_LOOP ( 'NONE', ( #170553, #94764, #184470, #154395 ) ) ;
#156986 = DIRECTION ( 'NONE',  ( -1.000000000000000000, 0.000000000000000000, 0.000000000000000000 ) ) ;
#156987 = DIRECTION ( 'NONE',  ( 0.000000000000000000, -6.454785026890489601E-15, 1.000000000000000000 ) ) ;
#156988 = ORIENTED_EDGE ( 'NONE', *, *, #133924, .T. ) ;
#156989 = ORIENTED_EDGE ( 'NONE', *, *, #139728, .T. ) ;
#156990 = DIRECTION ( 'NONE',  ( 1.000000000000000000, -0.000000000000000000, -0.000000000000000000 ) ) ;
#156991 = CARTESIAN_POINT ( 'NONE',  ( 21.05000000000000071, 84.73084112150691283, -59.92503276553992464 ) ) ;
#156992 = EDGE_LOOP ( 'NONE', ( #193224, #16332, #227990, #246082 ) ) ;
#156993 = EDGE_CURVE ( 'NONE', #32434, #172249, #126984, .T. ) ;
#156994 = AXIS2_PLACEMENT_3D ( 'NONE', #210547, #48894, #110153 ) ;
#156995 = ORIENTED_EDGE ( 'NONE', *, *, #176150, .T. ) ;
#156996 = VERTEX_POINT ( 'NONE', #74118 ) ;
#156997 = DIRECTION ( 'NONE',  ( -1.000000000000000000, 0.000000000000000000, 0.000000000000000000 ) ) ;
#156998 = EDGE_CURVE ( 'NONE', #91045, #237782, #174528, .T. ) ;
#156999 = CARTESIAN_POINT ( 'NONE',  ( 18.49999999999999645, 76.00000000001195133, -103.0231074845243171 ) ) ;
#157000 = EDGE_CURVE ( 'NONE', #203988, #73682, #110639, .T. ) ;
#157001 = FACE_OUTER_BOUND ( 'NONE', #106608, .T. ) ;
#157002 = CARTESIAN_POINT ( 'NONE',  ( -18.50000000000000000, 77.73625713160926409, -91.45445515550680682 ) ) ;
#157003 = VECTOR ( 'NONE', #22880, 1000.000000000000000 ) ;
#157004 = CARTESIAN_POINT ( 'NONE',  ( -21.14999999999999858, 64.25000000001165290, -69.52310748452438816 ) ) ;
#157005 = CARTESIAN_POINT ( 'NONE',  ( 18.59999999999999076, 66.40155400966892785, -213.5088390336144073 ) ) ;
#157006 = TOROIDAL_SURFACE ( 'NONE', #256891, 4.149999999999999467, 0.1000000000000000056 ) ;
#157007 = CARTESIAN_POINT ( 'NONE',  ( -23.15000000000000213, 85.60000000001262777, -193.6291383618718385 ) ) ;
#157009 = CARTESIAN_POINT ( 'NONE',  ( -21.14999999999999858, 6.257814610487270279, -167.4022097086911742 ) ) ;
#157008 = CARTESIAN_POINT ( 'NONE',  ( -16.86379686415369861, 9.975217759253158789, -12.56661011090972124 ) ) ;
#157011 = VECTOR ( 'NONE', #57600, 1000.000000000000000 ) ;
#157010 = DIRECTION ( 'NONE',  ( 0.000000000000000000, 0.000000000000000000, -1.000000000000000000 ) ) ;
#157012 = CIRCLE ( 'NONE', #177857, 0.5999999999999894307 ) ;
#157013 = CARTESIAN_POINT ( 'NONE',  ( 18.39999999999999503, 11.74999999999998224, -12.65000000000000213 ) ) ;
#157014 = ADVANCED_FACE ( 'NONE', ( #253989 ), #206278, .T. ) ;
#157015 = DIRECTION ( 'NONE',  ( 1.000000000000000000, 0.000000000000000000, 0.000000000000000000 ) ) ;
#157016 = CARTESIAN_POINT ( 'NONE',  ( 21.06600267594171783, 44.20901405692286090, -236.5533276467423320 ) ) ;
#157018 = ORIENTED_EDGE ( 'NONE', *, *, #27936, .F. ) ;
#157017 = CIRCLE ( 'NONE', #44581, 0.1000000000000045852 ) ;
#157020 = EDGE_LOOP ( 'NONE', ( #115656, #83039, #21783, #91711, #215006 ) ) ;
#157019 = CARTESIAN_POINT ( 'NONE',  ( -21.45000000000000284, 52.80902093404626640, -233.8693558107618173 ) ) ;
#157021 = ADVANCED_FACE ( 'NONE', ( #130188 ), #255228, .F. ) ;
#157022 = DIRECTION ( 'NONE',  ( 0.000000000000000000, -0.000000000000000000, 1.000000000000000000 ) ) ;
#157023 = AXIS2_PLACEMENT_3D ( 'NONE', #151235, #46964, #87376 ) ;
#157024 = DIRECTION ( 'NONE',  ( 0.000000000000000000, -0.1298341882520022694, -0.9915357197604852679 ) ) ;
#157025 = ORIENTED_EDGE ( 'NONE', *, *, #209243, .F. ) ;
#157026 = CARTESIAN_POINT ( 'NONE',  ( 20.94983749550516450, 10.29766095125288494, -206.4743663933275286 ) ) ;
#157027 = ADVANCED_BREP_SHAPE_REPRESENTATION ( '', ( #21402, #2425 ), #222606 ) ;
#157028 = CARTESIAN_POINT ( 'NONE',  ( -16.87331047859649757, 9.949999999999983302, -20.85000000000000142 ) ) ;
#157029 = ORIENTED_EDGE ( 'NONE', *, *, #50517, .F. ) ;
#157030 = AXIS2_PLACEMENT_3D ( 'NONE', #65744, #106132, #67032 ) ;
#157031 = DIRECTION ( 'NONE',  ( -1.000000000000000000, 0.000000000000000000, -0.000000000000000000 ) ) ;
#157032 = CYLINDRICAL_SURFACE ( 'NONE', #242114, 4.049999999999994493 ) ;
#157033 = FACE_OUTER_BOUND ( 'NONE', #123561, .T. ) ;
#157035 = ORIENTED_EDGE ( 'NONE', *, *, #173549, .T. ) ;
#157034 = DIRECTION ( 'NONE',  ( 0.000000000000000000, 0.000000000000000000, 1.000000000000000000 ) ) ;
#157037 = EDGE_LOOP ( 'NONE', ( #42206, #51343, #231742, #12866 ) ) ;
#157036 = DIRECTION ( 'NONE',  ( 0.000000000000000000, 0.9651348961777379554, -0.2617529984164210233 ) ) ;
#157038 = DIRECTION ( 'NONE',  ( 0.000000000000000000, -1.000000000000000000, 0.000000000000000000 ) ) ;
#157039 = CARTESIAN_POINT ( 'NONE',  ( 23.14999999999998437, 1.115600667400684642E-11, -100.5000000000000284 ) ) ;
#157040 = DIRECTION ( 'NONE',  ( 1.000000000000000000, 0.000000000000000000, 0.000000000000000000 ) ) ;
#157041 = DIRECTION ( 'NONE',  ( 7.304098846218134667E-16, 1.000000000000000000, 6.982962677686267499E-15 ) ) ;
#157043 = DIRECTION ( 'NONE',  ( 1.000000000000000000, 0.000000000000000000, 0.000000000000000000 ) ) ;
#157042 = CARTESIAN_POINT ( 'NONE',  ( -16.77180007708461318, 9.950000000011137047, -154.8643858810451945 ) ) ;
#157044 = CARTESIAN_POINT ( 'NONE',  ( -20.54999999999999716, 9.350000000000001421, -21.15000000000000213 ) ) ;
#157045 = CARTESIAN_POINT ( 'NONE',  ( 22.50497660315937054, -0.07871793021434786430, -155.7502044951045548 ) ) ;
#157046 = DIRECTION ( 'NONE',  ( 1.000000000000000000, 0.000000000000000000, 0.000000000000000000 ) ) ;
#157047 = CARTESIAN_POINT ( 'NONE',  ( -18.41817142474042157, 85.49870306661448183, -163.4191419968870491 ) ) ;
#157048 = VECTOR ( 'NONE', #132055, 999.9999999999998863 ) ;
#157049 = AXIS2_PLACEMENT_3D ( 'NONE', #212870, #36831, #94183 ) ;
#157050 = CARTESIAN_POINT ( 'NONE',  ( 21.14999999999999858, 87.75000000001156764, -57.27310748452423894 ) ) ;
#157051 = TOROIDAL_SURFACE ( 'NONE', #215292, 11.70000000000000462, 0.1000000000000000056 ) ;
#157052 = AXIS2_PLACEMENT_3D ( 'NONE', #204833, #226982, #90026 ) ;
#157053 = EDGE_LOOP ( 'NONE', ( #178982, #115431, #12308, #68432, #229456 ) ) ;
#157054 = EDGE_CURVE ( 'NONE', #237894, #69570, #251436, .T. ) ;
#157055 = CARTESIAN_POINT ( 'NONE',  ( 21.05000000000000071, 18.81732247075047937, -230.0377732242114632 ) ) ;
#157056 = ORIENTED_EDGE ( 'NONE', *, *, #137020, .T. ) ;
#157057 = VERTEX_POINT ( 'NONE', #209749 ) ;
#157058 = DIRECTION ( 'NONE',  ( 0.000000000000000000, 0.000000000000000000, 1.000000000000000000 ) ) ;
#157059 = DIRECTION ( 'NONE',  ( 0.000000000000000000, 0.000000000000000000, -1.000000000000000000 ) ) ;
#157060 = VERTEX_POINT ( 'NONE', #153681 ) ;
#157061 = EDGE_CURVE ( 'NONE', #241247, #153611, #131253, .T. ) ;
#157062 = ORIENTED_EDGE ( 'NONE', *, *, #118609, .F. ) ;
#157063 = EDGE_CURVE ( 'NONE', #178909, #135829, #43770, .T. ) ;
#157064 = EDGE_CURVE ( 'NONE', #126775, #223761, #93844, .T. ) ;
#157065 = CIRCLE ( 'NONE', #177911, 0.09999999999999939493 ) ;
#157066 = CIRCLE ( 'NONE', #211225, 0.09999999999999939493 ) ;
#157067 = VERTEX_POINT ( 'NONE', #252703 ) ;
#157068 = ORIENTED_EDGE ( 'NONE', *, *, #30199, .F. ) ;
#157069 = CARTESIAN_POINT ( 'NONE',  ( -21.07928932188134041, 6.328516656404449492, -133.9011048543456184 ) ) ;
#157070 = DIRECTION ( 'NONE',  ( 0.000000000000000000, 0.000000000000000000, -1.000000000000000000 ) ) ;
#157071 = VECTOR ( 'NONE', #253706, 1000.000000000000000 ) ;
#157072 = FACE_OUTER_BOUND ( 'NONE', #37142, .T. ) ;
#157073 = FACE_OUTER_BOUND ( 'NONE', #173228, .T. ) ;
#157074 = FACE_OUTER_BOUND ( 'NONE', #97954, .T. ) ;
#157075 = EDGE_CURVE ( 'NONE', #237838, #38064, #88185, .T. ) ;
#157076 = CARTESIAN_POINT ( 'NONE',  ( 21.05000000000000071, -0.09999999998884338825, -21.85042919245520210 ) ) ;
#157077 = SPHERICAL_SURFACE ( 'NONE', #165994, 0.1000000000000000056 ) ;
#157079 = EDGE_LOOP ( 'NONE', ( #227676, #163619, #182094, #147804 ) ) ;
#157078 = CARTESIAN_POINT ( 'NONE',  ( -21.65000000000000213, 68.75000000001256240, -182.6731074845244223 ) ) ;
#157081 = CARTESIAN_POINT ( 'NONE',  ( -21.53551880898958260, 65.35981425085753926, -242.3774659647530996 ) ) ;
#157080 = DIRECTION ( 'NONE',  ( 0.7071067811865493491, 0.7071067811865456854, 0.000000000000000000 ) ) ;
#157082 = ADVANCED_FACE ( 'NONE', ( #213583 ), #2236, .F. ) ;
#157083 = DIRECTION ( 'NONE',  ( 1.301042606982683734E-14, 0.8660254037844367092, -0.5000000000000037748 ) ) ;
#157084 = ORIENTED_EDGE ( 'NONE', *, *, #160448, .T. ) ;
#157085 = LINE ( 'NONE', #1825, #185585 ) ;
#157087 = EDGE_CURVE ( 'NONE', #23181, #34352, #19237, .T. ) ;
#157086 = CARTESIAN_POINT ( 'NONE',  ( 22.10000000000000142, -11.65000000000000036, 12.09999999999999787 ) ) ;
#157088 = B_SPLINE_CURVE_WITH_KNOTS ( 'NONE', 3,
 ( #35203, #216358, #212536, #37753, #117273, #211232, #156431, #73045, #170880, #175982, #91293, #250361, #151275 ),
 .UNSPECIFIED., .F., .F.,
 ( 4, 3, 3, 3, 4 ),
 ( 1.077764583621373145E-16, 1.946463881814408957E-05, 3.922356109942842209E-05, 4.215060953236330466E-05, 4.415117091090545512E-05 ),
 .UNSPECIFIED. ) ;
#157089 = ORIENTED_EDGE ( 'NONE', *, *, #233851, .F. ) ;
#157091 = DIRECTION ( 'NONE',  ( 0.000000000000000000, -1.000000000000000000, 0.000000000000000000 ) ) ;
#157090 = CARTESIAN_POINT ( 'NONE',  ( 20.94999999999999574, -1.835341550213255957, -112.0551512925630107 ) ) ;
#157092 = VECTOR ( 'NONE', #125575, 1000.000000000000000 ) ;
#157093 = CARTESIAN_POINT ( 'NONE',  ( -23.25000000000000000, 76.00000000001213607, -136.5231074845242745 ) ) ;
#157094 = CARTESIAN_POINT ( 'NONE',  ( 22.49533356619859958, 64.34999999370755575, -69.58823006484711016 ) ) ;
#157095 = ORIENTED_EDGE ( 'NONE', *, *, #1673, .T. ) ;
#157096 = VERTEX_POINT ( 'NONE', #218703 ) ;
#157097 = EDGE_CURVE ( 'NONE', #85287, #178254, #48051, .T. ) ;
#157098 = CARTESIAN_POINT ( 'NONE',  ( -18.39999999999999858, -7.667348966301519297, -236.4704904124130280 ) ) ;
#157099 = EDGE_CURVE ( 'NONE', #13417, #52066, #216145, .T. ) ;
#157100 = CARTESIAN_POINT ( 'NONE',  ( -22.50485643085240284, -0.07878633906603056680, -55.25020506082763916 ) ) ;
#157101 = CARTESIAN_POINT ( 'NONE',  ( 20.94999999999999574, 74.16465844978787914, -158.3679561919613832 ) ) ;
#157103 = ADVANCED_FACE ( 'NONE', ( #200449 ), #2224, .F. ) ;
#157102 = DIRECTION ( 'NONE',  ( -1.000000000000000000, 0.000000000000000000, 0.000000000000000000 ) ) ;
#157104 = ORIENTED_EDGE ( 'NONE', *, *, #9622, .T. ) ;
#157105 = EDGE_CURVE ( 'NONE', #54263, #24859, #197882, .T. ) ;
#157106 = VECTOR ( 'NONE', #106400, 1000.000000000000000 ) ;
#157107 = FACE_OUTER_BOUND ( 'NONE', #161935, .T. ) ;
#157108 = AXIS2_PLACEMENT_3D ( 'NONE', #599, #159710, #18899 ) ;
#157109 = DIRECTION ( 'NONE',  ( 0.000000000000000000, 0.7397360091702777085, -0.6728971962616808744 ) ) ;
#157110 = DIRECTION ( 'NONE',  ( 0.000000000000000000, 1.000000000000000000, 0.000000000000000000 ) ) ;
#157111 = AXIS2_PLACEMENT_3D ( 'NONE', #230313, #186065, #209472 ) ;
#157113 = CARTESIAN_POINT ( 'NONE',  ( 20.94999999999999929, 76.00000000001243450, -168.0231074845243597 ) ) ;
#157112 = VECTOR ( 'NONE', #20724, 1000.000000000000000 ) ;
#157114 = FACE_OUTER_BOUND ( 'NONE', #235219, .T. ) ;
#157115 = PRODUCT_DEFINITION_FORMATION_WITH_SPECIFIED_SOURCE ( 'ANY', '', #122620, .NOT_KNOWN. ) ;
#157117 = ORIENTED_EDGE ( 'NONE', *, *, #119452, .F. ) ;
#157116 = FACE_OUTER_BOUND ( 'NONE', #56979, .T. ) ;
#157118 = CYLINDRICAL_SURFACE ( 'NONE', #22669, 0.09999999999999149847 ) ;
#157119 = CIRCLE ( 'NONE', #190453, 4.050000000000001599 ) ;
#157121 = EDGE_CURVE ( 'NONE', #223778, #57698, #257795, .T. ) ;
#157120 = DIRECTION ( 'NONE',  ( 1.000000000000000000, 0.000000000000000000, 0.000000000000000000 ) ) ;
#157122 = CARTESIAN_POINT ( 'NONE',  ( 20.00000000000000355, 5.645774302107834153, 15.47947886955507890 ) ) ;
#157123 = DIRECTION ( 'NONE',  ( 0.000000000000000000, 0.000000000000000000, -1.000000000000000000 ) ) ;
#157124 = EDGE_CURVE ( 'NONE', #123360, #1569, #256501, .T. ) ;
#157125 = AXIS2_PLACEMENT_3D ( 'NONE', #4696, #65977, #84191 ) ;
#157126 = CARTESIAN_POINT ( 'NONE',  ( 20.95595012432474746, 10.60417921308754607, -175.0957693302182463 ) ) ;
#157128 = ORIENTED_EDGE ( 'NONE', *, *, #131792, .T. ) ;
#157127 = CARTESIAN_POINT ( 'NONE',  ( 18.59999999999999432, 77.16270174995034381, -161.9231074845243370 ) ) ;
#157129 = DIRECTION ( 'NONE',  ( 0.000000000000000000, 0.000000000000000000, 1.000000000000000000 ) ) ;
#157130 = CARTESIAN_POINT ( 'NONE',  ( -20.85000000000000142, 77.73670573947921980, -58.00568489690056850 ) ) ;
#157131 = CYLINDRICAL_SURFACE ( 'NONE', #3303, 0.1000000000000028644 ) ;
#157132 = ORIENTED_EDGE ( 'NONE', *, *, #234694, .F. ) ;
#157133 = CARTESIAN_POINT ( 'NONE',  ( -18.59999999999999787, 77.85161776048127535, -158.4199177649206831 ) ) ;
#157134 = LINE ( 'NONE', #142660, #77588 ) ;
#157135 = DIRECTION ( 'NONE',  ( 0.000000000000000000, 0.000000000000000000, 1.000000000000000000 ) ) ;
#157136 = LINE ( 'NONE', #57990, #216788 ) ;
#157137 = ADVANCED_FACE ( 'NONE', ( #220003 ), #133172, .T. ) ;
#157138 = DIRECTION ( 'NONE',  ( -1.000000000000000000, 0.000000000000000000, -0.000000000000000000 ) ) ;
#157139 = TOROIDAL_SURFACE ( 'NONE', #61259, 0.2000000000000000111, 0.1000000000000000056 ) ;
#157140 = FACE_OUTER_BOUND ( 'NONE', #61064, .T. ) ;
#157141 = AXIS2_PLACEMENT_3D ( 'NONE', #183251, #244496, #121990 ) ;
#157142 = EDGE_LOOP ( 'NONE', ( #127620, #17649, #144114, #923 ) ) ;
#157143 = EDGE_LOOP ( 'NONE', ( #33812, #19999, #45592, #146132 ) ) ;
#157144 = CIRCLE ( 'NONE', #190469, 4.000000000000000000 ) ;
#157145 = CARTESIAN_POINT ( 'NONE',  ( 22.39999999999999503, -0.1008583690875579364, -155.7504328765105868 ) ) ;
#157146 = DIRECTION ( 'NONE',  ( -1.000000000000000000, -0.000000000000000000, -0.000000000000000000 ) ) ;
#157147 = AXIS2_PLACEMENT_3D ( 'NONE', #21250, #202418, #138558 ) ;
#157148 = CARTESIAN_POINT ( 'NONE',  ( 18.79999999999999716, 6.644425182197215562, 9.641788261573355001 ) ) ;
#157149 = DIRECTION ( 'NONE',  ( 0.000000000000000000, -6.982962677686266711E-15, 1.000000000000000000 ) ) ;
#157150 = ORIENTED_EDGE ( 'NONE', *, *, #151790, .T. ) ;
#157151 = AXIS2_PLACEMENT_3D ( 'NONE', #58425, #192846, #18039 ) ;
#157152 = DIRECTION ( 'NONE',  ( 2.342056488767301376E-15, -0.1350103645451904977, -0.9908441862701596881 ) ) ;
#157153 = EDGE_CURVE ( 'NONE', #47571, #89242, #100029, .T. ) ;
#157154 = CARTESIAN_POINT ( 'NONE',  ( 20.19326291202132495, 11.57517403174952619, -206.4228608358838244 ) ) ;
#157155 = B_SPLINE_CURVE_WITH_KNOTS ( 'NONE', 3,
 ( #162860, #44187, #24642, #239820, #182416, #83266, #139398, #104122, #181134, #179850 ),
 .UNSPECIFIED., .F., .F.,
 ( 4, 3, 3, 4 ),
 ( 1.894194122894209342E-15, 3.877043166999724264E-05, 7.336897548476889550E-05, 7.659383120240112811E-05 ),
 .UNSPECIFIED. ) ;
#157156 = CARTESIAN_POINT ( 'NONE',  ( -20.54999999999999716, 1.115600667400684642E-11, -134.0000000000000284 ) ) ;
#157157 = EDGE_CURVE ( 'NONE', #257588, #230269, #239579, .T. ) ;
#157158 = VECTOR ( 'NONE', #182685, 1000.000000000000000 ) ;
#157159 = TOROIDAL_SURFACE ( 'NONE', #7287, 12.77500000000000036, 0.1000000000000000056 ) ;
#157160 = VECTOR ( 'NONE', #81981, 1000.000000000000000 ) ;
#157161 = ORIENTED_EDGE ( 'NONE', *, *, #54710, .T. ) ;
#157162 = DIRECTION ( 'NONE',  ( -0.7071067811865456854, -0.7071067811865493491, -4.937700262164544098E-15 ) ) ;
#157163 = EDGE_CURVE ( 'NONE', #143179, #94985, #127162, .T. ) ;
#157164 = EDGE_LOOP ( 'NONE', ( #88646, #240006, #85276 ) ) ;
#157165 = B_SPLINE_CURVE_WITH_KNOTS ( 'NONE', 3,
 ( #157922, #34113, #117470, #138281, #35394, #39234, #217819, #58738, #37946, #53637, #152769, #74530, #114895 ),
 .UNSPECIFIED., .F., .F.,
 ( 4, 3, 3, 3, 4 ),
 ( -3.224855718277970714E-06, 0.000000000000000000, 6.199515528665968749E-06, 4.034952380127321888E-05, 7.452715123699268278E-05 ),
 .UNSPECIFIED. ) ;
#157166 = ADVANCED_FACE ( 'NONE', ( #60919 ), #41394, .T. ) ;
#157167 = ORIENTED_EDGE ( 'NONE', *, *, #35057, .T. ) ;
#157168 = DIRECTION ( 'NONE',  ( 1.000000000000000000, 3.265361837132813093E-16, -0.000000000000000000 ) ) ;
#157169 = CARTESIAN_POINT ( 'NONE',  ( -18.59999999999999787, 13.66123737402873495, -238.6633470470287648 ) ) ;
#157170 = DIRECTION ( 'NONE',  ( 0.000000000000000000, -6.982962677686266711E-15, 1.000000000000000000 ) ) ;
#157171 = ORIENTED_EDGE ( 'NONE', *, *, #51860, .F. ) ;
#157172 = SPHERICAL_SURFACE ( 'NONE', #36609, 0.1000000000000000056 ) ;
#157174 = EDGE_CURVE ( 'NONE', #31427, #195402, #31350, .T. ) ;
#157173 = CARTESIAN_POINT ( 'NONE',  ( -15.75000000000000355, 13.18880795147152440, -215.2702608532411830 ) ) ;
#157175 = DIRECTION ( 'NONE',  ( 0.000000000000000000, 0.000000000000000000, 1.000000000000000000 ) ) ;
#157176 = ORIENTED_EDGE ( 'NONE', *, *, #161557, .T. ) ;
#157177 = LINE ( 'NONE', #153342, #183171 ) ;
#157178 = AXIS2_PLACEMENT_3D ( 'NONE', #160581, #240096, #220535 ) ;
#157180 = ORIENTED_EDGE ( 'NONE', *, *, #36304, .T. ) ;
#157179 = DIRECTION ( 'NONE',  ( 0.000000000000000000, 4.336808689941893885E-15, 1.000000000000000000 ) ) ;
#157181 = DIRECTION ( 'NONE',  ( -1.000000000000000000, -0.000000000000000000, -0.000000000000000000 ) ) ;
#157182 = AXIS2_PLACEMENT_3D ( 'NONE', #66586, #32625, #10462 ) ;
#157183 = CYLINDRICAL_SURFACE ( 'NONE', #85527, 0.1000000000000101225 ) ;
#157184 = ADVANCED_FACE ( 'NONE', ( #146862 ), #166483, .T. ) ;
#157185 = EDGE_CURVE ( 'NONE', #235804, #190202, #25664, .T. ) ;
#157186 = ORIENTED_EDGE ( 'NONE', *, *, #229832, .T. ) ;
#157187 = VECTOR ( 'NONE', #62057, 1000.000000000000000 ) ;
#157188 = DIRECTION ( 'NONE',  ( 0.000000000000000000, -1.000000000000000000, -6.982962677686266711E-15 ) ) ;
#157189 = CARTESIAN_POINT ( 'NONE',  ( -23.25000000000000000, 4.959819536546777642E-16, 4.049999999999998934 ) ) ;
#157190 = PLANE ( 'NONE',  #105934 ) ;
#157191 = ORIENTED_EDGE ( 'NONE', *, *, #18065, .F. ) ;
#157192 = DIRECTION ( 'NONE',  ( 0.000000000000000000, -6.982962677686266711E-15, 1.000000000000000000 ) ) ;
#157193 = EDGE_CURVE ( 'NONE', #29646, #199802, #202000, .T. ) ;
#157194 = CARTESIAN_POINT ( 'NONE',  ( 15.57250062127603663, 48.82262352862032628, -233.8339354177745690 ) ) ;
#157195 = DIRECTION ( 'NONE',  ( 0.000000000000000000, -1.000000000000000000, 0.000000000000000000 ) ) ;
#157196 = AXIS2_PLACEMENT_3D ( 'NONE', #61681, #60384, #62962 ) ;
#157197 = VECTOR ( 'NONE', #35449, 1000.000000000000000 ) ;
#157198 = ORIENTED_EDGE ( 'NONE', *, *, #55192, .T. ) ;
#157199 = AXIS2_PLACEMENT_3D ( 'NONE', #233412, #213822, #215106 ) ;
#157200 = VECTOR ( 'NONE', #17840, 1000.000000000000000 ) ;
#157201 = EDGE_LOOP ( 'NONE', ( #146060, #235185, #29097, #13022 ) ) ;
#157202 = ADVANCED_FACE ( 'NONE', ( #187315 ), #14775, .T. ) ;
#157203 = AXIS2_PLACEMENT_3D ( 'NONE', #57211, #100183, #196739 ) ;
#157204 = ADVANCED_FACE ( 'NONE', ( #184717 ), #127327, .T. ) ;
#157205 = EDGE_LOOP ( 'NONE', ( #102053, #71349, #95503, #142916, #133948 ) ) ;
#157206 = CARTESIAN_POINT ( 'NONE',  ( -22.94999999999999929, 3.461118860469513336, 28.84309995045515507 ) ) ;
#157207 = CARTESIAN_POINT ( 'NONE',  ( 21.09546886439553504, 8.878553113026073973, -45.73709385055541077 ) ) ;
#157209 = ORIENTED_EDGE ( 'NONE', *, *, #31425, .F. ) ;
#157208 = CARTESIAN_POINT ( 'NONE',  ( 20.94999999999999574, -11.48912529306490349, -70.10000000000005116 ) ) ;
#157210 = EDGE_CURVE ( 'NONE', #177788, #97714, #77087, .T. ) ;
#157211 = PLANE ( 'NONE',  #103278 ) ;
#157212 = DIRECTION ( 'NONE',  ( 0.000000000000000000, -0.5907332058517320572, 0.8068669527896995541 ) ) ;
#157213 = FACE_OUTER_BOUND ( 'NONE', #212295, .T. ) ;
#157214 = CARTESIAN_POINT ( 'NONE',  ( -18.37160782347004329, 11.47561641481354044, -76.25000000000004263 ) ) ;
#157215 = EDGE_CURVE ( 'NONE', #176760, #101907, #207729, .T. ) ;
#157216 = DIRECTION ( 'NONE',  ( 0.000000000000000000, 1.000000000000000000, -6.308085367188393199E-16 ) ) ;
#157217 = VECTOR ( 'NONE', #157489, 1000.000000000000000 ) ;
#157218 = CARTESIAN_POINT ( 'NONE',  ( 18.59999999999999076, 6.450000000000001066, -21.25000000000000000 ) ) ;
#157220 = ORIENTED_EDGE ( 'NONE', *, *, #76943, .T. ) ;
#157219 = CARTESIAN_POINT ( 'NONE',  ( 21.05000000000000071, 76.00000000001168132, -65.42310748452432279 ) ) ;
#157222 = ORIENTED_EDGE ( 'NONE', *, *, #93247, .F. ) ;
#157221 = DIRECTION ( 'NONE',  ( 0.000000000000000000, 0.000000000000000000, -1.000000000000000000 ) ) ;
#157224 = CARTESIAN_POINT ( 'NONE',  ( 23.14999999999998437, -4.049999999988842525, -67.00000000000004263 ) ) ;
#157223 = DIRECTION ( 'NONE',  ( -1.000000000000000000, -0.000000000000000000, 0.000000000000000000 ) ) ;
#157225 = ORIENTED_EDGE ( 'NONE', *, *, #106496, .T. ) ;
#157226 = VERTEX_POINT ( 'NONE', #244687 ) ;
#157227 = CARTESIAN_POINT ( 'NONE',  ( -18.59117750673696889, 10.33248238083634796, -106.0948465439131922 ) ) ;
#157228 = FACE_OUTER_BOUND ( 'NONE', #226271, .T. ) ;
#157229 = AXIS2_PLACEMENT_3D ( 'NONE', #2883, #137267, #236374 ) ;
#157231 = B_SPLINE_CURVE_WITH_KNOTS ( 'NONE', 3,
 ( #118146, #39923, #97253, #176856, #54305, #93432, #135119, #19041, #178143, #257591 ),
 .UNSPECIFIED., .F., .F.,
 ( 4, 3, 3, 4 ),
 ( 0.000000000000000000, 3.394313611809514494E-05, 6.779740500699831776E-05, 0.0001049857339142602552 ),
 .UNSPECIFIED. ) ;
#157230 = DIRECTION ( 'NONE',  ( 1.000000000000000000, -0.000000000000000000, -0.000000000000000000 ) ) ;
#157232 = PLANE ( 'NONE',  #127738 ) ;
#157233 = EDGE_CURVE ( 'NONE', #225538, #185736, #68723, .T. ) ;
#157234 = CARTESIAN_POINT ( 'NONE',  ( -22.10000000000000497, 6.322468214605804882, 12.11686199900910310 ) ) ;
#157235 = DIRECTION ( 'NONE',  ( 0.000000000000000000, 0.000000000000000000, -1.000000000000000000 ) ) ;
#157236 = DIRECTION ( 'NONE',  ( -1.000000000000000000, -0.000000000000000000, 0.000000000000000000 ) ) ;
#157237 = VERTEX_POINT ( 'NONE', #247254 ) ;
#157238 = VERTEX_POINT ( 'NONE', #66060 ) ;
#157239 = CARTESIAN_POINT ( 'NONE',  ( 18.79999999999999716, -1.885425182446133885, -11.49641995933507843 ) ) ;
#157240 = CONICAL_SURFACE ( 'NONE', #28065, 6.250000000000000000, 0.7853981633974431720 ) ;
#157241 = AXIS2_PLACEMENT_3D ( 'NONE', #153597, #253912, #15340 ) ;
#157242 = ORIENTED_EDGE ( 'NONE', *, *, #134636, .T. ) ;
#157244 = DIRECTION ( 'NONE',  ( -3.265361837132813093E-16, -0.9651348961777146407, 0.2617529984165072321 ) ) ;
#157243 = AXIS2_PLACEMENT_3D ( 'NONE', #48028, #108016, #68903 ) ;
#157245 = CARTESIAN_POINT ( 'NONE',  ( -17.01764560440449614, 51.52760218624815991, -231.9873527054617455 ) ) ;
#157246 = DIRECTION ( 'NONE',  ( 0.000000000000000000, 0.000000000000000000, 1.000000000000000000 ) ) ;
#157247 = CARTESIAN_POINT ( 'NONE',  ( 23.24999999999999645, 11.75000000001113953, -109.7500000000000426 ) ) ;
#157248 = ORIENTED_EDGE ( 'NONE', *, *, #167770, .F. ) ;
#157249 = EDGE_CURVE ( 'NONE', #222258, #128354, #26972, .T. ) ;
#157250 = CARTESIAN_POINT ( 'NONE',  ( -15.51798037960204546, 66.62334006147850118, -118.8949149363070887 ) ) ;
#157251 = EDGE_LOOP ( 'NONE', ( #31615, #239706, #23564, #255593 ) ) ;
#157252 = DIRECTION ( 'NONE',  ( 0.000000000000000000, -7.086529944415886769E-15, 1.000000000000000000 ) ) ;
#157253 = EDGE_LOOP ( 'NONE', ( #112136, #25624, #93120, #86633 ) ) ;
#157254 = CARTESIAN_POINT ( 'NONE',  ( -18.69999999999999929, -8.250000000000005329, 31.39999999999999858 ) ) ;
#157255 = DIRECTION ( 'NONE',  ( 1.000000000000000000, 0.000000000000000000, 0.000000000000000000 ) ) ;
#157256 = CARTESIAN_POINT ( 'NONE',  ( -16.86337532320262156, 9.979967204235514089, -113.0510755310172328 ) ) ;
#157257 = AXIS2_PLACEMENT_3D ( 'NONE', #43045, #47, #196958 ) ;
#157258 = VERTEX_POINT ( 'NONE', #144286 ) ;
#157260 = DIRECTION ( 'NONE',  ( 0.000000000000000000, 0.000000000000000000, -1.000000000000000000 ) ) ;
#157259 = AXIS2_PLACEMENT_3D ( 'NONE', #72823, #32416, #93637 ) ;
#157262 = EDGE_LOOP ( 'NONE', ( #405, #86196, #125550 ) ) ;
#157261 = DIRECTION ( 'NONE',  ( 1.000000000000000000, 2.952720810173289112E-16, -0.000000000000000000 ) ) ;
#157263 = EDGE_CURVE ( 'NONE', #50799, #149928, #68644, .T. ) ;
#157264 = DIRECTION ( 'NONE',  ( 0.000000000000000000, 0.000000000000000000, -1.000000000000000000 ) ) ;
#157265 = ORIENTED_EDGE ( 'NONE', *, *, #137954, .T. ) ;
#157266 = CIRCLE ( 'NONE', #15630, 11.74999999999999645 ) ;
#157267 = CARTESIAN_POINT ( 'NONE',  ( 23.14999999999999503, 11.75000000001116263, -179.6499999999999773 ) ) ;
#157268 = ORIENTED_EDGE ( 'NONE', *, *, #164199, .F. ) ;
#157269 = CARTESIAN_POINT ( 'NONE',  ( -21.05000000000000071, 11.65000000001115232, -67.10000000000005116 ) ) ;
#157270 = CARTESIAN_POINT ( 'NONE',  ( 21.11833042828127915, 69.55435530615625339, -69.53020799358364457 ) ) ;
#157271 = DIRECTION ( 'NONE',  ( 0.000000000000000000, 0.000000000000000000, -1.000000000000000000 ) ) ;
#157272 = DIRECTION ( 'NONE',  ( 0.000000000000000000, -0.1455152366551522025, -0.9893560106964505163 ) ) ;
#157273 = CARTESIAN_POINT ( 'NONE',  ( -18.59999999999999787, 1.115600667400684642E-11, -100.5000000000000284 ) ) ;
#157274 = ORIENTED_EDGE ( 'NONE', *, *, #113492, .F. ) ;
#157275 = FACE_OUTER_BOUND ( 'NONE', #79468, .T. ) ;
#157276 = CARTESIAN_POINT ( 'NONE',  ( 21.04999999999999716, 6.300183336278410984, -100.4486725676586474 ) ) ;
#157277 = CARTESIAN_POINT ( 'NONE',  ( 18.56579813702274961, 10.33025634372637747, -139.5870929282639281 ) ) ;
#157278 = AXIS2_PLACEMENT_3D ( 'NONE', #28799, #33938, #208691 ) ;
#157279 = VERTEX_POINT ( 'NONE', #45217 ) ;
#157280 = DIRECTION ( 'NONE',  ( 0.000000000000000000, 0.9126074666063545004, 0.4088369013363783999 ) ) ;
#157281 = EDGE_LOOP ( 'NONE', ( #18013, #113086, #64495, #66727 ) ) ;
#157282 = CARTESIAN_POINT ( 'NONE',  ( -22.39999999999999858, 76.00000000001237765, -170.0231074845243597 ) ) ;
#157283 = VECTOR ( 'NONE', #219769, 1000.000000000000000 ) ;
#157284 = ORIENTED_EDGE ( 'NONE', *, *, #76450, .F. ) ;
#157285 = DIRECTION ( 'NONE',  ( -0.000000000000000000, 0.1298341882519735979, 0.9915357197604890427 ) ) ;
#157286 = FACE_OUTER_BOUND ( 'NONE', #43185, .T. ) ;
#157288 = ORIENTED_EDGE ( 'NONE', *, *, #78791, .T. ) ;
#157287 = FACE_OUTER_BOUND ( 'NONE', #162276, .T. ) ;
#157289 = CARTESIAN_POINT ( 'NONE',  ( -18.42609945526393034, 8.812905974021688849, -245.4119551042256546 ) ) ;
#157290 = VERTEX_POINT ( 'NONE', #225116 ) ;
#157291 = AXIS2_PLACEMENT_3D ( 'NONE', #32055, #91990, #34615 ) ;
#157292 = CARTESIAN_POINT ( 'NONE',  ( -21.07928932188134041, 76.00000000001267608, -203.5231074845243597 ) ) ;
#157293 = EDGE_CURVE ( 'NONE', #126736, #33512, #7370, .T. ) ;
#157294 = CARTESIAN_POINT ( 'NONE',  ( 23.04999999999999716, 8.822561741677553471, -143.2500000000000284 ) ) ;
#157295 = ORIENTED_EDGE ( 'NONE', *, *, #187082, .T. ) ;
#157296 = CIRCLE ( 'NONE', #128056, 0.1000000000000002554 ) ;
#157297 = ORIENTED_EDGE ( 'NONE', *, *, #67249, .F. ) ;
#157298 = CARTESIAN_POINT ( 'NONE',  ( 23.14999999999998437, 1.115600667400684642E-11, -104.5500000000000256 ) ) ;
#157299 = CARTESIAN_POINT ( 'NONE',  ( -20.99780126800952829, 11.60538868788763089, -194.0873525717049972 ) ) ;
#157300 = EDGE_LOOP ( 'NONE', ( #113712, #39716, #170462, #250551 ) ) ;
#157301 = CARTESIAN_POINT ( 'NONE',  ( 20.94999999999999929, 36.65892442174935439, -249.5511627012433848 ) ) ;
#157302 = AXIS2_PLACEMENT_3D ( 'NONE', #58077, #197602, #171671 ) ;
#157303 = AXIS2_PLACEMENT_3D ( 'NONE', #115323, #55321, #216979 ) ;
#157305 = EDGE_LOOP ( 'NONE', ( #4384, #253298, #57707, #225919 ) ) ;
#157304 = VECTOR ( 'NONE', #197579, 1000.000000000000000 ) ;
#157306 = ORIENTED_EDGE ( 'NONE', *, *, #96733, .T. ) ;
#157307 = DIRECTION ( 'NONE',  ( -0.000000000000000000, 7.272083257015735086E-15, -1.000000000000000000 ) ) ;
#157309 = DIRECTION ( 'NONE',  ( 0.000000000000000000, -0.2128009952263664739, 0.9770955615653302839 ) ) ;
#157308 = VECTOR ( 'NONE', #133576, 1000.000000000000000 ) ;
#157310 = EDGE_CURVE ( 'NONE', #201109, #1289, #135334, .T. ) ;
#157311 = CIRCLE ( 'NONE', #210884, 0.09999999999999939493 ) ;
#157312 = EDGE_CURVE ( 'NONE', #172263, #10339, #67352, .T. ) ;
#157314 = ORIENTED_EDGE ( 'NONE', *, *, #159758, .F. ) ;
#157313 = DIRECTION ( 'NONE',  ( -1.000000000000000000, 0.000000000000000000, 0.000000000000000000 ) ) ;
#157315 = DIRECTION ( 'NONE',  ( 1.000000000000000000, 0.000000000000000000, 0.000000000000000000 ) ) ;
#157316 = CARTESIAN_POINT ( 'NONE',  ( -23.15000000000000213, 2.000000000011154189, -154.2753780772379173 ) ) ;
#157317 = CARTESIAN_POINT ( 'NONE',  ( -16.87683809663752754, 63.00406867418889334, -213.7537959572469788 ) ) ;
#157319 = DIRECTION ( 'NONE',  ( 1.000000000000000000, 0.000000000000000000, 0.000000000000000000 ) ) ;
#157318 = DIRECTION ( 'NONE',  ( 0.000000000000000000, 0.000000000000000000, 1.000000000000000000 ) ) ;
#157320 = CARTESIAN_POINT ( 'NONE',  ( -21.09096482362049940, 75.96055172123797661, -142.8866518499284268 ) ) ;
#157321 = DIRECTION ( 'NONE',  ( -0.000000000000000000, -0.1298341882519805091, -0.9915357197604881545 ) ) ;
#157322 = EDGE_CURVE ( 'NONE', #15847, #105736, #168733, .T. ) ;
#157323 = CARTESIAN_POINT ( 'NONE',  ( 18.39999999999999858, 85.50000000001136868, -29.42291809330221497 ) ) ;
#157324 = CYLINDRICAL_SURFACE ( 'NONE', #54948, 0.09999999999998898659 ) ;
#157325 = AXIS2_PLACEMENT_3D ( 'NONE', #128110, #188081, #107252 ) ;
#157326 = EDGE_LOOP ( 'NONE', ( #120689, #87961, #224048, #82341 ) ) ;
#157327 = ORIENTED_EDGE ( 'NONE', *, *, #124347, .F. ) ;
#157328 = ADVANCED_BREP_SHAPE_REPRESENTATION ( '', ( #104549, #2425 ), #114299 ) ;
#157329 = EDGE_CURVE ( 'NONE', #127614, #239082, #177073, .T. ) ;
#157331 = CARTESIAN_POINT ( 'NONE',  ( 21.98333005346336222, 76.00000000001219291, -143.8971828135809687 ) ) ;
#157330 = VECTOR ( 'NONE', #8832, 1000.000000000000000 ) ;
#157332 = TOROIDAL_SURFACE ( 'NONE', #228040, 0.2000000000000000111, 0.1000000000000000056 ) ;
#157334 = ORIENTED_EDGE ( 'NONE', *, *, #220438, .T. ) ;
#157333 = DIRECTION ( 'NONE',  ( 0.000000000000000000, -1.000000000000000000, 0.000000000000000000 ) ) ;
#157335 = CIRCLE ( 'NONE', #48965, 11.70000000000000462 ) ;
#157336 = ORIENTED_EDGE ( 'NONE', *, *, #49663, .T. ) ;
#157337 = DIRECTION ( 'NONE',  ( 1.000000000000000000, 0.000000000000000000, 0.000000000000000000 ) ) ;
#157338 = EDGE_LOOP ( 'NONE', ( #151057, #109779, #51244, #200292 ) ) ;
#157339 = CARTESIAN_POINT ( 'NONE',  ( 20.95392731769792150, 8.883061479188762988, -8.522227979571306733 ) ) ;
#157340 = AXIS2_PLACEMENT_3D ( 'NONE', #149567, #28351, #71312 ) ;
#157341 = EDGE_CURVE ( 'NONE', #154304, #30941, #148606, .T. ) ;
#157342 = ORIENTED_EDGE ( 'NONE', *, *, #42817, .F. ) ;
#157343 = EDGE_CURVE ( 'NONE', #172403, #40125, #55450, .T. ) ;
#157344 = CARTESIAN_POINT ( 'NONE',  ( 20.85000000000000142, 69.01799029515495931, -32.32695536626808064 ) ) ;
#157347 = ORIENTED_EDGE ( 'NONE', *, *, #248054, .T. ) ;
#157346 = ORIENTED_EDGE ( 'NONE', *, *, #106884, .T. ) ;
#157345 = VECTOR ( 'NONE', #199372, 999.9999999999998863 ) ;
#157348 = VERTEX_POINT ( 'NONE', #132461 ) ;
#157349 = VECTOR ( 'NONE', #102040, 1000.000000000000000 ) ;
#157350 = AXIS2_PLACEMENT_3D ( 'NONE', #155822, #97061, #254836 ) ;
#157351 = ORIENTED_EDGE ( 'NONE', *, *, #215977, .T. ) ;
#157352 = ORIENTED_EDGE ( 'NONE', *, *, #68785, .T. ) ;
#157353 = CARTESIAN_POINT ( 'NONE',  ( 18.59999999999999076, 11.65000000001115943, -155.7499999999999716 ) ) ;
#157355 = CLOSED_SHELL ( 'NONE', ( #207491, #45052, #10233, #75638, #34670, #166599, #1189, #3132, #172394, #99534, #244584, #242625, #152573, #15740, #123580, #140805, #25335, #97396, #216637, #674, #106418, #206079, #177904, #49698, #108923, #39395, #238787, #53039, #217810, #226049, #13767, #183399, #204033, #104597, #77374, #31632, #25016, #95189, #105166, #181839, #218326, #95296, #84096, #16251, #156267, #54354, #210635, #201631, #223677, #17949, #238663, #206065, #71192, #163573, #185680, #11662, #156796, #155493, #50476, #66551, #253564, #55804, #21675, #93555, #74474, #183567, #104965, #151563, #129156, #57196, #31023, #210999, #18447, #155875, #225211, #146476, #69753, #46597, #68162, #214543, #109167, #215495, #29353, #125548, #46141, #145865, #11579, #42832, #34906, #174653, #29242, #107393, #210707, #187084, #53879, #145050, #175202, #196638, #145906, #163340, #44847, #133759, #49024, #197302, #256943, #18729, #109928, #138433, #41151, #199514, #113633, #100542, #23051, #101003, #235146, #33035, #20626, #206757, #81023, #249365, #246780, #221304, #1736, #47867, #96468, #46409, #219180, #173778, #149979, #221822, #79773, #139955, #18717, #159505, #230724, #140430, #191914, #194010, #244015, #41446, #50894, #51627, #13023, #83348, #12051, #33301, #207064, #89512, #107001, #8507, #103940, #246990, #196535, #139164, #77602, #56062, #217671, #39252, #121120, #186589, #205676, #141125, #202219, #133010, #120835, #180398, #244890, #248003, #139986, #177382, #79277, #64733, #115055, #152406, #189293, #53516, #231539, #255223, #59498, #78659, #183284, #215372, #216248, #253166, #224496, #13324, #17860, #60356, #26450, #233457, #126565, #207777, #253453, #238401, #245869, #235420, #257643, #21629, #253727, #182999, #170093, #144963, #50711, #112009, #240251, #164272, #168091, #239710, #202422, #119596, #123501, #84349, #122349, #101304, #38593, #121507, #3035, #184221, #44041, #147017, #172802, #163824, #59490, #182834, #211715, #244401, #32230, #62708, #128631, #99125, #111544, #175185, #100449, #70612, #252142, #172500, #21766, #107096, #8501, #84904, #153034, #22616, #26988, #13739, #23063, #120375, #247307, #1652, #241891, #240196, #114382, #254773, #65768, #142388, #217128, #190729, #109472, #128420, #104465, #142894, #138515, #36841, #199813, #139918, #32706, #113943, #163895, #238011, #14133, #209052, #170554, #104439, #233653, #190888, #122245, #205998, #162731, #33494, #235334, #44658, #221190, #233696, #37951, #237978, #61644, #249520, #229686, #200740, #104758, #209688, #27617, #185374, #221978, #49643, #140993, #363, #254036, #102433, #198435, #13776, #50786, #82857, #55462, #80155, #173674, #219575, #193860, #105831, #60348, #119738, #70069, #52404, #187161, #2951, #119895, #225167, #92978, #231131, #163550, #105602, #89479, #55194, #215249, #78708, #158723, #233326, #194467, #240623, #205755, #43447, #66752, #61806, #165857, #255673, #185416, #225899, #215084, #24593, #128726, #132119, #212016, #149220, #199781, #119220, #247578, #177424, #248999, #123522, #236647, #61427, #95114, #144646, #205444, #215710, #191684, #218223, #246652, #108261, #7811, #33710, #51035, #249750, #172617, #491, #35777, #198663, #248031, #11121, #162112, #4257, #183388, #163988, #218133, #219157, #123998, #160878, #73553, #189385, #173399, #4509, #72396, #92402, #256662, #78630, #187329, #192709, #118262, #9219, #250731, #97133, #115025, #236691, #84632, #107644, #114204, #115322, #248683, #38937, #126206, #122637, #124979, #93289, #67347, #196086, #244536, #54691, #245075, #230267, #118240, #7458, #33676, #25845, #240791, #225554, #45482, #232203, #152092, #245206, #45209, #176146, #165789, #60230, #237498, #27970, #58599, #143464, #3480, #223243, #71867, #109490, #196398, #214531, #183899, #126123, #210384, #207640, #41828, #93571, #11010, #9612, #219871, #208913, #115227, #182462, #123933, #256959, #69495, #40494, #37554, #257109, #226156, #14950, #76101, #9546, #109457, #102014, #246116, #40853, #60300, #73145, #93692, #98852, #219184, #115339, #14475, #26371, #243734, #130409, #212692, #40508, #155721, #32637, #10898, #195515, #36428, #83765, #135916, #77427 ) ) ;
#157354 = LINE ( 'NONE', #97305, #495 ) ;
#157357 = ORIENTED_EDGE ( 'NONE', *, *, #136681, .F. ) ;
#157356 = DIRECTION ( 'NONE',  ( 0.000000000000000000, 0.000000000000000000, 1.000000000000000000 ) ) ;
#157358 = CARTESIAN_POINT ( 'NONE',  ( -20.64999999999999858, 76.00000000001192291, -105.0231074845243029 ) ) ;
#157360 = ORIENTED_EDGE ( 'NONE', *, *, #35803, .T. ) ;
#157359 = PLANE ( 'NONE',  #60218 ) ;
#157361 = DIRECTION ( 'NONE',  ( 0.000000000000000000, 0.8814952561688430555, -0.4721928772777346239 ) ) ;
#157362 = ORIENTED_EDGE ( 'NONE', *, *, #158371, .T. ) ;
#157363 = CARTESIAN_POINT ( 'NONE',  ( 21.05000000000000071, 71.00000000001223555, -148.9283735034374843 ) ) ;
#157365 = EDGE_CURVE ( 'NONE', #66860, #190582, #231244, .T. ) ;
#157364 = ORIENTED_EDGE ( 'NONE', *, *, #133002, .T. ) ;
#157366 = AXIS2_PLACEMENT_3D ( 'NONE', #78122, #201942, #102807 ) ;
#157367 = LINE ( 'NONE', #199027, #230466 ) ;
#157368 = DIRECTION ( 'NONE',  ( 0.000000000000000000, 0.4999999999999689138, 0.8660254037844565822 ) ) ;
#157369 = LINE ( 'NONE', #80325, #210800 ) ;
#157370 = ORIENTED_EDGE ( 'NONE', *, *, #177048, .T. ) ;
#157372 = DIRECTION ( 'NONE',  ( -2.915501640297152804E-16, -1.000000000000000000, -6.997203936713167125E-15 ) ) ;
#157371 = CARTESIAN_POINT ( 'NONE',  ( -16.87333278164147288, 9.882609784589883262, -46.63316780615359392 ) ) ;
#157373 = CARTESIAN_POINT ( 'NONE',  ( -14.11361717019516071, 66.54257354752292031, -84.52306561612432745 ) ) ;
#157374 = AXIS2_PLACEMENT_3D ( 'NONE', #150396, #173849, #193379 ) ;
#157375 = DIRECTION ( 'NONE',  ( -6.938893903907222856E-15, -1.000000000000000000, -6.982962677686266711E-15 ) ) ;
#157376 = FACE_OUTER_BOUND ( 'NONE', #192591, .T. ) ;
#157377 = DIRECTION ( 'NONE',  ( 0.000000000000000000, 0.000000000000000000, 1.000000000000000000 ) ) ;
#157378 = ORIENTED_EDGE ( 'NONE', *, *, #199663, .F. ) ;
#157379 = ORIENTED_EDGE ( 'NONE', *, *, #132833, .F. ) ;
#157381 = VERTEX_POINT ( 'NONE', #93324 ) ;
#157380 = AXIS2_PLACEMENT_3D ( 'NONE', #40924, #175302, #99547 ) ;
#157382 = EDGE_CURVE ( 'NONE', #149012, #134658, #164591, .T. ) ;
#157383 = CARTESIAN_POINT ( 'NONE',  ( 18.59999999999999076, 0.4810385098657082859, -209.0827657365571213 ) ) ;
#157384 = CARTESIAN_POINT ( 'NONE',  ( 21.05000000000000071, 76.00000000001190870, -103.0231074845243029 ) ) ;
#157385 = ORIENTED_EDGE ( 'NONE', *, *, #168943, .T. ) ;
#157386 = PLANE ( 'NONE',  #218409 ) ;
#157387 = VERTEX_POINT ( 'NONE', #131168 ) ;
#157388 = CARTESIAN_POINT ( 'NONE',  ( 21.30000000000002558, 76.00000000001237765, -170.0231074845243597 ) ) ;
#157389 = CARTESIAN_POINT ( 'NONE',  ( -23.15000000000000213, 7.128833340094563376, -233.7327013124401276 ) ) ;
#157390 = AXIS2_PLACEMENT_3D ( 'NONE', #198960, #56851, #16501 ) ;
#157391 = AXIS2_PLACEMENT_3D ( 'NONE', #242051, #238196, #59534 ) ;
#157392 = CIRCLE ( 'NONE', #111573, 2.599999999999998312 ) ;
#157393 = ORIENTED_EDGE ( 'NONE', *, *, #78514, .T. ) ;
#157394 = TOROIDAL_SURFACE ( 'NONE', #144872, 0.2000000000000000111, 0.1000000000000000056 ) ;
#157395 = CARTESIAN_POINT ( 'NONE',  ( -23.25000000000000000, 76.00000000001142553, -36.02310748452432421 ) ) ;
#157396 = SURFACE_SIDE_STYLE ('',( #156107 ) ) ;
#157397 = EDGE_CURVE ( 'NONE', #158507, #184576, #92041, .T. ) ;
#157398 = AXIS2_PLACEMENT_3D ( 'NONE', #202845, #183293, #24238 ) ;
#157399 = ADVANCED_FACE ( 'NONE', ( #71223 ), #174200, .F. ) ;
#157400 = ORIENTED_EDGE ( 'NONE', *, *, #195676, .T. ) ;
#157401 = VERTEX_POINT ( 'NONE', #210713 ) ;
#157402 = EDGE_LOOP ( 'NONE', ( #223326, #21451, #233596, #191419 ) ) ;
#157403 = CARTESIAN_POINT ( 'NONE',  ( -20.64999999999999858, 2.000000000011154189, -154.2753780772379173 ) ) ;
#157404 = CARTESIAN_POINT ( 'NONE',  ( 22.45301702632625762, 75.98478912030257959, -215.1728997087847404 ) ) ;
#157405 = CARTESIAN_POINT ( 'NONE',  ( -16.91247567987037925, 66.04091731634233042, -56.89438302598705377 ) ) ;
#157406 = DIRECTION ( 'NONE',  ( 0.000000000000000000, 1.000000000000000000, 0.000000000000000000 ) ) ;
#157407 = CARTESIAN_POINT ( 'NONE',  ( 22.50000000000000000, 0.1000000000111554016, -122.2500000000000284 ) ) ;
#157408 = EDGE_CURVE ( 'NONE', #154183, #157514, #239594, .T. ) ;
#157410 = FACE_OUTER_BOUND ( 'NONE', #141110, .T. ) ;
#157409 = CARTESIAN_POINT ( 'NONE',  ( 21.04999999999999716, 0.09843750001147316686, -161.2007690899076806 ) ) ;
#157411 = FACE_OUTER_BOUND ( 'NONE', #87048, .T. ) ;
#157413 = ORIENTED_EDGE ( 'NONE', *, *, #168683, .T. ) ;
#157412 = DIRECTION ( 'NONE',  ( 1.000000000000000000, -2.952720810173289112E-16, -2.061873921506763405E-30 ) ) ;
#157414 = CARTESIAN_POINT ( 'NONE',  ( -16.88495309932521593, 9.954627058484010860, -79.63454867381196323 ) ) ;
#157415 = EDGE_LOOP ( 'NONE', ( #24820, #127084 ) ) ;
#157416 = DIRECTION ( 'NONE',  ( 0.000000000000000000, 0.000000000000000000, -1.000000000000000000 ) ) ;
#157417 = ORIENTED_EDGE ( 'NONE', *, *, #143483, .T. ) ;
#157418 = ORIENTED_EDGE ( 'NONE', *, *, #97523, .F. ) ;
#157419 = DIRECTION ( 'NONE',  ( 2.879366945564059217E-14, -0.9875055080513751582, 0.1575844902526747915 ) ) ;
#157420 = CARTESIAN_POINT ( 'NONE',  ( 20.94999999999999929, 7.128833340094563376, -233.7327013124401276 ) ) ;
#157422 = EDGE_CURVE ( 'NONE', #20758, #77073, #39706, .T. ) ;
#157421 = DIRECTION ( 'NONE',  ( 1.000000000000000000, -0.000000000000000000, -0.000000000000000000 ) ) ;
#157424 = EDGE_CURVE ( 'NONE', #77397, #46041, #150742, .T. ) ;
#157423 = ORIENTED_EDGE ( 'NONE', *, *, #58752, .T. ) ;
#157425 = CIRCLE ( 'NONE', #240779, 0.2000000000000057288 ) ;
#157426 = CARTESIAN_POINT ( 'NONE',  ( 20.94999999999999929, 68.97833521811179480, -99.18954208262705663 ) ) ;
#157427 = ORIENTED_EDGE ( 'NONE', *, *, #36511, .T. ) ;
#157428 = ORIENTED_EDGE ( 'NONE', *, *, #13416, .F. ) ;
#157429 = ADVANCED_FACE ( 'NONE', ( #75085 ), #172795, .T. ) ;
#157430 = ORIENTED_EDGE ( 'NONE', *, *, #153245, .T. ) ;
#157431 = CARTESIAN_POINT ( 'NONE',  ( 20.00000000000000355, 1.350000000000000089, 16.50000000000000000 ) ) ;
#157432 = DIRECTION ( 'NONE',  ( 0.000000000000000000, -7.034366652768095332E-15, 1.000000000000000000 ) ) ;
#157433 = ORIENTED_EDGE ( 'NONE', *, *, #114380, .T. ) ;
#157434 = DIRECTION ( 'NONE',  ( -1.000000000000000000, -0.000000000000000000, -0.000000000000000000 ) ) ;
#157435 = LINE ( 'NONE', #79117, #231996 ) ;
#157436 = CARTESIAN_POINT ( 'NONE',  ( 22.49999999999999645, 11.64987090377452184, -133.9174801091270695 ) ) ;
#157437 = ORIENTED_EDGE ( 'NONE', *, *, #188029, .F. ) ;
#157438 = CARTESIAN_POINT ( 'NONE',  ( 22.50000000000000000, 75.90000000001199965, -110.8138870828976934 ) ) ;
#157439 = CARTESIAN_POINT ( 'NONE',  ( -20.95000000000000284, 11.65000000001115232, -93.48519422934610645 ) ) ;
#157440 = TOROIDAL_SURFACE ( 'NONE', #94850, 0.6000000000000017542, 0.1000000000000000056 ) ;
#157442 = AXIS2_PLACEMENT_3D ( 'NONE', #56656, #18847, #219606 ) ;
#157441 = CARTESIAN_POINT ( 'NONE',  ( -22.44366136229477249, 26.02348510400886639, -254.3054723516606259 ) ) ;
#157443 = TOROIDAL_SURFACE ( 'NONE', #78281, 7.800000000000000711, 0.1000000000000000056 ) ;
#157444 = EDGE_LOOP ( 'NONE', ( #244616, #112224, #199043, #132033, #197668, #58572, #29634, #16360, #111228, #71134, #92808, #253069, #172293, #42477, #154140, #54885, #34466, #90279, #97889, #177193, #194821, #61102, #252374, #69948, #106256 ) ) ;
#157445 = CARTESIAN_POINT ( 'NONE',  ( -21.05000000000000071, 11.65000000001115588, -33.60000000000000142 ) ) ;
#157446 = EDGE_LOOP ( 'NONE', ( #256297, #62231, #142868, #54106 ) ) ;
#157447 = EDGE_CURVE ( 'NONE', #230655, #115707, #239390, .T. ) ;
#157448 = DIRECTION ( 'NONE',  ( 0.000000000000000000, 0.1298341882519953583, 0.9915357197604862671 ) ) ;
#157449 = EDGE_CURVE ( 'NONE', #37340, #257831, #6133, .T. ) ;
#157450 = DIRECTION ( 'NONE',  ( 0.000000000000000000, 1.000000000000000000, 6.982962677686266711E-15 ) ) ;
#157451 = DIRECTION ( 'NONE',  ( -0.7071067811865389130, -5.024295867788141276E-15, 0.7071067811865561215 ) ) ;
#157452 = DIRECTION ( 'NONE',  ( 0.000000000000000000, 0.000000000000000000, 1.000000000000000000 ) ) ;
#157453 = DIRECTION ( 'NONE',  ( 0.000000000000000000, 0.000000000000000000, -1.000000000000000000 ) ) ;
#157454 = ORIENTED_EDGE ( 'NONE', *, *, #189191, .F. ) ;
#157455 = DIRECTION ( 'NONE',  ( -1.000000000000000000, -0.000000000000000000, -0.000000000000000000 ) ) ;
#157456 = DIRECTION ( 'NONE',  ( -0.7071067811865487940, -0.7071067811865463515, -4.216150419019404490E-15 ) ) ;
#157457 = VECTOR ( 'NONE', #36330, 1000.000000000000000 ) ;
#157458 = CARTESIAN_POINT ( 'NONE',  ( -18.41809261886931992, 77.26488344959624044, -241.9697967765189048 ) ) ;
#157459 = DIRECTION ( 'NONE',  ( 1.000000000000000000, -0.000000000000000000, -0.000000000000000000 ) ) ;
#157460 = ADVANCED_FACE ( 'NONE', ( #15090 ), #16385, .T. ) ;
#157461 = VECTOR ( 'NONE', #223211, 1000.000000000000227 ) ;
#157462 = DIRECTION ( 'NONE',  ( 0.000000000000000000, 4.510281037540195239E-13, 1.000000000000000000 ) ) ;
#157463 = AXIS2_PLACEMENT_3D ( 'NONE', #192920, #71703, #11732 ) ;
#157464 = ORIENTED_EDGE ( 'NONE', *, *, #200097, .F. ) ;
#157465 = ORIENTED_EDGE ( 'NONE', *, *, #246825, .T. ) ;
#157466 = CARTESIAN_POINT ( 'NONE',  ( -16.77683809663752257, 23.65833333334447985, -83.75000000000004263 ) ) ;
#157467 = CARTESIAN_POINT ( 'NONE',  ( -23.25000000000000000, 76.10085836911147794, -215.2726746080137445 ) ) ;
#157468 = DIRECTION ( 'NONE',  ( -0.000000000000000000, 1.000000000000000000, -0.000000000000000000 ) ) ;
#157469 = DIRECTION ( 'NONE',  ( 0.000000000000000000, 6.982962677686266711E-15, -1.000000000000000000 ) ) ;
#157470 = DIRECTION ( 'NONE',  ( -1.000000000000000000, -0.000000000000000000, -0.000000000000000000 ) ) ;
#157471 = ORIENTED_EDGE ( 'NONE', *, *, #122134, .F. ) ;
#157472 = DIRECTION ( 'NONE',  ( -1.000000000000000000, 0.000000000000000000, 0.000000000000000000 ) ) ;
#157473 = CARTESIAN_POINT ( 'NONE',  ( 21.05000000000000071, 67.23127455305841238, -235.8551265064783991 ) ) ;
#157474 = VERTEX_POINT ( 'NONE', #169060 ) ;
#157475 = CARTESIAN_POINT ( 'NONE',  ( 21.05000000000000071, 77.16270174994990327, -94.92310748452430857 ) ) ;
#157476 = DIRECTION ( 'NONE',  ( 0.000000000000000000, 0.1350103645451876666, -0.9908441862701600211 ) ) ;
#157477 = EDGE_CURVE ( 'NONE', #192885, #34352, #93644, .T. ) ;
#157478 = AXIS2_PLACEMENT_3D ( 'NONE', #254194, #157733, #135531 ) ;
#157479 = CIRCLE ( 'NONE', #53388, 0.5000000000000008882 ) ;
#157480 = CIRCLE ( 'NONE', #78323, 0.09999999999999939493 ) ;
#157481 = ORIENTED_EDGE ( 'NONE', *, *, #25039, .F. ) ;
#157482 = CARTESIAN_POINT ( 'NONE',  ( -20.94684162810195005, 12.93678149440677494, -205.1845283066507761 ) ) ;
#157483 = EDGE_CURVE ( 'NONE', #73958, #130466, #182780, .T. ) ;
#157484 = ORIENTED_EDGE ( 'NONE', *, *, #22755, .T. ) ;
#157485 = DIRECTION ( 'NONE',  ( -0.000000000000000000, -6.982962677686266711E-15, 1.000000000000000000 ) ) ;
#157486 = AXIS2_PLACEMENT_3D ( 'NONE', #52557, #211665, #133401 ) ;
#157487 = CARTESIAN_POINT ( 'NONE',  ( 20.94999999999999929, 28.32080209959243788, -238.8452605374484676 ) ) ;
#157488 = CARTESIAN_POINT ( 'NONE',  ( -18.59999999999999787, -1.164121893241208960, -41.41484808557160591 ) ) ;
#157489 = DIRECTION ( 'NONE',  ( 0.000000000000000000, 1.000000000000000000, 0.000000000000000000 ) ) ;
#157491 = EDGE_CURVE ( 'NONE', #214758, #4150, #159735, .T. ) ;
#157490 = DIRECTION ( 'NONE',  ( 1.000000000000000000, 0.000000000000000000, 0.000000000000000000 ) ) ;
#157492 = DIRECTION ( 'NONE',  ( 1.000000000000000000, -0.000000000000000000, -0.000000000000000000 ) ) ;
#157493 = CARTESIAN_POINT ( 'NONE',  ( 18.57071067811864040, 65.82071067813016896, -48.17310748452439384 ) ) ;
#157494 = CARTESIAN_POINT ( 'NONE',  ( -20.94999999999999929, 68.96868720525692709, -132.9139565462971007 ) ) ;
#157495 = CARTESIAN_POINT ( 'NONE',  ( 18.46858270002953617, -7.745884046994173211, -209.9554738686949520 ) ) ;
#157496 = ADVANCED_FACE ( 'NONE', ( #140144 ), #239270, .T. ) ;
#157497 = DIRECTION ( 'NONE',  ( -0.000000000000000000, 0.000000000000000000, -1.000000000000000000 ) ) ;
#157498 = DIRECTION ( 'NONE',  ( 0.000000000000000000, 0.000000000000000000, 1.000000000000000000 ) ) ;
#157499 = CARTESIAN_POINT ( 'NONE',  ( -21.05000000000000071, -1.162701749926853712, -175.4999999999999716 ) ) ;
#157500 = AXIS2_PLACEMENT_3D ( 'NONE', #73248, #152781, #232306 ) ;
#157501 = AXIS2_PLACEMENT_3D ( 'NONE', #132321, #210582, #211884 ) ;
#157502 = AXIS2_PLACEMENT_3D ( 'NONE', #74819, #72228, #55174 ) ;
#157503 = DIRECTION ( 'NONE',  ( -0.9880948137434723000, 0.1538461538461483591, -0.000000000000000000 ) ) ;
#157504 = LINE ( 'NONE', #199160, #162059 ) ;
#157505 = EDGE_CURVE ( 'NONE', #15770, #254139, #193602, .T. ) ;
#157508 = EDGE_CURVE ( 'NONE', #132241, #2617, #231033, .T. ) ;
#157507 = EDGE_CURVE ( 'NONE', #64319, #200486, #164382, .T. ) ;
#157506 = AXIS2_PLACEMENT_3D ( 'NONE', #156822, #78517, #116388 ) ;
#157509 = ORIENTED_EDGE ( 'NONE', *, *, #56454, .F. ) ;
#157510 = CARTESIAN_POINT ( 'NONE',  ( 21.05000000000000426, 6.300183336267740408, 0.05132743234154404921 ) ) ;
#157511 = FACE_OUTER_BOUND ( 'NONE', #124570, .T. ) ;
#157512 = CARTESIAN_POINT ( 'NONE',  ( -20.94999999999994600, 65.15000000001120384, -3.023107484524792277 ) ) ;
#157513 =( REPRESENTATION_RELATIONSHIP ('NONE','NONE', #36900, #233377 ) REPRESENTATION_RELATIONSHIP_WITH_TRANSFORMATION ( #106740 )SHAPE_REPRESENTATION_RELATIONSHIP( ) );
#157514 = VERTEX_POINT ( 'NONE', #198847 ) ;
#157515 = CARTESIAN_POINT ( 'NONE',  ( 23.14999999999999858, 36.65892442174935439, -249.5511627012433848 ) ) ;
#157516 = ORIENTED_EDGE ( 'NONE', *, *, #33333, .T. ) ;
#157517 = FACE_OUTER_BOUND ( 'NONE', #42488, .T. ) ;
#157518 = DIRECTION ( 'NONE',  ( 0.000000000000000000, -6.982962677686266711E-15, 1.000000000000000000 ) ) ;
#157519 = CIRCLE ( 'NONE', #190841, 0.09999999999999939493 ) ;
#157520 = ORIENTED_EDGE ( 'NONE', *, *, #232673, .T. ) ;
#157521 = EDGE_CURVE ( 'NONE', #63488, #55509, #10272, .T. ) ;
#157523 = EDGE_CURVE ( 'NONE', #103081, #127404, #120624, .T. ) ;
#157522 = AXIS2_PLACEMENT_3D ( 'NONE', #16850, #250308, #15579 ) ;
#157524 = AXIS2_PLACEMENT_3D ( 'NONE', #176912, #119488, #236847 ) ;
#157525 = CIRCLE ( 'NONE', #115790, 0.09999999999999939493 ) ;
#157527 = ORIENTED_EDGE ( 'NONE', *, *, #174964, .T. ) ;
#157526 = VECTOR ( 'NONE', #124843, 1000.000000000000000 ) ;
#157528 = DIRECTION ( 'NONE',  ( -1.000000000000000000, 0.000000000000000000, 0.000000000000000000 ) ) ;
#157529 = EDGE_CURVE ( 'NONE', #99797, #80905, #95885, .T. ) ;
#157530 =( BOUNDED_SURFACE ( )  B_SPLINE_SURFACE ( 3, 2, ( 
 ( #45133, #43857, #187234 ),
 ( #86807, #243320, #8579 ),
 ( #46399, #167671, #144213 ),
 ( #108945, #68555, #247170 ) ),
 .UNSPECIFIED., .F., .F., .F. ) 
 B_SPLINE_SURFACE_WITH_KNOTS ( ( 4, 4 ),
 ( 3, 3 ),
 ( 0.0006461284895274055275, 0.0007503702773986016886 ),
 ( 0.000000000000000000, 1.000000000000000000 ),
 .UNSPECIFIED. ) 
 GEOMETRIC_REPRESENTATION_ITEM ( )  RATIONAL_B_SPLINE_SURFACE ( (
 ( 1.000000000000000000, 0.7071067811865471286, 1.000000000000000000),
 ( 1.000000000000000000, 0.7076476444648464037, 1.000000000000000000),
 ( 1.000000000000000000, 0.7075727925192379919, 1.000000000000000000),
 ( 1.000000000000000000, 0.7071067811865229258, 1.000000000000000000) ) ) 
 REPRESENTATION_ITEM ( '' )  SURFACE ( )  );
#157531 = ORIENTED_EDGE ( 'NONE', *, *, #116792, .F. ) ;
#157532 = AXIS2_PLACEMENT_3D ( 'NONE', #206952, #150820, #6165 ) ;
#157533 = CARTESIAN_POINT ( 'NONE',  ( -22.39999999999999503, 68.20922040163873135, -136.6231074845243540 ) ) ;
#157534 = DIRECTION ( 'NONE',  ( 1.000000000000000000, 0.000000000000000000, 0.000000000000000000 ) ) ;
#157536 = DIRECTION ( 'NONE',  ( 0.000000000000000000, -0.4999999999999689138, -0.8660254037844565822 ) ) ;
#157535 = UNCERTAINTY_MEASURE_WITH_UNIT (LENGTH_MEASURE( 1.000000000000000082E-05 ), #111505, 'distance_accuracy_value', 'NONE');
#157537 = DIRECTION ( 'NONE',  ( 0.000000000000000000, -0.9868171638914230437, -0.1618390714546045217 ) ) ;
#157538 = ADVANCED_FACE ( 'NONE', ( #175462 ), #251847, .F. ) ;
#157539 = CARTESIAN_POINT ( 'NONE',  ( -12.25000000000000533, 47.91126876242805110, -234.2648823414209289 ) ) ;
#157540 = DIRECTION ( 'NONE',  ( 0.000000000000000000, 1.000000000000000000, 0.000000000000000000 ) ) ;
#157541 = CARTESIAN_POINT ( 'NONE',  ( 18.79999999999999716, 4.513204987021263825, 22.10000000000000142 ) ) ;
#157544 = ORIENTED_EDGE ( 'NONE', *, *, #90341, .T. ) ;
#157543 = EDGE_CURVE ( 'NONE', #113349, #48405, #106079, .T. ) ;
#157542 = CARTESIAN_POINT ( 'NONE',  ( 21.05000000000000071, 69.45934304831071415, -102.9231074845243512 ) ) ;
#157545 = VERTEX_POINT ( 'NONE', #161023 ) ;
#157547 = CARTESIAN_POINT ( 'NONE',  ( -18.40000000000000213, 64.52683809664958403, -123.9731074845243768 ) ) ;
#157546 = CYLINDRICAL_SURFACE ( 'NONE', #37008, 0.1000000000000028644 ) ;
#157549 = ORIENTED_EDGE ( 'NONE', *, *, #156937, .T. ) ;
#157548 = DIRECTION ( 'NONE',  ( 1.000000000000000000, -0.000000000000000000, 0.000000000000000000 ) ) ;
#157550 = B_SPLINE_CURVE_WITH_KNOTS ( 'NONE', 3,
 ( #194783, #175240, #53954, #56503, #255957, #215589, #12290 ),
 .UNSPECIFIED., .F., .F.,
 ( 4, 3, 4 ),
 ( 0.000000000000000000, 3.882884552234470657E-05, 5.798605692158470456E-05 ),
 .UNSPECIFIED. ) ;
#157551 = ORIENTED_EDGE ( 'NONE', *, *, #184123, .T. ) ;
#157552 = DIRECTION ( 'NONE',  ( 0.000000000000000000, -0.000000000000000000, -1.000000000000000000 ) ) ;
#157553 = AXIS2_PLACEMENT_3D ( 'NONE', #195432, #251523, #32525 ) ;
#157554 = CARTESIAN_POINT ( 'NONE',  ( -20.54999999999999716, 2.400000000011155432, -187.7753780772378889 ) ) ;
#157555 = CARTESIAN_POINT ( 'NONE',  ( 18.58703555225010362, -9.406336740788765027, -7.124944641246808708 ) ) ;
#157556 = LINE ( 'NONE', #97502, #73408 ) ;
#157557 = EDGE_CURVE ( 'NONE', #89456, #78170, #116745, .T. ) ;
#157558 = CARTESIAN_POINT ( 'NONE',  ( 23.15000000000000213, 85.60000000001251408, -179.9170766071767389 ) ) ;
#157559 = CARTESIAN_POINT ( 'NONE',  ( 23.25000000000000000, 64.25000000001179501, -81.67310748452439384 ) ) ;
#157560 = AXIS2_PLACEMENT_3D ( 'NONE', #170570, #33619, #55654 ) ;
#157561 = CIRCLE ( 'NONE', #195141, 0.09999999999999864553 ) ;
#157562 = CARTESIAN_POINT ( 'NONE',  ( -23.25000000000000000, 76.00000000001126921, -203.5231074845248997 ) ) ;
#157563 = EDGE_CURVE ( 'NONE', #159849, #997, #158472, .T. ) ;
#157564 = VERTEX_POINT ( 'NONE', #80150 ) ;
#157565 = ORIENTED_EDGE ( 'NONE', *, *, #133171, .F. ) ;
#157566 = DIRECTION ( 'NONE',  ( 0.000000000000000000, -1.000000000000000000, -8.717686153663073805E-15 ) ) ;
#157567 = AXIS2_PLACEMENT_3D ( 'NONE', #163229, #104495, #43275 ) ;
#157568 = ORIENTED_EDGE ( 'NONE', *, *, #67932, .T. ) ;
#157569 = CARTESIAN_POINT ( 'NONE',  ( 20.95083306685154056, 8.916842641901356004, -142.4773248532583807 ) ) ;
#157570 = VERTEX_POINT ( 'NONE', #41091 ) ;
#157571 = CARTESIAN_POINT ( 'NONE',  ( 20.85000000000000142, -1.835859311432481045, -145.5044391687985694 ) ) ;
#157572 = AXIS2_PLACEMENT_3D ( 'NONE', #103109, #125271, #126551 ) ;
#157573 = CARTESIAN_POINT ( 'NONE',  ( -15.51798037960204724, 48.91301996986818068, -233.7868972119375428 ) ) ;
#157574 = FACE_OUTER_BOUND ( 'NONE', #235633, .T. ) ;
#157575 = EDGE_CURVE ( 'NONE', #98560, #30925, #42352, .T. ) ;
#157577 = EDGE_LOOP ( 'NONE', ( #177209, #154480, #194987, #126369 ) ) ;
#157576 = CARTESIAN_POINT ( 'NONE',  ( -22.47071067811865319, 7.720074744509219933, -33.40090754529740025 ) ) ;
#157578 = DIRECTION ( 'NONE',  ( 1.000000000000000000, 0.000000000000000000, 0.000000000000000000 ) ) ;
#157579 = VERTEX_POINT ( 'NONE', #100983 ) ;
#157580 = AXIS2_PLACEMENT_3D ( 'NONE', #87714, #246797, #29091 ) ;
#157581 = CARTESIAN_POINT ( 'NONE',  ( -20.64999999999999858, 74.05981308412420105, -123.6939882734709926 ) ) ;
#157582 = FACE_OUTER_BOUND ( 'NONE', #38550, .T. ) ;
#157583 = CIRCLE ( 'NONE', #165939, 0.09999999999999938105 ) ;
#157585 = SPHERICAL_SURFACE ( 'NONE', #81218, 0.1000000000000000056 ) ;
#157584 = CIRCLE ( 'NONE', #145056, 0.1000000000000028644 ) ;
#157586 = CARTESIAN_POINT ( 'NONE',  ( -21.07928932188134041, 75.90110485435833709, -209.8516241409176644 ) ) ;
#157587 = CIRCLE ( 'NONE', #211729, 11.65000000000000746 ) ;
#157588 = DIRECTION ( 'NONE',  ( -1.000000000000000000, -3.265361837132813093E-16, 0.000000000000000000 ) ) ;
#157589 = EDGE_LOOP ( 'NONE', ( #119430, #30062, #132411 ) ) ;
#157590 = FACE_OUTER_BOUND ( 'NONE', #26367, .T. ) ;
#157591 = EDGE_LOOP ( 'NONE', ( #93303, #60807, #14536, #36484 ) ) ;
#157594 = ORIENTED_EDGE ( 'NONE', *, *, #73368, .F. ) ;
#157593 = DIRECTION ( 'NONE',  ( 1.000000000000000000, 0.000000000000000000, 0.000000000000000000 ) ) ;
#157592 = CARTESIAN_POINT ( 'NONE',  ( -22.48660254037843131, 64.35000000001267040, -203.5731074845244279 ) ) ;
#157595 = AXIS2_PLACEMENT_3D ( 'NONE', #197997, #44076, #61056 ) ;
#157596 = LINE ( 'NONE', #196663, #231112 ) ;
#157597 = FACE_OUTER_BOUND ( 'NONE', #32859, .T. ) ;
#157598 = ORIENTED_EDGE ( 'NONE', *, *, #153482, .T. ) ;
#157599 = DIRECTION ( 'NONE',  ( 1.000000000000000000, 0.000000000000000000, 0.000000000000000000 ) ) ;
#157600 = CYLINDRICAL_SURFACE ( 'NONE', #248901, 0.1999999999999987899 ) ;
#157601 = DIRECTION ( 'NONE',  ( 0.000000000000000000, 0.9908441862701605762, 0.1350103645451835310 ) ) ;
#157603 = ORIENTED_EDGE ( 'NONE', *, *, #231786, .T. ) ;
#157602 = CARTESIAN_POINT ( 'NONE',  ( -21.05000000000000071, 14.77103648604101060, -236.4083752604501001 ) ) ;
#157604 = AXIS2_PLACEMENT_3D ( 'NONE', #203350, #242458, #224181 ) ;
#157605 = CARTESIAN_POINT ( 'NONE',  ( 20.94999999999999929, 11.65000000001115943, -60.15839931010294350 ) ) ;
#157606 = ORIENTED_EDGE ( 'NONE', *, *, #241587, .T. ) ;
#157607 = LINE ( 'NONE', #37637, #145211 ) ;
#157608 = CARTESIAN_POINT ( 'NONE',  ( 18.41789779300687968, -9.499999999988844479, -74.03206966635994490 ) ) ;
#157609 = DIRECTION ( 'NONE',  ( 1.000000000000000000, 0.000000000000000000, 0.000000000000000000 ) ) ;
#157610 = VERTEX_POINT ( 'NONE', #97137 ) ;
#157611 = CARTESIAN_POINT ( 'NONE',  ( 23.14999999999998437, 1.115600667400684642E-11, -138.0500000000000114 ) ) ;
#157612 = ORIENTED_EDGE ( 'NONE', *, *, #96436, .F. ) ;
#157613 = LINE ( 'NONE', #58440, #64603 ) ;
#157614 = CARTESIAN_POINT ( 'NONE',  ( -21.45000000000000284, 63.02410583447655767, -221.9179669651492759 ) ) ;
#157615 = CYLINDRICAL_SURFACE ( 'NONE', #185032, 0.09999999999998898659 ) ;
#157616 = ORIENTED_EDGE ( 'NONE', *, *, #256427, .T. ) ;
#157617 = CARTESIAN_POINT ( 'NONE',  ( -6.099999999999939249, 64.25000000001119815, -51.02310748452479316 ) ) ;
#157618 = DIRECTION ( 'NONE',  ( 1.000000000000000000, 0.000000000000000000, 0.000000000000000000 ) ) ;
#157619 = EDGE_CURVE ( 'NONE', #196072, #239511, #167087, .T. ) ;
#157620 = CARTESIAN_POINT ( 'NONE',  ( -21.05000000000000071, 11.60000000001115517, -93.57179676972454274 ) ) ;
#157621 = EDGE_LOOP ( 'NONE', ( #192957, #64199, #86088, #76565 ) ) ;
#157622 = VECTOR ( 'NONE', #129232, 1000.000000000000000 ) ;
#157623 = AXIS2_PLACEMENT_3D ( 'NONE', #9552, #188203, #52526 ) ;
#157624 = PLANE ( 'NONE',  #168178 ) ;
#157625 = CARTESIAN_POINT ( 'NONE',  ( -20.54999999999999716, 76.00000000001190870, -103.0231074845243029 ) ) ;
#157626 = TOROIDAL_SURFACE ( 'NONE', #53534, 11.65000000000000036, 0.1000000000000000056 ) ;
#157627 = CARTESIAN_POINT ( 'NONE',  ( -19.99999999999999645, 4.513204987021263825, 22.00000000000000355 ) ) ;
#157628 = EDGE_LOOP ( 'NONE', ( #181560, #72418, #17102, #189535 ) ) ;
#157629 =( BOUNDED_SURFACE ( )  B_SPLINE_SURFACE ( 3, 2, ( 
 ( #220750, #143767, #182924 ),
 ( #42133, #203756, #62957 ),
 ( #141216, #199922, #219445 ),
 ( #40861, #120404, #162079 ) ),
 .UNSPECIFIED., .F., .F., .F. ) 
 B_SPLINE_SURFACE_WITH_KNOTS ( ( 4, 4 ),
 ( 3, 3 ),
 ( 0.000000000000000000, 0.001979672783031562362 ),
 ( 0.000000000000000000, 1.000000000000000000 ),
 .UNSPECIFIED. ) 
 GEOMETRIC_REPRESENTATION_ITEM ( )  RATIONAL_B_SPLINE_SURFACE ( (
 ( 1.000000000000000000, 0.7103081912008540888, 1.000000000000000000),
 ( 1.000000000000000000, 0.7104998333558795176, 1.000000000000000000),
 ( 1.000000000000000000, 0.7107238315754857982, 1.000000000000000000),
 ( 1.000000000000000000, 0.7110073749539714827, 1.000000000000000000) ) ) 
 REPRESENTATION_ITEM ( '' )  SURFACE ( )  );
#157630 = DIRECTION ( 'NONE',  ( 0.000000000000000000, 0.000000000000000000, -1.000000000000000000 ) ) ;
#157631 = ORIENTED_EDGE ( 'NONE', *, *, #159405, .T. ) ;
#157633 = ORIENTED_EDGE ( 'NONE', *, *, #106383, .T. ) ;
#157632 = DIRECTION ( 'NONE',  ( -1.000000000000000000, 0.000000000000000000, 0.000000000000000000 ) ) ;
#157634 = EDGE_CURVE ( 'NONE', #125569, #247253, #159826, .T. ) ;
#157635 = EDGE_CURVE ( 'NONE', #184466, #54594, #31147, .T. ) ;
#157638 = ORIENTED_EDGE ( 'NONE', *, *, #215345, .F. ) ;
#157637 = VERTEX_POINT ( 'NONE', #3200 ) ;
#157636 = CARTESIAN_POINT ( 'NONE',  ( -21.07971444708686093, 0.08782343631782563165, 6.329792081626551159 ) ) ;
#157640 = VECTOR ( 'NONE', #104782, 1000.000000000000000 ) ;
#157639 = DIRECTION ( 'NONE',  ( 1.000000000000000000, 0.000000000000000000, -0.000000000000000000 ) ) ;
#157641 = CARTESIAN_POINT ( 'NONE',  ( -21.65000000000000213, 7.250000000011139534, -113.1500000000000341 ) ) ;
#157642 = DIRECTION ( 'NONE',  ( -1.186688945009010077E-16, -1.000000000000000000, -6.789366196018717631E-15 ) ) ;
#157643 = AXIS2_PLACEMENT_3D ( 'NONE', #69303, #165842, #127984 ) ;
#157644 = PLANE ( 'NONE',  #144048 ) ;
#157645 = DIRECTION ( 'NONE',  ( -2.952720810173289112E-16, -1.000000000000000000, -6.982962677686266711E-15 ) ) ;
#157646 = CARTESIAN_POINT ( 'NONE',  ( 21.05000000000000071, 65.37127968600826478, -195.8581939154368570 ) ) ;
#157647 = DIRECTION ( 'NONE',  ( -0.000000000000000000, -0.09425075112713271475, -0.9955484899852801162 ) ) ;
#157648 = CIRCLE ( 'NONE', #70152, 3.999999999999999112 ) ;
#157649 = DIRECTION ( 'NONE',  ( 1.000000000000000000, 0.000000000000000000, 0.000000000000000000 ) ) ;
#157650 = ORIENTED_EDGE ( 'NONE', *, *, #133488, .T. ) ;
#157651 = VERTEX_POINT ( 'NONE', #103579 ) ;
#157652 = VERTEX_POINT ( 'NONE', #128322 ) ;
#157653 = EDGE_CURVE ( 'NONE', #251965, #200607, #160312, .T. ) ;
#157654 = CARTESIAN_POINT ( 'NONE',  ( -20.64999999999999858, 7.128833340094563376, -233.7327013124401276 ) ) ;
#157657 = ORIENTED_EDGE ( 'NONE', *, *, #242764, .T. ) ;
#157656 = EDGE_CURVE ( 'NONE', #147363, #235864, #8371, .T. ) ;
#157655 = CARTESIAN_POINT ( 'NONE',  ( -12.25000000000000178, 66.15000000001185754, -86.27310748452437394 ) ) ;
#157658 = LINE ( 'NONE', #237156, #13526 ) ;
#157659 = ORIENTED_EDGE ( 'NONE', *, *, #166481, .F. ) ;
#157660 = DIRECTION ( 'NONE',  ( 2.952720810173288619E-16, 0.4088369013363286064, -0.9126074666063768159 ) ) ;
#157661 = VERTEX_POINT ( 'NONE', #63180 ) ;
#157662 = CARTESIAN_POINT ( 'NONE',  ( -23.25000000000000000, -9.600000000000004974, -9.893969122652444881 ) ) ;
#157663 = EDGE_CURVE ( 'NONE', #113827, #101660, #106152, .T. ) ;
#157664 = EDGE_LOOP ( 'NONE', ( #35911, #73895, #102084, #245067, #189926, #25802 ) ) ;
#157665 = EDGE_CURVE ( 'NONE', #76854, #221539, #139413, .T. ) ;
#157666 = DIRECTION ( 'NONE',  ( 0.000000000000000000, 0.000000000000000000, -1.000000000000000000 ) ) ;
#157667 = CARTESIAN_POINT ( 'NONE',  ( 23.40000000000005542, 83.80000000001119531, -37.18565239344504647 ) ) ;
#157668 = AXIS2_PLACEMENT_3D ( 'NONE', #182076, #25573, #105049 ) ;
#157669 = VECTOR ( 'NONE', #217863, 1000.000000000000227 ) ;
#157670 = VECTOR ( 'NONE', #152031, 1000.000000000000000 ) ;
#157672 = ORIENTED_EDGE ( 'NONE', *, *, #144784, .F. ) ;
#157671 = EDGE_LOOP ( 'NONE', ( #80299, #108549, #165077, #50819 ) ) ;
#157673 = EDGE_LOOP ( 'NONE', ( #113870, #15297, #39118, #38981 ) ) ;
#157674 = LINE ( 'NONE', #179773, #177959 ) ;
#157676 = ORIENTED_EDGE ( 'NONE', *, *, #255374, .F. ) ;
#157675 = ADVANCED_FACE ( 'NONE', ( #43639 ), #22813, .T. ) ;
#157677 = ORIENTED_EDGE ( 'NONE', *, *, #104029, .T. ) ;
#157678 = DIRECTION ( 'NONE',  ( 0.000000000000000000, 1.000000000000000000, 0.000000000000000000 ) ) ;
#157680 = ORIENTED_EDGE ( 'NONE', *, *, #105908, .T. ) ;
#157679 = CARTESIAN_POINT ( 'NONE',  ( 21.14999999999999858, 31.98723526783714988, -238.8784020251475511 ) ) ;
#157681 = AXIS2_PLACEMENT_3D ( 'NONE', #203634, #164524, #144924 ) ;
#157683 = DIRECTION ( 'NONE',  ( 0.000000000000000000, -6.982962677686266711E-15, 1.000000000000000000 ) ) ;
#157682 = DIRECTION ( 'NONE',  ( -1.000000000000000000, 2.952720810173289112E-16, 2.061873921506763405E-30 ) ) ;
#157684 = DIRECTION ( 'NONE',  ( 0.000000000000000000, -1.000000000000000000, 0.000000000000000000 ) ) ;
#157685 = LINE ( 'NONE', #73003, #219357 ) ;
#157686 = PLANE ( 'NONE',  #13664 ) ;
#157687 = VERTEX_POINT ( 'NONE', #47464 ) ;
#157689 = EDGE_CURVE ( 'NONE', #56718, #59718, #86581, .T. ) ;
#157688 = ORIENTED_EDGE ( 'NONE', *, *, #172473, .T. ) ;
#157690 = CARTESIAN_POINT ( 'NONE',  ( 20.85000000000000142, 6.803341081522319200, -233.7601854879220298 ) ) ;
#157691 = DIRECTION ( 'NONE',  ( -1.000000000000000000, 0.000000000000000000, 0.000000000000000000 ) ) ;
#157692 = DIRECTION ( 'NONE',  ( 0.000000000000000000, -6.982962677686266711E-15, 1.000000000000000000 ) ) ;
#157693 = ORIENTED_EDGE ( 'NONE', *, *, #114540, .T. ) ;
#157694 = AXIS2_PLACEMENT_3D ( 'NONE', #52999, #66487, #204693 ) ;
#157696 = FACE_OUTER_BOUND ( 'NONE', #155530, .T. ) ;
#157695 = TOROIDAL_SURFACE ( 'NONE', #182606, 1.900000000000002576, 0.1000000000000000056 ) ;
#157697 = AXIS2_PLACEMENT_3D ( 'NONE', #190259, #50703, #11626 ) ;
#157698 = DIRECTION ( 'NONE',  ( 1.000000000000000000, 0.000000000000000000, 0.000000000000000000 ) ) ;
#157699 = CARTESIAN_POINT ( 'NONE',  ( -15.06774609480955718, 12.47031117194349292, -214.0029172826438071 ) ) ;
#157700 = TOROIDAL_SURFACE ( 'NONE', #245139, 11.89999999999999858, 0.1000000000000000056 ) ;
#157701 = ORIENTED_EDGE ( 'NONE', *, *, #126864, .T. ) ;
#157702 = ORIENTED_EDGE ( 'NONE', *, *, #248648, .F. ) ;
#157703 = CARTESIAN_POINT ( 'NONE',  ( -18.59999999999999787, 64.35000000001230092, -157.8731074845244393 ) ) ;
#157704 = CARTESIAN_POINT ( 'NONE',  ( -20.94999999999999929, 28.15345123516638282, -259.0759448016705733 ) ) ;
#157705 = EDGE_LOOP ( 'NONE', ( #216621, #78472, #173756, #51660 ) ) ;
#157706 = DIRECTION ( 'NONE',  ( 0.000000000000000000, 1.000000000000000000, 0.000000000000000000 ) ) ;
#157707 = VERTEX_POINT ( 'NONE', #107459 ) ;
#157708 = DIRECTION ( 'NONE',  ( 1.000000000000000000, 0.000000000000000000, 0.000000000000000000 ) ) ;
#157709 = CARTESIAN_POINT ( 'NONE',  ( 20.94999999999999929, -9.499999999988844479, -191.1060308773475072 ) ) ;
#157711 = CARTESIAN_POINT ( 'NONE',  ( -20.89192007715127630, 68.10318897902124036, -224.1464165264002872 ) ) ;
#157710 = CYLINDRICAL_SURFACE ( 'NONE', #65549, 0.1000000000000026007 ) ;
#157712 = TOROIDAL_SURFACE ( 'NONE', #203455, 0.9750000000000019762, 0.1000000000000000056 ) ;
#157713 = FACE_OUTER_BOUND ( 'NONE', #220743, .T. ) ;
#157714 = CARTESIAN_POINT ( 'NONE',  ( -23.15000000000000213, 64.35000000001180354, -81.67310748452439384 ) ) ;
#157715 = AXIS2_PLACEMENT_3D ( 'NONE', #10600, #152702, #151403 ) ;
#157716 = CARTESIAN_POINT ( 'NONE',  ( -16.27683809663751191, 22.60660220755888972, -231.4167412770961505 ) ) ;
#157717 = EDGE_CURVE ( 'NONE', #233060, #27358, #222604, .T. ) ;
#157720 = EDGE_LOOP ( 'NONE', ( #117703, #187007, #233817, #129934 ) ) ;
#157719 = EDGE_LOOP ( 'NONE', ( #221428, #8728, #26426, #37541 ) ) ;
#157718 = CIRCLE ( 'NONE', #253512, 0.09999999999999939493 ) ;
#157721 = ORIENTED_EDGE ( 'NONE', *, *, #71168, .T. ) ;
#157722 = AXIS2_PLACEMENT_3D ( 'NONE', #202330, #27590, #181504 ) ;
#157723 = TOROIDAL_SURFACE ( 'NONE', #191012, 0.2000000000000000111, 0.1000000000000000056 ) ;
#157724 = VECTOR ( 'NONE', #150392, 1000.000000000000000 ) ;
#157725 = DIRECTION ( 'NONE',  ( 4.336808689942043611E-14, -1.000000000000000000, -0.000000000000000000 ) ) ;
#157726 = CARTESIAN_POINT ( 'NONE',  ( -21.05000000000000071, -0.09999999999999939493, 6.540656951701240729 ) ) ;
#157727 = FACE_OUTER_BOUND ( 'NONE', #246074, .T. ) ;
#157728 = CARTESIAN_POINT ( 'NONE',  ( -20.94999999999999929, 76.00000000001213607, -136.5231074845243313 ) ) ;
#157729 = CIRCLE ( 'NONE', #57708, 7.900000000000000355 ) ;
#157730 = ADVANCED_FACE ( 'NONE', ( #222241 ), #244391, .F. ) ;
#157731 = EDGE_CURVE ( 'NONE', #36049, #119237, #144004, .T. ) ;
#157733 = DIRECTION ( 'NONE',  ( -1.000000000000000000, 3.265361837132813093E-16, 2.280189983783949500E-30 ) ) ;
#157732 = DIRECTION ( 'NONE',  ( 1.000000000000000000, 0.000000000000000000, 0.000000000000000000 ) ) ;
#157734 = DIRECTION ( 'NONE',  ( -0.000000000000000000, 0.000000000000000000, -1.000000000000000000 ) ) ;
#157735 = EDGE_LOOP ( 'NONE', ( #218911, #233296, #227246, #183472 ) ) ;
#157736 = CARTESIAN_POINT ( 'NONE',  ( -20.94999999999999929, 11.75000000001115552, -107.5148057706540357 ) ) ;
#157737 = ORIENTED_EDGE ( 'NONE', *, *, #221440, .F. ) ;
#157738 = ORIENTED_EDGE ( 'NONE', *, *, #225868, .F. ) ;
#157739 = CARTESIAN_POINT ( 'NONE',  ( 18.49999999999998934, 10.25000000001115552, -91.75000000000005684 ) ) ;
#157740 = CARTESIAN_POINT ( 'NONE',  ( -21.05000000000000071, 67.23127455305841238, -235.8551265064783991 ) ) ;
#157741 = EDGE_CURVE ( 'NONE', #143461, #219189, #44925, .T. ) ;
#157742 = EDGE_CURVE ( 'NONE', #153971, #31072, #104848, .T. ) ;
#157743 = CARTESIAN_POINT ( 'NONE',  ( -16.87036670365548474, 9.989418819312801290, -87.97956011730209980 ) ) ;
#157744 = ADVANCED_FACE ( 'NONE', ( #184421 ), #27032, .F. ) ;
#157746 = EDGE_CURVE ( 'NONE', #182918, #117533, #226095, .T. ) ;
#157745 = VECTOR ( 'NONE', #114271, 999.9999999999998863 ) ;
#157747 = TOROIDAL_SURFACE ( 'NONE', #45259, 11.90000000000000213, 0.1000000000000000056 ) ;
#157748 = DIRECTION ( 'NONE',  ( 2.952720810173288619E-16, -1.000000000000000000, 0.000000000000000000 ) ) ;
#157749 = ORIENTED_EDGE ( 'NONE', *, *, #154688, .F. ) ;
#157750 = ORIENTED_EDGE ( 'NONE', *, *, #112644, .T. ) ;
#157751 = DIRECTION ( 'NONE',  ( -0.7070776581708965169, 0.2891032514073239024, -0.6453375049857822399 ) ) ;
#157752 = EDGE_CURVE ( 'NONE', #252845, #174960, #185520, .T. ) ;
#157753 = DIRECTION ( 'NONE',  ( -1.020425574104004196E-15, 6.982962677686266711E-15, -1.000000000000000000 ) ) ;
#157754 = ORIENTED_EDGE ( 'NONE', *, *, #29664, .T. ) ;
#157755 = DIRECTION ( 'NONE',  ( -0.000000000000000000, -0.000000000000000000, 1.000000000000000000 ) ) ;
#157756 = LINE ( 'NONE', #56002, #160981 ) ;
#157757 = DIRECTION ( 'NONE',  ( 0.000000000000000000, -1.000000000000000000, 2.775557561562888827E-14 ) ) ;
#157758 = DIRECTION ( 'NONE',  ( 0.000000000000000000, 6.982962677686266711E-15, -1.000000000000000000 ) ) ;
#157759 = DIRECTION ( 'NONE',  ( 0.000000000000000000, 0.000000000000000000, -1.000000000000000000 ) ) ;
#157760 = CIRCLE ( 'NONE', #199422, 0.09999999999999864553 ) ;
#157762 = DIRECTION ( 'NONE',  ( -1.000000000000000000, -0.000000000000000000, -0.000000000000000000 ) ) ;
#157761 = CARTESIAN_POINT ( 'NONE',  ( -18.59999999999999787, 74.16465844978715438, -57.86795619196135476 ) ) ;
#157763 = CARTESIAN_POINT ( 'NONE',  ( 18.59999999999999432, -1.135018845899022466, -74.71697688343232358 ) ) ;
#157764 = TOROIDAL_SURFACE ( 'NONE', #20349, 1.900000000000002576, 0.1000000000000000056 ) ;
#157765 = CARTESIAN_POINT ( 'NONE',  ( 21.00000000000000000, 12.13349391679638778, -210.8946109257198032 ) ) ;
#157766 = DIRECTION ( 'NONE',  ( -4.391705002472927119E-16, -1.000000000000000000, -7.026728003956683390E-15 ) ) ;
#157768 = DIRECTION ( 'NONE',  ( 1.000000000000000000, 0.000000000000000000, 0.000000000000000000 ) ) ;
#157767 = AXIS2_PLACEMENT_3D ( 'NONE', #75690, #96494, #216455 ) ;
#157770 = ORIENTED_EDGE ( 'NONE', *, *, #129086, .F. ) ;
#157769 = CARTESIAN_POINT ( 'NONE',  ( 20.04999999999999716, 8.750000000011173285, -46.15000000000000568 ) ) ;
#157771 = CIRCLE ( 'NONE', #249304, 0.09999999999999799327 ) ;
#157772 = EDGE_CURVE ( 'NONE', #22057, #245427, #156020, .T. ) ;
#157773 = FACE_OUTER_BOUND ( 'NONE', #98881, .T. ) ;
#157774 = EDGE_LOOP ( 'NONE', ( #256881, #176691, #183486, #218383 ) ) ;
#157775 = EDGE_CURVE ( 'NONE', #25370, #161777, #151929, .T. ) ;
#157776 = EDGE_CURVE ( 'NONE', #34583, #16075, #110193, .T. ) ;
#157777 = CARTESIAN_POINT ( 'NONE',  ( 18.39999999999999503, 28.17589918783267322, -238.5974746063260739 ) ) ;
#157778 = AXIS2_PLACEMENT_3D ( 'NONE', #100309, #80748, #142022 ) ;
#157779 = TOROIDAL_SURFACE ( 'NONE', #45290, 2.100000000000002309, 0.1000000000000000056 ) ;
#157780 = ORIENTED_EDGE ( 'NONE', *, *, #170074, .T. ) ;
#157781 = CARTESIAN_POINT ( 'NONE',  ( -18.59999999999999787, 5.900000000011102586, -77.21909976465646253 ) ) ;
#157782 = FACE_OUTER_BOUND ( 'NONE', #131516, .T. ) ;
#157783 = LINE ( 'NONE', #79455, #29777 ) ;
#157784 = DIRECTION ( 'NONE',  ( 0.000000000000000000, 0.01562499999998609446, -0.9998779222360101304 ) ) ;
#157785 = DIRECTION ( 'NONE',  ( -0.000000000000000000, 1.000000000000000000, 6.982962677686267499E-15 ) ) ;
#157786 = CARTESIAN_POINT ( 'NONE',  ( -23.15000000000000213, 67.23127455305835554, -235.8551265064784559 ) ) ;
#157787 = ORIENTED_EDGE ( 'NONE', *, *, #243413, .T. ) ;
#157788 = CARTESIAN_POINT ( 'NONE',  ( -21.64999999999999858, 65.95000000001186891, -90.27310748452438816 ) ) ;
#157790 = ORIENTED_EDGE ( 'NONE', *, *, #155869, .T. ) ;
#157789 = FACE_OUTER_BOUND ( 'NONE', #26723, .T. ) ;
#157791 = DIRECTION ( 'NONE',  ( 0.000000000000000000, -1.000000000000000000, -1.445602896647339410E-16 ) ) ;
#157792 = LINE ( 'NONE', #40402, #137057 ) ;
#157793 = FACE_OUTER_BOUND ( 'NONE', #97620, .T. ) ;
#157794 = ORIENTED_EDGE ( 'NONE', *, *, #253872, .F. ) ;
#157795 = DIRECTION ( 'NONE',  ( -0.000000000000000000, -0.000000000000000000, 1.000000000000000000 ) ) ;
#157796 = VECTOR ( 'NONE', #75418, 1000.000000000000000 ) ;
#157797 = PRODUCT_CONTEXT ( 'NONE', #154098, 'mechanical' ) ;
#157798 = CARTESIAN_POINT ( 'NONE',  ( -23.24999999999999645, 87.01908966642815813, -199.5693496768551825 ) ) ;
#157799 = ORIENTED_EDGE ( 'NONE', *, *, #212165, .F. ) ;
#157800 = CARTESIAN_POINT ( 'NONE',  ( -23.25000000000000000, -1.164121893241208960, -41.41484808557160591 ) ) ;
#157801 = DIRECTION ( 'NONE',  ( 0.000000000000000000, 0.000000000000000000, -1.000000000000000000 ) ) ;
#157802 = DIRECTION ( 'NONE',  ( 6.938893903907270030E-14, 0.000000000000000000, -1.000000000000000000 ) ) ;
#157803 = ORIENTED_EDGE ( 'NONE', *, *, #134671, .F. ) ;
#157804 = ORIENTED_EDGE ( 'NONE', *, *, #220915, .T. ) ;
#157805 = FACE_OUTER_BOUND ( 'NONE', #4522, .T. ) ;
#157806 = LINE ( 'NONE', #179907, #117583 ) ;
#157807 = CYLINDRICAL_SURFACE ( 'NONE', #90463, 0.09999999999998898659 ) ;
#157808 = DIRECTION ( 'NONE',  ( 0.000000000000000000, 0.000000000000000000, -1.000000000000000000 ) ) ;
#157809 = EDGE_CURVE ( 'NONE', #15834, #16895, #72830, .T. ) ;
#157810 = CARTESIAN_POINT ( 'NONE',  ( 11.60000000000000320, -9.650000000000002132, 17.60000000000000497 ) ) ;
#157812 = DIRECTION ( 'NONE',  ( 1.000000000000000000, 0.000000000000000000, 0.000000000000000000 ) ) ;
#157811 = DIRECTION ( 'NONE',  ( 0.000000000000000000, 1.000000000000000000, 0.000000000000000000 ) ) ;
#157813 = CIRCLE ( 'NONE', #253425, 11.75000000000000178 ) ;
#157814 = DIRECTION ( 'NONE',  ( -1.000000000000000000, 0.000000000000000000, 0.000000000000000000 ) ) ;
#157815 = ADVANCED_FACE ( 'NONE', ( #190883 ), #248259, .T. ) ;
#157816 = DIRECTION ( 'NONE',  ( 0.7071067811865487940, -0.7071067811865462405, -4.216150419019403701E-15 ) ) ;
#157817 = CARTESIAN_POINT ( 'NONE',  ( 22.60000000000000142, 11.74956712350054744, -100.3991416309013260 ) ) ;
#157818 = CIRCLE ( 'NONE', #78636, 0.1000000000000028644 ) ;
#157819 = DIRECTION ( 'NONE',  ( 1.000000000000000000, 1.794895427898103559E-16, 3.909090864890002444E-17 ) ) ;
#157820 = ORIENTED_EDGE ( 'NONE', *, *, #95333, .T. ) ;
#157821 = EDGE_LOOP ( 'NONE', ( #40158, #52747, #79740, #257048 ) ) ;
#157822 = DIRECTION ( 'NONE',  ( 0.000000000000000000, 6.982962677686266711E-15, -1.000000000000000000 ) ) ;
#157824 = DIRECTION ( 'NONE',  ( 1.000000000000000000, 0.000000000000000000, 0.000000000000000000 ) ) ;
#157823 = CARTESIAN_POINT ( 'NONE',  ( 21.14999999999999858, 69.45934304831041572, -69.52310748452435973 ) ) ;
#157825 = EDGE_CURVE ( 'NONE', #121353, #177802, #176864, .T. ) ;
#157826 = AXIS2_PLACEMENT_3D ( 'NONE', #234022, #37136, #237879 ) ;
#157827 = EDGE_CURVE ( 'NONE', #113878, #242523, #101796, .T. ) ;
#157828 = CARTESIAN_POINT ( 'NONE',  ( -21.55000000000000426, 7.708578643773852157, -88.25000000000005684 ) ) ;
#157829 = FACE_OUTER_BOUND ( 'NONE', #152256, .T. ) ;
#157830 = DIRECTION ( 'NONE',  ( 1.000000000000000000, 0.000000000000000000, -0.000000000000000000 ) ) ;
#157831 = EDGE_LOOP ( 'NONE', ( #217396, #142701, #140132, #155081 ) ) ;
#157832 = ORIENTED_EDGE ( 'NONE', *, *, #214888, .F. ) ;
#157833 = AXIS2_PLACEMENT_3D ( 'NONE', #138389, #19776, #142267 ) ;
#157835 = VECTOR ( 'NONE', #211061, 1000.000000000000114 ) ;
#157834 = CARTESIAN_POINT ( 'NONE',  ( -20.07928932188135107, 9.220710678118654968, -21.15000000000000213 ) ) ;
#157836 = ORIENTED_EDGE ( 'NONE', *, *, #83625, .F. ) ;
#157837 = DIRECTION ( 'NONE',  ( 0.000000000000000000, 0.000000000000000000, -1.000000000000000000 ) ) ;
#157839 = EDGE_CURVE ( 'NONE', #205114, #135372, #56017, .T. ) ;
#157838 = VECTOR ( 'NONE', #191033, 1000.000000000000000 ) ;
#157840 = EDGE_CURVE ( 'NONE', #56045, #143848, #114889, .T. ) ;
#157841 = CARTESIAN_POINT ( 'NONE',  ( -18.59999999999999787, 4.288595810029049993, -211.9930862808554934 ) ) ;
#157842 = ORIENTED_EDGE ( 'NONE', *, *, #90946, .T. ) ;
#157843 = CARTESIAN_POINT ( 'NONE',  ( 21.14999999999999858, 69.45000000001205365, -124.3731074845243540 ) ) ;
#157844 = ORIENTED_EDGE ( 'NONE', *, *, #183233, .T. ) ;
#157845 = PLANE ( 'NONE',  #232839 ) ;
#157846 = CARTESIAN_POINT ( 'NONE',  ( 21.05000000000000071, 56.16603649944111254, -228.1013850343386480 ) ) ;
#157847 = FACE_OUTER_BOUND ( 'NONE', #97057, .T. ) ;
#157848 = CARTESIAN_POINT ( 'NONE',  ( 21.17356465864818915, 75.90108875899831276, -142.9459106107659920 ) ) ;
#157849 = CARTESIAN_POINT ( 'NONE',  ( 21.05000000000000071, 65.63508776066827011, -242.0675804128435971 ) ) ;
#157850 = EDGE_CURVE ( 'NONE', #8256, #62695, #53911, .T. ) ;
#157852 = FACE_OUTER_BOUND ( 'NONE', #113972, .T. ) ;
#157851 = CARTESIAN_POINT ( 'NONE',  ( -20.85000000000000142, 68.97833521811179480, -99.18954208262705663 ) ) ;
#157853 = CARTESIAN_POINT ( 'NONE',  ( 18.39999999999997371, 64.52683809664972614, -145.7731074845244450 ) ) ;
#157855 = ORIENTED_EDGE ( 'NONE', *, *, #251674, .F. ) ;
#157854 = EDGE_CURVE ( 'NONE', #72182, #72309, #29253, .T. ) ;
#157857 = DIRECTION ( 'NONE',  ( 0.000000000000000000, 0.000000000000000000, 1.000000000000000000 ) ) ;
#157856 = FACE_OUTER_BOUND ( 'NONE', #136814, .T. ) ;
#157859 = VERTEX_POINT ( 'NONE', #31811 ) ;
#157858 = AXIS2_PLACEMENT_3D ( 'NONE', #252849, #149931, #14274 ) ;
#157861 = ORIENTED_EDGE ( 'NONE', *, *, #133464, .F. ) ;
#157860 = DIRECTION ( 'NONE',  ( 1.186688945009009831E-16, -0.4721928772777346239, -0.8814952561688430555 ) ) ;
#157862 = AXIS2_PLACEMENT_3D ( 'NONE', #14465, #109671, #191826 ) ;
#157863 = ORIENTED_EDGE ( 'NONE', *, *, #130128, .T. ) ;
#157864 = DIRECTION ( 'NONE',  ( 0.000000000000000000, -0.4721928772777346239, -0.8814952561688430555 ) ) ;
#157865 = CARTESIAN_POINT ( 'NONE',  ( -22.00411653889210939, 0.09903810579712249429, -26.24655713235958032 ) ) ;
#157866 = CARTESIAN_POINT ( 'NONE',  ( 23.14999999999999503, 64.25000000001205080, -124.3731074845243825 ) ) ;
#157867 = CARTESIAN_POINT ( 'NONE',  ( -20.54999999999999716, -8.663551401858001100, -157.9758988819327215 ) ) ;
#157868 = EDGE_LOOP ( 'NONE', ( #140907, #171959, #73758, #207966 ) ) ;
#157869 = CARTESIAN_POINT ( 'NONE',  ( -18.59999999999999787, 66.65000000001229807, -157.8731074845244393 ) ) ;
#157870 = DIRECTION ( 'NONE',  ( 1.000000000000000000, 0.000000000000000000, 0.000000000000000000 ) ) ;
#157871 = AXIS2_PLACEMENT_3D ( 'NONE', #194871, #134846, #100835 ) ;
#157872 = DIRECTION ( 'NONE',  ( 0.000000000000000000, -6.982962677686266711E-15, 1.000000000000000000 ) ) ;
#157873 = EDGE_CURVE ( 'NONE', #2966, #26113, #110380, .T. ) ;
#157874 = ORIENTED_EDGE ( 'NONE', *, *, #64441, .F. ) ;
#157875 = ADVANCED_FACE ( 'NONE', ( #72206 ), #231281, .F. ) ;
#157876 = CARTESIAN_POINT ( 'NONE',  ( -18.50000000000000000, 46.33035574435032800, -243.0552603638195137 ) ) ;
#157877 = DIRECTION ( 'NONE',  ( -2.827886303505248766E-16, -0.8660254037844377084, -0.5000000000000015543 ) ) ;
#157878 = EDGE_CURVE ( 'NONE', #22668, #202617, #192157, .T. ) ;
#157879 = VECTOR ( 'NONE', #146641, 1000.000000000000000 ) ;
#157880 = VERTEX_POINT ( 'NONE', #93033 ) ;
#157881 = ORIENTED_EDGE ( 'NONE', *, *, #203329, .F. ) ;
#157882 = CIRCLE ( 'NONE', #178523, 11.75000000000001066 ) ;
#157883 = CARTESIAN_POINT ( 'NONE',  ( 20.90000000000000213, 1.212568896937007645, -7.900000000000000355 ) ) ;
#157884 = CIRCLE ( 'NONE', #203795, 0.09999999999999892308 ) ;
#157885 = ORIENTED_EDGE ( 'NONE', *, *, #24211, .T. ) ;
#157886 = DIRECTION ( 'NONE',  ( -1.000000000000000000, -2.885090398161910739E-16, -6.283419270304611573E-17 ) ) ;
#157888 = VERTEX_POINT ( 'NONE', #133445 ) ;
#157887 = CIRCLE ( 'NONE', #182972, 0.09999999999998898659 ) ;
#157889 = CARTESIAN_POINT ( 'NONE',  ( 20.94999027547553894, 10.29326151435327219, -172.9592822510415147 ) ) ;
#157890 = CARTESIAN_POINT ( 'NONE',  ( -20.64999999999999858, 54.18213181965657554, -236.9344197582443883 ) ) ;
#157891 = CARTESIAN_POINT ( 'NONE',  ( 22.39999999999999503, 68.20922040163929978, -203.5231074845243882 ) ) ;
#157892 = EDGE_CURVE ( 'NONE', #145138, #93015, #114673, .T. ) ;
#157893 = CARTESIAN_POINT ( 'NONE',  ( -23.25000000000000000, 11.75000000001115552, -33.50000000000000000 ) ) ;
#157894 = AXIS2_PLACEMENT_3D ( 'NONE', #30377, #109880, #189443 ) ;
#157895 = CIRCLE ( 'NONE', #74500, 11.80000000000000426 ) ;
#157896 = ADVANCED_FACE ( 'NONE', ( #129597 ), #208707, .F. ) ;
#157897 = DIRECTION ( 'NONE',  ( 0.000000000000000000, -1.000000000000000000, 0.000000000000000000 ) ) ;
#157898 = AXIS2_PLACEMENT_3D ( 'NONE', #256525, #76658, #113223 ) ;
#157899 = CARTESIAN_POINT ( 'NONE',  ( -21.08621493067320429, 0.05619483948720500194, -27.15070570882805967 ) ) ;
#157900 = DIRECTION ( 'NONE',  ( 0.000000000000000000, 6.982962677686267499E-15, -1.000000000000000000 ) ) ;
#157901 = ORIENTED_EDGE ( 'NONE', *, *, #94922, .T. ) ;
#157903 = DIRECTION ( 'NONE',  ( 1.000000000000000000, 0.000000000000000000, 0.000000000000000000 ) ) ;
#157902 = LINE ( 'NONE', #177447, #103953 ) ;
#157904 = ORIENTED_EDGE ( 'NONE', *, *, #69746, .F. ) ;
#157907 = ORIENTED_EDGE ( 'NONE', *, *, #56331, .F. ) ;
#157906 = CARTESIAN_POINT ( 'NONE',  ( 18.59999999999999076, 64.35000000001170406, -69.52310748452438816 ) ) ;
#157905 = LINE ( 'NONE', #24796, #40648 ) ;
#157908 = CIRCLE ( 'NONE', #107966, 0.09999999999999939493 ) ;
#157909 = ORIENTED_EDGE ( 'NONE', *, *, #218752, .F. ) ;
#157910 = DIRECTION ( 'NONE',  ( 1.000000000000000000, -0.000000000000000000, 0.000000000000000000 ) ) ;
#157911 = AXIS2_PLACEMENT_3D ( 'NONE', #125069, #25971, #222864 ) ;
#157912 = VECTOR ( 'NONE', #93835, 1000.000000000000000 ) ;
#157913 = FACE_OUTER_BOUND ( 'NONE', #202129, .T. ) ;
#157914 = TOROIDAL_SURFACE ( 'NONE', #70409, 0.6000000000000015321, 0.1000000000000000056 ) ;
#157915 = DIRECTION ( 'NONE',  ( -1.000000000000000000, -2.952720810173289112E-16, 0.000000000000000000 ) ) ;
#157916 = EDGE_LOOP ( 'NONE', ( #191544, #242475, #211065, #45709, #217502 ) ) ;
#157917 = CARTESIAN_POINT ( 'NONE',  ( 19.86930884467578196, 16.68375915355484196, -222.6855985437128140 ) ) ;
#157918 = VECTOR ( 'NONE', #87701, 1000.000000000000000 ) ;
#157919 = CARTESIAN_POINT ( 'NONE',  ( 23.24999999999999645, 76.00000000001170974, -69.52310748452431710 ) ) ;
#157921 = DIRECTION ( 'NONE',  ( 0.000000000000000000, 0.000000000000000000, -1.000000000000000000 ) ) ;
#157920 = LINE ( 'NONE', #118759, #13733 ) ;
#157923 = ORIENTED_EDGE ( 'NONE', *, *, #177190, .T. ) ;
#157922 = CARTESIAN_POINT ( 'NONE',  ( -16.94445028196807002, 9.992063609708893068, -54.39266982158155628 ) ) ;
#157924 = PRODUCT_DEFINITION_SHAPE ( 'NONE', 'NONE',  #258118 ) ;
#157925 = ORIENTED_EDGE ( 'NONE', *, *, #42292, .F. ) ;
#157926 = VECTOR ( 'NONE', #249813, 1000.000000000000000 ) ;
#157927 = CARTESIAN_POINT ( 'NONE',  ( -21.64999999999999858, 7.249999999999992895, -21.15000000000000213 ) ) ;
#157928 = ORIENTED_EDGE ( 'NONE', *, *, #225668, .F. ) ;
#157929 = CARTESIAN_POINT ( 'NONE',  ( 21.05000000000000071, 85.00000000001149658, -45.41707660717670336 ) ) ;
#157930 = ORIENTED_EDGE ( 'NONE', *, *, #188627, .F. ) ;
#157931 = CARTESIAN_POINT ( 'NONE',  ( 20.94999999999999574, 76.00000000001165290, -69.52310748452431710 ) ) ;
#157932 = LINE ( 'NONE', #122632, #32787 ) ;
#157933 = FACE_OUTER_BOUND ( 'NONE', #121275, .T. ) ;
#157934 = VERTEX_POINT ( 'NONE', #84844 ) ;
#157935 = CARTESIAN_POINT ( 'NONE',  ( -18.59999999999999787, 61.43991280424057777, -221.4883200034892923 ) ) ;
#157936 = AXIS2_PLACEMENT_3D ( 'NONE', #247529, #126283, #110577 ) ;
#157937 = CIRCLE ( 'NONE', #112119, 0.1000000000000000472 ) ;
#157938 = EDGE_CURVE ( 'NONE', #55661, #230402, #86135, .T. ) ;
#157939 = VECTOR ( 'NONE', #15408, 1000.000000000000000 ) ;
#157940 = DIRECTION ( 'NONE',  ( 0.000000000000000000, 1.000000000000000000, 0.000000000000000000 ) ) ;
#157941 = VECTOR ( 'NONE', #501, 1000.000000000000000 ) ;
#157942 = VERTEX_POINT ( 'NONE', #247812 ) ;
#157943 = ORIENTED_EDGE ( 'NONE', *, *, #135744, .T. ) ;
#157944 = VERTEX_POINT ( 'NONE', #83565 ) ;
#157945 = CARTESIAN_POINT ( 'NONE',  ( 20.94999999999999574, 74.16465844978765176, -124.9679561919613207 ) ) ;
#157947 = ADVANCED_FACE ( 'NONE', ( #203550 ), #243952, .T. ) ;
#157946 = ORIENTED_EDGE ( 'NONE', *, *, #15655, .F. ) ;
#157949 = ORIENTED_EDGE ( 'NONE', *, *, #246065, .T. ) ;
#157948 = DIRECTION ( 'NONE',  ( 0.000000000000000000, -0.8660254037844468122, -0.4999999999999859557 ) ) ;
#157950 = ORIENTED_EDGE ( 'NONE', *, *, #34479, .T. ) ;
#157951 = EDGE_CURVE ( 'NONE', #130077, #234784, #28816, .T. ) ;
#157953 = EDGE_CURVE ( 'NONE', #180782, #107411, #246519, .T. ) ;
#157952 = CIRCLE ( 'NONE', #253741, 12.77499999999999858 ) ;
#157956 = EDGE_LOOP ( 'NONE', ( #102346, #75354, #141356, #158204 ) ) ;
#157955 = ORIENTED_EDGE ( 'NONE', *, *, #227642, .F. ) ;
#157954 = CARTESIAN_POINT ( 'NONE',  ( -23.15000000000000213, 76.00000000001173817, -73.52310748452431710 ) ) ;
#157957 = CIRCLE ( 'NONE', #37301, 0.09999999999999993616 ) ;
#157958 = ORIENTED_EDGE ( 'NONE', *, *, #158656, .F. ) ;
#157959 = FACE_OUTER_BOUND ( 'NONE', #37193, .T. ) ;
#157960 = AXIS2_PLACEMENT_3D ( 'NONE', #200623, #46331, #220188 ) ;
#157961 = CARTESIAN_POINT ( 'NONE',  ( -20.64999999999999858, 67.23127455305835554, -235.8551265064784559 ) ) ;
#157962 = CARTESIAN_POINT ( 'NONE',  ( -20.54999999999999716, 36.65892442174935439, -249.5511627012433848 ) ) ;
#157963 = VERTEX_POINT ( 'NONE', #167028 ) ;
#157964 = EDGE_CURVE ( 'NONE', #227218, #223792, #56202, .T. ) ;
#157965 = CARTESIAN_POINT ( 'NONE',  ( -20.07928932188135107, 61.56469444049141515, -221.5221618711549354 ) ) ;
#157967 = ORIENTED_EDGE ( 'NONE', *, *, #51546, .T. ) ;
#157966 = CARTESIAN_POINT ( 'NONE',  ( -21.65000000000000213, 14.13772148853350430, -219.1573629999798811 ) ) ;
#157968 = DIRECTION ( 'NONE',  ( 0.000000000000000000, 0.9736512643735623085, 0.2280421351061316382 ) ) ;
#157970 = ORIENTED_EDGE ( 'NONE', *, *, #162882, .F. ) ;
#157969 = CARTESIAN_POINT ( 'NONE',  ( 23.24999999999999645, 70.35000000001261355, -190.8731074845244109 ) ) ;
#157971 = ORIENTED_EDGE ( 'NONE', *, *, #27012, .T. ) ;
#157972 = DIRECTION ( 'NONE',  ( 2.952720810173289112E-16, -1.000000000000000000, 0.000000000000000000 ) ) ;
#157973 = CARTESIAN_POINT ( 'NONE',  ( 18.52130828395273099, 85.48139550263771014, -95.99860076064064174 ) ) ;
#157974 = ORIENTED_EDGE ( 'NONE', *, *, #188015, .T. ) ;
#157975 = VERTEX_POINT ( 'NONE', #165730 ) ;
#157976 = TOROIDAL_SURFACE ( 'NONE', #91306, 11.65000000000000036, 0.1000000000000000056 ) ;
#157977 = CARTESIAN_POINT ( 'NONE',  ( -20.85000000000000142, 87.65000000001143121, -36.02310748452423894 ) ) ;
#157978 = CARTESIAN_POINT ( 'NONE',  ( 20.93284271247462414, 64.25000000001249134, -177.0379132551784380 ) ) ;
#157980 = ORIENTED_EDGE ( 'NONE', *, *, #189391, .T. ) ;
#157979 = ORIENTED_EDGE ( 'NONE', *, *, #200952, .T. ) ;
#157981 = ORIENTED_EDGE ( 'NONE', *, *, #179806, .F. ) ;
#157982 = CARTESIAN_POINT ( 'NONE',  ( 21.11747605621531321, 61.96368823759529221, -221.7396181602011040 ) ) ;
#157984 = EDGE_LOOP ( 'NONE', ( #174955, #62088, #140918 ) ) ;
#157983 = EDGE_CURVE ( 'NONE', #244695, #82729, #107000, .T. ) ;
#157985 = VERTEX_POINT ( 'NONE', #30078 ) ;
#157986 = DIRECTION ( 'NONE',  ( 0.000000000000000000, 1.000000000000000000, 6.982962677686266711E-15 ) ) ;
#157987 = ORIENTED_EDGE ( 'NONE', *, *, #188462, .T. ) ;
#157988 = LINE ( 'NONE', #75839, #31542 ) ;
#157990 = CARTESIAN_POINT ( 'NONE',  ( -23.25000000000000000, 76.00000000001142553, -36.02310748452432421 ) ) ;
#157989 = PLANE ( 'NONE',  #198808 ) ;
#157991 = ORIENTED_EDGE ( 'NONE', *, *, #109456, .T. ) ;
#157994 = EDGE_CURVE ( 'NONE', #155156, #161523, #252038, .T. ) ;
#157993 = EDGE_LOOP ( 'NONE', ( #7609, #184600, #117824, #241300 ) ) ;
#157992 = ORIENTED_EDGE ( 'NONE', *, *, #171223, .F. ) ;
#157996 = CIRCLE ( 'NONE', #45521, 0.09999999999999939493 ) ;
#157995 = CARTESIAN_POINT ( 'NONE',  ( -20.94999999999999929, -11.41227409414968541, -30.59999999999999432 ) ) ;
#157997 = DIRECTION ( 'NONE',  ( 0.000000000000000000, 0.000000000000000000, -1.000000000000000000 ) ) ;
#157998 = CIRCLE ( 'NONE', #212125, 0.09999999999999939493 ) ;
#157999 = AXIS2_PLACEMENT_3D ( 'NONE', #42623, #197840, #99998 ) ;
#158000 = AXIS2_PLACEMENT_3D ( 'NONE', #184581, #86749, #248417 ) ;
#158001 = ORIENTED_EDGE ( 'NONE', *, *, #1875, .T. ) ;
#158002 = VECTOR ( 'NONE', #61514, 1000.000000000000000 ) ;
#158003 = CARTESIAN_POINT ( 'NONE',  ( -23.25000000000000000, 76.00000000001142553, -36.02310748452432421 ) ) ;
#158004 = VERTEX_POINT ( 'NONE', #64037 ) ;
#158005 = VERTEX_POINT ( 'NONE', #5314 ) ;
#158006 = ORIENTED_EDGE ( 'NONE', *, *, #127372, .F. ) ;
#158007 = SPHERICAL_SURFACE ( 'NONE', #159632, 0.1000000000000000056 ) ;
#158008 = CARTESIAN_POINT ( 'NONE',  ( -20.94999999999999929, 87.41227409416185878, -139.4231074845242802 ) ) ;
#158009 = VERTEX_POINT ( 'NONE', #143573 ) ;
#158010 = CYLINDRICAL_SURFACE ( 'NONE', #114796, 0.09999999999999867328 ) ;
#158011 = CYLINDRICAL_SURFACE ( 'NONE', #53709, 7.900000000000003908 ) ;
#158013 = CARTESIAN_POINT ( 'NONE',  ( -16.87683809663752399, 9.950000000011137047, -120.5976359818037196 ) ) ;
#158012 = DIRECTION ( 'NONE',  ( -1.000000000000000000, 0.000000000000000000, 0.000000000000000000 ) ) ;
#158014 = CARTESIAN_POINT ( 'NONE',  ( -18.59999999999999787, 77.16270174995064224, -195.4231074845243370 ) ) ;
#158015 = EDGE_CURVE ( 'NONE', #82517, #237924, #77064, .T. ) ;
#158017 = CYLINDRICAL_SURFACE ( 'NONE', #8034, 0.09999999999999939493 ) ;
#158016 = VECTOR ( 'NONE', #45346, 1000.000000000000000 ) ;
#158019 = CARTESIAN_POINT ( 'NONE',  ( 21.08750232978087524, 65.27513661400213607, -157.7942493115248510 ) ) ;
#158018 = CIRCLE ( 'NONE', #45543, 0.09999999999999939493 ) ;
#158020 = CARTESIAN_POINT ( 'NONE',  ( -23.24999999999999645, 85.60000000001137721, -29.42291809330221142 ) ) ;
#158021 = CIRCLE ( 'NONE', #37188, 0.09999999999999967248 ) ;
#158022 = CARTESIAN_POINT ( 'NONE',  ( 22.46250603428203618, 75.97885582387343106, -148.1729705818643765 ) ) ;
#158023 = CARTESIAN_POINT ( 'NONE',  ( -22.19999999999999929, -11.65000000000000036, 6.100000000000001421 ) ) ;
#158024 = ORIENTED_EDGE ( 'NONE', *, *, #218446, .F. ) ;
#158025 = AXIS2_PLACEMENT_3D ( 'NONE', #49902, #166031, #47316 ) ;
#158026 = EDGE_CURVE ( 'NONE', #21107, #50892, #93815, .T. ) ;
#158028 = ORIENTED_EDGE ( 'NONE', *, *, #115614, .T. ) ;
#158027 = ORIENTED_EDGE ( 'NONE', *, *, #18943, .F. ) ;
#158029 = VERTEX_POINT ( 'NONE', #127872 ) ;
#158031 = ORIENTED_EDGE ( 'NONE', *, *, #87441, .T. ) ;
#158030 = EDGE_CURVE ( 'NONE', #179549, #182938, #207238, .T. ) ;
#158032 = DIRECTION ( 'NONE',  ( 0.000000000000000000, 0.2617529984165033463, 0.9651348961777156399 ) ) ;
#158033 = DIRECTION ( 'NONE',  ( 0.000000000000000000, -0.2617529984165032908, -0.9651348961777156399 ) ) ;
#158034 = EDGE_CURVE ( 'NONE', #60346, #120003, #156213, .T. ) ;
#158035 = EDGE_CURVE ( 'NONE', #255434, #32289, #247761, .T. ) ;
#158037 = DIRECTION ( 'NONE',  ( 0.000000000000000000, 0.008583690987128059571, -0.9999631594459056361 ) ) ;
#158036 = DIRECTION ( 'NONE',  ( -1.000000000000000000, 0.000000000000000000, -0.000000000000000000 ) ) ;
#158038 = ORIENTED_EDGE ( 'NONE', *, *, #98384, .T. ) ;
#158039 = CARTESIAN_POINT ( 'NONE',  ( -21.05000000000000071, -1.236118717437885595, -194.8647072476926496 ) ) ;
#158040 = DIRECTION ( 'NONE',  ( -1.000000000000000000, 0.000000000000000000, 0.000000000000000000 ) ) ;
#158041 = SPHERICAL_SURFACE ( 'NONE', #13994, 0.1000000000000000056 ) ;
#158042 = EDGE_CURVE ( 'NONE', #159239, #49118, #143706, .T. ) ;
#158043 = CARTESIAN_POINT ( 'NONE',  ( -20.54999999999999716, 82.48249193998721296, -215.5326005316167084 ) ) ;
#158044 = ORIENTED_EDGE ( 'NONE', *, *, #234358, .F. ) ;
#158045 = VECTOR ( 'NONE', #221594, 1000.000000000000227 ) ;
#158046 = EDGE_CURVE ( 'NONE', #177021, #174631, #222806, .T. ) ;
#158048 = EDGE_CURVE ( 'NONE', #239085, #27168, #43752, .T. ) ;
#158047 = ADVANCED_FACE ( 'NONE', ( #70497 ), #251662, .F. ) ;
#158049 = CARTESIAN_POINT ( 'NONE',  ( -20.94999999999999929, 67.23127455305835554, -235.8551265064784559 ) ) ;
#158050 = ORIENTED_EDGE ( 'NONE', *, *, #3507, .F. ) ;
#158051 = CARTESIAN_POINT ( 'NONE',  ( -23.25000000000000000, 67.23127455305841238, -235.8551265064783991 ) ) ;
#158052 = VECTOR ( 'NONE', #189422, 1000.000000000000000 ) ;
#158053 = LINE ( 'NONE', #253238, #11244 ) ;
#158054 = DIRECTION ( 'NONE',  ( 0.000000000000000000, 0.000000000000000000, -1.000000000000000000 ) ) ;
#158055 = DIRECTION ( 'NONE',  ( 1.000000000000000000, 0.000000000000000000, 0.000000000000000000 ) ) ;
#158056 = DIRECTION ( 'NONE',  ( 0.000000000000000000, 0.000000000000000000, -1.000000000000000000 ) ) ;
#158057 = ORIENTED_EDGE ( 'NONE', *, *, #113555, .F. ) ;
#158058 = PLANE ( 'NONE',  #177809 ) ;
#158059 = PLANE ( 'NONE',  #199974 ) ;
#158060 = CYLINDRICAL_SURFACE ( 'NONE', #249985, 0.09999999999999609201 ) ;
#158061 = ADVANCED_FACE ( 'NONE', ( #150020 ), #131716, .T. ) ;
#158063 = CARTESIAN_POINT ( 'NONE',  ( 21.05000000000000071, 76.00000000001190870, -103.0231074845243029 ) ) ;
#158062 = DIRECTION ( 'NONE',  ( 1.000000000000000000, 0.000000000000000000, 0.000000000000000000 ) ) ;
#158064 = DIRECTION ( 'NONE',  ( -1.000000000000000000, 0.000000000000000000, 0.000000000000000000 ) ) ;
#158065 = DIRECTION ( 'NONE',  ( 1.000000000000000000, 0.000000000000000000, 0.000000000000000000 ) ) ;
#158066 = CIRCLE ( 'NONE', #228756, 0.5000000000000004441 ) ;
#158067 = FACE_OUTER_BOUND ( 'NONE', #53179, .T. ) ;
#158068 = CARTESIAN_POINT ( 'NONE',  ( 18.49505816908824229, -9.437872553199969872, -207.7776572016708769 ) ) ;
#158069 = EDGE_CURVE ( 'NONE', #104851, #37861, #39687, .T. ) ;
#158070 = ADVANCED_FACE ( 'NONE', ( #134261 ), #31373, .F. ) ;
#158071 = VECTOR ( 'NONE', #120286, 1000.000000000000000 ) ;
#158072 = ORIENTED_EDGE ( 'NONE', *, *, #16144, .F. ) ;
#158073 = AXIS2_PLACEMENT_3D ( 'NONE', #48427, #5428, #206230 ) ;
#158074 = ORIENTED_EDGE ( 'NONE', *, *, #117105, .F. ) ;
#158075 = ADVANCED_FACE ( 'NONE', ( #215103 ), #249116, .F. ) ;
#158076 = DIRECTION ( 'NONE',  ( -0.5932847527679298016, 0.8049926720990051576, 0.000000000000000000 ) ) ;
#158077 = EDGE_LOOP ( 'NONE', ( #4812, #140868, #165846, #206961 ) ) ;
#158078 = CARTESIAN_POINT ( 'NONE',  ( -23.25000000000000000, 77.25000000001239187, -162.2226267301092548 ) ) ;
#158079 = EDGE_CURVE ( 'NONE', #243985, #34352, #206260, .T. ) ;
#158080 = CIRCLE ( 'NONE', #128998, 0.09999999999999939493 ) ;
#158081 = AXIS2_PLACEMENT_3D ( 'NONE', #222538, #123464, #13785 ) ;
#158082 = CARTESIAN_POINT ( 'NONE',  ( -20.64999999999999858, -8.999999999988844479, -57.10603087734755690 ) ) ;
#158083 = ORIENTED_EDGE ( 'NONE', *, *, #111407, .F. ) ;
#158084 = DIRECTION ( 'NONE',  ( 0.000000000000000000, -6.982962677686266711E-15, 1.000000000000000000 ) ) ;
#158085 = VECTOR ( 'NONE', #50319, 1000.000000000000000 ) ;
#158086 = AXIS2_PLACEMENT_3D ( 'NONE', #18793, #98298, #17508 ) ;
#158087 = CARTESIAN_POINT ( 'NONE',  ( -15.75000000000000355, 9.350000000011139178, -50.36426760761608534 ) ) ;
#158088 = CARTESIAN_POINT ( 'NONE',  ( -18.50000972452446035, 65.70673848566977426, -97.56382523348287350 ) ) ;
#158089 = AXIS2_PLACEMENT_3D ( 'NONE', #122375, #201906, #182354 ) ;
#158090 = CARTESIAN_POINT ( 'NONE',  ( 23.40000000000005542, 76.00000000001119815, -3.123107484524795474 ) ) ;
#158092 = VERTEX_POINT ( 'NONE', #91314 ) ;
#158091 = CARTESIAN_POINT ( 'NONE',  ( -16.88705144915408596, 9.950000000011078427, -188.0690214052869749 ) ) ;
#158094 = SPHERICAL_SURFACE ( 'NONE', #71217, 0.1000000000000000056 ) ;
#158093 = DIRECTION ( 'NONE',  ( 0.000000000000000000, -0.9876197685951252359, -0.1568667991644863424 ) ) ;
#158095 = CIRCLE ( 'NONE', #53809, 0.8750000000000007772 ) ;
#158096 = DIRECTION ( 'NONE',  ( 1.000000000000000000, 0.000000000000000000, 0.000000000000000000 ) ) ;
#158097 = PLANE ( 'NONE',  #18975 ) ;
#158098 = DIRECTION ( 'NONE',  ( 0.000000000000000000, 0.000000000000000000, 1.000000000000000000 ) ) ;
#158099 = ORIENTED_EDGE ( 'NONE', *, *, #24217, .F. ) ;
#158100 = DIRECTION ( 'NONE',  ( 0.000000000000000000, 0.000000000000000000, 1.000000000000000000 ) ) ;
#158101 = DIRECTION ( 'NONE',  ( 1.000000000000000000, 0.000000000000000000, 0.000000000000000000 ) ) ;
#158102 = VERTEX_POINT ( 'NONE', #110867 ) ;
#158103 = CARTESIAN_POINT ( 'NONE',  ( -16.89208623190940273, 66.04842205103706476, -182.6678352813061394 ) ) ;
#158105 = EDGE_LOOP ( 'NONE', ( #64444, #124249, #43739, #75700 ) ) ;
#158104 = CIRCLE ( 'NONE', #187292, 0.09999999999998898659 ) ;
#158106 = CARTESIAN_POINT ( 'NONE',  ( 18.49999999999999289, 55.01984530832636011, -230.0610957569644199 ) ) ;
#158107 = CARTESIAN_POINT ( 'NONE',  ( -20.64999999999999858, 7.150000000011155876, -54.75000000000000000 ) ) ;
#158108 = DIRECTION ( 'NONE',  ( 1.000000000000000000, -0.000000000000000000, 0.000000000000000000 ) ) ;
#158109 = ORIENTED_EDGE ( 'NONE', *, *, #161241, .F. ) ;
#158110 = ORIENTED_EDGE ( 'NONE', *, *, #241800, .F. ) ;
#158111 = CIRCLE ( 'NONE', #257971, 0.09999999999998898659 ) ;
#158112 = DIRECTION ( 'NONE',  ( 0.7071067811865475727, -0.2890913453342130457, 0.6453109281988448354 ) ) ;
#158113 = CARTESIAN_POINT ( 'NONE',  ( -18.50000000000000000, 13.58143519257360232, -219.8925810335774997 ) ) ;
#158114 = ADVANCED_FACE ( 'NONE', ( #233411 ), #141521, .T. ) ;
#158115 = DIRECTION ( 'NONE',  ( 0.000000000000000000, 1.000000000000000000, 0.000000000000000000 ) ) ;
#158116 = CARTESIAN_POINT ( 'NONE',  ( 18.39999999999997371, 64.52683809664929981, -78.77310748452438816 ) ) ;
#158117 = AXIS2_PLACEMENT_3D ( 'NONE', #228997, #90744, #51596 ) ;
#158119 = CARTESIAN_POINT ( 'NONE',  ( 21.13461538461538325, 10.61458296202553697, -12.35000000000000320 ) ) ;
#158118 = CARTESIAN_POINT ( 'NONE',  ( 23.04999999999999716, 52.07980129617636322, -232.9753775883424964 ) ) ;
#158120 = DIRECTION ( 'NONE',  ( 0.000000000000000000, -1.000000000000000000, 0.000000000000000000 ) ) ;
#158121 = EDGE_CURVE ( 'NONE', #9426, #253084, #73305, .T. ) ;
#158122 = LINE ( 'NONE', #237619, #193563 ) ;
#158123 = DIRECTION ( 'NONE',  ( -0.000000000000000000, -0.000000000000000000, -1.000000000000000000 ) ) ;
#158124 = VERTEX_POINT ( 'NONE', #173471 ) ;
#158125 = LINE ( 'NONE', #237622, #31729 ) ;
#158126 = VECTOR ( 'NONE', #151624, 1000.000000000000227 ) ;
#158128 = EDGE_LOOP ( 'NONE', ( #233865, #236477, #235405, #51442 ) ) ;
#158127 = DIRECTION ( 'NONE',  ( 0.000000000000000000, -7.487053152578127080E-15, 1.000000000000000000 ) ) ;
#158129 = FACE_OUTER_BOUND ( 'NONE', #110278, .T. ) ;
#158130 = LINE ( 'NONE', #238909, #57547 ) ;
#158132 = DIRECTION ( 'NONE',  ( 0.000000000000000000, 1.000000000000000000, 0.000000000000000000 ) ) ;
#158131 = CARTESIAN_POINT ( 'NONE',  ( -18.50000000000000000, 1.115600667400684642E-11, -167.5000000000000284 ) ) ;
#158133 = ADVANCED_FACE ( 'NONE', ( #93868 ), #54738, .T. ) ;
#158134 = ADVANCED_FACE ( 'NONE', ( #90010 ), #194286, .F. ) ;
#158135 = VERTEX_POINT ( 'NONE', #160505 ) ;
#158137 = DIRECTION ( 'NONE',  ( -1.000000000000000000, 0.000000000000000000, 0.000000000000000000 ) ) ;
#158136 = CARTESIAN_POINT ( 'NONE',  ( 20.73486653747090003, 7.250000000011182166, -188.3499999999999659 ) ) ;
#158138 = DIRECTION ( 'NONE',  ( 0.000000000000000000, -0.4930308989875313852, -0.8700118002898274971 ) ) ;
#158139 = DIRECTION ( 'NONE',  ( 0.000000000000000000, -0.2128009952263154869, 0.9770955615653412751 ) ) ;
#158140 = CARTESIAN_POINT ( 'NONE',  ( -2.995603634470891112E-16, 87.75000000001229239, -157.7731074845242745 ) ) ;
#158141 = CARTESIAN_POINT ( 'NONE',  ( -18.50000972452446035, 10.29326151435326508, -139.4592822510415431 ) ) ;
#158142 = ORIENTED_EDGE ( 'NONE', *, *, #106482, .F. ) ;
#158143 = CYLINDRICAL_SURFACE ( 'NONE', #43044, 2.000000000000001776 ) ;
#158145 = ORIENTED_EDGE ( 'NONE', *, *, #131124, .T. ) ;
#158144 = AXIS2_PLACEMENT_3D ( 'NONE', #174166, #133704, #253634 ) ;
#158146 = VECTOR ( 'NONE', #158917, 1000.000000000000000 ) ;
#158147 = DIRECTION ( 'NONE',  ( 1.000000000000000000, 0.000000000000000000, 0.000000000000000000 ) ) ;
#158148 = ORIENTED_EDGE ( 'NONE', *, *, #65070, .F. ) ;
#158149 = CYLINDRICAL_SURFACE ( 'NONE', #146860, 0.1000000000000021844 ) ;
#158150 = AXIS2_PLACEMENT_3D ( 'NONE', #158325, #39658, #134844 ) ;
#158151 = ORIENTED_EDGE ( 'NONE', *, *, #7855, .F. ) ;
#158152 = ADVANCED_FACE ( 'NONE', ( #195781 ), #243668, .T. ) ;
#158153 = CARTESIAN_POINT ( 'NONE',  ( -20.54999999999999716, 23.68770167995059595, -252.8127582590406348 ) ) ;
#158154 = EDGE_CURVE ( 'NONE', #125216, #251836, #214429, .T. ) ;
#158155 = CARTESIAN_POINT ( 'NONE',  ( 23.24999999999999645, 8.822561741666397950, -20.84999999999999432 ) ) ;
#158156 = ORIENTED_EDGE ( 'NONE', *, *, #214175, .F. ) ;
#158157 = CARTESIAN_POINT ( 'NONE',  ( -22.50485643085238863, 76.07878633908924826, -114.7729024236967206 ) ) ;
#158158 = DIRECTION ( 'NONE',  ( -1.000000000000000000, -0.000000000000000000, -0.000000000000000000 ) ) ;
#158159 = PLANE ( 'NONE',  #37527 ) ;
#158160 = DIRECTION ( 'NONE',  ( 1.000000000000000000, -0.000000000000000000, 0.000000000000000000 ) ) ;
#158161 = EDGE_CURVE ( 'NONE', #183644, #133216, #2221, .T. ) ;
#158163 = CIRCLE ( 'NONE', #78963, 0.1000000000000000472 ) ;
#158162 = SPHERICAL_SURFACE ( 'NONE', #112248, 0.1000000000000000056 ) ;
#158164 = CARTESIAN_POINT ( 'NONE',  ( 20.99999999999999645, 9.750000000011137757, -121.3500000000000227 ) ) ;
#158166 = ORIENTED_EDGE ( 'NONE', *, *, #15718, .F. ) ;
#158165 = EDGE_CURVE ( 'NONE', #125182, #223936, #181327, .T. ) ;
#158167 = LINE ( 'NONE', #241508, #157461 ) ;
#158169 = ORIENTED_EDGE ( 'NONE', *, *, #25923, .T. ) ;
#158168 = B_SPLINE_CURVE_WITH_KNOTS ( 'NONE', 3,
 ( #193381, #216765, #231223, #52549, #132105, #13448, #172567, #211657 ),
 .UNSPECIFIED., .F., .F.,
 ( 4, 2, 2, 4 ),
 ( 0.000000000000000000, 0.0001094981963948483559, 0.0002189963927896967119, 0.0004379927855793889243 ),
 .UNSPECIFIED. ) ;
#158171 = ORIENTED_EDGE ( 'NONE', *, *, #130826, .F. ) ;
#158170 = DIRECTION ( 'NONE',  ( 0.7071067811865463515, -0.7071067811865487940, 4.930380657631324879E-32 ) ) ;
#158172 = VERTEX_POINT ( 'NONE', #234892 ) ;
#158173 = CARTESIAN_POINT ( 'NONE',  ( -20.54999999999999716, 66.65000000001198543, -115.2731074845243597 ) ) ;
#158174 = CARTESIAN_POINT ( 'NONE',  ( 13.76927104934457446, 66.54401276639984530, -188.5115763176266626 ) ) ;
#158175 = DIRECTION ( 'NONE',  ( 1.000000000000000000, 0.000000000000000000, 0.000000000000000000 ) ) ;
#158176 = CARTESIAN_POINT ( 'NONE',  ( 18.49999999999999289, 43.24695311518262031, -245.0026972281755491 ) ) ;
#158177 = ORIENTED_EDGE ( 'NONE', *, *, #110604, .T. ) ;
#158178 = CARTESIAN_POINT ( 'NONE',  ( -18.79999999999999716, 1.350000000000000089, 21.90000000000000213 ) ) ;
#158179 = FACE_OUTER_BOUND ( 'NONE', #173341, .T. ) ;
#158180 = EDGE_CURVE ( 'NONE', #135829, #216206, #17138, .T. ) ;
#158181 = ORIENTED_EDGE ( 'NONE', *, *, #122451, .T. ) ;
#158183 = ORIENTED_EDGE ( 'NONE', *, *, #70126, .F. ) ;
#158182 = DIRECTION ( 'NONE',  ( 1.000000000000000000, 0.000000000000000000, 0.000000000000000000 ) ) ;
#158184 = EDGE_CURVE ( 'NONE', #231868, #84289, #85401, .T. ) ;
#158185 = FACE_OUTER_BOUND ( 'NONE', #24607, .T. ) ;
#158186 = CIRCLE ( 'NONE', #220501, 7.900000000000003908 ) ;
#158187 = VECTOR ( 'NONE', #106121, 999.9999999999998863 ) ;
#158189 = CIRCLE ( 'NONE', #8116, 0.1000000000000012546 ) ;
#158188 = CARTESIAN_POINT ( 'NONE',  ( -16.84981964351502626, 9.917318234110023667, -79.86960161401955816 ) ) ;
#158190 = VERTEX_POINT ( 'NONE', #61376 ) ;
#158191 = ADVANCED_FACE ( 'NONE', ( #256957 ), #219150, .T. ) ;
#158192 = AXIS2_PLACEMENT_3D ( 'NONE', #144574, #160333, #104161 ) ;
#158193 = DIRECTION ( 'NONE',  ( 1.000000000000000000, -1.836970198721029934E-16, -1.282749433769087582E-30 ) ) ;
#158194 = ORIENTED_EDGE ( 'NONE', *, *, #155403, .T. ) ;
#158195 = DIRECTION ( 'NONE',  ( 0.000000000000000000, 0.8814952561688432775, -0.4721928772777344019 ) ) ;
#158196 = DIRECTION ( 'NONE',  ( 0.000000000000000000, 0.9126074666063768159, 0.4088369013363282178 ) ) ;
#158197 = CARTESIAN_POINT ( 'NONE',  ( 12.68104795156994591, 66.60346600605763001, -51.61716770535109333 ) ) ;
#158198 = EDGE_CURVE ( 'NONE', #109963, #125, #185411, .T. ) ;
#158199 = CARTESIAN_POINT ( 'NONE',  ( 21.05000000000000071, 6.257814610487280937, -167.4022097086911742 ) ) ;
#158200 = AXIS2_PLACEMENT_3D ( 'NONE', #31078, #71473, #176998 ) ;
#158201 = AXIS2_PLACEMENT_3D ( 'NONE', #254357, #82135, #78296 ) ;
#158202 = EDGE_CURVE ( 'NONE', #152240, #235216, #214803, .T. ) ;
#158203 = AXIS2_PLACEMENT_3D ( 'NONE', #123384, #163801, #106356 ) ;
#158204 = ORIENTED_EDGE ( 'NONE', *, *, #189286, .F. ) ;
#158205 = DIRECTION ( 'NONE',  ( 0.000000000000000000, 1.000000000000000000, 6.982962677686266711E-15 ) ) ;
#158206 = ORIENTED_EDGE ( 'NONE', *, *, #97835, .T. ) ;
#158207 = CARTESIAN_POINT ( 'NONE',  ( -20.94999999999999929, -11.64999999998884483, -170.3999999999999773 ) ) ;
#158209 = EDGE_CURVE ( 'NONE', #226147, #1991, #231388, .T. ) ;
#158208 = CARTESIAN_POINT ( 'NONE',  ( -22.45305610364634674, -0.1008583690875579225, -21.75043287651061164 ) ) ;
#158211 = ORIENTED_EDGE ( 'NONE', *, *, #144632, .F. ) ;
#158210 = DIRECTION ( 'NONE',  ( 0.000000000000000000, 0.2617529984165031243, 0.9651348961777157509 ) ) ;
#158212 = FACE_OUTER_BOUND ( 'NONE', #83696, .T. ) ;
#158213 = CARTESIAN_POINT ( 'NONE',  ( 20.94999999999999929, -8.999999999988842703, -91.00603087734759811 ) ) ;
#158214 = DIRECTION ( 'NONE',  ( 1.000000000000000000, 0.000000000000000000, 0.000000000000000000 ) ) ;
#158215 = LINE ( 'NONE', #59029, #208671 ) ;
#158216 = CARTESIAN_POINT ( 'NONE',  ( 16.87683809663750267, 9.950000000011138823, -146.6500000000000341 ) ) ;
#158217 = FACE_OUTER_BOUND ( 'NONE', #33941, .T. ) ;
#158219 = ORIENTED_EDGE ( 'NONE', *, *, #231307, .F. ) ;
#158218 = CARTESIAN_POINT ( 'NONE',  ( 20.94999999999999929, 46.45388641681647357, -243.1520440498138385 ) ) ;
#158220 = VECTOR ( 'NONE', #124787, 1000.000000000000000 ) ;
#158221 = DIRECTION ( 'NONE',  ( 1.000000000000000000, -0.000000000000000000, -0.000000000000000000 ) ) ;
#158222 = ORIENTED_EDGE ( 'NONE', *, *, #163929, .T. ) ;
#158223 = ORIENTED_EDGE ( 'NONE', *, *, #86709, .F. ) ;
#158224 = CIRCLE ( 'NONE', #54118, 11.80000000000000249 ) ;
#158225 = CARTESIAN_POINT ( 'NONE',  ( -2.995603634470884209E-16, -11.75000000000000000, -24.75000000000000000 ) ) ;
#158226 = CARTESIAN_POINT ( 'NONE',  ( -18.42609945526432824, 85.49999971050360159, -196.5237449942749777 ) ) ;
#158227 = AXIS2_PLACEMENT_3D ( 'NONE', #143063, #122242, #182219 ) ;
#158228 = VERTEX_POINT ( 'NONE', #199630 ) ;
#158229 = DIRECTION ( 'NONE',  ( 1.000000000000000000, 0.000000000000000000, -0.000000000000000000 ) ) ;
#158230 = ORIENTED_EDGE ( 'NONE', *, *, #127928, .F. ) ;
#158231 = VECTOR ( 'NONE', #4141, 1000.000000000000000 ) ;
#158233 = ADVANCED_FACE ( 'NONE', ( #157959 ), #156664, .T. ) ;
#158232 = CARTESIAN_POINT ( 'NONE',  ( 18.49999999999999289, 11.65000000001115588, -100.5000000000000426 ) ) ;
#158234 = TOROIDAL_SURFACE ( 'NONE', #245687, 0.2000000000000000111, 0.1000000000000000056 ) ;
#158235 = DIRECTION ( 'NONE',  ( 0.000000000000000000, -7.429790795770644761E-15, 1.000000000000000000 ) ) ;
#158236 = EDGE_LOOP ( 'NONE', ( #17318, #28702, #96050, #152526 ) ) ;
#158237 = CARTESIAN_POINT ( 'NONE',  ( -17.78241384942737113, 65.14442424719348423, -46.27214515699470354 ) ) ;
#158238 = CIRCLE ( 'NONE', #41700, 0.09999999999999939493 ) ;
#158239 = ORIENTED_EDGE ( 'NONE', *, *, #126456, .F. ) ;
#158240 = DIRECTION ( 'NONE',  ( 0.000000000000000000, 0.2617529984164955192, 0.9651348961777178603 ) ) ;
#158241 = EDGE_CURVE ( 'NONE', #241724, #100962, #173171, .T. ) ;
#158243 = EDGE_LOOP ( 'NONE', ( #214624, #155659, #74635, #98771 ) ) ;
#158242 = CARTESIAN_POINT ( 'NONE',  ( 21.04999999999999361, 6.299230910098046365, -133.9015625000000114 ) ) ;
#158244 = VECTOR ( 'NONE', #202619, 1000.000000000000000 ) ;
#158245 = VECTOR ( 'NONE', #168438, 1000.000000000000000 ) ;
#158246 = LINE ( 'NONE', #100751, #235908 ) ;
#158247 = EDGE_LOOP ( 'NONE', ( #99515, #119399, #173252, #205632 ) ) ;
#158248 = ADVANCED_FACE ( 'NONE', ( #255676 ), #10629, .T. ) ;
#158249 = DIRECTION ( 'NONE',  ( 0.000000000000000000, 0.000000000000000000, 1.000000000000000000 ) ) ;
#158250 = ADVANCED_FACE ( 'NONE', ( #99193 ), #37988, .T. ) ;
#158251 = ORIENTED_EDGE ( 'NONE', *, *, #13130, .T. ) ;
#158253 = EDGE_LOOP ( 'NONE', ( #44697, #164054, #30200, #65444 ) ) ;
#158252 = ORIENTED_EDGE ( 'NONE', *, *, #137583, .F. ) ;
#158254 = DIRECTION ( 'NONE',  ( 1.000000000000000000, 0.000000000000000000, 0.000000000000000000 ) ) ;
#158255 = ORIENTED_EDGE ( 'NONE', *, *, #105533, .T. ) ;
#158256 = CYLINDRICAL_SURFACE ( 'NONE', #119038, 0.09999999999999939493 ) ;
#158257 = ORIENTED_EDGE ( 'NONE', *, *, #46920, .T. ) ;
#158258 = AXIS2_PLACEMENT_3D ( 'NONE', #13691, #93224, #208068 ) ;
#158259 = CIRCLE ( 'NONE', #24969, 0.09999999999998898659 ) ;
#158260 = AXIS2_PLACEMENT_3D ( 'NONE', #40681, #221812, #60188 ) ;
#158261 = AXIS2_PLACEMENT_3D ( 'NONE', #167620, #247119, #230136 ) ;
#158262 = CIRCLE ( 'NONE', #4096, 0.09999999999999939493 ) ;
#158263 = ORIENTED_EDGE ( 'NONE', *, *, #60851, .T. ) ;
#158264 = EDGE_CURVE ( 'NONE', #236861, #129669, #79631, .T. ) ;
#158265 = DIRECTION ( 'NONE',  ( 1.000000000000000000, 0.000000000000000000, 0.000000000000000000 ) ) ;
#158266 = CARTESIAN_POINT ( 'NONE',  ( 22.39999999999999503, 65.09550114356429162, -243.3481044654562879 ) ) ;
#158268 = EDGE_LOOP ( 'NONE', ( #175235, #195000, #188581, #80648 ) ) ;
#158267 = CARTESIAN_POINT ( 'NONE',  ( 18.59999999999999787, 0.000000000000000000, 0.000000000000000000 ) ) ;
#158269 = CARTESIAN_POINT ( 'NONE',  ( 20.12500000000000000, 66.25000000001199396, -115.2731074845243597 ) ) ;
#158270 = EDGE_LOOP ( 'NONE', ( #182369, #209633, #195102, #182322 ) ) ;
#158271 = DIRECTION ( 'NONE',  ( 0.000000000000000000, 0.5868805631290353597, 0.8096735173027127530 ) ) ;
#158272 = FACE_OUTER_BOUND ( 'NONE', #78576, .T. ) ;
#158273 = CARTESIAN_POINT ( 'NONE',  ( -21.05000000000000071, 76.00000000001213607, -136.5231074845242745 ) ) ;
#158274 = ORIENTED_EDGE ( 'NONE', *, *, #180929, .T. ) ;
#158275 = DIRECTION ( 'NONE',  ( -4.408576920032448588E-17, 0.1350103645451876666, -0.9908441862701600211 ) ) ;
#158276 = CARTESIAN_POINT ( 'NONE',  ( -18.46919391072097838, 37.97540340137230430, -261.2271828652933436 ) ) ;
#158277 = DIRECTION ( 'NONE',  ( 0.000000000000000000, -1.000000000000000000, -6.982962677686265922E-15 ) ) ;
#158278 = ORIENTED_EDGE ( 'NONE', *, *, #235289, .F. ) ;
#158279 = CARTESIAN_POINT ( 'NONE',  ( -16.93658623642905070, 66.01961832835475263, -90.41120475539514700 ) ) ;
#158280 = ORIENTED_EDGE ( 'NONE', *, *, #110199, .F. ) ;
#158281 = ORIENTED_EDGE ( 'NONE', *, *, #66062, .F. ) ;
#158282 = PLANE ( 'NONE',  #76397 ) ;
#158283 = ORIENTED_EDGE ( 'NONE', *, *, #112913, .F. ) ;
#158284 = ORIENTED_EDGE ( 'NONE', *, *, #68900, .F. ) ;
#158285 = CARTESIAN_POINT ( 'NONE',  ( -20.00857864376270001, 9.350000000011156942, -45.85000000000000142 ) ) ;
#158286 = ADVANCED_FACE ( 'NONE', ( #20999 ), #1382, .T. ) ;
#158287 = ORIENTED_EDGE ( 'NONE', *, *, #67965, .T. ) ;
#158288 = ADVANCED_FACE ( 'NONE', ( #180049 ), #45666, .T. ) ;
#158289 = ORIENTED_EDGE ( 'NONE', *, *, #36196, .T. ) ;
#158290 = LINE ( 'NONE', #440, #110412 ) ;
#158291 = CARTESIAN_POINT ( 'NONE',  ( 23.24999999999999289, 11.75000000001116263, -88.75000000000004263 ) ) ;
#158292 = TOROIDAL_SURFACE ( 'NONE', #75074, 0.9750000000000019762, 0.1000000000000000056 ) ;
#158293 = ORIENTED_EDGE ( 'NONE', *, *, #83314, .F. ) ;
#158294 = VECTOR ( 'NONE', #33841, 1000.000000000000000 ) ;
#158296 = EDGE_CURVE ( 'NONE', #126073, #248782, #93995, .T. ) ;
#158295 = VERTEX_POINT ( 'NONE', #7833 ) ;
#158297 = ORIENTED_EDGE ( 'NONE', *, *, #223582, .T. ) ;
#158298 = CIRCLE ( 'NONE', #237376, 0.09999999999999939493 ) ;
#158299 = CARTESIAN_POINT ( 'NONE',  ( 21.05000000000047677, 69.55891531154155416, -203.5053880512165279 ) ) ;
#158300 = CARTESIAN_POINT ( 'NONE',  ( -16.80939487329394666, 14.15900158805632891, -219.2550725561372644 ) ) ;
#158301 = DIRECTION ( 'NONE',  ( -1.000000000000000000, 7.304098846218134667E-16, 2.111765289898285610E-31 ) ) ;
#158302 = DIRECTION ( 'NONE',  ( 0.000000000000000000, -1.000000000000000000, 0.000000000000000000 ) ) ;
#158303 = AXIS2_PLACEMENT_3D ( 'NONE', #34336, #95558, #73465 ) ;
#158304 = CARTESIAN_POINT ( 'NONE',  ( 0.8999999999999993561, -8.279289321881350361, 26.00000000000000355 ) ) ;
#158306 = EDGE_CURVE ( 'NONE', #162622, #157661, #23578, .T. ) ;
#158305 = CYLINDRICAL_SURFACE ( 'NONE', #85497, 0.09999999999999939493 ) ;
#158307 = CIRCLE ( 'NONE', #133336, 0.1000000000000028644 ) ;
#158309 = CARTESIAN_POINT ( 'NONE',  ( 20.94999999999999929, -8.730841121484171907, -110.0980747189843640 ) ) ;
#158308 = CARTESIAN_POINT ( 'NONE',  ( -20.85000000000000142, -1.164121893230052995, -175.4148480855716059 ) ) ;
#158310 = DIRECTION ( 'NONE',  ( 1.000000000000000000, 0.000000000000000000, 0.000000000000000000 ) ) ;
#158311 = LINE ( 'NONE', #18755, #102774 ) ;
#158312 = CARTESIAN_POINT ( 'NONE',  ( -20.65000000000000568, 5.650000000011139001, -146.6500000000000341 ) ) ;
#158313 = CARTESIAN_POINT ( 'NONE',  ( 21.04999999999908411, 44.16625465172463549, -236.5712595585798965 ) ) ;
#158314 = AXIS2_PLACEMENT_3D ( 'NONE', #143846, #223380, #245543 ) ;
#158315 = EDGE_LOOP ( 'NONE', ( #29581, #202864, #24178, #19912, #109918, #76470, #154411, #30288, #246516 ) ) ;
#158316 = EDGE_CURVE ( 'NONE', #144289, #136156, #139776, .T. ) ;
#158317 = ORIENTED_EDGE ( 'NONE', *, *, #187171, .F. ) ;
#158318 = FACE_OUTER_BOUND ( 'NONE', #77042, .T. ) ;
#158319 =( BOUNDED_CURVE ( )  B_SPLINE_CURVE ( 3, ( #9536, #248158, #132062, #150355 ),
 .UNSPECIFIED., .F., .F. ) 
 B_SPLINE_CURVE_WITH_KNOTS ( ( 4, 4 ),
 ( -9.769962616701377556E-15, 1.570796326794891673 ),
 .UNSPECIFIED. ) 
 CURVE ( )  GEOMETRIC_REPRESENTATION_ITEM ( )  RATIONAL_B_SPLINE_CURVE ( ( 1.000000000000000000, 0.8047378541243637162, 0.8047378541243637162, 1.000000000000000000 ) ) 
 REPRESENTATION_ITEM ( '' )  );
#158320 = DIRECTION ( 'NONE',  ( 0.000000000000000000, 0.8814952561688432775, -0.4721928772777345129 ) ) ;
#158321 = EDGE_CURVE ( 'NONE', #193662, #192673, #152300, .T. ) ;
#158322 = EDGE_CURVE ( 'NONE', #101771, #72671, #185587, .T. ) ;
#158323 = CARTESIAN_POINT ( 'NONE',  ( -18.40000000000000213, 11.47316190336248809, -24.25000000000001066 ) ) ;
#158324 = ORIENTED_EDGE ( 'NONE', *, *, #48770, .F. ) ;
#158326 = CIRCLE ( 'NONE', #91839, 0.09999999999999971412 ) ;
#158325 = CARTESIAN_POINT ( 'NONE',  ( -23.15000000000000213, 4.350000000011156054, -45.85000000000000142 ) ) ;
#158327 = VECTOR ( 'NONE', #62915, 1000.000000000000227 ) ;
#158328 = CARTESIAN_POINT ( 'NONE',  ( -16.91256925476572093, 66.01426884188410327, -157.4907499735297165 ) ) ;
#158329 = ORIENTED_EDGE ( 'NONE', *, *, #51023, .F. ) ;
#158330 = EDGE_CURVE ( 'NONE', #77390, #163525, #2672, .T. ) ;
#158331 = CARTESIAN_POINT ( 'NONE',  ( -18.51024323315077424, 10.31104185824062291, -206.5204516983105805 ) ) ;
#158332 = CARTESIAN_POINT ( 'NONE',  ( 23.14999999999999503, 69.45000000001181206, -81.77310748452434552 ) ) ;
#158333 = EDGE_CURVE ( 'NONE', #110369, #129974, #135686, .T. ) ;
#158334 = CARTESIAN_POINT ( 'NONE',  ( 18.59999999999999076, 6.450000000011156587, -77.01702717044007329 ) ) ;
#158335 =( BOUNDED_SURFACE ( )  B_SPLINE_SURFACE ( 3, 2, ( 
 ( #247364, #191284, #110426 ),
 ( #169157, #27077, #248657 ),
 ( #246103, #210816, #109133 ),
 ( #92148, #67446, #170458 ) ),
 .UNSPECIFIED., .F., .F., .F. ) 
 B_SPLINE_SURFACE_WITH_KNOTS ( ( 4, 4 ),
 ( 3, 3 ),
 ( -5.692061405548898279E-19, 0.0003124336117481331431 ),
 ( 0.000000000000000000, 1.000000000000000000 ),
 .UNSPECIFIED. ) 
 GEOMETRIC_REPRESENTATION_ITEM ( )  RATIONAL_B_SPLINE_SURFACE ( (
 ( 1.000000000000000000, 0.7040654476015839602, 1.000000000000000000),
 ( 1.000000000000000000, 0.7039193538781509663, 1.000000000000000000),
 ( 1.000000000000000000, 0.7089171279144148574, 1.000000000000000000),
 ( 1.000000000000000000, 0.7071067811866490471, 1.000000000000000000) ) ) 
 REPRESENTATION_ITEM ( '' )  SURFACE ( )  );
#158336 = CARTESIAN_POINT ( 'NONE',  ( 18.69999999999999929, -11.75000000000000000, 6.100000000000001421 ) ) ;
#158338 = ORIENTED_EDGE ( 'NONE', *, *, #231044, .T. ) ;
#158337 = CARTESIAN_POINT ( 'NONE',  ( -21.05000000000000071, 18.82290990851282331, -233.3604470821920529 ) ) ;
#158339 = EDGE_CURVE ( 'NONE', #159190, #105103, #198052, .T. ) ;
#158341 = ORIENTED_EDGE ( 'NONE', *, *, #7129, .T. ) ;
#158340 = DIRECTION ( 'NONE',  ( 0.000000000000000000, 0.8814952561688438326, -0.4721928772777331806 ) ) ;
#158342 = CARTESIAN_POINT ( 'NONE',  ( 21.14999999999999858, 10.71339244339988461, -12.25000000000000000 ) ) ;
#158343 = DIRECTION ( 'NONE',  ( -0.000000000000000000, -6.982962677686266711E-15, 1.000000000000000000 ) ) ;
#158344 = DIRECTION ( 'NONE',  ( -0.000000000000000000, -0.000000000000000000, -1.000000000000000000 ) ) ;
#158345 = CIRCLE ( 'NONE', #191671, 0.09999999999999939493 ) ;
#158346 = EDGE_CURVE ( 'NONE', #63327, #153891, #135498, .T. ) ;
#158349 = DIRECTION ( 'NONE',  ( -1.387778780781259631E-13, 0.1675535138457220907, -0.9858629823651720026 ) ) ;
#158348 = CIRCLE ( 'NONE', #45889, 0.1000000000000124678 ) ;
#158347 = DIRECTION ( 'NONE',  ( 1.000000000000000000, 0.000000000000000000, 0.000000000000000000 ) ) ;
#158350 = CARTESIAN_POINT ( 'NONE',  ( -16.94389599338512298, 66.00880201025755412, -190.9154626827142067 ) ) ;
#158351 = CARTESIAN_POINT ( 'NONE',  ( 20.94999999999999574, 40.74071615341952679, -237.9411309446948337 ) ) ;
#158352 = CIRCLE ( 'NONE', #200016, 0.1000000000000028644 ) ;
#158353 = CIRCLE ( 'NONE', #79189, 0.09999999999999609201 ) ;
#158354 = CARTESIAN_POINT ( 'NONE',  ( -20.54999999999999716, 87.75000000001229239, -157.6731074845242517 ) ) ;
#158355 = DIRECTION ( 'NONE',  ( 1.000000000000000000, 0.000000000000000000, 0.000000000000000000 ) ) ;
#158356 = LINE ( 'NONE', #39684, #172654 ) ;
#158357 = EDGE_CURVE ( 'NONE', #62147, #41411, #247938, .T. ) ;
#158358 = ADVANCED_FACE ( 'NONE', ( #101750 ), #222988, .T. ) ;
#158359 =( BOUNDED_CURVE ( )  B_SPLINE_CURVE ( 3, ( #135524, #173449, #138094, #115999 ),
 .UNSPECIFIED., .F., .F. ) 
 B_SPLINE_CURVE_WITH_KNOTS ( ( 4, 4 ),
 ( 0.5235987755983326775, 1.570796326794896558 ),
 .UNSPECIFIED. ) 
 CURVE ( )  GEOMETRIC_REPRESENTATION_ITEM ( )  RATIONAL_B_SPLINE_CURVE ( ( 1.000000000000000000, 0.9106836025229647635, 0.9106836025229647635, 1.000000000000000000 ) ) 
 REPRESENTATION_ITEM ( '' )  );
#158360 = VERTEX_POINT ( 'NONE', #126481 ) ;
#158361 = CARTESIAN_POINT ( 'NONE',  ( 21.11825140030092030, 0.007203620643717282591, -94.05459243457964646 ) ) ;
#158362 = AXIS2_PLACEMENT_3D ( 'NONE', #204560, #140737, #5048 ) ;
#158363 = EDGE_LOOP ( 'NONE', ( #79483, #129663, #9694, #229195 ) ) ;
#158364 = EDGE_LOOP ( 'NONE', ( #115517, #235886, #185532, #145554 ) ) ;
#158365 = EDGE_CURVE ( 'NONE', #56902, #202204, #127324, .T. ) ;
#158366 = CARTESIAN_POINT ( 'NONE',  ( -20.85000000000000142, 76.00000000001213607, -136.5231074845243313 ) ) ;
#158367 = DIRECTION ( 'NONE',  ( 0.000000000000000000, -0.8700118002898359348, 0.4930308989875165082 ) ) ;
#158368 = VERTEX_POINT ( 'NONE', #86037 ) ;
#158369 = ADVANCED_FACE ( 'NONE', ( #220467 ), #241313, .F. ) ;
#158370 = AXIS2_PLACEMENT_3D ( 'NONE', #88095, #242060, #127258 ) ;
#158371 = EDGE_CURVE ( 'NONE', #231172, #188954, #123055, .T. ) ;
#158372 = ORIENTED_EDGE ( 'NONE', *, *, #80618, .F. ) ;
#158373 = VECTOR ( 'NONE', #38665, 999.9999999999998863 ) ;
#158374 = ADVANCED_FACE ( 'NONE', ( #181344 ), #227276, .F. ) ;
#158375 = EDGE_LOOP ( 'NONE', ( #133338, #69179, #17448, #230498 ) ) ;
#158376 = ORIENTED_EDGE ( 'NONE', *, *, #249436, .F. ) ;
#158377 = FACE_OUTER_BOUND ( 'NONE', #256047, .T. ) ;
#158378 = DIRECTION ( 'NONE',  ( 0.000000000000000000, 0.2617529984164915779, 0.9651348961777187485 ) ) ;
#158379 = DIRECTION ( 'NONE',  ( 0.000000000000000000, 0.000000000000000000, -1.000000000000000000 ) ) ;
#158380 = DIRECTION ( 'NONE',  ( 8.673617379884087537E-15, 1.000000000000000000, 0.000000000000000000 ) ) ;
#158381 = DIRECTION ( 'NONE',  ( 0.000000000000000000, 0.000000000000000000, 1.000000000000000000 ) ) ;
#158383 = ORIENTED_EDGE ( 'NONE', *, *, #215893, .F. ) ;
#158382 = CYLINDRICAL_SURFACE ( 'NONE', #233935, 0.8750000000000007772 ) ;
#158385 = CARTESIAN_POINT ( 'NONE',  ( 18.39999999999999503, 11.75000000001113953, -146.6500000000000341 ) ) ;
#158384 = CARTESIAN_POINT ( 'NONE',  ( -16.91256925476569606, 63.08204023972218977, -213.0047279777397193 ) ) ;
#158386 = EDGE_CURVE ( 'NONE', #127210, #29232, #27410, .T. ) ;
#158387 = CARTESIAN_POINT ( 'NONE',  ( -21.64999999999999858, 10.05000000001113847, -79.75000000000004263 ) ) ;
#158388 = EDGE_CURVE ( 'NONE', #39343, #232002, #105606, .T. ) ;
#158389 = ORIENTED_EDGE ( 'NONE', *, *, #125864, .T. ) ;
#158390 = CARTESIAN_POINT ( 'NONE',  ( -16.94389599337535657, 63.05705733563543447, -213.0759594097623335 ) ) ;
#158391 = LINE ( 'NONE', #57947, #42088 ) ;
#158392 = ORIENTED_EDGE ( 'NONE', *, *, #246065, .F. ) ;
#158394 = CYLINDRICAL_SURFACE ( 'NONE', #124888, 0.5000000000000008882 ) ;
#158393 = CARTESIAN_POINT ( 'NONE',  ( 18.59999999999999076, 5.950000000011100632, -77.30570230503489881 ) ) ;
#158395 = CIRCLE ( 'NONE', #50183, 0.1000000000000043771 ) ;
#158396 = DIRECTION ( 'NONE',  ( 0.000000000000000000, 0.000000000000000000, 1.000000000000000000 ) ) ;
#158397 = CARTESIAN_POINT ( 'NONE',  ( -22.59999999999999432, 64.25012875563618309, -203.5885370755380848 ) ) ;
#158398 = ORIENTED_EDGE ( 'NONE', *, *, #74771, .F. ) ;
#158399 = DIRECTION ( 'NONE',  ( 0.000000000000000000, 1.000000000000000000, 0.000000000000000000 ) ) ;
#158401 = DIRECTION ( 'NONE',  ( -0.000000000000000000, -0.000000000000000000, 1.000000000000000000 ) ) ;
#158400 = AXIS2_PLACEMENT_3D ( 'NONE', #46714, #149708, #150969 ) ;
#158402 = FACE_OUTER_BOUND ( 'NONE', #228845, .T. ) ;
#158403 = CARTESIAN_POINT ( 'NONE',  ( -18.59999999999999787, 1.115600667400684642E-11, -141.9000000000000341 ) ) ;
#158404 = EDGE_LOOP ( 'NONE', ( #8943, #87238, #215312, #21375 ) ) ;
#158405 = CARTESIAN_POINT ( 'NONE',  ( 21.03675099975492202, 8.875180032795963569, -179.8255421367780400 ) ) ;
#158406 = DIRECTION ( 'NONE',  ( 0.000000000000000000, 0.000000000000000000, -1.000000000000000000 ) ) ;
#158407 = EDGE_CURVE ( 'NONE', #93820, #72763, #31502, .T. ) ;
#158408 = DIRECTION ( 'NONE',  ( 0.000000000000000000, 0.000000000000000000, -1.000000000000000000 ) ) ;
#158409 = CIRCLE ( 'NONE', #58386, 0.09999999999999939493 ) ;
#158410 = FACE_OUTER_BOUND ( 'NONE', #2546, .T. ) ;
#158411 = EDGE_CURVE ( 'NONE', #30084, #144435, #60662, .T. ) ;
#158413 = CARTESIAN_POINT ( 'NONE',  ( -18.46856557590793457, 85.47421590779882195, -162.9211212436420055 ) ) ;
#158412 = VECTOR ( 'NONE', #136304, 1000.000000000000000 ) ;
#158415 = ORIENTED_EDGE ( 'NONE', *, *, #54667, .T. ) ;
#158414 = CARTESIAN_POINT ( 'NONE',  ( -20.94999999999999929, 74.93036000061670165, -233.6816308724374949 ) ) ;
#158416 = DIRECTION ( 'NONE',  ( 1.000000000000000000, 0.000000000000000000, -0.000000000000000000 ) ) ;
#158417 = CARTESIAN_POINT ( 'NONE',  ( -16.84793658983426923, 66.05000000001189164, -90.28946080671389041 ) ) ;
#158418 = CARTESIAN_POINT ( 'NONE',  ( -18.40000000000000213, 62.23844973457045882, -209.3750075427748811 ) ) ;
#158419 = AXIS2_PLACEMENT_3D ( 'NONE', #15999, #193336, #215448 ) ;
#158420 = CARTESIAN_POINT ( 'NONE',  ( -16.87683809663752399, 48.78215419113038109, -213.4964773079645681 ) ) ;
#158421 = CARTESIAN_POINT ( 'NONE',  ( -21.05000000000000071, 1.115600667400684642E-11, -104.7999999999999972 ) ) ;
#158423 = ORIENTED_EDGE ( 'NONE', *, *, #18411, .F. ) ;
#158422 = DIRECTION ( 'NONE',  ( -1.000000000000000000, -0.000000000000000000, -0.000000000000000000 ) ) ;
#158424 = CYLINDRICAL_SURFACE ( 'NONE', #9211, 11.74999999999999645 ) ;
#158425 = AXIS2_PLACEMENT_3D ( 'NONE', #184025, #101898, #181483 ) ;
#158426 = FACE_OUTER_BOUND ( 'NONE', #226767, .T. ) ;
#158427 = DIRECTION ( 'NONE',  ( -0.000000000000000000, -0.000000000000000000, 1.000000000000000000 ) ) ;
#158428 = ORIENTED_EDGE ( 'NONE', *, *, #59982, .F. ) ;
#158429 = CARTESIAN_POINT ( 'NONE',  ( -12.42749937872396870, 66.62931007840965947, -152.4966423578633794 ) ) ;
#158430 = CARTESIAN_POINT ( 'NONE',  ( 21.04999999999999716, 76.01759718702130897, -176.4638783781849440 ) ) ;
#158431 = CARTESIAN_POINT ( 'NONE',  ( -18.43707690579160996, 87.08727414655713517, -199.6327537731850441 ) ) ;
#158432 = EDGE_CURVE ( 'NONE', #3727, #24355, #2402, .T. ) ;
#158433 = CARTESIAN_POINT ( 'NONE',  ( -23.15000000000000213, 64.25000000001175238, -76.36470817442145176 ) ) ;
#158434 = CARTESIAN_POINT ( 'NONE',  ( 21.14999999999999858, 1.115600667400684642E-11, -167.4999999999999716 ) ) ;
#158436 = ORIENTED_EDGE ( 'NONE', *, *, #101821, .T. ) ;
#158435 = AXIS2_PLACEMENT_3D ( 'NONE', #76878, #174754, #134278 ) ;
#158437 = ORIENTED_EDGE ( 'NONE', *, *, #94026, .F. ) ;
#158438 = AXIS2_PLACEMENT_3D ( 'NONE', #49908, #229835, #167320 ) ;
#158439 = AXIS2_PLACEMENT_3D ( 'NONE', #49617, #91322, #129164 ) ;
#158440 = DIRECTION ( 'NONE',  ( 0.000000000000000000, -1.000000000000000000, -6.982962677686265922E-15 ) ) ;
#158441 = DIRECTION ( 'NONE',  ( 1.000000000000000000, 0.000000000000000000, 0.000000000000000000 ) ) ;
#158442 = DIRECTION ( 'NONE',  ( 0.000000000000000000, -1.000000000000000000, -6.982962677686266711E-15 ) ) ;
#158443 = CARTESIAN_POINT ( 'NONE',  ( 20.94999999999999929, 4.813084112160684214, -189.0584822434761634 ) ) ;
#158444 = ORIENTED_EDGE ( 'NONE', *, *, #107735, .F. ) ;
#158445 = CARTESIAN_POINT ( 'NONE',  ( -21.98333005346336932, 76.00000000001200817, -110.3971828135809972 ) ) ;
#158446 = CARTESIAN_POINT ( 'NONE',  ( 20.30531438145591139, 11.52463756055922417, -206.4688238028691671 ) ) ;
#158447 = VECTOR ( 'NONE', #117828, 1000.000000000000000 ) ;
#158448 = CARTESIAN_POINT ( 'NONE',  ( -18.40000000000000213, 5.650000000011139001, -146.6500000000000341 ) ) ;
#158449 = DIRECTION ( 'NONE',  ( 0.000000000000000000, -6.982962677686266711E-15, 1.000000000000000000 ) ) ;
#158450 = ORIENTED_EDGE ( 'NONE', *, *, #79657, .T. ) ;
#158451 = DIRECTION ( 'NONE',  ( 0.000000000000000000, 1.000000000000000000, 0.000000000000000000 ) ) ;
#158452 = ORIENTED_EDGE ( 'NONE', *, *, #215547, .T. ) ;
#158453 = CARTESIAN_POINT ( 'NONE',  ( 20.85000000000000142, 77.36242903720497566, -61.63422623660309796 ) ) ;
#158454 = VERTEX_POINT ( 'NONE', #14261 ) ;
#158455 = CARTESIAN_POINT ( 'NONE',  ( -21.07928932188134397, 0.09889514566555071551, -27.17148334360670248 ) ) ;
#158456 = CARTESIAN_POINT ( 'NONE',  ( 23.14999999999999858, 4.813084112160680661, -145.9415177565238366 ) ) ;
#158457 = DIRECTION ( 'NONE',  ( -1.000000000000000000, 0.000000000000000000, 0.000000000000000000 ) ) ;
#158458 = ORIENTED_EDGE ( 'NONE', *, *, #220846, .T. ) ;
#158459 = FACE_OUTER_BOUND ( 'NONE', #233814, .T. ) ;
#158460 = CARTESIAN_POINT ( 'NONE',  ( -20.64999999999999858, 34.98408343502854478, -248.6539962344157004 ) ) ;
#158461 = EDGE_CURVE ( 'NONE', #96396, #201799, #52290, .T. ) ;
#158463 = VERTEX_POINT ( 'NONE', #70398 ) ;
#158462 = AXIS2_PLACEMENT_3D ( 'NONE', #2651, #77057, #82166 ) ;
#158464 = DIRECTION ( 'NONE',  ( 0.000000000000000000, 0.9651348961777163060, -0.2617529984165013479 ) ) ;
#158466 = EDGE_LOOP ( 'NONE', ( #124012, #172062, #22273, #118228 ) ) ;
#158465 = CARTESIAN_POINT ( 'NONE',  ( -18.40000000000000213, 8.212522512469059066, -212.1579332307740344 ) ) ;
#158467 = AXIS2_PLACEMENT_3D ( 'NONE', #191306, #192561, #174328 ) ;
#158469 = ADVANCED_FACE ( 'NONE', ( #10401 ), #147327, .T. ) ;
#158468 = DIRECTION ( 'NONE',  ( 0.000000000000000000, 0.8814952561688434995, -0.4721928772777337913 ) ) ;
#158470 = CARTESIAN_POINT ( 'NONE',  ( -18.43599941264930209, 85.51932742860702774, -163.0501306950028777 ) ) ;
#158471 = ORIENTED_EDGE ( 'NONE', *, *, #249286, .F. ) ;
#158472 = LINE ( 'NONE', #21520, #14554 ) ;
#158474 = EDGE_CURVE ( 'NONE', #16895, #253739, #163333, .T. ) ;
#158473 = DIRECTION ( 'NONE',  ( 0.000000000000000000, 0.000000000000000000, 1.000000000000000000 ) ) ;
#158475 = AXIS2_PLACEMENT_3D ( 'NONE', #15307, #132675, #235602 ) ;
#158476 = CYLINDRICAL_SURFACE ( 'NONE', #101442, 0.1000000000000046685 ) ;
#158477 = ORIENTED_EDGE ( 'NONE', *, *, #166920, .T. ) ;
#158478 = DIRECTION ( 'NONE',  ( 2.952720810173289112E-16, -1.000000000000000000, -0.000000000000000000 ) ) ;
#158480 = ADVANCED_FACE ( 'NONE', ( #228162 ), #181512, .F. ) ;
#158479 = CARTESIAN_POINT ( 'NONE',  ( 12.33938619321247110, 48.63273434562352548, -233.9299239298080124 ) ) ;
#158481 = DIRECTION ( 'NONE',  ( 0.7071359030026941328, -0.1850796971396165280, -0.6824253222084246673 ) ) ;
#158482 = TOROIDAL_SURFACE ( 'NONE', #116754, 0.2000000000000000111, 0.1000000000000000056 ) ;
#158483 = ORIENTED_EDGE ( 'NONE', *, *, #21809, .T. ) ;
#158484 = EDGE_CURVE ( 'NONE', #140050, #129734, #77242, .T. ) ;
#158485 = EDGE_LOOP ( 'NONE', ( #34841, #257825, #253277, #172073 ) ) ;
#158486 = TOROIDAL_SURFACE ( 'NONE', #25206, 0.2000000000000000111, 0.1000000000000000056 ) ;
#158487 = AXIS2_PLACEMENT_3D ( 'NONE', #221458, #42851, #139358 ) ;
#158488 = AXIS2_PLACEMENT_3D ( 'NONE', #170502, #164687, #218528 ) ;
#158489 = ORIENTED_EDGE ( 'NONE', *, *, #6508, .F. ) ;
#158490 = CARTESIAN_POINT ( 'NONE',  ( -19.89999999999999858, 1.250000000000000000, 21.90000000000000213 ) ) ;
#158492 = ADVANCED_FACE ( 'NONE', ( #92482 ), #243840, .T. ) ;
#158491 = CARTESIAN_POINT ( 'NONE',  ( 20.95512820512820440, 8.876151316299269567, -45.65000000000000568 ) ) ;
#158494 = ORIENTED_EDGE ( 'NONE', *, *, #152740, .F. ) ;
#158493 = CARTESIAN_POINT ( 'NONE',  ( 20.94999999999999929, 70.88170441948386724, -234.2197789011331679 ) ) ;
#158495 = LINE ( 'NONE', #39831, #157304 ) ;
#158496 = DIRECTION ( 'NONE',  ( 0.000000000000000000, -0.8814952561688449428, 0.4721928772777310157 ) ) ;
#158497 = DIRECTION ( 'NONE',  ( 2.952720810173289112E-16, -1.000000000000000000, 0.000000000000000000 ) ) ;
#158498 = CARTESIAN_POINT ( 'NONE',  ( -16.87331047859649757, 51.61886293219124155, -231.9464690156495692 ) ) ;
#158499 = FACE_BOUND ( 'NONE', #245131, .T. ) ;
#158500 = DIRECTION ( 'NONE',  ( -1.000000000000000000, 0.000000000000000000, 0.000000000000000000 ) ) ;
#158502 = VERTEX_POINT ( 'NONE', #12983 ) ;
#158501 = CARTESIAN_POINT ( 'NONE',  ( 21.30000000000002558, 76.00000000001267608, -203.5231074845243597 ) ) ;
#158504 = VERTEX_POINT ( 'NONE', #187761 ) ;
#158503 = CARTESIAN_POINT ( 'NONE',  ( -18.40000000000000213, 64.25000000001199396, -112.2731074845243739 ) ) ;
#158505 = CARTESIAN_POINT ( 'NONE',  ( 20.99999999999999645, 66.25000000001162448, -60.27310748452439526 ) ) ;
#158506 = VECTOR ( 'NONE', #137014, 1000.000000000000000 ) ;
#158507 = VERTEX_POINT ( 'NONE', #190327 ) ;
#158508 = ORIENTED_EDGE ( 'NONE', *, *, #151543, .F. ) ;
#158509 = CARTESIAN_POINT ( 'NONE',  ( -23.25000000000000355, 10.05000000001113847, -188.2499999999999716 ) ) ;
#158510 = CARTESIAN_POINT ( 'NONE',  ( -23.15000000000000213, 68.76258920191057200, -222.5680764032308048 ) ) ;
#158511 = LINE ( 'NONE', #116789, #80143 ) ;
#158512 = DIRECTION ( 'NONE',  ( 0.000000000000000000, -0.9126074666063769270, -0.4088369013363280513 ) ) ;
#158513 = DIRECTION ( 'NONE',  ( 0.7071067811865485719, 0.6233112732207607420, -0.3338907855510728773 ) ) ;
#158514 = CARTESIAN_POINT ( 'NONE',  ( 20.94999999999999929, 74.16465844978715438, -57.96795619196134908 ) ) ;
#158515 = FACE_OUTER_BOUND ( 'NONE', #131544, .T. ) ;
#158516 = AXIS2_PLACEMENT_3D ( 'NONE', #11917, #211383, #168455 ) ;
#158517 = ORIENTED_EDGE ( 'NONE', *, *, #153884, .T. ) ;
#158518 = EDGE_LOOP ( 'NONE', ( #231011, #230062, #155701, #152642 ) ) ;
#158519 = AXIS2_PLACEMENT_3D ( 'NONE', #214132, #38079, #173775 ) ;
#158520 = VECTOR ( 'NONE', #172824, 1000.000000000000000 ) ;
#158521 = ORIENTED_EDGE ( 'NONE', *, *, #87392, .F. ) ;
#158522 = FACE_OUTER_BOUND ( 'NONE', #85434, .T. ) ;
#158523 = CARTESIAN_POINT ( 'NONE',  ( 18.54148534481893407, 68.09306500613196533, -224.1549646960459086 ) ) ;
#158525 = EDGE_CURVE ( 'NONE', #179511, #108455, #98066, .T. ) ;
#158524 = CARTESIAN_POINT ( 'NONE',  ( -12.25000000000000178, 66.65000000001154490, -53.00453852712173841 ) ) ;
#158526 = TOROIDAL_SURFACE ( 'NONE', #250095, 0.2000000000000000111, 0.1000000000000000056 ) ;
#158527 = PLANE ( 'NONE',  #84582 ) ;
#158528 = EDGE_LOOP ( 'NONE', ( #255092, #195106, #147090, #38322, #195706, #135460, #216671, #127000, #123541, #178788, #135762, #228217, #33825, #51817, #177427, #256097 ) ) ;
#158529 = CARTESIAN_POINT ( 'NONE',  ( -16.94107738177414291, 65.98576071487562444, -149.0731074845244279 ) ) ;
#158530 = ORIENTED_EDGE ( 'NONE', *, *, #201182, .T. ) ;
#158532 = ADVANCED_FACE ( 'NONE', ( #11689 ), #168223, .F. ) ;
#158531 = DIRECTION ( 'NONE',  ( 0.000000000000000000, -0.1455152366551522025, -0.9893560106964505163 ) ) ;
#158533 = ORIENTED_EDGE ( 'NONE', *, *, #168561, .F. ) ;
#158534 = VECTOR ( 'NONE', #16315, 1000.000000000000000 ) ;
#158535 = CARTESIAN_POINT ( 'NONE',  ( 23.14999999999999858, 1.115600667400684642E-11, -100.5000000000000426 ) ) ;
#158536 = CARTESIAN_POINT ( 'NONE',  ( -21.59142135623730852, 7.850000000011158718, -45.85000000000000142 ) ) ;
#158537 = ADVANCED_FACE ( 'NONE', ( #29981 ), #77413, .T. ) ;
#158538 = DIRECTION ( 'NONE',  ( 1.000000000000000000, 0.000000000000000000, 0.000000000000000000 ) ) ;
#158539 = EDGE_CURVE ( 'NONE', #45068, #105564, #256432, .T. ) ;
#158540 = ORIENTED_EDGE ( 'NONE', *, *, #134124, .T. ) ;
#158541 = DIRECTION ( 'NONE',  ( -1.000000000000000000, 0.000000000000000000, 0.000000000000000000 ) ) ;
#158543 = ORIENTED_EDGE ( 'NONE', *, *, #141183, .F. ) ;
#158542 = CARTESIAN_POINT ( 'NONE',  ( 23.14999999999999858, 76.00000000001244871, -170.0231074845243597 ) ) ;
#158544 = CARTESIAN_POINT ( 'NONE',  ( 20.94999999999999574, 70.47363787294415260, -228.3418745167492432 ) ) ;
#158545 = ORIENTED_EDGE ( 'NONE', *, *, #173324, .F. ) ;
#158546 = LINE ( 'NONE', #180658, #32445 ) ;
#158547 = EDGE_LOOP ( 'NONE', ( #71818, #99645, #10120, #193002, #124228, #122947, #12089, #148082 ) ) ;
#158548 = EDGE_CURVE ( 'NONE', #201062, #223504, #164917, .T. ) ;
#158549 = CARTESIAN_POINT ( 'NONE',  ( -23.15000000000000213, -11.48087284838115885, -203.5004116939112464 ) ) ;
#158551 = CARTESIAN_POINT ( 'NONE',  ( 18.39999999999999503, 70.35000000001159037, -56.87310748452436115 ) ) ;
#158550 = CIRCLE ( 'NONE', #121155, 0.09999999999999520384 ) ;
#158552 = CARTESIAN_POINT ( 'NONE',  ( -18.40000000000000213, 54.02969457822032950, -229.1974241798695004 ) ) ;
#158553 = DIRECTION ( 'NONE',  ( -1.000000000000000000, 0.000000000000000000, 0.000000000000000000 ) ) ;
#158554 = EDGE_CURVE ( 'NONE', #75372, #110439, #235645, .T. ) ;
#158555 = FACE_OUTER_BOUND ( 'NONE', #155297, .T. ) ;
#158556 = AXIS2_PLACEMENT_3D ( 'NONE', #177004, #199101, #256435 ) ;
#158557 = ORIENTED_EDGE ( 'NONE', *, *, #224924, .F. ) ;
#158558 = LINE ( 'NONE', #60695, #90145 ) ;
#158559 = CARTESIAN_POINT ( 'NONE',  ( 21.05000000000001492, 6.540656951712398914, -100.5000000000000426 ) ) ;
#158560 = CARTESIAN_POINT ( 'NONE',  ( -20.94999999999999929, 76.00000000001145395, -40.12310748452431852 ) ) ;
#158561 = AXIS2_PLACEMENT_3D ( 'NONE', #101351, #195404, #98805 ) ;
#158562 = ORIENTED_EDGE ( 'NONE', *, *, #180288, .F. ) ;
#158563 = CYLINDRICAL_SURFACE ( 'NONE', #209452, 2.000000000000013323 ) ;
#158564 = ORIENTED_EDGE ( 'NONE', *, *, #143168, .F. ) ;
#158565 = CARTESIAN_POINT ( 'NONE',  ( -21.29999999999995808, 76.00000000001195133, -103.0231074845243171 ) ) ;
#158566 = VERTEX_POINT ( 'NONE', #174651 ) ;
#158567 = CARTESIAN_POINT ( 'NONE',  ( -21.07928932188134041, 69.67148334361938566, -203.6220026301787982 ) ) ;
#158568 = CARTESIAN_POINT ( 'NONE',  ( 21.05000000000000071, 12.62988036037870998, -223.4632815780722410 ) ) ;
#158569 = ADVANCED_FACE ( 'NONE', ( #97589 ), #1395, .F. ) ;
#158570 = AXIS2_PLACEMENT_3D ( 'NONE', #26239, #7958, #163181 ) ;
#158572 = ORIENTED_EDGE ( 'NONE', *, *, #31124, .F. ) ;
#158571 = DIRECTION ( 'NONE',  ( 0.000000000000000000, 0.000000000000000000, 1.000000000000000000 ) ) ;
#158573 = EDGE_CURVE ( 'NONE', #136758, #132345, #169242, .T. ) ;
#158574 = CARTESIAN_POINT ( 'NONE',  ( -18.59999996769639097, 9.038014976666358891, -245.3774329978512014 ) ) ;
#158575 = EDGE_LOOP ( 'NONE', ( #62805, #69613, #182915, #77308 ) ) ;
#158576 = ADVANCED_FACE ( 'NONE', ( #35126 ), #157644, .F. ) ;
#158577 = FACE_OUTER_BOUND ( 'NONE', #42135, .T. ) ;
#158578 = DIRECTION ( 'NONE',  ( -1.000000000000000000, 0.000000000000000000, 0.000000000000000000 ) ) ;
#158579 = VERTEX_POINT ( 'NONE', #58471 ) ;
#158580 = ORIENTED_EDGE ( 'NONE', *, *, #136041, .T. ) ;
#158581 = DIRECTION ( 'NONE',  ( 1.000000000000000000, 0.000000000000000000, 0.000000000000000000 ) ) ;
#158582 = LINE ( 'NONE', #119442, #73464 ) ;
#158583 = ORIENTED_EDGE ( 'NONE', *, *, #95209, .T. ) ;
#158584 = DIRECTION ( 'NONE',  ( 1.000000000000000000, 0.000000000000000000, 0.000000000000000000 ) ) ;
#158585 = CIRCLE ( 'NONE', #229310, 11.75000000000000533 ) ;
#158586 = VECTOR ( 'NONE', #211403, 1000.000000000000000 ) ;
#158587 = ORIENTED_EDGE ( 'NONE', *, *, #44973, .F. ) ;
#158588 = ORIENTED_EDGE ( 'NONE', *, *, #190099, .T. ) ;
#158589 = CIRCLE ( 'NONE', #91916, 0.2000000000000057288 ) ;
#158590 = CARTESIAN_POINT ( 'NONE',  ( 23.04999999999999716, 67.17743825834622839, -194.2731074845244166 ) ) ;
#158591 = AXIS2_PLACEMENT_3D ( 'NONE', #98037, #78492, #158098 ) ;
#158592 = AXIS2_PLACEMENT_3D ( 'NONE', #108357, #91365, #50909 ) ;
#158593 = AXIS2_PLACEMENT_3D ( 'NONE', #229028, #203025, #47789 ) ;
#158595 = EDGE_LOOP ( 'NONE', ( #205728, #134414, #217545, #141327 ) ) ;
#158594 = CARTESIAN_POINT ( 'NONE',  ( 20.85000000000000142, 64.35000000001214460, -136.5231074845244166 ) ) ;
#158596 = CARTESIAN_POINT ( 'NONE',  ( -2.995603634470829482E-16, -8.874060656858240748, -215.4698323230865640 ) ) ;
#158597 = CARTESIAN_POINT ( 'NONE',  ( -5.899999999999938183, 64.65000000001120384, -25.92310748452479174 ) ) ;
#158598 = EDGE_CURVE ( 'NONE', #229077, #146391, #248306, .T. ) ;
#158600 = DIRECTION ( 'NONE',  ( 0.000000000000000000, 0.000000000000000000, 1.000000000000000000 ) ) ;
#158599 = CARTESIAN_POINT ( 'NONE',  ( 20.95512820512820440, 8.876151316299271343, -42.05862899514094977 ) ) ;
#158601 = CARTESIAN_POINT ( 'NONE',  ( -21.05000000000000071, 76.02110330807134631, -142.8276238137879091 ) ) ;
#158602 = DIRECTION ( 'NONE',  ( 0.000000000000000000, 0.9915357197604973694, -0.1298341882519105928 ) ) ;
#158603 = LINE ( 'NONE', #213401, #201713 ) ;
#158604 = CIRCLE ( 'NONE', #104392, 11.70000000000000284 ) ;
#158605 = DIRECTION ( 'NONE',  ( 0.000000000000000000, 0.8700118002898321601, -0.4930308989875230030 ) ) ;
#158606 = CIRCLE ( 'NONE', #196176, 0.2000000000000101419 ) ;
#158607 = AXIS2_PLACEMENT_3D ( 'NONE', #128868, #130127, #227955 ) ;
#158608 = CIRCLE ( 'NONE', #357, 0.1999999999999987899 ) ;
#158610 = ORIENTED_EDGE ( 'NONE', *, *, #107102, .T. ) ;
#158609 = AXIS2_PLACEMENT_3D ( 'NONE', #5021, #102839, #6321 ) ;
#158612 = ORIENTED_EDGE ( 'NONE', *, *, #52221, .T. ) ;
#158611 = DIRECTION ( 'NONE',  ( 0.000000000000000000, 1.000000000000000000, 1.224646799147353207E-16 ) ) ;
#158613 = ORIENTED_EDGE ( 'NONE', *, *, #119823, .T. ) ;
#158614 = EDGE_CURVE ( 'NONE', #196929, #254440, #60858, .T. ) ;
#158615 = VERTEX_POINT ( 'NONE', #216276 ) ;
#158616 = CARTESIAN_POINT ( 'NONE',  ( -18.50000000000000000, 61.47936603916259912, -212.1738987416902376 ) ) ;
#158617 = EDGE_CURVE ( 'NONE', #238448, #164498, #173349, .T. ) ;
#158618 = CIRCLE ( 'NONE', #79476, 0.09999999999999939493 ) ;
#158619 = ORIENTED_EDGE ( 'NONE', *, *, #184549, .T. ) ;
#158620 = PRESENTATION_STYLE_ASSIGNMENT (( #241975 ) ) ;
#158622 = EDGE_CURVE ( 'NONE', #22349, #193539, #181682, .T. ) ;
#158621 = DIRECTION ( 'NONE',  ( 0.000000000000000000, 0.000000000000000000, 1.000000000000000000 ) ) ;
#158624 = VERTEX_POINT ( 'NONE', #76771 ) ;
#158623 = ORIENTED_EDGE ( 'NONE', *, *, #124523, .F. ) ;
#158625 = VERTEX_POINT ( 'NONE', #257926 ) ;
#158626 = EDGE_LOOP ( 'NONE', ( #213891, #10555, #140368 ) ) ;
#158627 = EDGE_CURVE ( 'NONE', #164610, #248838, #16925, .T. ) ;
#158628 = DIRECTION ( 'NONE',  ( -0.000000000000000000, -1.000000000000000000, 0.000000000000000000 ) ) ;
#158629 = CARTESIAN_POINT ( 'NONE',  ( 20.94999999999999929, 82.09643798151613225, -215.4278993322501208 ) ) ;
#158632 = EDGE_CURVE ( 'NONE', #144175, #151159, #89892, .T. ) ;
#158631 = EDGE_LOOP ( 'NONE', ( #74714, #110203, #200250, #133723 ) ) ;
#158630 = CARTESIAN_POINT ( 'NONE',  ( 20.99999999999998934, 7.900000000000000355, 1.212568896937007867 ) ) ;
#158633 = B_SPLINE_CURVE_WITH_KNOTS ( 'NONE', 3,
 ( #55719, #79158, #40084, #156176, #136566, #218670 ),
 .UNSPECIFIED., .F., .F.,
 ( 4, 2, 4 ),
 ( 0.000000000000000000, 0.0002113392456165950461, 0.0004226784912331900922 ),
 .UNSPECIFIED. ) ;
#158634 = FACE_OUTER_BOUND ( 'NONE', #75565, .T. ) ;
#158635 = DIRECTION ( 'NONE',  ( 0.000000000000000000, -7.056502275159894776E-15, 1.000000000000000000 ) ) ;
#158637 = EDGE_LOOP ( 'NONE', ( #156980, #69353, #237155, #219353 ) ) ;
#158636 = DIRECTION ( 'NONE',  ( 2.840903330521632269E-16, -0.9550021345545507412, 0.2965989261549202838 ) ) ;
#158638 = CARTESIAN_POINT ( 'NONE',  ( -21.55000000000000071, 7.350000000011155166, -112.7500000000000284 ) ) ;
#158639 = ORIENTED_EDGE ( 'NONE', *, *, #64179, .F. ) ;
#158640 = DIRECTION ( 'NONE',  ( 0.000000000000000000, -7.086529944415893080E-15, 1.000000000000000000 ) ) ;
#158641 = AXIS2_PLACEMENT_3D ( 'NONE', #226504, #47877, #28371 ) ;
#158643 = VERTEX_POINT ( 'NONE', #225246 ) ;
#158642 = LINE ( 'NONE', #178202, #156167 ) ;
#158644 = CARTESIAN_POINT ( 'NONE',  ( 23.24999999999999645, 1.115600667400684642E-11, -67.00000000000000000 ) ) ;
#158645 = DIRECTION ( 'NONE',  ( 1.000000000000000000, 0.000000000000000000, 0.000000000000000000 ) ) ;
#158646 = FACE_OUTER_BOUND ( 'NONE', #141401, .T. ) ;
#158647 = ORIENTED_EDGE ( 'NONE', *, *, #170606, .F. ) ;
#158649 = DIRECTION ( 'NONE',  ( 0.000000000000000000, 0.3488585713686311318, 0.9371753822965249725 ) ) ;
#158648 = CARTESIAN_POINT ( 'NONE',  ( -22.39999999999999858, 11.65000000001115588, -167.4999999999999716 ) ) ;
#158650 = DIRECTION ( 'NONE',  ( 1.000000000000000000, 0.000000000000000000, 0.000000000000000000 ) ) ;
#158651 = CARTESIAN_POINT ( 'NONE',  ( 18.41832399655379504, 85.68240326668673390, -163.3662638644972844 ) ) ;
#158652 = VECTOR ( 'NONE', #124552, 1000.000000000000000 ) ;
#158653 = ADVANCED_FACE ( 'NONE', ( #220151 ), #141877, .F. ) ;
#158654 = DIRECTION ( 'NONE',  ( -0.8660254037844515862, -0.4407476280843962146, 0.2360964386388669234 ) ) ;
#158655 = DIRECTION ( 'NONE',  ( 0.000000000000000000, 0.8814952561688437216, -0.4721928772777334582 ) ) ;
#158656 = EDGE_CURVE ( 'NONE', #250352, #47156, #185764, .T. ) ;
#158657 = ORIENTED_EDGE ( 'NONE', *, *, #60927, .F. ) ;
#158658 = ORIENTED_EDGE ( 'NONE', *, *, #257363, .T. ) ;
#158659 = ORIENTED_EDGE ( 'NONE', *, *, #205662, .T. ) ;
#158661 = AXIS2_PLACEMENT_3D ( 'NONE', #204175, #189761, #223735 ) ;
#158660 = DIRECTION ( 'NONE',  ( 4.408576920032446123E-17, 0.07893460099012301889, -0.9968797965484754720 ) ) ;
#158662 = ORIENTED_EDGE ( 'NONE', *, *, #132905, .T. ) ;
#158663 = FACE_OUTER_BOUND ( 'NONE', #21936, .T. ) ;
#158664 = VERTEX_POINT ( 'NONE', #45352 ) ;
#158665 = EDGE_CURVE ( 'NONE', #588, #141897, #160847, .T. ) ;
#158666 = DIRECTION ( 'NONE',  ( 1.000000000000000000, 0.000000000000000000, -0.000000000000000000 ) ) ;
#158667 = CARTESIAN_POINT ( 'NONE',  ( 21.14999999999999503, 7.128833340093095217, -233.7327013124392749 ) ) ;
#158668 = CIRCLE ( 'NONE', #104443, 0.09999999999998898659 ) ;
#158669 = EDGE_CURVE ( 'NONE', #37535, #129928, #52479, .T. ) ;
#158670 = ORIENTED_EDGE ( 'NONE', *, *, #34653, .T. ) ;
#158671 = CARTESIAN_POINT ( 'NONE',  ( -20.54999999999999716, 4.350000000011156054, -179.8499999999999943 ) ) ;
#158672 = EDGE_CURVE ( 'NONE', #225371, #88314, #227447, .T. ) ;
#158673 = AXIS2_PLACEMENT_3D ( 'NONE', #208389, #170583, #145812 ) ;
#158675 = ORIENTED_EDGE ( 'NONE', *, *, #89228, .F. ) ;
#158674 = CIRCLE ( 'NONE', #108577, 3.999999999999998224 ) ;
#158676 = ORIENTED_EDGE ( 'NONE', *, *, #46695, .T. ) ;
#158677 = EDGE_LOOP ( 'NONE', ( #153154, #200481, #128718, #50485, #166662, #117814, #226274, #83677, #180168, #17158, #78746, #139934, #172538, #140798, #56295, #150218, #76230, #212638, #135466, #221697, #193469, #119403, #217057, #131429, #64925 ) ) ;
#158678 = CIRCLE ( 'NONE', #179514, 0.09999999999999949207 ) ;
#158679 = EDGE_CURVE ( 'NONE', #141625, #221154, #1061, .T. ) ;
#158680 = DIRECTION ( 'NONE',  ( -0.000000000000000000, -1.000000000000000000, -6.982962677686266711E-15 ) ) ;
#158681 = CARTESIAN_POINT ( 'NONE',  ( 18.59999999999999076, 6.450000000011156587, -177.5170271704400022 ) ) ;
#158682 = CYLINDRICAL_SURFACE ( 'NONE', #121712, 0.5000000000000004441 ) ;
#158683 = CARTESIAN_POINT ( 'NONE',  ( -23.25000000000000355, 67.23581240663841641, -214.2531594801197627 ) ) ;
#158684 = CARTESIAN_POINT ( 'NONE',  ( 18.59999999999999076, 74.16465844978787914, -158.4679561919613775 ) ) ;
#158686 = CARTESIAN_POINT ( 'NONE',  ( 18.59999999999999076, 4.252251777740764460, -211.8999245327126744 ) ) ;
#158685 = DIRECTION ( 'NONE',  ( -1.000000000000000000, -0.000000000000000000, -0.000000000000000000 ) ) ;
#158687 = FACE_OUTER_BOUND ( 'NONE', #95089, .T. ) ;
#158689 = ORIENTED_EDGE ( 'NONE', *, *, #256294, .T. ) ;
#158688 = DIRECTION ( 'NONE',  ( 0.000000000000000000, 1.000000000000000000, 0.000000000000000000 ) ) ;
#158690 = CARTESIAN_POINT ( 'NONE',  ( -20.85000000000000142, -11.74999999998884448, -64.10000000000000853 ) ) ;
#158691 = ORIENTED_EDGE ( 'NONE', *, *, #197065, .F. ) ;
#158692 = DIRECTION ( 'NONE',  ( 0.000000000000000000, -1.411300455031978166E-14, 1.000000000000000000 ) ) ;
#158693 = ADVANCED_FACE ( 'NONE', ( #80599 ), #160196, .T. ) ;
#158694 = ORIENTED_EDGE ( 'NONE', *, *, #90828, .F. ) ;
#158695 = ORIENTED_EDGE ( 'NONE', *, *, #27689, .T. ) ;
#158696 = FACE_OUTER_BOUND ( 'NONE', #91669, .T. ) ;
#158697 = CARTESIAN_POINT ( 'NONE',  ( 21.05000000000000071, 76.00000000001142553, -36.02310748452432421 ) ) ;
#158698 = FACE_OUTER_BOUND ( 'NONE', #227879, .T. ) ;
#158699 = VERTEX_POINT ( 'NONE', #201858 ) ;
#158700 = CIRCLE ( 'NONE', #225267, 4.000000000000000000 ) ;
#158701 = CARTESIAN_POINT ( 'NONE',  ( -21.05000000000000071, 1.115600667400684642E-11, -200.9999999999999432 ) ) ;
#158702 = EDGE_LOOP ( 'NONE', ( #110327, #71072, #145246, #63539 ) ) ;
#158703 = ORIENTED_EDGE ( 'NONE', *, *, #182951, .T. ) ;
#158704 = DIRECTION ( 'NONE',  ( -1.000000000000000000, -0.000000000000000000, -0.000000000000000000 ) ) ;
#158705 = ORIENTED_EDGE ( 'NONE', *, *, #9065, .F. ) ;
#158706 = CARTESIAN_POINT ( 'NONE',  ( 20.00889983613310719, 5.561941060815491333, 16.56258203121810268 ) ) ;
#158707 = DIRECTION ( 'NONE',  ( 0.000000000000000000, 0.000000000000000000, -1.000000000000000000 ) ) ;
#158708 = VERTEX_POINT ( 'NONE', #61055 ) ;
#158709 = CARTESIAN_POINT ( 'NONE',  ( 22.39999999999999503, 7.790779598384535376, -67.00000000000004263 ) ) ;
#158710 = DIRECTION ( 'NONE',  ( 0.000000000000000000, 0.000000000000000000, -1.000000000000000000 ) ) ;
#158711 = LINE ( 'NONE', #238203, #80113 ) ;
#158712 = ORIENTED_EDGE ( 'NONE', *, *, #45576, .F. ) ;
#158713 = FACE_OUTER_BOUND ( 'NONE', #15073, .T. ) ;
#158714 = CIRCLE ( 'NONE', #246167, 4.049999999999995381 ) ;
#158715 = VECTOR ( 'NONE', #26216, 1000.000000000000000 ) ;
#158717 = DIRECTION ( 'NONE',  ( 0.000000000000000000, 0.000000000000000000, -1.000000000000000000 ) ) ;
#158716 = CIRCLE ( 'NONE', #238347, 0.09999999999998898659 ) ;
#158718 = CIRCLE ( 'NONE', #133731, 0.09999999999998898659 ) ;
#158719 = FACE_OUTER_BOUND ( 'NONE', #238023, .T. ) ;
#158720 = ORIENTED_EDGE ( 'NONE', *, *, #115519, .T. ) ;
#158721 = VECTOR ( 'NONE', #29196, 1000.000000000000000 ) ;
#158724 = ORIENTED_EDGE ( 'NONE', *, *, #44290, .F. ) ;
#158723 = ADVANCED_FACE ( 'NONE', ( #2355 ), #164024, .T. ) ;
#158722 = DIRECTION ( 'NONE',  ( 0.000000000000000000, -0.7397360091702647189, -0.6728971962616949742 ) ) ;
#158725 = ORIENTED_EDGE ( 'NONE', *, *, #40448, .T. ) ;
#158726 = DIRECTION ( 'NONE',  ( -1.000000000000000000, 0.000000000000000000, 0.000000000000000000 ) ) ;
#158727 = DIRECTION ( 'NONE',  ( 0.000000000000000000, 0.000000000000000000, -1.000000000000000000 ) ) ;
#158728 = CARTESIAN_POINT ( 'NONE',  ( 20.04142135623730070, 31.44980407958351165, -233.5445995079518866 ) ) ;
#158729 = CARTESIAN_POINT ( 'NONE',  ( 23.24999999999999289, 69.35000000001222986, -148.6731074845243938 ) ) ;
#158730 = CARTESIAN_POINT ( 'NONE',  ( -21.65000000000000213, 7.250000000011138646, -176.7499999999999716 ) ) ;
#158731 = CARTESIAN_POINT ( 'NONE',  ( -2.995603634470891112E-16, 87.75000000001196554, -111.7731074845242034 ) ) ;
#158732 = AXIS2_PLACEMENT_3D ( 'NONE', #149764, #164179, #66355 ) ;
#158733 = ORIENTED_EDGE ( 'NONE', *, *, #43565, .F. ) ;
#158734 = FACE_OUTER_BOUND ( 'NONE', #73037, .T. ) ;
#158735 = DIRECTION ( 'NONE',  ( 0.000000000000000000, 0.000000000000000000, -1.000000000000000000 ) ) ;
#158736 = CARTESIAN_POINT ( 'NONE',  ( -18.31572283045078109, 77.38696040852184410, -241.7683136019773542 ) ) ;
#158737 = LINE ( 'NONE', #77869, #221426 ) ;
#158738 = ADVANCED_FACE ( 'NONE', ( #83152 ), #145719, .F. ) ;
#158739 = CARTESIAN_POINT ( 'NONE',  ( 20.75572585718182950, 67.11768327161557579, -61.02584908581751222 ) ) ;
#158740 = ORIENTED_EDGE ( 'NONE', *, *, #109341, .T. ) ;
#158741 = EDGE_LOOP ( 'NONE', ( #62514, #236180, #134454, #191763, #195236 ) ) ;
#158742 = CARTESIAN_POINT ( 'NONE',  ( -21.65000000000000213, 68.29142135624910281, -81.87310748452436826 ) ) ;
#158743 = CARTESIAN_POINT ( 'NONE',  ( 20.94999999999999929, 30.48727911274996671, -240.1192265702093209 ) ) ;
#158744 = CARTESIAN_POINT ( 'NONE',  ( 23.25000000000000000, 51.33926024308902214, -230.0993571250899095 ) ) ;
#158745 = DIRECTION ( 'NONE',  ( 1.000000000000000000, 0.000000000000000000, 0.000000000000000000 ) ) ;
#158746 = DIRECTION ( 'NONE',  ( -0.000000000000000000, -1.000000000000000000, -0.000000000000000000 ) ) ;
#158747 = VECTOR ( 'NONE', #63807, 1000.000000000000000 ) ;
#158748 = ORIENTED_EDGE ( 'NONE', *, *, #215515, .F. ) ;
#158749 = CARTESIAN_POINT ( 'NONE',  ( -18.50000000000000711, 47.12422580718823895, -255.1840357777358577 ) ) ;
#158750 = CARTESIAN_POINT ( 'NONE',  ( -21.05000000000000071, 18.92285928089247804, -233.3572654221044900 ) ) ;
#158751 = VECTOR ( 'NONE', #179253, 1000.000000000000114 ) ;
#158752 = DIRECTION ( 'NONE',  ( 0.000000000000000000, 0.000000000000000000, 1.000000000000000000 ) ) ;
#158753 = CARTESIAN_POINT ( 'NONE',  ( -21.05000000000000071, 0.2561057921033771945, -167.4651035583276553 ) ) ;
#158754 = CIRCLE ( 'NONE', #67138, 0.09999999999999939493 ) ;
#158755 = VECTOR ( 'NONE', #252293, 1000.000000000000000 ) ;
#158756 = ORIENTED_EDGE ( 'NONE', *, *, #127131, .T. ) ;
#158757 = DIRECTION ( 'NONE',  ( 0.000000000000000000, 0.7092521942342977503, 0.7049548389605067023 ) ) ;
#158758 = CIRCLE ( 'NONE', #150548, 7.899999999999990585 ) ;
#158759 = ORIENTED_EDGE ( 'NONE', *, *, #175193, .T. ) ;
#158760 = CARTESIAN_POINT ( 'NONE',  ( 21.05000000000000071, 69.45934304831114048, -169.9231074845244223 ) ) ;
#158761 = CARTESIAN_POINT ( 'NONE',  ( 15.74999999999999645, 66.15000000001228386, -153.2731074845244450 ) ) ;
#158762 = CARTESIAN_POINT ( 'NONE',  ( 18.39999999999999503, 11.75000000001113953, -191.7499999999999716 ) ) ;
#158763 = CARTESIAN_POINT ( 'NONE',  ( -20.94999999999999929, 11.59999999999999609, -6.928203230275558511 ) ) ;
#158764 = CARTESIAN_POINT ( 'NONE',  ( -20.64999999999999858, -8.999999999988844479, -157.6060308773475924 ) ) ;
#158766 = CARTESIAN_POINT ( 'NONE',  ( -18.50000000000000000, 74.13328508995456900, -91.27043223824230722 ) ) ;
#158765 = AXIS2_PLACEMENT_3D ( 'NONE', #108890, #111467, #9795 ) ;
#158767 = EDGE_CURVE ( 'NONE', #68348, #127173, #48389, .T. ) ;
#158768 = CYLINDRICAL_SURFACE ( 'NONE', #1765, 0.09999999999999939493 ) ;
#158769 = DIRECTION ( 'NONE',  ( 1.000000000000000000, 0.000000000000000000, 0.000000000000000000 ) ) ;
#158770 = DIRECTION ( 'NONE',  ( -0.000000000000000000, 1.000000000000000000, 6.982962677686266711E-15 ) ) ;
#158772 = EDGE_CURVE ( 'NONE', #157934, #240710, #63533, .T. ) ;
#158771 = CARTESIAN_POINT ( 'NONE',  ( -21.64999999999999858, 9.350000000011133849, -121.3500000000000369 ) ) ;
#158773 = DIRECTION ( 'NONE',  ( -1.000000000000000000, 0.000000000000000000, 0.000000000000000000 ) ) ;
#158774 = CIRCLE ( 'NONE', #208651, 0.09999999999999939493 ) ;
#158775 = AXIS2_PLACEMENT_3D ( 'NONE', #105535, #222941, #164279 ) ;
#158776 = CARTESIAN_POINT ( 'NONE',  ( 21.09551895715237180, 10.62143732717995270, -79.23712466590011161 ) ) ;
#158777 = LINE ( 'NONE', #102588, #212123 ) ;
#158778 = VERTEX_POINT ( 'NONE', #12669 ) ;
#158779 = AXIS2_PLACEMENT_3D ( 'NONE', #56044, #191769, #170941 ) ;
#158780 = CARTESIAN_POINT ( 'NONE',  ( -20.64999999999999858, 85.00000000001188027, -93.12913836187181005 ) ) ;
#158782 = EDGE_CURVE ( 'NONE', #202894, #172095, #148308, .T. ) ;
#158781 = CARTESIAN_POINT ( 'NONE',  ( 22.60000000000000142, 7.128833340093095217, -233.7327013124392749 ) ) ;
#158783 = CARTESIAN_POINT ( 'NONE',  ( 20.77526135991777068, 8.932009016633434939, -41.96856854272417081 ) ) ;
#158784 = AXIS2_PLACEMENT_3D ( 'NONE', #164895, #26687, #65788 ) ;
#158785 = ORIENTED_EDGE ( 'NONE', *, *, #66536, .F. ) ;
#158787 = EDGE_CURVE ( 'NONE', #197707, #31916, #102522, .T. ) ;
#158786 = CARTESIAN_POINT ( 'NONE',  ( -18.59999999999999787, 64.35000000001264198, -196.5083017138704236 ) ) ;
#158788 = CARTESIAN_POINT ( 'NONE',  ( -18.50000000000000711, 11.75000000001115197, -107.5148057706540357 ) ) ;
#158789 = ORIENTED_EDGE ( 'NONE', *, *, #125671, .T. ) ;
#158790 = DIRECTION ( 'NONE',  ( 1.000000000000000000, 0.000000000000000000, -0.000000000000000000 ) ) ;
#158791 = DIRECTION ( 'NONE',  ( 0.000000000000000000, -0.000000000000000000, -1.000000000000000000 ) ) ;
#158792 = EDGE_CURVE ( 'NONE', #162858, #203841, #56552, .T. ) ;
#158793 = AXIS2_PLACEMENT_3D ( 'NONE', #137516, #198788, #117974 ) ;
#158794 = ORIENTED_EDGE ( 'NONE', *, *, #111778, .F. ) ;
#158795 = CIRCLE ( 'NONE', #42248, 0.1000000000000028644 ) ;
#158796 = CIRCLE ( 'NONE', #92124, 0.09999999999999961697 ) ;
#158797 = CIRCLE ( 'NONE', #121397, 0.1000000000000028644 ) ;
#158798 = ORIENTED_EDGE ( 'NONE', *, *, #102349, .T. ) ;
#158799 = ORIENTED_EDGE ( 'NONE', *, *, #202284, .T. ) ;
#158800 = EDGE_CURVE ( 'NONE', #48124, #229112, #156592, .T. ) ;
#158801 = DIRECTION ( 'NONE',  ( 0.000000000000000000, -0.2128009952263678062, 0.9770955615653298398 ) ) ;
#158802 = DIRECTION ( 'NONE',  ( 0.000000000000000000, -7.026728003956683390E-15, 1.000000000000000000 ) ) ;
#158803 = DIRECTION ( 'NONE',  ( -2.952720810173289605E-16, -1.000000000000000000, -7.086529944415894657E-15 ) ) ;
#158804 = CARTESIAN_POINT ( 'NONE',  ( -23.25000000000000000, -0.1008583690875562017, -88.75043287651064361 ) ) ;
#158805 = CYLINDRICAL_SURFACE ( 'NONE', #168423, 0.1000000000000070832 ) ;
#158806 = LINE ( 'NONE', #177086, #124880 ) ;
#158807 = DIRECTION ( 'NONE',  ( 0.000000000000000000, 0.000000000000000000, 1.000000000000000000 ) ) ;
#158808 = DIRECTION ( 'NONE',  ( -5.603264701231743991E-32, 0.2617529984165029577, 0.9651348961777157509 ) ) ;
#158809 = B_SPLINE_CURVE_WITH_KNOTS ( 'NONE', 3,
 ( #97715, #19509, #59878, #139419, #176028, #80730, #218967 ),
 .UNSPECIFIED., .F., .F.,
 ( 4, 3, 4 ),
 ( 0.000000000000000000, 4.520325912680675046E-05, 5.794988040901435228E-05 ),
 .UNSPECIFIED. ) ;
#158811 = ORIENTED_EDGE ( 'NONE', *, *, #206247, .F. ) ;
#158810 = CARTESIAN_POINT ( 'NONE',  ( -20.94999999999999929, 1.750000000011155743, -179.1695115579016147 ) ) ;
#158812 = ORIENTED_EDGE ( 'NONE', *, *, #152861, .F. ) ;
#158814 = CARTESIAN_POINT ( 'NONE',  ( -23.15000000000000213, 74.00000000001186606, -90.29848556176222019 ) ) ;
#158813 = CARTESIAN_POINT ( 'NONE',  ( 22.49999999999999645, 0.09999999999999939493, 11.64957080754480323 ) ) ;
#158817 = VERTEX_POINT ( 'NONE', #88295 ) ;
#158816 = CARTESIAN_POINT ( 'NONE',  ( 21.13507111622890022, 10.71768338700954537, -146.2491685863608097 ) ) ;
#158815 = DIRECTION ( 'NONE',  ( 1.000000000000000000, -0.000000000000000000, -0.000000000000000000 ) ) ;
#158818 = ORIENTED_EDGE ( 'NONE', *, *, #8854, .F. ) ;
#158819 = PLANE ( 'NONE',  #220587 ) ;
#158820 = DIRECTION ( 'NONE',  ( 0.000000000000000000, 0.000000000000000000, 1.000000000000000000 ) ) ;
#158821 = SURFACE_STYLE_FILL_AREA ( #224851 ) ;
#158822 = FACE_OUTER_BOUND ( 'NONE', #20923, .T. ) ;
#158823 = CARTESIAN_POINT ( 'NONE',  ( -18.59999999999999787, -1.164121893230052995, -175.4148480855716059 ) ) ;
#158824 = DIRECTION ( 'NONE',  ( 1.000000000000000000, -2.849773892568378313E-16, 7.728835255496647986E-17 ) ) ;
#158825 = AXIS2_PLACEMENT_3D ( 'NONE', #38924, #101396, #19350 ) ;
#158826 = EDGE_CURVE ( 'NONE', #36165, #47498, #166617, .T. ) ;
#158827 = DIRECTION ( 'NONE',  ( 0.000000000000000000, 6.982962677686266711E-15, -1.000000000000000000 ) ) ;
#158828 = ORIENTED_EDGE ( 'NONE', *, *, #20852, .F. ) ;
#158829 = ORIENTED_EDGE ( 'NONE', *, *, #173455, .F. ) ;
#158830 = DIRECTION ( 'NONE',  ( 0.000000000000000000, 0.000000000000000000, -1.000000000000000000 ) ) ;
#158831 = EDGE_LOOP ( 'NONE', ( #174624, #152837, #68086, #21611 ) ) ;
#158832 = CARTESIAN_POINT ( 'NONE',  ( 20.95224633520496127, 8.900522166568386240, -142.4932764479212892 ) ) ;
#158833 = VERTEX_POINT ( 'NONE', #110455 ) ;
#158834 = ADVANCED_FACE ( 'NONE', ( #227833 ), #190003, .T. ) ;
#158835 = VECTOR ( 'NONE', #167354, 1000.000000000000000 ) ;
#158836 = B_SPLINE_CURVE_WITH_KNOTS ( 'NONE', 3,
 ( #123842, #162980, #121305, #24765, #82107, #61293, #22185, #202092, #164257, #178709 ),
 .UNSPECIFIED., .F., .F.,
 ( 4, 2, 2, 2, 4 ),
 ( 0.000000000000000000, 0.0001660831991682130656, 0.0002491247987523196390, 0.0002906455985443753788, 0.0003321663983364311727 ),
 .UNSPECIFIED. ) ;
#158837 = DIRECTION ( 'NONE',  ( 0.000000000000000000, -0.9394191166662618775, -0.3427706569150580362 ) ) ;
#158838 = DIRECTION ( 'NONE',  ( 0.000000000000000000, -0.9126074666063769270, -0.4088369013363280513 ) ) ;
#158839 = CARTESIAN_POINT ( 'NONE',  ( 18.79999999999999716, 5.488301202077013663, 16.39999999999999858 ) ) ;
#158840 = CARTESIAN_POINT ( 'NONE',  ( -18.59999999999999787, 66.65000000001150227, -48.37310748452438958 ) ) ;
#158841 = VERTEX_POINT ( 'NONE', #167899 ) ;
#158843 = EDGE_CURVE ( 'NONE', #9710, #61341, #186148, .T. ) ;
#158842 = LINE ( 'NONE', #141808, #71263 ) ;
#158844 = CARTESIAN_POINT ( 'NONE',  ( 20.94999999999999574, 74.75000000001232081, -162.1231074845243540 ) ) ;
#158845 = CARTESIAN_POINT ( 'NONE',  ( -21.05000000000000071, -11.48912529306489994, -164.4000000000000057 ) ) ;
#158846 = DIRECTION ( 'NONE',  ( 0.000000000000000000, -0.8660254037844383745, 0.5000000000000003331 ) ) ;
#158847 = CARTESIAN_POINT ( 'NONE',  ( 23.14999999999999858, 73.90000000001170122, -69.52310748452431710 ) ) ;
#158848 = EDGE_CURVE ( 'NONE', #149361, #227159, #64955, .T. ) ;
#158849 = ORIENTED_EDGE ( 'NONE', *, *, #165243, .F. ) ;
#158851 = FACE_OUTER_BOUND ( 'NONE', #186729, .T. ) ;
#158850 = AXIS2_PLACEMENT_3D ( 'NONE', #159336, #110228, #32012 ) ;
#158852 = VERTEX_POINT ( 'NONE', #188708 ) ;
#158855 = ORIENTED_EDGE ( 'NONE', *, *, #15751, .F. ) ;
#158854 = CARTESIAN_POINT ( 'NONE',  ( -21.14999999999999858, -11.48087284838115885, -203.5004116939112464 ) ) ;
#158853 = CARTESIAN_POINT ( 'NONE',  ( 20.94999999999999929, -8.663551401858002876, -177.0241011180672785 ) ) ;
#158856 = AXIS2_PLACEMENT_3D ( 'NONE', #253833, #255073, #17787 ) ;
#158857 = DIRECTION ( 'NONE',  ( 0.000000000000000000, 0.000000000000000000, 1.000000000000000000 ) ) ;
#158858 = CARTESIAN_POINT ( 'NONE',  ( -22.48660254037843131, 64.35000000001164722, -69.57310748452438531 ) ) ;
#158859 = VERTEX_POINT ( 'NONE', #127458 ) ;
#158860 = CARTESIAN_POINT ( 'NONE',  ( 18.47135592147661853, 85.47108861327768636, -129.8395125446803320 ) ) ;
#158862 = EDGE_CURVE ( 'NONE', #68820, #99123, #194166, .T. ) ;
#158861 = DIRECTION ( 'NONE',  ( 0.000000000000000000, 1.000000000000000000, 0.000000000000000000 ) ) ;
#158863 = UNCERTAINTY_MEASURE_WITH_UNIT (LENGTH_MEASURE( 1.000000000000000082E-05 ), #45316, 'distance_accuracy_value', 'NONE');
#158865 = ORIENTED_EDGE ( 'NONE', *, *, #22129, .F. ) ;
#158864 = CARTESIAN_POINT ( 'NONE',  ( -18.43569575749026512, 8.780520186313282238, -245.4165333277510399 ) ) ;
#158866 = EDGE_CURVE ( 'NONE', #88637, #201039, #2596, .T. ) ;
#158867 = EDGE_CURVE ( 'NONE', #34960, #237722, #214982, .T. ) ;
#158868 = FACE_OUTER_BOUND ( 'NONE', #112488, .T. ) ;
#158869 = AXIS2_PLACEMENT_3D ( 'NONE', #189329, #51053, #109771 ) ;
#158870 = ORIENTED_EDGE ( 'NONE', *, *, #47098, .T. ) ;
#158871 = CARTESIAN_POINT ( 'NONE',  ( -16.94107738177415712, 10.01423928514777550, -180.0499999999999545 ) ) ;
#158872 = DIRECTION ( 'NONE',  ( 0.000000000000000000, 0.000000000000000000, -1.000000000000000000 ) ) ;
#158873 = CARTESIAN_POINT ( 'NONE',  ( -16.77828822508139694, 44.14854791318649774, -235.2972098120475266 ) ) ;
#158874 = ORIENTED_EDGE ( 'NONE', *, *, #251499, .T. ) ;
#158875 = DIRECTION ( 'NONE',  ( -1.000000000000000000, -0.000000000000000000, -0.000000000000000000 ) ) ;
#158876 = ORIENTED_EDGE ( 'NONE', *, *, #7855, .T. ) ;
#158877 = CARTESIAN_POINT ( 'NONE',  ( -23.25000000000000000, 4.150000000011156764, -179.8499999999999943 ) ) ;
#158878 = EDGE_CURVE ( 'NONE', #201172, #13472, #130001, .T. ) ;
#158879 = DIRECTION ( 'NONE',  ( 1.000000000000000000, 0.000000000000000000, 0.000000000000000000 ) ) ;
#158880 = CARTESIAN_POINT ( 'NONE',  ( 22.60000000000000142, 11.45898712536580177, -198.4011321578509808 ) ) ;
#158881 = ORIENTED_EDGE ( 'NONE', *, *, #201004, .T. ) ;
#158882 = ADVANCED_FACE ( 'NONE', ( #209564 ), #212143, .F. ) ;
#158883 = DIRECTION ( 'NONE',  ( 0.000000000000000000, 0.9654727137038715545, -0.2605042016806676242 ) ) ;
#158884 = EDGE_CURVE ( 'NONE', #215604, #137004, #87019, .T. ) ;
#158885 = DIRECTION ( 'NONE',  ( 0.000000000000000000, 0.8660254037844377084, 0.5000000000000016653 ) ) ;
#158886 = CIRCLE ( 'NONE', #25599, 0.09999999999999939493 ) ;
#158887 = AXIS2_PLACEMENT_3D ( 'NONE', #240872, #123485, #59624 ) ;
#158888 = DIRECTION ( 'NONE',  ( 0.000000000000000000, -0.8659859643398405415, 0.5000683049008369796 ) ) ;
#158889 = ORIENTED_EDGE ( 'NONE', *, *, #45901, .F. ) ;
#158890 = AXIS2_PLACEMENT_3D ( 'NONE', #193991, #216087, #97400 ) ;
#158891 = CARTESIAN_POINT ( 'NONE',  ( 18.59999999999999787, 77.83534155023627932, -91.46795619196132066 ) ) ;
#158892 = CARTESIAN_POINT ( 'NONE',  ( 21.05000000000000071, -11.64999999999999147, -30.59999999999999432 ) ) ;
#158893 = FACE_OUTER_BOUND ( 'NONE', #92078, .T. ) ;
#158894 = VERTEX_POINT ( 'NONE', #191318 ) ;
#158895 = DIRECTION ( 'NONE',  ( 1.000000000000000000, 0.000000000000000000, 0.000000000000000000 ) ) ;
#158896 = EDGE_LOOP ( 'NONE', ( #19938, #114983, #235260 ) ) ;
#158898 = ORIENTED_EDGE ( 'NONE', *, *, #46501, .T. ) ;
#158897 = DIRECTION ( 'NONE',  ( 0.000000000000000000, 0.8814952561688430555, -0.4721928772777346239 ) ) ;
#158899 = EDGE_CURVE ( 'NONE', #221804, #131374, #85772, .T. ) ;
#158900 = EDGE_CURVE ( 'NONE', #10704, #118654, #97269, .T. ) ;
#158901 = AXIS2_PLACEMENT_3D ( 'NONE', #216117, #221242, #257765 ) ;
#158904 = ORIENTED_EDGE ( 'NONE', *, *, #84988, .T. ) ;
#158903 = ORIENTED_EDGE ( 'NONE', *, *, #44759, .T. ) ;
#158902 = CARTESIAN_POINT ( 'NONE',  ( -21.65000000000000213, 66.05000000001207638, -123.7731074845243739 ) ) ;
#158905 = CARTESIAN_POINT ( 'NONE',  ( 20.95595012432476523, 65.39582078693575795, -95.42733815430624134 ) ) ;
#158906 = DIRECTION ( 'NONE',  ( 1.000000000000000000, 0.000000000000000000, 0.000000000000000000 ) ) ;
#158908 = EDGE_CURVE ( 'NONE', #172111, #158643, #188013, .T. ) ;
#158907 = DIRECTION ( 'NONE',  ( 0.000000000000000000, 0.000000000000000000, 1.000000000000000000 ) ) ;
#158909 = CARTESIAN_POINT ( 'NONE',  ( 20.86777300164945004, 46.46797214202639026, -243.0846070113367432 ) ) ;
#158910 = CARTESIAN_POINT ( 'NONE',  ( -21.65000000000000213, 14.25671114421267127, -219.2337924566137701 ) ) ;
#158911 = DIRECTION ( 'NONE',  ( 1.000000000000000000, -0.000000000000000000, -0.000000000000000000 ) ) ;
#158912 = LINE ( 'NONE', #59755, #59846 ) ;
#158914 = DIRECTION ( 'NONE',  ( 0.000000000000000000, 0.000000000000000000, 1.000000000000000000 ) ) ;
#158913 = DIRECTION ( 'NONE',  ( 0.000000000000000000, -0.2128009952261912530, 0.9770955615653682536 ) ) ;
#158915 = ORIENTED_EDGE ( 'NONE', *, *, #182553, .F. ) ;
#158916 = ORIENTED_EDGE ( 'NONE', *, *, #235593, .T. ) ;
#158917 = DIRECTION ( 'NONE',  ( 1.000000000000000000, 0.000000000000000000, 0.000000000000000000 ) ) ;
#158919 = ORIENTED_EDGE ( 'NONE', *, *, #136132, .F. ) ;
#158918 = DIRECTION ( 'NONE',  ( 0.000000000000000000, -0.4791956752371546169, -0.8777080977375152360 ) ) ;
#158920 = FACE_OUTER_BOUND ( 'NONE', #113898, .T. ) ;
#158921 = EDGE_LOOP ( 'NONE', ( #40167, #47221, #238541, #143382 ) ) ;
#158922 = B_SPLINE_CURVE_WITH_KNOTS ( 'NONE', 3,
 ( #187129, #245796, #67156, #204083, #123282, #144104, #45024, #247058, #68449, #227502, #241928, #124572, #5877, #128417, #65867, #184519 ),
 .UNSPECIFIED., .F., .F.,
 ( 4, 3, 3, 3, 3, 4 ),
 ( 0.000000000000000000, 2.209075297430740031E-05, 5.594258369009624354E-05, 8.979524372342012487E-05, 0.0001236472815274586301, 0.0001574990747609554737 ),
 .UNSPECIFIED. ) ;
#158924 = DIRECTION ( 'NONE',  ( 0.000000000000000000, 0.000000000000000000, -1.000000000000000000 ) ) ;
#158923 = AXIS2_PLACEMENT_3D ( 'NONE', #94081, #13283, #92796 ) ;
#158925 = ORIENTED_EDGE ( 'NONE', *, *, #141194, .F. ) ;
#158926 = DIRECTION ( 'NONE',  ( 1.000000000000000000, 0.000000000000000000, 0.000000000000000000 ) ) ;
#158927 = AXIS2_PLACEMENT_3D ( 'NONE', #82292, #161887, #221806 ) ;
#158928 = EDGE_CURVE ( 'NONE', #61955, #108295, #37361, .T. ) ;
#158929 = EDGE_LOOP ( 'NONE', ( #202267, #205002, #44254, #256813 ) ) ;
#158931 = AXIS2_PLACEMENT_3D ( 'NONE', #98481, #198911, #159804 ) ;
#158930 = FACE_OUTER_BOUND ( 'NONE', #192172, .T. ) ;
#158933 = EDGE_CURVE ( 'NONE', #101417, #233526, #96579, .T. ) ;
#158932 = DIRECTION ( 'NONE',  ( 0.000000000000000000, -0.1480365673253065117, 0.9889818879709273425 ) ) ;
#158935 = ORIENTED_EDGE ( 'NONE', *, *, #21274, .F. ) ;
#158934 = EDGE_LOOP ( 'NONE', ( #182022, #147669, #241863, #2393 ) ) ;
#158936 = ORIENTED_EDGE ( 'NONE', *, *, #230352, .F. ) ;
#158938 = DIRECTION ( 'NONE',  ( 1.000000000000000000, -0.000000000000000000, -0.000000000000000000 ) ) ;
#158937 = AXIS2_PLACEMENT_3D ( 'NONE', #60212, #58906, #241443 ) ;
#158939 = ORIENTED_EDGE ( 'NONE', *, *, #118830, .T. ) ;
#158940 = VERTEX_POINT ( 'NONE', #174338 ) ;
#158941 = CARTESIAN_POINT ( 'NONE',  ( -21.14999999999999858, 11.65000000001115588, -33.60000000000000142 ) ) ;
#158942 = TOROIDAL_SURFACE ( 'NONE', #63036, 11.70000000000000107, 0.1000000000000000056 ) ;
#158945 = EDGE_CURVE ( 'NONE', #164707, #14295, #161020, .T. ) ;
#158944 = ORIENTED_EDGE ( 'NONE', *, *, #256332, .F. ) ;
#158943 = CARTESIAN_POINT ( 'NONE',  ( 18.52326479938708559, -9.642364444904341525, -107.2147574134056924 ) ) ;
#158947 = CARTESIAN_POINT ( 'NONE',  ( -18.50000000000000000, 74.73788286442776041, -233.7359682632885267 ) ) ;
#158946 = CARTESIAN_POINT ( 'NONE',  ( 21.15000000000005187, 64.25000000001119815, -3.123107484524795474 ) ) ;
#158948 = CARTESIAN_POINT ( 'NONE',  ( -18.50000000000000355, -1.263275465217258198, -41.40186466674640542 ) ) ;
#158949 = DIRECTION ( 'NONE',  ( 0.000000000000000000, -0.4230464831072829335, 0.9061079809440810706 ) ) ;
#158950 = CARTESIAN_POINT ( 'NONE',  ( -21.14999999999999858, -11.74999999998884448, -134.0000000000000000 ) ) ;
#158951 = ORIENTED_EDGE ( 'NONE', *, *, #159619, .F. ) ;
#158952 = ADVANCED_FACE ( 'NONE', ( #257608 ), #195164, .T. ) ;
#158953 = VECTOR ( 'NONE', #207713, 1000.000000000000000 ) ;
#158954 = ORIENTED_EDGE ( 'NONE', *, *, #181821, .T. ) ;
#158955 = CYLINDRICAL_SURFACE ( 'NONE', #249681, 0.09999999999998304689 ) ;
#158956 = DIRECTION ( 'NONE',  ( 0.000000000000000000, -1.000000000000000000, -1.734723475976807292E-15 ) ) ;
#158957 = LINE ( 'NONE', #178519, #33179 ) ;
#158958 = EDGE_CURVE ( 'NONE', #155298, #78597, #85963, .T. ) ;
#158960 = ORIENTED_EDGE ( 'NONE', *, *, #227183, .F. ) ;
#158959 = AXIS2_PLACEMENT_3D ( 'NONE', #101661, #37899, #120013 ) ;
#158961 = DIRECTION ( 'NONE',  ( -2.915501640297154283E-16, -0.9651348961777159730, 0.2617529984165023471 ) ) ;
#158962 = CIRCLE ( 'NONE', #42402, 0.09999999999998898659 ) ;
#158963 = EDGE_CURVE ( 'NONE', #125216, #222808, #218517, .T. ) ;
#158964 = DIRECTION ( 'NONE',  ( 0.000000000000000000, 0.2868887416115947775, -0.9579639084728169829 ) ) ;
#158965 = CARTESIAN_POINT ( 'NONE',  ( -14.87779219673429054, 12.45596502558539243, -213.8760425650930870 ) ) ;
#158967 = EDGE_CURVE ( 'NONE', #172421, #35530, #136031, .T. ) ;
#158966 = ADVANCED_FACE ( 'NONE', ( #154745 ), #217237, .F. ) ;
#158968 = EDGE_LOOP ( 'NONE', ( #117565, #240875, #140627, #118248 ) ) ;
#158969 = ORIENTED_EDGE ( 'NONE', *, *, #170682, .F. ) ;
#158970 = DIRECTION ( 'NONE',  ( 1.000000000000000000, -0.000000000000000000, -0.000000000000000000 ) ) ;
#158971 = DIRECTION ( 'NONE',  ( 1.000000000000000000, 0.000000000000000000, 0.000000000000000000 ) ) ;
#158972 = ORIENTED_EDGE ( 'NONE', *, *, #201553, .T. ) ;
#158973 = CARTESIAN_POINT ( 'NONE',  ( -13.39999999999994351, 63.75000000001119815, -21.02310748452479316 ) ) ;
#158974 = ORIENTED_EDGE ( 'NONE', *, *, #145880, .T. ) ;
#158975 = CARTESIAN_POINT ( 'NONE',  ( -20.94999999999999929, 1.115600667400684642E-11, -167.4999999999999716 ) ) ;
#158976 = FACE_OUTER_BOUND ( 'NONE', #23338, .T. ) ;
#158978 = SURFACE_STYLE_USAGE ( .BOTH. , #79390 ) ;
#158977 = DIRECTION ( 'NONE',  ( 0.000000000000000000, 0.000000000000000000, 1.000000000000000000 ) ) ;
#158979 = LINE ( 'NONE', #220216, #228273 ) ;
#158980 = CYLINDRICAL_SURFACE ( 'NONE', #95318, 4.000000000000006217 ) ;
#158981 = VERTEX_POINT ( 'NONE', #55580 ) ;
#158982 = AXIS2_PLACEMENT_3D ( 'NONE', #126368, #205898, #106792 ) ;
#158983 = EDGE_CURVE ( 'NONE', #141200, #39669, #10979, .T. ) ;
#158984 = ADVANCED_FACE ( 'NONE', ( #153494 ), #48572, .T. ) ;
#158985 = AXIS2_PLACEMENT_3D ( 'NONE', #222844, #84574, #142028 ) ;
#158986 = AXIS2_PLACEMENT_3D ( 'NONE', #84276, #43924, #83016 ) ;
#158988 = ORIENTED_EDGE ( 'NONE', *, *, #162121, .F. ) ;
#158987 = VERTEX_POINT ( 'NONE', #178161 ) ;
#158990 = ORIENTED_EDGE ( 'NONE', *, *, #137294, .T. ) ;
#158989 = VECTOR ( 'NONE', #199410, 1000.000000000000000 ) ;
#158991 = EDGE_CURVE ( 'NONE', #242144, #14565, #256555, .T. ) ;
#158992 = CARTESIAN_POINT ( 'NONE',  ( 22.37643362114956247, 7.625789993969535274, -33.40091862631862085 ) ) ;
#158993 = DIRECTION ( 'NONE',  ( 1.000000000000000000, -0.000000000000000000, -0.000000000000000000 ) ) ;
#158994 = DIRECTION ( 'NONE',  ( 0.000000000000000000, 0.9908441862701782288, 0.1350103645450542456 ) ) ;
#158995 = DIRECTION ( 'NONE',  ( 0.000000000000000000, -0.9999631594459057471, 0.008583690987121077309 ) ) ;
#158997 = CARTESIAN_POINT ( 'NONE',  ( -14.87779219673428521, 66.56936653093906386, -87.79134168970027474 ) ) ;
#158996 = CYLINDRICAL_SURFACE ( 'NONE', #232882, 0.09999999999999939493 ) ;
#158998 = EDGE_CURVE ( 'NONE', #89961, #33900, #177618, .T. ) ;
#158999 = ORIENTED_EDGE ( 'NONE', *, *, #209159, .T. ) ;
#159000 = ORIENTED_EDGE ( 'NONE', *, *, #187147, .F. ) ;
#159001 = DIRECTION ( 'NONE',  ( 1.000000000000000000, 1.186688945009009831E-16, 0.000000000000000000 ) ) ;
#159002 = ADVANCED_FACE ( 'NONE', ( #114308 ), #240673, .T. ) ;
#159003 = ORIENTED_EDGE ( 'NONE', *, *, #238321, .T. ) ;
#159004 = ORIENTED_EDGE ( 'NONE', *, *, #109038, .T. ) ;
#159005 = CARTESIAN_POINT ( 'NONE',  ( -23.25000000000000000, -11.64999999998884483, -122.2500000000000284 ) ) ;
#159006 = DIRECTION ( 'NONE',  ( 0.000000000000000000, 1.000000000000000000, 0.000000000000000000 ) ) ;
#159007 = DIRECTION ( 'NONE',  ( 1.000000000000000000, 0.000000000000000000, 0.000000000000000000 ) ) ;
#159008 = LINE ( 'NONE', #59847, #141600 ) ;
#159009 = AXIS2_PLACEMENT_3D ( 'NONE', #214114, #95443, #89323 ) ;
#159010 = EDGE_LOOP ( 'NONE', ( #135207, #73291, #156510, #117804 ) ) ;
#159011 = EDGE_LOOP ( 'NONE', ( #58699, #114342, #1328, #25099 ) ) ;
#159012 = CARTESIAN_POINT ( 'NONE',  ( 20.94999999999999574, 1.162701749949165642, -175.5999999999999659 ) ) ;
#159013 = CARTESIAN_POINT ( 'NONE',  ( -18.58671080940900566, -9.406932858815460818, -40.62415446490468440 ) ) ;
#159015 = EDGE_CURVE ( 'NONE', #211977, #179202, #91745, .T. ) ;
#159014 = ORIENTED_EDGE ( 'NONE', *, *, #122282, .T. ) ;
#159016 = FACE_OUTER_BOUND ( 'NONE', #23744, .T. ) ;
#159017 = FACE_OUTER_BOUND ( 'NONE', #115632, .T. ) ;
#159018 = ADVANCED_FACE ( 'NONE', ( #239401 ), #60736, .F. ) ;
#159019 = DIRECTION ( 'NONE',  ( 1.000000000000000000, 0.000000000000000000, 0.000000000000000000 ) ) ;
#159020 = DIRECTION ( 'NONE',  ( 1.000000000000000000, 0.000000000000000000, 0.000000000000000000 ) ) ;
#159021 = CARTESIAN_POINT ( 'NONE',  ( -20.54999999999999716, -11.75000000000000178, -12.35000000000000675 ) ) ;
#159022 = CYLINDRICAL_SURFACE ( 'NONE', #137540, 0.1000000000000098310 ) ;
#159024 = CARTESIAN_POINT ( 'NONE',  ( -21.45000000000000284, 7.708578643773852157, -54.75000000000000000 ) ) ;
#159023 = LINE ( 'NONE', #199423, #99357 ) ;
#159025 = FACE_OUTER_BOUND ( 'NONE', #45056, .T. ) ;
#159027 = ADVANCED_FACE ( 'NONE', ( #45043 ), #164990, .T. ) ;
#159026 = LINE ( 'NONE', #181142, #229138 ) ;
#159028 = LINE ( 'NONE', #220271, #120405 ) ;
#159030 = VERTEX_POINT ( 'NONE', #145418 ) ;
#159029 = CIRCLE ( 'NONE', #13257, 0.09999999999999609201 ) ;
#159032 = EDGE_CURVE ( 'NONE', #232478, #103372, #69447, .T. ) ;
#159031 = CARTESIAN_POINT ( 'NONE',  ( 21.14999999999999858, 11.75000000001116263, -100.6000000000000369 ) ) ;
#159033 = ORIENTED_EDGE ( 'NONE', *, *, #3042, .T. ) ;
#159034 = CARTESIAN_POINT ( 'NONE',  ( 18.49999999999999289, 64.25000000001176659, -78.17310748452439384 ) ) ;
#159035 = CARTESIAN_POINT ( 'NONE',  ( -21.07928932188134041, 0.09889514566555068775, -94.17148334360673800 ) ) ;
#159036 = DIRECTION ( 'NONE',  ( 0.000000000000000000, 1.000000000000000000, 6.853228547068871147E-15 ) ) ;
#159037 = VERTEX_POINT ( 'NONE', #82845 ) ;
#159038 = CARTESIAN_POINT ( 'NONE',  ( 22.48660254037844197, 11.65000000001116298, -100.4500000000000455 ) ) ;
#159039 = DIRECTION ( 'NONE',  ( -3.265361837132813586E-16, 0.9770955615653313941, 0.2128009952263609783 ) ) ;
#159040 = FACE_OUTER_BOUND ( 'NONE', #133406, .T. ) ;
#159041 = AXIS2_PLACEMENT_3D ( 'NONE', #215132, #213847, #133042 ) ;
#159042 = EDGE_CURVE ( 'NONE', #201516, #175441, #3326, .T. ) ;
#159043 = CIRCLE ( 'NONE', #196412, 0.09999999999998898659 ) ;
#159044 = CARTESIAN_POINT ( 'NONE',  ( -21.14999999999999858, 87.65000000001269598, -203.5231074845243029 ) ) ;
#159045 = CARTESIAN_POINT ( 'NONE',  ( 18.39999999999999858, 85.68240343348806221, -62.86626410711144786 ) ) ;
#159047 = DIRECTION ( 'NONE',  ( -1.000000000000000000, -7.304098846218135653E-16, -5.100424963727256530E-30 ) ) ;
#159046 = CIRCLE ( 'NONE', #753, 0.5000000000000004441 ) ;
#159048 = ORIENTED_EDGE ( 'NONE', *, *, #248568, .T. ) ;
#159049 = LINE ( 'NONE', #68930, #100025 ) ;
#159051 = EDGE_LOOP ( 'NONE', ( #96097, #175936, #4613, #159166, #162206, #77551, #151861, #89476, #221610, #93007, #32257, #202199, #255135, #4280 ) ) ;
#159050 = DIRECTION ( 'NONE',  ( -1.000000000000000000, -0.000000000000000000, -0.000000000000000000 ) ) ;
#159052 = FACE_OUTER_BOUND ( 'NONE', #186421, .T. ) ;
#159053 =( BOUNDED_SURFACE ( )  B_SPLINE_SURFACE ( 3, 2, ( 
 ( #201058, #224463, #142361 ),
 ( #1560, #141096, #221878 ),
 ( #122826, #163230, #202343 ),
 ( #43276, #45835, #83638 ) ),
 .UNSPECIFIED., .F., .F., .F. ) 
 B_SPLINE_SURFACE_WITH_KNOTS ( ( 4, 4 ),
 ( 3, 3 ),
 ( -3.469446951953614189E-18, 0.001979672783031532438 ),
 ( 0.000000000000000000, 1.000000000000000000 ),
 .UNSPECIFIED. ) 
 GEOMETRIC_REPRESENTATION_ITEM ( )  RATIONAL_B_SPLINE_SURFACE ( (
 ( 1.000000000000000000, 0.7103081912008384347, 1.000000000000000000),
 ( 1.000000000000000000, 0.7104998333558171231, 1.000000000000000000),
 ( 1.000000000000000000, 0.7107238315755857183, 1.000000000000000000),
 ( 1.000000000000000000, 0.7110073749538864396, 1.000000000000000000) ) ) 
 REPRESENTATION_ITEM ( '' )  SURFACE ( )  );
#159054 = CARTESIAN_POINT ( 'NONE',  ( -20.00857864376270001, 66.75000000001158185, -57.17310748452438673 ) ) ;
#159055 = CARTESIAN_POINT ( 'NONE',  ( -23.24999999999999645, -9.600000000000003197, -40.10018939122204529 ) ) ;
#159056 = ORIENTED_EDGE ( 'NONE', *, *, #250987, .F. ) ;
#159057 = DIRECTION ( 'NONE',  ( 0.000000000000000000, -6.938893903907222067E-15, 1.000000000000000000 ) ) ;
#159058 = APPLICATION_PROTOCOL_DEFINITION ( 'draft international standard', 'automotive_design', 1998, #243908 ) ;
#159059 = LINE ( 'NONE', #136898, #50602 ) ;
#159060 = VECTOR ( 'NONE', #28571, 1000.000000000000000 ) ;
#159061 = ORIENTED_EDGE ( 'NONE', *, *, #166495, .T. ) ;
#159062 = CARTESIAN_POINT ( 'NONE',  ( 20.94999999999999929, 74.93036000061670165, -233.6816308724374949 ) ) ;
#159063 = LINE ( 'NONE', #42944, #246653 ) ;
#159064 = CARTESIAN_POINT ( 'NONE',  ( 20.95512820512820440, 8.876151316299271343, -176.0586289951409071 ) ) ;
#159065 = ORIENTED_EDGE ( 'NONE', *, *, #1960, .F. ) ;
#159066 = EDGE_LOOP ( 'NONE', ( #51062, #42124, #237703, #68518 ) ) ;
#159067 = CARTESIAN_POINT ( 'NONE',  ( -22.39999999999999858, 76.00000000001203659, -114.6726782920691079 ) ) ;
#159068 = DIRECTION ( 'NONE',  ( 1.000000000000000000, 0.000000000000000000, 0.000000000000000000 ) ) ;
#159069 = DIRECTION ( 'NONE',  ( -0.7071067811865388020, 0.7071067811865561215, 0.000000000000000000 ) ) ;
#159070 = LINE ( 'NONE', #57353, #186047 ) ;
#159072 = CARTESIAN_POINT ( 'NONE',  ( 18.52928932188133970, 10.27928932189250055, -125.1500000000000341 ) ) ;
#159071 = CIRCLE ( 'NONE', #225657, 0.1000000000000056677 ) ;
#159074 = ADVANCED_FACE ( 'NONE', ( #42468 ), #26561, .T. ) ;
#159073 = TOROIDAL_SURFACE ( 'NONE', #79897, 7.800000000000000711, 0.1000000000000000056 ) ;
#159075 = DIRECTION ( 'NONE',  ( -0.7071067811865463515, -0.7071067811865487940, -4.937700262164540154E-15 ) ) ;
#159078 = DIRECTION ( 'NONE',  ( -1.000000000000000000, 0.000000000000000000, 0.000000000000000000 ) ) ;
#159077 = TOROIDAL_SURFACE ( 'NONE', #213196, 0.4000000000000009104, 0.1000000000000000056 ) ;
#159076 = CARTESIAN_POINT ( 'NONE',  ( -20.94999999999999929, 4.617781596423509605, -222.2029736859691980 ) ) ;
#159079 = DIRECTION ( 'NONE',  ( -0.000000000000000000, 0.2617529984165031243, 0.9651348961777157509 ) ) ;
#159080 = PLANE ( 'NONE',  #255870 ) ;
#159081 = CARTESIAN_POINT ( 'NONE',  ( 18.50211644919734866, 65.69792220476270472, -30.53355541284614816 ) ) ;
#159082 = CARTESIAN_POINT ( 'NONE',  ( -16.86578989773641979, 9.984809801269951990, -146.5353351133777835 ) ) ;
#159083 = ORIENTED_EDGE ( 'NONE', *, *, #14604, .T. ) ;
#159084 = VERTEX_POINT ( 'NONE', #179438 ) ;
#159085 = CARTESIAN_POINT ( 'NONE',  ( -23.15000000000000213, 86.19075908668452257, -209.4719249499869136 ) ) ;
#159087 = CARTESIAN_POINT ( 'NONE',  ( -23.15000000000000213, 64.35000000001249987, -177.0379132551783812 ) ) ;
#159086 = DIRECTION ( 'NONE',  ( 0.000000000000000000, 0.2617529984165152257, 0.9651348961777124202 ) ) ;
#159088 = DIRECTION ( 'NONE',  ( 1.000000000000000000, 0.000000000000000000, 0.000000000000000000 ) ) ;
#159089 = EDGE_CURVE ( 'NONE', #203821, #238502, #52658, .T. ) ;
#159090 = CARTESIAN_POINT ( 'NONE',  ( 18.49999999999999289, 69.55000000001223270, -148.2731074845243597 ) ) ;
#159091 = ORIENTED_EDGE ( 'NONE', *, *, #22064, .T. ) ;
#159092 = CARTESIAN_POINT ( 'NONE',  ( -23.25000000000000000, 1.115600667400684642E-11, -100.5000000000000426 ) ) ;
#159094 = ORIENTED_EDGE ( 'NONE', *, *, #161914, .F. ) ;
#159093 = VECTOR ( 'NONE', #244663, 1000.000000000000000 ) ;
#159095 = ADVANCED_FACE ( 'NONE', ( #745 ), #80281, .T. ) ;
#159096 = CARTESIAN_POINT ( 'NONE',  ( -16.94878442675512886, 51.63668200512650230, -231.8927611518110155 ) ) ;
#159097 = EDGE_LOOP ( 'NONE', ( #25155, #41569, #248605, #192221 ) ) ;
#159098 = CARTESIAN_POINT ( 'NONE',  ( -18.58735405345342073, -9.566478620325440829, -73.82271464626597890 ) ) ;
#159099 = EDGE_CURVE ( 'NONE', #135145, #17786, #194362, .T. ) ;
#159100 = CARTESIAN_POINT ( 'NONE',  ( 18.36493879433316323, 85.50000080620192477, -29.10095882417419944 ) ) ;
#159101 = ADVANCED_FACE ( 'NONE', ( #50166 ), #170179, .T. ) ;
#159102 = EDGE_CURVE ( 'NONE', #31603, #247198, #140141, .T. ) ;
#159103 = ORIENTED_EDGE ( 'NONE', *, *, #23974, .F. ) ;
#159104 = DIRECTION ( 'NONE',  ( -1.000000000000000000, 0.000000000000000000, 0.000000000000000000 ) ) ;
#159105 = TOROIDAL_SURFACE ( 'NONE', #242452, 0.4000000000000003553, 0.1000000000000000056 ) ;
#159106 = VERTEX_POINT ( 'NONE', #46313 ) ;
#159107 = EDGE_CURVE ( 'NONE', #59070, #17019, #248494, .T. ) ;
#159108 = CARTESIAN_POINT ( 'NONE',  ( 23.25000000000000000, -11.74999999999999112, -30.39999999999999858 ) ) ;
#159109 = CARTESIAN_POINT ( 'NONE',  ( 20.99142135623731065, 56.16603649944111254, -228.1013850343386196 ) ) ;
#159111 = CIRCLE ( 'NONE', #84194, 0.1000000000000028644 ) ;
#159110 = LINE ( 'NONE', #238623, #174171 ) ;
#159112 = CARTESIAN_POINT ( 'NONE',  ( -23.25000000000000000, 0.000000000000000000, -4.149999999999999467 ) ) ;
#159113 = CYLINDRICAL_SURFACE ( 'NONE', #89441, 0.09999999999999982514 ) ;
#159115 = CARTESIAN_POINT ( 'NONE',  ( 18.51697539158856998, 65.68434038414380893, -130.9866880726065688 ) ) ;
#159114 = CARTESIAN_POINT ( 'NONE',  ( 20.94999999999999929, -1.835341550213257733, -179.0551512925629538 ) ) ;
#159117 = ADVANCED_FACE ( 'NONE', ( #230099 ), #127151, .F. ) ;
#159116 = AXIS2_PLACEMENT_3D ( 'NONE', #169467, #108176, #186433 ) ;
#159119 = CARTESIAN_POINT ( 'NONE',  ( 17.74533788810829904, 65.18150020854140791, -146.8367301594720118 ) ) ;
#159118 = AXIS2_PLACEMENT_3D ( 'NONE', #210047, #52220, #13124 ) ;
#159120 = AXIS2_PLACEMENT_3D ( 'NONE', #194524, #57536, #176242 ) ;
#159122 = EDGE_LOOP ( 'NONE', ( #159330, #27705, #15241, #35459 ) ) ;
#159121 = CARTESIAN_POINT ( 'NONE',  ( 20.21567752745066215, 65.80188589878011385, -128.6404871368697229 ) ) ;
#159124 = DIRECTION ( 'NONE',  ( 0.000000000000000000, -1.000000000000000000, 0.000000000000000000 ) ) ;
#159123 = CARTESIAN_POINT ( 'NONE',  ( -18.54270223418609831, 38.05659262219499794, -261.2177875638973319 ) ) ;
#159125 = ORIENTED_EDGE ( 'NONE', *, *, #189455, .F. ) ;
#159127 = ORIENTED_EDGE ( 'NONE', *, *, #220382, .T. ) ;
#159126 = FACE_OUTER_BOUND ( 'NONE', #227894, .T. ) ;
#159128 = ORIENTED_EDGE ( 'NONE', *, *, #249335, .F. ) ;
#159129 = CARTESIAN_POINT ( 'NONE',  ( 21.05000000000000071, 69.65000000001262492, -193.6792853948412869 ) ) ;
#159130 = CIRCLE ( 'NONE', #84203, 0.09999999999999939493 ) ;
#159131 = CARTESIAN_POINT ( 'NONE',  ( -21.05000000000000071, -11.64999999998884306, -164.5000000000000000 ) ) ;
#159132 = CARTESIAN_POINT ( 'NONE',  ( -20.94999999999999929, 1.115600667400684642E-11, -167.5000000000000284 ) ) ;
#159133 = ORIENTED_EDGE ( 'NONE', *, *, #136688, .F. ) ;
#159134 = CARTESIAN_POINT ( 'NONE',  ( -20.85000000000000142, 7.021664781911246322, -104.3335654018973315 ) ) ;
#159135 = PLANE ( 'NONE',  #230641 ) ;
#159136 = FACE_OUTER_BOUND ( 'NONE', #147413, .T. ) ;
#159137 = VERTEX_POINT ( 'NONE', #29378 ) ;
#159138 = AXIS2_PLACEMENT_3D ( 'NONE', #80683, #175046, #234975 ) ;
#159140 = ADVANCED_FACE ( 'NONE', ( #110150 ), #206689, .F. ) ;
#159139 = DIRECTION ( 'NONE',  ( 2.915501640297155269E-16, -1.000000000000000000, 0.000000000000000000 ) ) ;
#159141 = AXIS2_PLACEMENT_3D ( 'NONE', #43545, #21431, #42258 ) ;
#159142 = DIRECTION ( 'NONE',  ( -1.000000000000000000, -0.000000000000000000, -0.000000000000000000 ) ) ;
#159143 = AXIS2_PLACEMENT_3D ( 'NONE', #182216, #205605, #105185 ) ;
#159144 = ORIENTED_EDGE ( 'NONE', *, *, #107179, .T. ) ;
#159145 = ORIENTED_EDGE ( 'NONE', *, *, #224276, .F. ) ;
#159146 = CYLINDRICAL_SURFACE ( 'NONE', #56200, 0.1000000000000075273 ) ;
#159147 = EDGE_LOOP ( 'NONE', ( #244215, #175823, #122248, #245741 ) ) ;
#159148 = DIRECTION ( 'NONE',  ( 0.000000000000000000, 0.000000000000000000, 1.000000000000000000 ) ) ;
#159149 = ORIENTED_EDGE ( 'NONE', *, *, #242490, .F. ) ;
#159150 = CARTESIAN_POINT ( 'NONE',  ( 20.94999999999999929, 10.29288807859936838, -172.9580020160121876 ) ) ;
#159152 =( BOUNDED_SURFACE ( )  B_SPLINE_SURFACE ( 3, 2, ( 
 ( #247581, #213579, #51919 ),
 ( #53231, #118008, #228021 ),
 ( #173229, #212327, #70262 ),
 ( #34992, #149792, #229313 ),
 ( #72826, #192754, #151058 ),
 ( #170667, #230596, #113202 ),
 ( #168090, #91075, #152362 ),
 ( #188893, #31143, #252697 ),
 ( #88478, #131482, #231892 ),
 ( #32421, #89776, #169373 ) ),
 .UNSPECIFIED., .F., .F., .F. ) 
 B_SPLINE_SURFACE_WITH_KNOTS ( ( 4, 2, 2, 2, 4 ),
 ( 3, 3 ),
 ( 0.0001836757140119128328, 0.0004000170051583585109, 0.0005081876507315813635, 0.0005622729735181927627, 0.0006163582963048041619 ),
 ( 0.000000000000000000, 1.000000000000000000 ),
 .UNSPECIFIED. ) 
 GEOMETRIC_REPRESENTATION_ITEM ( )  RATIONAL_B_SPLINE_SURFACE ( (
 ( 1.000000000000000000, 0.7071067811865475727, 1.000000000000000000),
 ( 1.000000000000000000, 0.6461995200029642117, 1.000000000000000000),
 ( 1.000000000000000000, 0.5776453529549738786, 1.000000000000000000),
 ( 1.000000000000000000, 0.4585233068351608487, 1.000000000000000000),
 ( 1.000000000000000000, 0.4154092989935744829, 1.000000000000000000),
 ( 1.000000000000000000, 0.3550093145838208453, 1.000000000000000000),
 ( 1.000000000000000000, 0.3354498651685166033, 1.000000000000000000),
 ( 1.000000000000000000, 0.3060347992257089755, 1.000000000000000000),
 ( 1.000000000000000000, 0.2963555829625726945, 1.000000000000000000),
 ( 1.000000000000000000, 0.2966190024560417804, 1.000000000000000000) ) ) 
 REPRESENTATION_ITEM ( '' )  SURFACE ( )  );
#159151 = CIRCLE ( 'NONE', #242315, 0.09999999999998898659 ) ;
#159153 = EDGE_CURVE ( 'NONE', #66665, #96344, #237674, .T. ) ;
#159154 = DIRECTION ( 'NONE',  ( 1.000000000000000000, -0.000000000000000000, 0.000000000000000000 ) ) ;
#159155 = CARTESIAN_POINT ( 'NONE',  ( -21.14999999999999858, 0.000000000000000000, 6.258578643762700011 ) ) ;
#159156 = AXIS2_PLACEMENT_3D ( 'NONE', #242196, #44002, #163961 ) ;
#159157 = CARTESIAN_POINT ( 'NONE',  ( 20.95000000000005258, 66.25000000001119815, -4.623107484524796362 ) ) ;
#159158 = CARTESIAN_POINT ( 'NONE',  ( -20.54999999999999716, 70.12557831835937350, -215.6322690948981915 ) ) ;
#159159 = CARTESIAN_POINT ( 'NONE',  ( -22.50000000000088463, 0.04536165659886851748, -88.84949116579235806 ) ) ;
#159160 = DIRECTION ( 'NONE',  ( 2.952720810173289112E-16, 0.9651348961777157509, -0.2617529984165031243 ) ) ;
#159161 = AXIS2_PLACEMENT_3D ( 'NONE', #106156, #185726, #7073 ) ;
#159162 = ORIENTED_EDGE ( 'NONE', *, *, #19825, .T. ) ;
#159164 = FACE_OUTER_BOUND ( 'NONE', #251209, .T. ) ;
#159163 = DIRECTION ( 'NONE',  ( 0.000000000000000000, -0.4930308989875170078, -0.8700118002898356018 ) ) ;
#159165 = CIRCLE ( 'NONE', #254757, 0.1000000000000024342 ) ;
#159166 = ORIENTED_EDGE ( 'NONE', *, *, #107989, .F. ) ;
#159169 = ORIENTED_EDGE ( 'NONE', *, *, #110517, .F. ) ;
#159168 = LINE ( 'NONE', #195727, #233609 ) ;
#159167 = CARTESIAN_POINT ( 'NONE',  ( -40.23850191057533010, 66.25000000001114131, -51.02310748452476474 ) ) ;
#159170 = AXIS2_PLACEMENT_3D ( 'NONE', #226084, #29245, #209113 ) ;
#159171 = ADVANCED_FACE ( 'NONE', ( #128436 ), #185835, .T. ) ;
#159172 = ORIENTED_EDGE ( 'NONE', *, *, #147089, .T. ) ;
#159173 = TOROIDAL_SURFACE ( 'NONE', #217378, 11.65000000000000036, 0.1000000000000000056 ) ;
#159174 = CARTESIAN_POINT ( 'NONE',  ( -18.59999999999999787, 76.00000000001267608, -203.5231074845243597 ) ) ;
#159175 = CARTESIAN_POINT ( 'NONE',  ( -20.54999999999999716, 76.00000000001185185, -90.04810748452430857 ) ) ;
#159176 = CARTESIAN_POINT ( 'NONE',  ( -16.83794237512074332, 9.926359221118628895, -113.3035421586989884 ) ) ;
#159177 = ORIENTED_EDGE ( 'NONE', *, *, #229119, .T. ) ;
#159178 = DIRECTION ( 'NONE',  ( -4.408576920032447355E-17, -0.1350103645451945777, 0.9908441862701589109 ) ) ;
#159180 = EDGE_CURVE ( 'NONE', #249547, #239889, #249675, .T. ) ;
#159179 = CARTESIAN_POINT ( 'NONE',  ( -21.14999999999999858, 76.10000000001203091, -114.6726782920691221 ) ) ;
#159181 = CARTESIAN_POINT ( 'NONE',  ( 22.10000000000000497, -11.75000000000000000, 12.09999999999999609 ) ) ;
#159183 = EDGE_LOOP ( 'NONE', ( #44315, #131948, #165418, #9856, #229256 ) ) ;
#159182 = DIRECTION ( 'NONE',  ( 0.000000000000000000, 0.000000000000000000, -1.000000000000000000 ) ) ;
#159184 = EDGE_CURVE ( 'NONE', #6953, #252227, #206801, .T. ) ;
#159185 = EDGE_CURVE ( 'NONE', #172105, #182409, #12366, .T. ) ;
#159186 = ORIENTED_EDGE ( 'NONE', *, *, #52203, .T. ) ;
#159187 = AXIS2_PLACEMENT_3D ( 'NONE', #33940, #13065, #55988 ) ;
#159188 = EDGE_CURVE ( 'NONE', #151298, #141855, #108047, .T. ) ;
#159189 = CARTESIAN_POINT ( 'NONE',  ( -16.92973740335530053, 44.06694468412165122, -235.2830613104084421 ) ) ;
#159190 = VERTEX_POINT ( 'NONE', #250929 ) ;
#159191 = ORIENTED_EDGE ( 'NONE', *, *, #93551, .F. ) ;
#159192 = ADVANCED_FACE ( 'NONE', ( #224947 ), #198428, .T. ) ;
#159193 = CARTESIAN_POINT ( 'NONE',  ( 20.85000000000000142, 42.92545512184477730, -254.1955779480491344 ) ) ;
#159194 = CARTESIAN_POINT ( 'NONE',  ( 21.14999999999999858, 30.68987205111126926, -252.2252246220829193 ) ) ;
#159195 = LINE ( 'NONE', #199604, #114101 ) ;
#159196 = ORIENTED_EDGE ( 'NONE', *, *, #203450, .F. ) ;
#159197 = FACE_OUTER_BOUND ( 'NONE', #78878, .T. ) ;
#159198 = DIRECTION ( 'NONE',  ( 1.836970198721029934E-16, -1.000000000000000000, -0.000000000000000000 ) ) ;
#159199 = EDGE_CURVE ( 'NONE', #172696, #112449, #94352, .T. ) ;
#159201 = EDGE_LOOP ( 'NONE', ( #186380, #53663, #58383, #133097 ) ) ;
#159200 = TOROIDAL_SURFACE ( 'NONE', #46740, 2.699999999999999734, 0.1000000000000000056 ) ;
#159202 = ORIENTED_EDGE ( 'NONE', *, *, #153434, .F. ) ;
#159203 = ORIENTED_EDGE ( 'NONE', *, *, #2280, .F. ) ;
#159204 = ORIENTED_EDGE ( 'NONE', *, *, #206297, .T. ) ;
#159206 = ORIENTED_EDGE ( 'NONE', *, *, #117720, .F. ) ;
#159205 = FACE_OUTER_BOUND ( 'NONE', #211908, .T. ) ;
#159207 = EDGE_CURVE ( 'NONE', #43971, #12920, #228831, .T. ) ;
#159208 = ADVANCED_FACE ( 'NONE', ( #233951 ), #117847, .F. ) ;
#159209 = ORIENTED_EDGE ( 'NONE', *, *, #255682, .F. ) ;
#159212 = VERTEX_POINT ( 'NONE', #54029 ) ;
#159211 = EDGE_LOOP ( 'NONE', ( #191548, #1777, #200734, #85008 ) ) ;
#159210 = DIRECTION ( 'NONE',  ( 0.000000000000000000, -1.000000000000000000, 0.000000000000000000 ) ) ;
#159213 = EDGE_CURVE ( 'NONE', #106026, #66961, #56732, .T. ) ;
#159214 = TOROIDAL_SURFACE ( 'NONE', #104977, 12.97499999999999609, 0.1000000000000000056 ) ;
#159215 = EDGE_LOOP ( 'NONE', ( #196750, #66147, #174138, #198390 ) ) ;
#159216 = CARTESIAN_POINT ( 'NONE',  ( -18.40000000000000213, 11.75000000001113953, -146.6500000000000341 ) ) ;
#159217 = DIRECTION ( 'NONE',  ( 1.000000000000000000, 0.000000000000000000, 0.000000000000000000 ) ) ;
#159218 = CIRCLE ( 'NONE', #209256, 0.09999999999999439892 ) ;
#159219 = CARTESIAN_POINT ( 'NONE',  ( -16.92280123533708647, 14.11630683194439051, -219.0590356125378548 ) ) ;
#159220 = ORIENTED_EDGE ( 'NONE', *, *, #114190, .T. ) ;
#159221 = CIRCLE ( 'NONE', #142781, 0.1000000000000028644 ) ;
#159222 = CYLINDRICAL_SURFACE ( 'NONE', #70641, 0.1000000000000000056 ) ;
#159224 = ORIENTED_EDGE ( 'NONE', *, *, #250324, .T. ) ;
#159223 = LINE ( 'NONE', #256964, #157669 ) ;
#159225 = DIRECTION ( 'NONE',  ( 0.000000000000000000, -1.000000000000000000, 0.000000000000000000 ) ) ;
#159227 = VERTEX_POINT ( 'NONE', #213101 ) ;
#159226 = DIRECTION ( 'NONE',  ( 0.000000000000000000, 0.1298341882520022694, 0.9915357197604852679 ) ) ;
#159228 = VERTEX_POINT ( 'NONE', #252219 ) ;
#159229 = CARTESIAN_POINT ( 'NONE',  ( 20.85000000000000142, 11.65000000001115943, -127.2161343370219413 ) ) ;
#159230 = EDGE_CURVE ( 'NONE', #63258, #66650, #44318, .T. ) ;
#159231 = AXIS2_PLACEMENT_3D ( 'NONE', #175591, #71362, #214692 ) ;
#159232 = TOROIDAL_SURFACE ( 'NONE', #209266, 0.2000000000000000111, 0.1000000000000000056 ) ;
#159233 = VERTEX_POINT ( 'NONE', #17469 ) ;
#159234 = ORIENTED_EDGE ( 'NONE', *, *, #226259, .F. ) ;
#159235 = CARTESIAN_POINT ( 'NONE',  ( -18.39999999999999858, -0.9152171842607024210, -242.2974985173726452 ) ) ;
#159236 = DIRECTION ( 'NONE',  ( 0.000000000000000000, 0.2128009952263485993, -0.9770955615653341697 ) ) ;
#159238 = ORIENTED_EDGE ( 'NONE', *, *, #177492, .F. ) ;
#159237 = ORIENTED_EDGE ( 'NONE', *, *, #20523, .T. ) ;
#159239 = VERTEX_POINT ( 'NONE', #176567 ) ;
#159240 = CARTESIAN_POINT ( 'NONE',  ( 18.49999999999999289, 64.25000000001207923, -128.4231074845243654 ) ) ;
#159241 = ORIENTED_EDGE ( 'NONE', *, *, #248653, .T. ) ;
#159242 = VERTEX_POINT ( 'NONE', #115286 ) ;
#159243 = CARTESIAN_POINT ( 'NONE',  ( 20.94999999999999929, -9.499999999988844479, -90.60603087734760663 ) ) ;
#159244 = EDGE_LOOP ( 'NONE', ( #23408, #8543, #166324, #58732 ) ) ;
#159245 = CARTESIAN_POINT ( 'NONE',  ( -16.93658211146646408, 12.44557776047770581, -211.1804511121877965 ) ) ;
#159247 = FACE_OUTER_BOUND ( 'NONE', #66515, .T. ) ;
#159246 = DIRECTION ( 'NONE',  ( 0.000000000000000000, 0.000000000000000000, -1.000000000000000000 ) ) ;
#159248 = EDGE_LOOP ( 'NONE', ( #5183, #237718, #77350, #26438 ) ) ;
#159249 = EDGE_CURVE ( 'NONE', #163131, #105444, #148549, .T. ) ;
#159250 = CIRCLE ( 'NONE', #109138, 0.09999999999999939493 ) ;
#159252 = ORIENTED_EDGE ( 'NONE', *, *, #241203, .F. ) ;
#159251 = VERTEX_POINT ( 'NONE', #177853 ) ;
#159253 = VECTOR ( 'NONE', #138492, 1000.000000000000000 ) ;
#159254 = DIRECTION ( 'NONE',  ( -0.000000000000000000, 1.000000000000000000, -0.000000000000000000 ) ) ;
#159255 = DIRECTION ( 'NONE',  ( 0.000000000000000000, 0.000000000000000000, -1.000000000000000000 ) ) ;
#159256 = EDGE_CURVE ( 'NONE', #65925, #14799, #133568, .T. ) ;
#159257 = ORIENTED_EDGE ( 'NONE', *, *, #610, .F. ) ;
#159258 = ADVANCED_FACE ( 'NONE', ( #174026 ), #134669, .T. ) ;
#159259 = DIRECTION ( 'NONE',  ( 1.000000000000000000, 0.000000000000000000, 0.000000000000000000 ) ) ;
#159260 = EDGE_CURVE ( 'NONE', #190837, #226215, #153660, .T. ) ;
#159261 = ORIENTED_EDGE ( 'NONE', *, *, #130032, .F. ) ;
#159262 = EDGE_LOOP ( 'NONE', ( #148411, #102949, #213191, #255674, #228501 ) ) ;
#159263 = DIRECTION ( 'NONE',  ( 1.186688945009010077E-16, -1.000000000000000000, -0.000000000000000000 ) ) ;
#159264 = ORIENTED_EDGE ( 'NONE', *, *, #118928, .F. ) ;
#159265 = FACE_OUTER_BOUND ( 'NONE', #37910, .T. ) ;
#159266 = FACE_OUTER_BOUND ( 'NONE', #202626, .T. ) ;
#159267 = ORIENTED_EDGE ( 'NONE', *, *, #19921, .F. ) ;
#159268 = DIRECTION ( 'NONE',  ( 0.000000000000000000, 0.000000000000000000, 1.000000000000000000 ) ) ;
#159269 = CARTESIAN_POINT ( 'NONE',  ( -17.78241384941079062, 10.85557575279146469, -43.74903767243881703 ) ) ;
#159270 = CARTESIAN_POINT ( 'NONE',  ( -23.15000000000000213, 68.76258920191057200, -222.5680764032308048 ) ) ;
#159271 = FACE_OUTER_BOUND ( 'NONE', #142458, .T. ) ;
#159272 = DIRECTION ( 'NONE',  ( 0.000000000000000000, 0.9126074666063771490, 0.4088369013363281623 ) ) ;
#159273 = DIRECTION ( 'NONE',  ( -1.000000000000000000, 0.000000000000000000, 0.000000000000000000 ) ) ;
#159274 = LINE ( 'NONE', #167000, #253004 ) ;
#159275 = CARTESIAN_POINT ( 'NONE',  ( 16.87683809663750267, 66.05000000001207638, -123.8731074845243683 ) ) ;
#159276 = CARTESIAN_POINT ( 'NONE',  ( 20.94999999999999574, 4.184122562697137226, -245.3714803909117279 ) ) ;
#159277 = ORIENTED_EDGE ( 'NONE', *, *, #186929, .F. ) ;
#159278 = AXIS2_PLACEMENT_3D ( 'NONE', #190381, #112130, #230792 ) ;
#159279 = EDGE_CURVE ( 'NONE', #132550, #102379, #37069, .T. ) ;
#159280 = ADVANCED_FACE ( 'NONE', ( #197384 ), #18752, .F. ) ;
#159282 = ORIENTED_EDGE ( 'NONE', *, *, #238083, .F. ) ;
#159281 = EDGE_LOOP ( 'NONE', ( #215828, #69962, #114669, #234096 ) ) ;
#159283 = ORIENTED_EDGE ( 'NONE', *, *, #99034, .T. ) ;
#159284 = ORIENTED_EDGE ( 'NONE', *, *, #39434, .F. ) ;
#159285 = DIRECTION ( 'NONE',  ( 0.000000000000000000, 0.9915357197604804940, -0.1298341882520397950 ) ) ;
#159286 = CIRCLE ( 'NONE', #238363, 0.09999999999999939493 ) ;
#159287 = DIRECTION ( 'NONE',  ( 0.000000000000000000, -1.000000000000000000, -6.982962677686265922E-15 ) ) ;
#159289 = CARTESIAN_POINT ( 'NONE',  ( 18.59999999999998366, 76.00000000001213607, -136.5231074845243313 ) ) ;
#159288 = CARTESIAN_POINT ( 'NONE',  ( 18.49999999999999289, 21.76214302935564859, -245.0385711982110877 ) ) ;
#159290 = DIRECTION ( 'NONE',  ( 0.000000000000000000, 0.01562500000001045344, 0.9998779222360096863 ) ) ;
#159291 = ORIENTED_EDGE ( 'NONE', *, *, #3776, .F. ) ;
#159292 = AXIS2_PLACEMENT_3D ( 'NONE', #64709, #47698, #8592 ) ;
#159293 = CARTESIAN_POINT ( 'NONE',  ( -23.25000000000000355, 70.35000000001153353, -48.67310748452436542 ) ) ;
#159294 = ADVANCED_FACE ( 'NONE', ( #142542 ), #160856, .F. ) ;
#159295 = DIRECTION ( 'NONE',  ( -0.000000000000000000, -6.982962677686266711E-15, 1.000000000000000000 ) ) ;
#159296 = CIRCLE ( 'NONE', #225874, 11.64999999999999325 ) ;
#159297 = DIRECTION ( 'NONE',  ( -3.469446951953749873E-14, 0.4088369013363783999, -0.9126074666063545004 ) ) ;
#159298 = CIRCLE ( 'NONE', #13542, 4.150000000000001243 ) ;
#159299 = VECTOR ( 'NONE', #194219, 1000.000000000000000 ) ;
#159300 = EDGE_CURVE ( 'NONE', #213068, #83513, #219427, .T. ) ;
#159301 = CARTESIAN_POINT ( 'NONE',  ( 18.59999999999999076, 65.50857864377418593, -44.77310748452440237 ) ) ;
#159302 = VERTEX_POINT ( 'NONE', #219511 ) ;
#159303 = DIRECTION ( 'NONE',  ( 0.000000000000000000, -0.9910827722268055195, 0.1332476588733540468 ) ) ;
#159304 = AXIS2_PLACEMENT_3D ( 'NONE', #151124, #113269, #230661 ) ;
#159305 = DIRECTION ( 'NONE',  ( -1.000000000000000000, 0.000000000000000000, 0.000000000000000000 ) ) ;
#159306 = VERTEX_POINT ( 'NONE', #202530 ) ;
#159307 = DIRECTION ( 'NONE',  ( -5.603264701231743991E-32, 1.897661533703519897E-16, -1.000000000000000000 ) ) ;
#159308 = CARTESIAN_POINT ( 'NONE',  ( 21.05000000000000071, 76.00000000001145395, -38.92310748452432279 ) ) ;
#159309 = ADVANCED_FACE ( 'NONE', ( #220805 ), #42186, .T. ) ;
#159310 = CARTESIAN_POINT ( 'NONE',  ( 18.59999999999999787, -1.362429037182151470, -175.3888812479212334 ) ) ;
#159311 = DIRECTION ( 'NONE',  ( 0.000000000000000000, -0.2617529984165024026, -0.9651348961777158619 ) ) ;
#159312 = DIRECTION ( 'NONE',  ( 1.000000000000000000, 0.000000000000000000, 0.000000000000000000 ) ) ;
#159313 = ORIENTED_EDGE ( 'NONE', *, *, #196238, .T. ) ;
#159314 = DIRECTION ( 'NONE',  ( 1.000000000000000000, 0.000000000000000000, 0.000000000000000000 ) ) ;
#159315 = DIRECTION ( 'NONE',  ( -0.7071067811865388020, 0.7071067811865561215, 0.000000000000000000 ) ) ;
#159316 = TOROIDAL_SURFACE ( 'NONE', #163396, 0.2000000000000000111, 0.1000000000000000056 ) ;
#159318 = FACE_OUTER_BOUND ( 'NONE', #103095, .T. ) ;
#159317 = CARTESIAN_POINT ( 'NONE',  ( -23.25000000000000000, 11.75000000000000000, -12.15000000000000036 ) ) ;
#159319 = CARTESIAN_POINT ( 'NONE',  ( 18.39999999999998082, 11.47316190337362585, -176.7499999999999716 ) ) ;
#159322 = ADVANCED_FACE ( 'NONE', ( #3026 ), #211082, .F. ) ;
#159321 = CARTESIAN_POINT ( 'NONE',  ( 21.07946286933444924, 0.07668384326756222391, -27.17096268099230372 ) ) ;
#159320 = CIRCLE ( 'NONE', #42584, 7.899999999999990585 ) ;
#159323 = AXIS2_PLACEMENT_3D ( 'NONE', #157703, #102782, #177251 ) ;
#159324 = DIRECTION ( 'NONE',  ( -1.000000000000000000, -0.000000000000000000, -0.000000000000000000 ) ) ;
#159325 = DIRECTION ( 'NONE',  ( -1.000000000000000000, 0.000000000000000000, 0.000000000000000000 ) ) ;
#159326 = VECTOR ( 'NONE', #188212, 1000.000000000000000 ) ;
#159327 = EDGE_LOOP ( 'NONE', ( #122729, #115943, #123981 ) ) ;
#159328 = AXIS2_PLACEMENT_3D ( 'NONE', #96903, #61670, #79909 ) ;
#159329 = CIRCLE ( 'NONE', #192628, 0.09999999999999939493 ) ;
#159330 = ORIENTED_EDGE ( 'NONE', *, *, #47586, .T. ) ;
#159331 = EDGE_LOOP ( 'NONE', ( #102759, #244452, #104424, #232453 ) ) ;
#159332 = EDGE_CURVE ( 'NONE', #115296, #164855, #152855, .T. ) ;
#159333 = CIRCLE ( 'NONE', #146814, 0.09999999999998898659 ) ;
#159334 = CYLINDRICAL_SURFACE ( 'NONE', #225980, 0.09999999999999939493 ) ;
#159335 =( LENGTH_UNIT ( ) NAMED_UNIT ( * ) SI_UNIT ( .MILLI., .METRE. ) );
#159336 = CARTESIAN_POINT ( 'NONE',  ( -21.05000000000000071, 76.00000000001165290, -69.52310748452431710 ) ) ;
#159337 = CARTESIAN_POINT ( 'NONE',  ( 20.04142135623730070, 61.54970422893870818, -212.2965875311496688 ) ) ;
#159338 = AXIS2_PLACEMENT_3D ( 'NONE', #77560, #115425, #136250 ) ;
#159339 = EDGE_LOOP ( 'NONE', ( #123804, #255370, #1070, #43094 ) ) ;
#159341 = CARTESIAN_POINT ( 'NONE',  ( 21.05000000000000071, 67.22371710471946926, -103.0231074845243739 ) ) ;
#159340 = AXIS2_PLACEMENT_3D ( 'NONE', #247177, #105067, #142928 ) ;
#159342 = DIRECTION ( 'NONE',  ( 0.000000000000000000, -0.9126074666063771490, -0.4088369013363281623 ) ) ;
#159343 = CARTESIAN_POINT ( 'NONE',  ( -18.50000000000000000, 65.70711192142367452, -97.56510546851220056 ) ) ;
#159344 = CYLINDRICAL_SURFACE ( 'NONE', #66191, 14.30833333333333890 ) ;
#159346 = VERTEX_POINT ( 'NONE', #21354 ) ;
#159345 = CARTESIAN_POINT ( 'NONE',  ( -16.92280123533721792, 9.950000000011137047, -188.1493676859139157 ) ) ;
#159348 = CARTESIAN_POINT ( 'NONE',  ( -18.41431012584569515, 11.48747202921932775, -158.2732360131017231 ) ) ;
#159347 = DIRECTION ( 'NONE',  ( 0.000000000000000000, 0.000000000000000000, 1.000000000000000000 ) ) ;
#159349 = CARTESIAN_POINT ( 'NONE',  ( -20.65000000000000568, 7.250000000011138646, -176.7499999999999716 ) ) ;
#159350 =( NAMED_UNIT ( * ) SI_UNIT ( $, .STERADIAN. ) SOLID_ANGLE_UNIT ( ) );
#159351 = ORIENTED_EDGE ( 'NONE', *, *, #64909, .F. ) ;
#159352 = DIRECTION ( 'NONE',  ( 0.000000000000000000, 0.000000000000000000, 1.000000000000000000 ) ) ;
#159353 = DIRECTION ( 'NONE',  ( 0.000000000000000000, -0.1575844902526687130, -0.9875055080513762684 ) ) ;
#159354 = CARTESIAN_POINT ( 'NONE',  ( 21.97500000000000497, 66.25000000001179501, -81.87310748452438247 ) ) ;
#159355 = EDGE_LOOP ( 'NONE', ( #207074, #50017, #247359 ) ) ;
#159356 = CARTESIAN_POINT ( 'NONE',  ( -21.44999999999999929, 7.349999999999998757, -21.25000000000000000 ) ) ;
#159357 = DIRECTION ( 'NONE',  ( 0.000000000000000000, -6.982962677686266711E-15, 1.000000000000000000 ) ) ;
#159358 = AXIS2_PLACEMENT_3D ( 'NONE', #120808, #21691, #240736 ) ;
#159359 = ORIENTED_EDGE ( 'NONE', *, *, #107275, .F. ) ;
#159360 = CARTESIAN_POINT ( 'NONE',  ( 22.50000000000000000, -3.092988775432913506, -228.1437074281570858 ) ) ;
#159361 = AXIS2_PLACEMENT_3D ( 'NONE', #158131, #235063, #282 ) ;
#159362 = CARTESIAN_POINT ( 'NONE',  ( 20.85000000000000142, -0.3238857010591806307, -133.9575895893140398 ) ) ;
#159363 = DIRECTION ( 'NONE',  ( 0.000000000000000000, 0.000000000000000000, 1.000000000000000000 ) ) ;
#159364 = EDGE_LOOP ( 'NONE', ( #2716, #194722, #114994, #150515 ) ) ;
#159365 = ORIENTED_EDGE ( 'NONE', *, *, #60620, .T. ) ;
#159366 = CARTESIAN_POINT ( 'NONE',  ( -1.820710678118657944, 63.30541909908242104, -248.4939929664152203 ) ) ;
#159367 = DIRECTION ( 'NONE',  ( -0.000000000000000000, -1.000000000000000000, -6.982962677686266711E-15 ) ) ;
#159368 = DIRECTION ( 'NONE',  ( 0.000000000000000000, 0.000000000000000000, 1.000000000000000000 ) ) ;
#159369 = EDGE_CURVE ( 'NONE', #973, #92460, #143825, .T. ) ;
#159371 = CARTESIAN_POINT ( 'NONE',  ( 19.92426406871192412, 64.25000000001250555, -178.6731074845244507 ) ) ;
#159370 = DIRECTION ( 'NONE',  ( 0.000000000000000000, 0.9126074666063660468, 0.4088369013363524762 ) ) ;
#159372 = CARTESIAN_POINT ( 'NONE',  ( -18.59999999999999787, 25.65398771707549841, -256.3298696899526021 ) ) ;
#159373 = DIRECTION ( 'NONE',  ( 0.000000000000000000, 1.000000000000000000, 6.982962677686266711E-15 ) ) ;
#159374 = CARTESIAN_POINT ( 'NONE',  ( -20.94999999999999929, 7.021664781911246322, -70.83356540189728889 ) ) ;
#159375 = ORIENTED_EDGE ( 'NONE', *, *, #206587, .T. ) ;
#159376 = DIRECTION ( 'NONE',  ( -0.7071067811865487940, 0.7071067811865463515, 0.000000000000000000 ) ) ;
#159377 = AXIS2_PLACEMENT_3D ( 'NONE', #207839, #209087, #231240 ) ;
#159379 = ORIENTED_EDGE ( 'NONE', *, *, #114715, .T. ) ;
#159378 = DIRECTION ( 'NONE',  ( 0.000000000000000000, 0.000000000000000000, 1.000000000000000000 ) ) ;
#159380 = DIRECTION ( 'NONE',  ( 0.000000000000000000, -0.3738317757009225195, 0.9274965247785541544 ) ) ;
#159381 = CARTESIAN_POINT ( 'NONE',  ( 22.49999999999999645, 11.36403278914770176, -198.4341430231427807 ) ) ;
#159383 = DIRECTION ( 'NONE',  ( 0.000000000000000000, -1.000000000000000000, -6.982962677686266711E-15 ) ) ;
#159382 = LINE ( 'NONE', #74738, #250907 ) ;
#159384 = VERTEX_POINT ( 'NONE', #61736 ) ;
#159386 = DIRECTION ( 'NONE',  ( 0.000000000000000000, -0.000000000000000000, 1.000000000000000000 ) ) ;
#159385 = DIRECTION ( 'NONE',  ( -1.000000000000000000, -0.000000000000000000, -0.000000000000000000 ) ) ;
#159387 = DIRECTION ( 'NONE',  ( 0.000000000000000000, 0.000000000000000000, -1.000000000000000000 ) ) ;
#159388 = DIRECTION ( 'NONE',  ( 1.000000000000000000, 0.000000000000000000, 0.000000000000000000 ) ) ;
#159389 = DIRECTION ( 'NONE',  ( 1.000000000000000000, 0.000000000000000000, 0.000000000000000000 ) ) ;
#159390 = CARTESIAN_POINT ( 'NONE',  ( -1.739115166359751801E-14, 64.35000000001200249, -115.1731074845243796 ) ) ;
#159391 = ORIENTED_EDGE ( 'NONE', *, *, #13825, .T. ) ;
#159392 = LINE ( 'NONE', #238920, #155501 ) ;
#159394 = EDGE_CURVE ( 'NONE', #109277, #191054, #182043, .T. ) ;
#159393 = EDGE_LOOP ( 'NONE', ( #219272, #173062, #176219, #36067 ) ) ;
#159396 = CIRCLE ( 'NONE', #42855, 11.64999999999998970 ) ;
#159395 = CARTESIAN_POINT ( 'NONE',  ( 21.05000000000000071, 0.09779029131994770863, -127.7421853895238968 ) ) ;
#159397 = ORIENTED_EDGE ( 'NONE', *, *, #14181, .F. ) ;
#159398 = FACE_OUTER_BOUND ( 'NONE', #194439, .T. ) ;
#159399 = EDGE_LOOP ( 'NONE', ( #19142, #186826, #28514, #16607 ) ) ;
#159400 = CIRCLE ( 'NONE', #5412, 0.1000000000000028644 ) ;
#159401 = DIRECTION ( 'NONE',  ( 0.000000000000000000, -0.1568667991644863147, -0.9876197685951252359 ) ) ;
#159402 = VECTOR ( 'NONE', #57626, 1000.000000000000000 ) ;
#159403 = EDGE_CURVE ( 'NONE', #106574, #142904, #40431, .T. ) ;
#159405 = EDGE_CURVE ( 'NONE', #78560, #13712, #22633, .T. ) ;
#159404 = CARTESIAN_POINT ( 'NONE',  ( -18.50000000000000000, 66.75000000001179501, -81.77310748452437394 ) ) ;
#159406 = ORIENTED_EDGE ( 'NONE', *, *, #134402, .F. ) ;
#159407 = EDGE_CURVE ( 'NONE', #66243, #208701, #131964, .T. ) ;
#159408 = CARTESIAN_POINT ( 'NONE',  ( -16.81453563122428818, 9.939100205448113456, -87.78825866064536854 ) ) ;
#159409 = CARTESIAN_POINT ( 'NONE',  ( -18.46907102845852577, -9.473727364752955182, -174.1760347387365471 ) ) ;
#159410 = DIRECTION ( 'NONE',  ( -0.000000000000000000, 0.9770955615653315052, 0.2128009952263602844 ) ) ;
#159411 = AXIS2_PLACEMENT_3D ( 'NONE', #214393, #213107, #231405 ) ;
#159412 = CIRCLE ( 'NONE', #76168, 0.09999999999999789613 ) ;
#159413 = DIRECTION ( 'NONE',  ( -1.000000000000000000, -0.000000000000000000, 0.000000000000000000 ) ) ;
#159414 = DIRECTION ( 'NONE',  ( 1.000000000000000000, -0.000000000000000000, -0.000000000000000000 ) ) ;
#159415 = EDGE_CURVE ( 'NONE', #43374, #231379, #103403, .T. ) ;
#159416 = CARTESIAN_POINT ( 'NONE',  ( 20.01093837587850288, 62.37047727546982401, -208.8881959771026686 ) ) ;
#159417 = ORIENTED_EDGE ( 'NONE', *, *, #32555, .T. ) ;
#159418 = CARTESIAN_POINT ( 'NONE',  ( -21.05000000000000071, 74.16465844978787914, -158.4679561919613775 ) ) ;
#159419 = EDGE_LOOP ( 'NONE', ( #155664, #60247 ) ) ;
#159421 = ORIENTED_EDGE ( 'NONE', *, *, #83808, .F. ) ;
#159420 = DIRECTION ( 'NONE',  ( 0.000000000000000000, -0.1350103645451807555, -0.9908441862701610203 ) ) ;
#159422 = EDGE_LOOP ( 'NONE', ( #209481, #136751, #119308, #144070 ) ) ;
#159423 = DIRECTION ( 'NONE',  ( -1.000000000000000000, -0.000000000000000000, -0.000000000000000000 ) ) ;
#159425 = ADVANCED_FACE ( 'NONE', ( #162142 ), #241656, .F. ) ;
#159424 = DIRECTION ( 'NONE',  ( 0.000000000000000000, 0.9651348961777118651, -0.2617529984165174461 ) ) ;
#159426 = CARTESIAN_POINT ( 'NONE',  ( 15.52844286134409124, 66.62433047358679516, -187.6553174751384745 ) ) ;
#159427 = CARTESIAN_POINT ( 'NONE',  ( 21.06089410995839728, 60.07392730735723063, -221.2708047820654826 ) ) ;
#159428 = VECTOR ( 'NONE', #254347, 1000.000000000000227 ) ;
#159429 = CARTESIAN_POINT ( 'NONE',  ( 23.25000000000000000, 87.65000000001275282, -215.2731074845242745 ) ) ;
#159430 = ORIENTED_EDGE ( 'NONE', *, *, #50486, .T. ) ;
#159431 = CYLINDRICAL_SURFACE ( 'NONE', #159715, 0.1000000000000028644 ) ;
#159432 = CARTESIAN_POINT ( 'NONE',  ( 18.49999999999999289, 10.24999999999999822, -21.35000000000000142 ) ) ;
#159433 = AXIS2_PLACEMENT_3D ( 'NONE', #66004, #46430, #110257 ) ;
#159435 = ORIENTED_EDGE ( 'NONE', *, *, #197409, .T. ) ;
#159434 = CARTESIAN_POINT ( 'NONE',  ( 21.13461538461538325, 8.885417037985616773, -79.35000000000005116 ) ) ;
#159436 = VECTOR ( 'NONE', #196640, 999.9999999999998863 ) ;
#159437 = AXIS2_PLACEMENT_3D ( 'NONE', #173864, #254601, #238924 ) ;
#159439 = ADVANCED_FACE ( 'NONE', ( #83821 ), #100814, .F. ) ;
#159438 = CARTESIAN_POINT ( 'NONE',  ( -20.94788355080264353, 10.30207779524867462, -38.98955207167824000 ) ) ;
#159440 = AXIS2_PLACEMENT_3D ( 'NONE', #66244, #221433, #41568 ) ;
#159441 = CARTESIAN_POINT ( 'NONE',  ( -16.87333278164142314, 9.882609784590052016, -80.13316780615271284 ) ) ;
#159442 = ORIENTED_EDGE ( 'NONE', *, *, #220678, .T. ) ;
#159443 = DIRECTION ( 'NONE',  ( 0.000000000000000000, 0.000000000000000000, 1.000000000000000000 ) ) ;
#159444 = ORIENTED_EDGE ( 'NONE', *, *, #212283, .T. ) ;
#159445 = CARTESIAN_POINT ( 'NONE',  ( -17.78043020864320667, 10.85359211201683927, -177.8369508342797474 ) ) ;
#159446 = CARTESIAN_POINT ( 'NONE',  ( 21.04999999999999716, 6.304455821958825368, -134.0210354765401348 ) ) ;
#159447 = DIRECTION ( 'NONE',  ( 0.000000000000000000, -1.000000000000000000, -6.352154140967427193E-15 ) ) ;
#159448 = CARTESIAN_POINT ( 'NONE',  ( 21.05000000000000071, 84.73084112150795022, -193.9250327655399531 ) ) ;
#159449 = ORIENTED_EDGE ( 'NONE', *, *, #131290, .F. ) ;
#159450 = EDGE_CURVE ( 'NONE', #105637, #77397, #141147, .T. ) ;
#159451 = EDGE_CURVE ( 'NONE', #229756, #46556, #194538, .T. ) ;
#159452 = ORIENTED_EDGE ( 'NONE', *, *, #18426, .F. ) ;
#159453 = CARTESIAN_POINT ( 'NONE',  ( -22.39999999999999858, -0.1008583690875579364, -21.75043287651061164 ) ) ;
#159454 = CIRCLE ( 'NONE', #46997, 0.09999999999999961697 ) ;
#159456 = VERTEX_POINT ( 'NONE', #134215 ) ;
#159455 = DIRECTION ( 'NONE',  ( -1.000000000000000000, 4.625929269271478222E-14, 0.000000000000000000 ) ) ;
#159458 = EDGE_CURVE ( 'NONE', #244808, #127337, #256812, .T. ) ;
#159457 = CARTESIAN_POINT ( 'NONE',  ( 19.58285714285715073, 40.65800978083061779, -237.8813314257687352 ) ) ;
#159460 = EDGE_CURVE ( 'NONE', #191879, #141200, #244387, .T. ) ;
#159459 = CARTESIAN_POINT ( 'NONE',  ( -23.15000000000000213, 1.115600667400684642E-11, -33.50000000000000000 ) ) ;
#159461 = CARTESIAN_POINT ( 'NONE',  ( -16.81453046979149235, 9.939102281452072418, -79.71172652360306188 ) ) ;
#159462 = AXIS2_PLACEMENT_3D ( 'NONE', #172224, #174790, #14410 ) ;
#159463 = DIRECTION ( 'NONE',  ( 0.9880948137434723000, -0.1538461538461484146, -1.074301950413233906E-15 ) ) ;
#159464 = CARTESIAN_POINT ( 'NONE',  ( -21.55000000000000071, 63.34400729675436281, -222.1083394899400503 ) ) ;
#159466 = ORIENTED_EDGE ( 'NONE', *, *, #122767, .T. ) ;
#159465 = DIRECTION ( 'NONE',  ( -1.073024830501117725E-15, -6.982962677686266711E-15, 1.000000000000000000 ) ) ;
#159467 = CIRCLE ( 'NONE', #242843, 0.09999999999999939493 ) ;
#159468 = ADVANCED_FACE ( 'NONE', ( #33901 ), #246782, .T. ) ;
#159469 = TOROIDAL_SURFACE ( 'NONE', #155218, 0.2000000000000000111, 0.1000000000000000056 ) ;
#159470 = CIRCLE ( 'NONE', #197036, 11.65000000000000213 ) ;
#159471 = EDGE_CURVE ( 'NONE', #156063, #53590, #136206, .T. ) ;
#159473 = ADVANCED_FACE ( 'NONE', ( #29073 ), #14315, .T. ) ;
#159472 = ADVANCED_FACE ( 'NONE', ( #206389 ), #227224, .T. ) ;
#159474 = CIRCLE ( 'NONE', #5310, 0.1000000000000028644 ) ;
#159475 = DIRECTION ( 'NONE',  ( 1.000000000000000000, -0.000000000000000000, -0.000000000000000000 ) ) ;
#159476 = VERTEX_POINT ( 'NONE', #27781 ) ;
#159477 = VERTEX_POINT ( 'NONE', #107276 ) ;
#159478 = EDGE_CURVE ( 'NONE', #239027, #112332, #124788, .T. ) ;
#159479 = DIRECTION ( 'NONE',  ( -0.000000000000000000, 0.9274965247785350586, 0.3738317757009704811 ) ) ;
#159480 = LINE ( 'NONE', #35700, #93071 ) ;
#159481 = AXIS2_PLACEMENT_3D ( 'NONE', #136170, #106040, #1813 ) ;
#159482 = ORIENTED_EDGE ( 'NONE', *, *, #26803, .T. ) ;
#159483 = CARTESIAN_POINT ( 'NONE',  ( -23.25000000000000355, 11.75000000001113953, -188.3499999999999659 ) ) ;
#159484 = VECTOR ( 'NONE', #198142, 1000.000000000000000 ) ;
#159485 = EDGE_CURVE ( 'NONE', #18097, #190202, #19558, .T. ) ;
#159486 = CARTESIAN_POINT ( 'NONE',  ( -18.45037301276633812, 85.49020044755350511, -62.51043334810935193 ) ) ;
#159487 = AXIS2_PLACEMENT_3D ( 'NONE', #97231, #77693, #59393 ) ;
#159488 = ORIENTED_EDGE ( 'NONE', *, *, #149765, .F. ) ;
#159489 = EDGE_CURVE ( 'NONE', #176630, #45783, #73013, .T. ) ;
#159490 = ADVANCED_FACE ( 'NONE', ( #186836 ), #9463, .T. ) ;
#159491 = DIRECTION ( 'NONE',  ( -1.000000000000000000, -0.000000000000000000, -0.000000000000000000 ) ) ;
#159492 = VECTOR ( 'NONE', #15538, 999.9999999999998863 ) ;
#159493 = AXIS2_PLACEMENT_3D ( 'NONE', #76272, #22760, #141386 ) ;
#159495 = AXIS2_PLACEMENT_3D ( 'NONE', #73229, #234841, #37944 ) ;
#159494 = CARTESIAN_POINT ( 'NONE',  ( 21.05000000000000071, 71.18691588786276725, -158.0815897280005800 ) ) ;
#159496 = EDGE_CURVE ( 'NONE', #191837, #201531, #231946, .T. ) ;
#159497 = ORIENTED_EDGE ( 'NONE', *, *, #173420, .T. ) ;
#159498 = EDGE_LOOP ( 'NONE', ( #55537, #121667, #138695, #143164 ) ) ;
#159499 = CARTESIAN_POINT ( 'NONE',  ( -20.07928932188135107, 63.86812082655664113, -213.0289747847910462 ) ) ;
#159500 = ORIENTED_EDGE ( 'NONE', *, *, #248670, .T. ) ;
#159501 = DIRECTION ( 'NONE',  ( 0.000000000000000000, 0.000000000000000000, -1.000000000000000000 ) ) ;
#159503 = ORIENTED_EDGE ( 'NONE', *, *, #245246, .F. ) ;
#159502 = DIRECTION ( 'NONE',  ( 0.000000000000000000, 0.000000000000000000, 1.000000000000000000 ) ) ;
#159504 = EDGE_CURVE ( 'NONE', #191668, #167725, #119437, .T. ) ;
#159505 = ADVANCED_FACE ( 'NONE', ( #225910 ), #8198, .T. ) ;
#159506 = DIRECTION ( 'NONE',  ( 0.000000000000000000, -0.8814952561688430555, 0.4721928772777346239 ) ) ;
#159507 = ORIENTED_EDGE ( 'NONE', *, *, #193021, .T. ) ;
#159508 = DIRECTION ( 'NONE',  ( 1.000000000000000000, -0.000000000000000000, -0.000000000000000000 ) ) ;
#159509 = ORIENTED_EDGE ( 'NONE', *, *, #149297, .F. ) ;
#159511 = ORIENTED_EDGE ( 'NONE', *, *, #255913, .T. ) ;
#159510 = ORIENTED_EDGE ( 'NONE', *, *, #178662, .T. ) ;
#159512 = CARTESIAN_POINT ( 'NONE',  ( 21.05000000000000071, 69.50331341424531217, -136.5084513660147252 ) ) ;
#159513 = ORIENTED_EDGE ( 'NONE', *, *, #251993, .F. ) ;
#159514 = DIRECTION ( 'NONE',  ( -0.000000000000000000, 1.000000000000000000, 0.000000000000000000 ) ) ;
#159516 = ORIENTED_EDGE ( 'NONE', *, *, #201907, .F. ) ;
#159515 = AXIS2_PLACEMENT_3D ( 'NONE', #181300, #2626, #60031 ) ;
#159517 = AXIS2_PLACEMENT_3D ( 'NONE', #23194, #101364, #45301 ) ;
#159518 = VECTOR ( 'NONE', #552, 1000.000000000000000 ) ;
#159519 = VERTEX_POINT ( 'NONE', #53411 ) ;
#159520 = CARTESIAN_POINT ( 'NONE',  ( -18.40000000000000213, 16.64129698264336099, -222.1941556740511032 ) ) ;
#159521 = CARTESIAN_POINT ( 'NONE',  ( 23.14999999999999858, 30.73962027982165424, -265.0781340245722504 ) ) ;
#159523 = ORIENTED_EDGE ( 'NONE', *, *, #84618, .F. ) ;
#159522 = CARTESIAN_POINT ( 'NONE',  ( 21.05000000000000071, -4.161311414658873886, -226.0656773515597706 ) ) ;
#159524 = CARTESIAN_POINT ( 'NONE',  ( -23.25000000000000000, 54.89227652059045681, -239.1913228807104588 ) ) ;
#159525 = ORIENTED_EDGE ( 'NONE', *, *, #229081, .F. ) ;
#159526 = DIRECTION ( 'NONE',  ( 1.000000000000000000, 0.000000000000000000, 0.000000000000000000 ) ) ;
#159527 = LINE ( 'NONE', #21317, #114719 ) ;
#159528 = CARTESIAN_POINT ( 'NONE',  ( 21.15000000000005542, 77.73640333653723644, -47.54092689884382850 ) ) ;
#159529 = VERTEX_POINT ( 'NONE', #212506 ) ;
#159530 = LINE ( 'NONE', #196080, #204394 ) ;
#159531 = CARTESIAN_POINT ( 'NONE',  ( 23.14999999999999858, 36.02918351690956200, -236.0543695120161374 ) ) ;
#159532 = LINE ( 'NONE', #236480, #198991 ) ;
#159533 = ORIENTED_EDGE ( 'NONE', *, *, #229133, .F. ) ;
#159535 = DIRECTION ( 'NONE',  ( 0.000000000000000000, 1.000000000000000000, -0.000000000000000000 ) ) ;
#159534 = CIRCLE ( 'NONE', #26263, 0.1999999999999987899 ) ;
#159536 = ORIENTED_EDGE ( 'NONE', *, *, #245643, .T. ) ;
#159537 = ORIENTED_EDGE ( 'NONE', *, *, #149762, .F. ) ;
#159538 = CARTESIAN_POINT ( 'NONE',  ( 21.14999999999999503, 0.000000000000000000, 0.000000000000000000 ) ) ;
#159539 = VERTEX_POINT ( 'NONE', #113390 ) ;
#159540 = AXIS2_PLACEMENT_3D ( 'NONE', #218381, #39802, #180569 ) ;
#159541 = ORIENTED_EDGE ( 'NONE', *, *, #45261, .F. ) ;
#159542 = CARTESIAN_POINT ( 'NONE',  ( -22.39999999999999858, -1.560176095955062348, -193.3663837337744837 ) ) ;
#159543 = ORIENTED_EDGE ( 'NONE', *, *, #222749, .T. ) ;
#159544 = VERTEX_POINT ( 'NONE', #173416 ) ;
#159545 = PLANE ( 'NONE',  #118814 ) ;
#159546 = CARTESIAN_POINT ( 'NONE',  ( 22.60000000000000142, 75.95218160930798490, -215.2731299035715722 ) ) ;
#159547 = EDGE_LOOP ( 'NONE', ( #17350, #50850, #48361, #111098 ) ) ;
#159548 = EDGE_CURVE ( 'NONE', #179560, #111061, #198594, .T. ) ;
#159549 = ORIENTED_EDGE ( 'NONE', *, *, #216849, .T. ) ;
#159550 = EDGE_CURVE ( 'NONE', #62719, #180643, #156935, .T. ) ;
#159551 = ORIENTED_EDGE ( 'NONE', *, *, #175412, .T. ) ;
#159552 = VECTOR ( 'NONE', #189224, 1000.000000000000000 ) ;
#159553 = EDGE_CURVE ( 'NONE', #190980, #111426, #218885, .T. ) ;
#159554 = LINE ( 'NONE', #61728, #146960 ) ;
#159555 = EDGE_CURVE ( 'NONE', #109039, #224041, #90253, .T. ) ;
#159556 = CARTESIAN_POINT ( 'NONE',  ( 18.48536876927988715, 85.46352724988010152, -196.4744892194416650 ) ) ;
#159557 = CYLINDRICAL_SURFACE ( 'NONE', #105428, 0.09999999999999939493 ) ;
#159558 = CARTESIAN_POINT ( 'NONE',  ( -20.94999999999999929, 86.48473784507379492, -209.3714211149925575 ) ) ;
#159559 = CARTESIAN_POINT ( 'NONE',  ( 21.98333005346336577, 0.6286209188979451357, -230.2507154655492343 ) ) ;
#159560 = CARTESIAN_POINT ( 'NONE',  ( -22.50000000000000000, 11.64976291804307884, -66.91119002361310208 ) ) ;
#159561 = DIRECTION ( 'NONE',  ( 1.000000000000000000, 0.000000000000000000, 0.000000000000000000 ) ) ;
#159563 = LINE ( 'NONE', #239097, #120310 ) ;
#159562 = CARTESIAN_POINT ( 'NONE',  ( -16.80117486205003630, 66.05034273169992787, -149.1742526115989449 ) ) ;
#159564 = DIRECTION ( 'NONE',  ( 1.000000000000000000, 0.000000000000000000, 0.000000000000000000 ) ) ;
#159565 = CARTESIAN_POINT ( 'NONE',  ( 18.59999999999999076, -1.249999999988843369, -108.5000000000000284 ) ) ;
#159566 = DIRECTION ( 'NONE',  ( 1.000000000000000000, 0.000000000000000000, 0.000000000000000000 ) ) ;
#159567 = CARTESIAN_POINT ( 'NONE',  ( 21.09706851349342216, 44.23730524916371110, -236.5399123196797007 ) ) ;
#159568 = EDGE_LOOP ( 'NONE', ( #60179, #64779, #58365, #211345 ) ) ;
#159569 = ADVANCED_FACE ( 'NONE', ( #19428 ), #37728, .F. ) ;
#159570 = EDGE_CURVE ( 'NONE', #74560, #18090, #236020, .T. ) ;
#159571 = CIRCLE ( 'NONE', #26487, 0.1000000000000028644 ) ;
#159573 = ORIENTED_EDGE ( 'NONE', *, *, #57963, .F. ) ;
#159572 = DIRECTION ( 'NONE',  ( 1.000000000000000000, -0.000000000000000000, -0.000000000000000000 ) ) ;
#159574 = CARTESIAN_POINT ( 'NONE',  ( -21.44999999999999929, 68.65000000001157332, -57.17310748452437252 ) ) ;
#159575 = FACE_OUTER_BOUND ( 'NONE', #99523, .T. ) ;
#159576 = PRESENTATION_STYLE_ASSIGNMENT (( #218232 ) ) ;
#159577 = ORIENTED_EDGE ( 'NONE', *, *, #147414, .T. ) ;
#159579 = VECTOR ( 'NONE', #257279, 1000.000000000000000 ) ;
#159578 =( NAMED_UNIT ( * ) SI_UNIT ( $, .STERADIAN. ) SOLID_ANGLE_UNIT ( ) );
#159580 = ADVANCED_FACE ( 'NONE', ( #157696 ), #255408, .T. ) ;
#159582 = AXIS2_PLACEMENT_3D ( 'NONE', #174182, #35930, #115436 ) ;
#159581 = CYLINDRICAL_SURFACE ( 'NONE', #33236, 0.09999999999999939493 ) ;
#159583 = EDGE_CURVE ( 'NONE', #30065, #5530, #118545, .T. ) ;
#159584 = CARTESIAN_POINT ( 'NONE',  ( -22.39999999999999858, 0.09999999999999939493, 0.000000000000000000 ) ) ;
#159585 = ORIENTED_EDGE ( 'NONE', *, *, #71734, .T. ) ;
#159586 = CARTESIAN_POINT ( 'NONE',  ( -21.00219873199047171, 11.60538868788763089, -140.9126474282950312 ) ) ;
#159587 = FACE_OUTER_BOUND ( 'NONE', #173605, .T. ) ;
#159588 = AXIS2_PLACEMENT_3D ( 'NONE', #139022, #20420, #239457 ) ;
#159589 = PLANE ( 'NONE',  #199507 ) ;
#159591 = ORIENTED_EDGE ( 'NONE', *, *, #156858, .T. ) ;
#159590 = CARTESIAN_POINT ( 'NONE',  ( 23.24999999999999645, 1.115600667400684642E-11, -200.9999999999999432 ) ) ;
#159592 = EDGE_CURVE ( 'NONE', #200182, #26287, #206982, .T. ) ;
#159594 = ORIENTED_EDGE ( 'NONE', *, *, #59003, .F. ) ;
#159593 = CARTESIAN_POINT ( 'NONE',  ( -18.59999999999999787, 85.48068669529084218, -96.08199231576638510 ) ) ;
#159595 = VECTOR ( 'NONE', #227333, 1000.000000000000114 ) ;
#159596 = DIRECTION ( 'NONE',  ( 0.000000000000000000, -1.000000000000000000, -6.982962677686265922E-15 ) ) ;
#159598 = DIRECTION ( 'NONE',  ( -1.000000000000000000, 0.000000000000000000, 0.000000000000000000 ) ) ;
#159597 = VECTOR ( 'NONE', #210159, 1000.000000000000000 ) ;
#159599 = AXIS2_PLACEMENT_3D ( 'NONE', #178674, #79512, #153988 ) ;
#159600 = DIRECTION ( 'NONE',  ( 0.000000000000000000, 0.000000000000000000, -1.000000000000000000 ) ) ;
#159601 = EDGE_CURVE ( 'NONE', #15247, #126382, #27956, .T. ) ;
#159602 = DIRECTION ( 'NONE',  ( -1.000000000000000000, 0.000000000000000000, 0.000000000000000000 ) ) ;
#159603 = VECTOR ( 'NONE', #110262, 1000.000000000000000 ) ;
#159605 = CARTESIAN_POINT ( 'NONE',  ( 18.50000000000000000, 26.26588584238432489, -255.7307459359297468 ) ) ;
#159604 = DIRECTION ( 'NONE',  ( 0.000000000000000000, 0.9126074666063769270, 0.4088369013363280513 ) ) ;
#159606 = CARTESIAN_POINT ( 'NONE',  ( -16.94445028196808778, 66.00793639031486748, -190.9157773061059800 ) ) ;
#159607 = CARTESIAN_POINT ( 'NONE',  ( 6.099999999999998757, -11.75000000000000000, 10.10000000000000142 ) ) ;
#159609 = EDGE_CURVE ( 'NONE', #104833, #229356, #177780, .T. ) ;
#159608 = CARTESIAN_POINT ( 'NONE',  ( -23.25000000000000000, -11.64999999998884483, -36.60000000000000853 ) ) ;
#159610 = CARTESIAN_POINT ( 'NONE',  ( 21.17356465864818915, 0.09891124102502621418, -161.0771968737582540 ) ) ;
#159611 = CARTESIAN_POINT ( 'NONE',  ( -20.85000000000000142, 68.92903212821303782, -99.27654326265604823 ) ) ;
#159612 = ORIENTED_EDGE ( 'NONE', *, *, #15827, .T. ) ;
#159613 = CARTESIAN_POINT ( 'NONE',  ( 21.14999999999999858, 1.115486826172573664E-11, -93.95934304829877703 ) ) ;
#159614 = VERTEX_POINT ( 'NONE', #156400 ) ;
#159615 = ORIENTED_EDGE ( 'NONE', *, *, #34849, .T. ) ;
#159616 = DIRECTION ( 'NONE',  ( 0.000000000000000000, -6.608470384673536824E-15, 1.000000000000000000 ) ) ;
#159617 = DIRECTION ( 'NONE',  ( 2.694716079187272946E-16, -1.000000000000000000, 0.000000000000000000 ) ) ;
#159618 = VERTEX_POINT ( 'NONE', #40305 ) ;
#159619 = EDGE_CURVE ( 'NONE', #252329, #155690, #61240, .T. ) ;
#159620 = EDGE_LOOP ( 'NONE', ( #65508, #152984, #151604, #219124, #234260, #158530, #229730, #14793 ) ) ;
#159621 = ADVANCED_FACE ( 'NONE', ( #235887 ), #57238, .F. ) ;
#159622 = AXIS2_PLACEMENT_3D ( 'NONE', #118362, #238280, #197873 ) ;
#159623 = TOROIDAL_SURFACE ( 'NONE', #80464, 11.65000000000000036, 0.1000000000000000056 ) ;
#159624 = ORIENTED_EDGE ( 'NONE', *, *, #75939, .F. ) ;
#159625 = ORIENTED_EDGE ( 'NONE', *, *, #202221, .F. ) ;
#159626 = CYLINDRICAL_SURFACE ( 'NONE', #83923, 0.1000000000000028644 ) ;
#159627 = CARTESIAN_POINT ( 'NONE',  ( -21.53752568622134689, 0.09897446126636658126, 6.786807874548587804 ) ) ;
#159628 = DIRECTION ( 'NONE',  ( 0.000000000000000000, -6.982962677686266711E-15, 1.000000000000000000 ) ) ;
#159629 = DIRECTION ( 'NONE',  ( 1.000000000000000000, 0.000000000000000000, -0.000000000000000000 ) ) ;
#159630 = DIRECTION ( 'NONE',  ( 0.000000000000000000, 1.000000000000000000, -6.308085367188393199E-16 ) ) ;
#159631 = CIRCLE ( 'NONE', #192959, 11.90000000000000036 ) ;
#159632 = AXIS2_PLACEMENT_3D ( 'NONE', #61431, #181401, #152 ) ;
#159633 = LINE ( 'NONE', #254817, #116701 ) ;
#159634 = DIRECTION ( 'NONE',  ( 2.952720810173289112E-16, 1.000000000000000000, 6.982962677686266711E-15 ) ) ;
#159636 = ORIENTED_EDGE ( 'NONE', *, *, #180911, .F. ) ;
#159635 = CARTESIAN_POINT ( 'NONE',  ( 20.94999999999999574, 1.835341550235569663, -78.55515129256302487 ) ) ;
#159638 = CARTESIAN_POINT ( 'NONE',  ( -20.65000000000000568, 5.650000000011139001, -46.15000000000000568 ) ) ;
#159637 = CARTESIAN_POINT ( 'NONE',  ( -17.29838795458127976, 63.00731216765596798, -211.8062850501013088 ) ) ;
#159639 = CYLINDRICAL_SURFACE ( 'NONE', #153225, 0.09999999999999939493 ) ;
#159640 = ORIENTED_EDGE ( 'NONE', *, *, #44792, .F. ) ;
#159641 = AXIS2_PLACEMENT_3D ( 'NONE', #79473, #218991, #40405 ) ;
#159642 = DIRECTION ( 'NONE',  ( 0.000000000000000000, 0.1350103645451876666, -0.9908441862701600211 ) ) ;
#159643 = SURFACE_STYLE_USAGE ( .BOTH. , #220881 ) ;
#159644 = ORIENTED_EDGE ( 'NONE', *, *, #212774, .F. ) ;
#159645 = CIRCLE ( 'NONE', #47189, 11.65000000000000036 ) ;
#159648 = DIRECTION ( 'NONE',  ( 1.000000000000000000, -0.000000000000000000, -0.000000000000000000 ) ) ;
#159647 = CARTESIAN_POINT ( 'NONE',  ( -23.25000000000000000, 5.950000000011167245, -190.6942976949651438 ) ) ;
#159646 = TOROIDAL_SURFACE ( 'NONE', #109559, 11.65000000000000036, 0.1000000000000000056 ) ;
#159649 = CIRCLE ( 'NONE', #143047, 1.999999999999990452 ) ;
#159650 = CIRCLE ( 'NONE', #72767, 0.3999999999999948597 ) ;
#159651 = CARTESIAN_POINT ( 'NONE',  ( -16.87683809663752399, 66.13411015067987364, -82.79053429159371547 ) ) ;
#159652 = CARTESIAN_POINT ( 'NONE',  ( 22.49544290803783753, 64.25012976215460014, -69.58841944378183086 ) ) ;
#159653 = VERTEX_POINT ( 'NONE', #139341 ) ;
#159654 = AXIS2_PLACEMENT_3D ( 'NONE', #129644, #209176, #219429 ) ;
#159655 = CARTESIAN_POINT ( 'NONE',  ( 21.07954763557417266, 6.329290990048654919, -66.93412408138154035 ) ) ;
#159656 = DIRECTION ( 'NONE',  ( 1.000000000000000000, -0.000000000000000000, 0.000000000000000000 ) ) ;
#159657 = CARTESIAN_POINT ( 'NONE',  ( -18.43634282235123578, -0.9118504197709764725, -242.3006630565730006 ) ) ;
#159658 = DIRECTION ( 'NONE',  ( 1.000000000000000000, -1.836970198721029934E-16, -1.282749433769087582E-30 ) ) ;
#159659 = DIRECTION ( 'NONE',  ( 0.7071067811865127117, 0.7071067811865821007, 0.000000000000000000 ) ) ;
#159660 = ORIENTED_EDGE ( 'NONE', *, *, #99960, .T. ) ;
#159661 = CIRCLE ( 'NONE', #51294, 0.5000000000000004441 ) ;
#159663 = AXIS2_PLACEMENT_3D ( 'NONE', #61963, #103621, #118072 ) ;
#159662 = DIRECTION ( 'NONE',  ( 0.000000000000000000, 1.000000000000000000, 8.717686153663073805E-15 ) ) ;
#159664 = CARTESIAN_POINT ( 'NONE',  ( -14.00000000000000178, 9.850000000011133849, -83.75000000000004263 ) ) ;
#159665 = AXIS2_PLACEMENT_3D ( 'NONE', #153807, #29985, #232026 ) ;
#159666 = DIRECTION ( 'NONE',  ( 0.000000000000000000, -6.982962677686266711E-15, 1.000000000000000000 ) ) ;
#159667 = LINE ( 'NONE', #202630, #167523 ) ;
#159668 = DIRECTION ( 'NONE',  ( 0.000000000000000000, 0.2128009952263603954, -0.9770955615653315052 ) ) ;
#159669 = DIRECTION ( 'NONE',  ( -1.000000000000000000, -0.000000000000000000, 0.000000000000000000 ) ) ;
#159670 = AXIS2_PLACEMENT_3D ( 'NONE', #28386, #50448, #247379 ) ;
#159671 = AXIS2_PLACEMENT_3D ( 'NONE', #66697, #186655, #49694 ) ;
#159672 = AXIS2_PLACEMENT_3D ( 'NONE', #50726, #130281, #125792 ) ;
#159674 = VERTEX_POINT ( 'NONE', #97643 ) ;
#159673 = CARTESIAN_POINT ( 'NONE',  ( 21.05000000000000071, 8.776282895303632259, -179.6499999999999773 ) ) ;
#159675 = COLOUR_RGB ( '', 0.72549020, 0.75294118, 0.79215686) ;
#159676 = CARTESIAN_POINT ( 'NONE',  ( 20.94999999999999929, 70.60000000001222986, -148.9283735034374843 ) ) ;
#159677 = FACE_OUTER_BOUND ( 'NONE', #107472, .T. ) ;
#159678 = CARTESIAN_POINT ( 'NONE',  ( 18.52351027002948314, 77.30154854284161559, -241.9092773799638962 ) ) ;
#159679 = DIRECTION ( 'NONE',  ( 0.000000000000000000, 0.000000000000000000, -1.000000000000000000 ) ) ;
#159680 = EDGE_CURVE ( 'NONE', #2708, #156996, #80652, .T. ) ;
#159681 = CARTESIAN_POINT ( 'NONE',  ( 21.05000000000000071, 10.72371681401022592, -175.0943992358841683 ) ) ;
#159683 = ORIENTED_EDGE ( 'NONE', *, *, #27657, .T. ) ;
#159682 = CARTESIAN_POINT ( 'NONE',  ( 21.05095171578076574, 67.22382012124053574, -57.35723420788649918 ) ) ;
#159684 = CARTESIAN_POINT ( 'NONE',  ( -18.59999999999999787, 11.60000000000000320, -6.928203230275554958 ) ) ;
#159685 = CARTESIAN_POINT ( 'NONE',  ( 18.49999999999999289, 69.35000000001180354, -81.67310748452436542 ) ) ;
#159686 = DIRECTION ( 'NONE',  ( 1.000000000000000000, 0.000000000000000000, 0.000000000000000000 ) ) ;
#159687 = ORIENTED_EDGE ( 'NONE', *, *, #133294, .T. ) ;
#159688 = CARTESIAN_POINT ( 'NONE',  ( -22.50000000000000000, 1.115600667400684642E-11, -122.3504291924552234 ) ) ;
#159689 = CARTESIAN_POINT ( 'NONE',  ( -20.54999999999999716, -8.999999999988846255, -76.89396912265249284 ) ) ;
#159690 = EDGE_CURVE ( 'NONE', #151221, #58482, #199357, .T. ) ;
#159691 = EDGE_CURVE ( 'NONE', #155954, #208580, #207184, .T. ) ;
#159692 = CARTESIAN_POINT ( 'NONE',  ( -20.64999999999999858, 68.85000000001205933, -124.1731074845243370 ) ) ;
#159693 = CARTESIAN_POINT ( 'NONE',  ( -22.39999999999999858, -0.1008583690875579364, -88.75043287651064361 ) ) ;
#159694 = AXIS2_PLACEMENT_3D ( 'NONE', #92070, #171654, #251128 ) ;
#159695 = CARTESIAN_POINT ( 'NONE',  ( -23.25000000000000000, 85.00000000001159606, -59.62913836187181715 ) ) ;
#159696 = AXIS2_PLACEMENT_3D ( 'NONE', #108802, #247024, #89238 ) ;
#159697 = AXIS2_PLACEMENT_3D ( 'NONE', #176871, #175578, #214678 ) ;
#159698 = ORIENTED_EDGE ( 'NONE', *, *, #150518, .F. ) ;
#159699 = ORIENTED_EDGE ( 'NONE', *, *, #65773, .T. ) ;
#159700 = DIRECTION ( 'NONE',  ( 1.000000000000000000, 0.000000000000000000, 0.000000000000000000 ) ) ;
#159701 = CYLINDRICAL_SURFACE ( 'NONE', #191447, 0.1000000000000124678 ) ;
#159702 = ADVANCED_FACE ( 'NONE', ( #1110 ), #36446, .F. ) ;
#159703 = CARTESIAN_POINT ( 'NONE',  ( 21.05000000000000071, 67.23127455305841238, -235.8551265064783991 ) ) ;
#159704 = CARTESIAN_POINT ( 'NONE',  ( -23.25000000000000000, 1.115651490242849210E-11, -129.8500000000000227 ) ) ;
#159705 = EDGE_LOOP ( 'NONE', ( #242640, #132958, #95084, #78937 ) ) ;
#159706 = CYLINDRICAL_SURFACE ( 'NONE', #255116, 0.09999999999999939493 ) ;
#159707 = CARTESIAN_POINT ( 'NONE',  ( 20.97107704358301916, 10.49354833045136637, -207.4742241701343062 ) ) ;
#159708 = CARTESIAN_POINT ( 'NONE',  ( 23.14999999999999858, 45.58907629467868361, -240.2765730862633404 ) ) ;
#159709 = CARTESIAN_POINT ( 'NONE',  ( -20.94999999999999574, 17.02177226667168597, -224.5487030889150901 ) ) ;
#159710 = DIRECTION ( 'NONE',  ( 0.000000000000000000, 6.982962677686266711E-15, -1.000000000000000000 ) ) ;
#159711 = ORIENTED_EDGE ( 'NONE', *, *, #59561, .F. ) ;
#159713 = EDGE_LOOP ( 'NONE', ( #118064, #229160, #72365, #79041, #87032 ) ) ;
#159712 = DIRECTION ( 'NONE',  ( 0.000000000000000000, 0.000000000000000000, 1.000000000000000000 ) ) ;
#159714 = VERTEX_POINT ( 'NONE', #75572 ) ;
#159715 = AXIS2_PLACEMENT_3D ( 'NONE', #215528, #135979, #175177 ) ;
#159716 = CARTESIAN_POINT ( 'NONE',  ( -23.39999999999994529, 77.16254490893143725, -44.02310748452479316 ) ) ;
#159717 = ORIENTED_EDGE ( 'NONE', *, *, #2277, .F. ) ;
#159718 = ADVANCED_FACE ( 'NONE', ( #244875 ), #85768, .T. ) ;
#159719 = CARTESIAN_POINT ( 'NONE',  ( -21.11833042828140350, 0.007100509070575833880, -27.05435530614471773 ) ) ;
#159720 = EDGE_CURVE ( 'NONE', #253241, #155399, #194729, .T. ) ;
#159721 = CARTESIAN_POINT ( 'NONE',  ( -22.50000000000000000, 0.1000000000111554016, -25.70922040162659883 ) ) ;
#159722 = ORIENTED_EDGE ( 'NONE', *, *, #151444, .F. ) ;
#159723 = DIRECTION ( 'NONE',  ( 1.000000000000000000, -0.000000000000000000, -0.000000000000000000 ) ) ;
#159724 = DIRECTION ( 'NONE',  ( 0.000000000000000000, 0.000000000000000000, -1.000000000000000000 ) ) ;
#159725 = ORIENTED_EDGE ( 'NONE', *, *, #6296, .F. ) ;
#159726 = DIRECTION ( 'NONE',  ( -1.000000000000000000, -7.304098846218135653E-16, -5.100424963727256530E-30 ) ) ;
#159728 = ORIENTED_EDGE ( 'NONE', *, *, #14990, .F. ) ;
#159727 = CARTESIAN_POINT ( 'NONE',  ( -22.50000000000000000, 75.90000000001165859, -69.52310748452431710 ) ) ;
#159729 = FACE_OUTER_BOUND ( 'NONE', #44294, .T. ) ;
#159730 = EDGE_CURVE ( 'NONE', #67483, #210104, #162867, .T. ) ;
#159731 = AXIS2_PLACEMENT_3D ( 'NONE', #213016, #193474, #110061 ) ;
#159732 = TOROIDAL_SURFACE ( 'NONE', #176491, 0.6000000000000009770, 0.1000000000000000056 ) ;
#159733 = ORIENTED_EDGE ( 'NONE', *, *, #54897, .F. ) ;
#159734 = AXIS2_PLACEMENT_3D ( 'NONE', #95445, #177595, #237538 ) ;
#159735 = LINE ( 'NONE', #254911, #60313 ) ;
#159736 = DIRECTION ( 'NONE',  ( 3.469446951953498700E-14, -0.7899159663865300551, -0.6132151058540831201 ) ) ;
#159737 = DIRECTION ( 'NONE',  ( -0.000000000000000000, -6.982962677686266711E-15, 1.000000000000000000 ) ) ;
#159738 = EDGE_LOOP ( 'NONE', ( #211460, #53742, #85270, #61907 ) ) ;
#159739 = CARTESIAN_POINT ( 'NONE',  ( 21.05000000000000071, -8.663551401858002876, -177.0241011180672785 ) ) ;
#159740 = CARTESIAN_POINT ( 'NONE',  ( 13.88638282980484107, 49.67565583792541162, -233.3567449137544543 ) ) ;
#159741 = DIRECTION ( 'NONE',  ( 0.000000000000000000, 0.000000000000000000, 1.000000000000000000 ) ) ;
#159742 = EDGE_CURVE ( 'NONE', #256826, #245711, #105330, .T. ) ;
#159743 = ORIENTED_EDGE ( 'NONE', *, *, #123126, .F. ) ;
#159744 = VECTOR ( 'NONE', #205265, 999.9999999999998863 ) ;
#159745 = TOROIDAL_SURFACE ( 'NONE', #47289, 0.2000000000000000111, 0.1000000000000000056 ) ;
#159746 = CIRCLE ( 'NONE', #231074, 11.80000000000000426 ) ;
#159747 = ORIENTED_EDGE ( 'NONE', *, *, #47166, .F. ) ;
#159748 = AXIS2_PLACEMENT_3D ( 'NONE', #208592, #190305, #10384 ) ;
#159749 = EDGE_CURVE ( 'NONE', #55172, #162005, #67525, .T. ) ;
#159750 = ADVANCED_FACE ( 'NONE', ( #7555 ), #36516, .T. ) ;
#159751 = ORIENTED_EDGE ( 'NONE', *, *, #112336, .T. ) ;
#159752 = CARTESIAN_POINT ( 'NONE',  ( -16.86733706339143524, 9.965990529650820662, -87.90311530199875278 ) ) ;
#159753 = DIRECTION ( 'NONE',  ( -1.000000000000000000, -0.000000000000000000, -0.000000000000000000 ) ) ;
#159755 = ORIENTED_EDGE ( 'NONE', *, *, #164141, .F. ) ;
#159754 = CARTESIAN_POINT ( 'NONE',  ( -20.85000000000000142, 10.33248238083634440, -106.0948465439131922 ) ) ;
#159756 = CARTESIAN_POINT ( 'NONE',  ( -21.37071067811865532, 8.070710678129811910, -188.6499999999999488 ) ) ;
#159757 = FACE_OUTER_BOUND ( 'NONE', #179892, .T. ) ;
#159758 = EDGE_CURVE ( 'NONE', #201700, #88139, #111318, .T. ) ;
#159760 = EDGE_CURVE ( 'NONE', #17520, #25751, #28123, .T. ) ;
#159759 = CARTESIAN_POINT ( 'NONE',  ( 19.75857864376268935, 64.35000000001147669, -44.77310748452440237 ) ) ;
#159761 = DIRECTION ( 'NONE',  ( 1.000000000000000000, 0.000000000000000000, -0.000000000000000000 ) ) ;
#159762 = CARTESIAN_POINT ( 'NONE',  ( -23.15000000000000213, 80.83132476063447314, -52.55341054232553688 ) ) ;
#159763 = AXIS2_PLACEMENT_3D ( 'NONE', #15283, #111807, #93508 ) ;
#159764 = CARTESIAN_POINT ( 'NONE',  ( 23.14999999999999503, 51.28888318656201761, -230.2315015618841869 ) ) ;
#159765 = TOROIDAL_SURFACE ( 'NONE', #97369, 11.65000000000000036, 0.1000000000000000056 ) ;
#159767 = EDGE_LOOP ( 'NONE', ( #114640, #8453, #84410, #129634 ) ) ;
#159766 = CARTESIAN_POINT ( 'NONE',  ( -16.92570016628982543, 66.04121104227267836, -182.6437581545634146 ) ) ;
#159769 = EDGE_LOOP ( 'NONE', ( #65250, #149289, #123926, #96932 ) ) ;
#159768 = DIRECTION ( 'NONE',  ( 0.000000000000000000, -6.982962677686266711E-15, 1.000000000000000000 ) ) ;
#159771 = CARTESIAN_POINT ( 'NONE',  ( -16.90202395485713183, 60.91009262921385670, -221.0887195956053404 ) ) ;
#159770 = TOROIDAL_SURFACE ( 'NONE', #93115, 0.2000000000000000111, 0.1000000000000000056 ) ;
#159772 = ORIENTED_EDGE ( 'NONE', *, *, #83834, .F. ) ;
#159773 = ORIENTED_EDGE ( 'NONE', *, *, #96685, .T. ) ;
#159774 = DIRECTION ( 'NONE',  ( 1.000000000000000000, 0.000000000000000000, 0.000000000000000000 ) ) ;
#159775 = CARTESIAN_POINT ( 'NONE',  ( 20.09999999999999787, 66.25000000001205080, -115.6731074845243796 ) ) ;
#159776 = EDGE_CURVE ( 'NONE', #121217, #136766, #11553, .T. ) ;
#159777 = ADVANCED_FACE ( 'NONE', ( #126208 ), #214637, .F. ) ;
#159778 = CARTESIAN_POINT ( 'NONE',  ( -22.48970261584617703, 64.35000000001195986, -103.0784769727418109 ) ) ;
#159779 = AXIS2_PLACEMENT_3D ( 'NONE', #220852, #194901, #185589 ) ;
#159780 = DIRECTION ( 'NONE',  ( 3.469446951953635015E-14, -0.000000000000000000, 1.000000000000000000 ) ) ;
#159781 = DIRECTION ( 'NONE',  ( -1.000000000000000000, 7.510212038922847255E-17, -1.676432719286211941E-16 ) ) ;
#159782 = EDGE_CURVE ( 'NONE', #87098, #149860, #107196, .T. ) ;
#159783 = CARTESIAN_POINT ( 'NONE',  ( -20.54999999999999716, 84.66355140188167638, -179.5472086025916099 ) ) ;
#159784 = TOROIDAL_SURFACE ( 'NONE', #43081, 2.699999999999999734, 0.1000000000000000056 ) ;
#159785 = CIRCLE ( 'NONE', #151428, 0.1000000000000002831 ) ;
#159786 = AXIS2_PLACEMENT_3D ( 'NONE', #243421, #79201, #43941 ) ;
#159788 = AXIS2_PLACEMENT_3D ( 'NONE', #244991, #6378, #202023 ) ;
#159787 = CARTESIAN_POINT ( 'NONE',  ( -20.64999999999999858, 74.05981308412469843, -182.8522266955776843 ) ) ;
#159790 = VERTEX_POINT ( 'NONE', #230456 ) ;
#159789 = EDGE_CURVE ( 'NONE', #252796, #221674, #19742, .T. ) ;
#159791 = ORIENTED_EDGE ( 'NONE', *, *, #246872, .F. ) ;
#159792 = DIRECTION ( 'NONE',  ( 6.484947573744954877E-15, -0.9274965247785555977, 0.3738317757009190223 ) ) ;
#159793 = VERTEX_POINT ( 'NONE', #68829 ) ;
#159794 = EDGE_CURVE ( 'NONE', #71706, #108747, #130055, .T. ) ;
#159795 = DIRECTION ( 'NONE',  ( 0.000000000000000000, 0.07893460099012301889, -0.9968797965484755830 ) ) ;
#159796 = EDGE_CURVE ( 'NONE', #116061, #127095, #148352, .T. ) ;
#159797 = DIRECTION ( 'NONE',  ( 0.000000000000000000, 0.8700118002898356018, -0.4930308989875170078 ) ) ;
#159798 = CARTESIAN_POINT ( 'NONE',  ( 18.49999999999999289, 10.29270135741298731, -172.9573618871519614 ) ) ;
#159799 = LINE ( 'NONE', #254964, #138577 ) ;
#159800 = EDGE_CURVE ( 'NONE', #63414, #118225, #228019, .T. ) ;
#159801 = ORIENTED_EDGE ( 'NONE', *, *, #206007, .F. ) ;
#159802 = CARTESIAN_POINT ( 'NONE',  ( -12.25000000000000178, 48.12247445990688988, -234.1702647910923361 ) ) ;
#159803 = ORIENTED_EDGE ( 'NONE', *, *, #229422, .T. ) ;
#159804 = DIRECTION ( 'NONE',  ( 0.000000000000000000, 0.000000000000000000, 1.000000000000000000 ) ) ;
#159805 = EDGE_LOOP ( 'NONE', ( #193817, #172336, #91532, #156681 ) ) ;
#159806 = EDGE_CURVE ( 'NONE', #144388, #4003, #115576, .T. ) ;
#159807 = DIRECTION ( 'NONE',  ( -1.000000000000000000, 0.000000000000000000, 0.000000000000000000 ) ) ;
#159808 = ADVANCED_FACE ( 'NONE', ( #171803 ), #241325, .F. ) ;
#159809 = CARTESIAN_POINT ( 'NONE',  ( 15.06592377766031809, 9.417789466963361278, -182.8573845439768206 ) ) ;
#159811 = ORIENTED_EDGE ( 'NONE', *, *, #229025, .F. ) ;
#159810 = EDGE_CURVE ( 'NONE', #47226, #35900, #232137, .T. ) ;
#159812 = CIRCLE ( 'NONE', #188846, 0.1000000000000028644 ) ;
#159813 = CARTESIAN_POINT ( 'NONE',  ( -21.05000000000000071, 16.53615870702968138, -240.8540256063542984 ) ) ;
#159815 = ORIENTED_EDGE ( 'NONE', *, *, #140323, .F. ) ;
#159814 = CYLINDRICAL_SURFACE ( 'NONE', #238987, 11.74999999999999645 ) ;
#159816 = CIRCLE ( 'NONE', #76595, 0.09999999999999895084 ) ;
#159817 = CARTESIAN_POINT ( 'NONE',  ( 20.94999999999999929, 23.68770167995059239, -252.8127582590406348 ) ) ;
#159818 = ORIENTED_EDGE ( 'NONE', *, *, #106455, .T. ) ;
#159819 = CIRCLE ( 'NONE', #189035, 11.75000000000000178 ) ;
#159820 = AXIS2_PLACEMENT_3D ( 'NONE', #158973, #19438, #16881 ) ;
#159821 = CARTESIAN_POINT ( 'NONE',  ( -20.54999999999999716, 1.115600667400684642E-11, -100.5000000000000426 ) ) ;
#159822 = ORIENTED_EDGE ( 'NONE', *, *, #24691, .T. ) ;
#159823 = ADVANCED_FACE ( 'NONE', ( #89645, #150921 ), #111800, .F. ) ;
#159824 = PLANE ( 'NONE',  #24285 ) ;
#159825 = CARTESIAN_POINT ( 'NONE',  ( 19.86930884467575353, 64.31308993304160992, -178.7838848455857317 ) ) ;
#159826 =( BOUNDED_CURVE ( )  B_SPLINE_CURVE ( 3, ( #215824, #245689, #87868, #48763 ),
 .UNSPECIFIED., .F., .F. ) 
 B_SPLINE_CURVE_WITH_KNOTS ( ( 4, 4 ),
 ( 1.570796326794931197, 3.141592653589758477 ),
 .UNSPECIFIED. ) 
 CURVE ( )  GEOMETRIC_REPRESENTATION_ITEM ( )  RATIONAL_B_SPLINE_CURVE ( ( 1.000000000000000000, 0.8047378541243812577, 0.8047378541243812577, 1.000000000000000000 ) ) 
 REPRESENTATION_ITEM ( '' )  );
#159827 = CARTESIAN_POINT ( 'NONE',  ( 23.25000000000000000, 30.69873658968802133, -264.9868732779115703 ) ) ;
#159828 = CARTESIAN_POINT ( 'NONE',  ( -16.86379686415369150, 9.975217759264314310, -121.4333898890903214 ) ) ;
#159829 = AXIS2_PLACEMENT_3D ( 'NONE', #81401, #3166, #21487 ) ;
#159830 = DIRECTION ( 'NONE',  ( -1.000000000000000000, 2.952720810173289112E-16, 2.061873921506763405E-30 ) ) ;
#159831 = TOROIDAL_SURFACE ( 'NONE', #172535, 0.6000000000000004219, 0.1000000000000000056 ) ;
#159832 = ORIENTED_EDGE ( 'NONE', *, *, #25219, .T. ) ;
#159833 = AXIS2_PLACEMENT_3D ( 'NONE', #111930, #17934, #192746 ) ;
#159834 = DIRECTION ( 'NONE',  ( 0.000000000000000000, 0.000000000000000000, 1.000000000000000000 ) ) ;
#159835 = CARTESIAN_POINT ( 'NONE',  ( 21.04999999999976978, 6.441084688482524356, -100.5177194333089119 ) ) ;
#159837 = CARTESIAN_POINT ( 'NONE',  ( 22.01447462590973458, 0.7725924869657057048, -230.2154859497122459 ) ) ;
#159836 = AXIS2_PLACEMENT_3D ( 'NONE', #194562, #15928, #56288 ) ;
#159838 = ORIENTED_EDGE ( 'NONE', *, *, #64078, .F. ) ;
#159839 = LINE ( 'NONE', #181961, #34695 ) ;
#159840 = ORIENTED_EDGE ( 'NONE', *, *, #156509, .T. ) ;
#159841 = DIRECTION ( 'NONE',  ( 1.000000000000000000, 1.186688945009010077E-16, 0.000000000000000000 ) ) ;
#159843 = ORIENTED_EDGE ( 'NONE', *, *, #72076, .F. ) ;
#159842 = CIRCLE ( 'NONE', #5866, 0.1000000000000075273 ) ;
#159844 =( BOUNDED_SURFACE ( )  B_SPLINE_SURFACE ( 3, 2, ( 
 ( #160146, #117150, #196666 ),
 ( #18037, #161422, #97543 ),
 ( #177145, #81825, #179697 ),
 ( #257881, #59709, #256596 ),
 ( #78003, #237093, #58424 ),
 ( #200527, #79276, #217503 ),
 ( #158860, #139243, #40203 ),
 ( #119722, #141830, #21897 ),
 ( #199258, #20629, #61008 ),
 ( #140538, #220096, #31864 ) ),
 .UNSPECIFIED., .F., .F., .F. ) 
 B_SPLINE_SURFACE_WITH_KNOTS ( ( 4, 2, 2, 2, 4 ),
 ( 3, 3 ),
 ( 0.0001701955120502350236, 0.0002247052511886071975, 0.0002792149903269793444, 0.0003882344686037236380, 0.0006062734251572122254 ),
 ( 0.000000000000000000, 1.000000000000000000 ),
 .UNSPECIFIED. ) 
 GEOMETRIC_REPRESENTATION_ITEM ( )  RATIONAL_B_SPLINE_SURFACE ( (
 ( 1.000000000000000000, 0.2966190024561151661, 1.000000000000000000),
 ( 1.000000000000000000, 0.2964522492709388279, 1.000000000000000000),
 ( 1.000000000000000000, 0.3059923531885315184, 1.000000000000000000),
 ( 1.000000000000000000, 0.3355751146943017904, 1.000000000000000000),
 ( 1.000000000000000000, 0.3550672384958052930, 1.000000000000000000),
 ( 1.000000000000000000, 0.4157034672192139180, 1.000000000000000000),
 ( 1.000000000000000000, 0.4588031877657839930, 1.000000000000000000),
 ( 1.000000000000000000, 0.5771441759654667436, 1.000000000000000000),
 ( 1.000000000000000000, 0.6469377121776090922, 1.000000000000000000),
 ( 1.000000000000000000, 0.7071067811865870967, 1.000000000000000000) ) ) 
 REPRESENTATION_ITEM ( '' )  SURFACE ( )  );
#159845 = CARTESIAN_POINT ( 'NONE',  ( -21.12642695952773764, 69.62434007797752145, -203.6220107677137605 ) ) ;
#159846 = CARTESIAN_POINT ( 'NONE',  ( -20.89192007715127986, 10.32898536001801304, -72.58266832227644727 ) ) ;
#159847 = ORIENTED_EDGE ( 'NONE', *, *, #177064, .T. ) ;
#159849 = VERTEX_POINT ( 'NONE', #51795 ) ;
#159848 = CARTESIAN_POINT ( 'NONE',  ( -23.15000000000000213, 2.500000000011154633, -53.77537807723791019 ) ) ;
#159850 = DIRECTION ( 'NONE',  ( -0.000000000000000000, -0.000000000000000000, -1.000000000000000000 ) ) ;
#159851 = VERTEX_POINT ( 'NONE', #13987 ) ;
#159852 = AXIS2_PLACEMENT_3D ( 'NONE', #177332, #15684, #235970 ) ;
#159853 = LINE ( 'NONE', #20346, #223392 ) ;
#159854 = CYLINDRICAL_SURFACE ( 'NONE', #22908, 0.09999999999999939493 ) ;
#159855 = EDGE_LOOP ( 'NONE', ( #119388, #203107, #174982, #204791 ) ) ;
#159856 = ORIENTED_EDGE ( 'NONE', *, *, #7065, .T. ) ;
#159857 = VECTOR ( 'NONE', #143151, 1000.000000000000000 ) ;
#159858 = EDGE_CURVE ( 'NONE', #233386, #23148, #93505, .T. ) ;
#159859 = CYLINDRICAL_SURFACE ( 'NONE', #35254, 14.30833333333335311 ) ;
#159860 = LINE ( 'NONE', #141553, #190149 ) ;
#159861 = VERTEX_POINT ( 'NONE', #207047 ) ;
#159862 = DIRECTION ( 'NONE',  ( 1.073024830501117725E-15, -6.982962677686266711E-15, 1.000000000000000000 ) ) ;
#159863 = EDGE_CURVE ( 'NONE', #117188, #92906, #190449, .T. ) ;
#159864 = B_SPLINE_CURVE_WITH_KNOTS ( 'NONE', 3,
 ( #36851, #78491, #175094, #98036, #17267, #236293, #137195, #117636 ),
 .UNSPECIFIED., .F., .F.,
 ( 4, 2, 2, 4 ),
 ( 0.000000000000000000, 0.0002181133598169092088, 0.0003271700397253594493, 0.0004362267196338096898 ),
 .UNSPECIFIED. ) ;
#159866 = ORIENTED_EDGE ( 'NONE', *, *, #81399, .T. ) ;
#159865 = AXIS2_PLACEMENT_3D ( 'NONE', #185824, #128425, #48881 ) ;
#159867 = ORIENTED_EDGE ( 'NONE', *, *, #32037, .T. ) ;
#159868 =( BOUNDED_SURFACE ( )  B_SPLINE_SURFACE ( 3, 2, ( 
 ( #105365, #182392, #81954 ),
 ( #80687, #164107, #161552 ),
 ( #66289, #23336, #220237 ),
 ( #44162, #184943, #6291 ),
 ( #102814, #181115, #85803 ),
 ( #165389, #41610, #160280 ) ),
 .UNSPECIFIED., .F., .F., .F. ) 
 B_SPLINE_SURFACE_WITH_KNOTS ( ( 4, 2, 4 ),
 ( 3, 3 ),
 ( 6.719893378900182717E-05, 0.0002757154632485606582, 0.0004842319927081195434 ),
 ( 0.000000000000000000, 1.000000000000000000 ),
 .UNSPECIFIED. ) 
 GEOMETRIC_REPRESENTATION_ITEM ( )  RATIONAL_B_SPLINE_SURFACE ( (
 ( 1.000000000000000000, 0.7250110520819763593, 1.000000000000000000),
 ( 1.000000000000000000, 0.7277932058357685641, 1.000000000000000000),
 ( 1.000000000000000000, 0.7278452872619538550, 1.000000000000000000),
 ( 1.000000000000000000, 0.7221445671547270795, 1.000000000000000000),
 ( 1.000000000000000000, 0.7163662143781618363, 1.000000000000000000),
 ( 1.000000000000000000, 0.7071067811865475727, 1.000000000000000000) ) ) 
 REPRESENTATION_ITEM ( '' )  SURFACE ( )  );
#159869 = CIRCLE ( 'NONE', #189076, 0.09999999999998898659 ) ;
#159870 = VECTOR ( 'NONE', #62190, 1000.000000000000000 ) ;
#159871 = DIRECTION ( 'NONE',  ( 1.000000000000000000, 0.000000000000000000, 0.000000000000000000 ) ) ;
#159872 = ADVANCED_FACE ( 'NONE', ( #32284 ), #92218, .T. ) ;
#159873 = ADVANCED_FACE ( 'NONE', ( #110499 ), #248742, .F. ) ;
#159875 = VERTEX_POINT ( 'NONE', #187500 ) ;
#159874 = CARTESIAN_POINT ( 'NONE',  ( 18.45068634130097962, 85.48650607335470397, -95.95432905335616169 ) ) ;
#159876 = DIRECTION ( 'NONE',  ( 1.000000000000000000, 0.000000000000000000, 0.000000000000000000 ) ) ;
#159877 = DIRECTION ( 'NONE',  ( 0.000000000000000000, 0.2617529984165030132, 0.9651348961777156399 ) ) ;
#159878 = DIRECTION ( 'NONE',  ( 0.000000000000000000, 1.776356839400254803E-15, 1.000000000000000000 ) ) ;
#159880 = DIRECTION ( 'NONE',  ( 0.000000000000000000, 0.8814952561688429444, -0.4721928772777349015 ) ) ;
#159879 = CARTESIAN_POINT ( 'NONE',  ( -16.93906926870270624, 65.98785312906531431, -90.46965517729756812 ) ) ;
#159881 = CARTESIAN_POINT ( 'NONE',  ( 20.94999999999999929, -9.000000000000000000, -23.60603087734755690 ) ) ;
#159882 = FACE_OUTER_BOUND ( 'NONE', #108209, .T. ) ;
#159883 = DIRECTION ( 'NONE',  ( 1.000000000000000000, -2.952720810173289112E-16, -2.061873921506763405E-30 ) ) ;
#159884 = CIRCLE ( 'NONE', #14145, 0.1000000000000028644 ) ;
#159885 = CARTESIAN_POINT ( 'NONE',  ( -21.52071067811865746, 21.68862476185342558, -232.7068767132159621 ) ) ;
#159886 = AXIS2_PLACEMENT_3D ( 'NONE', #217184, #38571, #63251 ) ;
#159887 = TOROIDAL_SURFACE ( 'NONE', #226480, 11.65000000000000036, 0.1000000000000000056 ) ;
#159888 = ORIENTED_EDGE ( 'NONE', *, *, #186580, .F. ) ;
#159889 = VERTEX_POINT ( 'NONE', #152232 ) ;
#159890 = ORIENTED_EDGE ( 'NONE', *, *, #159601, .F. ) ;
#159891 = DIRECTION ( 'NONE',  ( 0.000000000000000000, 0.9915357197604882655, -0.1298341882519793711 ) ) ;
#159892 = ORIENTED_EDGE ( 'NONE', *, *, #61408, .T. ) ;
#159893 = DIRECTION ( 'NONE',  ( 1.000000000000000000, 7.304098846218163263E-16, -4.217023435051627211E-16 ) ) ;
#159894 = CARTESIAN_POINT ( 'NONE',  ( -20.00857864376270001, 9.250000000011157297, -112.8500000000000369 ) ) ;
#159895 = ORIENTED_EDGE ( 'NONE', *, *, #98151, .F. ) ;
#159896 =( NAMED_UNIT ( * ) PLANE_ANGLE_UNIT ( ) SI_UNIT ( $, .RADIAN. ) );
#159897 = DIRECTION ( 'NONE',  ( 2.940209281316622495E-16, -1.000000000000000000, 2.352167425053297996E-15 ) ) ;
#159899 = ORIENTED_EDGE ( 'NONE', *, *, #15494, .T. ) ;
#159898 = ORIENTED_EDGE ( 'NONE', *, *, #145875, .F. ) ;
#159900 = EDGE_CURVE ( 'NONE', #128506, #231943, #148915, .T. ) ;
#159901 = ORIENTED_EDGE ( 'NONE', *, *, #27712, .T. ) ;
#159902 = ORIENTED_EDGE ( 'NONE', *, *, #24959, .T. ) ;
#159903 = CARTESIAN_POINT ( 'NONE',  ( 21.30000000000002558, 0.000000000000000000, 0.000000000000000000 ) ) ;
#159905 = B_SPLINE_CURVE_WITH_KNOTS ( 'NONE', 3,
 ( #193812, #155987, #92134, #234199, #56824, #71316, #249931, #150825, #230357, #51695, #131260, #171709, #240630, #99803, #41177, #38583, #97221, #197643, #162395 ),
 .UNSPECIFIED., .F., .F.,
 ( 4, 3, 3, 3, 3, 3, 4 ),
 ( -2.000416914641864300E-06, 0.000000000000000000, 4.714008503747964783E-05, 9.979203887779479183E-05, 0.0001372215519229583246, 0.0001635031576221121225, 0.0001900083748504222147 ),
 .UNSPECIFIED. ) ;
#159904 = AXIS2_PLACEMENT_3D ( 'NONE', #165539, #32469, #49427 ) ;
#159906 = DIRECTION ( 'NONE',  ( 0.000000000000000000, 0.000000000000000000, 1.000000000000000000 ) ) ;
#159908 = ORIENTED_EDGE ( 'NONE', *, *, #227, .F. ) ;
#159907 = LINE ( 'NONE', #138997, #216734 ) ;
#159909 = FACE_OUTER_BOUND ( 'NONE', #26104, .T. ) ;
#159910 = DIRECTION ( 'NONE',  ( 1.000000000000000000, 0.000000000000000000, 0.000000000000000000 ) ) ;
#159912 = ORIENTED_EDGE ( 'NONE', *, *, #175092, .F. ) ;
#159911 = LINE ( 'NONE', #63337, #47737 ) ;
#159913 = CARTESIAN_POINT ( 'NONE',  ( -22.37643362114956957, 0.09908137369253962323, -59.37421000604164334 ) ) ;
#159914 = ORIENTED_EDGE ( 'NONE', *, *, #1108, .F. ) ;
#159915 = DIRECTION ( 'NONE',  ( -0.000000000000000000, -6.982962677686266711E-15, 1.000000000000000000 ) ) ;
#159916 = ADVANCED_FACE ( 'NONE', ( #212191 ), #47953, .T. ) ;
#159918 = ORIENTED_EDGE ( 'NONE', *, *, #68146, .F. ) ;
#159917 = CARTESIAN_POINT ( 'NONE',  ( 21.98333005346336932, 1.115600667400684642E-11, -59.62592467094338389 ) ) ;
#159919 = DIRECTION ( 'NONE',  ( -0.000000000000000000, -0.000000000000000000, 1.000000000000000000 ) ) ;
#159920 = DIRECTION ( 'NONE',  ( 1.296989514748957922E-15, 0.9887567792719351711, -0.1495327102803594987 ) ) ;
#159921 = EDGE_CURVE ( 'NONE', #185471, #128716, #248869, .T. ) ;
#159922 = CARTESIAN_POINT ( 'NONE',  ( 21.05315837390880418, 11.74999999924401273, -60.15835600047963538 ) ) ;
#159923 = VERTEX_POINT ( 'NONE', #56914 ) ;
#159925 = DIRECTION ( 'NONE',  ( 1.000000000000000000, 0.000000000000000000, 0.000000000000000000 ) ) ;
#159924 = LINE ( 'NONE', #64646, #11350 ) ;
#159926 = CARTESIAN_POINT ( 'NONE',  ( 20.94999999999999574, 6.350000000011161383, -76.84382208968317229 ) ) ;
#159927 = CIRCLE ( 'NONE', #155829, 0.1000000000000028644 ) ;
#159928 = DIRECTION ( 'NONE',  ( -1.000000000000000000, 0.000000000000000000, 0.000000000000000000 ) ) ;
#159929 = AXIS2_PLACEMENT_3D ( 'NONE', #2232, #182187, #200457 ) ;
#159930 = CARTESIAN_POINT ( 'NONE',  ( 21.05000000000000071, -9.399999999988844834, -57.10603087734755690 ) ) ;
#159931 = CARTESIAN_POINT ( 'NONE',  ( -20.99142135623731065, 36.02918351690956200, -236.0543695120160805 ) ) ;
#159932 = EDGE_LOOP ( 'NONE', ( #158171, #100441, #166019, #202038 ) ) ;
#159934 = VERTEX_POINT ( 'NONE', #196453 ) ;
#159933 = AXIS2_PLACEMENT_3D ( 'NONE', #97684, #15647, #233402 ) ;
#159935 = ORIENTED_EDGE ( 'NONE', *, *, #255603, .F. ) ;
#159936 = EDGE_CURVE ( 'NONE', #173723, #134395, #244566, .T. ) ;
#159937 = CARTESIAN_POINT ( 'NONE',  ( -21.05000000000000071, -0.08579911626261706170, -127.5860211185120221 ) ) ;
#159938 = ORIENTED_EDGE ( 'NONE', *, *, #173329, .F. ) ;
#159939 = CARTESIAN_POINT ( 'NONE',  ( 22.39999999999999503, 64.18196446391819165, -247.0985338183330668 ) ) ;
#159940 = VERTEX_POINT ( 'NONE', #80329 ) ;
#159941 = FACE_OUTER_BOUND ( 'NONE', #130932, .T. ) ;
#159942 = ADVANCED_FACE ( 'NONE', ( #16558 ), #9776, .F. ) ;
#159943 = EDGE_CURVE ( 'NONE', #72309, #224010, #214735, .T. ) ;
#159944 = VERTEX_POINT ( 'NONE', #158648 ) ;
#159945 = AXIS2_PLACEMENT_3D ( 'NONE', #181278, #200824, #24781 ) ;
#159946 = EDGE_CURVE ( 'NONE', #38057, #127487, #119504, .T. ) ;
#159947 = DIRECTION ( 'NONE',  ( 0.000000000000000000, 0.000000000000000000, -1.000000000000000000 ) ) ;
#159948 = AXIS2_PLACEMENT_3D ( 'NONE', #43883, #244636, #26914 ) ;
#159949 = VERTEX_POINT ( 'NONE', #235575 ) ;
#159950 = ORIENTED_EDGE ( 'NONE', *, *, #80906, .T. ) ;
#159951 = TOROIDAL_SURFACE ( 'NONE', #222251, 11.65000000000000036, 0.1000000000000000056 ) ;
#159952 = ORIENTED_EDGE ( 'NONE', *, *, #124439, .T. ) ;
#159953 = VECTOR ( 'NONE', #75191, 1000.000000000000000 ) ;
#159954 = DIRECTION ( 'NONE',  ( 0.000000000000000000, -1.000000000000000000, -6.352154140967427193E-15 ) ) ;
#159955 = CARTESIAN_POINT ( 'NONE',  ( 22.49806830649814060, 75.92253568368725780, -215.1729971393634457 ) ) ;
#159956 = CYLINDRICAL_SURFACE ( 'NONE', #234104, 1.749999999999998002 ) ;
#159957 = PLANE ( 'NONE',  #82129 ) ;
#159958 = DIRECTION ( 'NONE',  ( -1.000000000000000000, -0.000000000000000000, -0.000000000000000000 ) ) ;
#159959 = CARTESIAN_POINT ( 'NONE',  ( -21.05000000000000071, 1.116121084443477685E-11, -103.4000000000000199 ) ) ;
#159960 = EDGE_CURVE ( 'NONE', #52350, #212886, #169789, .T. ) ;
#159962 = LINE ( 'NONE', #222444, #32766 ) ;
#159961 = DIRECTION ( 'NONE',  ( 1.000000000000000000, -0.000000000000000000, -0.000000000000000000 ) ) ;
#159964 = ORIENTED_EDGE ( 'NONE', *, *, #167466, .T. ) ;
#159963 = CARTESIAN_POINT ( 'NONE',  ( 23.24999999999999645, 5.650000000011139001, -87.85000000000003695 ) ) ;
#159965 = CARTESIAN_POINT ( 'NONE',  ( 21.13498764882293557, 69.50438185653807466, -103.0247638792556870 ) ) ;
#159966 = VERTEX_POINT ( 'NONE', #34851 ) ;
#159967 = CARTESIAN_POINT ( 'NONE',  ( -18.41799967126738480, -9.499999999988851584, -141.0320698132550774 ) ) ;
#159968 = ORIENTED_EDGE ( 'NONE', *, *, #13314, .T. ) ;
#159969 = ORIENTED_EDGE ( 'NONE', *, *, #93239, .F. ) ;
#159970 = CARTESIAN_POINT ( 'NONE',  ( -20.54999999999999716, 44.01574086017817677, -236.0100308471058099 ) ) ;
#159972 = AXIS2_PLACEMENT_3D ( 'NONE', #211889, #54074, #250977 ) ;
#159971 = DIRECTION ( 'NONE',  ( -3.265361837132813093E-16, -1.000000000000000000, -6.982962677686266711E-15 ) ) ;
#159973 = DIRECTION ( 'NONE',  ( -1.000000000000000000, 6.731126513909287799E-15, -1.502524917684071019E-14 ) ) ;
#159974 = VECTOR ( 'NONE', #99725, 1000.000000000000000 ) ;
#159975 = VERTEX_POINT ( 'NONE', #15278 ) ;
#159976 = B_SPLINE_CURVE_WITH_KNOTS ( 'NONE', 3,
 ( #54138, #234060, #39753, #55393, #119273, #198785, #93267, #41029 ),
 .UNSPECIFIED., .F., .F.,
 ( 4, 2, 2, 4 ),
 ( 0.000000000000000000, 0.0001881495939909276559, 0.0002822243909863914567, 0.0003762991879818553117 ),
 .UNSPECIFIED. ) ;
#159977 = TOROIDAL_SURFACE ( 'NONE', #5798, 0.4000000000000009104, 0.1000000000000000056 ) ;
#159978 = AXIS2_PLACEMENT_3D ( 'NONE', #210462, #231319, #110059 ) ;
#159979 = DIRECTION ( 'NONE',  ( 6.938893903907030216E-14, 0.000000000000000000, -1.000000000000000000 ) ) ;
#159980 = ORIENTED_EDGE ( 'NONE', *, *, #228719, .F. ) ;
#159981 = ORIENTED_EDGE ( 'NONE', *, *, #177151, .F. ) ;
#159982 = AXIS2_PLACEMENT_3D ( 'NONE', #126905, #42234, #102163 ) ;
#159983 = LINE ( 'NONE', #218627, #228285 ) ;
#159984 = ORIENTED_EDGE ( 'NONE', *, *, #65959, .F. ) ;
#159985 = CARTESIAN_POINT ( 'NONE',  ( -21.07928932188134041, 75.90110485435778287, -142.8516241409176075 ) ) ;
#159986 = DIRECTION ( 'NONE',  ( -1.000000000000000000, 0.000000000000000000, 0.000000000000000000 ) ) ;
#159987 = DIRECTION ( 'NONE',  ( -1.000000000000000000, 0.000000000000000000, -0.000000000000000000 ) ) ;
#159988 = CARTESIAN_POINT ( 'NONE',  ( -20.94999999999999929, 7.120270961697594103, -37.15956304183931991 ) ) ;
#159989 = DIRECTION ( 'NONE',  ( 0.000000000000000000, -0.9910465087640860649, -0.1335171055202901413 ) ) ;
#159990 = ORIENTED_EDGE ( 'NONE', *, *, #58745, .T. ) ;
#159991 = CIRCLE ( 'NONE', #35105, 0.09999999999999939493 ) ;
#159992 = AXIS2_PLACEMENT_3D ( 'NONE', #5455, #2895, #122874 ) ;
#159993 = AXIS2_PLACEMENT_3D ( 'NONE', #211993, #8643, #68622 ) ;
#159994 = CYLINDRICAL_SURFACE ( 'NONE', #67187, 0.09999999999999939493 ) ;
#159995 = PLANE ( 'NONE',  #204102 ) ;
#159996 = CARTESIAN_POINT ( 'NONE',  ( -20.64999999999999858, 76.00000000001190870, -103.0231074845243029 ) ) ;
#159997 = ADVANCED_FACE ( 'NONE', ( #75261 ), #151469, .T. ) ;
#159998 = VERTEX_POINT ( 'NONE', #41271 ) ;
#160000 = VERTEX_POINT ( 'NONE', #223706 ) ;
#159999 = FACE_OUTER_BOUND ( 'NONE', #199015, .T. ) ;
#160001 = CARTESIAN_POINT ( 'NONE',  ( -23.15000000000000213, 76.00000000001170974, -69.52310748452431710 ) ) ;
#160002 = ADVANCED_FACE ( 'NONE', ( #182038 ), #219619, .T. ) ;
#160003 = FACE_OUTER_BOUND ( 'NONE', #132439, .T. ) ;
#160004 = FACE_OUTER_BOUND ( 'NONE', #157281, .T. ) ;
#160005 = CARTESIAN_POINT ( 'NONE',  ( -18.50000000000000000, 85.50000000001263345, -195.4231074845242802 ) ) ;
#160006 = DIRECTION ( 'NONE',  ( 0.000000000000000000, 0.9915357197604982575, -0.1298341882519033486 ) ) ;
#160007 = ORIENTED_EDGE ( 'NONE', *, *, #14679, .F. ) ;
#160008 = CARTESIAN_POINT ( 'NONE',  ( -20.64999999999999858, 68.75000000001205080, -124.2731074845243455 ) ) ;
#160009 = AXIS2_PLACEMENT_3D ( 'NONE', #28930, #150132, #168446 ) ;
#160010 = CARTESIAN_POINT ( 'NONE',  ( -23.49999999999994316, 77.83551161375991967, -47.52760213295649550 ) ) ;
#160011 = EDGE_CURVE ( 'NONE', #213246, #2766, #40614, .T. ) ;
#160012 = EDGE_CURVE ( 'NONE', #237128, #186823, #200314, .T. ) ;
#160013 = CARTESIAN_POINT ( 'NONE',  ( -18.39999999999999858, 77.13860723519890428, -241.8264964602989266 ) ) ;
#160015 = VECTOR ( 'NONE', #205293, 1000.000000000000000 ) ;
#160014 = CARTESIAN_POINT ( 'NONE',  ( 23.24999999999999289, 8.930358663153430854, -211.6945637661233377 ) ) ;
#160016 = CARTESIAN_POINT ( 'NONE',  ( 21.05000000000005400, 67.65000000001118963, -25.49719488170504533 ) ) ;
#160017 = VERTEX_POINT ( 'NONE', #43810 ) ;
#160018 = ORIENTED_EDGE ( 'NONE', *, *, #75518, .F. ) ;
#160019 = CARTESIAN_POINT ( 'NONE',  ( 21.05000000000000071, 1.148907358139439339E-11, -201.0000000000015064 ) ) ;
#160020 = CIRCLE ( 'NONE', #168428, 0.09999999999999824307 ) ;
#160021 = DIRECTION ( 'NONE',  ( 0.000000000000000000, -1.000000000000000000, -6.982962677686266711E-15 ) ) ;
#160022 = DIRECTION ( 'NONE',  ( 0.000000000000000000, 0.000000000000000000, 1.000000000000000000 ) ) ;
#160023 = CARTESIAN_POINT ( 'NONE',  ( 20.04142135623730070, 11.75000000001115907, -155.7499999999999716 ) ) ;
#160024 = ADVANCED_FACE ( 'NONE', ( #82891 ), #94725, .T. ) ;
#160025 = VERTEX_POINT ( 'NONE', #180756 ) ;
#160026 = CARTESIAN_POINT ( 'NONE',  ( -21.05000000000000071, 70.65782965956557859, -228.4198064469268559 ) ) ;
#160027 = AXIS2_PLACEMENT_3D ( 'NONE', #117998, #197524, #18891 ) ;
#160028 = EDGE_CURVE ( 'NONE', #132474, #22954, #159924, .T. ) ;
#160030 = AXIS2_PLACEMENT_3D ( 'NONE', #1256, #181217, #104209 ) ;
#160029 = CARTESIAN_POINT ( 'NONE',  ( -18.40000000000000213, 28.17589918783267322, -238.5974746063260739 ) ) ;
#160031 = CARTESIAN_POINT ( 'NONE',  ( 23.14999999999999858, 7.128833340094563376, -233.7327013124401276 ) ) ;
#160032 = PRODUCT_DEFINITION ( 'UNKNOWN', '', #202882, #40142 ) ;
#160033 = CARTESIAN_POINT ( 'NONE',  ( -23.25000000000000355, 70.35000000001207354, -123.8731074845243398 ) ) ;
#160034 = ORIENTED_EDGE ( 'NONE', *, *, #57080, .T. ) ;
#160035 = DIRECTION ( 'NONE',  ( 0.000000000000000000, -1.000000000000000000, -6.352154140967427193E-15 ) ) ;
#160036 = EDGE_CURVE ( 'NONE', #184931, #93175, #177952, .T. ) ;
#160037 = EDGE_LOOP ( 'NONE', ( #66946, #194872, #234938, #187741 ) ) ;
#160038 = EDGE_CURVE ( 'NONE', #93827, #29926, #165489, .T. ) ;
#160039 = DIRECTION ( 'NONE',  ( -1.000000000000000000, 0.000000000000000000, -0.000000000000000000 ) ) ;
#160040 = ADVANCED_FACE ( 'NONE', ( #145458 ), #211443, .F. ) ;
#160041 = CARTESIAN_POINT ( 'NONE',  ( 23.24999999999999645, 5.649999999999983480, -12.65000000000000746 ) ) ;
#160043 = AXIS2_PLACEMENT_3D ( 'NONE', #570, #175407, #217046 ) ;
#160042 = DIRECTION ( 'NONE',  ( 0.000000000000000000, 0.000000000000000000, -1.000000000000000000 ) ) ;
#160044 = CARTESIAN_POINT ( 'NONE',  ( 18.50596464788227280, 65.69367753730634263, -64.01892380663478832 ) ) ;
#160045 = CARTESIAN_POINT ( 'NONE',  ( 21.05000000000000071, 36.65892442174472876, -249.5511627012454596 ) ) ;
#160046 = LINE ( 'NONE', #218687, #238780 ) ;
#160047 = DIRECTION ( 'NONE',  ( 0.000000000000000000, 0.000000000000000000, 1.000000000000000000 ) ) ;
#160048 = DIRECTION ( 'NONE',  ( -1.000000000000000000, -7.136802563874199107E-16, -1.554319503706929991E-16 ) ) ;
#160049 = CARTESIAN_POINT ( 'NONE',  ( -20.94999999999999929, 64.35000000001141984, -36.02310748452440237 ) ) ;
#160050 = VECTOR ( 'NONE', #210548, 1000.000000000000000 ) ;
#160051 = DIRECTION ( 'NONE',  ( 1.000000000000000000, 0.000000000000000000, 0.000000000000000000 ) ) ;
#160052 = DIRECTION ( 'NONE',  ( -1.000000000000000000, 0.000000000000000000, 0.000000000000000000 ) ) ;
#160054 = EDGE_CURVE ( 'NONE', #220241, #192597, #69996, .T. ) ;
#160053 = CARTESIAN_POINT ( 'NONE',  ( -18.50000000000000000, 2.859758780633683273, -208.6670499591424459 ) ) ;
#160055 = VECTOR ( 'NONE', #192265, 1000.000000000000114 ) ;
#160056 = CARTESIAN_POINT ( 'NONE',  ( -21.05000000000000426, 69.58624026620138636, -69.43749442372039482 ) ) ;
#160057 = CARTESIAN_POINT ( 'NONE',  ( -18.39999999999999858, 85.68240343348850274, -129.8662641071115047 ) ) ;
#160058 = AXIS2_PLACEMENT_3D ( 'NONE', #34143, #112370, #255669 ) ;
#160059 = VECTOR ( 'NONE', #17326, 1000.000000000000000 ) ;
#160060 = ORIENTED_EDGE ( 'NONE', *, *, #79067, .F. ) ;
#160061 = CARTESIAN_POINT ( 'NONE',  ( 21.05000000000000071, 6.496686585767979416, -0.01465611851322024678 ) ) ;
#160062 = DIRECTION ( 'NONE',  ( 0.000000000000000000, -7.116814260417668513E-15, 1.000000000000000000 ) ) ;
#160063 = DIRECTION ( 'NONE',  ( 0.000000000000000000, -0.000000000000000000, 1.000000000000000000 ) ) ;
#160064 = ORIENTED_EDGE ( 'NONE', *, *, #24345, .T. ) ;
#160065 = CARTESIAN_POINT ( 'NONE',  ( -22.48479450179659977, 0.04699158119804078271, -55.35000155374843445 ) ) ;
#160066 = EDGE_CURVE ( 'NONE', #228447, #111770, #184592, .T. ) ;
#160067 = DIRECTION ( 'NONE',  ( 0.000000000000000000, -0.8814952561685545085, 0.4721928772782730821 ) ) ;
#160068 = ORIENTED_EDGE ( 'NONE', *, *, #88974, .T. ) ;
#160069 = CARTESIAN_POINT ( 'NONE',  ( -16.86420534634261514, 9.970615445602874161, -188.4183365492373525 ) ) ;
#160070 = LINE ( 'NONE', #102602, #10059 ) ;
#160071 = EDGE_LOOP ( 'NONE', ( #122462, #219876, #92624, #253104 ) ) ;
#160072 = CIRCLE ( 'NONE', #80920, 0.1000000000000017680 ) ;
#160073 = ORIENTED_EDGE ( 'NONE', *, *, #168617, .F. ) ;
#160074 = DIRECTION ( 'NONE',  ( 0.000000000000000000, 0.9998779222360102414, 0.01562499999996356907 ) ) ;
#160075 = ADVANCED_FACE ( 'NONE', ( #140319 ), #122064, .F. ) ;
#160076 = VECTOR ( 'NONE', #76592, 1000.000000000000000 ) ;
#160077 = EDGE_LOOP ( 'NONE', ( #240284, #45952, #47795, #246937 ) ) ;
#160078 = CARTESIAN_POINT ( 'NONE',  ( 21.04999999999999716, 0.01471785652413675274, 6.344723404090222729 ) ) ;
#160079 = CYLINDRICAL_SURFACE ( 'NONE', #103091, 0.09999999999999939493 ) ;
#160081 = CARTESIAN_POINT ( 'NONE',  ( 21.09813707148777340, 34.01986380303547008, -243.7369249987247883 ) ) ;
#160080 = UNCERTAINTY_MEASURE_WITH_UNIT (LENGTH_MEASURE( 1.000000000000000082E-05 ), #208057, 'distance_accuracy_value', 'NONE');
#160082 = EDGE_CURVE ( 'NONE', #36165, #209893, #57483, .T. ) ;
#160083 = CARTESIAN_POINT ( 'NONE',  ( 21.05000000000000071, 1.115600667400684642E-11, -69.00000000000000000 ) ) ;
#160084 = CARTESIAN_POINT ( 'NONE',  ( -20.54999999999999361, 64.35000000001198828, -115.1731074845243796 ) ) ;
#160085 = FACE_OUTER_BOUND ( 'NONE', #153436, .T. ) ;
#160086 = CARTESIAN_POINT ( 'NONE',  ( -23.25000000000000000, 76.00000000001165290, -69.52310748452431710 ) ) ;
#160087 = CARTESIAN_POINT ( 'NONE',  ( -23.15000000000000213, 11.65000000000000036, -21.34999999999999787 ) ) ;
#160089 = ORIENTED_EDGE ( 'NONE', *, *, #183764, .F. ) ;
#160088 = CARTESIAN_POINT ( 'NONE',  ( 23.25000000000000000, 69.45000000001229523, -157.6731074845243938 ) ) ;
#160090 = ORIENTED_EDGE ( 'NONE', *, *, #256443, .F. ) ;
#160092 = DIRECTION ( 'NONE',  ( 1.000000000000000000, -0.000000000000000000, -0.000000000000000000 ) ) ;
#160091 = CARTESIAN_POINT ( 'NONE',  ( -20.94999999999999574, 11.62071067812980907, -160.6315833476590456 ) ) ;
#160094 = EDGE_LOOP ( 'NONE', ( #253745, #25036, #91094, #113917 ) ) ;
#160093 = CARTESIAN_POINT ( 'NONE',  ( -16.80070461187903774, 60.93856303923769957, -221.0446580500125435 ) ) ;
#160095 = ORIENTED_EDGE ( 'NONE', *, *, #227842, .T. ) ;
#160096 = CARTESIAN_POINT ( 'NONE',  ( 22.39999999999999503, 68.20922040163875977, -136.6231074845243540 ) ) ;
#160097 = DIRECTION ( 'NONE',  ( -1.000000000000000000, -0.000000000000000000, -0.000000000000000000 ) ) ;
#160098 = ADVANCED_FACE ( 'NONE', ( #22991 ), #124631, .T. ) ;
#160099 = CONICAL_SURFACE ( 'NONE', #226698, 6.250000000000005329, 0.7853981633974431720 ) ;
#160100 = ADVANCED_FACE ( 'NONE', ( #103745 ), #223891, .F. ) ;
#160101 = CARTESIAN_POINT ( 'NONE',  ( 21.05000000000000071, -8.999999999988842703, -90.60603087734760663 ) ) ;
#160102 = CYLINDRICAL_SURFACE ( 'NONE', #243456, 0.09999999999999939493 ) ;
#160103 = CYLINDRICAL_SURFACE ( 'NONE', #77436, 0.09999999999999939493 ) ;
#160104 = CARTESIAN_POINT ( 'NONE',  ( 23.25000000000000000, 87.75000000001229239, -157.8731074845242688 ) ) ;
#160105 = DIRECTION ( 'NONE',  ( 0.000000000000000000, 0.000000000000000000, 1.000000000000000000 ) ) ;
#160106 = CARTESIAN_POINT ( 'NONE',  ( -21.14999999999999503, 11.75000000001115197, -73.91914724595881125 ) ) ;
#160107 = ORIENTED_EDGE ( 'NONE', *, *, #62413, .F. ) ;
#160108 = EDGE_LOOP ( 'NONE', ( #59476, #237161, #117561, #130276 ) ) ;
#160109 = DIRECTION ( 'NONE',  ( -1.000000000000000000, 0.000000000000000000, -0.000000000000000000 ) ) ;
#160110 = TOROIDAL_SURFACE ( 'NONE', #210171, 0.2000000000000000111, 0.1000000000000000056 ) ;
#160111 = EDGE_CURVE ( 'NONE', #98224, #192518, #232316, .T. ) ;
#160112 = AXIS2_PLACEMENT_3D ( 'NONE', #144298, #118365, #21825 ) ;
#160113 = ORIENTED_EDGE ( 'NONE', *, *, #147360, .T. ) ;
#160114 = CARTESIAN_POINT ( 'NONE',  ( 18.59999999999999432, 2.859758780633683273, -208.6670499591424459 ) ) ;
#160116 = ADVANCED_FACE ( 'NONE', ( #149350 ), #50204, .F. ) ;
#160115 = ORIENTED_EDGE ( 'NONE', *, *, #215171, .T. ) ;
#160117 = CARTESIAN_POINT ( 'NONE',  ( 21.14999999999999858, 75.90220970870321082, -109.2809220950004345 ) ) ;
#160118 = CIRCLE ( 'NONE', #72628, 11.69999999999998863 ) ;
#160119 = CARTESIAN_POINT ( 'NONE',  ( 23.14999999999999858, -2.099999999988846344, -100.5000000000000426 ) ) ;
#160120 = CARTESIAN_POINT ( 'NONE',  ( -21.14999999999999858, 31.98723526783714988, -238.8784020251475511 ) ) ;
#160121 = EDGE_CURVE ( 'NONE', #13346, #156025, #194895, .T. ) ;
#160122 = DIRECTION ( 'NONE',  ( 0.000000000000000000, -0.9126074666063545004, -0.4088369013363783999 ) ) ;
#160123 = CARTESIAN_POINT ( 'NONE',  ( 20.94999999999999929, 6.650000000011155876, -121.7500000000000426 ) ) ;
#160124 = ORIENTED_EDGE ( 'NONE', *, *, #183465, .T. ) ;
#160125 = DIRECTION ( 'NONE',  ( 0.000000000000000000, 0.9887567792719329507, 0.1495327102803732933 ) ) ;
#160126 = ORIENTED_EDGE ( 'NONE', *, *, #169361, .F. ) ;
#160127 = DIRECTION ( 'NONE',  ( 0.000000000000000000, 0.000000000000000000, -1.000000000000000000 ) ) ;
#160128 = CARTESIAN_POINT ( 'NONE',  ( 20.94999999999999574, -1.162701749926853712, -175.5999999999999659 ) ) ;
#160129 = EDGE_CURVE ( 'NONE', #67500, #51561, #178147, .T. ) ;
#160130 = DIRECTION ( 'NONE',  ( 0.000000000000000000, -6.982962677686266711E-15, 1.000000000000000000 ) ) ;
#160131 = CARTESIAN_POINT ( 'NONE',  ( 20.85000000000000142, 7.070967871809997973, -204.7465642218682547 ) ) ;
#160133 = ORIENTED_EDGE ( 'NONE', *, *, #246271, .F. ) ;
#160132 = EDGE_CURVE ( 'NONE', #198388, #66243, #249065, .T. ) ;
#160134 = CARTESIAN_POINT ( 'NONE',  ( -23.25000000000000000, 67.23127455305841238, -235.8551265064783991 ) ) ;
#160136 = VERTEX_POINT ( 'NONE', #51474 ) ;
#160135 = CIRCLE ( 'NONE', #134952, 0.2000000000000042577 ) ;
#160139 = ORIENTED_EDGE ( 'NONE', *, *, #160867, .T. ) ;
#160138 = CARTESIAN_POINT ( 'NONE',  ( 18.59999999999999432, 22.88260507592945814, -249.4775442468527729 ) ) ;
#160137 = DIRECTION ( 'NONE',  ( 0.000000000000000000, 0.000000000000000000, 1.000000000000000000 ) ) ;
#160140 = DIRECTION ( 'NONE',  ( -1.000000000000000000, 0.000000000000000000, 0.000000000000000000 ) ) ;
#160141 = AXIS2_PLACEMENT_3D ( 'NONE', #133184, #211433, #171072 ) ;
#160142 = AXIS2_PLACEMENT_3D ( 'NONE', #81851, #143127, #162729 ) ;
#160143 = DIRECTION ( 'NONE',  ( 1.000000000000000000, 0.000000000000000000, 0.000000000000000000 ) ) ;
#160144 = EDGE_LOOP ( 'NONE', ( #162295, #27456, #158903, #143261 ) ) ;
#160146 = CARTESIAN_POINT ( 'NONE',  ( 18.39999999999999858, 85.50000000001209344, -129.9229180933022576 ) ) ;
#160145 = VECTOR ( 'NONE', #155249, 1000.000000000000000 ) ;
#160147 = CARTESIAN_POINT ( 'NONE',  ( -16.93234230245721861, 9.998107370558241058, -54.41769028166626043 ) ) ;
#160148 = EDGE_CURVE ( 'NONE', #50342, #98958, #245859, .T. ) ;
#160149 = DIRECTION ( 'NONE',  ( 0.000000000000000000, -1.000000000000000000, 0.000000000000000000 ) ) ;
#160150 = ADVANCED_FACE ( 'NONE', ( #206727 ), #47628, .F. ) ;
#160152 = ORIENTED_EDGE ( 'NONE', *, *, #51416, .T. ) ;
#160151 = DIRECTION ( 'NONE',  ( 0.000000000000000000, -1.000000000000000000, -6.982962677686265922E-15 ) ) ;
#160153 = VECTOR ( 'NONE', #247588, 1000.000000000000000 ) ;
#160154 = TOROIDAL_SURFACE ( 'NONE', #1709, 0.2000000000000000111, 0.1000000000000000056 ) ;
#160155 = DIRECTION ( 'NONE',  ( 1.000000000000000000, 0.000000000000000000, 0.000000000000000000 ) ) ;
#160156 = VECTOR ( 'NONE', #133751, 1000.000000000000114 ) ;
#160157 = ORIENTED_EDGE ( 'NONE', *, *, #205067, .T. ) ;
#160158 = DIRECTION ( 'NONE',  ( -1.000000000000000000, 0.000000000000000000, 0.000000000000000000 ) ) ;
#160159 = CARTESIAN_POINT ( 'NONE',  ( 20.94999999999999574, -11.48912529306490349, -170.4999999999999716 ) ) ;
#160160 = VECTOR ( 'NONE', #37499, 1000.000000000000000 ) ;
#160161 = CARTESIAN_POINT ( 'NONE',  ( -18.46919391072055561, -9.670724388266535243, -140.6738035317996491 ) ) ;
#160162 = ORIENTED_EDGE ( 'NONE', *, *, #231325, .F. ) ;
#160163 = DIRECTION ( 'NONE',  ( -1.000000000000000000, -0.000000000000000000, -0.000000000000000000 ) ) ;
#160164 = ORIENTED_EDGE ( 'NONE', *, *, #103284, .T. ) ;
#160165 = DIRECTION ( 'NONE',  ( -1.734723475976746257E-13, 0.9228863568391486583, 0.3850724248244262182 ) ) ;
#160166 = AXIS2_PLACEMENT_3D ( 'NONE', #246092, #83110, #144380 ) ;
#160167 = CARTESIAN_POINT ( 'NONE',  ( -21.00000000000000000, 6.841561409100513025, 9.675512259591560138 ) ) ;
#160168 = CARTESIAN_POINT ( 'NONE',  ( 20.85000000000000142, -1.164121893230052995, -74.91484808557160591 ) ) ;
#160169 = ORIENTED_EDGE ( 'NONE', *, *, #79891, .F. ) ;
#160170 = LINE ( 'NONE', #200546, #125484 ) ;
#160171 = AXIS2_PLACEMENT_3D ( 'NONE', #33492, #175550, #210801 ) ;
#160172 = VECTOR ( 'NONE', #170718, 1000.000000000000000 ) ;
#160173 = CARTESIAN_POINT ( 'NONE',  ( -20.54999999999999716, 76.00000000001126921, -203.5231074845248997 ) ) ;
#160174 = CARTESIAN_POINT ( 'NONE',  ( -20.87155475150660777, 64.25000000001250555, -176.9275209553668162 ) ) ;
#160175 = ORIENTED_EDGE ( 'NONE', *, *, #231462, .F. ) ;
#160176 = DIRECTION ( 'NONE',  ( 1.000000000000000000, 0.000000000000000000, 0.000000000000000000 ) ) ;
#160177 = FACE_OUTER_BOUND ( 'NONE', #182670, .T. ) ;
#160178 = ORIENTED_EDGE ( 'NONE', *, *, #93735, .F. ) ;
#160179 = CARTESIAN_POINT ( 'NONE',  ( 21.05000000000000071, 85.00000000001179501, -78.91707660717668205 ) ) ;
#160181 = EDGE_CURVE ( 'NONE', #42935, #60608, #103276, .T. ) ;
#160180 = B_SPLINE_CURVE_WITH_KNOTS ( 'NONE', 3,
 ( #29000, #83746, #108489, #44676, #188037, #45946, #162064, #204997, #241578, #105890, #23848, #124216, #64227, #103334, #247992, #152789, #13255, #10682, #69383 ),
 .UNSPECIFIED., .F., .F.,
 ( 4, 3, 3, 3, 3, 3, 4 ),
 ( 0.000000000000000000, 7.110282409889723450E-05, 0.0001508797727291417718, 0.0002027344179858366850, 0.0002343294522349049320, 0.0002454816334821112531, 0.0002619873080085701302 ),
 .UNSPECIFIED. ) ;
#160182 = EDGE_LOOP ( 'NONE', ( #170567, #205804, #87324, #221743, #119129 ) ) ;
#160183 = VERTEX_POINT ( 'NONE', #31969 ) ;
#160184 = DIRECTION ( 'NONE',  ( 0.000000000000000000, 0.000000000000000000, -1.000000000000000000 ) ) ;
#160185 = EDGE_LOOP ( 'NONE', ( #237157, #191471, #205637, #78100 ) ) ;
#160187 = ORIENTED_EDGE ( 'NONE', *, *, #244043, .F. ) ;
#160186 = CARTESIAN_POINT ( 'NONE',  ( -23.25000000000000000, 1.115600667400684642E-11, -200.9999999999999432 ) ) ;
#160190 = VERTEX_POINT ( 'NONE', #30690 ) ;
#160189 = VERTEX_POINT ( 'NONE', #33265 ) ;
#160188 = FACE_OUTER_BOUND ( 'NONE', #32543, .T. ) ;
#160191 = CIRCLE ( 'NONE', #126846, 0.1000000000000001305 ) ;
#160192 = CARTESIAN_POINT ( 'NONE',  ( -33.72168855820451938, 44.13548170601888643, -235.2989316066074821 ) ) ;
#160193 = CARTESIAN_POINT ( 'NONE',  ( -20.91682497891422798, 65.67736539654895012, -30.46251168765720152 ) ) ;
#160194 = AXIS2_PLACEMENT_3D ( 'NONE', #95317, #212709, #53625 ) ;
#160195 = DIRECTION ( 'NONE',  ( 1.000000000000000000, 0.000000000000000000, 0.000000000000000000 ) ) ;
#160196 = PLANE ( 'NONE',  #252382 ) ;
#160197 = EDGE_CURVE ( 'NONE', #11112, #67142, #111482, .T. ) ;
#160198 = VECTOR ( 'NONE', #254660, 999.9999999999998863 ) ;
#160199 = DIRECTION ( 'NONE',  ( 2.952720810173289112E-16, -1.000000000000000000, 0.000000000000000000 ) ) ;
#160200 = DIRECTION ( 'NONE',  ( 1.000000000000000000, 0.000000000000000000, 0.000000000000000000 ) ) ;
#160201 = CARTESIAN_POINT ( 'NONE',  ( 23.14999999999999858, 1.148907358139439339E-11, -201.0000000000015064 ) ) ;
#160202 = ORIENTED_EDGE ( 'NONE', *, *, #61908, .F. ) ;
#160204 = VERTEX_POINT ( 'NONE', #12404 ) ;
#160203 = AXIS2_PLACEMENT_3D ( 'NONE', #223584, #171383, #170102 ) ;
#160205 = DIRECTION ( 'NONE',  ( 0.000000000000000000, 6.982962677686267499E-15, -1.000000000000000000 ) ) ;
#160206 = VECTOR ( 'NONE', #143575, 1000.000000000000000 ) ;
#160208 = VERTEX_POINT ( 'NONE', #170228 ) ;
#160207 = CYLINDRICAL_SURFACE ( 'NONE', #216059, 0.09999999999998898659 ) ;
#160209 = CARTESIAN_POINT ( 'NONE',  ( -20.54999999999999716, 85.50000000001207923, -126.6291383618717816 ) ) ;
#160210 = ORIENTED_EDGE ( 'NONE', *, *, #190122, .F. ) ;
#160211 = CARTESIAN_POINT ( 'NONE',  ( -22.59999999999999787, 11.74956712348939192, 0.1008583690987087389 ) ) ;
#160212 = ORIENTED_EDGE ( 'NONE', *, *, #91479, .T. ) ;
#160213 = DIRECTION ( 'NONE',  ( 0.000000000000000000, 1.000000000000000000, 0.000000000000000000 ) ) ;
#160214 = VECTOR ( 'NONE', #189726, 1000.000000000000000 ) ;
#160215 = AXIS2_PLACEMENT_3D ( 'NONE', #199829, #144948, #43309 ) ;
#160216 = VERTEX_POINT ( 'NONE', #28119 ) ;
#160217 = AXIS2_PLACEMENT_3D ( 'NONE', #132324, #31972, #68514 ) ;
#160218 = CARTESIAN_POINT ( 'NONE',  ( -21.14999999999999858, 11.75000000001115552, -140.7838656629781724 ) ) ;
#160219 = DIRECTION ( 'NONE',  ( 0.000000000000000000, -1.000000000000000000, -0.000000000000000000 ) ) ;
#160220 = VECTOR ( 'NONE', #70309, 1000.000000000000000 ) ;
#160222 = ORIENTED_EDGE ( 'NONE', *, *, #79583, .T. ) ;
#160221 = ORIENTED_EDGE ( 'NONE', *, *, #106530, .F. ) ;
#160223 = ORIENTED_EDGE ( 'NONE', *, *, #228591, .F. ) ;
#160224 = CARTESIAN_POINT ( 'NONE',  ( -18.59999999999999787, 5.950000000011100632, -43.80570230503486329 ) ) ;
#160225 = ORIENTED_EDGE ( 'NONE', *, *, #35631, .T. ) ;
#160226 = ORIENTED_EDGE ( 'NONE', *, *, #180054, .T. ) ;
#160227 = DIRECTION ( 'NONE',  ( 1.000000000000000000, 0.000000000000000000, 0.000000000000000000 ) ) ;
#160229 = VERTEX_POINT ( 'NONE', #11102 ) ;
#160228 = DIRECTION ( 'NONE',  ( 0.000000000000000000, -0.2128009952262243931, 0.9770955615653611481 ) ) ;
#160230 = TOROIDAL_SURFACE ( 'NONE', #101908, 3.899999999999999467, 0.1000000000000000056 ) ;
#160232 = DIRECTION ( 'NONE',  ( 0.000000000000000000, -6.982962677686266711E-15, 1.000000000000000000 ) ) ;
#160231 = CARTESIAN_POINT ( 'NONE',  ( -20.64999999999999858, 73.50000000001254818, -183.2477294072864709 ) ) ;
#160233 = LINE ( 'NONE', #58511, #90962 ) ;
#160234 = FACE_OUTER_BOUND ( 'NONE', #56893, .T. ) ;
#160235 = CARTESIAN_POINT ( 'NONE',  ( 21.05000000000000071, 67.22371710471989559, -170.0231074845244166 ) ) ;
#160236 = ORIENTED_EDGE ( 'NONE', *, *, #218316, .T. ) ;
#160237 = ORIENTED_EDGE ( 'NONE', *, *, #5960, .F. ) ;
#160238 = CARTESIAN_POINT ( 'NONE',  ( -16.92507428761700439, 66.05000000001182059, -82.23650494414594903 ) ) ;
#160239 = LINE ( 'NONE', #241042, #22570 ) ;
#160240 = DIRECTION ( 'NONE',  ( 1.000000000000000000, -0.000000000000000000, -0.000000000000000000 ) ) ;
#160241 = EDGE_CURVE ( 'NONE', #72361, #15545, #128479, .T. ) ;
#160242 = ORIENTED_EDGE ( 'NONE', *, *, #244998, .T. ) ;
#160243 = CARTESIAN_POINT ( 'NONE',  ( -23.15000000000000213, 64.35000000001238618, -170.0231074845244166 ) ) ;
#160244 = AXIS2_PLACEMENT_3D ( 'NONE', #186500, #189060, #6562 ) ;
#160245 = AXIS2_PLACEMENT_3D ( 'NONE', #29686, #170505, #212156 ) ;
#160246 = DIRECTION ( 'NONE',  ( 0.000000000000000000, 0.8814952561688430555, -0.4721928772777346239 ) ) ;
#160247 = AXIS2_PLACEMENT_3D ( 'NONE', #52251, #186668, #9295 ) ;
#160248 = CARTESIAN_POINT ( 'NONE',  ( -13.22483237240078147, 12.45018385075468537, -213.8211107588515745 ) ) ;
#160249 = VERTEX_POINT ( 'NONE', #110185 ) ;
#160250 = EDGE_LOOP ( 'NONE', ( #149318, #31584, #241804, #159513 ) ) ;
#160251 = EDGE_CURVE ( 'NONE', #201551, #96655, #236555, .T. ) ;
#160252 = CARTESIAN_POINT ( 'NONE',  ( 20.94999999999999929, 68.05808644172607558, -213.7045301755741491 ) ) ;
#160253 = DIRECTION ( 'NONE',  ( 0.000000000000000000, -1.000000000000000000, 0.000000000000000000 ) ) ;
#160254 = ORIENTED_EDGE ( 'NONE', *, *, #196399, .T. ) ;
#160255 = DIRECTION ( 'NONE',  ( 0.000000000000000000, 0.000000000000000000, -1.000000000000000000 ) ) ;
#160256 = ORIENTED_EDGE ( 'NONE', *, *, #144705, .T. ) ;
#160257 = DIRECTION ( 'NONE',  ( 0.000000000000000000, 0.000000000000000000, 1.000000000000000000 ) ) ;
#160258 = DIRECTION ( 'NONE',  ( 0.000000000000000000, 0.000000000000000000, -1.000000000000000000 ) ) ;
#160260 = CARTESIAN_POINT ( 'NONE',  ( 23.14999999999998437, 11.75000000001115552, -167.4999999999999716 ) ) ;
#160259 = DIRECTION ( 'NONE',  ( 0.000000000000000000, 0.000000000000000000, -1.000000000000000000 ) ) ;
#160261 = EDGE_CURVE ( 'NONE', #47267, #240428, #257185, .T. ) ;
#160262 = CARTESIAN_POINT ( 'NONE',  ( -23.15000000000000213, 85.60000000001276987, -215.2731074845242745 ) ) ;
#160263 = CARTESIAN_POINT ( 'NONE',  ( -20.07928932188135107, 66.77928932189284694, -48.27310748452438816 ) ) ;
#160264 = EDGE_LOOP ( 'NONE', ( #4869, #93275, #45379 ) ) ;
#160265 = EDGE_CURVE ( 'NONE', #167384, #195708, #112768, .T. ) ;
#160266 = CARTESIAN_POINT ( 'NONE',  ( -23.25000000000000000, 1.999999999999998224, -20.87537807723790095 ) ) ;
#160267 = CIRCLE ( 'NONE', #56162, 0.09999999999999971412 ) ;
#160269 = EDGE_LOOP ( 'NONE', ( #7843, #192675, #216174, #174412, #171913, #111105 ) ) ;
#160268 = ORIENTED_EDGE ( 'NONE', *, *, #154416, .F. ) ;
#160270 = ORIENTED_EDGE ( 'NONE', *, *, #124467, .T. ) ;
#160271 = ORIENTED_EDGE ( 'NONE', *, *, #188638, .T. ) ;
#160272 = CARTESIAN_POINT ( 'NONE',  ( 22.47071067811865319, 7.720074744509199505, -33.40090754529740025 ) ) ;
#160273 = CARTESIAN_POINT ( 'NONE',  ( -18.49499033040907392, -7.690199103985159823, -210.0417310202402632 ) ) ;
#160274 = AXIS2_PLACEMENT_3D ( 'NONE', #167099, #69261, #230910 ) ;
#160275 = CARTESIAN_POINT ( 'NONE',  ( -20.64999999999999858, 7.150000000011155876, -155.2500000000000284 ) ) ;
#160276 = DIRECTION ( 'NONE',  ( 1.000000000000000000, 2.952720810173289112E-16, -0.000000000000000000 ) ) ;
#160277 = CARTESIAN_POINT ( 'NONE',  ( 21.05000000000000071, 87.65000000001246860, -173.0231074845243029 ) ) ;
#160278 = EDGE_CURVE ( 'NONE', #32613, #49225, #208033, .T. ) ;
#160280 = CARTESIAN_POINT ( 'NONE',  ( 20.94999999999999929, 59.10678033798691189, -225.7992625810339575 ) ) ;
#160279 = CARTESIAN_POINT ( 'NONE',  ( 20.97250901189795513, 10.62456803370188041, -7.664545716966992828 ) ) ;
#160281 = EDGE_LOOP ( 'NONE', ( #199226, #191531, #132122, #158874 ) ) ;
#160282 = DIRECTION ( 'NONE',  ( 0.000000000000000000, 8.881784197000696176E-16, -1.000000000000000000 ) ) ;
#160283 = ORIENTED_EDGE ( 'NONE', *, *, #195427, .F. ) ;
#160284 = FACE_OUTER_BOUND ( 'NONE', #244572, .T. ) ;
#160285 = ORIENTED_EDGE ( 'NONE', *, *, #15598, .T. ) ;
#160286 = ORIENTED_EDGE ( 'NONE', *, *, #46324, .T. ) ;
#160287 = FACE_OUTER_BOUND ( 'NONE', #70410, .T. ) ;
#160288 = CYLINDRICAL_SURFACE ( 'NONE', #47638, 0.1000000000000028644 ) ;
#160289 = DIRECTION ( 'NONE',  ( 1.000000000000000000, 3.190570557967288949E-16, 6.948722487160392945E-17 ) ) ;
#160290 = CARTESIAN_POINT ( 'NONE',  ( 12.93225390519044460, 9.417651958852157890, -82.35878739244050450 ) ) ;
#160291 = AXIS2_PLACEMENT_3D ( 'NONE', #95633, #74837, #194773 ) ;
#160292 = AXIS2_PLACEMENT_3D ( 'NONE', #120364, #19960, #199883 ) ;
#160293 = CARTESIAN_POINT ( 'NONE',  ( -20.93284271247462058, 56.02567683926421438, -227.9999002286039058 ) ) ;
#160294 = VERTEX_POINT ( 'NONE', #231446 ) ;
#160295 = ORIENTED_EDGE ( 'NONE', *, *, #25811, .F. ) ;
#160296 = DIRECTION ( 'NONE',  ( -0.7071067811865487940, 0.7071067811865463515, -7.215498431451184074E-16 ) ) ;
#160297 = ORIENTED_EDGE ( 'NONE', *, *, #167076, .F. ) ;
#160298 = CYLINDRICAL_SURFACE ( 'NONE', #35501, 0.09999999999999939493 ) ;
#160299 = LINE ( 'NONE', #243654, #123550 ) ;
#160300 = DIRECTION ( 'NONE',  ( 1.000000000000000000, 0.000000000000000000, 0.000000000000000000 ) ) ;
#160301 = CARTESIAN_POINT ( 'NONE',  ( -18.39999999999999858, -9.399999999988850163, -88.75000000000004263 ) ) ;
#160302 = CARTESIAN_POINT ( 'NONE',  ( 22.24259225415828567, 0.09906588346399246292, -59.50806212943462725 ) ) ;
#160303 = DIRECTION ( 'NONE',  ( 1.000000000000000000, 0.000000000000000000, 0.000000000000000000 ) ) ;
#160304 = FACE_OUTER_BOUND ( 'NONE', #207347, .T. ) ;
#160305 = DIRECTION ( 'NONE',  ( 1.000000000000000000, 0.000000000000000000, 0.000000000000000000 ) ) ;
#160306 = CARTESIAN_POINT ( 'NONE',  ( 21.13736287352038445, 8.046642376395153562, -121.3500000000000227 ) ) ;
#160307 = CARTESIAN_POINT ( 'NONE',  ( -22.59999999999999787, 11.74956712350054566, -133.8991416309013118 ) ) ;
#160308 = CIRCLE ( 'NONE', #193594, 0.09999999999999939493 ) ;
#160309 = FACE_OUTER_BOUND ( 'NONE', #7912, .T. ) ;
#160310 = AXIS2_PLACEMENT_3D ( 'NONE', #83691, #163288, #64180 ) ;
#160311 = AXIS2_PLACEMENT_3D ( 'NONE', #41004, #176652, #59205 ) ;
#160312 = CIRCLE ( 'NONE', #47823, 1.900000000000012790 ) ;
#160313 = EDGE_CURVE ( 'NONE', #110538, #187394, #40794, .T. ) ;
#160314 = ORIENTED_EDGE ( 'NONE', *, *, #99640, .T. ) ;
#160315 =( GEOMETRIC_REPRESENTATION_CONTEXT ( 3 ) GLOBAL_UNCERTAINTY_ASSIGNED_CONTEXT ( ( #94628 ) ) GLOBAL_UNIT_ASSIGNED_CONTEXT ( ( #172462, #171181, #91597 ) ) REPRESENTATION_CONTEXT ( 'NONE', 'WORKASPACE' ) );
#160316 = CARTESIAN_POINT ( 'NONE',  ( -18.40000000000000213, 23.66078093222370882, -229.5728445495489893 ) ) ;
#160317 = EDGE_LOOP ( 'NONE', ( #182249, #196768, #95720, #217123 ) ) ;
#160318 = ADVANCED_FACE ( 'NONE', ( #148046 ), #168238, .F. ) ;
#160319 = CARTESIAN_POINT ( 'NONE',  ( -22.39999999999999858, 0.1000000000111554016, -25.70922040162659883 ) ) ;
#160320 = DIRECTION ( 'NONE',  ( 0.000000000000000000, 0.7049548389605067023, -0.7092521942342977503 ) ) ;
#160321 = CARTESIAN_POINT ( 'NONE',  ( 22.45305468355011413, 64.25313205997872501, -247.2214437328679821 ) ) ;
#160322 = EDGE_LOOP ( 'NONE', ( #61186, #299, #256291, #137359 ) ) ;
#160323 = DIRECTION ( 'NONE',  ( -0.000000000000000000, 0.08413937888706959911, -0.9964539953858875254 ) ) ;
#160324 = ADVANCED_FACE ( 'NONE', ( #177889 ), #19934, .F. ) ;
#160325 = CARTESIAN_POINT ( 'NONE',  ( 21.05000000000000071, 84.66355140188063899, -45.54720860259157433 ) ) ;
#160326 = CARTESIAN_POINT ( 'NONE',  ( -21.65000000000000213, 62.65526179112262639, -225.0299194783148948 ) ) ;
#160327 = CARTESIAN_POINT ( 'NONE',  ( 23.14999999999999858, 36.65892442174935439, -249.5511627012433848 ) ) ;
#160328 = AXIS2_PLACEMENT_3D ( 'NONE', #7804, #28690, #224261 ) ;
#160329 = CARTESIAN_POINT ( 'NONE',  ( -16.93234230245721861, 9.998107370558241058, -121.4176902816662817 ) ) ;
#160330 = CARTESIAN_POINT ( 'NONE',  ( -16.81744102076749314, 66.05000000001157900, -56.87310748452438958 ) ) ;
#160331 = CIRCLE ( 'NONE', #131064, 0.1000000000000028644 ) ;
#160332 = VERTEX_POINT ( 'NONE', #252260 ) ;
#160333 = DIRECTION ( 'NONE',  ( -1.073024830501117725E-15, -6.982962677686266711E-15, 1.000000000000000000 ) ) ;
#160335 = ORIENTED_EDGE ( 'NONE', *, *, #163708, .F. ) ;
#160334 = CARTESIAN_POINT ( 'NONE',  ( -20.94999999999999929, 1.162701749949165642, -41.60000000000000142 ) ) ;
#160336 = CARTESIAN_POINT ( 'NONE',  ( -21.05000000000000071, 61.95000000001191154, -97.50941241376341395 ) ) ;
#160337 = EDGE_CURVE ( 'NONE', #206320, #213275, #45030, .T. ) ;
#160338 = CARTESIAN_POINT ( 'NONE',  ( 20.85000000000000142, 77.14957036958736580, -61.70719500002233815 ) ) ;
#160339 = DIRECTION ( 'NONE',  ( -3.469446951953635015E-14, -1.000000000000000000, 0.000000000000000000 ) ) ;
#160340 = ORIENTED_EDGE ( 'NONE', *, *, #156715, .F. ) ;
#160341 = CARTESIAN_POINT ( 'NONE',  ( -21.05000000000000071, 70.10000000001149090, -46.24220724918072989 ) ) ;
#160342 = CIRCLE ( 'NONE', #43606, 0.1000000000000106498 ) ;
#160343 = EDGE_CURVE ( 'NONE', #53624, #132943, #221432, .T. ) ;
#160344 = PRODUCT_CONTEXT ( 'NONE', #203932, 'mechanical' ) ;
#160345 = EDGE_CURVE ( 'NONE', #25296, #77581, #240662, .T. ) ;
#160346 = AXIS2_PLACEMENT_3D ( 'NONE', #237704, #36967, #59021 ) ;
#160347 = DIRECTION ( 'NONE',  ( -1.000000000000000000, -7.304098846218134667E-16, 4.217023435051678980E-16 ) ) ;
#160348 = ORIENTED_EDGE ( 'NONE', *, *, #167685, .F. ) ;
#160349 = CARTESIAN_POINT ( 'NONE',  ( -23.15000000000000213, 7.128833340094563376, -233.7327013124401276 ) ) ;
#160350 = CARTESIAN_POINT ( 'NONE',  ( -16.97683809663752186, 12.31632387104345305, -211.2641690508233125 ) ) ;
#160351 = EDGE_CURVE ( 'NONE', #60608, #42935, #128245, .T. ) ;
#160352 = CIRCLE ( 'NONE', #47870, 0.5000000000000008882 ) ;
#160354 = ORIENTED_EDGE ( 'NONE', *, *, #58089, .F. ) ;
#160353 = VECTOR ( 'NONE', #245980, 1000.000000000000000 ) ;
#160355 = EDGE_LOOP ( 'NONE', ( #48494, #54146, #174742, #97428 ) ) ;
#160356 = EDGE_CURVE ( 'NONE', #92109, #242050, #253121, .T. ) ;
#160357 = CARTESIAN_POINT ( 'NONE',  ( -16.87331047859649757, 66.05000000001224691, -149.1731074845244223 ) ) ;
#160358 = EDGE_CURVE ( 'NONE', #215216, #28556, #53230, .T. ) ;
#160359 = DIRECTION ( 'NONE',  ( 1.000000000000000000, -0.000000000000000000, -0.000000000000000000 ) ) ;
#160360 = CIRCLE ( 'NONE', #222662, 0.09999999999998304689 ) ;
#160361 = CARTESIAN_POINT ( 'NONE',  ( -21.05000000000000071, -0.09999999998884338825, -127.4593430482987912 ) ) ;
#160362 = CARTESIAN_POINT ( 'NONE',  ( 22.50000000000000000, 64.35042919246788529, -203.6231074845244393 ) ) ;
#160363 = CARTESIAN_POINT ( 'NONE',  ( 18.49999999999999289, 10.20857864377384416, -125.1500000000000341 ) ) ;
#160364 = LINE ( 'NONE', #82038, #201335 ) ;
#160366 = CARTESIAN_POINT ( 'NONE',  ( -15.75000000000000355, 9.850000000011133849, -150.7500000000000284 ) ) ;
#160365 = FACE_OUTER_BOUND ( 'NONE', #118500, .T. ) ;
#160367 = CARTESIAN_POINT ( 'NONE',  ( 19.75857864376268935, 62.39550153362034735, -208.7959266050682459 ) ) ;
#160368 = CARTESIAN_POINT ( 'NONE',  ( -23.25000000000000000, 76.00000000001136868, -28.12310748452432208 ) ) ;
#160369 = CARTESIAN_POINT ( 'NONE',  ( 18.51024323315077069, 65.68895814178189596, -30.50265578621380769 ) ) ;
#160370 = DIRECTION ( 'NONE',  ( -1.000000000000000000, 7.304098846218164250E-16, -4.217023435051628197E-16 ) ) ;
#160371 = ORIENTED_EDGE ( 'NONE', *, *, #21973, .F. ) ;
#160372 = ORIENTED_EDGE ( 'NONE', *, *, #36266, .T. ) ;
#160373 = DIRECTION ( 'NONE',  ( 1.000000000000000000, 0.000000000000000000, 0.000000000000000000 ) ) ;
#160375 = CARTESIAN_POINT ( 'NONE',  ( -23.25000000000000000, 76.00000000001267608, -203.5231074845243597 ) ) ;
#160374 = DIRECTION ( 'NONE',  ( 1.000000000000000000, 0.000000000000000000, 0.000000000000000000 ) ) ;
#160376 = EDGE_CURVE ( 'NONE', #168461, #30860, #190616, .T. ) ;
#160377 = DIRECTION ( 'NONE',  ( 7.304098846218134667E-16, -1.000000000000000000, 0.000000000000000000 ) ) ;
#160379 = EDGE_CURVE ( 'NONE', #236931, #100676, #28316, .T. ) ;
#160378 = LINE ( 'NONE', #236030, #187253 ) ;
#160380 = CYLINDRICAL_SURFACE ( 'NONE', #6565, 2.000000000000001776 ) ;
#160381 = ORIENTED_EDGE ( 'NONE', *, *, #205610, .F. ) ;
#160382 = CARTESIAN_POINT ( 'NONE',  ( -23.15000000000000213, 11.65000000001115588, -160.4851942293460638 ) ) ;
#160383 = ORIENTED_EDGE ( 'NONE', *, *, #242263, .T. ) ;
#160384 = CIRCLE ( 'NONE', #143598, 0.1000000000000028644 ) ;
#160385 = EDGE_CURVE ( 'NONE', #57380, #228673, #136596, .T. ) ;
#160386 = CARTESIAN_POINT ( 'NONE',  ( -14.11361717019516426, 9.457426452488903124, -18.50004186840003939 ) ) ;
#160387 = ORIENTED_EDGE ( 'NONE', *, *, #149237, .T. ) ;
#160388 = DIRECTION ( 'NONE',  ( -1.000000000000000000, 2.952720810173289112E-16, 2.061873921506763405E-30 ) ) ;
#160389 = LINE ( 'NONE', #59951, #129722 ) ;
#160390 = CIRCLE ( 'NONE', #177140, 0.1000000000000002554 ) ;
#160391 = CIRCLE ( 'NONE', #60390, 11.75000000000001066 ) ;
#160392 = ORIENTED_EDGE ( 'NONE', *, *, #207044, .T. ) ;
#160393 = CARTESIAN_POINT ( 'NONE',  ( -16.97092634996621996, 65.99911103366474663, -190.8929647182265228 ) ) ;
#160394 = VERTEX_POINT ( 'NONE', #4356 ) ;
#160395 = DIRECTION ( 'NONE',  ( -1.000000000000000000, 2.952720810173289112E-16, 2.061873921506763405E-30 ) ) ;
#160397 = AXIS2_PLACEMENT_3D ( 'NONE', #196142, #102141, #61766 ) ;
#160396 = CARTESIAN_POINT ( 'NONE',  ( -18.40000000000000213, 5.650000000011139001, -191.7499999999999716 ) ) ;
#160398 = CYLINDRICAL_SURFACE ( 'NONE', #145073, 0.5000000000000004441 ) ;
#160399 = EDGE_CURVE ( 'NONE', #156378, #40297, #63048, .T. ) ;
#160400 = CARTESIAN_POINT ( 'NONE',  ( -18.39999999999999858, 77.13860723519891849, -241.8264964602989266 ) ) ;
#160401 = LINE ( 'NONE', #239922, #84748 ) ;
#160403 = CARTESIAN_POINT ( 'NONE',  ( 18.50596464788227280, 65.69367753730676895, -131.0189238066348310 ) ) ;
#160402 = CARTESIAN_POINT ( 'NONE',  ( -20.54999999999999716, 7.250000000011155521, -121.7500000000000426 ) ) ;
#160404 = AXIS2_PLACEMENT_3D ( 'NONE', #7799, #202140, #105566 ) ;
#160405 = DIRECTION ( 'NONE',  ( 0.000000000000000000, 6.982962677686266711E-15, -1.000000000000000000 ) ) ;
#160406 = EDGE_CURVE ( 'NONE', #71369, #94746, #20094, .T. ) ;
#160408 = VERTEX_POINT ( 'NONE', #102151 ) ;
#160407 = CARTESIAN_POINT ( 'NONE',  ( 20.74897398619119215, 65.40430697834564455, -128.8437960282674624 ) ) ;
#160410 = DIRECTION ( 'NONE',  ( -0.000000000000000000, 0.000000000000000000, -1.000000000000000000 ) ) ;
#160409 = CARTESIAN_POINT ( 'NONE',  ( 21.00000000000000000, 66.25000000001223555, -148.7731074845244450 ) ) ;
#160411 = ORIENTED_EDGE ( 'NONE', *, *, #29664, .F. ) ;
#160413 = ORIENTED_EDGE ( 'NONE', *, *, #187727, .T. ) ;
#160412 = CARTESIAN_POINT ( 'NONE',  ( 21.14999999999999503, 1.115600667400684642E-11, -161.2499999999999716 ) ) ;
#160414 = ORIENTED_EDGE ( 'NONE', *, *, #98244, .T. ) ;
#160415 = FACE_OUTER_BOUND ( 'NONE', #107643, .T. ) ;
#160416 = DIRECTION ( 'NONE',  ( -0.000000000000000000, 1.000000000000000000, 6.982962677686266711E-15 ) ) ;
#160417 = CARTESIAN_POINT ( 'NONE',  ( -21.05000000000000071, -11.74999999998884448, -164.4000000000000057 ) ) ;
#160418 = EDGE_CURVE ( 'NONE', #143129, #240241, #82585, .T. ) ;
#160419 = VERTEX_POINT ( 'NONE', #1786 ) ;
#160420 = EDGE_CURVE ( 'NONE', #174146, #170518, #32419, .T. ) ;
#160421 = DIRECTION ( 'NONE',  ( -0.000000000000000000, -6.982962677686266711E-15, 1.000000000000000000 ) ) ;
#160422 = FACE_OUTER_BOUND ( 'NONE', #199262, .T. ) ;
#160424 = DIRECTION ( 'NONE',  ( 0.000000000000000000, 0.000000000000000000, -1.000000000000000000 ) ) ;
#160423 = AXIS2_PLACEMENT_3D ( 'NONE', #34018, #116092, #195641 ) ;
#160425 = EDGE_CURVE ( 'NONE', #6219, #185072, #184285, .T. ) ;
#160426 = CARTESIAN_POINT ( 'NONE',  ( -16.85718274719485876, 9.976142314632889807, -154.9366536678175237 ) ) ;
#160427 = CARTESIAN_POINT ( 'NONE',  ( -18.56579813702276027, 46.46179379974391566, -243.0832762246653544 ) ) ;
#160428 = CARTESIAN_POINT ( 'NONE',  ( 21.07928932188134397, 69.67148334361883144, -136.6220026301787414 ) ) ;
#160429 = ORIENTED_EDGE ( 'NONE', *, *, #182856, .F. ) ;
#160430 = ORIENTED_EDGE ( 'NONE', *, *, #169526, .T. ) ;
#160431 = DIRECTION ( 'NONE',  ( -1.000000000000000000, 0.000000000000000000, -0.000000000000000000 ) ) ;
#160432 = AXIS2_PLACEMENT_3D ( 'NONE', #21651, #122027, #221114 ) ;
#160433 = ADVANCED_FACE ( 'NONE', ( #145148 ), #183026, .T. ) ;
#160434 = EDGE_LOOP ( 'NONE', ( #157464, #183905, #88308, #10418 ) ) ;
#160435 = CIRCLE ( 'NONE', #23056, 0.09999999999999817368 ) ;
#160436 = CYLINDRICAL_SURFACE ( 'NONE', #225830, 0.1000000000000006162 ) ;
#160438 = EDGE_CURVE ( 'NONE', #155345, #172111, #28943, .T. ) ;
#160437 = ORIENTED_EDGE ( 'NONE', *, *, #99597, .T. ) ;
#160439 = CARTESIAN_POINT ( 'NONE',  ( 20.90851465518106167, 10.32532329027886320, -173.0699343018359855 ) ) ;
#160440 = CARTESIAN_POINT ( 'NONE',  ( 20.94999999999999574, 87.75000000001190870, -100.1231074845242262 ) ) ;
#160441 = DIRECTION ( 'NONE',  ( -7.304098846217948299E-16, -1.000000000000000000, 0.000000000000000000 ) ) ;
#160442 = ADVANCED_FACE ( 'NONE', ( #42224 ), #149936, .T. ) ;
#160443 = DIRECTION ( 'NONE',  ( 0.000000000000000000, -1.000000000000000000, 0.000000000000000000 ) ) ;
#160444 = ORIENTED_EDGE ( 'NONE', *, *, #177955, .F. ) ;
#160445 = CARTESIAN_POINT ( 'NONE',  ( -21.05000000000000071, -11.64999999998884306, -97.40000000000004832 ) ) ;
#160446 = CARTESIAN_POINT ( 'NONE',  ( 18.57071067811864040, 10.17928932189250091, -88.35000000000003695 ) ) ;
#160447 = DIRECTION ( 'NONE',  ( 0.000000000000000000, 0.000000000000000000, -1.000000000000000000 ) ) ;
#160449 = VERTEX_POINT ( 'NONE', #104714 ) ;
#160448 = EDGE_CURVE ( 'NONE', #255325, #88867, #161590, .T. ) ;
#160450 = AXIS2_PLACEMENT_3D ( 'NONE', #165029, #224975, #240719 ) ;
#160452 = DIRECTION ( 'NONE',  ( -0.000000000000000000, 0.000000000000000000, 1.000000000000000000 ) ) ;
#160451 = CARTESIAN_POINT ( 'NONE',  ( -21.53551880898957904, 75.90103026544076670, -176.8079052459406739 ) ) ;
#160453 = ORIENTED_EDGE ( 'NONE', *, *, #63454, .T. ) ;
#160456 = ORIENTED_EDGE ( 'NONE', *, *, #107950, .F. ) ;
#160455 = DIRECTION ( 'NONE',  ( 1.000000000000000000, 0.000000000000000000, 0.000000000000000000 ) ) ;
#160454 = DIRECTION ( 'NONE',  ( 0.000000000000000000, 1.000000000000000000, -6.308085367188393199E-16 ) ) ;
#160457 = ORIENTED_EDGE ( 'NONE', *, *, #129078, .T. ) ;
#160458 = CARTESIAN_POINT ( 'NONE',  ( -18.59999999999999787, 11.65000000001115232, -55.25000000000004974 ) ) ;
#160459 = CARTESIAN_POINT ( 'NONE',  ( 27.30103769104855971, 12.20000000000000284, -347.0000000000001137 ) ) ;
#160460 = EDGE_CURVE ( 'NONE', #153611, #70242, #174254, .T. ) ;
#160461 = FACE_OUTER_BOUND ( 'NONE', #83414, .T. ) ;
#160462 = VECTOR ( 'NONE', #44250, 1000.000000000000000 ) ;
#160463 = ORIENTED_EDGE ( 'NONE', *, *, #127451, .T. ) ;
#160464 = CARTESIAN_POINT ( 'NONE',  ( -33.72168855820452649, 42.27269979661959098, -221.1123729563994402 ) ) ;
#160465 = PLANE ( 'NONE',  #207016 ) ;
#160466 = ADVANCED_FACE ( 'NONE', ( #23958 ), #248114, .T. ) ;
#160468 = DIRECTION ( 'NONE',  ( -1.000000000000000000, 0.000000000000000000, -0.000000000000000000 ) ) ;
#160467 = DIRECTION ( 'NONE',  ( 1.000000000000000000, -0.000000000000000000, -0.000000000000000000 ) ) ;
#160469 = ADVANCED_FACE ( 'NONE', ( #185575 ), #157695, .F. ) ;
#160471 = ORIENTED_EDGE ( 'NONE', *, *, #102467, .F. ) ;
#160470 = CYLINDRICAL_SURFACE ( 'NONE', #155715, 0.1000000000000024342 ) ;
#160472 = ORIENTED_EDGE ( 'NONE', *, *, #170322, .T. ) ;
#160473 = AXIS2_PLACEMENT_3D ( 'NONE', #3305, #222343, #82826 ) ;
#160474 = TOROIDAL_SURFACE ( 'NONE', #185390, 4.041421356237307805, 0.1000000000000000056 ) ;
#160475 = DIRECTION ( 'NONE',  ( 1.000000000000000000, 0.000000000000000000, 0.000000000000000000 ) ) ;
#160476 = ORIENTED_EDGE ( 'NONE', *, *, #202594, .T. ) ;
#160477 = FACE_OUTER_BOUND ( 'NONE', #182923, .T. ) ;
#160478 = ORIENTED_EDGE ( 'NONE', *, *, #36252, .T. ) ;
#160479 = CYLINDRICAL_SURFACE ( 'NONE', #218188, 0.09999999999999939493 ) ;
#160481 = EDGE_CURVE ( 'NONE', #43391, #97776, #169918, .T. ) ;
#160480 = CARTESIAN_POINT ( 'NONE',  ( -21.05000000000000071, 64.35000000001264198, -196.7392418215462726 ) ) ;
#160482 = CARTESIAN_POINT ( 'NONE',  ( 21.07094088545303734, 6.320167221927647461, -33.40110629744778237 ) ) ;
#160483 = VERTEX_POINT ( 'NONE', #208993 ) ;
#160484 = CARTESIAN_POINT ( 'NONE',  ( -18.59999999999999787, 77.83585931145570669, -125.0186683157258329 ) ) ;
#160485 = EDGE_CURVE ( 'NONE', #146074, #87859, #249417, .T. ) ;
#160486 = AXIS2_PLACEMENT_3D ( 'NONE', #18407, #156673, #91848 ) ;
#160487 = FACE_OUTER_BOUND ( 'NONE', #36708, .T. ) ;
#160488 = AXIS2_PLACEMENT_3D ( 'NONE', #1305, #45589, #123852 ) ;
#160489 = AXIS2_PLACEMENT_3D ( 'NONE', #133357, #90359, #253282 ) ;
#160490 = AXIS2_PLACEMENT_3D ( 'NONE', #45754, #186571, #26211 ) ;
#160491 = ORIENTED_EDGE ( 'NONE', *, *, #120150, .T. ) ;
#160492 = ORIENTED_EDGE ( 'NONE', *, *, #191753, .F. ) ;
#160493 = VERTEX_POINT ( 'NONE', #150320 ) ;
#160494 = CARTESIAN_POINT ( 'NONE',  ( -22.50000000000000000, 33.38250548509083160, -242.4821227592188961 ) ) ;
#160495 = EDGE_CURVE ( 'NONE', #53791, #95344, #70798, .T. ) ;
#160496 = ORIENTED_EDGE ( 'NONE', *, *, #130520, .T. ) ;
#160498 = ORIENTED_EDGE ( 'NONE', *, *, #66572, .F. ) ;
#160497 = DIRECTION ( 'NONE',  ( 0.000000000000000000, 8.896017825522085641E-15, -1.000000000000000000 ) ) ;
#160499 = ORIENTED_EDGE ( 'NONE', *, *, #154283, .T. ) ;
#160503 = ORIENTED_EDGE ( 'NONE', *, *, #246345, .T. ) ;
#160502 = ORIENTED_EDGE ( 'NONE', *, *, #232448, .F. ) ;
#160501 = DIRECTION ( 'NONE',  ( 1.000000000000000000, 0.000000000000000000, 0.000000000000000000 ) ) ;
#160500 = B_SPLINE_CURVE_WITH_KNOTS ( 'NONE', 3,
 ( #99973, #197815, #221219, #139093, #875, #23066, #80402, #118298, #59557, #239526 ),
 .UNSPECIFIED., .F., .F.,
 ( 4, 3, 3, 4 ),
 ( 1.957469226477651626E-15, 8.145022132840017156E-06, 1.905645951092857371E-05, 2.061107371226198839E-05 ),
 .UNSPECIFIED. ) ;
#160504 = ORIENTED_EDGE ( 'NONE', *, *, #141754, .T. ) ;
#160505 = CARTESIAN_POINT ( 'NONE',  ( 18.49999999999999645, 5.949999999999945111, -10.30570230503485796 ) ) ;
#160506 = ADVANCED_FACE ( 'NONE', ( #86442 ), #206424, .T. ) ;
#160507 = CIRCLE ( 'NONE', #252062, 12.97499999999998721 ) ;
#160508 = CARTESIAN_POINT ( 'NONE',  ( -23.15000000000000213, 1.115600667400684642E-11, -167.5000000000000284 ) ) ;
#160509 = AXIS2_PLACEMENT_3D ( 'NONE', #198018, #18107, #33871 ) ;
#160510 = CARTESIAN_POINT ( 'NONE',  ( -16.88783316861813688, 14.13723969814692083, -219.1551508146100105 ) ) ;
#160511 = AXIS2_PLACEMENT_3D ( 'NONE', #173233, #190194, #12849 ) ;
#160512 = ORIENTED_EDGE ( 'NONE', *, *, #32269, .T. ) ;
#160513 = DIRECTION ( 'NONE',  ( 0.000000000000000000, -1.000000000000000000, 0.000000000000000000 ) ) ;
#160515 = ORIENTED_EDGE ( 'NONE', *, *, #188159, .F. ) ;
#160514 = CARTESIAN_POINT ( 'NONE',  ( 20.90000000000000213, 11.59510167572422112, -1.901609089591594470 ) ) ;
#160516 = CARTESIAN_POINT ( 'NONE',  ( 20.94999999999999929, 7.476371755685457643, -241.7308184205399471 ) ) ;
#160518 = ORIENTED_EDGE ( 'NONE', *, *, #150498, .F. ) ;
#160517 = DIRECTION ( 'NONE',  ( 0.000000000000000000, 0.9915357197604971473, -0.1298341882519111479 ) ) ;
#160519 = VERTEX_POINT ( 'NONE', #6935 ) ;
#160520 = CONICAL_SURFACE ( 'NONE', #139616, 4.299999999999956302, 0.7853981633974466137 ) ;
#160521 = AXIS2_PLACEMENT_3D ( 'NONE', #117736, #18638, #89480 ) ;
#160522 = AXIS2_PLACEMENT_3D ( 'NONE', #3304, #63291, #142808 ) ;
#160523 = DIRECTION ( 'NONE',  ( 0.000000000000000000, 0.000000000000000000, -1.000000000000000000 ) ) ;
#160524 = ORIENTED_EDGE ( 'NONE', *, *, #233549, .F. ) ;
#160525 = ORIENTED_EDGE ( 'NONE', *, *, #184789, .F. ) ;
#160526 = CARTESIAN_POINT ( 'NONE',  ( -22.48660254037843487, 64.35000000001268461, -203.5731074845244279 ) ) ;
#160527 = CARTESIAN_POINT ( 'NONE',  ( -18.50000000000000000, 1.115600667400684642E-11, -200.9999999999999432 ) ) ;
#160530 = ORIENTED_EDGE ( 'NONE', *, *, #5773, .T. ) ;
#160529 = ORIENTED_EDGE ( 'NONE', *, *, #40825, .F. ) ;
#160528 = TOROIDAL_SURFACE ( 'NONE', #118822, 11.65000000000000036, 0.1000000000000000056 ) ;
#160531 = ORIENTED_EDGE ( 'NONE', *, *, #104142, .T. ) ;
#160532 = CARTESIAN_POINT ( 'NONE',  ( -18.59999999999999787, 11.65000000001115232, -174.4148057706539987 ) ) ;
#160533 = ORIENTED_EDGE ( 'NONE', *, *, #38458, .F. ) ;
#160534 = CIRCLE ( 'NONE', #68946, 0.1999999999999987899 ) ;
#160535 = ORIENTED_EDGE ( 'NONE', *, *, #217838, .T. ) ;
#160536 = LINE ( 'NONE', #63977, #138399 ) ;
#160537 = ORIENTED_EDGE ( 'NONE', *, *, #67883, .T. ) ;
#160538 = DIRECTION ( 'NONE',  ( 1.000000000000000000, 0.000000000000000000, 0.000000000000000000 ) ) ;
#160539 = AXIS2_PLACEMENT_3D ( 'NONE', #109654, #66699, #71851 ) ;
#160540 = AXIS2_PLACEMENT_3D ( 'NONE', #155951, #136323, #118080 ) ;
#160541 = DIRECTION ( 'NONE',  ( 0.000000000000000000, 0.000000000000000000, 1.000000000000000000 ) ) ;
#160542 = ORIENTED_EDGE ( 'NONE', *, *, #78547, .F. ) ;
#160543 = EDGE_CURVE ( 'NONE', #20995, #171172, #166042, .T. ) ;
#160545 = ORIENTED_EDGE ( 'NONE', *, *, #246973, .T. ) ;
#160544 = ORIENTED_EDGE ( 'NONE', *, *, #229683, .T. ) ;
#160546 = DIRECTION ( 'NONE',  ( -0.000000000000000000, 0.8700118002898356018, -0.4930308989875170078 ) ) ;
#160547 = DIRECTION ( 'NONE',  ( -1.000000000000000000, 0.000000000000000000, 0.000000000000000000 ) ) ;
#160548 = ORIENTED_EDGE ( 'NONE', *, *, #61257, .T. ) ;
#160549 = VERTEX_POINT ( 'NONE', #228570 ) ;
#160550 = VERTEX_POINT ( 'NONE', #27824 ) ;
#160551 = EDGE_CURVE ( 'NONE', #158841, #141135, #210292, .T. ) ;
#160552 = DIRECTION ( 'NONE',  ( 1.000000000000000000, -3.265361837132813093E-16, -2.280189983783949500E-30 ) ) ;
#160553 = ORIENTED_EDGE ( 'NONE', *, *, #52774, .F. ) ;
#160554 = DIRECTION ( 'NONE',  ( 1.000000000000000000, 0.000000000000000000, 0.000000000000000000 ) ) ;
#160555 = DIRECTION ( 'NONE',  ( -1.073024830501117725E-15, 0.000000000000000000, -1.000000000000000000 ) ) ;
#160556 = ORIENTED_EDGE ( 'NONE', *, *, #151999, .F. ) ;
#160557 = DIRECTION ( 'NONE',  ( 0.000000000000000000, 0.000000000000000000, 1.000000000000000000 ) ) ;
#160558 = CARTESIAN_POINT ( 'NONE',  ( 18.54286124688534798, 85.62391757880992316, -129.7819051526616079 ) ) ;
#160560 = CARTESIAN_POINT ( 'NONE',  ( -21.05000000000000071, 6.257814610487270279, -66.90220970869124528 ) ) ;
#160559 = LINE ( 'NONE', #21051, #69674 ) ;
#160561 = ADVANCED_FACE ( 'NONE', ( #109879 ), #190749, .F. ) ;
#160562 = FACE_OUTER_BOUND ( 'NONE', #111192, .T. ) ;
#160563 = VECTOR ( 'NONE', #210138, 1000.000000000000000 ) ;
#160564 = LINE ( 'NONE', #237516, #20510 ) ;
#160565 = CARTESIAN_POINT ( 'NONE',  ( 21.05563370358598263, 65.27576964416579131, -157.8400166685613328 ) ) ;
#160566 = CARTESIAN_POINT ( 'NONE',  ( -23.39999999999994529, 74.83745509109094485, -44.02310748452479316 ) ) ;
#160567 = VECTOR ( 'NONE', #11310, 1000.000000000000000 ) ;
#160568 = CARTESIAN_POINT ( 'NONE',  ( 18.59999999999999076, 53.37395138337728895, -234.8857996415767104 ) ) ;
#160569 = CARTESIAN_POINT ( 'NONE',  ( 18.59999999999999432, 1.162701749949165642, -142.1000000000000227 ) ) ;
#160570 = AXIS2_PLACEMENT_3D ( 'NONE', #55515, #37298, #38565 ) ;
#160571 = ADVANCED_FACE ( 'NONE', ( #246826 ), #103455, .T. ) ;
#160572 = VERTEX_POINT ( 'NONE', #151622 ) ;
#160573 = CIRCLE ( 'NONE', #189759, 0.1999999999999987899 ) ;
#160574 = EDGE_CURVE ( 'NONE', #109956, #53442, #12105, .T. ) ;
#160576 = ORIENTED_EDGE ( 'NONE', *, *, #103498, .T. ) ;
#160575 = ORIENTED_EDGE ( 'NONE', *, *, #160644, .F. ) ;
#160577 = AXIS2_PLACEMENT_3D ( 'NONE', #96421, #50867, #172180 ) ;
#160578 = VERTEX_POINT ( 'NONE', #66910 ) ;
#160579 = VERTEX_POINT ( 'NONE', #91616 ) ;
#160580 = EDGE_CURVE ( 'NONE', #108404, #5236, #70197, .T. ) ;
#160581 = CARTESIAN_POINT ( 'NONE',  ( 23.15000000000000213, 75.39949836213487799, -250.2448839681187849 ) ) ;
#160582 =( BOUNDED_SURFACE ( )  B_SPLINE_SURFACE ( 3, 2, ( 
 ( #118717, #95280, #113561 ),
 ( #97815, #253062, #193110 ),
 ( #177420, #58697, #19610 ),
 ( #21, #152725, #14489 ),
 ( #5131, #122564, #40485 ),
 ( #63858, #65130, #43020 ) ),
 .UNSPECIFIED., .F., .F., .F. ) 
 B_SPLINE_SURFACE_WITH_KNOTS ( ( 4, 2, 4 ),
 ( 3, 3 ),
 ( 0.0001381104793128061785, 0.0002947094729387751515, 0.0004513084665647441244 ),
 ( 0.000000000000000000, 1.000000000000000000 ),
 .UNSPECIFIED. ) 
 GEOMETRIC_REPRESENTATION_ITEM ( )  RATIONAL_B_SPLINE_SURFACE ( (
 ( 1.000000000000000000, 0.7071067811865966446, 1.000000000000000000),
 ( 1.000000000000000000, 0.6919563088098851233, 1.000000000000000000),
 ( 1.000000000000000000, 0.6959445945717438464, 1.000000000000000000),
 ( 1.000000000000000000, 0.7137882985313120932, 1.000000000000000000),
 ( 1.000000000000000000, 0.7257496306096493655, 1.000000000000000000),
 ( 1.000000000000000000, 0.7250110520819876836, 1.000000000000000000) ) ) 
 REPRESENTATION_ITEM ( '' )  SURFACE ( )  );
#160583 = DIRECTION ( 'NONE',  ( 0.000000000000000000, -0.9893560106964500722, 0.1455152366551550613 ) ) ;
#160584 = EDGE_CURVE ( 'NONE', #233370, #254577, #91012, .T. ) ;
#160585 = CIRCLE ( 'NONE', #198534, 0.1999999999999987899 ) ;
#160587 = DIRECTION ( 'NONE',  ( 1.000000000000000000, 0.000000000000000000, 0.000000000000000000 ) ) ;
#160586 = CARTESIAN_POINT ( 'NONE',  ( 23.14999999999999858, 67.23127455305835554, -235.8551265064784559 ) ) ;
#160588 = DIRECTION ( 'NONE',  ( -1.000000000000000000, 0.000000000000000000, 0.000000000000000000 ) ) ;
#160590 = ORIENTED_EDGE ( 'NONE', *, *, #27317, .T. ) ;
#160589 = AXIS2_PLACEMENT_3D ( 'NONE', #16601, #256401, #56952 ) ;
#160591 = DIRECTION ( 'NONE',  ( -1.000000000000000000, -0.000000000000000000, 0.000000000000000000 ) ) ;
#160592 = DIRECTION ( 'NONE',  ( 0.000000000000000000, -0.9908441862701610203, 0.1350103645451807555 ) ) ;
#160593 = EDGE_CURVE ( 'NONE', #66484, #210865, #215875, .T. ) ;
#160594 = CIRCLE ( 'NONE', #18897, 0.09999999999999939493 ) ;
#160595 = CARTESIAN_POINT ( 'NONE',  ( -23.25000000000000000, 7.021664781911246322, -171.3335654018973173 ) ) ;
#160596 = CARTESIAN_POINT ( 'NONE',  ( 22.88900146558018989, 12.94144749016466456, -219.5202428567343702 ) ) ;
#160597 = VERTEX_POINT ( 'NONE', #205117 ) ;
#160598 = CARTESIAN_POINT ( 'NONE',  ( 20.85000000000000142, 77.14957036958807635, -162.2071950000224092 ) ) ;
#160599 = CARTESIAN_POINT ( 'NONE',  ( -21.04999999999989768, 0.01485563490472031727, -94.15564095795694755 ) ) ;
#160600 = EDGE_LOOP ( 'NONE', ( #87363, #114022, #196683 ) ) ;
#160601 = CARTESIAN_POINT ( 'NONE',  ( 18.39999999999999503, 5.650000000011139001, -87.85000000000003695 ) ) ;
#160602 = AXIS2_PLACEMENT_3D ( 'NONE', #84745, #136068, #233911 ) ;
#160603 = DIRECTION ( 'NONE',  ( 1.000000000000000000, 0.000000000000000000, 0.000000000000000000 ) ) ;
#160604 = DIRECTION ( 'NONE',  ( 0.000000000000000000, -0.2128009952263485993, 0.9770955615653341697 ) ) ;
#160605 = DIRECTION ( 'NONE',  ( 1.000000000000000000, 0.000000000000000000, -0.000000000000000000 ) ) ;
#160606 = FACE_OUTER_BOUND ( 'NONE', #211495, .T. ) ;
#160607 = ORIENTED_EDGE ( 'NONE', *, *, #64741, .T. ) ;
#160608 = DIRECTION ( 'NONE',  ( 9.044546369203339308E-15, -0.7397360091702694929, -0.6728971962616898672 ) ) ;
#160609 = CARTESIAN_POINT ( 'NONE',  ( -20.94999999999999929, 61.95000000001146390, -41.53680255528533394 ) ) ;
#160611 = EDGE_CURVE ( 'NONE', #55329, #103697, #244948, .T. ) ;
#160610 = CARTESIAN_POINT ( 'NONE',  ( 23.14999999999998437, 76.00000000001234923, -165.9731074845243768 ) ) ;
#160613 = DIRECTION ( 'NONE',  ( 0.7071359030027362103, -0.3338770338704923346, -0.6232856014206863415 ) ) ;
#160612 = DIRECTION ( 'NONE',  ( 1.000000000000000000, 0.000000000000000000, 0.000000000000000000 ) ) ;
#160614 = CARTESIAN_POINT ( 'NONE',  ( 21.08489834409762409, 10.62232389474667293, -45.85000000000001563 ) ) ;
#160615 = DIRECTION ( 'NONE',  ( 0.000000000000000000, 0.000000000000000000, -1.000000000000000000 ) ) ;
#160616 = DIRECTION ( 'NONE',  ( 0.000000000000000000, 0.4721928772777652106, 0.8814952561688266242 ) ) ;
#160617 = CARTESIAN_POINT ( 'NONE',  ( 23.15000000000000213, -9.499999999988848032, -76.89396912265249284 ) ) ;
#160618 = AXIS2_PLACEMENT_3D ( 'NONE', #130782, #193346, #113787 ) ;
#160621 = ORIENTED_EDGE ( 'NONE', *, *, #256288, .F. ) ;
#160620 = CIRCLE ( 'NONE', #139719, 0.09999999999999134581 ) ;
#160619 = CARTESIAN_POINT ( 'NONE',  ( -16.87036670365549540, 9.989418819312804843, -146.5204398826979855 ) ) ;
#160622 = AXIS2_PLACEMENT_3D ( 'NONE', #165856, #206252, #8060 ) ;
#160623 = ORIENTED_EDGE ( 'NONE', *, *, #156955, .T. ) ;
#160624 = EDGE_CURVE ( 'NONE', #245180, #199913, #134571, .T. ) ;
#160625 = ORIENTED_EDGE ( 'NONE', *, *, #50614, .T. ) ;
#160626 = CARTESIAN_POINT ( 'NONE',  ( -21.64999999999999858, 7.350000000011155166, -146.3500000000000227 ) ) ;
#160627 = CYLINDRICAL_SURFACE ( 'NONE', #229208, 0.09999999999999939493 ) ;
#160628 = CARTESIAN_POINT ( 'NONE',  ( 22.47071067811865319, 65.11488425470513164, -243.2801022963548405 ) ) ;
#160629 = EDGE_CURVE ( 'NONE', #153879, #102509, #153406, .T. ) ;
#160630 = LINE ( 'NONE', #235010, #8707 ) ;
#160631 = AXIS2_PLACEMENT_3D ( 'NONE', #142572, #26513, #183018 ) ;
#160632 = ORIENTED_EDGE ( 'NONE', *, *, #219311, .F. ) ;
#160633 = ADVANCED_FACE ( 'NONE', ( #34245 ), #38084, .T. ) ;
#160634 = CARTESIAN_POINT ( 'NONE',  ( -21.05000000000000071, -1.835341550213255957, -112.0551512925630107 ) ) ;
#160635 = CARTESIAN_POINT ( 'NONE',  ( -20.94999999999999929, 70.10000000001251408, -180.2422072491807796 ) ) ;
#160636 = CARTESIAN_POINT ( 'NONE',  ( -18.40000000000000213, 70.35000000001261355, -190.8731074845244109 ) ) ;
#160637 = AXIS2_PLACEMENT_3D ( 'NONE', #204270, #124758, #227689 ) ;
#160638 = DIRECTION ( 'NONE',  ( 0.000000000000000000, 0.8814952561688437216, -0.4721928772777334582 ) ) ;
#160640 = ORIENTED_EDGE ( 'NONE', *, *, #129180, .F. ) ;
#160639 = DIRECTION ( 'NONE',  ( 0.000000000000000000, -0.5868805631290353597, -0.8096735173027127530 ) ) ;
#160642 = FACE_OUTER_BOUND ( 'NONE', #251955, .T. ) ;
#160641 = FACE_OUTER_BOUND ( 'NONE', #93387, .T. ) ;
#160643 = CARTESIAN_POINT ( 'NONE',  ( -18.50000000000000000, 66.75000000001158185, -57.17310748452438673 ) ) ;
#160644 = EDGE_CURVE ( 'NONE', #209999, #244761, #236731, .T. ) ;
#160645 = SURFACE_STYLE_USAGE ( .BOTH. , #81053 ) ;
#160646 = VERTEX_POINT ( 'NONE', #156758 ) ;
#160647 = EDGE_CURVE ( 'NONE', #32098, #67123, #192023, .T. ) ;
#160648 = DIRECTION ( 'NONE',  ( 0.000000000000000000, 0.000000000000000000, 1.000000000000000000 ) ) ;
#160649 = CARTESIAN_POINT ( 'NONE',  ( -18.59999999999999787, -1.835859311432481045, -212.5044391687984842 ) ) ;
#160650 = ADVANCED_FACE ( 'NONE', ( #234991 ), #194601, .T. ) ;
#160651 = LINE ( 'NONE', #124076, #43981 ) ;
#160652 = ORIENTED_EDGE ( 'NONE', *, *, #9258, .T. ) ;
#160653 = DIRECTION ( 'NONE',  ( 0.000000000000000000, 8.783410004945868831E-15, -1.000000000000000000 ) ) ;
#160654 = DIRECTION ( 'NONE',  ( 0.000000000000000000, -6.938893903907222067E-15, 1.000000000000000000 ) ) ;
#160655 = VERTEX_POINT ( 'NONE', #195876 ) ;
#160656 = CIRCLE ( 'NONE', #48191, 0.09999999999999939493 ) ;
#160658 = LINE ( 'NONE', #182771, #151123 ) ;
#160657 = AXIS2_PLACEMENT_3D ( 'NONE', #227975, #49331, #44214 ) ;
#160659 = EDGE_CURVE ( 'NONE', #118730, #102393, #98007, .T. ) ;
#160660 = DIRECTION ( 'NONE',  ( 0.000000000000000000, 0.2128009952263603677, -0.9770955615653313941 ) ) ;
#160661 = CARTESIAN_POINT ( 'NONE',  ( -22.43310005002225438, 0.005636942152031573783, -122.3503378728656230 ) ) ;
#160662 = ORIENTED_EDGE ( 'NONE', *, *, #50828, .T. ) ;
#160663 = ORIENTED_EDGE ( 'NONE', *, *, #182778, .F. ) ;
#160664 = DIRECTION ( 'NONE',  ( 1.000000000000000000, 0.000000000000000000, 0.000000000000000000 ) ) ;
#160665 = CARTESIAN_POINT ( 'NONE',  ( -20.85000000000000142, -11.64999999998884306, -134.0000000000000284 ) ) ;
#160666 = CARTESIAN_POINT ( 'NONE',  ( 20.95429693346634181, 10.54330487990709209, -141.5608825383131659 ) ) ;
#160667 = DIRECTION ( 'NONE',  ( 0.000000000000000000, 0.000000000000000000, -1.000000000000000000 ) ) ;
#160670 = DIRECTION ( 'NONE',  ( 0.000000000000000000, -1.000000000000000000, 0.000000000000000000 ) ) ;
#160669 = AXIS2_PLACEMENT_3D ( 'NONE', #13803, #248554, #93330 ) ;
#160668 = CARTESIAN_POINT ( 'NONE',  ( -21.07016717457011268, 76.00000000001219291, -142.8440483226251843 ) ) ;
#160671 = LINE ( 'NONE', #36881, #90069 ) ;
#160672 = AXIS2_PLACEMENT_3D ( 'NONE', #246047, #106501, #66119 ) ;
#160673 = FACE_OUTER_BOUND ( 'NONE', #210567, .T. ) ;
#160674 = CARTESIAN_POINT ( 'NONE',  ( 18.39999999999999858, -9.499999999988842703, -107.1001893912220879 ) ) ;
#160676 = EDGE_LOOP ( 'NONE', ( #252020, #81048, #169644, #49223 ) ) ;
#160675 = VECTOR ( 'NONE', #229269, 999.9999999999998863 ) ;
#160677 = CARTESIAN_POINT ( 'NONE',  ( 19.75857864376268935, 34.58225676390223668, -235.1091250528070589 ) ) ;
#160678 = AXIS2_PLACEMENT_3D ( 'NONE', #36711, #56219, #96618 ) ;
#160680 = ORIENTED_EDGE ( 'NONE', *, *, #61126, .F. ) ;
#160679 = CYLINDRICAL_SURFACE ( 'NONE', #252993, 0.1000000000000028644 ) ;
#160681 = CARTESIAN_POINT ( 'NONE',  ( -21.05439746398122836, 64.25000000001209344, -129.5331909970393838 ) ) ;
#160682 = CYLINDRICAL_SURFACE ( 'NONE', #165922, 0.09999999999998898659 ) ;
#160684 = DIRECTION ( 'NONE',  ( 0.000000000000000000, 0.000000000000000000, -1.000000000000000000 ) ) ;
#160683 = CARTESIAN_POINT ( 'NONE',  ( 20.94999999999999929, 69.35000000001187459, -93.00608031408432907 ) ) ;
#160685 =( BOUNDED_SURFACE ( )  B_SPLINE_SURFACE ( 3, 2, ( 
 ( #210659, #91988, #90701 ),
 ( #170298, #249788, #32052 ),
 ( #191125, #13746, #28208 ),
 ( #251055, #72452, #67294 ),
 ( #231521, #107703, #187265 ),
 ( #39757, #35897, #218337 ) ),
 .UNSPECIFIED., .F., .F., .T. ) 
 B_SPLINE_SURFACE_WITH_KNOTS ( ( 4, 2, 4 ),
 ( 3, 3 ),
 ( 0.0001381104793128061785, 0.0002947094729387687547, 0.0004513084665647313309 ),
 ( 0.000000000000000000, 1.000000000000000000 ),
 .UNSPECIFIED. ) 
 GEOMETRIC_REPRESENTATION_ITEM ( )  RATIONAL_B_SPLINE_SURFACE ( (
 ( 1.000000000000000000, 0.7071067811865494601, 1.000000000000000000),
 ( 1.000000000000000000, 0.6919563088099097703, 1.000000000000000000),
 ( 1.000000000000000000, 0.6959445945717440685, 1.000000000000000000),
 ( 1.000000000000000000, 0.7137882985313291906, 1.000000000000000000),
 ( 1.000000000000000000, 0.7257496306096434813, 1.000000000000000000),
 ( 1.000000000000000000, 0.7250110520819876836, 1.000000000000000000) ) ) 
 REPRESENTATION_ITEM ( '' )  SURFACE ( )  );
#160686 = STYLED_ITEM ( 'NONE', ( #211907 ), #26318 ) ;
#160687 = EDGE_CURVE ( 'NONE', #23430, #211300, #61784, .T. ) ;
#160688 = ORIENTED_EDGE ( 'NONE', *, *, #40307, .F. ) ;
#160690 = CARTESIAN_POINT ( 'NONE',  ( -18.40000000000000213, 67.17743825834591576, -160.7731074845244166 ) ) ;
#160689 = CARTESIAN_POINT ( 'NONE',  ( -16.88783316861822215, 66.05000000001157900, -56.77084344254470949 ) ) ;
#160692 = EDGE_CURVE ( 'NONE', #69026, #118647, #253245, .T. ) ;
#160691 = DIRECTION ( 'NONE',  ( 0.000000000000000000, 1.000000000000000000, 6.688090509790097607E-15 ) ) ;
#160693 = CARTESIAN_POINT ( 'NONE',  ( -18.50000000000000000, 7.120270961708746960, -137.6595630418393625 ) ) ;
#160694 = LINE ( 'NONE', #240209, #53399 ) ;
#160695 = CARTESIAN_POINT ( 'NONE',  ( -15.75000000000000355, 66.65000000001258229, -186.7731074845243882 ) ) ;
#160696 = ORIENTED_EDGE ( 'NONE', *, *, #56143, .F. ) ;
#160697 = DIRECTION ( 'NONE',  ( -0.000000000000000000, -6.982962677686266711E-15, 1.000000000000000000 ) ) ;
#160698 = ORIENTED_EDGE ( 'NONE', *, *, #79249, .F. ) ;
#160699 = EDGE_CURVE ( 'NONE', #231649, #108629, #120081, .T. ) ;
#160700 = CARTESIAN_POINT ( 'NONE',  ( -16.79363873026997922, 9.948850229429586634, -54.34615378144547293 ) ) ;
#160701 = ORIENTED_EDGE ( 'NONE', *, *, #100838, .F. ) ;
#160702 = DIRECTION ( 'NONE',  ( -1.000000000000000000, 1.335000415235278971E-16, -2.979993593738921214E-16 ) ) ;
#160703 = CIRCLE ( 'NONE', #131436, 0.1999999999999987899 ) ;
#160704 = ORIENTED_EDGE ( 'NONE', *, *, #198695, .T. ) ;
#160705 = CIRCLE ( 'NONE', #156425, 4.049999999999998046 ) ;
#160706 = DIRECTION ( 'NONE',  ( 0.000000000000000000, 0.000000000000000000, -1.000000000000000000 ) ) ;
#160707 = AXIS2_PLACEMENT_3D ( 'NONE', #252767, #37602, #257860 ) ;
#160708 = FACE_OUTER_BOUND ( 'NONE', #140253, .T. ) ;
#160710 = ORIENTED_EDGE ( 'NONE', *, *, #110851, .F. ) ;
#160709 = VECTOR ( 'NONE', #182848, 1000.000000000000000 ) ;
#160711 = AXIS2_PLACEMENT_3D ( 'NONE', #110684, #250196, #88530 ) ;
#160713 = CIRCLE ( 'NONE', #223021, 12.97499999999999964 ) ;
#160712 = CARTESIAN_POINT ( 'NONE',  ( -16.85939681242905763, 9.905225185936458843, -87.53992195519153086 ) ) ;
#160715 = LINE ( 'NONE', #254617, #237794 ) ;
#160714 = VECTOR ( 'NONE', #68137, 1000.000000000000000 ) ;
#160716 = CARTESIAN_POINT ( 'NONE',  ( 20.96077737575349786, 11.62390063401585394, -160.6407919571063303 ) ) ;
#160717 = DIRECTION ( 'NONE',  ( 0.000000000000000000, 0.000000000000000000, -1.000000000000000000 ) ) ;
#160718 = CARTESIAN_POINT ( 'NONE',  ( -13.39999999999994351, 66.35000000001119247, -18.42310748452479174 ) ) ;
#160719 = CARTESIAN_POINT ( 'NONE',  ( 19.75857864376269646, 62.36932623377868623, -208.8924400946860089 ) ) ;
#160720 = EDGE_CURVE ( 'NONE', #172722, #190117, #20102, .T. ) ;
#160721 = EDGE_LOOP ( 'NONE', ( #175068, #27391, #108136, #115750 ) ) ;
#160722 = FACE_OUTER_BOUND ( 'NONE', #79706, .T. ) ;
#160723 = VERTEX_POINT ( 'NONE', #236261 ) ;
#160725 = VERTEX_POINT ( 'NONE', #57609 ) ;
#160724 = CARTESIAN_POINT ( 'NONE',  ( -18.50000000000000000, 47.92640890138473253, -246.4059919526569900 ) ) ;
#160726 = AXIS2_PLACEMENT_3D ( 'NONE', #232998, #13936, #128749 ) ;
#160727 = ORIENTED_EDGE ( 'NONE', *, *, #193251, .T. ) ;
#160728 = LINE ( 'NONE', #141139, #244665 ) ;
#160729 = CARTESIAN_POINT ( 'NONE',  ( -18.59999999999999787, 9.350000000011156942, -179.8499999999999943 ) ) ;
#160730 = AXIS2_PLACEMENT_3D ( 'NONE', #204889, #86211, #67959 ) ;
#160731 = DIRECTION ( 'NONE',  ( 0.000000000000000000, 0.000000000000000000, 1.000000000000000000 ) ) ;
#160732 = CARTESIAN_POINT ( 'NONE',  ( -21.07928932188134041, 61.09751618602744827, -234.2940654522722639 ) ) ;
#160733 = VERTEX_POINT ( 'NONE', #197126 ) ;
#160734 = EDGE_CURVE ( 'NONE', #74091, #63287, #74667, .T. ) ;
#160735 = AXIS2_PLACEMENT_3D ( 'NONE', #41703, #62537, #39143 ) ;
#160736 = AXIS2_PLACEMENT_3D ( 'NONE', #187899, #168373, #229589 ) ;
#160737 = ADVANCED_FACE ( 'NONE', ( #73370 ), #133318, .T. ) ;
#160738 = VERTEX_POINT ( 'NONE', #172492 ) ;
#160739 = DIRECTION ( 'NONE',  ( 1.000000000000000000, 0.000000000000000000, 0.000000000000000000 ) ) ;
#160740 = EDGE_CURVE ( 'NONE', #56104, #184009, #62583, .T. ) ;
#160741 = CYLINDRICAL_SURFACE ( 'NONE', #189008, 0.09999999999999939493 ) ;
#160742 = ORIENTED_EDGE ( 'NONE', *, *, #71658, .F. ) ;
#160743 = CARTESIAN_POINT ( 'NONE',  ( -16.87998658237741978, 9.950000000011138823, -146.8636395677385167 ) ) ;
#160744 = EDGE_CURVE ( 'NONE', #185693, #71575, #240127, .T. ) ;
#160745 = CARTESIAN_POINT ( 'NONE',  ( 18.59999999999999076, 62.94087027993914063, -212.6738838931263444 ) ) ;
#160748 = EDGE_CURVE ( 'NONE', #144360, #180506, #74295, .T. ) ;
#160747 = ADVANCED_FACE ( 'NONE', ( #183992 ), #82295, .T. ) ;
#160746 = ORIENTED_EDGE ( 'NONE', *, *, #23705, .T. ) ;
#160749 = CARTESIAN_POINT ( 'NONE',  ( -21.45000000000000284, 21.56708615768143034, -232.7219885528102736 ) ) ;
#160750 = DIRECTION ( 'NONE',  ( 0.000000000000000000, 1.000000000000000000, 1.224646799147353207E-16 ) ) ;
#160751 = DIRECTION ( 'NONE',  ( 0.000000000000000000, -7.189901751995743170E-15, 1.000000000000000000 ) ) ;
#160752 = CARTESIAN_POINT ( 'NONE',  ( -23.15000000000000213, 1.115600667400684642E-11, -87.62500000000005684 ) ) ;
#160753 = AXIS2_PLACEMENT_3D ( 'NONE', #44335, #142135, #123875 ) ;
#160754 = AXIS2_PLACEMENT_3D ( 'NONE', #147638, #169813, #227169 ) ;
#160755 = VECTOR ( 'NONE', #239766, 1000.000000000000227 ) ;
#160756 = CIRCLE ( 'NONE', #119217, 0.5000000000000004441 ) ;
#160757 = DIRECTION ( 'NONE',  ( -1.000000000000000000, -3.190570557967288949E-16, -6.948722487160392945E-17 ) ) ;
#160758 = EDGE_CURVE ( 'NONE', #111888, #109469, #120209, .T. ) ;
#160759 = EDGE_CURVE ( 'NONE', #236966, #174683, #139712, .T. ) ;
#160760 = ORIENTED_EDGE ( 'NONE', *, *, #68350, .F. ) ;
#160761 = AXIS2_PLACEMENT_3D ( 'NONE', #124876, #221381, #143128 ) ;
#160762 = ORIENTED_EDGE ( 'NONE', *, *, #244680, .F. ) ;
#160763 = CARTESIAN_POINT ( 'NONE',  ( -20.85000000000000142, 76.00000000001136868, -28.12310748452432208 ) ) ;
#160764 = EDGE_CURVE ( 'NONE', #250378, #81173, #257349, .T. ) ;
#160765 = CARTESIAN_POINT ( 'NONE',  ( 20.94999999999999574, -10.58757034444203704, -206.3761839813444396 ) ) ;
#160767 = EDGE_LOOP ( 'NONE', ( #137584, #240981, #69980 ) ) ;
#160766 = DIRECTION ( 'NONE',  ( 1.000000000000000000, -0.000000000000000000, 0.000000000000000000 ) ) ;
#160768 = CARTESIAN_POINT ( 'NONE',  ( -18.50000000000000000, 85.40000000001209912, -129.6410656363516125 ) ) ;
#160769 = FACE_OUTER_BOUND ( 'NONE', #100028, .T. ) ;
#160771 = FACE_OUTER_BOUND ( 'NONE', #83789, .T. ) ;
#160770 = AXIS2_PLACEMENT_3D ( 'NONE', #9462, #88983, #248075 ) ;
#160772 = DIRECTION ( 'NONE',  ( -0.000000000000000000, 1.000000000000000000, 0.000000000000000000 ) ) ;
#160773 = CYLINDRICAL_SURFACE ( 'NONE', #163972, 0.1000000000000028644 ) ;
#160775 = ADVANCED_FACE ( 'NONE', ( #121485 ), #199730, .T. ) ;
#160774 = CARTESIAN_POINT ( 'NONE',  ( -18.45037301276613917, 85.49020044755425829, -129.5104333481091601 ) ) ;
#160776 = VERTEX_POINT ( 'NONE', #83575 ) ;
#160777 = CIRCLE ( 'NONE', #194078, 0.09999999999999543976 ) ;
#160778 = EDGE_CURVE ( 'NONE', #220140, #256420, #41940, .T. ) ;
#160779 = FACE_OUTER_BOUND ( 'NONE', #153441, .T. ) ;
#160780 = ORIENTED_EDGE ( 'NONE', *, *, #35886, .T. ) ;
#160781 = VERTEX_POINT ( 'NONE', #181446 ) ;
#160782 = AXIS2_PLACEMENT_3D ( 'NONE', #104012, #68771, #225244 ) ;
#160784 = ADVANCED_FACE ( 'NONE', ( #24947 ), #211640, .F. ) ;
#160783 = CARTESIAN_POINT ( 'NONE',  ( -20.64999999999999858, 65.86663596189677605, -213.5709895136416776 ) ) ;
#160785 = CARTESIAN_POINT ( 'NONE',  ( -23.15000000000000213, 85.00000000001179501, -79.41707660717668205 ) ) ;
#160786 = EDGE_LOOP ( 'NONE', ( #224962, #241582, #230959, #78282 ) ) ;
#160787 = LINE ( 'NONE', #62937, #216695 ) ;
#160788 = CARTESIAN_POINT ( 'NONE',  ( -18.43599941264908182, 85.51932742860678616, -62.55013069500345324 ) ) ;
#160789 = EDGE_CURVE ( 'NONE', #212207, #243532, #53197, .T. ) ;
#160790 = VERTEX_POINT ( 'NONE', #200996 ) ;
#160791 = AXIS2_PLACEMENT_3D ( 'NONE', #35216, #209976, #173467 ) ;
#160792 = AXIS2_PLACEMENT_3D ( 'NONE', #256385, #59496, #139026 ) ;
#160793 = FACE_OUTER_BOUND ( 'NONE', #39482, .T. ) ;
#160794 = TOROIDAL_SURFACE ( 'NONE', #235765, 3.899999999999999467, 0.1000000000000000056 ) ;
#160795 = CIRCLE ( 'NONE', #144002, 2.000000000000002665 ) ;
#160796 = LINE ( 'NONE', #223288, #72185 ) ;
#160797 = ORIENTED_EDGE ( 'NONE', *, *, #97142, .T. ) ;
#160798 = ORIENTED_EDGE ( 'NONE', *, *, #182513, .F. ) ;
#160799 = LINE ( 'NONE', #61666, #40452 ) ;
#160800 = ORIENTED_EDGE ( 'NONE', *, *, #6977, .T. ) ;
#160801 = ADVANCED_FACE ( 'NONE', ( #237554 ), #99295, .F. ) ;
#160802 = ORIENTED_EDGE ( 'NONE', *, *, #232926, .T. ) ;
#160804 = ORIENTED_EDGE ( 'NONE', *, *, #98846, .F. ) ;
#160803 = DIRECTION ( 'NONE',  ( 0.000000000000000000, -0.9651348961777157509, 0.2617529984165031243 ) ) ;
#160805 = DIRECTION ( 'NONE',  ( -1.000000000000000000, -0.000000000000000000, -0.000000000000000000 ) ) ;
#160806 = VERTEX_POINT ( 'NONE', #198419 ) ;
#160807 = CARTESIAN_POINT ( 'NONE',  ( 22.45380639572243453, 1.426819239903859335E-07, -88.74956710889316014 ) ) ;
#160808 = ORIENTED_EDGE ( 'NONE', *, *, #135064, .F. ) ;
#160810 = ORIENTED_EDGE ( 'NONE', *, *, #6174, .T. ) ;
#160809 = EDGE_LOOP ( 'NONE', ( #42613, #44881, #46692, #191639 ) ) ;
#160811 = CARTESIAN_POINT ( 'NONE',  ( -21.14999999999999858, 11.75000000001115552, -33.60000000000000142 ) ) ;
#160812 = TOROIDAL_SURFACE ( 'NONE', #190002, 11.70000000000000462, 0.1000000000000000056 ) ;
#160813 = CARTESIAN_POINT ( 'NONE',  ( -20.54999999999999716, 82.57900542960499024, -215.5587758314583482 ) ) ;
#160814 = VECTOR ( 'NONE', #9200, 1000.000000000000114 ) ;
#160815 = ORIENTED_EDGE ( 'NONE', *, *, #29457, .F. ) ;
#160816 = TOROIDAL_SURFACE ( 'NONE', #148317, 1.900000000000002576, 0.1000000000000000056 ) ;
#160817 = ORIENTED_EDGE ( 'NONE', *, *, #213695, .F. ) ;
#160818 = DIRECTION ( 'NONE',  ( 0.000000000000000000, 0.9126074666063759278, 0.4088369013363304383 ) ) ;
#160819 = CARTESIAN_POINT ( 'NONE',  ( 21.05000000000000071, 77.25000000001263345, -195.6231074845243540 ) ) ;
#160821 = VERTEX_POINT ( 'NONE', #22376 ) ;
#160820 = DIRECTION ( 'NONE',  ( 1.476360405086644309E-16, -1.000000000000000000, -1.445602896647339410E-16 ) ) ;
#160822 = CARTESIAN_POINT ( 'NONE',  ( 20.09999999999999787, 41.11438369982452912, -236.8714985644722617 ) ) ;
#160823 = VERTEX_POINT ( 'NONE', #241413 ) ;
#160824 = FACE_OUTER_BOUND ( 'NONE', #125262, .T. ) ;
#160825 = ORIENTED_EDGE ( 'NONE', *, *, #190126, .T. ) ;
#160826 = FACE_OUTER_BOUND ( 'NONE', #250449, .T. ) ;
#160827 = DIRECTION ( 'NONE',  ( -0.7071067811865474617, 0.7071067811865474617, 0.000000000000000000 ) ) ;
#160828 = DIRECTION ( 'NONE',  ( 1.000000000000000000, 0.000000000000000000, 0.000000000000000000 ) ) ;
#160829 = ORIENTED_EDGE ( 'NONE', *, *, #198667, .F. ) ;
#160830 = FACE_OUTER_BOUND ( 'NONE', #62966, .T. ) ;
#160831 = ORIENTED_EDGE ( 'NONE', *, *, #158048, .T. ) ;
#160832 = ORIENTED_EDGE ( 'NONE', *, *, #96387, .T. ) ;
#160833 = VECTOR ( 'NONE', #123967, 1000.000000000000000 ) ;
#160834 = ORIENTED_EDGE ( 'NONE', *, *, #110004, .F. ) ;
#160835 = ORIENTED_EDGE ( 'NONE', *, *, #133531, .F. ) ;
#160836 = LINE ( 'NONE', #102089, #186536 ) ;
#160837 = ORIENTED_EDGE ( 'NONE', *, *, #208335, .F. ) ;
#160838 = ORIENTED_EDGE ( 'NONE', *, *, #139476, .T. ) ;
#160839 = FACE_OUTER_BOUND ( 'NONE', #157444, .T. ) ;
#160840 = CARTESIAN_POINT ( 'NONE',  ( 20.94999999999999929, 0.000000000000000000, -33.50000000000000000 ) ) ;
#160841 = ORIENTED_EDGE ( 'NONE', *, *, #189132, .T. ) ;
#160842 = ADVANCED_FACE ( 'NONE', ( #62767 ), #221808, .T. ) ;
#160843 = VERTEX_POINT ( 'NONE', #182730 ) ;
#160844 = AXIS2_PLACEMENT_3D ( 'NONE', #15722, #208769, #193054 ) ;
#160845 = ORIENTED_EDGE ( 'NONE', *, *, #151334, .T. ) ;
#160846 = CIRCLE ( 'NONE', #202517, 4.000000000000003553 ) ;
#160847 = CIRCLE ( 'NONE', #152478, 4.049999999999998046 ) ;
#160848 = CARTESIAN_POINT ( 'NONE',  ( 21.04999999999999716, 69.50331341424610798, -203.5084513660146968 ) ) ;
#160849 = DIRECTION ( 'NONE',  ( 6.938893903906363786E-14, -0.2617529984165152257, -0.9651348961777124202 ) ) ;
#160850 = CARTESIAN_POINT ( 'NONE',  ( 21.05000000000000071, 19.92792862942048870, -235.1286901285539841 ) ) ;
#160851 = LINE ( 'NONE', #25195, #226679 ) ;
#160852 = DIRECTION ( 'NONE',  ( 0.000000000000000000, -0.8660254037844384856, 0.5000000000000003331 ) ) ;
#160853 = CARTESIAN_POINT ( 'NONE',  ( 21.05000000000000426, 0.06570161033324331545, -127.7416839426680184 ) ) ;
#160854 = EDGE_CURVE ( 'NONE', #229203, #126474, #132519, .T. ) ;
#160855 = CARTESIAN_POINT ( 'NONE',  ( -16.94445028196808778, 66.00793639031486748, -190.9157773061059800 ) ) ;
#160857 = CARTESIAN_POINT ( 'NONE',  ( 21.14999999999999858, 6.540656951712400691, -100.5000000000000284 ) ) ;
#160856 = CYLINDRICAL_SURFACE ( 'NONE', #240307, 0.4999999999999944489 ) ;
#160858 = SPHERICAL_SURFACE ( 'NONE', #7312, 0.1000000000000000056 ) ;
#160859 = DIRECTION ( 'NONE',  ( 1.000000000000000000, 0.000000000000000000, 0.000000000000000000 ) ) ;
#160860 = CARTESIAN_POINT ( 'NONE',  ( 23.15000000000000213, 81.82295291318693842, -214.8938525951558915 ) ) ;
#160861 = CIRCLE ( 'NONE', #194182, 1.749999999999999778 ) ;
#160862 = ORIENTED_EDGE ( 'NONE', *, *, #207833, .F. ) ;
#160863 = VECTOR ( 'NONE', #67409, 1000.000000000000000 ) ;
#160864 = EDGE_CURVE ( 'NONE', #120254, #142271, #86881, .T. ) ;
#160866 = ORIENTED_EDGE ( 'NONE', *, *, #113262, .F. ) ;
#160865 = DIRECTION ( 'NONE',  ( -1.000000000000000000, 0.000000000000000000, 0.000000000000000000 ) ) ;
#160867 = EDGE_CURVE ( 'NONE', #52869, #232805, #109198, .T. ) ;
#160868 = VECTOR ( 'NONE', #228062, 1000.000000000000114 ) ;
#160869 = SPHERICAL_SURFACE ( 'NONE', #103345, 0.1000000000000000056 ) ;
#160870 = FACE_OUTER_BOUND ( 'NONE', #55693, .T. ) ;
#160871 = AXIS2_PLACEMENT_3D ( 'NONE', #214914, #57098, #256552 ) ;
#160872 = EDGE_CURVE ( 'NONE', #144682, #129320, #107749, .T. ) ;
#160873 = AXIS2_PLACEMENT_3D ( 'NONE', #211189, #30015, #191663 ) ;
#160874 = CARTESIAN_POINT ( 'NONE',  ( 20.04142135623730070, 64.35000000001254250, -182.1731074845244507 ) ) ;
#160875 = ORIENTED_EDGE ( 'NONE', *, *, #142467, .F. ) ;
#160876 = FILL_AREA_STYLE ('',( #121751 ) ) ;
#160877 = DIRECTION ( 'NONE',  ( 0.000000000000000000, 0.4088369013363198357, -0.9126074666063807017 ) ) ;
#160878 = ADVANCED_FACE ( 'NONE', ( #229555 ), #161945, .T. ) ;
#160879 = DIRECTION ( 'NONE',  ( 0.000000000000000000, 0.9126074666063767049, 0.4088369013363286619 ) ) ;
#160880 = EDGE_LOOP ( 'NONE', ( #118093, #87034, #159950, #213677, #253673, #169764, #241528 ) ) ;
#160882 = DIRECTION ( 'NONE',  ( 0.000000000000000000, -0.5000000000000016653, 0.8660254037844377084 ) ) ;
#160881 = VECTOR ( 'NONE', #43758, 1000.000000000000000 ) ;
#160883 = LINE ( 'NONE', #40948, #217154 ) ;
#160884 = ADVANCED_FACE ( 'NONE', ( #45764 ), #167037, .T. ) ;
#160885 = DIRECTION ( 'NONE',  ( 0.000000000000000000, -1.000000000000000000, 0.000000000000000000 ) ) ;
#160886 = CIRCLE ( 'NONE', #173394, 7.800000000000007816 ) ;
#160887 = CARTESIAN_POINT ( 'NONE',  ( 20.85000000000000142, 77.75000000001162448, -57.90415744590205094 ) ) ;
#160889 = ORIENTED_EDGE ( 'NONE', *, *, #168921, .T. ) ;
#160888 = CARTESIAN_POINT ( 'NONE',  ( -20.94999999999999929, 70.15000000001178648, -79.65560470880228650 ) ) ;
#160890 = AXIS2_PLACEMENT_3D ( 'NONE', #249952, #15205, #209539 ) ;
#160892 = ORIENTED_EDGE ( 'NONE', *, *, #98746, .F. ) ;
#160891 = CARTESIAN_POINT ( 'NONE',  ( -23.15000000000000213, 1.115600667400684642E-11, -155.7000000000000455 ) ) ;
#160893 = DIRECTION ( 'NONE',  ( 1.000000000000000000, 0.000000000000000000, 0.000000000000000000 ) ) ;
#160894 = FACE_OUTER_BOUND ( 'NONE', #149866, .T. ) ;
#160895 = DIRECTION ( 'NONE',  ( -1.000000000000000000, -0.000000000000000000, -0.000000000000000000 ) ) ;
#160897 = EDGE_CURVE ( 'NONE', #127125, #75787, #245263, .T. ) ;
#160896 = LINE ( 'NONE', #137439, #144308 ) ;
#160899 = CARTESIAN_POINT ( 'NONE',  ( -20.64999999999999858, 44.96555909964510533, -237.8856228368455845 ) ) ;
#160898 = CARTESIAN_POINT ( 'NONE',  ( -17.22767730083791804, 65.65075578754621688, -80.88067879395967452 ) ) ;
#160900 = CARTESIAN_POINT ( 'NONE',  ( -21.05000000000000071, -4.656943609564678788, -233.1535107627236414 ) ) ;
#160901 = CYLINDRICAL_SURFACE ( 'NONE', #40843, 4.000000000000003553 ) ;
#160902 = CIRCLE ( 'NONE', #77462, 0.5000000000000004441 ) ;
#160903 = CARTESIAN_POINT ( 'NONE',  ( -20.94999999999999929, 64.40000000001234071, -163.0949042542488883 ) ) ;
#160904 = DIRECTION ( 'NONE',  ( 0.000000000000000000, -0.4999999999999943379, -0.8660254037844420383 ) ) ;
#160905 = DIRECTION ( 'NONE',  ( 1.000000000000000000, -0.000000000000000000, -0.000000000000000000 ) ) ;
#160906 = ORIENTED_EDGE ( 'NONE', *, *, #253646, .T. ) ;
#160907 = CARTESIAN_POINT ( 'NONE',  ( 20.94999999999999574, 62.00000000001161737, -64.09601495414187866 ) ) ;
#160908 = ORIENTED_EDGE ( 'NONE', *, *, #4953, .F. ) ;
#160909 = ORIENTED_EDGE ( 'NONE', *, *, #213307, .F. ) ;
#160910 = CARTESIAN_POINT ( 'NONE',  ( 20.94999999999999574, 1.849084418638171856, -145.6560105214471434 ) ) ;
#160911 = VERTEX_POINT ( 'NONE', #208716 ) ;
#160912 = AXIS2_PLACEMENT_3D ( 'NONE', #212086, #88241, #248627 ) ;
#160913 = VECTOR ( 'NONE', #187625, 1000.000000000000000 ) ;
#160914 = ORIENTED_EDGE ( 'NONE', *, *, #123244, .F. ) ;
#160915 = AXIS2_PLACEMENT_3D ( 'NONE', #148930, #138096, #239789 ) ;
#160916 = B_SPLINE_CURVE_WITH_KNOTS ( 'NONE', 3,
 ( #49890, #250647, #208966, #132001, #189414, #10775, #231126, #169895 ),
 .UNSPECIFIED., .F., .F.,
 ( 4, 2, 2, 4 ),
 ( 0.000000000000000000, 0.0001306511400391350121, 0.0001959767100587021793, 0.0002613022800782693737 ),
 .UNSPECIFIED. ) ;
#160917 = ORIENTED_EDGE ( 'NONE', *, *, #137161, .F. ) ;
#160918 = FACE_OUTER_BOUND ( 'NONE', #232776, .T. ) ;
#160919 = ORIENTED_EDGE ( 'NONE', *, *, #39947, .T. ) ;
#160920 = AXIS2_PLACEMENT_3D ( 'NONE', #237471, #199649, #82206 ) ;
#160921 = EDGE_CURVE ( 'NONE', #107353, #214060, #124513, .T. ) ;
#160922 = LINE ( 'NONE', #102176, #150622 ) ;
#160923 = DIRECTION ( 'NONE',  ( 1.000000000000000000, 0.000000000000000000, 0.000000000000000000 ) ) ;
#160924 = CARTESIAN_POINT ( 'NONE',  ( -16.77779411440718604, 66.05389855290421508, -82.18616490152891174 ) ) ;
#160925 = FACE_OUTER_BOUND ( 'NONE', #209979, .T. ) ;
#160926 = DIRECTION ( 'NONE',  ( -0.000000000000000000, 0.000000000000000000, 1.000000000000000000 ) ) ;
#160927 = FACE_BOUND ( 'NONE', #142162, .T. ) ;
#160928 = LINE ( 'NONE', #4392, #107697 ) ;
#160930 = ORIENTED_EDGE ( 'NONE', *, *, #31028, .T. ) ;
#160929 = CARTESIAN_POINT ( 'NONE',  ( -20.64999999999999858, 7.150000000011155876, -179.7499999999999716 ) ) ;
#160932 = CARTESIAN_POINT ( 'NONE',  ( 18.60000000000000497, 85.52394631232910172, -29.14107948918604407 ) ) ;
#160931 = CARTESIAN_POINT ( 'NONE',  ( 20.85000000000000142, 69.34766280046808617, -247.6726305063181144 ) ) ;
#160933 = EDGE_CURVE ( 'NONE', #140884, #18374, #204824, .T. ) ;
#160934 = DIRECTION ( 'NONE',  ( 1.000000000000000000, -0.000000000000000000, -0.000000000000000000 ) ) ;
#160936 = EDGE_CURVE ( 'NONE', #121315, #201117, #28825, .T. ) ;
#160935 = AXIS2_PLACEMENT_3D ( 'NONE', #69804, #209288, #103741 ) ;
#160937 = ORIENTED_EDGE ( 'NONE', *, *, #231207, .F. ) ;
#160938 = CARTESIAN_POINT ( 'NONE',  ( -18.44362607810620958, 8.869041504298024847, -245.4312441985596820 ) ) ;
#160940 = ORIENTED_EDGE ( 'NONE', *, *, #3527, .T. ) ;
#160939 = AXIS2_PLACEMENT_3D ( 'NONE', #226029, #85233, #68286 ) ;
#160941 = EDGE_CURVE ( 'NONE', #147468, #35933, #174453, .T. ) ;
#160943 = FACE_OUTER_BOUND ( 'NONE', #47728, .T. ) ;
#160942 = DIRECTION ( 'NONE',  ( -1.000000000000000000, 0.000000000000000000, 0.000000000000000000 ) ) ;
#160944 = ADVANCED_FACE ( 'NONE', ( #105709 ), #16201, .T. ) ;
#160945 = EDGE_CURVE ( 'NONE', #242008, #111920, #82767, .T. ) ;
#160946 = VERTEX_POINT ( 'NONE', #65326 ) ;
#160947 = SPHERICAL_SURFACE ( 'NONE', #246963, 0.1000000000000000056 ) ;
#160948 = PLANE ( 'NONE',  #24470 ) ;
#160949 = EDGE_CURVE ( 'NONE', #215142, #207750, #224455, .T. ) ;
#160950 = CARTESIAN_POINT ( 'NONE',  ( -21.05000000000000071, 77.16270174995034381, -161.9231074845243370 ) ) ;
#160951 = AXIS2_PLACEMENT_3D ( 'NONE', #30641, #232688, #110148 ) ;
#160952 = CARTESIAN_POINT ( 'NONE',  ( -20.64999999999999858, 23.68770167995059595, -252.8127582590406348 ) ) ;
#160953 = ORIENTED_EDGE ( 'NONE', *, *, #237370, .T. ) ;
#160954 = EDGE_CURVE ( 'NONE', #153949, #53791, #147437, .T. ) ;
#160955 = CARTESIAN_POINT ( 'NONE',  ( 20.94999999999999929, -11.64999999998883595, -131.0000000000000284 ) ) ;
#160956 = DIRECTION ( 'NONE',  ( 0.000000000000000000, -0.9908441862701791170, 0.1350103645450472789 ) ) ;
#160957 = CARTESIAN_POINT ( 'NONE',  ( -20.64999999999999858, 85.00000000001149658, -45.91707660717669626 ) ) ;
#160958 = EDGE_CURVE ( 'NONE', #118232, #92094, #157882, .T. ) ;
#160959 = AXIS2_PLACEMENT_3D ( 'NONE', #189468, #9526, #69533 ) ;
#160960 = CARTESIAN_POINT ( 'NONE',  ( -21.07928932188134041, 69.67148334361884565, -136.6220026301787414 ) ) ;
#160961 = CIRCLE ( 'NONE', #202634, 0.09999999999999516220 ) ;
#160962 = CARTESIAN_POINT ( 'NONE',  ( -18.45068461519106862, 85.48650652910143322, -162.9543303156196146 ) ) ;
#160963 = EDGE_CURVE ( 'NONE', #230288, #219800, #232675, .T. ) ;
#160965 = ORIENTED_EDGE ( 'NONE', *, *, #112499, .T. ) ;
#160964 = CARTESIAN_POINT ( 'NONE',  ( 21.07964655665547582, 8.774889614989714204, -179.7219165829640417 ) ) ;
#160966 = LINE ( 'NONE', #132102, #239313 ) ;
#160967 = FACE_OUTER_BOUND ( 'NONE', #131581, .T. ) ;
#160968 = CARTESIAN_POINT ( 'NONE',  ( 18.43709777086140278, 77.26488334054519669, -241.9697969554615042 ) ) ;
#160969 = CARTESIAN_POINT ( 'NONE',  ( 21.05000000000000071, 6.540656951712400691, -167.5999999999999659 ) ) ;
#160970 = DIRECTION ( 'NONE',  ( 0.000000000000000000, 0.9856811345164829818, 0.1686199900910294314 ) ) ;
#160971 = EDGE_CURVE ( 'NONE', #143516, #174236, #252369, .T. ) ;
#160973 = EDGE_LOOP ( 'NONE', ( #216354, #119126, #98785, #167645 ) ) ;
#160972 = LINE ( 'NONE', #237918, #94276 ) ;
#160974 = CARTESIAN_POINT ( 'NONE',  ( 21.14999999999999858, 6.550000000011156231, -146.3500000000000227 ) ) ;
#160975 = EDGE_CURVE ( 'NONE', #193742, #11383, #56006, .T. ) ;
#160976 = CARTESIAN_POINT ( 'NONE',  ( -17.11825945287481332, 63.08573235307419935, -213.1276215869287967 ) ) ;
#160977 = DIRECTION ( 'NONE',  ( 0.000000000000000000, 0.000000000000000000, -1.000000000000000000 ) ) ;
#160978 = ORIENTED_EDGE ( 'NONE', *, *, #157653, .T. ) ;
#160979 = CARTESIAN_POINT ( 'NONE',  ( 23.15000000000000213, -8.999999999988842703, -124.1060308773475924 ) ) ;
#160980 = CARTESIAN_POINT ( 'NONE',  ( 18.59999999999999432, 77.83585931145498193, -24.51866831572578320 ) ) ;
#160981 = VECTOR ( 'NONE', #194291, 999.9999999999998863 ) ;
#160983 = AXIS2_PLACEMENT_3D ( 'NONE', #54891, #157915, #152760 ) ;
#160982 = DIRECTION ( 'NONE',  ( 0.000000000000000000, -0.2617529984165031243, -0.9651348961777157509 ) ) ;
#160984 = VERTEX_POINT ( 'NONE', #37782 ) ;
#160985 = ORIENTED_EDGE ( 'NONE', *, *, #22381, .F. ) ;
#160987 = CARTESIAN_POINT ( 'NONE',  ( -22.94999999999999929, 11.59510167572422112, -1.901609089591594692 ) ) ;
#160986 = AXIS2_PLACEMENT_3D ( 'NONE', #12230, #30507, #232567 ) ;
#160988 = CARTESIAN_POINT ( 'NONE',  ( -21.09610168723072476, 34.02031789858177291, -243.7434127162948698 ) ) ;
#160989 = DIRECTION ( 'NONE',  ( 0.000000000000000000, -8.556632174375010717E-15, 1.000000000000000000 ) ) ;
#160990 = ORIENTED_EDGE ( 'NONE', *, *, #134985, .T. ) ;
#160991 = CARTESIAN_POINT ( 'NONE',  ( -13.39999999999994529, 67.65000000001118963, -21.02310748452479316 ) ) ;
#160992 = DIRECTION ( 'NONE',  ( 6.938893903907131190E-14, -0.8814952561688476074, 0.4721928772777262417 ) ) ;
#160993 = CARTESIAN_POINT ( 'NONE',  ( -21.14999999999999858, -0.09999999998884338825, -93.95934304829879125 ) ) ;
#160994 = CARTESIAN_POINT ( 'NONE',  ( -21.05000000000000071, 16.98881331171929787, -224.4946931418895417 ) ) ;
#160995 = CARTESIAN_POINT ( 'NONE',  ( -16.83233564386403813, 9.930221796584607574, -20.72452066347563004 ) ) ;
#160996 = TOROIDAL_SURFACE ( 'NONE', #52822, 12.77499999999999858, 0.1000000000000000056 ) ;
#160997 = ORIENTED_EDGE ( 'NONE', *, *, #134574, .T. ) ;
#160999 = ORIENTED_EDGE ( 'NONE', *, *, #153062, .T. ) ;
#160998 = CARTESIAN_POINT ( 'NONE',  ( -16.92507428761700083, 66.05000000001153637, -48.73650494414594192 ) ) ;
#161000 = ORIENTED_EDGE ( 'NONE', *, *, #144280, .T. ) ;
#161001 = CARTESIAN_POINT ( 'NONE',  ( -20.94999999999999929, 7.031312794755200102, -37.10915093822730881 ) ) ;
#161002 = ORIENTED_EDGE ( 'NONE', *, *, #40219, .T. ) ;
#161003 = CARTESIAN_POINT ( 'NONE',  ( 21.08479644141223375, 75.94144555744830427, -176.3681461422563075 ) ) ;
#161004 = CARTESIAN_POINT ( 'NONE',  ( 20.89999999999999503, 8.000000000000000000, 1.212568896937007867 ) ) ;
#161005 = CARTESIAN_POINT ( 'NONE',  ( 20.94999999999999574, 4.260086453440762533, -245.2296700999207246 ) ) ;
#161006 = ORIENTED_EDGE ( 'NONE', *, *, #127289, .F. ) ;
#161007 = CARTESIAN_POINT ( 'NONE',  ( -16.92973740335341404, 66.00749618554429787, -56.92916651972676334 ) ) ;
#161008 = FACE_BOUND ( 'NONE', #99503, .T. ) ;
#161009 = CIRCLE ( 'NONE', #119908, 0.2000000000000057288 ) ;
#161010 = ORIENTED_EDGE ( 'NONE', *, *, #82271, .F. ) ;
#161011 = CARTESIAN_POINT ( 'NONE',  ( -16.86337532320260735, 9.979967204235514089, -54.44892446898280980 ) ) ;
#161012 = EDGE_CURVE ( 'NONE', #233248, #87397, #220194, .T. ) ;
#161014 = ORIENTED_EDGE ( 'NONE', *, *, #193251, .F. ) ;
#161013 = DIRECTION ( 'NONE',  ( 1.000000000000000000, 0.000000000000000000, 0.000000000000000000 ) ) ;
#161015 = FACE_OUTER_BOUND ( 'NONE', #99899, .T. ) ;
#161016 = CARTESIAN_POINT ( 'NONE',  ( -20.64999999999999858, 1.115600667400684642E-11, -67.00000000000000000 ) ) ;
#161017 = VECTOR ( 'NONE', #144602, 1000.000000000000000 ) ;
#161018 = EDGE_CURVE ( 'NONE', #216543, #176995, #152606, .T. ) ;
#161019 = AXIS2_PLACEMENT_3D ( 'NONE', #198353, #120148, #19737 ) ;
#161020 = CIRCLE ( 'NONE', #2780, 0.1000000000000057648 ) ;
#161021 = ORIENTED_EDGE ( 'NONE', *, *, #80195, .F. ) ;
#161023 = CARTESIAN_POINT ( 'NONE',  ( 18.79999999999999716, 1.786320531569725478, -11.50977166988710820 ) ) ;
#161022 = AXIS2_PLACEMENT_3D ( 'NONE', #2810, #82330, #176353 ) ;
#161025 = EDGE_CURVE ( 'NONE', #254110, #206570, #224273, .T. ) ;
#161024 = CARTESIAN_POINT ( 'NONE',  ( 21.07189867249812210, 10.72498027010430377, -79.21245144227678736 ) ) ;
#161026 = CARTESIAN_POINT ( 'NONE',  ( 21.05000000000000071, 5.400000000011154988, -45.90526601891310321 ) ) ;
#161028 = EDGE_CURVE ( 'NONE', #70737, #74558, #252941, .T. ) ;
#161027 = ORIENTED_EDGE ( 'NONE', *, *, #53792, .T. ) ;
#161029 = DIRECTION ( 'NONE',  ( -1.000000000000000000, 7.304098846218135653E-16, 4.639676173203994055E-30 ) ) ;
#161030 = CARTESIAN_POINT ( 'NONE',  ( 12.68104795156995301, 49.15836891943283860, -233.6552066833104107 ) ) ;
#161031 = DIRECTION ( 'NONE',  ( 0.000000000000000000, 0.4721928772778128947, 0.8814952561688012000 ) ) ;
#161032 = VERTEX_POINT ( 'NONE', #96427 ) ;
#161033 = AXIS2_PLACEMENT_3D ( 'NONE', #235044, #43259, #120263 ) ;
#161035 = ADVANCED_FACE ( 'NONE', ( #71774 ), #134271, .T. ) ;
#161034 = VECTOR ( 'NONE', #172676, 1000.000000000000000 ) ;
#161036 = EDGE_LOOP ( 'NONE', ( #115050, #128674, #52515, #31622 ) ) ;
#161037 = VECTOR ( 'NONE', #91906, 1000.000000000000000 ) ;
#161038 = ORIENTED_EDGE ( 'NONE', *, *, #246478, .T. ) ;
#161039 =( GEOMETRIC_REPRESENTATION_CONTEXT ( 3 ) GLOBAL_UNCERTAINTY_ASSIGNED_CONTEXT ( ( #89489 ) ) GLOBAL_UNIT_ASSIGNED_CONTEXT ( ( #53275, #55795, #151095 ) ) REPRESENTATION_CONTEXT ( 'NONE', 'WORKASPACE' ) );
#161040 = CARTESIAN_POINT ( 'NONE',  ( 18.58222699835054570, 10.33200063079656772, -39.09316749566428939 ) ) ;
#161041 = DIRECTION ( 'NONE',  ( 0.000000000000000000, 0.000000000000000000, -1.000000000000000000 ) ) ;
#161043 = ORIENTED_EDGE ( 'NONE', *, *, #248971, .T. ) ;
#161042 = CARTESIAN_POINT ( 'NONE',  ( -16.78493832629886739, 9.945835743215301505, -146.6639490191042228 ) ) ;
#161044 = LINE ( 'NONE', #220992, #44852 ) ;
#161046 = AXIS2_PLACEMENT_3D ( 'NONE', #244435, #246998, #204023 ) ;
#161045 = CARTESIAN_POINT ( 'NONE',  ( -20.00857864376270001, 9.150000000011157653, -79.35000000000005116 ) ) ;
#161047 = CARTESIAN_POINT ( 'NONE',  ( -22.59999985501179154, 11.46678616150632379, -198.4355198451642366 ) ) ;
#161048 = AXIS2_PLACEMENT_3D ( 'NONE', #233348, #75556, #195505 ) ;
#161049 = DIRECTION ( 'NONE',  ( 0.000000000000000000, 0.000000000000000000, 1.000000000000000000 ) ) ;
#161050 = CARTESIAN_POINT ( 'NONE',  ( -20.85000000000000142, 64.25000000001148237, -42.86470817442146597 ) ) ;
#161053 = ORIENTED_EDGE ( 'NONE', *, *, #14446, .F. ) ;
#161052 = EDGE_CURVE ( 'NONE', #31313, #197247, #215112, .T. ) ;
#161051 = CARTESIAN_POINT ( 'NONE',  ( 23.14999999999999858, 4.813084112160680661, -78.94151775652387926 ) ) ;
#161055 = VERTEX_POINT ( 'NONE', #14376 ) ;
#161054 = DIRECTION ( 'NONE',  ( 0.000000000000000000, -0.1298341882519953583, -0.9915357197604861561 ) ) ;
#161056 = CARTESIAN_POINT ( 'NONE',  ( -16.92778301347280490, 60.86963669884748640, -221.1041733168329131 ) ) ;
#161057 = ORIENTED_EDGE ( 'NONE', *, *, #128741, .F. ) ;
#161058 = ORIENTED_EDGE ( 'NONE', *, *, #34705, .T. ) ;
#161059 = EDGE_CURVE ( 'NONE', #238843, #83407, #174751, .T. ) ;
#161060 = LINE ( 'NONE', #240586, #51611 ) ;
#161061 = DIRECTION ( 'NONE',  ( 0.000000000000000000, 1.897661533703519897E-16, -1.000000000000000000 ) ) ;
#161062 = AXIS2_PLACEMENT_3D ( 'NONE', #98248, #218209, #154454 ) ;
#161063 = VECTOR ( 'NONE', #30390, 1000.000000000000000 ) ;
#161064 = AXIS2_PLACEMENT_3D ( 'NONE', #1890, #179296, #24074 ) ;
#161065 = CARTESIAN_POINT ( 'NONE',  ( -17.78043020864321022, 65.14640788800693372, -193.1861566502446408 ) ) ;
#161066 = CARTESIAN_POINT ( 'NONE',  ( 23.14999999999999503, 64.35000000001222986, -148.7731074845244450 ) ) ;
#161067 = DIRECTION ( 'NONE',  ( -0.000000000000000000, -1.000000000000000000, 6.308085367188393199E-16 ) ) ;
#161069 = EDGE_CURVE ( 'NONE', #238889, #154195, #66053, .T. ) ;
#161068 = CARTESIAN_POINT ( 'NONE',  ( 20.30466543256828160, 66.69576306075845196, -195.2694448331317005 ) ) ;
#161070 = EDGE_CURVE ( 'NONE', #43988, #257957, #93878, .T. ) ;
#161071 = CARTESIAN_POINT ( 'NONE',  ( -21.45000000000000284, 68.29142135624984178, -182.3731074845244109 ) ) ;
#161072 = ORIENTED_EDGE ( 'NONE', *, *, #170227, .F. ) ;
#161073 = ORIENTED_EDGE ( 'NONE', *, *, #48043, .F. ) ;
#161074 = CARTESIAN_POINT ( 'NONE',  ( -23.15000000000000213, 1.115600667400684642E-11, -67.00000000000000000 ) ) ;
#161075 = AXIS2_PLACEMENT_3D ( 'NONE', #136409, #97271, #98553 ) ;
#161076 = EDGE_CURVE ( 'NONE', #18553, #57931, #211822, .T. ) ;
#161077 = VERTEX_POINT ( 'NONE', #36505 ) ;
#161078 = CARTESIAN_POINT ( 'NONE',  ( 21.14999999999999503, 11.65000000001116298, -167.4999999999999716 ) ) ;
#161079 = DIRECTION ( 'NONE',  ( 2.952720810173288619E-16, 0.4088369013363239990, -0.9126074666063788143 ) ) ;
#161080 = CARTESIAN_POINT ( 'NONE',  ( 22.00356870069842330, 76.00000000001244871, -177.2773498462712496 ) ) ;
#161081 = DIRECTION ( 'NONE',  ( -1.000000000000000000, -1.394253735153569469E-16, -2.602809386958778209E-16 ) ) ;
#161082 = ORIENTED_EDGE ( 'NONE', *, *, #76993, .T. ) ;
#161083 = LINE ( 'NONE', #21575, #219283 ) ;
#161084 = EDGE_LOOP ( 'NONE', ( #87854, #235511, #189641, #23782 ) ) ;
#161085 = EDGE_CURVE ( 'NONE', #43467, #70620, #53475, .T. ) ;
#161086 = CARTESIAN_POINT ( 'NONE',  ( -17.01825945287481545, 9.950000000011138823, -54.25000000000000711 ) ) ;
#161087 = ORIENTED_EDGE ( 'NONE', *, *, #75636, .T. ) ;
#161088 = CIRCLE ( 'NONE', #256890, 0.09999999999999824307 ) ;
#161089 = DIRECTION ( 'NONE',  ( 1.000000000000000000, -3.265361837132813093E-16, -2.280189983783949500E-30 ) ) ;
#161090 = VECTOR ( 'NONE', #26752, 1000.000000000000000 ) ;
#161091 = EDGE_CURVE ( 'NONE', #81561, #213031, #3441, .T. ) ;
#161092 = DIRECTION ( 'NONE',  ( 0.000000000000000000, 0.9770955615653316162, 0.2128009952263604232 ) ) ;
#161093 = VECTOR ( 'NONE', #72060, 1000.000000000000000 ) ;
#161094 = AXIS2_PLACEMENT_3D ( 'NONE', #196790, #42867, #122408 ) ;
#161095 = ORIENTED_EDGE ( 'NONE', *, *, #250623, .F. ) ;
#161096 = FACE_OUTER_BOUND ( 'NONE', #123319, .T. ) ;
#161098 = ORIENTED_EDGE ( 'NONE', *, *, #231296, .F. ) ;
#161097 = CARTESIAN_POINT ( 'NONE',  ( -21.40925344232282512, 6.658518859401606704, -100.4010498113803891 ) ) ;
#161099 = DIRECTION ( 'NONE',  ( 1.186688945009010077E-16, -1.000000000000000000, -0.000000000000000000 ) ) ;
#161100 = ORIENTED_EDGE ( 'NONE', *, *, #88382, .F. ) ;
#161101 = CIRCLE ( 'NONE', #148636, 0.5000000000000004441 ) ;
#161102 = CARTESIAN_POINT ( 'NONE',  ( -23.25000000000000000, 2.000000000011154189, -113.7246219227621395 ) ) ;
#161103 = ORIENTED_EDGE ( 'NONE', *, *, #190660, .T. ) ;
#161104 = PLANE ( 'NONE',  #165945 ) ;
#161105 = CARTESIAN_POINT ( 'NONE',  ( 20.04142135391667168, 64.25000000001250555, -178.8206006188949289 ) ) ;
#161106 = AXIS2_PLACEMENT_3D ( 'NONE', #4354, #205116, #223400 ) ;
#161107 = DIRECTION ( 'NONE',  ( 0.000000000000000000, 0.000000000000000000, -1.000000000000000000 ) ) ;
#161108 = CARTESIAN_POINT ( 'NONE',  ( -16.93658211146646408, 66.00589133767039129, -56.92740255448007503 ) ) ;
#161109 = CIRCLE ( 'NONE', #40349, 0.09999999999999939493 ) ;
#161110 = FACE_OUTER_BOUND ( 'NONE', #234116, .T. ) ;
#161111 = VECTOR ( 'NONE', #143323, 999.9999999999998863 ) ;
#161112 = VERTEX_POINT ( 'NONE', #243327 ) ;
#161113 = CYLINDRICAL_SURFACE ( 'NONE', #27842, 1.749999999999999778 ) ;
#161114 = CARTESIAN_POINT ( 'NONE',  ( 21.13422380239052245, 6.493326514816728512, -100.5000000000000426 ) ) ;
#161115 = DIRECTION ( 'NONE',  ( -1.000000000000000000, 0.000000000000000000, 0.000000000000000000 ) ) ;
#161116 = VERTEX_POINT ( 'NONE', #205481 ) ;
#161117 = CARTESIAN_POINT ( 'NONE',  ( -21.05000000000068638, 75.94867256767054187, -109.3232908207938294 ) ) ;
#161118 = ORIENTED_EDGE ( 'NONE', *, *, #868, .T. ) ;
#161119 = CARTESIAN_POINT ( 'NONE',  ( 18.59999999999999076, 6.550000000011156231, -121.7500000000000426 ) ) ;
#161120 = ORIENTED_EDGE ( 'NONE', *, *, #31614, .F. ) ;
#161121 = DIRECTION ( 'NONE',  ( 1.000000000000000000, 0.000000000000000000, 0.000000000000000000 ) ) ;
#161122 = CARTESIAN_POINT ( 'NONE',  ( -20.91682497891422798, 10.32263460347359363, -72.56059579686719019 ) ) ;
#161123 = ORIENTED_EDGE ( 'NONE', *, *, #126168, .T. ) ;
#161125 = ORIENTED_EDGE ( 'NONE', *, *, #188749, .T. ) ;
#161124 = CARTESIAN_POINT ( 'NONE',  ( -1.739115166359751801E-14, 11.65000000001114699, -54.85000000000000142 ) ) ;
#161126 = ORIENTED_EDGE ( 'NONE', *, *, #28625, .T. ) ;
#161127 = DIRECTION ( 'NONE',  ( 0.000000000000000000, 0.000000000000000000, 1.000000000000000000 ) ) ;
#161128 = DIRECTION ( 'NONE',  ( 1.000000000000000000, 0.000000000000000000, 0.000000000000000000 ) ) ;
#161129 = ORIENTED_EDGE ( 'NONE', *, *, #151558, .F. ) ;
#161130 = VERTEX_POINT ( 'NONE', #157761 ) ;
#161131 = CYLINDRICAL_SURFACE ( 'NONE', #118437, 0.09999999999998898659 ) ;
#161133 = EDGE_CURVE ( 'NONE', #5347, #111551, #86810, .T. ) ;
#161132 = CARTESIAN_POINT ( 'NONE',  ( 21.05000000000000071, 75.96513199699965924, -209.7931933482134923 ) ) ;
#161134 = CARTESIAN_POINT ( 'NONE',  ( 23.15000000000000213, 87.75000000001186606, -90.87310748452424036 ) ) ;
#161135 = CIRCLE ( 'NONE', #48685, 0.09999999999998898659 ) ;
#161136 = AXIS2_PLACEMENT_3D ( 'NONE', #31692, #126910, #70813 ) ;
#161137 = VECTOR ( 'NONE', #38239, 1000.000000000000000 ) ;
#161138 = ORIENTED_EDGE ( 'NONE', *, *, #104156, .F. ) ;
#161139 = ORIENTED_EDGE ( 'NONE', *, *, #209238, .T. ) ;
#161140 = CARTESIAN_POINT ( 'NONE',  ( -23.15000000000000213, 0.000000000000000000, -33.50000000000000000 ) ) ;
#161141 = EDGE_CURVE ( 'NONE', #245477, #207912, #159023, .T. ) ;
#161143 = ORIENTED_EDGE ( 'NONE', *, *, #140414, .F. ) ;
#161142 = DIRECTION ( 'NONE',  ( 1.000000000000000000, 0.000000000000000000, -0.000000000000000000 ) ) ;
#161144 = ADVANCED_FACE ( 'NONE', ( #198115 ), #226313, .F. ) ;
#161145 = CARTESIAN_POINT ( 'NONE',  ( -23.25000000000000355, 11.75000000001113953, -146.6500000000000341 ) ) ;
#161146 = EDGE_CURVE ( 'NONE', #176380, #26537, #253491, .T. ) ;
#161147 = CARTESIAN_POINT ( 'NONE',  ( 21.87500000000000355, 30.46448808713892831, -235.1722212069449256 ) ) ;
#161148 = CARTESIAN_POINT ( 'NONE',  ( -20.64999999999999858, 45.00644278977874535, -237.9768835835062077 ) ) ;
#161149 = AXIS2_PLACEMENT_3D ( 'NONE', #152960, #112520, #53820 ) ;
#161151 = LINE ( 'NONE', #3327, #128451 ) ;
#161150 = CARTESIAN_POINT ( 'NONE',  ( -17.22767730083365123, 65.65075578754337471, -125.1655361750991204 ) ) ;
#161152 = CARTESIAN_POINT ( 'NONE',  ( -21.07928932188134397, 75.90110485435778287, -142.8516241409176075 ) ) ;
#161153 = CARTESIAN_POINT ( 'NONE',  ( 5.900000000000060751, 64.65000000001120384, -22.12310748452479103 ) ) ;
#161154 = AXIS2_PLACEMENT_3D ( 'NONE', #40044, #239505, #219930 ) ;
#161155 = CIRCLE ( 'NONE', #256955, 6.258578643762696458 ) ;
#161156 = CARTESIAN_POINT ( 'NONE',  ( -16.86757978335471719, 60.91064310117739211, -221.0878137256144100 ) ) ;
#161157 = CARTESIAN_POINT ( 'NONE',  ( 23.24999999999999289, 11.65000000001116298, -88.75000000000004263 ) ) ;
#161158 = ORIENTED_EDGE ( 'NONE', *, *, #67026, .T. ) ;
#161159 = AXIS2_PLACEMENT_3D ( 'NONE', #38530, #118056, #649 ) ;
#161160 = ORIENTED_EDGE ( 'NONE', *, *, #121500, .T. ) ;
#161161 = ADVANCED_FACE ( 'NONE', ( #237249 ), #132720, .F. ) ;
#161162 = DIRECTION ( 'NONE',  ( 0.000000000000000000, 0.000000000000000000, 1.000000000000000000 ) ) ;
#161163 = EDGE_LOOP ( 'NONE', ( #94037, #183257, #209550, #249511 ) ) ;
#161164 = DIRECTION ( 'NONE',  ( 1.000000000000000000, 0.000000000000000000, 0.000000000000000000 ) ) ;
#161165 = VERTEX_POINT ( 'NONE', #65983 ) ;
#161166 =( LENGTH_UNIT ( ) NAMED_UNIT ( * ) SI_UNIT ( .MILLI., .METRE. ) );
#161167 = CARTESIAN_POINT ( 'NONE',  ( -21.05000000000000426, 69.52295361822253028, -169.9231074845244507 ) ) ;
#161170 = ORIENTED_EDGE ( 'NONE', *, *, #65579, .F. ) ;
#161169 = VERTEX_POINT ( 'NONE', #144216 ) ;
#161168 = CIRCLE ( 'NONE', #115372, 0.09999999999998898659 ) ;
#161171 = ORIENTED_EDGE ( 'NONE', *, *, #37480, .T. ) ;
#161172 = ORIENTED_EDGE ( 'NONE', *, *, #52973, .T. ) ;
#161173 = DIRECTION ( 'NONE',  ( -1.000000000000000000, 0.000000000000000000, -0.000000000000000000 ) ) ;
#161174 = DIRECTION ( 'NONE',  ( 1.000000000000000000, 1.186688945009010077E-16, 0.000000000000000000 ) ) ;
#161176 = EDGE_LOOP ( 'NONE', ( #229531, #27514, #171073 ) ) ;
#161175 = CARTESIAN_POINT ( 'NONE',  ( -23.15000000000000213, 65.31479887318495514, -236.7136839992847399 ) ) ;
#161177 = EDGE_CURVE ( 'NONE', #86653, #140654, #170348, .T. ) ;
#161178 = CARTESIAN_POINT ( 'NONE',  ( 20.13684514580175033, 40.20805984460254479, -237.5560023261490699 ) ) ;
#161179 = DIRECTION ( 'NONE',  ( 0.000000000000000000, -1.000000000000000000, 0.000000000000000000 ) ) ;
#161181 = ORIENTED_EDGE ( 'NONE', *, *, #208638, .T. ) ;
#161180 = CARTESIAN_POINT ( 'NONE',  ( -20.54999999999999716, 1.925233644859811521, -20.76975646687386501 ) ) ;
#161182 = CARTESIAN_POINT ( 'NONE',  ( 19.83283456528358002, 11.75000000001116263, -125.3499999994178182 ) ) ;
#161183 = ORIENTED_EDGE ( 'NONE', *, *, #211440, .F. ) ;
#161185 = DIRECTION ( 'NONE',  ( 0.000000000000000000, 0.000000000000000000, -1.000000000000000000 ) ) ;
#161184 = VECTOR ( 'NONE', #98034, 1000.000000000000000 ) ;
#161187 = ORIENTED_EDGE ( 'NONE', *, *, #203593, .F. ) ;
#161186 = DIRECTION ( 'NONE',  ( 0.000000000000000000, -0.8814952561688476074, 0.4721928772777262417 ) ) ;
#161188 = DIRECTION ( 'NONE',  ( 0.000000000000000000, -7.147358527629766941E-15, 1.000000000000000000 ) ) ;
#161189 = CARTESIAN_POINT ( 'NONE',  ( -14.45422546970484667, 27.84954713259351777, -234.1111166998237536 ) ) ;
#161191 = EDGE_CURVE ( 'NONE', #239027, #109775, #3746, .T. ) ;
#161190 = DIRECTION ( 'NONE',  ( -1.000000000000000000, -0.000000000000000000, -0.000000000000000000 ) ) ;
#161192 = AXIS2_PLACEMENT_3D ( 'NONE', #104822, #9609, #168748 ) ;
#161193 = ORIENTED_EDGE ( 'NONE', *, *, #208905, .T. ) ;
#161195 = DIRECTION ( 'NONE',  ( 0.000000000000000000, 0.9126074666063772600, 0.4088369013363274407 ) ) ;
#161194 = CARTESIAN_POINT ( 'NONE',  ( -23.15000000000000213, 11.65000000001115588, -54.85000000000000142 ) ) ;
#161196 = DIRECTION ( 'NONE',  ( 0.000000000000000000, -0.8660254037844411501, -0.4999999999999956146 ) ) ;
#161197 = CYLINDRICAL_SURFACE ( 'NONE', #101532, 0.09999999999999939493 ) ;
#161198 = CIRCLE ( 'NONE', #65500, 0.1000000000000006717 ) ;
#161199 = AXIS2_PLACEMENT_3D ( 'NONE', #87700, #147699, #93812 ) ;
#161200 = CARTESIAN_POINT ( 'NONE',  ( -18.59999999999999787, 74.14897176987143723, -158.3691942151018850 ) ) ;
#161201 = CARTESIAN_POINT ( 'NONE',  ( -18.40000000000000213, 8.822561741666397950, -9.250000000000001776 ) ) ;
#161202 = VERTEX_POINT ( 'NONE', #238523 ) ;
#161203 = ORIENTED_EDGE ( 'NONE', *, *, #76319, .F. ) ;
#161204 = ORIENTED_EDGE ( 'NONE', *, *, #144210, .F. ) ;
#161205 = DIRECTION ( 'NONE',  ( 0.000000000000000000, 0.000000000000000000, -1.000000000000000000 ) ) ;
#161206 = DIRECTION ( 'NONE',  ( -1.000000000000000000, 0.000000000000000000, -0.000000000000000000 ) ) ;
#161207 = VECTOR ( 'NONE', #155094, 1000.000000000000000 ) ;
#161208 = EDGE_LOOP ( 'NONE', ( #202466, #157327, #237624, #77983 ) ) ;
#161209 = FACE_OUTER_BOUND ( 'NONE', #34135, .T. ) ;
#161210 = ORIENTED_EDGE ( 'NONE', *, *, #80478, .T. ) ;
#161212 = CARTESIAN_POINT ( 'NONE',  ( -20.94999999999999929, 64.35000000001214460, -136.5231074845244166 ) ) ;
#161211 = AXIS2_PLACEMENT_3D ( 'NONE', #250076, #130116, #173157 ) ;
#161213 = LINE ( 'NONE', #139028, #220984 ) ;
#161214 = ORIENTED_EDGE ( 'NONE', *, *, #37644, .T. ) ;
#161215 = CARTESIAN_POINT ( 'NONE',  ( -21.00000000000000000, 6.258114003436814343, 11.90000000000000036 ) ) ;
#161216 = AXIS2_PLACEMENT_3D ( 'NONE', #185334, #65381, #144900 ) ;
#161217 = ORIENTED_EDGE ( 'NONE', *, *, #135947, .F. ) ;
#161218 = ORIENTED_EDGE ( 'NONE', *, *, #119723, .T. ) ;
#161219 = CIRCLE ( 'NONE', #32063, 0.1000000000000026007 ) ;
#161220 = EDGE_LOOP ( 'NONE', ( #94261, #48741, #196786, #250625 ) ) ;
#161221 = EDGE_CURVE ( 'NONE', #212847, #193307, #25586, .T. ) ;
#161223 = CARTESIAN_POINT ( 'NONE',  ( 18.59999999999999787, 79.24821784679177483, -196.3217825494968736 ) ) ;
#161222 = VECTOR ( 'NONE', #64044, 1000.000000000000000 ) ;
#161224 = DIRECTION ( 'NONE',  ( 0.000000000000000000, 1.561251128379298294E-13, 1.000000000000000000 ) ) ;
#161225 = FACE_OUTER_BOUND ( 'NONE', #240665, .T. ) ;
#161226 = ADVANCED_FACE ( 'NONE', ( #59862 ), #26888, .T. ) ;
#161227 = DIRECTION ( 'NONE',  ( 0.000000000000000000, 0.000000000000000000, -1.000000000000000000 ) ) ;
#161228 = CARTESIAN_POINT ( 'NONE',  ( 20.94999999999999929, -8.999999999988844479, -177.3939691226524076 ) ) ;
#161229 = AXIS2_PLACEMENT_3D ( 'NONE', #91768, #206575, #8387 ) ;
#161230 = DIRECTION ( 'NONE',  ( -1.000000000000000000, 0.000000000000000000, 0.000000000000000000 ) ) ;
#161232 = DIRECTION ( 'NONE',  ( -1.000000000000000000, -1.394253735153569469E-16, -2.602809386958778209E-16 ) ) ;
#161231 = CARTESIAN_POINT ( 'NONE',  ( 23.14999999999999858, 5.000000000011153745, -54.59473398108690390 ) ) ;
#161233 = DIRECTION ( 'NONE',  ( 0.000000000000000000, 0.000000000000000000, 1.000000000000000000 ) ) ;
#161235 = EDGE_LOOP ( 'NONE', ( #116259, #102431, #142051, #220670, #93983, #83967, #150552, #123873, #189266, #131311, #242318, #224311 ) ) ;
#161234 = CARTESIAN_POINT ( 'NONE',  ( -23.15000000000000213, 76.00000000001244871, -170.0231074845243597 ) ) ;
#161236 = CARTESIAN_POINT ( 'NONE',  ( 21.07928932188134397, 69.67148334361864670, -103.1220026301787414 ) ) ;
#161237 = AXIS2_PLACEMENT_3D ( 'NONE', #83430, #200849, #104289 ) ;
#161238 = EDGE_CURVE ( 'NONE', #54023, #72236, #57848, .T. ) ;
#161240 = B_SPLINE_CURVE_WITH_KNOTS ( 'NONE', 3,
 ( #218263, #119196, #57908, #157045, #32300, #152249 ),
 .UNSPECIFIED., .F., .F.,
 ( 4, 2, 4 ),
 ( 1.138412281109779656E-18, 0.0001569047307838639517, 0.0003138094615677267650 ),
 .UNSPECIFIED. ) ;
#161239 = DIRECTION ( 'NONE',  ( -6.938893903907222856E-15, 1.000000000000000000, 2.891205793294679805E-16 ) ) ;
#161241 = EDGE_CURVE ( 'NONE', #103372, #241878, #203616, .T. ) ;
#161242 = AXIS2_PLACEMENT_3D ( 'NONE', #134545, #130705, #169893 ) ;
#161243 = ORIENTED_EDGE ( 'NONE', *, *, #27033, .F. ) ;
#161244 = DIRECTION ( 'NONE',  ( -0.000000000000000000, -1.000000000000000000, -6.982962677686266711E-15 ) ) ;
#161245 = CARTESIAN_POINT ( 'NONE',  ( 11.60000000000006004, 64.25000000001119815, -21.02310748452479316 ) ) ;
#161246 = ORIENTED_EDGE ( 'NONE', *, *, #208898, .F. ) ;
#161247 = EDGE_CURVE ( 'NONE', #56184, #112707, #45398, .T. ) ;
#161248 = ADVANCED_FACE ( 'NONE', ( #256751 ), #78152, .F. ) ;
#161249 = DIRECTION ( 'NONE',  ( 0.000000000000000000, 0.000000000000000000, 1.000000000000000000 ) ) ;
#161251 = EDGE_CURVE ( 'NONE', #155284, #257108, #12112, .T. ) ;
#161250 = EDGE_CURVE ( 'NONE', #194499, #7029, #9857, .T. ) ;
#161253 = ORIENTED_EDGE ( 'NONE', *, *, #38838, .F. ) ;
#161252 = CIRCLE ( 'NONE', #123836, 0.1000000000000055844 ) ;
#161254 = ORIENTED_EDGE ( 'NONE', *, *, #67960, .T. ) ;
#161255 = CARTESIAN_POINT ( 'NONE',  ( -16.85718274719414467, 9.976142314621760931, -12.56334633218240349 ) ) ;
#161256 = EDGE_LOOP ( 'NONE', ( #87166, #35502, #31003, #192486 ) ) ;
#161257 = DIRECTION ( 'NONE',  ( -1.000000000000000000, -0.000000000000000000, -0.000000000000000000 ) ) ;
#161258 = DIRECTION ( 'NONE',  ( 1.186688945009010077E-16, 1.000000000000000000, 6.982962677686266711E-15 ) ) ;
#161259 = EDGE_CURVE ( 'NONE', #95790, #207406, #187237, .T. ) ;
#161260 = DIRECTION ( 'NONE',  ( 1.000000000000000000, 0.000000000000000000, 0.000000000000000000 ) ) ;
#161261 = DIRECTION ( 'NONE',  ( 1.073024830501117725E-15, 6.982962677686266711E-15, -1.000000000000000000 ) ) ;
#161262 = ORIENTED_EDGE ( 'NONE', *, *, #51988, .T. ) ;
#161263 = DIRECTION ( 'NONE',  ( -1.000000000000000000, -0.000000000000000000, -0.000000000000000000 ) ) ;
#161264 = VECTOR ( 'NONE', #173749, 1000.000000000000000 ) ;
#161265 = EDGE_CURVE ( 'NONE', #202658, #248652, #37224, .T. ) ;
#161266 = DIRECTION ( 'NONE',  ( -0.8049926720990042694, -0.5932847527679310229, 0.000000000000000000 ) ) ;
#161267 = AXIS2_PLACEMENT_3D ( 'NONE', #25203, #104677, #166010 ) ;
#161268 = CARTESIAN_POINT ( 'NONE',  ( 18.50000000000000711, 10.37342005529115241, -192.2657881246250042 ) ) ;
#161269 = DIRECTION ( 'NONE',  ( 0.000000000000000000, -1.776356839400277286E-15, -1.000000000000000000 ) ) ;
#161270 = EDGE_CURVE ( 'NONE', #78078, #240241, #252304, .T. ) ;
#161271 = EDGE_CURVE ( 'NONE', #211300, #232157, #28883, .T. ) ;
#161272 = VERTEX_POINT ( 'NONE', #28174 ) ;
#161273 = CIRCLE ( 'NONE', #190513, 0.09999999999998712696 ) ;
#161274 = EDGE_CURVE ( 'NONE', #230526, #70322, #19167, .T. ) ;
#161276 = ORIENTED_EDGE ( 'NONE', *, *, #99233, .T. ) ;
#161275 = CARTESIAN_POINT ( 'NONE',  ( 22.39999999999999503, 55.86476422312858858, -232.8760422647022494 ) ) ;
#161277 = LINE ( 'NONE', #219948, #168354 ) ;
#161278 = DIRECTION ( 'NONE',  ( 0.000000000000000000, 1.000000000000000000, 0.000000000000000000 ) ) ;
#161279 = CARTESIAN_POINT ( 'NONE',  ( -23.15000000000000213, 0.000000000000000000, -33.50000000000000000 ) ) ;
#161280 = CYLINDRICAL_SURFACE ( 'NONE', #217104, 11.80000000000000426 ) ;
#161281 = ADVANCED_FACE ( 'NONE', ( #248475 ), #115749, .T. ) ;
#161282 = VECTOR ( 'NONE', #234548, 1000.000000000000000 ) ;
#161283 = CARTESIAN_POINT ( 'NONE',  ( 21.05000000000000071, 67.25744985290005218, -235.7586130168606076 ) ) ;
#161284 = FACE_OUTER_BOUND ( 'NONE', #171658, .T. ) ;
#161286 = EDGE_LOOP ( 'NONE', ( #149319, #203451, #113641, #50412 ) ) ;
#161285 = AXIS2_PLACEMENT_3D ( 'NONE', #18721, #57825, #56531 ) ;
#161287 = DIRECTION ( 'NONE',  ( 0.000000000000000000, 0.8814952561688476074, -0.4721928772777262417 ) ) ;
#161288 = DIRECTION ( 'NONE',  ( 0.000000000000000000, 0.000000000000000000, -1.000000000000000000 ) ) ;
#161289 = AXIS2_PLACEMENT_3D ( 'NONE', #73070, #108310, #152600 ) ;
#161290 = VECTOR ( 'NONE', #216042, 1000.000000000000000 ) ;
#161292 = EDGE_CURVE ( 'NONE', #82116, #97495, #69857, .T. ) ;
#161291 = CARTESIAN_POINT ( 'NONE',  ( -22.39999999999999858, -1.124859753953710850E-15, 11.64957080754479968 ) ) ;
#161293 = CARTESIAN_POINT ( 'NONE',  ( -20.64999999999999858, 62.33780030268294325, -247.9091949332902232 ) ) ;
#161294 = DIRECTION ( 'NONE',  ( 0.000000000000000000, 0.000000000000000000, 1.000000000000000000 ) ) ;
#161295 = CARTESIAN_POINT ( 'NONE',  ( 20.50589344625198507, 65.51681206853606909, -61.95011250585200457 ) ) ;
#161296 = CIRCLE ( 'NONE', #7335, 0.1000000000000028644 ) ;
#161297 = ORIENTED_EDGE ( 'NONE', *, *, #209001, .F. ) ;
#161298 = EDGE_LOOP ( 'NONE', ( #173997, #219032, #103014, #246117 ) ) ;
#161299 = CARTESIAN_POINT ( 'NONE',  ( -20.94999999999999929, 76.00000000001142553, -36.02310748452432421 ) ) ;
#161300 = DIRECTION ( 'NONE',  ( 0.000000000000000000, 0.9126074666063660468, 0.4088369013363524762 ) ) ;
#161301 = CARTESIAN_POINT ( 'NONE',  ( 21.53699400384038753, 1.197367947672160239E-11, -127.2122882067533709 ) ) ;
#161302 = CARTESIAN_POINT ( 'NONE',  ( 21.05000000000000071, 16.98881331171930498, -224.4946931418895701 ) ) ;
#161303 = EDGE_CURVE ( 'NONE', #57260, #88879, #49677, .T. ) ;
#161304 = ORIENTED_EDGE ( 'NONE', *, *, #75920, .F. ) ;
#161305 = CYLINDRICAL_SURFACE ( 'NONE', #238746, 0.09999999999999939493 ) ;
#161306 = VECTOR ( 'NONE', #7893, 1000.000000000000000 ) ;
#161307 = CARTESIAN_POINT ( 'NONE',  ( -16.98495255085918032, 10.00556436600591681, -113.1346172062205397 ) ) ;
#161308 = AXIS2_PLACEMENT_3D ( 'NONE', #206847, #162597, #141728 ) ;
#161309 = DIRECTION ( 'NONE',  ( 0.000000000000000000, 1.000000000000000000, 0.000000000000000000 ) ) ;
#161310 = PLANE ( 'NONE',  #162062 ) ;
#161311 = CIRCLE ( 'NONE', #115496, 0.09999999999999939493 ) ;
#161312 = ORIENTED_EDGE ( 'NONE', *, *, #168846, .T. ) ;
#161313 = DIRECTION ( 'NONE',  ( 0.000000000000000000, -0.2617529984165046231, -0.9651348961777154178 ) ) ;
#161314 = VERTEX_POINT ( 'NONE', #208082 ) ;
#161315 = CARTESIAN_POINT ( 'NONE',  ( 20.90000000000000213, -1.885425182446133885, -11.49641995933507843 ) ) ;
#161316 = SPHERICAL_SURFACE ( 'NONE', #88080, 0.1000000000000000056 ) ;
#161317 = DIRECTION ( 'NONE',  ( 0.000000000000000000, 0.000000000000000000, 1.000000000000000000 ) ) ;
#161318 = DIRECTION ( 'NONE',  ( 1.000000000000000000, -0.000000000000000000, -0.000000000000000000 ) ) ;
#161319 = DIRECTION ( 'NONE',  ( 0.000000000000000000, 0.2617529984165033463, 0.9651348961777156399 ) ) ;
#161320 = CARTESIAN_POINT ( 'NONE',  ( 20.95595624212427666, 18.87084431528031914, -227.9704499331523664 ) ) ;
#161321 = CYLINDRICAL_SURFACE ( 'NONE', #233064, 11.74999999999999645 ) ;
#161322 = CARTESIAN_POINT ( 'NONE',  ( 21.05000000000000071, -8.999999999988842703, -158.1060308773475640 ) ) ;
#161323 = DIRECTION ( 'NONE',  ( 0.000000000000000000, -0.4999999999999949485, 0.8660254037844415942 ) ) ;
#161324 = ADVANCED_FACE ( 'NONE', ( #51519 ), #62160, .F. ) ;
#161325 = CARTESIAN_POINT ( 'NONE',  ( 23.24999999999999289, 64.35000000001146248, -43.03791325517834565 ) ) ;
#161326 = CYLINDRICAL_SURFACE ( 'NONE', #256394, 0.09999999999999939493 ) ;
#161327 = CARTESIAN_POINT ( 'NONE',  ( -16.27683809663751191, 9.350000000011133849, -42.74999999999997158 ) ) ;
#161328 = VECTOR ( 'NONE', #203276, 1000.000000000000000 ) ;
#161329 = AXIS2_PLACEMENT_3D ( 'NONE', #109265, #188814, #248804 ) ;
#161330 = ADVANCED_FACE ( 'NONE', ( #29466 ), #216255, .T. ) ;
#161331 = VECTOR ( 'NONE', #189303, 1000.000000000000000 ) ;
#161332 = CIRCLE ( 'NONE', #123913, 0.09999999999999939493 ) ;
#161333 = CARTESIAN_POINT ( 'NONE',  ( 22.60000000000000142, 0.1008583691098682150, -122.2504328765106294 ) ) ;
#161334 = CARTESIAN_POINT ( 'NONE',  ( 21.05000000000000071, 56.02567683926420727, -227.9999002286038774 ) ) ;
#161335 = ORIENTED_EDGE ( 'NONE', *, *, #255197, .T. ) ;
#161336 = CARTESIAN_POINT ( 'NONE',  ( 23.24999999999999289, 64.25000000001205080, -124.3731074845243825 ) ) ;
#161338 = EDGE_CURVE ( 'NONE', #178845, #35121, #162126, .T. ) ;
#161337 = DIRECTION ( 'NONE',  ( 0.000000000000000000, 0.000000000000000000, -1.000000000000000000 ) ) ;
#161339 = EDGE_CURVE ( 'NONE', #242581, #2766, #82404, .T. ) ;
#161340 = ORIENTED_EDGE ( 'NONE', *, *, #192803, .F. ) ;
#161341 = EDGE_CURVE ( 'NONE', #81511, #92883, #199552, .T. ) ;
#161342 = CARTESIAN_POINT ( 'NONE',  ( -23.15000000000000213, 73.50000000001223555, -149.7477294072864709 ) ) ;
#161343 = VERTEX_POINT ( 'NONE', #94516 ) ;
#161344 = AXIS2_PLACEMENT_3D ( 'NONE', #227099, #49757, #225800 ) ;
#161345 = CARTESIAN_POINT ( 'NONE',  ( -22.94999999999999929, 1.901609089591594692, -11.59510167572422112 ) ) ;
#161346 = CARTESIAN_POINT ( 'NONE',  ( 18.79999999999999716, -11.65000000000000036, 32.89999999999999858 ) ) ;
#161347 = CIRCLE ( 'NONE', #211404, 0.1000000000000013933 ) ;
#161348 = ORIENTED_EDGE ( 'NONE', *, *, #100583, .F. ) ;
#161349 = EDGE_CURVE ( 'NONE', #251571, #164116, #236592, .T. ) ;
#161350 = AXIS2_PLACEMENT_3D ( 'NONE', #157219, #236706, #141474 ) ;
#161351 = ORIENTED_EDGE ( 'NONE', *, *, #149750, .T. ) ;
#161352 = CARTESIAN_POINT ( 'NONE',  ( -23.15000000000000213, 74.00000000001199396, -115.6477294072864055 ) ) ;
#161353 = ORIENTED_EDGE ( 'NONE', *, *, #82560, .T. ) ;
#161355 =( BOUNDED_CURVE ( )  B_SPLINE_CURVE ( 3, ( #42758, #243521, #66172, #184825 ),
 .UNSPECIFIED., .F., .F. ) 
 B_SPLINE_CURVE_WITH_KNOTS ( ( 4, 4 ),
 ( 4.712388980384689674, 6.231880751915385375 ),
 .UNSPECIFIED. ) 
 CURVE ( )  GEOMETRIC_REPRESENTATION_ITEM ( )  RATIONAL_B_SPLINE_CURVE ( ( 1.000000000000000000, 0.8166740347213230500, 0.8166740347213230500, 1.000000000000000000 ) ) 
 REPRESENTATION_ITEM ( '' )  );
#161354 = DIRECTION ( 'NONE',  ( 1.000000000000000000, -0.000000000000000000, -0.000000000000000000 ) ) ;
#161356 = FACE_OUTER_BOUND ( 'NONE', #152177, .T. ) ;
#161357 = LINE ( 'NONE', #62243, #161867 ) ;
#161358 = FACE_OUTER_BOUND ( 'NONE', #120801, .T. ) ;
#161359 = CARTESIAN_POINT ( 'NONE',  ( -16.87998658237755834, 66.05000000001230376, -157.1594679167859283 ) ) ;
#161360 = CARTESIAN_POINT ( 'NONE',  ( 23.15000000000000213, -11.64999999999999147, 11.75000000000000000 ) ) ;
#161361 = DIRECTION ( 'NONE',  ( -1.000000000000000000, 0.000000000000000000, 0.000000000000000000 ) ) ;
#161362 = DIRECTION ( 'NONE',  ( 0.000000000000000000, -0.8814952561688425003, 0.4721928772777359007 ) ) ;
#161364 = ORIENTED_EDGE ( 'NONE', *, *, #56704, .T. ) ;
#161363 = CARTESIAN_POINT ( 'NONE',  ( -18.51991288638512501, -9.392436789662260921, -40.64326640395893264 ) ) ;
#161365 = ORIENTED_EDGE ( 'NONE', *, *, #131137, .F. ) ;
#161367 = CARTESIAN_POINT ( 'NONE',  ( -23.15000000000000213, 11.75000000001115552, -100.5000000000000284 ) ) ;
#161366 = DIRECTION ( 'NONE',  ( 1.000000000000000000, -0.000000000000000000, -0.000000000000000000 ) ) ;
#161369 = EDGE_LOOP ( 'NONE', ( #172335, #97621, #133179, #137342 ) ) ;
#161368 = CARTESIAN_POINT ( 'NONE',  ( 20.95289811251229750, 8.893168004469750088, -109.0018094939185431 ) ) ;
#161370 = ORIENTED_EDGE ( 'NONE', *, *, #195750, .T. ) ;
#161371 = EDGE_CURVE ( 'NONE', #242736, #77452, #178716, .T. ) ;
#161372 = FACE_OUTER_BOUND ( 'NONE', #146895, .T. ) ;
#161373 = DIRECTION ( 'NONE',  ( 0.000000000000000000, 0.000000000000000000, -1.000000000000000000 ) ) ;
#161374 = CYLINDRICAL_SURFACE ( 'NONE', #29960, 0.1000000000000064587 ) ;
#161375 = CARTESIAN_POINT ( 'NONE',  ( 22.39999999999999503, 64.35000000001213039, -136.4231074845243938 ) ) ;
#161377 = FACE_OUTER_BOUND ( 'NONE', #70394, .T. ) ;
#161376 = VECTOR ( 'NONE', #122146, 1000.000000000000114 ) ;
#161379 = EDGE_CURVE ( 'NONE', #195188, #155038, #103819, .T. ) ;
#161378 = CARTESIAN_POINT ( 'NONE',  ( 23.24999999999999645, 67.17743825834511995, -48.67310748452439384 ) ) ;
#161380 = ADVANCED_FACE ( 'NONE', ( #117936 ), #136187, .F. ) ;
#161382 = AXIS2_PLACEMENT_3D ( 'NONE', #87236, #186370, #224188 ) ;
#161381 = DIRECTION ( 'NONE',  ( 1.000000000000000000, 0.000000000000000000, 0.000000000000000000 ) ) ;
#161383 = ORIENTED_EDGE ( 'NONE', *, *, #199109, .F. ) ;
#161384 = EDGE_LOOP ( 'NONE', ( #37684, #167975, #155934 ) ) ;
#161385 = CARTESIAN_POINT ( 'NONE',  ( -16.27683809663751191, 66.65000000001160174, -56.97310748452439100 ) ) ;
#161386 = TOROIDAL_SURFACE ( 'NONE', #228017, 0.2000000000000000111, 0.1000000000000000056 ) ;
#161387 = AXIS2_PLACEMENT_3D ( 'NONE', #177241, #15602, #100209 ) ;
#161388 = ORIENTED_EDGE ( 'NONE', *, *, #230794, .F. ) ;
#161389 = DIRECTION ( 'NONE',  ( -0.7071067811865127117, -0.7071067811865821007, 0.000000000000000000 ) ) ;
#161390 = ORIENTED_EDGE ( 'NONE', *, *, #208451, .F. ) ;
#161391 = LINE ( 'NONE', #119696, #72464 ) ;
#161392 =( BOUNDED_CURVE ( )  B_SPLINE_CURVE ( 3, ( #190241, #91130, #170721, #27351 ),
 .UNSPECIFIED., .F., .F. ) 
 B_SPLINE_CURVE_WITH_KNOTS ( ( 4, 4 ),
 ( 3.432212674861197854, 3.693332928900581180 ),
 .UNSPECIFIED. ) 
 CURVE ( )  GEOMETRIC_REPRESENTATION_ITEM ( )  RATIONAL_B_SPLINE_CURVE ( ( 1.000000000000000000, 0.9943260843901262636, 0.9943260843901262636, 1.000000000000000000 ) ) 
 REPRESENTATION_ITEM ( '' )  );
#161393 = EDGE_CURVE ( 'NONE', #100823, #238889, #17545, .T. ) ;
#161394 = AXIS2_PLACEMENT_3D ( 'NONE', #207025, #106610, #145747 ) ;
#161395 = DIRECTION ( 'NONE',  ( -0.000000000000000000, 6.982962677686266711E-15, -1.000000000000000000 ) ) ;
#161396 = CIRCLE ( 'NONE', #194734, 0.09999999999999979738 ) ;
#161397 = DIRECTION ( 'NONE',  ( 0.000000000000000000, -1.000000000000000000, 0.000000000000000000 ) ) ;
#161398 = EDGE_CURVE ( 'NONE', #51843, #19120, #137485, .T. ) ;
#161399 = DIRECTION ( 'NONE',  ( 0.000000000000000000, 0.000000000000000000, -1.000000000000000000 ) ) ;
#161400 = VERTEX_POINT ( 'NONE', #116658 ) ;
#161401 = ADVANCED_FACE ( 'NONE', ( #134909 ), #214468, .T. ) ;
#161402 = DIRECTION ( 'NONE',  ( 1.000000000000000000, 7.304098846218133681E-16, 5.100424963727255128E-30 ) ) ;
#161403 = ORIENTED_EDGE ( 'NONE', *, *, #63547, .F. ) ;
#161404 = FACE_OUTER_BOUND ( 'NONE', #48457, .T. ) ;
#161405 = CARTESIAN_POINT ( 'NONE',  ( 20.94999999999999574, 63.48629093094752562, -224.6400281563320505 ) ) ;
#161406 = DIRECTION ( 'NONE',  ( -0.000000000000000000, -0.000000000000000000, -1.000000000000000000 ) ) ;
#161407 = EDGE_CURVE ( 'NONE', #18425, #205739, #41334, .T. ) ;
#161408 = CARTESIAN_POINT ( 'NONE',  ( -23.15000000000000213, 62.82351852614503684, -207.2177435922979214 ) ) ;
#161409 = ORIENTED_EDGE ( 'NONE', *, *, #65173, .F. ) ;
#161410 = CARTESIAN_POINT ( 'NONE',  ( -21.14999999893415250, 64.25000000001189449, -96.17861214099801259 ) ) ;
#161411 = CIRCLE ( 'NONE', #28143, 0.09999999999999939493 ) ;
#161412 = ORIENTED_EDGE ( 'NONE', *, *, #131989, .F. ) ;
#161415 = ORIENTED_EDGE ( 'NONE', *, *, #187421, .F. ) ;
#161414 = DIRECTION ( 'NONE',  ( -1.000000000000000000, -0.000000000000000000, -0.000000000000000000 ) ) ;
#161413 = CARTESIAN_POINT ( 'NONE',  ( 18.58703555224985493, 47.00685966653406922, -255.2225155549824933 ) ) ;
#161416 = FACE_OUTER_BOUND ( 'NONE', #13647, .T. ) ;
#161417 = AXIS2_PLACEMENT_3D ( 'NONE', #86683, #68444, #91851 ) ;
#161418 = ORIENTED_EDGE ( 'NONE', *, *, #235263, .F. ) ;
#161419 = AXIS2_PLACEMENT_3D ( 'NONE', #60108, #40605, #1419 ) ;
#161420 = DIRECTION ( 'NONE',  ( 1.000000000000000000, 0.000000000000000000, -0.000000000000000000 ) ) ;
#161421 = EDGE_LOOP ( 'NONE', ( #79303, #179412, #158206, #121932, #85351, #97932, #236373 ) ) ;
#161423 = AXIS2_PLACEMENT_3D ( 'NONE', #79940, #160828, #116546 ) ;
#161422 = CARTESIAN_POINT ( 'NONE',  ( 18.36493879433253440, 85.50000080620210952, -129.6009588241725226 ) ) ;
#161424 = AXIS2_PLACEMENT_3D ( 'NONE', #41786, #238675, #22215 ) ;
#161425 = EDGE_CURVE ( 'NONE', #65312, #89282, #182969, .T. ) ;
#161426 = CARTESIAN_POINT ( 'NONE',  ( 21.05000000000000071, 40.58313652815218830, -247.7931640254992658 ) ) ;
#161427 = CIRCLE ( 'NONE', #82263, 0.09999999999998898659 ) ;
#161428 = CARTESIAN_POINT ( 'NONE',  ( -21.14999999999994174, 64.25000000001119815, -36.02310748452479316 ) ) ;
#161430 = ORIENTED_EDGE ( 'NONE', *, *, #191068, .T. ) ;
#161429 = SPHERICAL_SURFACE ( 'NONE', #147679, 0.1000000000000000056 ) ;
#161431 = FACE_OUTER_BOUND ( 'NONE', #72034, .T. ) ;
#161432 = ORIENTED_EDGE ( 'NONE', *, *, #21090, .F. ) ;
#161433 = DIRECTION ( 'NONE',  ( 1.186688945009009584E-16, -0.4721928772777346239, -0.8814952561688430555 ) ) ;
#161434 = DIRECTION ( 'NONE',  ( 0.000000000000000000, 0.1568667991644863147, 0.9876197685951252359 ) ) ;
#161435 = CARTESIAN_POINT ( 'NONE',  ( -14.11697426661282506, 66.54258905524487488, -155.0230235107343333 ) ) ;
#161436 = CIRCLE ( 'NONE', #132197, 4.041421356237314022 ) ;
#161437 = VERTEX_POINT ( 'NONE', #95791 ) ;
#161438 = DIRECTION ( 'NONE',  ( 1.000000000000000000, 0.000000000000000000, 0.000000000000000000 ) ) ;
#161439 = ORIENTED_EDGE ( 'NONE', *, *, #231318, .F. ) ;
#161440 = CARTESIAN_POINT ( 'NONE',  ( -20.94999999999999929, 1.115600667400684642E-11, -33.50000000000000000 ) ) ;
#161441 = CYLINDRICAL_SURFACE ( 'NONE', #172355, 0.09999999999999939493 ) ;
#161442 = SPHERICAL_SURFACE ( 'NONE', #43568, 0.1000000000000000056 ) ;
#161444 = ORIENTED_EDGE ( 'NONE', *, *, #127357, .T. ) ;
#161443 = CARTESIAN_POINT ( 'NONE',  ( 18.69999999999999929, 11.75000000000000000, 32.89999999999999858 ) ) ;
#161445 = CARTESIAN_POINT ( 'NONE',  ( 21.05000000000005400, 67.85000000001119247, -25.49719488170504533 ) ) ;
#161446 = DIRECTION ( 'NONE',  ( 0.000000000000000000, -0.5000000000000209832, 0.8660254037844264952 ) ) ;
#161447 = CARTESIAN_POINT ( 'NONE',  ( 18.59999999999999076, 6.450000000011156587, -177.5170271704400022 ) ) ;
#161448 = VECTOR ( 'NONE', #173736, 1000.000000000000000 ) ;
#161449 = ORIENTED_EDGE ( 'NONE', *, *, #181365, .T. ) ;
#161450 = DIRECTION ( 'NONE',  ( 0.000000000000000000, -0.8103668758649578141, 0.5859227990963212784 ) ) ;
#161451 = CARTESIAN_POINT ( 'NONE',  ( -18.40000000000000213, 54.07421472284888608, -229.1714396514910561 ) ) ;
#161452 = ORIENTED_EDGE ( 'NONE', *, *, #10635, .T. ) ;
#161453 = ORIENTED_EDGE ( 'NONE', *, *, #129365, .T. ) ;
#161454 = VECTOR ( 'NONE', #209250, 1000.000000000000114 ) ;
#161455 = FACE_OUTER_BOUND ( 'NONE', #95099, .T. ) ;
#161456 = EDGE_LOOP ( 'NONE', ( #100968, #92797, #65251, #94644 ) ) ;
#161458 = VERTEX_POINT ( 'NONE', #176656 ) ;
#161457 = CARTESIAN_POINT ( 'NONE',  ( -20.94999999999999929, 11.60000000001115161, -107.4282032302755852 ) ) ;
#161459 = EDGE_CURVE ( 'NONE', #17513, #95681, #256103, .T. ) ;
#161460 = CIRCLE ( 'NONE', #253201, 0.4000000000000010214 ) ;
#161463 = VERTEX_POINT ( 'NONE', #254830 ) ;
#161462 = EDGE_LOOP ( 'NONE', ( #64972, #104695, #136765, #244277 ) ) ;
#161461 = CARTESIAN_POINT ( 'NONE',  ( 18.59999999999999432, -1.162701749938009677, -8.099999999999999645 ) ) ;
#161464 = ADVANCED_FACE ( 'NONE', ( #15015 ), #87067, .T. ) ;
#161465 = CARTESIAN_POINT ( 'NONE',  ( -20.90000000000000213, -1.885425182446134107, -11.59641995933507808 ) ) ;
#161467 = EDGE_CURVE ( 'NONE', #121900, #26458, #158066, .T. ) ;
#161466 = AXIS2_PLACEMENT_3D ( 'NONE', #40361, #125001, #119882 ) ;
#161468 = CARTESIAN_POINT ( 'NONE',  ( -21.11927991906891222, 0.009083679485029434036, -161.0515068815084589 ) ) ;
#161469 = CIRCLE ( 'NONE', #144870, 11.74999999999999645 ) ;
#161470 = CARTESIAN_POINT ( 'NONE',  ( 21.05000000000005400, 74.63923853664559260, -43.99645795275012006 ) ) ;
#161471 = CIRCLE ( 'NONE', #86406, 0.09999999999999939493 ) ;
#161473 = CYLINDRICAL_SURFACE ( 'NONE', #233597, 0.09999999999999939493 ) ;
#161472 = CARTESIAN_POINT ( 'NONE',  ( 20.94999027547553894, 46.33166059915855328, -243.0555356998360423 ) ) ;
#161474 = CARTESIAN_POINT ( 'NONE',  ( -2.995603634470829482E-16, 60.85566667783209738, -251.5865162804734041 ) ) ;
#161475 = CARTESIAN_POINT ( 'NONE',  ( -16.92925196614877237, 44.09600274329658021, -235.2921473758737818 ) ) ;
#161476 = AXIS2_PLACEMENT_3D ( 'NONE', #136432, #137728, #119478 ) ;
#161477 = CARTESIAN_POINT ( 'NONE',  ( 23.14999999999999858, 36.65892442174935439, -249.5511627012433848 ) ) ;
#161479 = LINE ( 'NONE', #201865, #230695 ) ;
#161478 = LINE ( 'NONE', #218843, #163555 ) ;
#161480 = ORIENTED_EDGE ( 'NONE', *, *, #28230, .T. ) ;
#161481 = VERTEX_POINT ( 'NONE', #80059 ) ;
#161482 = DIRECTION ( 'NONE',  ( 0.000000000000000000, 0.000000000000000000, -1.000000000000000000 ) ) ;
#161483 = ORIENTED_EDGE ( 'NONE', *, *, #122347, .T. ) ;
#161484 = ORIENTED_EDGE ( 'NONE', *, *, #96471, .F. ) ;
#161485 = EDGE_CURVE ( 'NONE', #188354, #58504, #120449, .T. ) ;
#161486 = CARTESIAN_POINT ( 'NONE',  ( -21.07094088545303734, 6.320167221916481282, 0.09889370255222133810 ) ) ;
#161487 = EDGE_LOOP ( 'NONE', ( #224127, #8837, #160804, #124915 ) ) ;
#161488 = SPHERICAL_SURFACE ( 'NONE', #208695, 0.1000000000000000056 ) ;
#161489 = B_SPLINE_CURVE_WITH_KNOTS ( 'NONE', 3,
 ( #49289, #132694, #11469, #212240, #188801, #127551, #72745, #230508, #152273, #207096, #229228, #50550, #70171 ),
 .UNSPECIFIED., .F., .F.,
 ( 4, 3, 3, 3, 4 ),
 ( -3.224855718277970714E-06, 0.000000000000000000, 6.199515528666914038E-06, 4.034952380127174165E-05, 7.452715123699336041E-05 ),
 .UNSPECIFIED. ) ;
#161490 = VECTOR ( 'NONE', #183146, 1000.000000000000227 ) ;
#161491 = ORIENTED_EDGE ( 'NONE', *, *, #87554, .F. ) ;
#161492 = DIRECTION ( 'NONE',  ( 0.000000000000000000, 0.9126074666063769270, 0.4088369013363280513 ) ) ;
#161493 = CARTESIAN_POINT ( 'NONE',  ( -18.59999999999999787, 66.65000000001180069, -81.67310748452437963 ) ) ;
#161494 = CIRCLE ( 'NONE', #232422, 2.000000000000001776 ) ;
#161496 = ORIENTED_EDGE ( 'NONE', *, *, #250511, .F. ) ;
#161495 = ORIENTED_EDGE ( 'NONE', *, *, #255243, .T. ) ;
#161497 = VERTEX_POINT ( 'NONE', #39724 ) ;
#161498 = DIRECTION ( 'NONE',  ( 0.000000000000000000, 0.7745938767306564943, 0.6324589521315772123 ) ) ;
#161499 = ORIENTED_EDGE ( 'NONE', *, *, #185169, .T. ) ;
#161500 = ORIENTED_EDGE ( 'NONE', *, *, #81811, .F. ) ;
#161501 = VERTEX_POINT ( 'NONE', #215744 ) ;
#161502 = EDGE_CURVE ( 'NONE', #18319, #104084, #133657, .T. ) ;
#161503 = EDGE_CURVE ( 'NONE', #172317, #210574, #197471, .T. ) ;
#161505 = DIRECTION ( 'NONE',  ( 0.000000000000000000, 0.2617529984165031243, 0.9651348961777157509 ) ) ;
#161504 = CARTESIAN_POINT ( 'NONE',  ( -23.15000000000000213, 76.00000000001141132, -33.92310748452431568 ) ) ;
#161506 = CARTESIAN_POINT ( 'NONE',  ( 21.14999999999999858, 1.115600667400684642E-11, -60.45934304829879835 ) ) ;
#161507 = CYLINDRICAL_SURFACE ( 'NONE', #140224, 0.1000000000000028644 ) ;
#161508 = CARTESIAN_POINT ( 'NONE',  ( 21.97500000000000497, 61.02768354592785727, -221.4801322937404677 ) ) ;
#161509 = VERTEX_POINT ( 'NONE', #253589 ) ;
#161510 = B_SPLINE_CURVE_WITH_KNOTS ( 'NONE', 3,
 ( #65122, #144651, #224192, #125121 ),
 .UNSPECIFIED., .F., .F.,
 ( 4, 4 ),
 ( 0.000000000000000000, 0.001767853679387121216 ),
 .UNSPECIFIED. ) ;
#161511 = ORIENTED_EDGE ( 'NONE', *, *, #103927, .T. ) ;
#161512 = DIRECTION ( 'NONE',  ( 1.000000000000000000, 0.000000000000000000, 0.000000000000000000 ) ) ;
#161513 = CARTESIAN_POINT ( 'NONE',  ( -18.50000000000000000, -1.135018845910178431, -41.21697688343231647 ) ) ;
#161514 = FACE_OUTER_BOUND ( 'NONE', #23248, .T. ) ;
#161515 = ADVANCED_FACE ( 'NONE', ( #55363 ), #223449, .F. ) ;
#161516 = VERTEX_POINT ( 'NONE', #81351 ) ;
#161517 = CIRCLE ( 'NONE', #178279, 0.09999999999999939493 ) ;
#161518 = DIRECTION ( 'NONE',  ( 0.000000000000000000, -0.8814952561688437216, 0.4721928772777334582 ) ) ;
#161519 = AXIS2_PLACEMENT_3D ( 'NONE', #50579, #31079, #96127 ) ;
#161520 = DIRECTION ( 'NONE',  ( -1.000000000000000000, -0.000000000000000000, -0.000000000000000000 ) ) ;
#161521 = CARTESIAN_POINT ( 'NONE',  ( 20.94999999999999929, 70.60000000001221565, -146.4170766071768526 ) ) ;
#161522 = ORIENTED_EDGE ( 'NONE', *, *, #142996, .T. ) ;
#161523 = VERTEX_POINT ( 'NONE', #243019 ) ;
#161524 = CARTESIAN_POINT ( 'NONE',  ( 21.00000000000000000, -1.212568896937008089, -8.000000000000000000 ) ) ;
#161525 = FACE_OUTER_BOUND ( 'NONE', #113611, .T. ) ;
#161526 = ORIENTED_EDGE ( 'NONE', *, *, #80765, .F. ) ;
#161527 = DIRECTION ( 'NONE',  ( 1.000000000000000000, 0.000000000000000000, 0.000000000000000000 ) ) ;
#161528 = VERTEX_POINT ( 'NONE', #1828 ) ;
#161529 = DIRECTION ( 'NONE',  ( 1.000000000000000000, -0.000000000000000000, -0.000000000000000000 ) ) ;
#161531 = CARTESIAN_POINT ( 'NONE',  ( -20.94999027547553894, 68.00519115550238780, -224.2294631537215821 ) ) ;
#161530 = CARTESIAN_POINT ( 'NONE',  ( -18.59999999999999787, 66.65000000001222702, -148.7731074845244166 ) ) ;
#161532 = CARTESIAN_POINT ( 'NONE',  ( 18.59999999999999076, 10.20857864377385127, -54.85000000000000142 ) ) ;
#161533 = EDGE_CURVE ( 'NONE', #148669, #146220, #3110, .T. ) ;
#161534 = DIRECTION ( 'NONE',  ( 0.000000000000000000, -0.2128009952263601456, 0.9770955615653316162 ) ) ;
#161535 = AXIS2_PLACEMENT_3D ( 'NONE', #256584, #216215, #255299 ) ;
#161536 = ORIENTED_EDGE ( 'NONE', *, *, #120389, .F. ) ;
#161537 = AXIS2_PLACEMENT_3D ( 'NONE', #195981, #52587, #151731 ) ;
#161538 = CARTESIAN_POINT ( 'NONE',  ( -18.52328366898032996, 85.64232108905291341, -62.80828814695419027 ) ) ;
#161539 = B_SPLINE_CURVE_WITH_KNOTS ( 'NONE', 3,
 ( #29890, #207231, #28633, #229359, #7741, #149829, #148532 ),
 .UNSPECIFIED., .F., .F.,
 ( 4, 3, 4 ),
 ( 0.000000000000000000, 4.520325912680675723E-05, 5.794988040901448781E-05 ),
 .UNSPECIFIED. ) ;
#161541 = VERTEX_POINT ( 'NONE', #64397 ) ;
#161540 = ORIENTED_EDGE ( 'NONE', *, *, #90412, .T. ) ;
#161542 = VECTOR ( 'NONE', #179783, 1000.000000000000114 ) ;
#161543 = VERTEX_POINT ( 'NONE', #100900 ) ;
#161544 = ORIENTED_EDGE ( 'NONE', *, *, #240003, .F. ) ;
#161545 = EDGE_CURVE ( 'NONE', #47477, #60767, #240461, .T. ) ;
#161546 = DIRECTION ( 'NONE',  ( -1.000000000000000000, -0.000000000000000000, -0.000000000000000000 ) ) ;
#161547 = CARTESIAN_POINT ( 'NONE',  ( -18.46856557590794168, -7.745904572654687570, -209.9554418084320560 ) ) ;
#161548 = DIRECTION ( 'NONE',  ( 1.000000000000000000, -7.049440681616512959E-16, 1.911869773728117674E-16 ) ) ;
#161549 = CARTESIAN_POINT ( 'NONE',  ( 20.94999999999999929, 1.360870587203197646, -175.5729979270909382 ) ) ;
#161550 = LINE ( 'NONE', #184940, #88438 ) ;
#161552 = CARTESIAN_POINT ( 'NONE',  ( 20.95595624212415586, 58.97486571184673920, -225.7106661587678218 ) ) ;
#161551 = DIRECTION ( 'NONE',  ( 1.000000000000000000, 0.000000000000000000, -0.000000000000000000 ) ) ;
#161554 = VERTEX_POINT ( 'NONE', #201333 ) ;
#161553 = CARTESIAN_POINT ( 'NONE',  ( 18.48413544395637587, 77.28145018450004500, -241.9425425904620681 ) ) ;
#161555 = CARTESIAN_POINT ( 'NONE',  ( -22.50000000000000000, 11.64957080755595520, -100.4000000000000483 ) ) ;
#161556 = ORIENTED_EDGE ( 'NONE', *, *, #220141, .T. ) ;
#161557 = EDGE_CURVE ( 'NONE', #229500, #230038, #187068, .T. ) ;
#161558 = FACE_OUTER_BOUND ( 'NONE', #17320, .T. ) ;
#161559 = ADVANCED_FACE ( 'NONE', ( #164782 ), #141357, .F. ) ;
#161560 = EDGE_LOOP ( 'NONE', ( #43054, #38760, #70567, #199771, #178597 ) ) ;
#161561 = ORIENTED_EDGE ( 'NONE', *, *, #226448, .F. ) ;
#161562 = DIRECTION ( 'NONE',  ( 1.000000000000000000, -0.000000000000000000, -0.000000000000000000 ) ) ;
#161563 = DIRECTION ( 'NONE',  ( 1.000000000000000000, 0.000000000000000000, 0.000000000000000000 ) ) ;
#161564 = CARTESIAN_POINT ( 'NONE',  ( -21.04999999999998650, 75.90156250001273008, -209.8223383946112222 ) ) ;
#161565 = CARTESIAN_POINT ( 'NONE',  ( 21.05000000000000071, 65.57661458509971908, -196.0310555606543517 ) ) ;
#161566 = AXIS2_PLACEMENT_3D ( 'NONE', #155462, #40654, #38063 ) ;
#161567 = AXIS2_PLACEMENT_3D ( 'NONE', #125517, #225864, #244163 ) ;
#161568 = ADVANCED_FACE ( 'NONE', ( #65667 ), #4406, .T. ) ;
#161569 = LINE ( 'NONE', #221496, #238237 ) ;
#161570 = EDGE_CURVE ( 'NONE', #183490, #69221, #195450, .T. ) ;
#161571 = ORIENTED_EDGE ( 'NONE', *, *, #209204, .T. ) ;
#161572 = EDGE_LOOP ( 'NONE', ( #149626, #257264, #108444, #92559 ) ) ;
#161573 = DIRECTION ( 'NONE',  ( -1.000000000000000000, 1.646408749285563322E-14, -1.073024830501002749E-15 ) ) ;
#161574 = VERTEX_POINT ( 'NONE', #121813 ) ;
#161575 = DIRECTION ( 'NONE',  ( 0.000000000000000000, 0.000000000000000000, 1.000000000000000000 ) ) ;
#161576 = CARTESIAN_POINT ( 'NONE',  ( 23.24999999999999289, 10.80300742114540391, -220.2930047078982625 ) ) ;
#161577 = AXIS2_PLACEMENT_3D ( 'NONE', #123128, #202647, #103535 ) ;
#161579 = EDGE_CURVE ( 'NONE', #59101, #203487, #3892, .T. ) ;
#161578 = DIRECTION ( 'NONE',  ( 0.000000000000000000, 0.000000000000000000, -1.000000000000000000 ) ) ;
#161580 = DIRECTION ( 'NONE',  ( 1.000000000000000000, 0.000000000000000000, 0.000000000000000000 ) ) ;
#161581 = CARTESIAN_POINT ( 'NONE',  ( -16.77828822508139694, 66.05377062509111852, -90.36047923315042851 ) ) ;
#161582 = DIRECTION ( 'NONE',  ( 1.000000000000000000, 0.000000000000000000, 0.000000000000000000 ) ) ;
#161583 = DIRECTION ( 'NONE',  ( 1.000000000000000000, 0.000000000000000000, 0.000000000000000000 ) ) ;
#161584 = DIRECTION ( 'NONE',  ( 0.000000000000000000, 0.2128009952263603122, -0.9770955615653315052 ) ) ;
#161585 = CARTESIAN_POINT ( 'NONE',  ( -21.05000000000000071, 6.093673009697585741, -199.5727803633465385 ) ) ;
#161586 = ADVANCED_FACE ( 'NONE', ( #241741 ), #70560, .T. ) ;
#161587 = CARTESIAN_POINT ( 'NONE',  ( -22.50000000000000000, 11.64957080755595520, -133.9000000000000057 ) ) ;
#161588 = TOROIDAL_SURFACE ( 'NONE', #57482, 0.4000000000000003553, 0.1000000000000000056 ) ;
#161589 = CARTESIAN_POINT ( 'NONE',  ( 21.05000000000000071, 76.00000000001210765, -132.2231074845242631 ) ) ;
#161590 = CIRCLE ( 'NONE', #3506, 11.80000000000000426 ) ;
#161591 = ADVANCED_FACE ( 'NONE', ( #43555, #25283, #21441 ), #222150, .T. ) ;
#161592 = EDGE_CURVE ( 'NONE', #230368, #71963, #58028, .T. ) ;
#161593 = AXIS2_PLACEMENT_3D ( 'NONE', #183476, #243436, #218721 ) ;
#161594 = ORIENTED_EDGE ( 'NONE', *, *, #705, .T. ) ;
#161595 = AXIS2_PLACEMENT_3D ( 'NONE', #29086, #107288, #108580 ) ;
#161596 = ADVANCED_FACE ( 'NONE', ( #120540 ), #200056, .F. ) ;
#161597 = CARTESIAN_POINT ( 'NONE',  ( 20.95325940946048249, 10.52339007070744437, -41.06446212924009131 ) ) ;
#161598 = EDGE_LOOP ( 'NONE', ( #131522, #22028, #185721, #208348 ) ) ;
#161599 = EDGE_CURVE ( 'NONE', #255894, #232658, #142037, .T. ) ;
#161600 = CARTESIAN_POINT ( 'NONE',  ( -18.59999999999999787, 85.50000000001205080, -124.3731074845242262 ) ) ;
#161601 = LINE ( 'NONE', #96440, #81136 ) ;
#161602 = EDGE_CURVE ( 'NONE', #164082, #21483, #115938, .T. ) ;
#161603 = ORIENTED_EDGE ( 'NONE', *, *, #116442, .T. ) ;
#161604 = DIRECTION ( 'NONE',  ( -1.000000000000000000, 0.000000000000000000, -0.000000000000000000 ) ) ;
#161606 = EDGE_CURVE ( 'NONE', #208096, #192900, #243714, .T. ) ;
#161605 = CARTESIAN_POINT ( 'NONE',  ( -20.85000000000000142, 1.115600667400684642E-11, -134.0000000000000284 ) ) ;
#161607 = FACE_OUTER_BOUND ( 'NONE', #203495, .T. ) ;
#161608 = VECTOR ( 'NONE', #25645, 1000.000000000000227 ) ;
#161609 = CARTESIAN_POINT ( 'NONE',  ( -23.15000000000000213, 80.83132476063518368, -153.0534105423255653 ) ) ;
#161610 = TOROIDAL_SURFACE ( 'NONE', #165704, 0.2000000000000000111, 0.1000000000000000056 ) ;
#161611 = PLANE ( 'NONE',  #199443 ) ;
#161612 = CARTESIAN_POINT ( 'NONE',  ( -18.59999999999999787, 9.350000000011156942, -79.25000000000004263 ) ) ;
#161613 = AXIS2_PLACEMENT_3D ( 'NONE', #123652, #201897, #23287 ) ;
#161614 = AXIS2_PLACEMENT_3D ( 'NONE', #241328, #43121, #202190 ) ;
#161615 = ORIENTED_EDGE ( 'NONE', *, *, #92015, .F. ) ;
#161616 = DIRECTION ( 'NONE',  ( -1.000000000000000000, -0.000000000000000000, 0.000000000000000000 ) ) ;
#161618 = VERTEX_POINT ( 'NONE', #161636 ) ;
#161617 = AXIS2_PLACEMENT_3D ( 'NONE', #256902, #168172, #224236 ) ;
#161619 = CARTESIAN_POINT ( 'NONE',  ( -22.94999999999999929, 11.99999999999999822, 12.00000000000000000 ) ) ;
#161620 = DIRECTION ( 'NONE',  ( 1.000000000000000000, 0.000000000000000000, 0.000000000000000000 ) ) ;
#161621 = ADVANCED_FACE ( 'NONE', ( #62516 ), #90790, .T. ) ;
#161622 = AXIS2_PLACEMENT_3D ( 'NONE', #257559, #162389, #219764 ) ;
#161623 = DIRECTION ( 'NONE',  ( -0.000000000000000000, 0.9910465087640865089, 0.1335171055202867274 ) ) ;
#161624 = EDGE_LOOP ( 'NONE', ( #255963, #6355, #188492, #250113, #72751 ) ) ;
#161625 = CARTESIAN_POINT ( 'NONE',  ( -22.39999999999999858, 76.00000000001222134, -148.1726782920690937 ) ) ;
#161626 = EDGE_CURVE ( 'NONE', #52869, #14621, #244993, .T. ) ;
#161627 = SHAPE_DEFINITION_REPRESENTATION ( #137026, #151872 ) ;
#161628 = CARTESIAN_POINT ( 'NONE',  ( -20.85000000000000142, 87.65000000001171543, -69.52310748452423184 ) ) ;
#161629 = EDGE_LOOP ( 'NONE', ( #166109, #222629, #213586, #119455 ) ) ;
#161630 = CIRCLE ( 'NONE', #215748, 7.791421356237338891 ) ;
#161631 = AXIS2_PLACEMENT_3D ( 'NONE', #129516, #109936, #30426 ) ;
#161632 = DIRECTION ( 'NONE',  ( 1.000000000000000000, -0.000000000000000000, 0.000000000000000000 ) ) ;
#161633 = ORIENTED_EDGE ( 'NONE', *, *, #226193, .T. ) ;
#161634 = ORIENTED_EDGE ( 'NONE', *, *, #114124, .T. ) ;
#161635 = CARTESIAN_POINT ( 'NONE',  ( -21.05000000000000071, 87.48912529308871910, -200.4231074845242802 ) ) ;
#161636 = CARTESIAN_POINT ( 'NONE',  ( -18.59999999999999787, 42.20719072976272912, -239.1935934412594804 ) ) ;
#161637 = FACE_OUTER_BOUND ( 'NONE', #248155, .T. ) ;
#161639 = AXIS2_PLACEMENT_3D ( 'NONE', #130088, #72725, #50533 ) ;
#161638 = CARTESIAN_POINT ( 'NONE',  ( -18.50000000000000000, 70.65875701002055109, -146.3297576910123610 ) ) ;
#161640 = CARTESIAN_POINT ( 'NONE',  ( 18.53691006697058796, 10.30215155716188669, -125.2021987172991260 ) ) ;
#161641 = CARTESIAN_POINT ( 'NONE',  ( 12.25000000000000000, 9.850000000011137402, -117.2500000000000284 ) ) ;
#161642 = CIRCLE ( 'NONE', #36754, 0.5000000000000004441 ) ;
#161643 = CARTESIAN_POINT ( 'NONE',  ( 20.95017935633852346, 65.52451072038657287, -95.44566768713390559 ) ) ;
#161644 = ADVANCED_FACE ( 'NONE', ( #241161 ), #48075, .F. ) ;
#161645 = CARTESIAN_POINT ( 'NONE',  ( 21.14999999999999858, 1.115600667400684642E-11, -33.50000000000000000 ) ) ;
#161646 = SPHERICAL_SURFACE ( 'NONE', #181298, 0.1000000000000000056 ) ;
#161647 = DIRECTION ( 'NONE',  ( -0.000000000000000000, 1.000000000000000000, -0.000000000000000000 ) ) ;
#161648 = LINE ( 'NONE', #179921, #168200 ) ;
#161649 = ORIENTED_EDGE ( 'NONE', *, *, #216630, .T. ) ;
#161650 = EDGE_CURVE ( 'NONE', #68241, #137554, #143321, .T. ) ;
#161651 = ORIENTED_EDGE ( 'NONE', *, *, #700, .F. ) ;
#161652 = DIRECTION ( 'NONE',  ( 1.000000000000000000, 0.000000000000000000, 0.000000000000000000 ) ) ;
#161653 = DIRECTION ( 'NONE',  ( -1.000000000000000000, 0.000000000000000000, 0.000000000000000000 ) ) ;
#161655 = DIRECTION ( 'NONE',  ( -1.000000000000000000, -0.000000000000000000, -0.000000000000000000 ) ) ;
#161654 = CARTESIAN_POINT ( 'NONE',  ( 11.60000000000000142, -8.250000000000003553, 15.00000000000000355 ) ) ;
#161656 = AXIS2_PLACEMENT_3D ( 'NONE', #80981, #138380, #18459 ) ;
#161657 = CARTESIAN_POINT ( 'NONE',  ( -23.15000000000000213, 1.910280373842930812, -87.86863214480109718 ) ) ;
#161658 = FACE_OUTER_BOUND ( 'NONE', #23305, .T. ) ;
#161659 = CARTESIAN_POINT ( 'NONE',  ( 21.05000000000000071, 0.000000000000000000, 0.000000000000000000 ) ) ;
#161660 = ORIENTED_EDGE ( 'NONE', *, *, #4860, .F. ) ;
#161661 = AXIS2_PLACEMENT_3D ( 'NONE', #127133, #206675, #8484 ) ;
#161662 = DIRECTION ( 'NONE',  ( 1.000000000000000000, 0.000000000000000000, -0.000000000000000000 ) ) ;
#161663 = ORIENTED_EDGE ( 'NONE', *, *, #17752, .F. ) ;
#161664 = AXIS2_PLACEMENT_3D ( 'NONE', #16614, #58268, #231808 ) ;
#161665 = CARTESIAN_POINT ( 'NONE',  ( -14.22969084473441725, 9.456007326069306274, -18.48863349414676094 ) ) ;
#161666 = VECTOR ( 'NONE', #190457, 1000.000000000000000 ) ;
#161667 = ORIENTED_EDGE ( 'NONE', *, *, #219186, .F. ) ;
#161668 = ADVANCED_FACE ( 'NONE', ( #221553 ), #61760, .F. ) ;
#161669 = AXIS2_PLACEMENT_3D ( 'NONE', #71665, #132916, #151193 ) ;
#161670 = CARTESIAN_POINT ( 'NONE',  ( -20.85000000000000142, 68.97833521811159585, -65.68954208262705663 ) ) ;
#161671 = ORIENTED_EDGE ( 'NONE', *, *, #163691, .F. ) ;
#161672 = FACE_OUTER_BOUND ( 'NONE', #186645, .T. ) ;
#161673 = ORIENTED_EDGE ( 'NONE', *, *, #132873, .T. ) ;
#161674 = CARTESIAN_POINT ( 'NONE',  ( -18.40000000000000213, 64.52683809664929981, -78.84905355133234650 ) ) ;
#161675 = CARTESIAN_POINT ( 'NONE',  ( -22.47007471830798409, 68.27928934808515749, -69.52310748452437394 ) ) ;
#161677 = DIRECTION ( 'NONE',  ( 1.000000000000000000, -0.000000000000000000, -0.000000000000000000 ) ) ;
#161676 = AXIS2_PLACEMENT_3D ( 'NONE', #220356, #219043, #142078 ) ;
#161678 = DIRECTION ( 'NONE',  ( 0.000000000000000000, 0.9371753822965315228, -0.3488585713686134238 ) ) ;
#161679 = SPHERICAL_SURFACE ( 'NONE', #109718, 0.1000000000000000056 ) ;
#161681 = CARTESIAN_POINT ( 'NONE',  ( -20.94999999999999929, 1.115600667400684642E-11, -163.4000000000000341 ) ) ;
#161680 = CARTESIAN_POINT ( 'NONE',  ( -16.89021194854739605, 66.05000000001254534, -182.7805393529200728 ) ) ;
#161682 = DIRECTION ( 'NONE',  ( -3.469446951953515108E-14, 1.000000000000000000, 0.000000000000000000 ) ) ;
#161684 = ORIENTED_EDGE ( 'NONE', *, *, #50005, .T. ) ;
#161683 = CARTESIAN_POINT ( 'NONE',  ( 20.50589344625199217, 65.51681206853655226, -128.9501125058533546 ) ) ;
#161686 = CARTESIAN_POINT ( 'NONE',  ( 21.05000000000000071, 6.540656951712400691, -33.60000000000000142 ) ) ;
#161685 = DIRECTION ( 'NONE',  ( 0.000000000000000000, -1.000000000000000000, 0.000000000000000000 ) ) ;
#161687 = VERTEX_POINT ( 'NONE', #127623 ) ;
#161689 = ORIENTED_EDGE ( 'NONE', *, *, #91321, .T. ) ;
#161688 = DIRECTION ( 'NONE',  ( 0.000000000000000000, -0.1350103645451876666, 0.9908441862701600211 ) ) ;
#161690 = AXIS2_PLACEMENT_3D ( 'NONE', #39180, #157864, #237359 ) ;
#161691 = ORIENTED_EDGE ( 'NONE', *, *, #125347, .T. ) ;
#161692 = DIRECTION ( 'NONE',  ( 1.000000000000000000, -0.000000000000000000, 0.000000000000000000 ) ) ;
#161693 = CARTESIAN_POINT ( 'NONE',  ( 20.94999999999999574, -1.162701749926853712, -108.6000000000000227 ) ) ;
#161694 = CARTESIAN_POINT ( 'NONE',  ( 20.94999999999999929, 76.00000000001213607, -136.5231074845243313 ) ) ;
#161695 = ORIENTED_EDGE ( 'NONE', *, *, #104678, .T. ) ;
#161696 = DIRECTION ( 'NONE',  ( -1.000000000000000000, 7.049440681616512959E-16, -1.911869773728117674E-16 ) ) ;
#161697 = PLANE ( 'NONE',  #243254 ) ;
#161698 = CARTESIAN_POINT ( 'NONE',  ( 22.50000000000000000, 68.20922040163929978, -203.6231074845244109 ) ) ;
#161699 = CARTESIAN_POINT ( 'NONE',  ( -16.86445178670583900, 9.962211629127157408, -154.8907774381173681 ) ) ;
#161700 = EDGE_CURVE ( 'NONE', #132923, #145505, #5067, .T. ) ;
#161701 = LINE ( 'NONE', #178711, #48343 ) ;
#161702 = EDGE_CURVE ( 'NONE', #230341, #236908, #157480, .T. ) ;
#161703 = CARTESIAN_POINT ( 'NONE',  ( 21.11927991906888025, 69.55150688152073712, -136.5321911639982204 ) ) ;
#161704 = TOROIDAL_SURFACE ( 'NONE', #124276, 12.97499999999999787, 0.1000000000000000056 ) ;
#161705 = ORIENTED_EDGE ( 'NONE', *, *, #14697, .F. ) ;
#161707 = ORIENTED_EDGE ( 'NONE', *, *, #203219, .T. ) ;
#161706 = VECTOR ( 'NONE', #223152, 1000.000000000000000 ) ;
#161708 = AXIS2_PLACEMENT_3D ( 'NONE', #65887, #206685, #187143 ) ;
#161709 = CARTESIAN_POINT ( 'NONE',  ( -21.65000000000000213, 9.950000000011138823, -79.75000000000004263 ) ) ;
#161710 = VECTOR ( 'NONE', #198772, 1000.000000000000000 ) ;
#161711 = ORIENTED_EDGE ( 'NONE', *, *, #192029, .F. ) ;
#161712 = DIRECTION ( 'NONE',  ( 0.000000000000000000, 1.000000000000000000, 0.000000000000000000 ) ) ;
#161713 = ORIENTED_EDGE ( 'NONE', *, *, #82807, .F. ) ;
#161714 = FACE_OUTER_BOUND ( 'NONE', #223635, .T. ) ;
#161715 = EDGE_CURVE ( 'NONE', #254127, #72948, #186690, .T. ) ;
#161716 = LINE ( 'NONE', #140849, #235487 ) ;
#161717 = CARTESIAN_POINT ( 'NONE',  ( -23.25000000000000000, 3.558777552609281525, -231.8203201594644725 ) ) ;
#161718 = CARTESIAN_POINT ( 'NONE',  ( 18.39999999999999503, 11.47316190337363828, -87.85000000000003695 ) ) ;
#161719 = EDGE_CURVE ( 'NONE', #43643, #129705, #11714, .T. ) ;
#161720 = CARTESIAN_POINT ( 'NONE',  ( 20.85000000000000142, -1.749999999988843813, -78.61895003862224485 ) ) ;
#161721 = ORIENTED_EDGE ( 'NONE', *, *, #127846, .F. ) ;
#161722 = CARTESIAN_POINT ( 'NONE',  ( 20.94999999999999929, 16.44800918141279666, -240.8068063186265135 ) ) ;
#161723 = VECTOR ( 'NONE', #100918, 1000.000000000000114 ) ;
#161725 = VECTOR ( 'NONE', #13175, 1000.000000000000000 ) ;
#161724 = DIRECTION ( 'NONE',  ( -0.8191520442889921316, 0.5735764363510457153, -0.000000000000000000 ) ) ;
#161726 = EDGE_CURVE ( 'NONE', #10248, #97608, #57469, .T. ) ;
#161727 = LINE ( 'NONE', #117442, #173863 ) ;
#161728 = CARTESIAN_POINT ( 'NONE',  ( 20.85000000000000142, -1.835859311432481045, -112.0044391687985694 ) ) ;
#161729 = ORIENTED_EDGE ( 'NONE', *, *, #252200, .T. ) ;
#161731 = CARTESIAN_POINT ( 'NONE',  ( -21.45000000000000284, 7.708578643762696636, -12.25000000000000000 ) ) ;
#161730 = CARTESIAN_POINT ( 'NONE',  ( 18.59999999999999076, 10.82428752066803845, -220.3907142640547931 ) ) ;
#161732 = VERTEX_POINT ( 'NONE', #104184 ) ;
#161736 = EDGE_LOOP ( 'NONE', ( #248935, #166888, #172718, #175151 ) ) ;
#161735 = LINE ( 'NONE', #199578, #100298 ) ;
#161734 =( BOUNDED_SURFACE ( )  B_SPLINE_SURFACE ( 3, 2, ( 
 ( #101157, #240729, #201586 ),
 ( #22992, #102457, #3375 ),
 ( #82893, #63353, #243272 ),
 ( #222406, #45089, #124633 ),
 ( #204145, #192310, #73668 ),
 ( #250974, #128480, #132322 ),
 ( #129758, #108906, #252261 ),
 ( #13666, #131040, #172785 ),
 ( #68510, #52772, #211885 ),
 ( #210583, #171491, #31970 ),
 ( #51475, #12406, #208035 ),
 ( #247126, #8533, #90616 ) ),
 .UNSPECIFIED., .F., .F., .T. ) 
 B_SPLINE_SURFACE_WITH_KNOTS ( ( 4, 2, 2, 2, 2, 4 ),
 ( 3, 3 ),
 ( 3.174653483277205090, 3.943930578431714018, 4.713207673586222946, 5.482484768740731873, 5.867123316317986337, 6.251761863895240801 ),
 ( 0.000000000000000000, 1.000000000000000000 ),
 .UNSPECIFIED. ) 
 GEOMETRIC_REPRESENTATION_ITEM ( )  RATIONAL_B_SPLINE_SURFACE ( (
 ( 1.000000000000000000, 0.8659465255642401216, 1.000000000000000000),
 ( 1.000000000000000000, 0.8648614068469322458, 1.000000000000000000),
 ( 1.000000000000000000, 0.8489031841349031771, 1.000000000000000000),
 ( 1.000000000000000000, 0.7927507630136544359, 1.000000000000000000),
 ( 1.000000000000000000, 0.7523013858965486023, 1.000000000000000000),
 ( 1.000000000000000000, 0.6616226951240427034, 1.000000000000000000),
 ( 1.000000000000000000, 0.6112214368649029339, 1.000000000000000000),
 ( 1.000000000000000000, 0.5507684314535757908, 1.000000000000000000),
 ( 1.000000000000000000, 0.5333267243109209854, 1.000000000000000000),
 ( 1.000000000000000000, 0.5084565446523154897, 1.000000000000000000),
 ( 1.000000000000000000, 0.5010722703418952761, 1.000000000000000000),
 ( 1.000000000000000000, 0.5001234037138393429, 1.000000000000000000) ) ) 
 REPRESENTATION_ITEM ( '' )  SURFACE ( )  );
#161733 = CARTESIAN_POINT ( 'NONE',  ( 18.49999999999999289, 10.20857864377385127, -58.15000000000000568 ) ) ;
#161737 = EDGE_LOOP ( 'NONE', ( #200591, #22800, #181552, #11342 ) ) ;
#161738 = CIRCLE ( 'NONE', #32753, 0.09999999999999990841 ) ;
#161739 = LINE ( 'NONE', #241265, #51811 ) ;
#161740 = DIRECTION ( 'NONE',  ( 0.000000000000000000, -0.3896596508879864307, -0.9209589331071459384 ) ) ;
#161741 = CYLINDRICAL_SURFACE ( 'NONE', #46039, 0.09999999999999939493 ) ;
#161742 = VERTEX_POINT ( 'NONE', #144594 ) ;
#161743 = CARTESIAN_POINT ( 'NONE',  ( 19.94784844284960101, 16.70146065711004724, -222.6438515326542813 ) ) ;
#161744 = ADVANCED_FACE ( 'NONE', ( #82035 ), #99159, .T. ) ;
#161745 = DIRECTION ( 'NONE',  ( 0.000000000000000000, -0.6728971962617862346, 0.7397360091701815632 ) ) ;
#161747 = CARTESIAN_POINT ( 'NONE',  ( -18.50000000000000000, 66.65000000001198543, -115.1731074845243654 ) ) ;
#161746 = CARTESIAN_POINT ( 'NONE',  ( 21.05000000000000071, -9.499999999988844479, -157.6060308773475640 ) ) ;
#161749 = ORIENTED_EDGE ( 'NONE', *, *, #125621, .F. ) ;
#161748 = CARTESIAN_POINT ( 'NONE',  ( -23.25000000000000000, 76.00000000001212186, -134.4231074845243370 ) ) ;
#161750 = EDGE_LOOP ( 'NONE', ( #64392, #77079, #207963, #144702 ) ) ;
#161751 = VECTOR ( 'NONE', #192657, 1000.000000000000000 ) ;
#161752 = CARTESIAN_POINT ( 'NONE',  ( -18.34804628011471195, 11.47316190337353525, -176.7499999999999716 ) ) ;
#161753 = AXIS2_PLACEMENT_3D ( 'NONE', #240030, #177520, #23586 ) ;
#161754 = CIRCLE ( 'NONE', #32774, 0.9000000000000014655 ) ;
#161755 = DIRECTION ( 'NONE',  ( -0.000000000000000000, -0.4791956752371546169, -0.8777080977375152360 ) ) ;
#161756 = ORIENTED_EDGE ( 'NONE', *, *, #132024, .F. ) ;
#161757 = CARTESIAN_POINT ( 'NONE',  ( -18.50000000000000000, 11.65000000001115232, -45.65000000000000568 ) ) ;
#161758 = EDGE_LOOP ( 'NONE', ( #154133, #134259, #98207, #240898 ) ) ;
#161759 = FACE_OUTER_BOUND ( 'NONE', #128997, .T. ) ;
#161760 = FACE_OUTER_BOUND ( 'NONE', #35570, .T. ) ;
#161761 = DIRECTION ( 'NONE',  ( -1.073024830501117725E-15, 6.982962677686266711E-15, -1.000000000000000000 ) ) ;
#161762 = AXIS2_PLACEMENT_3D ( 'NONE', #92974, #152995, #12188 ) ;
#161763 = ORIENTED_EDGE ( 'NONE', *, *, #61792, .F. ) ;
#161764 = CYLINDRICAL_SURFACE ( 'NONE', #8595, 0.09999999999999939493 ) ;
#161765 = AXIS2_PLACEMENT_3D ( 'NONE', #70670, #11975, #52339 ) ;
#161766 = VECTOR ( 'NONE', #87743, 1000.000000000000000 ) ;
#161767 = CARTESIAN_POINT ( 'NONE',  ( 21.14999999999999858, 64.35000000001258513, -191.3731074845244393 ) ) ;
#161768 = VECTOR ( 'NONE', #232598, 1000.000000000000000 ) ;
#161769 = ADVANCED_FACE ( 'NONE', ( #185022 ), #85889, .T. ) ;
#161770 = ORIENTED_EDGE ( 'NONE', *, *, #70003, .F. ) ;
#161771 = ORIENTED_EDGE ( 'NONE', *, *, #180539, .T. ) ;
#161772 = CIRCLE ( 'NONE', #90809, 11.80000000000000426 ) ;
#161773 = ORIENTED_EDGE ( 'NONE', *, *, #103494, .F. ) ;
#161774 = DIRECTION ( 'NONE',  ( 0.000000000000000000, -1.000000000000000000, -6.982962677686266711E-15 ) ) ;
#161775 = ORIENTED_EDGE ( 'NONE', *, *, #99794, .T. ) ;
#161777 = VERTEX_POINT ( 'NONE', #166780 ) ;
#161776 = CARTESIAN_POINT ( 'NONE',  ( 13.77030915526559340, 66.54399267394325079, -185.0344739903776770 ) ) ;
#161778 = ADVANCED_FACE ( 'NONE', ( #246288 ), #120065, .F. ) ;
#161779 = EDGE_LOOP ( 'NONE', ( #31207, #62556, #169496, #250094 ) ) ;
#161780 = VECTOR ( 'NONE', #118957, 1000.000000000000000 ) ;
#161783 = ORIENTED_EDGE ( 'NONE', *, *, #35076, .T. ) ;
#161782 = ORIENTED_EDGE ( 'NONE', *, *, #43398, .T. ) ;
#161781 = CARTESIAN_POINT ( 'NONE',  ( 18.39999999999999858, 37.99112772578902764, -261.0419300540664835 ) ) ;
#161784 = EDGE_CURVE ( 'NONE', #55132, #54225, #91059, .T. ) ;
#161785 = EDGE_CURVE ( 'NONE', #119397, #3198, #190800, .T. ) ;
#161787 = ORIENTED_EDGE ( 'NONE', *, *, #229810, .T. ) ;
#161786 = AXIS2_PLACEMENT_3D ( 'NONE', #86246, #121590, #203657 ) ;
#161788 = CARTESIAN_POINT ( 'NONE',  ( 20.85000000000000142, 71.99422445362657186, -246.4870034924427671 ) ) ;
#161789 = VECTOR ( 'NONE', #208965, 1000.000000000000000 ) ;
#161790 = DIRECTION ( 'NONE',  ( -0.8191520442889921316, -0.5735764363510457153, 0.000000000000000000 ) ) ;
#161791 = AXIS2_PLACEMENT_3D ( 'NONE', #147497, #47086, #227024 ) ;
#161792 = TOROIDAL_SURFACE ( 'NONE', #99199, 11.89999999999999858, 0.1000000000000000056 ) ;
#161793 = EDGE_LOOP ( 'NONE', ( #158954, #24495, #117234, #252931 ) ) ;
#161794 = VECTOR ( 'NONE', #213338, 1000.000000000000114 ) ;
#161795 = DIRECTION ( 'NONE',  ( -1.000000000000000000, 0.000000000000000000, 0.000000000000000000 ) ) ;
#161797 = ORIENTED_EDGE ( 'NONE', *, *, #221640, .T. ) ;
#161796 = DIRECTION ( 'NONE',  ( 1.000000000000000000, 0.000000000000000000, 0.000000000000000000 ) ) ;
#161798 = LINE ( 'NONE', #199640, #50723 ) ;
#161800 = ORIENTED_EDGE ( 'NONE', *, *, #228588, .F. ) ;
#161799 = DIRECTION ( 'NONE',  ( 0.000000000000000000, -0.9651348961777379554, 0.2617529984164210233 ) ) ;
#161801 = EDGE_CURVE ( 'NONE', #91362, #161574, #224070, .T. ) ;
#161802 = ORIENTED_EDGE ( 'NONE', *, *, #161801, .T. ) ;
#161803 = EDGE_CURVE ( 'NONE', #235224, #181106, #93627, .T. ) ;
#161804 = DIRECTION ( 'NONE',  ( 0.000000000000000000, 1.897661533703519897E-16, -1.000000000000000000 ) ) ;
#161805 = ORIENTED_EDGE ( 'NONE', *, *, #98706, .F. ) ;
#161806 = ORIENTED_EDGE ( 'NONE', *, *, #166621, .F. ) ;
#161807 = CARTESIAN_POINT ( 'NONE',  ( -18.50000000000000000, 74.16465844978787914, -158.4679561919613775 ) ) ;
#161808 = LINE ( 'NONE', #255698, #19641 ) ;
#161809 = CIRCLE ( 'NONE', #145018, 0.09999999999999939493 ) ;
#161810 = TOROIDAL_SURFACE ( 'NONE', #236779, 0.6000000000000009770, 0.1000000000000000056 ) ;
#161812 = ORIENTED_EDGE ( 'NONE', *, *, #204222, .F. ) ;
#161811 = ORIENTED_EDGE ( 'NONE', *, *, #204653, .F. ) ;
#161813 = ORIENTED_EDGE ( 'NONE', *, *, #159153, .F. ) ;
#161814 = CARTESIAN_POINT ( 'NONE',  ( 21.10710606213542206, 61.96450539493646659, -221.7435352673221587 ) ) ;
#161815 = VERTEX_POINT ( 'NONE', #11537 ) ;
#161816 = ORIENTED_EDGE ( 'NONE', *, *, #210086, .T. ) ;
#161817 = ADVANCED_FACE ( 'NONE', ( #251415 ), #213117, .F. ) ;
#161818 = FACE_OUTER_BOUND ( 'NONE', #41738, .T. ) ;
#161820 = VERTEX_POINT ( 'NONE', #29833 ) ;
#161819 = DIRECTION ( 'NONE',  ( 1.000000000000000000, 0.000000000000000000, 0.000000000000000000 ) ) ;
#161821 = EDGE_CURVE ( 'NONE', #5146, #97897, #70245, .T. ) ;
#161822 = CARTESIAN_POINT ( 'NONE',  ( -18.40000000000000213, 19.44861527341281615, -230.3234391047226666 ) ) ;
#161823 = EDGE_CURVE ( 'NONE', #9380, #62433, #252682, .T. ) ;
#161825 = CARTESIAN_POINT ( 'NONE',  ( 18.50000000000000355, -9.421456145484059519, -107.7419820840196252 ) ) ;
#161824 = CYLINDRICAL_SURFACE ( 'NONE', #252971, 0.1000000000000089567 ) ;
#161826 = ORIENTED_EDGE ( 'NONE', *, *, #69419, .F. ) ;
#161827 = VECTOR ( 'NONE', #132028, 1000.000000000000000 ) ;
#161829 = VERTEX_POINT ( 'NONE', #89760 ) ;
#161828 = ORIENTED_EDGE ( 'NONE', *, *, #250214, .F. ) ;
#161830 = DIRECTION ( 'NONE',  ( 1.000000000000000000, 0.000000000000000000, 0.000000000000000000 ) ) ;
#161831 = TOROIDAL_SURFACE ( 'NONE', #82652, 0.2000000000000000111, 0.1000000000000000056 ) ;
#161832 = ORIENTED_EDGE ( 'NONE', *, *, #159279, .T. ) ;
#161833 = AXIS2_PLACEMENT_3D ( 'NONE', #70467, #110828, #190395 ) ;
#161834 = DIRECTION ( 'NONE',  ( 0.000000000000000000, 0.5341055959866798375, -0.8454177738465836756 ) ) ;
#161835 = VERTEX_POINT ( 'NONE', #74099 ) ;
#161836 = ADVANCED_FACE ( 'NONE', ( #149775 ), #36863, .T. ) ;
#161837 = VERTEX_POINT ( 'NONE', #230581 ) ;
#161838 = CARTESIAN_POINT ( 'NONE',  ( 23.14999999999999503, 11.65000000001116298, -59.98519422934606382 ) ) ;
#161839 = ORIENTED_EDGE ( 'NONE', *, *, #98082, .T. ) ;
#161840 = DIRECTION ( 'NONE',  ( 0.000000000000000000, 0.9887567792719341719, -0.1495327102803664099 ) ) ;
#161841 = CARTESIAN_POINT ( 'NONE',  ( 21.05000000000000426, 75.96513199699892027, -109.2931933482134355 ) ) ;
#161842 = ORIENTED_EDGE ( 'NONE', *, *, #106496, .F. ) ;
#161843 = DIRECTION ( 'NONE',  ( 1.000000000000000000, 0.000000000000000000, 0.000000000000000000 ) ) ;
#161844 = FACE_OUTER_BOUND ( 'NONE', #237218, .T. ) ;
#161846 = CARTESIAN_POINT ( 'NONE',  ( -23.49999999999994316, 76.00000000001119815, -36.02310748452479316 ) ) ;
#161845 = DIRECTION ( 'NONE',  ( 1.000000000000000000, 1.541880601228652843E-16, 2.878400969107353907E-16 ) ) ;
#161847 = CARTESIAN_POINT ( 'NONE',  ( -18.59999999999999787, 47.93499546395150190, -254.9093547331817717 ) ) ;
#161849 = CIRCLE ( 'NONE', #232585, 0.1000000000000052097 ) ;
#161848 = CARTESIAN_POINT ( 'NONE',  ( 23.15000000000000213, 87.65000000001246860, -173.0231074845243029 ) ) ;
#161850 = AXIS2_PLACEMENT_3D ( 'NONE', #207761, #190778, #108637 ) ;
#161851 = DIRECTION ( 'NONE',  ( -0.7071067811865462405, 0.6909108974501249056, 0.1504730267678058564 ) ) ;
#161852 = ADVANCED_FACE ( 'NONE', ( #51904 ), #28572, .T. ) ;
#161853 = DIRECTION ( 'NONE',  ( 0.000000000000000000, 0.5000000000000209832, 0.8660254037844264952 ) ) ;
#161855 = SPHERICAL_SURFACE ( 'NONE', #143256, 0.1000000000000000056 ) ;
#161854 = VECTOR ( 'NONE', #160320, 1000.000000000000114 ) ;
#161856 = ORIENTED_EDGE ( 'NONE', *, *, #72842, .T. ) ;
#161858 = ORIENTED_EDGE ( 'NONE', *, *, #101570, .T. ) ;
#161857 = ORIENTED_EDGE ( 'NONE', *, *, #21957, .F. ) ;
#161859 = EDGE_LOOP ( 'NONE', ( #166091, #46483, #85928, #88165 ) ) ;
#161860 = EDGE_CURVE ( 'NONE', #205806, #156025, #32583, .T. ) ;
#161861 = DIRECTION ( 'NONE',  ( 0.000000000000000000, 0.1495327102803792052, 0.9887567792719320625 ) ) ;
#161862 = CARTESIAN_POINT ( 'NONE',  ( 18.49999999999999645, 5.950000000011100632, -43.80570230503486329 ) ) ;
#161864 = CARTESIAN_POINT ( 'NONE',  ( -15.75000000000000355, 9.349999999999983658, -16.75000000000000355 ) ) ;
#161863 = CARTESIAN_POINT ( 'NONE',  ( 21.97500000000000497, 9.750000000011153745, -121.7500000000000426 ) ) ;
#161865 = CARTESIAN_POINT ( 'NONE',  ( -21.12757541349819590, 75.99483878420245730, -142.9964880557758704 ) ) ;
#161866 = ORIENTED_EDGE ( 'NONE', *, *, #31208, .F. ) ;
#161867 = VECTOR ( 'NONE', #235732, 999.9999999999998863 ) ;
#161868 = EDGE_CURVE ( 'NONE', #168114, #227236, #53389, .T. ) ;
#161869 = CARTESIAN_POINT ( 'NONE',  ( -20.89878130938411616, 10.32747123227773045, -106.0774032850249711 ) ) ;
#161870 = DIRECTION ( 'NONE',  ( 0.000000000000000000, -0.9876197685951252359, -0.1568667991644863424 ) ) ;
#161871 = DIRECTION ( 'NONE',  ( 1.000000000000000000, -0.000000000000000000, -0.000000000000000000 ) ) ;
#161872 = EDGE_CURVE ( 'NONE', #145080, #178265, #211622, .T. ) ;
#161873 = CARTESIAN_POINT ( 'NONE',  ( 21.05000000000000071, -11.29603075032412995, -103.5478991596638991 ) ) ;
#161874 = ORIENTED_EDGE ( 'NONE', *, *, #107151, .T. ) ;
#161875 = LINE ( 'NONE', #43195, #255431 ) ;
#161876 = EDGE_CURVE ( 'NONE', #171099, #108499, #117046, .T. ) ;
#161877 = CARTESIAN_POINT ( 'NONE',  ( -21.05000000000000071, 1.115526128501326264E-11, -93.95934304829879125 ) ) ;
#161878 = EDGE_CURVE ( 'NONE', #2383, #109875, #80434, .T. ) ;
#161879 = ORIENTED_EDGE ( 'NONE', *, *, #33281, .F. ) ;
#161880 = DIRECTION ( 'NONE',  ( -1.000000000000000000, -0.000000000000000000, -0.000000000000000000 ) ) ;
#161881 = CARTESIAN_POINT ( 'NONE',  ( 21.05000000000000071, 76.00000000001190870, -103.0231074845243029 ) ) ;
#161882 = CYLINDRICAL_SURFACE ( 'NONE', #193509, 11.80000000000000426 ) ;
#161883 = DIRECTION ( 'NONE',  ( 0.000000000000000000, 0.000000000000000000, 1.000000000000000000 ) ) ;
#161884 = DIRECTION ( 'NONE',  ( 1.000000000000000000, 0.000000000000000000, -0.000000000000000000 ) ) ;
#161885 = ORIENTED_EDGE ( 'NONE', *, *, #192417, .T. ) ;
#161886 = CARTESIAN_POINT ( 'NONE',  ( -21.00000000000000000, 6.223900101154156594, 12.00000000000000000 ) ) ;
#161887 = DIRECTION ( 'NONE',  ( -1.000000000000000000, -1.541880601228652843E-16, -2.878400969107353907E-16 ) ) ;
#161888 = CARTESIAN_POINT ( 'NONE',  ( -21.05000000000000071, 1.115600667400684642E-11, -67.00000000000004263 ) ) ;
#161890 = DIRECTION ( 'NONE',  ( 1.000000000000000000, 0.000000000000000000, 0.000000000000000000 ) ) ;
#161889 = CARTESIAN_POINT ( 'NONE',  ( 20.94999999999999929, 76.00000000001213607, -136.5231074845242745 ) ) ;
#161891 = CARTESIAN_POINT ( 'NONE',  ( -18.59999999999999787, 85.48068669529138219, -163.0819923157664562 ) ) ;
#161892 = FACE_OUTER_BOUND ( 'NONE', #254693, .T. ) ;
#161893 = CIRCLE ( 'NONE', #16138, 0.1000000000000072220 ) ;
#161894 = VECTOR ( 'NONE', #35774, 1000.000000000000000 ) ;
#161895 = DIRECTION ( 'NONE',  ( 1.000000000000000000, 0.000000000000000000, 0.000000000000000000 ) ) ;
#161896 = TOROIDAL_SURFACE ( 'NONE', #124466, 0.6000000000000013101, 0.1000000000000000056 ) ;
#161898 = ORIENTED_EDGE ( 'NONE', *, *, #62538, .F. ) ;
#161897 = CARTESIAN_POINT ( 'NONE',  ( -18.44085059012131822, 11.51401249349495437, -143.2596946808784821 ) ) ;
#161899 = ADVANCED_FACE ( 'NONE', ( #137865 ), #238259, .F. ) ;
#161900 = EDGE_CURVE ( 'NONE', #227765, #68874, #20080, .T. ) ;
#161901 = ORIENTED_EDGE ( 'NONE', *, *, #60149, .T. ) ;
#161902 = AXIS2_PLACEMENT_3D ( 'NONE', #116648, #197460, #95782 ) ;
#161903 = ADVANCED_FACE ( 'NONE', ( #196567 ), #20527, .F. ) ;
#161904 = DIRECTION ( 'NONE',  ( -1.000000000000000000, 0.000000000000000000, -0.000000000000000000 ) ) ;
#161905 = AXIS2_PLACEMENT_3D ( 'NONE', #79932, #27744, #90222 ) ;
#161906 = AXIS2_PLACEMENT_3D ( 'NONE', #50846, #211234, #113419 ) ;
#161908 = AXIS2_PLACEMENT_3D ( 'NONE', #173269, #154963, #190220 ) ;
#161907 = CARTESIAN_POINT ( 'NONE',  ( -18.50000324121759121, 65.70692517833182933, -30.56446533783035946 ) ) ;
#161909 = ADVANCED_FACE ( 'NONE', ( #60903, #136583 ), #38794, .T. ) ;
#161910 = CARTESIAN_POINT ( 'NONE',  ( 13.76927104934457802, 9.455987233623899257, -149.0115311668978677 ) ) ;
#161911 = ORIENTED_EDGE ( 'NONE', *, *, #53342, .T. ) ;
#161912 = DIRECTION ( 'NONE',  ( 0.000000000000000000, 0.000000000000000000, -1.000000000000000000 ) ) ;
#161913 = CARTESIAN_POINT ( 'NONE',  ( 20.85000000000000142, 0.1610488207298751417, -200.7158101556397582 ) ) ;
#161914 = EDGE_CURVE ( 'NONE', #80617, #235459, #17926, .T. ) ;
#161915 = ORIENTED_EDGE ( 'NONE', *, *, #100580, .T. ) ;
#161916 = DIRECTION ( 'NONE',  ( 0.000000000000000000, -6.652207440891569552E-15, 1.000000000000000000 ) ) ;
#161917 = EDGE_LOOP ( 'NONE', ( #79132, #37947, #139630, #89754 ) ) ;
#161919 = CARTESIAN_POINT ( 'NONE',  ( -16.91256925476569961, 9.985731158139333985, -154.9676424890052999 ) ) ;
#161918 = CARTESIAN_POINT ( 'NONE',  ( -16.94445028196808778, 9.992063609708889516, -146.6073301784184935 ) ) ;
#161920 = CARTESIAN_POINT ( 'NONE',  ( 20.12481660106788439, 66.47365600773738947, -161.7969658154282229 ) ) ;
#161921 = CARTESIAN_POINT ( 'NONE',  ( -18.59999999999999787, 1.162701749938009677, -8.000000000000000000 ) ) ;
#161922 = VERTEX_POINT ( 'NONE', #77899 ) ;
#161923 = EDGE_CURVE ( 'NONE', #182666, #113374, #103258, .T. ) ;
#161924 = DIRECTION ( 'NONE',  ( 0.000000000000000000, 0.000000000000000000, 1.000000000000000000 ) ) ;
#161925 = DIRECTION ( 'NONE',  ( -1.000000000000000000, 0.000000000000000000, 0.000000000000000000 ) ) ;
#161926 = CARTESIAN_POINT ( 'NONE',  ( -21.65000000000000213, 68.29142135624910281, -81.77310748452435973 ) ) ;
#161927 = ORIENTED_EDGE ( 'NONE', *, *, #126351, .F. ) ;
#161928 = DIRECTION ( 'NONE',  ( 0.000000000000000000, 0.8814952561688432775, -0.4721928772777344019 ) ) ;
#161929 = AXIS2_PLACEMENT_3D ( 'NONE', #191078, #249744, #188479 ) ;
#161930 = CIRCLE ( 'NONE', #124501, 11.65000000000000924 ) ;
#161931 = CIRCLE ( 'NONE', #3671, 0.2000000000000057288 ) ;
#161932 = CARTESIAN_POINT ( 'NONE',  ( -22.50000000000000000, -1.330006220153263641, -194.8931527402181700 ) ) ;
#161933 = DIRECTION ( 'NONE',  ( 0.000000000000000000, 0.000000000000000000, -1.000000000000000000 ) ) ;
#161934 = EDGE_CURVE ( 'NONE', #72090, #206303, #136577, .T. ) ;
#161935 = EDGE_LOOP ( 'NONE', ( #185858, #217069, #138485, #157180 ) ) ;
#161936 = VECTOR ( 'NONE', #88797, 1000.000000000000000 ) ;
#161937 = ORIENTED_EDGE ( 'NONE', *, *, #251511, .T. ) ;
#161938 = PLANE ( 'NONE',  #11368 ) ;
#161939 = CARTESIAN_POINT ( 'NONE',  ( 23.24999999999999645, 14.17280543801757986, -210.8598471598932633 ) ) ;
#161940 = DIRECTION ( 'NONE',  ( 0.000000000000000000, 0.000000000000000000, -1.000000000000000000 ) ) ;
#161941 = DIRECTION ( 'NONE',  ( 0.000000000000000000, 0.8660254037844352659, -0.5000000000000058842 ) ) ;
#161943 = DIRECTION ( 'NONE',  ( 1.000000000000000000, -0.000000000000000000, -0.000000000000000000 ) ) ;
#161942 = CARTESIAN_POINT ( 'NONE',  ( -16.85312841634288361, 12.43107187334904395, -211.4921453644653866 ) ) ;
#161944 = CIRCLE ( 'NONE', #241046, 0.9750000000000036415 ) ;
#161946 = CARTESIAN_POINT ( 'NONE',  ( -18.59999999999999787, -9.480686695278977894, -40.44111516875783963 ) ) ;
#161945 = TOROIDAL_SURFACE ( 'NONE', #191169, 11.65000000000000036, 0.1000000000000000056 ) ;
#161947 = LINE ( 'NONE', #61546, #139371 ) ;
#161948 = FACE_OUTER_BOUND ( 'NONE', #232413, .T. ) ;
#161949 = CIRCLE ( 'NONE', #49502, 0.3999999999999975797 ) ;
#161950 = ORIENTED_EDGE ( 'NONE', *, *, #61470, .T. ) ;
#161951 = FACE_OUTER_BOUND ( 'NONE', #108622, .T. ) ;
#161953 = ORIENTED_EDGE ( 'NONE', *, *, #160406, .T. ) ;
#161952 = CARTESIAN_POINT ( 'NONE',  ( 20.94999999999999929, 8.776282895303632259, -188.7499999999999716 ) ) ;
#161954 = CARTESIAN_POINT ( 'NONE',  ( 23.14999999999999503, 64.35000000001150511, -48.17310748452440095 ) ) ;
#161955 = AXIS2_PLACEMENT_3D ( 'NONE', #218366, #15397, #174516 ) ;
#161956 = CARTESIAN_POINT ( 'NONE',  ( 21.30000000000002558, 1.115600667400684642E-11, -134.0000000000000000 ) ) ;
#161958 = FACE_OUTER_BOUND ( 'NONE', #166186, .T. ) ;
#161957 = LINE ( 'NONE', #121559, #192676 ) ;
#161959 = EDGE_CURVE ( 'NONE', #60391, #180491, #34979, .T. ) ;
#161960 = ORIENTED_EDGE ( 'NONE', *, *, #2633, .T. ) ;
#161962 = CARTESIAN_POINT ( 'NONE',  ( 20.94999999999999929, 23.49882452903949570, -253.1653563615082305 ) ) ;
#161961 = CARTESIAN_POINT ( 'NONE',  ( -16.77308656112215601, 66.05000000001157900, -56.87291429282210942 ) ) ;
#161963 = CARTESIAN_POINT ( 'NONE',  ( -16.77683809663752257, 66.05000000001201954, -115.6731074845243796 ) ) ;
#161964 = CARTESIAN_POINT ( 'NONE',  ( 21.08489834409762054, 65.37767610527653517, -124.1731074845243512 ) ) ;
#161965 = CARTESIAN_POINT ( 'NONE',  ( 20.09999999999999787, 19.88654501311280498, -229.5059066796121101 ) ) ;
#161966 = CARTESIAN_POINT ( 'NONE',  ( -20.54999999999999716, -6.794814075650357665, -212.0940144922642219 ) ) ;
#161967 = ORIENTED_EDGE ( 'NONE', *, *, #224347, .T. ) ;
#161968 = AXIS2_PLACEMENT_3D ( 'NONE', #253544, #115324, #16262 ) ;
#161969 = VECTOR ( 'NONE', #217714, 1000.000000000000000 ) ;
#161970 = VERTEX_POINT ( 'NONE', #194034 ) ;
#161971 = B_SPLINE_CURVE_WITH_KNOTS ( 'NONE', 3,
 ( #61888, #119296, #240522, #58005, #102252, #60583, #181834, #76293, #237943, #215799, #155876, #197532, #218365 ),
 .UNSPECIFIED., .F., .F.,
 ( 4, 3, 3, 3, 4 ),
 ( 1.084999851846394431E-16, 1.946463881814436062E-05, 3.922356109943672979E-05, 4.215060953238128886E-05, 4.415117091092174526E-05 ),
 .UNSPECIFIED. ) ;
#161972 = LINE ( 'NONE', #103235, #71942 ) ;
#161973 = VECTOR ( 'NONE', #246325, 1000.000000000000114 ) ;
#161974 = ORIENTED_EDGE ( 'NONE', *, *, #22865, .T. ) ;
#161975 = EDGE_CURVE ( 'NONE', #205348, #110564, #19222, .T. ) ;
#161976 = SPHERICAL_SURFACE ( 'NONE', #51350, 0.1000000000000000056 ) ;
#161977 = ORIENTED_EDGE ( 'NONE', *, *, #68268, .T. ) ;
#161978 = B_SPLINE_CURVE_WITH_KNOTS ( 'NONE', 3,
 ( #136950, #152704, #157848, #251766, #15760, #134365, #213925, #35329, #191828, #97795 ),
 .UNSPECIFIED., .F., .F.,
 ( 4, 3, 3, 4 ),
 ( 3.103167691559091397E-17, 0.0002000000000008536833, 0.001000000000082982687, 0.001967863649483335420 ),
 .UNSPECIFIED. ) ;
#161979 = VECTOR ( 'NONE', #130404, 1000.000000000000000 ) ;
#161980 = DIRECTION ( 'NONE',  ( 0.000000000000000000, 0.000000000000000000, -1.000000000000000000 ) ) ;
#161981 = CIRCLE ( 'NONE', #161791, 0.1000000000000075273 ) ;
#161982 = AXIS2_PLACEMENT_3D ( 'NONE', #200648, #122394, #221461 ) ;
#161983 = AXIS2_PLACEMENT_3D ( 'NONE', #230784, #168269, #172120 ) ;
#161984 = DIRECTION ( 'NONE',  ( 1.000000000000000000, 0.000000000000000000, -0.000000000000000000 ) ) ;
#161985 = EDGE_LOOP ( 'NONE', ( #190622, #133013, #107765, #173582 ) ) ;
#161986 = VECTOR ( 'NONE', #25201, 1000.000000000000000 ) ;
#161987 = CARTESIAN_POINT ( 'NONE',  ( -16.79140778683509438, 9.944941598865721488, -87.82973723377084241 ) ) ;
#161988 = DIRECTION ( 'NONE',  ( 0.000000000000000000, 0.000000000000000000, 1.000000000000000000 ) ) ;
#161989 = CARTESIAN_POINT ( 'NONE',  ( 21.02374657821588855, 11.60000000083178406, -160.5717967701983184 ) ) ;
#161990 = CYLINDRICAL_SURFACE ( 'NONE', #162139, 0.1000000000000012546 ) ;
#161991 = FACE_OUTER_BOUND ( 'NONE', #190942, .T. ) ;
#161992 = DIRECTION ( 'NONE',  ( -0.000000000000000000, 0.000000000000000000, -1.000000000000000000 ) ) ;
#161993 = LINE ( 'NONE', #257157, #244560 ) ;
#161994 = ORIENTED_EDGE ( 'NONE', *, *, #42561, .T. ) ;
#161997 = CARTESIAN_POINT ( 'NONE',  ( -20.85000000000000142, 67.23127455305835554, -235.8551265064784559 ) ) ;
#161996 = AXIS2_PLACEMENT_3D ( 'NONE', #55244, #250897, #210506 ) ;
#161995 = DIRECTION ( 'NONE',  ( 0.000000000000000000, 0.000000000000000000, 1.000000000000000000 ) ) ;
#161998 = ORIENTED_EDGE ( 'NONE', *, *, #243685, .T. ) ;
#161999 = VERTEX_POINT ( 'NONE', #37517 ) ;
#162000 = ORIENTED_EDGE ( 'NONE', *, *, #110446, .T. ) ;
#162001 = CARTESIAN_POINT ( 'NONE',  ( -21.65000000000000213, 9.950000000011140600, -79.65000000000004832 ) ) ;
#162002 = DIRECTION ( 'NONE',  ( 1.000000000000000000, -0.000000000000000000, -0.000000000000000000 ) ) ;
#162003 = CARTESIAN_POINT ( 'NONE',  ( -23.25000000000000000, 74.00000000001151079, -49.24772940728643533 ) ) ;
#162004 = DIRECTION ( 'NONE',  ( 0.7071067811865474617, 0.7071067811865474617, -0.000000000000000000 ) ) ;
#162005 = VERTEX_POINT ( 'NONE', #114471 ) ;
#162006 = LINE ( 'NONE', #5447, #113914 ) ;
#162007 = CARTESIAN_POINT ( 'NONE',  ( 23.14999999999999503, 69.45000000001199680, -115.2731074845243455 ) ) ;
#162008 = AXIS2_PLACEMENT_3D ( 'NONE', #141683, #120879, #180830 ) ;
#162009 = VERTEX_POINT ( 'NONE', #119622 ) ;
#162010 = EDGE_CURVE ( 'NONE', #188452, #132235, #75375, .T. ) ;
#162011 = VECTOR ( 'NONE', #187992, 1000.000000000000000 ) ;
#162012 = DIRECTION ( 'NONE',  ( 1.000000000000000000, 0.000000000000000000, 0.000000000000000000 ) ) ;
#162013 = VECTOR ( 'NONE', #167759, 1000.000000000000000 ) ;
#162014 = DIRECTION ( 'NONE',  ( 0.000000000000000000, 0.000000000000000000, 1.000000000000000000 ) ) ;
#162015 = EDGE_LOOP ( 'NONE', ( #114193, #168867, #117564, #169721 ) ) ;
#162016 = DIRECTION ( 'NONE',  ( -1.836970198721029441E-16, 0.4721928772777346239, 0.8814952561688430555 ) ) ;
#162017 = VECTOR ( 'NONE', #59168, 1000.000000000000000 ) ;
#162018 = DIRECTION ( 'NONE',  ( 0.000000000000000000, 0.9651348961777157509, -0.2617529984165031243 ) ) ;
#162019 = ORIENTED_EDGE ( 'NONE', *, *, #63237, .T. ) ;
#162020 = DIRECTION ( 'NONE',  ( 0.000000000000000000, -0.2617529984165031243, -0.9651348961777157509 ) ) ;
#162021 = EDGE_CURVE ( 'NONE', #225961, #117247, #128407, .T. ) ;
#162022 = DIRECTION ( 'NONE',  ( 0.000000000000000000, 0.000000000000000000, -1.000000000000000000 ) ) ;
#162023 = FACE_OUTER_BOUND ( 'NONE', #15577, .T. ) ;
#162024 = EDGE_CURVE ( 'NONE', #221, #166775, #161754, .T. ) ;
#162025 = DIRECTION ( 'NONE',  ( 1.000000000000000000, -3.265361837132813093E-16, -2.280189983783949500E-30 ) ) ;
#162026 = CIRCLE ( 'NONE', #241135, 0.09999999999998900047 ) ;
#162027 = AXIS2_PLACEMENT_3D ( 'NONE', #79924, #4265, #163365 ) ;
#162028 = EDGE_CURVE ( 'NONE', #40334, #108241, #175753, .T. ) ;
#162029 = CYLINDRICAL_SURFACE ( 'NONE', #170821, 0.1000000000000024342 ) ;
#162030 = SPHERICAL_SURFACE ( 'NONE', #122404, 0.1000000000000000056 ) ;
#162032 = CARTESIAN_POINT ( 'NONE',  ( 20.94999999999999574, 74.83729825007462466, -195.4231074845243654 ) ) ;
#162031 = AXIS2_PLACEMENT_3D ( 'NONE', #244111, #167192, #229704 ) ;
#162033 = EDGE_LOOP ( 'NONE', ( #124338, #217252, #218084, #190223, #155062, #157780, #250425 ) ) ;
#162035 = DIRECTION ( 'NONE',  ( 0.000000000000000000, -0.9651348961777379554, 0.2617529984164210233 ) ) ;
#162034 = CARTESIAN_POINT ( 'NONE',  ( -20.00857864376270001, 66.75000000001223555, -148.7731074845244166 ) ) ;
#162036 = VERTEX_POINT ( 'NONE', #236993 ) ;
#162037 = CARTESIAN_POINT ( 'NONE',  ( -21.05000000000000071, 74.75000000001159606, -61.52310748452433131 ) ) ;
#162038 = DIRECTION ( 'NONE',  ( 0.000000000000000000, 0.000000000000000000, 1.000000000000000000 ) ) ;
#162040 = ORIENTED_EDGE ( 'NONE', *, *, #174223, .F. ) ;
#162039 = CARTESIAN_POINT ( 'NONE',  ( 20.94999999999999574, -1.162701749926853712, -142.1000000000000227 ) ) ;
#162042 = ORIENTED_EDGE ( 'NONE', *, *, #49583, .F. ) ;
#162041 = FACE_OUTER_BOUND ( 'NONE', #143685, .T. ) ;
#162043 = EDGE_CURVE ( 'NONE', #89644, #102088, #217404, .T. ) ;
#162044 = DIRECTION ( 'NONE',  ( 1.000000000000000000, -0.000000000000000000, -0.000000000000000000 ) ) ;
#162045 = DIRECTION ( 'NONE',  ( -1.000000000000000000, 0.000000000000000000, 0.000000000000000000 ) ) ;
#162046 = CARTESIAN_POINT ( 'NONE',  ( -21.59142135623730852, 7.850000000000003197, -12.25000000000000000 ) ) ;
#162048 = ORIENTED_EDGE ( 'NONE', *, *, #245877, .F. ) ;
#162047 = DIRECTION ( 'NONE',  ( -1.000000000000000000, 0.000000000000000000, -0.000000000000000000 ) ) ;
#162049 = EDGE_CURVE ( 'NONE', #21483, #33839, #20269, .T. ) ;
#162050 = LINE ( 'NONE', #62929, #84897 ) ;
#162051 = EDGE_LOOP ( 'NONE', ( #28392, #186454, #76087, #62811 ) ) ;
#162052 = ORIENTED_EDGE ( 'NONE', *, *, #32872, .T. ) ;
#162053 = DIRECTION ( 'NONE',  ( 0.000000000000000000, -0.000000000000000000, 1.000000000000000000 ) ) ;
#162054 = LINE ( 'NONE', #65492, #138833 ) ;
#162055 = VERTEX_POINT ( 'NONE', #201705 ) ;
#162056 = DIRECTION ( 'NONE',  ( -1.000000000000000000, 0.000000000000000000, 0.000000000000000000 ) ) ;
#162057 = EDGE_CURVE ( 'NONE', #94760, #20464, #199330, .T. ) ;
#162058 = CARTESIAN_POINT ( 'NONE',  ( -20.64999999999999858, 2.000000000011154189, -154.6753780772379514 ) ) ;
#162059 = VECTOR ( 'NONE', #196582, 1000.000000000000000 ) ;
#162060 = CIRCLE ( 'NONE', #32912, 0.09999999999999939493 ) ;
#162061 = ORIENTED_EDGE ( 'NONE', *, *, #8192, .F. ) ;
#162062 = AXIS2_PLACEMENT_3D ( 'NONE', #102562, #101260, #257767 ) ;
#162063 = AXIS2_PLACEMENT_3D ( 'NONE', #131030, #19780, #120187 ) ;
#162064 = CARTESIAN_POINT ( 'NONE',  ( 21.10320863425824811, 6.248357867143764288, -199.6135654718238186 ) ) ;
#162065 = DIRECTION ( 'NONE',  ( -0.000000000000000000, -6.982962677686266711E-15, 1.000000000000000000 ) ) ;
#162066 = ADVANCED_FACE ( 'NONE', ( #184702 ), #245978, .T. ) ;
#162067 = ORIENTED_EDGE ( 'NONE', *, *, #235110, .T. ) ;
#162068 = AXIS2_PLACEMENT_3D ( 'NONE', #121509, #139737, #43234 ) ;
#162069 = ORIENTED_EDGE ( 'NONE', *, *, #128636, .T. ) ;
#162070 = DIRECTION ( 'NONE',  ( -1.000000000000000000, 2.952720810173289112E-16, 2.061873921506763405E-30 ) ) ;
#162071 = VERTEX_POINT ( 'NONE', #102574 ) ;
#162072 = DIRECTION ( 'NONE',  ( -6.938893903907224433E-15, -1.000000000000000000, -6.982962677686266711E-15 ) ) ;
#162073 = VERTEX_POINT ( 'NONE', #23096 ) ;
#162075 = EDGE_LOOP ( 'NONE', ( #151201, #86326, #34210, #85164 ) ) ;
#162074 = DIRECTION ( 'NONE',  ( 1.000000000000000000, 0.000000000000000000, 0.000000000000000000 ) ) ;
#162076 = ADVANCED_FACE ( 'NONE', ( #204260 ), #6061, .F. ) ;
#162077 = CARTESIAN_POINT ( 'NONE',  ( 20.94999999999999929, 30.92427036846531863, -234.3138941982948040 ) ) ;
#162078 = VERTEX_POINT ( 'NONE', #81721 ) ;
#162079 = CARTESIAN_POINT ( 'NONE',  ( -21.00023020733502932, 1.115542391533913547E-11, -94.10913075473168021 ) ) ;
#162080 = AXIS2_PLACEMENT_3D ( 'NONE', #210209, #118487, #136732 ) ;
#162081 = CIRCLE ( 'NONE', #41291, 0.09999999999998898659 ) ;
#162082 = ORIENTED_EDGE ( 'NONE', *, *, #88998, .T. ) ;
#162084 = VERTEX_POINT ( 'NONE', #85567 ) ;
#162083 = ORIENTED_EDGE ( 'NONE', *, *, #226601, .F. ) ;
#162086 = CARTESIAN_POINT ( 'NONE',  ( 21.05000000000000071, 69.69548367074810358, -136.5020041764652206 ) ) ;
#162085 = AXIS2_PLACEMENT_3D ( 'NONE', #214586, #217137, #16420 ) ;
#162087 = EDGE_CURVE ( 'NONE', #208239, #22313, #190975, .T. ) ;
#162088 = CARTESIAN_POINT ( 'NONE',  ( -20.87155475150660777, 56.12642167632806434, -227.9547677828175836 ) ) ;
#162089 = ORIENTED_EDGE ( 'NONE', *, *, #64093, .T. ) ;
#162090 = ADVANCED_FACE ( 'NONE', ( #165155 ), #239793, .T. ) ;
#162091 = CIRCLE ( 'NONE', #182935, 0.5000000000000004441 ) ;
#162092 = ORIENTED_EDGE ( 'NONE', *, *, #15054, .T. ) ;
#162093 = DIRECTION ( 'NONE',  ( 1.000000000000000000, 0.000000000000000000, 0.000000000000000000 ) ) ;
#162094 = PLANE ( 'NONE',  #163917 ) ;
#162096 = EDGE_CURVE ( 'NONE', #99738, #99483, #43917, .T. ) ;
#162095 =( BOUNDED_SURFACE ( )  B_SPLINE_SURFACE ( 3, 2, ( 
 ( #118922, #231, #79749 ),
 ( #199750, #134591, #21116 ),
 ( #100587, #1510, #214158 ),
 ( #206149, #165759, #245283 ) ),
 .UNSPECIFIED., .F., .F., .F. ) 
 B_SPLINE_SURFACE_WITH_KNOTS ( ( 4, 4 ),
 ( 3, 3 ),
 ( -1.387778780781445676E-17, 0.001979672783031532872 ),
 ( 0.000000000000000000, 1.000000000000000000 ),
 .UNSPECIFIED. ) 
 GEOMETRIC_REPRESENTATION_ITEM ( )  RATIONAL_B_SPLINE_SURFACE ( (
 ( 1.000000000000000000, 0.7103081912008362142, 1.000000000000000000),
 ( 1.000000000000000000, 0.7104998333558978363, 1.000000000000000000),
 ( 1.000000000000000000, 0.7107238315755931568, 1.000000000000000000),
 ( 1.000000000000000000, 0.7110073749539214116, 1.000000000000000000) ) ) 
 REPRESENTATION_ITEM ( '' )  SURFACE ( )  );
#162098 = ORIENTED_EDGE ( 'NONE', *, *, #123596, .T. ) ;
#162097 = DIRECTION ( 'NONE',  ( 1.000000000000000000, 0.000000000000000000, 0.000000000000000000 ) ) ;
#162099 = CARTESIAN_POINT ( 'NONE',  ( -20.94999999999999929, 74.93036000061670165, -233.6816308724374949 ) ) ;
#162100 = ORIENTED_EDGE ( 'NONE', *, *, #45278, .T. ) ;
#162101 = CARTESIAN_POINT ( 'NONE',  ( -18.50000000000000000, 65.70711192142388768, -131.0651054685122574 ) ) ;
#162102 = CARTESIAN_POINT ( 'NONE',  ( -21.05000000000000071, -1.162701749926853712, -142.0000000000000284 ) ) ;
#162104 = ORIENTED_EDGE ( 'NONE', *, *, #165937, .F. ) ;
#162103 = ADVANCED_FACE ( 'NONE', ( #244671 ), #84269, .F. ) ;
#162105 = ADVANCED_FACE ( 'NONE', ( #66042 ), #178498, .F. ) ;
#162106 = CARTESIAN_POINT ( 'NONE',  ( 21.97500000000000497, 9.749999999999998224, -12.25000000000000178 ) ) ;
#162107 = CARTESIAN_POINT ( 'NONE',  ( -21.05000000000000071, 76.00000000001145395, -40.02310748452431710 ) ) ;
#162108 = EDGE_LOOP ( 'NONE', ( #252531, #77971, #118780, #99236 ) ) ;
#162109 = DIRECTION ( 'NONE',  ( 1.000000000000000000, 0.000000000000000000, 0.000000000000000000 ) ) ;
#162110 = ORIENTED_EDGE ( 'NONE', *, *, #241721, .F. ) ;
#162111 = CIRCLE ( 'NONE', #24553, 0.1000000000000054040 ) ;
#162112 = ADVANCED_FACE ( 'NONE', ( #185998 ), #126011, .F. ) ;
#162114 = EDGE_LOOP ( 'NONE', ( #101619, #134397, #149772 ) ) ;
#162113 = ORIENTED_EDGE ( 'NONE', *, *, #215127, .T. ) ;
#162115 = ORIENTED_EDGE ( 'NONE', *, *, #212347, .F. ) ;
#162116 = CARTESIAN_POINT ( 'NONE',  ( -20.54999999999999716, 71.65000000001228386, -157.6731074845243938 ) ) ;
#162117 = VERTEX_POINT ( 'NONE', #7356 ) ;
#162118 = CARTESIAN_POINT ( 'NONE',  ( 21.00000000000000000, 66.25000000001229239, -157.6731074845244223 ) ) ;
#162119 = AXIS2_PLACEMENT_3D ( 'NONE', #164716, #186861, #202552 ) ;
#162120 = EDGE_LOOP ( 'NONE', ( #132036, #213097, #34880, #115658 ) ) ;
#162121 = EDGE_CURVE ( 'NONE', #84696, #223817, #41380, .T. ) ;
#162122 = ADVANCED_FACE ( 'NONE', ( #72486 ), #52896, .F. ) ;
#162123 = CARTESIAN_POINT ( 'NONE',  ( 21.87500000000000355, 9.750000000011153745, -155.1500000000000057 ) ) ;
#162124 = VERTEX_POINT ( 'NONE', #110306 ) ;
#162125 = VERTEX_POINT ( 'NONE', #93309 ) ;
#162126 = CIRCLE ( 'NONE', #245320, 0.09999999999999971412 ) ;
#162128 = EDGE_LOOP ( 'NONE', ( #1109, #83485, #108289, #27686 ) ) ;
#162127 = AXIS2_PLACEMENT_3D ( 'NONE', #139790, #177684, #96797 ) ;
#162129 = VECTOR ( 'NONE', #40769, 1000.000000000000000 ) ;
#162130 = FACE_OUTER_BOUND ( 'NONE', #187636, .T. ) ;
#162131 = ADVANCED_FACE ( 'NONE', ( #109011 ), #232663, .T. ) ;
#162132 = ORIENTED_EDGE ( 'NONE', *, *, #117449, .F. ) ;
#162133 = EDGE_CURVE ( 'NONE', #126428, #85926, #69927, .T. ) ;
#162134 = CARTESIAN_POINT ( 'NONE',  ( -21.05000000000000071, 77.26178616857710324, -128.4366085209788366 ) ) ;
#162135 = DIRECTION ( 'NONE',  ( 0.000000000000000000, 0.000000000000000000, -1.000000000000000000 ) ) ;
#162136 = CARTESIAN_POINT ( 'NONE',  ( -18.59999999999999787, 11.65000000001115232, -155.3500000000000227 ) ) ;
#162137 = AXIS2_PLACEMENT_3D ( 'NONE', #134572, #116334, #152910 ) ;
#162139 = AXIS2_PLACEMENT_3D ( 'NONE', #44592, #196266, #142393 ) ;
#162138 = CARTESIAN_POINT ( 'NONE',  ( 20.95262331984766746, 65.49584273722238947, -162.4622191549311481 ) ) ;
#162140 = CARTESIAN_POINT ( 'NONE',  ( -23.15000000000000213, 73.40000000001245439, -181.7731074845243882 ) ) ;
#162141 = DIRECTION ( 'NONE',  ( 0.000000000000000000, 0.000000000000000000, 1.000000000000000000 ) ) ;
#162143 = CARTESIAN_POINT ( 'NONE',  ( -20.64999999999999858, 68.75000000001230660, -157.6731074845243938 ) ) ;
#162142 = FACE_OUTER_BOUND ( 'NONE', #13284, .T. ) ;
#162144 = DIRECTION ( 'NONE',  ( 0.000000000000000000, -1.000000000000000000, 0.000000000000000000 ) ) ;
#162145 = CARTESIAN_POINT ( 'NONE',  ( -20.54999999999999716, 73.60000000001221565, -146.4170766071768242 ) ) ;
#162146 = EDGE_CURVE ( 'NONE', #102393, #18238, #188561, .T. ) ;
#162147 = CARTESIAN_POINT ( 'NONE',  ( 18.59999999999998721, 67.85125148167622910, -227.9794913823769491 ) ) ;
#162148 = DIRECTION ( 'NONE',  ( 1.000000000000000000, 0.000000000000000000, -0.000000000000000000 ) ) ;
#162149 = VERTEX_POINT ( 'NONE', #9924 ) ;
#162150 = CONICAL_SURFACE ( 'NONE', #187092, 4.049999999999995381, 0.7853981633974604915 ) ;
#162151 = AXIS2_PLACEMENT_3D ( 'NONE', #36574, #118664, #39125 ) ;
#162152 = VECTOR ( 'NONE', #147067, 1000.000000000000000 ) ;
#162153 = CIRCLE ( 'NONE', #199585, 0.1000000000000046685 ) ;
#162155 = ORIENTED_EDGE ( 'NONE', *, *, #161339, .T. ) ;
#162154 = FACE_BOUND ( 'NONE', #199121, .T. ) ;
#162156 = ORIENTED_EDGE ( 'NONE', *, *, #253073, .F. ) ;
#162157 = AXIS2_PLACEMENT_3D ( 'NONE', #21055, #45400, #66253 ) ;
#162158 = DIRECTION ( 'NONE',  ( -6.938893903907209445E-14, -0.9999176327611370985, -0.01283462868040260302 ) ) ;
#162159 = CARTESIAN_POINT ( 'NONE',  ( 20.21494484322224849, 9.303170737879936425, -142.3402651917702997 ) ) ;
#162160 = DIRECTION ( 'NONE',  ( 1.000000000000000000, 0.000000000000000000, 0.000000000000000000 ) ) ;
#162161 = ORIENTED_EDGE ( 'NONE', *, *, #1280, .T. ) ;
#162162 = EDGE_CURVE ( 'NONE', #120394, #142601, #120257, .T. ) ;
#162163 =( NAMED_UNIT ( * ) SI_UNIT ( $, .STERADIAN. ) SOLID_ANGLE_UNIT ( ) );
#162164 = LINE ( 'NONE', #63028, #12548 ) ;
#162165 = PRODUCT ( 'Snap Open Cable Crossbars 5', 'Snap Open Cable Crossbars 5', '', ( #203292 ) ) ;
#162166 = EDGE_CURVE ( 'NONE', #76531, #219544, #29524, .T. ) ;
#162167 = DIRECTION ( 'NONE',  ( 0.000000000000000000, -0.8814952561688103039, 0.4721928772777957972 ) ) ;
#162168 = VECTOR ( 'NONE', #42316, 1000.000000000000000 ) ;
#162169 = ORIENTED_EDGE ( 'NONE', *, *, #34963, .T. ) ;
#162170 = DIRECTION ( 'NONE',  ( 0.000000000000000000, 0.000000000000000000, -1.000000000000000000 ) ) ;
#162171 = SPHERICAL_SURFACE ( 'NONE', #58928, 0.1000000000000000056 ) ;
#162172 = DIRECTION ( 'NONE',  ( 0.000000000000000000, -0.7049548389605022614, 0.7092521942343023023 ) ) ;
#162173 = EDGE_CURVE ( 'NONE', #50332, #74935, #169040, .T. ) ;
#162174 = DIRECTION ( 'NONE',  ( 1.000000000000000000, 0.000000000000000000, 0.000000000000000000 ) ) ;
#162176 = ORIENTED_EDGE ( 'NONE', *, *, #153156, .F. ) ;
#162175 = CARTESIAN_POINT ( 'NONE',  ( -20.94999027547553894, 67.49459761544871128, -195.5598716110968951 ) ) ;
#162177 = DIRECTION ( 'NONE',  ( 0.000000000000000000, -0.8814952561688428334, 0.4721928772777350680 ) ) ;
#162179 = ORIENTED_EDGE ( 'NONE', *, *, #31543, .T. ) ;
#162178 = LINE ( 'NONE', #1779, #110714 ) ;
#162181 = EDGE_CURVE ( 'NONE', #37535, #250224, #28241, .T. ) ;
#162180 = CARTESIAN_POINT ( 'NONE',  ( -20.64999999999999858, 21.39147882631411335, -233.2615922652120730 ) ) ;
#162182 = DIRECTION ( 'NONE',  ( 0.000000000000000000, 7.162729191130023213E-15, -1.000000000000000000 ) ) ;
#162183 = DIRECTION ( 'NONE',  ( 1.000000000000000000, 0.000000000000000000, 0.000000000000000000 ) ) ;
#162184 = TOROIDAL_SURFACE ( 'NONE', #191229, 11.70000000000000107, 0.1000000000000000056 ) ;
#162185 = CARTESIAN_POINT ( 'NONE',  ( -12.25000000000000355, 9.350000000011133849, -184.0185689574025787 ) ) ;
#162187 = DIRECTION ( 'NONE',  ( 1.000000000000000000, -0.000000000000000000, -0.000000000000000000 ) ) ;
#162186 = DIRECTION ( 'NONE',  ( 0.000000000000000000, -6.853228547068871147E-15, 1.000000000000000000 ) ) ;
#162189 = EDGE_CURVE ( 'NONE', #206663, #35927, #149462, .T. ) ;
#162188 = DIRECTION ( 'NONE',  ( 0.000000000000000000, 6.997203936713175802E-15, -1.000000000000000000 ) ) ;
#162190 = CIRCLE ( 'NONE', #49740, 0.09999999999999939493 ) ;
#162191 = CARTESIAN_POINT ( 'NONE',  ( -22.50000000000000000, 76.00000000001222134, -148.1726782920690937 ) ) ;
#162192 = CARTESIAN_POINT ( 'NONE',  ( -18.56579813702275672, 10.33025634371521662, -39.08709292826389259 ) ) ;
#162193 = LINE ( 'NONE', #242979, #110294 ) ;
#162194 = CARTESIAN_POINT ( 'NONE',  ( 23.15000000000000213, -4.756823075239757337, -233.1486023682345490 ) ) ;
#162196 = VERTEX_POINT ( 'NONE', #228983 ) ;
#162195 = AXIS2_PLACEMENT_3D ( 'NONE', #132027, #92889, #53774 ) ;
#162197 = EDGE_CURVE ( 'NONE', #83997, #231898, #71625, .T. ) ;
#162198 = CARTESIAN_POINT ( 'NONE',  ( 21.00000000000000000, 66.25000000001158185, -57.17310748452438673 ) ) ;
#162200 = EDGE_CURVE ( 'NONE', #90934, #87279, #128588, .T. ) ;
#162199 = EDGE_CURVE ( 'NONE', #76100, #106358, #112881, .T. ) ;
#162201 = VERTEX_POINT ( 'NONE', #127308 ) ;
#162202 =( BOUNDED_CURVE ( )  B_SPLINE_CURVE ( 3, ( #110937, #11868, #173538, #253011 ),
 .UNSPECIFIED., .F., .T. ) 
 B_SPLINE_CURVE_WITH_KNOTS ( ( 4, 4 ),
 ( 5.731445031868799056, 5.983100554402348337 ),
 .UNSPECIFIED. ) 
 CURVE ( )  GEOMETRIC_REPRESENTATION_ITEM ( )  RATIONAL_B_SPLINE_CURVE ( ( 1.000000000000000000, 0.9947294176030464508, 0.9947294176030464508, 1.000000000000000000 ) ) 
 REPRESENTATION_ITEM ( '' )  );
#162203 = ORIENTED_EDGE ( 'NONE', *, *, #158787, .T. ) ;
#162204 = CARTESIAN_POINT ( 'NONE',  ( -23.25000000000000000, 76.00000000001142553, -36.02310748452432421 ) ) ;
#162205 = CARTESIAN_POINT ( 'NONE',  ( -21.14999999999999858, 12.71802988599559292, -223.5105008658000258 ) ) ;
#162206 = ORIENTED_EDGE ( 'NONE', *, *, #175617, .T. ) ;
#162207 = VECTOR ( 'NONE', #68609, 1000.000000000000000 ) ;
#162208 = ORIENTED_EDGE ( 'NONE', *, *, #198860, .T. ) ;
#162209 = AXIS2_PLACEMENT_3D ( 'NONE', #22274, #40578, #139608 ) ;
#162210 = ORIENTED_EDGE ( 'NONE', *, *, #74999, .F. ) ;
#162211 = EDGE_CURVE ( 'NONE', #150376, #75474, #174434, .T. ) ;
#162212 = CARTESIAN_POINT ( 'NONE',  ( 23.04999999999999716, 41.49355468354239207, -237.7178856438439141 ) ) ;
#162214 = ADVANCED_FACE ( 'NONE', ( #12519 ), #92025, .T. ) ;
#162213 = AXIS2_PLACEMENT_3D ( 'NONE', #227549, #188420, #248404 ) ;
#162215 = ORIENTED_EDGE ( 'NONE', *, *, #31554, .T. ) ;
#162216 = CARTESIAN_POINT ( 'NONE',  ( 18.69999999999999929, 8.000000000000000000, 1.212568896937007867 ) ) ;
#162217 = CARTESIAN_POINT ( 'NONE',  ( -20.54999999999999716, 7.250000000011155521, -146.2500000000000284 ) ) ;
#162218 = CARTESIAN_POINT ( 'NONE',  ( 21.14999999999999503, -0.09999999998884338825, -55.35042919245524473 ) ) ;
#162219 = DIRECTION ( 'NONE',  ( 0.000000000000000000, -0.1298341882520124002, -0.9915357197604841577 ) ) ;
#162220 = CYLINDRICAL_SURFACE ( 'NONE', #206731, 0.09999999999999939493 ) ;
#162221 = EDGE_CURVE ( 'NONE', #215277, #53042, #95272, .T. ) ;
#162222 = SPHERICAL_SURFACE ( 'NONE', #224837, 0.1000000000000000056 ) ;
#162223 = CARTESIAN_POINT ( 'NONE',  ( -23.25000000000000000, 11.75000000001115552, -33.50000000000000000 ) ) ;
#162225 = EDGE_LOOP ( 'NONE', ( #130849, #129854, #256219, #228279 ) ) ;
#162224 = CARTESIAN_POINT ( 'NONE',  ( 22.39999999999999503, 0.1000000000111554016, -159.7092204016265669 ) ) ;
#162227 = CARTESIAN_POINT ( 'NONE',  ( -18.59999999999999787, 74.26374286841490857, -158.4544551555068779 ) ) ;
#162226 = CYLINDRICAL_SURFACE ( 'NONE', #83846, 0.09999999999998898659 ) ;
#162228 = CARTESIAN_POINT ( 'NONE',  ( -22.47007471830798409, 76.00000000001170974, -77.24381813645081252 ) ) ;
#162229 = ADVANCED_FACE ( 'NONE', ( #23765 ), #11912, .T. ) ;
#162230 = ORIENTED_EDGE ( 'NONE', *, *, #150311, .T. ) ;
#162231 = DIRECTION ( 'NONE',  ( 0.000000000000000000, 0.000000000000000000, -1.000000000000000000 ) ) ;
#162232 = ORIENTED_EDGE ( 'NONE', *, *, #118401, .T. ) ;
#162233 = ADVANCED_FACE ( 'NONE', ( #121588 ), #35932, .T. ) ;
#162235 = CARTESIAN_POINT ( 'NONE',  ( -16.94132844910801339, 66.00756324483165827, -115.6269057285420558 ) ) ;
#162234 = DIRECTION ( 'NONE',  ( 0.000000000000000000, 1.000000000000000000, 6.982962677686266711E-15 ) ) ;
#162236 = VECTOR ( 'NONE', #132816, 1000.000000000000000 ) ;
#162237 = LINE ( 'NONE', #551, #127262 ) ;
#162238 = ORIENTED_EDGE ( 'NONE', *, *, #196703, .T. ) ;
#162239 = CYLINDRICAL_SURFACE ( 'NONE', #28602, 0.09999999999999939493 ) ;
#162240 = CARTESIAN_POINT ( 'NONE',  ( -22.45354308602486526, 2.198892876589933535E-07, -21.74956710954100814 ) ) ;
#162241 = DIRECTION ( 'NONE',  ( 4.504528286903032433E-15, 0.1298341882520054891, 0.9915357197604850459 ) ) ;
#162242 = EDGE_CURVE ( 'NONE', #50377, #217495, #253475, .T. ) ;
#162243 = ORIENTED_EDGE ( 'NONE', *, *, #58975, .T. ) ;
#162245 = EDGE_CURVE ( 'NONE', #1805, #241566, #223995, .T. ) ;
#162244 = CARTESIAN_POINT ( 'NONE',  ( 21.13461538461538680, 67.11458296203741725, -90.77310748452435973 ) ) ;
#162246 = AXIS2_PLACEMENT_3D ( 'NONE', #64474, #203967, #185703 ) ;
#162247 = LINE ( 'NONE', #241753, #107690 ) ;
#162248 = CARTESIAN_POINT ( 'NONE',  ( 18.39999999999997371, 64.52683809664949877, -112.2731074845243739 ) ) ;
#162249 = CIRCLE ( 'NONE', #124819, 0.09999999999999939493 ) ;
#162250 = AXIS2_PLACEMENT_3D ( 'NONE', #50849, #130406, #113422 ) ;
#162251 = CARTESIAN_POINT ( 'NONE',  ( -18.50000000000000000, 11.75000000000000000, -12.14999999999999680 ) ) ;
#162252 = CARTESIAN_POINT ( 'NONE',  ( 21.05000000000000071, 77.83534155023646406, -124.9679561919612922 ) ) ;
#162253 = ORIENTED_EDGE ( 'NONE', *, *, #251693, .T. ) ;
#162254 = AXIS2_PLACEMENT_3D ( 'NONE', #11836, #246550, #245290 ) ;
#162255 = CARTESIAN_POINT ( 'NONE',  ( 18.49999999999999289, 66.54223038922117439, -213.7542166125332415 ) ) ;
#162256 = CARTESIAN_POINT ( 'NONE',  ( 20.94999999999999574, 79.03091752131670944, -235.9469187808398942 ) ) ;
#162257 = CARTESIAN_POINT ( 'NONE',  ( -21.08035267497491816, 75.91731137523568407, -75.85481432430736959 ) ) ;
#162258 = CARTESIAN_POINT ( 'NONE',  ( 23.25000000000000000, 21.10816309994747186, -233.7904894189133813 ) ) ;
#162259 = ADVANCED_FACE ( 'NONE', ( #238938 ), #74467, .F. ) ;
#162260 = DIRECTION ( 'NONE',  ( 0.000000000000000000, 0.2128009952263604232, -0.9770955615653316162 ) ) ;
#162262 = ORIENTED_EDGE ( 'NONE', *, *, #25604, .F. ) ;
#162261 = CARTESIAN_POINT ( 'NONE',  ( 21.05995757104869526, 67.22461075529028562, -57.32820236153317950 ) ) ;
#162263 = CYLINDRICAL_SURFACE ( 'NONE', #192369, 0.09999999999999939493 ) ;
#162264 = DIRECTION ( 'NONE',  ( 0.000000000000000000, 0.9126074666064696306, 0.4088369013361212723 ) ) ;
#162265 = CARTESIAN_POINT ( 'NONE',  ( -22.50000000000000000, 76.00000000001222134, -148.1726782920690937 ) ) ;
#162266 = VERTEX_POINT ( 'NONE', #240230 ) ;
#162267 = DIRECTION ( 'NONE',  ( 0.000000000000000000, 8.896017825522085641E-15, -1.000000000000000000 ) ) ;
#162268 = CARTESIAN_POINT ( 'NONE',  ( -20.94999999999999929, 1.115600667400684642E-11, -67.00000000000000000 ) ) ;
#162269 = AXIS2_PLACEMENT_3D ( 'NONE', #89711, #46736, #123728 ) ;
#162270 = DIRECTION ( 'NONE',  ( -0.000000000000000000, 0.2617529984165031243, 0.9651348961777157509 ) ) ;
#162271 = CIRCLE ( 'NONE', #87409, 0.1000000000000028644 ) ;
#162272 = DIRECTION ( 'NONE',  ( -0.000000000000000000, 1.000000000000000000, -0.000000000000000000 ) ) ;
#162273 = EDGE_LOOP ( 'NONE', ( #112368, #194478, #61767, #41294, #76214, #11701, #89006, #54681, #73042 ) ) ;
#162274 = ADVANCED_FACE ( 'NONE', ( #134982 ), #153333, .T. ) ;
#162275 = CARTESIAN_POINT ( 'NONE',  ( -18.59999999999999787, 52.91185528119410719, -244.1460391050142960 ) ) ;
#162276 = EDGE_LOOP ( 'NONE', ( #228839, #256202 ) ) ;
#162277 = ORIENTED_EDGE ( 'NONE', *, *, #226144, .T. ) ;
#162278 = DIRECTION ( 'NONE',  ( 0.000000000000000000, 0.000000000000000000, 1.000000000000000000 ) ) ;
#162279 = LINE ( 'NONE', #241792, #220642 ) ;
#162280 = FILL_AREA_STYLE ('',( #85254 ) ) ;
#162281 = DIRECTION ( 'NONE',  ( 0.000000000000000000, 0.000000000000000000, -1.000000000000000000 ) ) ;
#162282 = ORIENTED_EDGE ( 'NONE', *, *, #193658, .T. ) ;
#162283 = DIRECTION ( 'NONE',  ( 0.000000000000000000, 0.000000000000000000, 1.000000000000000000 ) ) ;
#162284 = LINE ( 'NONE', #24062, #171204 ) ;
#162285 = CARTESIAN_POINT ( 'NONE',  ( 21.13461538461539035, 12.97827409159657464, -210.7106268109450298 ) ) ;
#162286 = CARTESIAN_POINT ( 'NONE',  ( -18.59999999999999787, -10.63400887967554986, 6.002871413764276909 ) ) ;
#162288 = SPHERICAL_SURFACE ( 'NONE', #169423, 0.1000000000000000056 ) ;
#162287 = CIRCLE ( 'NONE', #195622, 11.79999999999999716 ) ;
#162289 = CARTESIAN_POINT ( 'NONE',  ( 20.73486653747088582, 9.052352027204005225, -208.4953267290897259 ) ) ;
#162290 = ORIENTED_EDGE ( 'NONE', *, *, #165592, .T. ) ;
#162292 = EDGE_LOOP ( 'NONE', ( #59285, #164126, #209172, #27914 ) ) ;
#162291 = DIRECTION ( 'NONE',  ( 1.000000000000000000, 0.000000000000000000, 0.000000000000000000 ) ) ;
#162293 = ORIENTED_EDGE ( 'NONE', *, *, #111160, .F. ) ;
#162294 = CARTESIAN_POINT ( 'NONE',  ( -16.78493211734303259, 9.945835743204170853, -20.83605098089596908 ) ) ;
#162295 = ORIENTED_EDGE ( 'NONE', *, *, #179030, .F. ) ;
#162296 = CARTESIAN_POINT ( 'NONE',  ( -20.64999999999999858, 68.85000000001151932, -48.27310748452437394 ) ) ;
#162297 = DIRECTION ( 'NONE',  ( 1.000000000000000000, 0.000000000000000000, 0.000000000000000000 ) ) ;
#162298 = DIRECTION ( 'NONE',  ( -1.000000000000000000, -0.000000000000000000, -0.000000000000000000 ) ) ;
#162299 = AXIS2_PLACEMENT_3D ( 'NONE', #246805, #212842, #113727 ) ;
#162300 = ORIENTED_EDGE ( 'NONE', *, *, #37578, .F. ) ;
#162301 = CARTESIAN_POINT ( 'NONE',  ( 23.14999999999999503, 16.00289399696429271, -219.2628689893550700 ) ) ;
#162302 = LINE ( 'NONE', #64478, #38733 ) ;
#162303 = ORIENTED_EDGE ( 'NONE', *, *, #69070, .F. ) ;
#162304 = CARTESIAN_POINT ( 'NONE',  ( -14.45422546970483779, 9.450602096099679272, -152.4438959630966792 ) ) ;
#162306 = VERTEX_POINT ( 'NONE', #103243 ) ;
#162305 = CARTESIAN_POINT ( 'NONE',  ( 18.59999999999999787, 77.83534155023646406, -124.9679561919613064 ) ) ;
#162307 = EDGE_CURVE ( 'NONE', #211067, #24355, #161931, .T. ) ;
#162308 = CARTESIAN_POINT ( 'NONE',  ( -20.64999999999999858, 76.00000000001165290, -69.52310748452431710 ) ) ;
#162309 = FACE_OUTER_BOUND ( 'NONE', #181566, .T. ) ;
#162310 = VECTOR ( 'NONE', #22452, 1000.000000000000000 ) ;
#162311 = CIRCLE ( 'NONE', #128988, 0.09999999999999917288 ) ;
#162312 = ORIENTED_EDGE ( 'NONE', *, *, #76645, .T. ) ;
#162313 = CARTESIAN_POINT ( 'NONE',  ( -18.40000000000000213, 14.17280543801757986, -210.8598471598932349 ) ) ;
#162314 = CARTESIAN_POINT ( 'NONE',  ( 21.09696443733127325, 10.72400988392963228, -79.23477752704826571 ) ) ;
#162315 = CYLINDRICAL_SURFACE ( 'NONE', #110053, 0.1000000000000024342 ) ;
#162316 = ORIENTED_EDGE ( 'NONE', *, *, #58498, .F. ) ;
#162317 = CARTESIAN_POINT ( 'NONE',  ( -18.40000000000000213, 15.91777359887373500, -218.8720307647289758 ) ) ;
#162318 = AXIS2_PLACEMENT_3D ( 'NONE', #205478, #183372, #244610 ) ;
#162319 = ADVANCED_FACE ( 'NONE', ( #79829 ), #149454, .T. ) ;
#162320 = CARTESIAN_POINT ( 'NONE',  ( -20.85000000000000142, -1.249999999999999334, -41.30048075441508360 ) ) ;
#162321 = VECTOR ( 'NONE', #108319, 1000.000000000000000 ) ;
#162322 = EDGE_CURVE ( 'NONE', #161829, #233373, #73783, .T. ) ;
#162323 = ORIENTED_EDGE ( 'NONE', *, *, #229452, .T. ) ;
#162324 = EDGE_CURVE ( 'NONE', #119487, #204355, #70363, .T. ) ;
#162325 = TOROIDAL_SURFACE ( 'NONE', #120637, 0.6000000000000015321, 0.1000000000000000056 ) ;
#162326 = CIRCLE ( 'NONE', #208128, 0.2000000000000111688 ) ;
#162327 = CIRCLE ( 'NONE', #74866, 0.09999999999999609201 ) ;
#162328 = ORIENTED_EDGE ( 'NONE', *, *, #131211, .F. ) ;
#162329 = CIRCLE ( 'NONE', #183174, 11.74999999999999645 ) ;
#162330 = VECTOR ( 'NONE', #238317, 1000.000000000000000 ) ;
#162331 = EDGE_CURVE ( 'NONE', #135761, #59396, #1588, .T. ) ;
#162332 = ORIENTED_EDGE ( 'NONE', *, *, #228940, .T. ) ;
#162333 = EDGE_CURVE ( 'NONE', #9389, #30313, #95865, .T. ) ;
#162334 = CARTESIAN_POINT ( 'NONE',  ( 18.59999999999999787, -1.851028230129704522, -45.15391326942249606 ) ) ;
#162335 = VECTOR ( 'NONE', #34537, 1000.000000000000114 ) ;
#162336 = CARTESIAN_POINT ( 'NONE',  ( -16.83233564386387471, 66.06977820342792995, -182.7985868210483318 ) ) ;
#162338 = VERTEX_POINT ( 'NONE', #108411 ) ;
#162337 = DIRECTION ( 'NONE',  ( -1.000000000000000000, 0.000000000000000000, -0.000000000000000000 ) ) ;
#162339 = CARTESIAN_POINT ( 'NONE',  ( 21.04386569057559697, 11.75000000001105427, -127.1428373517806563 ) ) ;
#162340 = CARTESIAN_POINT ( 'NONE',  ( 18.59999999999999787, 7.128833340093095217, -233.7327013124392749 ) ) ;
#162341 = EDGE_CURVE ( 'NONE', #175390, #71001, #104518, .T. ) ;
#162342 = DIRECTION ( 'NONE',  ( -0.000000000000000000, -0.1350103645451876666, -0.9908441862701600211 ) ) ;
#162343 = DIRECTION ( 'NONE',  ( 1.000000000000000000, 0.000000000000000000, 0.000000000000000000 ) ) ;
#162344 = CARTESIAN_POINT ( 'NONE',  ( -18.45068461519106151, 85.48650652910120584, -129.4543303156195577 ) ) ;
#162345 = DIRECTION ( 'NONE',  ( -3.265361837132813093E-16, -0.9651348961777157509, 0.2617529984165031243 ) ) ;
#162347 = ORIENTED_EDGE ( 'NONE', *, *, #67249, .T. ) ;
#162346 = CARTESIAN_POINT ( 'NONE',  ( -21.05000000000000071, 76.25610579210459150, -170.0580039261966192 ) ) ;
#162349 = EDGE_LOOP ( 'NONE', ( #21616, #142374, #97279, #153592 ) ) ;
#162348 = CARTESIAN_POINT ( 'NONE',  ( 18.49999999999998934, 65.75000000001196554, -111.7731074845243739 ) ) ;
#162350 = DIRECTION ( 'NONE',  ( 2.952720810173289112E-16, 1.000000000000000000, -6.088138035986627436E-46 ) ) ;
#162351 = ADVANCED_FACE ( 'NONE', ( #244051 ), #249223, .T. ) ;
#162352 = VERTEX_POINT ( 'NONE', #223202 ) ;
#162353 = DIRECTION ( 'NONE',  ( 1.000000000000000000, 0.000000000000000000, 0.000000000000000000 ) ) ;
#162354 = CARTESIAN_POINT ( 'NONE',  ( 18.59999999999999432, 78.48087866980282001, -232.8271061603568910 ) ) ;
#162355 = FACE_OUTER_BOUND ( 'NONE', #168589, .T. ) ;
#162356 = ADVANCED_FACE ( 'NONE', ( #6733 ), #184086, .T. ) ;
#162357 = CARTESIAN_POINT ( 'NONE',  ( -18.50000000000000000, 77.83585931145498193, -24.51866831572578320 ) ) ;
#162358 = CARTESIAN_POINT ( 'NONE',  ( 23.30000000000000426, -11.79999999999999538, -347.0000000000001137 ) ) ;
#162359 = ORIENTED_EDGE ( 'NONE', *, *, #73351, .F. ) ;
#162360 = AXIS2_PLACEMENT_3D ( 'NONE', #178408, #60986, #76698 ) ;
#162361 = EDGE_CURVE ( 'NONE', #64755, #107188, #44588, .T. ) ;
#162362 = DIRECTION ( 'NONE',  ( -0.000000000000000000, 0.8660254037844411501, 0.4999999999999956701 ) ) ;
#162363 = EDGE_LOOP ( 'NONE', ( #148503, #159687, #115268, #92300 ) ) ;
#162364 = ORIENTED_EDGE ( 'NONE', *, *, #106822, .F. ) ;
#162365 = DIRECTION ( 'NONE',  ( 1.000000000000000000, -7.710376986078650754E-15, 1.458655703008169508E-14 ) ) ;
#162366 = AXIS2_PLACEMENT_3D ( 'NONE', #43090, #39263, #78347 ) ;
#162367 = ORIENTED_EDGE ( 'NONE', *, *, #110445, .T. ) ;
#162368 = VECTOR ( 'NONE', #23672, 1000.000000000000000 ) ;
#162369 = CARTESIAN_POINT ( 'NONE',  ( -18.59999999999999787, 74.83729825007408465, -128.4231074845243086 ) ) ;
#162370 = CARTESIAN_POINT ( 'NONE',  ( -18.50000000000000000, 86.87366311306884370, -199.3414869250131858 ) ) ;
#162371 = EDGE_CURVE ( 'NONE', #256858, #191840, #178699, .T. ) ;
#162372 = EDGE_LOOP ( 'NONE', ( #138612, #60364, #138634, #77764 ) ) ;
#162373 = CARTESIAN_POINT ( 'NONE',  ( 18.59999999999999076, 62.46583972339646351, -208.9186153945276487 ) ) ;
#162374 = ORIENTED_EDGE ( 'NONE', *, *, #179472, .F. ) ;
#162375 = DIRECTION ( 'NONE',  ( 0.000000000000000000, 0.000000000000000000, 1.000000000000000000 ) ) ;
#162376 = VERTEX_POINT ( 'NONE', #66716 ) ;
#162377 = CIRCLE ( 'NONE', #74907, 0.09999999999999939493 ) ;
#162378 = CYLINDRICAL_SURFACE ( 'NONE', #227168, 0.1000000000000065836 ) ;
#162379 = CIRCLE ( 'NONE', #237387, 12.87499999999999467 ) ;
#162380 = CARTESIAN_POINT ( 'NONE',  ( -18.59999999999999787, 43.27008861172207332, -245.2265230569236110 ) ) ;
#162381 = ORIENTED_EDGE ( 'NONE', *, *, #184894, .T. ) ;
#162382 = CYLINDRICAL_SURFACE ( 'NONE', #181927, 0.09999999999999939493 ) ;
#162384 = ORIENTED_EDGE ( 'NONE', *, *, #40912, .F. ) ;
#162383 = DIRECTION ( 'NONE',  ( 1.000000000000000000, 2.952720810173289112E-16, -0.000000000000000000 ) ) ;
#162385 = CARTESIAN_POINT ( 'NONE',  ( -22.39999999999999858, 76.00000000001276135, -215.1726782920691505 ) ) ;
#162386 = AXIS2_PLACEMENT_3D ( 'NONE', #157690, #217588, #121115 ) ;
#162387 = ORIENTED_EDGE ( 'NONE', *, *, #27039, .F. ) ;
#162388 = EDGE_CURVE ( 'NONE', #132417, #27579, #149633, .T. ) ;
#162389 = DIRECTION ( 'NONE',  ( -1.000000000000000000, 0.000000000000000000, 0.000000000000000000 ) ) ;
#162390 = ORIENTED_EDGE ( 'NONE', *, *, #183769, .T. ) ;
#162391 = DIRECTION ( 'NONE',  ( 8.673617379884087537E-15, -0.000000000000000000, 1.000000000000000000 ) ) ;
#162392 = DIRECTION ( 'NONE',  ( 0.000000000000000000, 1.000000000000000000, 0.000000000000000000 ) ) ;
#162393 = EDGE_CURVE ( 'NONE', #204559, #162455, #49662, .T. ) ;
#162394 = CARTESIAN_POINT ( 'NONE',  ( -15.75000000000000355, 66.15000000001258229, -186.7731074845244166 ) ) ;
#162395 = CARTESIAN_POINT ( 'NONE',  ( 18.59999999999996945, 67.49222854868494892, -195.4187676019683693 ) ) ;
#162396 = CARTESIAN_POINT ( 'NONE',  ( -15.06774609480957494, 66.58234804117157069, -188.1643200920839547 ) ) ;
#162398 = ORIENTED_EDGE ( 'NONE', *, *, #130697, .F. ) ;
#162397 = EDGE_CURVE ( 'NONE', #168403, #225332, #187060, .T. ) ;
#162400 = EDGE_CURVE ( 'NONE', #241262, #220817, #224440, .T. ) ;
#162399 = CARTESIAN_POINT ( 'NONE',  ( -16.94445028196807002, 66.00793639031481064, -182.6304376629428816 ) ) ;
#162401 = CARTESIAN_POINT ( 'NONE',  ( -21.05000000000000071, 87.48912529308871910, -200.6231074845242688 ) ) ;
#162402 = LINE ( 'NONE', #176833, #28742 ) ;
#162403 = VECTOR ( 'NONE', #50356, 1000.000000000000000 ) ;
#162404 = DIRECTION ( 'NONE',  ( -1.000000000000000000, 0.000000000000000000, 0.000000000000000000 ) ) ;
#162405 = CIRCLE ( 'NONE', #25052, 0.2000000000000057288 ) ;
#162406 = ORIENTED_EDGE ( 'NONE', *, *, #169165, .T. ) ;
#162407 = DIRECTION ( 'NONE',  ( 1.000000000000000000, 0.000000000000000000, -0.000000000000000000 ) ) ;
#162409 = EDGE_CURVE ( 'NONE', #85479, #42935, #91175, .T. ) ;
#162408 = ORIENTED_EDGE ( 'NONE', *, *, #164182, .T. ) ;
#162410 = FACE_OUTER_BOUND ( 'NONE', #173415, .T. ) ;
#162411 = ORIENTED_EDGE ( 'NONE', *, *, #29329, .F. ) ;
#162412 = DIRECTION ( 'NONE',  ( 0.000000000000000000, -0.2617529984165033463, -0.9651348961777157509 ) ) ;
#162413 = CARTESIAN_POINT ( 'NONE',  ( -20.87600722750343252, 10.33112638556969465, -72.59012289269746532 ) ) ;
#162414 = ADVANCED_FACE ( 'NONE', ( #247907 ), #207906, .F. ) ;
#162415 = VERTEX_POINT ( 'NONE', #8035 ) ;
#162417 = ORIENTED_EDGE ( 'NONE', *, *, #30763, .T. ) ;
#162416 = CARTESIAN_POINT ( 'NONE',  ( -21.59142135623730852, 12.19222130685950312, -220.0927928707378669 ) ) ;
#162418 = CARTESIAN_POINT ( 'NONE',  ( 20.94999999999999929, 0.000000000000000000, -33.50000000000000000 ) ) ;
#162419 = ORIENTED_EDGE ( 'NONE', *, *, #4399, .F. ) ;
#162420 = DIRECTION ( 'NONE',  ( 0.7071067811865388020, -0.7071067811865561215, 0.000000000000000000 ) ) ;
#162421 = DIRECTION ( 'NONE',  ( -1.000000000000000000, -3.265361837132813093E-16, 0.000000000000000000 ) ) ;
#162422 = VERTEX_POINT ( 'NONE', #224493 ) ;
#162423 = ORIENTED_EDGE ( 'NONE', *, *, #201371, .F. ) ;
#162424 = CIRCLE ( 'NONE', #45888, 2.000000000000001776 ) ;
#162426 = VECTOR ( 'NONE', #163447, 1000.000000000000000 ) ;
#162425 = CARTESIAN_POINT ( 'NONE',  ( -20.94999999999999929, 11.75000000001115552, -174.5148057706539930 ) ) ;
#162427 = CARTESIAN_POINT ( 'NONE',  ( -23.25000000000000000, 77.83585931145546510, -91.51866831572576189 ) ) ;
#162428 = CIRCLE ( 'NONE', #70862, 0.09999999999998898659 ) ;
#162430 = CARTESIAN_POINT ( 'NONE',  ( 16.87683809663750267, 66.05000000001230376, -157.3731074845244393 ) ) ;
#162429 = AXIS2_PLACEMENT_3D ( 'NONE', #166395, #51512, #46393 ) ;
#162431 = ORIENTED_EDGE ( 'NONE', *, *, #66069, .T. ) ;
#162432 = ORIENTED_EDGE ( 'NONE', *, *, #2647, .F. ) ;
#162433 = ADVANCED_FACE ( 'NONE', ( #242765 ), #167128, .F. ) ;
#162434 = VECTOR ( 'NONE', #131443, 1000.000000000000000 ) ;
#162435 = FACE_OUTER_BOUND ( 'NONE', #171831, .T. ) ;
#162436 = EDGE_CURVE ( 'NONE', #125974, #233400, #162111, .T. ) ;
#162437 = APPLICATION_CONTEXT ( 'automotive_design' ) ;
#162438 = ADVANCED_FACE ( 'NONE', ( #185373 ), #246620, .F. ) ;
#162440 = ORIENTED_EDGE ( 'NONE', *, *, #221494, .T. ) ;
#162439 = FACE_OUTER_BOUND ( 'NONE', #10858, .T. ) ;
#162441 = DIRECTION ( 'NONE',  ( 0.000000000000000000, 0.2617529984165031243, 0.9651348961777157509 ) ) ;
#162442 = AXIS2_PLACEMENT_3D ( 'NONE', #165102, #6011, #227627 ) ;
#162443 = LINE ( 'NONE', #102409, #19214 ) ;
#162444 = CARTESIAN_POINT ( 'NONE',  ( -16.87683809663752399, 62.98531230502843670, -213.8799296553602005 ) ) ;
#162446 = DIRECTION ( 'NONE',  ( 0.000000000000000000, 0.000000000000000000, -1.000000000000000000 ) ) ;
#162445 = CARTESIAN_POINT ( 'NONE',  ( -18.44085059012131822, 64.48598750652828926, -127.2634128036459202 ) ) ;
#162447 = CARTESIAN_POINT ( 'NONE',  ( -18.40000000000000213, 11.47867410001105526, -158.2253067836594198 ) ) ;
#162448 = DIRECTION ( 'NONE',  ( 0.000000000000000000, 0.8700118002898357128, -0.4930308989875170633 ) ) ;
#162449 = CARTESIAN_POINT ( 'NONE',  ( -16.86578989773641979, 60.87574773424856289, -221.1432832491776992 ) ) ;
#162450 = FACE_OUTER_BOUND ( 'NONE', #256402, .T. ) ;
#162451 = EDGE_LOOP ( 'NONE', ( #147318, #20869, #91170, #240399 ) ) ;
#162452 = B_SPLINE_CURVE_WITH_KNOTS ( 'NONE', 3,
 ( #93932, #114786, #213882, #230904, #95219, #14431, #13128 ),
 .UNSPECIFIED., .F., .F.,
 ( 4, 3, 4 ),
 ( 0.000000000000000000, 0.0009834301579440022593, 0.001767853679402679300 ),
 .UNSPECIFIED. ) ;
#162453 = ORIENTED_EDGE ( 'NONE', *, *, #199231, .F. ) ;
#162454 = DIRECTION ( 'NONE',  ( -0.000000000000000000, -0.000000000000000000, 1.000000000000000000 ) ) ;
#162455 = VERTEX_POINT ( 'NONE', #64148 ) ;
#162456 = CARTESIAN_POINT ( 'NONE',  ( -20.99142135623731065, 64.40000000001175806, -76.45131071479988805 ) ) ;
#162458 = EDGE_CURVE ( 'NONE', #129962, #129045, #228361, .T. ) ;
#162457 = VERTEX_POINT ( 'NONE', #148830 ) ;
#162459 = FILL_AREA_STYLE ('',( #219840 ) ) ;
#162460 = CARTESIAN_POINT ( 'NONE',  ( 20.89192007715127986, 65.67101464000523947, -130.9404391622479977 ) ) ;
#162461 = AXIS2_PLACEMENT_3D ( 'NONE', #2241, #145608, #225136 ) ;
#162463 = ORIENTED_EDGE ( 'NONE', *, *, #77842, .T. ) ;
#162462 = ORIENTED_EDGE ( 'NONE', *, *, #135064, .T. ) ;
#162464 = DIRECTION ( 'NONE',  ( -1.000000000000000000, 0.000000000000000000, 3.469446951953635015E-14 ) ) ;
#162465 = ORIENTED_EDGE ( 'NONE', *, *, #129655, .F. ) ;
#162466 = ORIENTED_EDGE ( 'NONE', *, *, #243109, .T. ) ;
#162467 = FACE_OUTER_BOUND ( 'NONE', #239751, .T. ) ;
#162468 = DIRECTION ( 'NONE',  ( 1.000000000000000000, 0.000000000000000000, 0.000000000000000000 ) ) ;
#162470 = ORIENTED_EDGE ( 'NONE', *, *, #174879, .T. ) ;
#162469 = CARTESIAN_POINT ( 'NONE',  ( 22.39999999999999858, 0.3085173699977246109, -229.9658011520297975 ) ) ;
#162471 = AXIS2_PLACEMENT_3D ( 'NONE', #90001, #50857, #32653 ) ;
#162472 = CARTESIAN_POINT ( 'NONE',  ( 20.59588692710267921, 39.39129011228262556, -236.9654500441737071 ) ) ;
#162473 = CARTESIAN_POINT ( 'NONE',  ( 20.94999999999999929, 65.70729864261004138, -97.56574559737244101 ) ) ;
#162475 = ORIENTED_EDGE ( 'NONE', *, *, #88227, .T. ) ;
#162474 = CARTESIAN_POINT ( 'NONE',  ( 20.95576188350343116, 10.60898054497455512, -141.6112337227543208 ) ) ;
#162476 = CARTESIAN_POINT ( 'NONE',  ( -22.14074124539699895, 0.09905289585522827900, -59.60992214895627939 ) ) ;
#162477 = EDGE_LOOP ( 'NONE', ( #128798, #34913, #83560, #153856 ) ) ;
#162478 = DIRECTION ( 'NONE',  ( 1.000000000000000000, 0.000000000000000000, -0.000000000000000000 ) ) ;
#162480 = ORIENTED_EDGE ( 'NONE', *, *, #238701, .F. ) ;
#162479 = CARTESIAN_POINT ( 'NONE',  ( 21.14999999999999858, 67.21339244341174890, -90.77310748452437394 ) ) ;
#162481 = CARTESIAN_POINT ( 'NONE',  ( 18.50000972452444969, 10.29326151435342851, -172.9592822510414578 ) ) ;
#162483 = EDGE_CURVE ( 'NONE', #210308, #130026, #74651, .T. ) ;
#162482 = CARTESIAN_POINT ( 'NONE',  ( -18.59117750673696889, 10.33248238083634796, -72.59484654391314962 ) ) ;
#162484 = CARTESIAN_POINT ( 'NONE',  ( -21.05000000000000071, 1.835341550235567887, -78.55515129256302487 ) ) ;
#162485 = EDGE_LOOP ( 'NONE', ( #150135, #92223, #61879, #249088, #164627, #115994, #143451 ) ) ;
#162487 = CARTESIAN_POINT ( 'NONE',  ( -20.85000000000000142, -11.74999999998884448, -100.5000000000000426 ) ) ;
#162486 = CARTESIAN_POINT ( 'NONE',  ( -17.05016517656263275, 9.950000000011140600, -121.3273020039994634 ) ) ;
#162489 = ADVANCED_FACE ( 'NONE', ( #173569 ), #74451, .T. ) ;
#162488 = CARTESIAN_POINT ( 'NONE',  ( -12.92414019175886430, 66.58236703690553782, -84.87415901879208491 ) ) ;
#162490 = TOROIDAL_SURFACE ( 'NONE', #104370, 3.899999999999999467, 0.1000000000000000056 ) ;
#162491 = LINE ( 'NONE', #3378, #214357 ) ;
#162492 = DIRECTION ( 'NONE',  ( 0.000000000000000000, 0.000000000000000000, 1.000000000000000000 ) ) ;
#162493 = DIRECTION ( 'NONE',  ( -1.000000000000000000, -0.000000000000000000, -0.000000000000000000 ) ) ;
#162494 = CIRCLE ( 'NONE', #191549, 0.09999999999999939493 ) ;
#162495 = VERTEX_POINT ( 'NONE', #251763 ) ;
#162496 = EDGE_LOOP ( 'NONE', ( #247690, #54716, #219326, #47290 ) ) ;
#162497 = ORIENTED_EDGE ( 'NONE', *, *, #159921, .T. ) ;
#162498 = EDGE_CURVE ( 'NONE', #37447, #119237, #28869, .T. ) ;
#162499 = DIRECTION ( 'NONE',  ( 0.7071067811865456854, 0.7071067811865493491, 4.937700262164544098E-15 ) ) ;
#162500 = EDGE_CURVE ( 'NONE', #201217, #221407, #220369, .T. ) ;
#162501 = ORIENTED_EDGE ( 'NONE', *, *, #125872, .F. ) ;
#162503 = DIRECTION ( 'NONE',  ( 0.000000000000000000, -0.9908441862701605762, 0.1350103645451835310 ) ) ;
#162502 = AXIS2_PLACEMENT_3D ( 'NONE', #72108, #51211, #108650 ) ;
#162504 = EDGE_LOOP ( 'NONE', ( #183924, #129082, #237200, #85620 ) ) ;
#162505 = CYLINDRICAL_SURFACE ( 'NONE', #148486, 0.1000000000000028644 ) ;
#162506 = DIRECTION ( 'NONE',  ( -0.000000000000000000, 1.000000000000000000, 1.626303258728266709E-15 ) ) ;
#162507 = VECTOR ( 'NONE', #108009, 1000.000000000000000 ) ;
#162508 = ORIENTED_EDGE ( 'NONE', *, *, #231633, .T. ) ;
#162509 = CARTESIAN_POINT ( 'NONE',  ( 13.22461703343584638, 9.436662931810237964, -152.3230367322948950 ) ) ;
#162510 =( NAMED_UNIT ( * ) PLANE_ANGLE_UNIT ( ) SI_UNIT ( $, .RADIAN. ) );
#162512 = ORIENTED_EDGE ( 'NONE', *, *, #99537, .F. ) ;
#162511 = VECTOR ( 'NONE', #66942, 1000.000000000000114 ) ;
#162513 = ADVANCED_FACE ( 'NONE', ( #11898 ), #95449, .F. ) ;
#162514 = ORIENTED_EDGE ( 'NONE', *, *, #187468, .F. ) ;
#162515 = EDGE_CURVE ( 'NONE', #100678, #115794, #250472, .T. ) ;
#162516 = AXIS2_PLACEMENT_3D ( 'NONE', #54749, #155182, #203251 ) ;
#162517 = ORIENTED_EDGE ( 'NONE', *, *, #76590, .T. ) ;
#162518 = AXIS2_PLACEMENT_3D ( 'NONE', #103442, #21389, #163446 ) ;
#162519 = AXIS2_PLACEMENT_3D ( 'NONE', #161888, #125314, #27532 ) ;
#162520 = CARTESIAN_POINT ( 'NONE',  ( -18.59999999999999787, 71.84303044094815505, -225.1053209871248271 ) ) ;
#162521 = DIRECTION ( 'NONE',  ( 1.000000000000000000, 0.000000000000000000, 0.000000000000000000 ) ) ;
#162522 = DIRECTION ( 'NONE',  ( -1.000000000000000000, 0.000000000000000000, 0.000000000000000000 ) ) ;
#162523 = CARTESIAN_POINT ( 'NONE',  ( -18.35235881385853318, 20.70033119311990077, -227.9867209999219426 ) ) ;
#162524 = CARTESIAN_POINT ( 'NONE',  ( -21.09610168723073897, 61.06592963697848830, -234.2178341264986159 ) ) ;
#162525 = LINE ( 'NONE', #142911, #55289 ) ;
#162527 = CARTESIAN_POINT ( 'NONE',  ( 21.05000000000000071, 87.65000000001194280, -103.0231074845242318 ) ) ;
#162526 = CYLINDRICAL_SURFACE ( 'NONE', #116530, 0.5000000000000004441 ) ;
#162528 = DIRECTION ( 'NONE',  ( 0.000000000000000000, -1.000000000000000000, 0.000000000000000000 ) ) ;
#162530 = ORIENTED_EDGE ( 'NONE', *, *, #101950, .F. ) ;
#162529 = DIRECTION ( 'NONE',  ( 0.000000000000000000, -0.9876197685951265681, -0.1568667991644790149 ) ) ;
#162531 = CARTESIAN_POINT ( 'NONE',  ( -16.94445028196808778, 12.44605341304038859, -211.1922452800140775 ) ) ;
#162532 = DIRECTION ( 'NONE',  ( 3.265361837132813093E-16, 1.000000000000000000, 6.982962677686266711E-15 ) ) ;
#162533 = ORIENTED_EDGE ( 'NONE', *, *, #14581, .T. ) ;
#162534 = CARTESIAN_POINT ( 'NONE',  ( 20.12500000000000000, 9.750000000011153745, -41.61177128211428311 ) ) ;
#162535 = CARTESIAN_POINT ( 'NONE',  ( -21.09610168723073542, 69.62104428478687623, -69.55669699141586193 ) ) ;
#162536 = DIRECTION ( 'NONE',  ( -4.448008912761043807E-16, 1.000000000000000000, 0.000000000000000000 ) ) ;
#162537 = ORIENTED_EDGE ( 'NONE', *, *, #193929, .T. ) ;
#162538 = EDGE_CURVE ( 'NONE', #249207, #174346, #191149, .T. ) ;
#162539 = CIRCLE ( 'NONE', #50080, 0.09999999999999939493 ) ;
#162540 = ADVANCED_FACE ( 'NONE', ( #135651 ), #54829, .F. ) ;
#162541 = DIRECTION ( 'NONE',  ( 0.000000000000000000, -0.4721928772777346794, -0.8814952561688431665 ) ) ;
#162542 = CARTESIAN_POINT ( 'NONE',  ( -18.41353343127310893, 78.24072131640579641, -231.5548844243369615 ) ) ;
#162543 = EDGE_LOOP ( 'NONE', ( #3695, #249572, #127706, #113814, #153384 ) ) ;
#162544 = ORIENTED_EDGE ( 'NONE', *, *, #31808, .F. ) ;
#162545 = DIRECTION ( 'NONE',  ( 0.000000000000000000, 0.9126074666063767049, 0.4088369013363286619 ) ) ;
#162546 = ORIENTED_EDGE ( 'NONE', *, *, #206112, .F. ) ;
#162547 = CARTESIAN_POINT ( 'NONE',  ( 21.00023020733438273, 6.390869245278871347, -67.00000000000004263 ) ) ;
#162548 = CARTESIAN_POINT ( 'NONE',  ( -18.31331870001081086, -9.536294719169568168, -174.3685786909853732 ) ) ;
#162549 = CARTESIAN_POINT ( 'NONE',  ( 23.25000000000000000, -9.599999999988845900, -43.39396912265245021 ) ) ;
#162551 = EDGE_CURVE ( 'NONE', #6193, #62328, #71864, .T. ) ;
#162550 = DIRECTION ( 'NONE',  ( -0.000000000000000000, -0.1350103645451807555, -0.9908441862701610203 ) ) ;
#162552 = ORIENTED_EDGE ( 'NONE', *, *, #240429, .F. ) ;
#162553 = CIRCLE ( 'NONE', #233289, 4.299999999999956302 ) ;
#162554 = DIRECTION ( 'NONE',  ( -1.000000000000000000, -0.000000000000000000, -0.000000000000000000 ) ) ;
#162555 = CARTESIAN_POINT ( 'NONE',  ( -18.50000000000000000, 77.16412189325286874, -61.60825939895269698 ) ) ;
#162556 = AXIS2_PLACEMENT_3D ( 'NONE', #220136, #178463, #197985 ) ;
#162558 = EDGE_CURVE ( 'NONE', #118915, #170795, #216238, .T. ) ;
#162557 = CARTESIAN_POINT ( 'NONE',  ( 18.49999999999999289, 10.25000000001115730, -192.1499999999999773 ) ) ;
#162559 = CARTESIAN_POINT ( 'NONE',  ( 21.05000000000000071, 8.776282895303634035, -41.98800072158436336 ) ) ;
#162560 = AXIS2_PLACEMENT_3D ( 'NONE', #44195, #81985, #182425 ) ;
#162561 = ORIENTED_EDGE ( 'NONE', *, *, #157174, .F. ) ;
#162563 = ORIENTED_EDGE ( 'NONE', *, *, #207417, .T. ) ;
#162562 = DIRECTION ( 'NONE',  ( 1.000000000000000000, 0.000000000000000000, 0.000000000000000000 ) ) ;
#162564 = DIRECTION ( 'NONE',  ( 0.000000000000000000, 0.000000000000000000, 1.000000000000000000 ) ) ;
#162565 = DIRECTION ( 'NONE',  ( -1.000000000000000000, 0.000000000000000000, 0.000000000000000000 ) ) ;
#162566 = EDGE_CURVE ( 'NONE', #115264, #126560, #120436, .T. ) ;
#162567 = CARTESIAN_POINT ( 'NONE',  ( -16.89318236219975589, 9.951535257886286345, -87.85512963210589987 ) ) ;
#162568 = CARTESIAN_POINT ( 'NONE',  ( 22.47071067811865319, 68.27992525551434255, -170.1221999392270163 ) ) ;
#162569 = DIRECTION ( 'NONE',  ( -1.000000000000000000, -2.952720810173289112E-16, 0.000000000000000000 ) ) ;
#162570 = AXIS2_PLACEMENT_3D ( 'NONE', #219256, #79728, #60181 ) ;
#162571 = EDGE_LOOP ( 'NONE', ( #204113, #112586, #36996, #119963 ) ) ;
#162572 = CARTESIAN_POINT ( 'NONE',  ( 20.95512820512821150, 61.85802300103158302, -221.7569547192959476 ) ) ;
#162573 = TOROIDAL_SURFACE ( 'NONE', #50107, 4.150000000000000355, 0.1000000000000000056 ) ;
#162574 = DIRECTION ( 'NONE',  ( -0.000000000000000000, -0.000000000000000000, -1.000000000000000000 ) ) ;
#162575 = CARTESIAN_POINT ( 'NONE',  ( -21.05000000000000071, -11.41227409413852989, -36.50000000000000711 ) ) ;
#162576 = CARTESIAN_POINT ( 'NONE',  ( 18.59999999999999076, 64.25000000001277556, -215.2731074845244450 ) ) ;
#162578 = AXIS2_PLACEMENT_3D ( 'NONE', #124014, #43187, #243938 ) ;
#162577 = DIRECTION ( 'NONE',  ( 0.000000000000000000, 1.000000000000000000, -0.000000000000000000 ) ) ;
#162579 = DIRECTION ( 'NONE',  ( 1.000000000000000000, -7.304098846218134667E-16, -5.100424963727255829E-30 ) ) ;
#162580 = AXIS2_PLACEMENT_3D ( 'NONE', #23684, #103167, #104442 ) ;
#162581 = ORIENTED_EDGE ( 'NONE', *, *, #11929, .T. ) ;
#162582 = ORIENTED_EDGE ( 'NONE', *, *, #43645, .T. ) ;
#162583 = DIRECTION ( 'NONE',  ( 1.000000000000000000, 0.000000000000000000, 0.000000000000000000 ) ) ;
#162584 = CARTESIAN_POINT ( 'NONE',  ( -22.48660254037843487, 11.65000000001115588, -133.9500000000000455 ) ) ;
#162585 = CYLINDRICAL_SURFACE ( 'NONE', #193006, 0.09999999999998898659 ) ;
#162586 = FACE_OUTER_BOUND ( 'NONE', #4303, .T. ) ;
#162587 = ORIENTED_EDGE ( 'NONE', *, *, #112561, .F. ) ;
#162588 = DIRECTION ( 'NONE',  ( 0.000000000000000000, 1.000000000000000000, 0.000000000000000000 ) ) ;
#162589 = LINE ( 'NONE', #66031, #117621 ) ;
#162590 = DIRECTION ( 'NONE',  ( 1.000000000000000000, 0.000000000000000000, 0.000000000000000000 ) ) ;
#162591 = ORIENTED_EDGE ( 'NONE', *, *, #148255, .T. ) ;
#162592 = DIRECTION ( 'NONE',  ( 1.000000000000000000, 0.000000000000000000, -0.000000000000000000 ) ) ;
#162593 = EDGE_LOOP ( 'NONE', ( #101945, #30968, #229954, #135810, #148655, #137416, #227698, #46759 ) ) ;
#162594 = CARTESIAN_POINT ( 'NONE',  ( -21.14999999999999858, 1.611925955256642951, -230.7774450549719916 ) ) ;
#162595 = CARTESIAN_POINT ( 'NONE',  ( 21.05000000000000426, 0.03486800301310592765, 6.270085863689147665 ) ) ;
#162596 = DIRECTION ( 'NONE',  ( 0.000000000000000000, 0.1350103645451876666, -0.9908441862701600211 ) ) ;
#162597 = DIRECTION ( 'NONE',  ( 0.000000000000000000, -0.000000000000000000, 1.000000000000000000 ) ) ;
#162598 = CARTESIAN_POINT ( 'NONE',  ( -18.59999999999999787, -1.263275465206102233, -108.4018646667464481 ) ) ;
#162599 = CARTESIAN_POINT ( 'NONE',  ( -21.05000000000000071, 64.21185867012613357, -224.4479740254296303 ) ) ;
#162600 = CARTESIAN_POINT ( 'NONE',  ( 18.54999999999999716, 23.65833333334447985, -83.75000000000004263 ) ) ;
#162601 = CARTESIAN_POINT ( 'NONE',  ( 21.00023020733502932, 1.115541036281197940E-11, -94.10913075473168021 ) ) ;
#162602 = VECTOR ( 'NONE', #243433, 1000.000000000000000 ) ;
#162603 = LINE ( 'NONE', #100015, #696 ) ;
#162604 = TOROIDAL_SURFACE ( 'NONE', #191674, 0.2000000000000000111, 0.1000000000000000056 ) ;
#162605 = ADVANCED_FACE ( 'NONE', ( #189234 ), #170998, .F. ) ;
#162606 = DIRECTION ( 'NONE',  ( 0.000000000000000000, -0.4930308989874980785, -0.8700118002898462599 ) ) ;
#162607 = DIRECTION ( 'NONE',  ( 0.000000000000000000, 0.000000000000000000, 1.000000000000000000 ) ) ;
#162608 = VECTOR ( 'NONE', #184318, 1000.000000000000000 ) ;
#162609 = CARTESIAN_POINT ( 'NONE',  ( -21.05000000000000071, 69.45934304831041572, -69.42310748452437963 ) ) ;
#162610 = DIRECTION ( 'NONE',  ( 0.000000000000000000, -1.000000000000000000, 0.000000000000000000 ) ) ;
#162611 = AXIS2_PLACEMENT_3D ( 'NONE', #240824, #102548, #182134 ) ;
#162612 = ORIENTED_EDGE ( 'NONE', *, *, #17025, .T. ) ;
#162613 = CARTESIAN_POINT ( 'NONE',  ( 21.05000000000000426, 6.299230910086890844, 0.09843749999999837352 ) ) ;
#162614 = CYLINDRICAL_SURFACE ( 'NONE', #183503, 0.09999999999999939493 ) ;
#162615 = EDGE_CURVE ( 'NONE', #53042, #34471, #37205, .T. ) ;
#162616 = ORIENTED_EDGE ( 'NONE', *, *, #99045, .T. ) ;
#162617 = LINE ( 'NONE', #143015, #209881 ) ;
#162618 = CARTESIAN_POINT ( 'NONE',  ( 21.09787244211748103, 11.17890107025148261, -211.0915125386900968 ) ) ;
#162620 = EDGE_CURVE ( 'NONE', #77834, #251907, #70545, .T. ) ;
#162619 = AXIS2_PLACEMENT_3D ( 'NONE', #170950, #65370, #210039 ) ;
#162621 = DIRECTION ( 'NONE',  ( -1.000000000000000000, -0.000000000000000000, -0.000000000000000000 ) ) ;
#162622 = VERTEX_POINT ( 'NONE', #133110 ) ;
#162623 = DIRECTION ( 'NONE',  ( -2.578261006436899437E-14, -0.1350103645451973811, 0.9908441862701586889 ) ) ;
#162624 = CARTESIAN_POINT ( 'NONE',  ( -23.25000000000000000, -0.8618440306552699326, -197.0427629756619297 ) ) ;
#162625 = EDGE_LOOP ( 'NONE', ( #32478, #119159, #162779, #131318 ) ) ;
#162626 = VERTEX_POINT ( 'NONE', #169707 ) ;
#162627 = CARTESIAN_POINT ( 'NONE',  ( -18.79999999999999716, 7.986648289447971116, 1.311673547813416718 ) ) ;
#162628 = EDGE_CURVE ( 'NONE', #109963, #66884, #211365, .T. ) ;
#162629 = VERTEX_POINT ( 'NONE', #113539 ) ;
#162630 = ADVANCED_FACE ( 'NONE', ( #93964 ), #228746, .T. ) ;
#162631 = CARTESIAN_POINT ( 'NONE',  ( -17.22767730081888971, 22.02731797329168018, -229.9728559097052312 ) ) ;
#162632 = DIRECTION ( 'NONE',  ( 0.000000000000000000, 0.9126074666063751506, 0.4088369013363322146 ) ) ;
#162633 = DIRECTION ( 'NONE',  ( -1.000000000000000000, 0.000000000000000000, 0.000000000000000000 ) ) ;
#162635 = DIRECTION ( 'NONE',  ( 0.000000000000000000, 0.000000000000000000, 1.000000000000000000 ) ) ;
#162634 = UNCERTAINTY_MEASURE_WITH_UNIT (LENGTH_MEASURE( 1.000000000000000082E-05 ), #72395, 'distance_accuracy_value', 'NONE');
#162636 = EDGE_CURVE ( 'NONE', #102720, #82676, #15756, .T. ) ;
#162637 = CARTESIAN_POINT ( 'NONE',  ( 20.94999999999999929, 76.00000000001173817, -73.62310748452429721 ) ) ;
#162638 = CARTESIAN_POINT ( 'NONE',  ( -18.59999999999999787, 77.68707439010378835, -149.3376804510659213 ) ) ;
#162639 = DIRECTION ( 'NONE',  ( 1.000000000000000000, 0.000000000000000000, 0.000000000000000000 ) ) ;
#162640 = CARTESIAN_POINT ( 'NONE',  ( 21.00000000000000000, 66.25000000001179501, -81.77310748452437394 ) ) ;
#162641 = DIRECTION ( 'NONE',  ( 0.000000000000000000, -7.056502275159894776E-15, 1.000000000000000000 ) ) ;
#162643 = VERTEX_POINT ( 'NONE', #96514 ) ;
#162642 = FACE_OUTER_BOUND ( 'NONE', #19686, .T. ) ;
#162644 = ORIENTED_EDGE ( 'NONE', *, *, #122270, .T. ) ;
#162646 = CYLINDRICAL_SURFACE ( 'NONE', #247834, 0.09999999999998898659 ) ;
#162645 = CARTESIAN_POINT ( 'NONE',  ( 18.39999999999999503, 64.25000000001207923, -123.8731074845243683 ) ) ;
#162648 = ORIENTED_EDGE ( 'NONE', *, *, #93735, .T. ) ;
#162647 = CARTESIAN_POINT ( 'NONE',  ( -16.87333278164111050, 61.13086903662161831, -220.5930452161097719 ) ) ;
#162649 = AXIS2_PLACEMENT_3D ( 'NONE', #125746, #185739, #205277 ) ;
#162650 = ORIENTED_EDGE ( 'NONE', *, *, #121474, .F. ) ;
#162651 = DIRECTION ( 'NONE',  ( -1.020425574104004196E-15, -6.982962677686266711E-15, 1.000000000000000000 ) ) ;
#162652 = CARTESIAN_POINT ( 'NONE',  ( -23.25000000000000000, 18.41524492703432614, -237.0006385043383546 ) ) ;
#162653 = ADVANCED_FACE ( 'NONE', ( #255560 ), #257705, .T. ) ;
#162654 = DIRECTION ( 'NONE',  ( 1.000000000000000000, 0.000000000000000000, 0.000000000000000000 ) ) ;
#162655 = VECTOR ( 'NONE', #63073, 1000.000000000000000 ) ;
#162656 = LINE ( 'NONE', #199215, #40088 ) ;
#162657 = DIRECTION ( 'NONE',  ( 0.000000000000000000, -6.938893903907234689E-15, 1.000000000000000000 ) ) ;
#162658 = CARTESIAN_POINT ( 'NONE',  ( -21.45000000000000284, 44.77807522791015060, -237.4671205425215135 ) ) ;
#162659 = ADVANCED_FACE ( 'NONE', ( #61268 ), #41724, .T. ) ;
#162660 = DIRECTION ( 'NONE',  ( 0.000000000000000000, 0.2617529984165152257, 0.9651348961777124202 ) ) ;
#162661 = EDGE_LOOP ( 'NONE', ( #117500, #216668, #71262, #216093 ) ) ;
#162662 = ORIENTED_EDGE ( 'NONE', *, *, #565, .F. ) ;
#162663 = DIRECTION ( 'NONE',  ( 0.000000000000000000, -6.769652589177772835E-15, 1.000000000000000000 ) ) ;
#162664 = CIRCLE ( 'NONE', #146079, 0.1999999999999996503 ) ;
#162665 = ORIENTED_EDGE ( 'NONE', *, *, #191450, .T. ) ;
#162666 = DIRECTION ( 'NONE',  ( 1.000000000000000000, 0.000000000000000000, 0.000000000000000000 ) ) ;
#162668 = ORIENTED_EDGE ( 'NONE', *, *, #151209, .F. ) ;
#162667 = VECTOR ( 'NONE', #28289, 1000.000000000000000 ) ;
#162669 = DIRECTION ( 'NONE',  ( 1.000000000000000000, -3.265361837132813093E-16, -2.280189983783949500E-30 ) ) ;
#162670 = TOROIDAL_SURFACE ( 'NONE', #66805, 11.65000000000000036, 0.1000000000000000056 ) ;
#162671 = CARTESIAN_POINT ( 'NONE',  ( 18.53691006697101784, 65.69784844286101588, -44.82090876722582351 ) ) ;
#162672 = CARTESIAN_POINT ( 'NONE',  ( -23.25000000000000000, 1.115600667400684642E-11, -167.4999999999999716 ) ) ;
#162673 = ORIENTED_EDGE ( 'NONE', *, *, #180931, .F. ) ;
#162674 = CIRCLE ( 'NONE', #241771, 0.09999999999999939493 ) ;
#162676 = VECTOR ( 'NONE', #77939, 1000.000000000000000 ) ;
#162675 = DIRECTION ( 'NONE',  ( 0.000000000000000000, -1.000000000000000000, -6.982962677686265922E-15 ) ) ;
#162677 = ORIENTED_EDGE ( 'NONE', *, *, #137878, .F. ) ;
#162678 = CARTESIAN_POINT ( 'NONE',  ( 22.46250603428203618, 0.02114417614996233138, -122.3501369026599264 ) ) ;
#162679 = DIRECTION ( 'NONE',  ( 0.000000000000000000, 0.000000000000000000, 1.000000000000000000 ) ) ;
#162680 = LINE ( 'NONE', #244758, #125779 ) ;
#162681 = FACE_OUTER_BOUND ( 'NONE', #44820, .T. ) ;
#162682 = ORIENTED_EDGE ( 'NONE', *, *, #206567, .T. ) ;
#162683 = CARTESIAN_POINT ( 'NONE',  ( -20.94999999999999929, 64.25000000001189449, -96.18150679462726771 ) ) ;
#162684 = ORIENTED_EDGE ( 'NONE', *, *, #108338, .F. ) ;
#162687 = VERTEX_POINT ( 'NONE', #217747 ) ;
#162686 = CARTESIAN_POINT ( 'NONE',  ( -21.04999999999994387, 76.00000000001119815, -36.02310748452479316 ) ) ;
#162685 = DIRECTION ( 'NONE',  ( -0.000000000000000000, 0.2617529984165031243, 0.9651348961777157509 ) ) ;
#162688 = VECTOR ( 'NONE', #2167, 1000.000000000000000 ) ;
#162689 = FACE_OUTER_BOUND ( 'NONE', #149281, .T. ) ;
#162690 = AXIS2_PLACEMENT_3D ( 'NONE', #169977, #112538, #175119 ) ;
#162692 = ORIENTED_EDGE ( 'NONE', *, *, #152792, .F. ) ;
#162691 = VECTOR ( 'NONE', #48024, 1000.000000000000000 ) ;
#162693 = VECTOR ( 'NONE', #170585, 1000.000000000000000 ) ;
#162694 = AXIS2_PLACEMENT_3D ( 'NONE', #225363, #84535, #183699 ) ;
#162695 = EDGE_CURVE ( 'NONE', #161815, #231129, #32957, .T. ) ;
#162696 = CARTESIAN_POINT ( 'NONE',  ( -23.15000000000000213, 72.62993014539878800, -215.9492192728129965 ) ) ;
#162697 = ORIENTED_EDGE ( 'NONE', *, *, #118850, .F. ) ;
#162699 = EDGE_CURVE ( 'NONE', #109083, #42440, #139504, .T. ) ;
#162698 = DIRECTION ( 'NONE',  ( 0.000000000000000000, -0.2128009952263403282, 0.9770955615653358350 ) ) ;
#162700 = FACE_OUTER_BOUND ( 'NONE', #177737, .T. ) ;
#162701 = ADVANCED_FACE ( 'NONE', ( #219041 ), #157845, .F. ) ;
#162702 = CARTESIAN_POINT ( 'NONE',  ( -14.00000000000000178, 66.15000000001155911, -52.77310748452439526 ) ) ;
#162703 = ADVANCED_FACE ( 'NONE', ( #256840 ), #80804, .T. ) ;
#162704 = CARTESIAN_POINT ( 'NONE',  ( -20.94999999999999929, 7.031312794766356511, -204.6091509382272591 ) ) ;
#162705 = DIRECTION ( 'NONE',  ( 6.938893903907030216E-14, 0.000000000000000000, -1.000000000000000000 ) ) ;
#162706 = CIRCLE ( 'NONE', #196032, 0.2000000000000104194 ) ;
#162708 = ORIENTED_EDGE ( 'NONE', *, *, #39652, .T. ) ;
#162707 = EDGE_CURVE ( 'NONE', #41827, #28455, #132883, .T. ) ;
#162709 = FACE_OUTER_BOUND ( 'NONE', #138250, .T. ) ;
#162710 = CARTESIAN_POINT ( 'NONE',  ( 20.94999999999999929, -11.48912529306489994, -197.8999999999999773 ) ) ;
#162711 = CARTESIAN_POINT ( 'NONE',  ( 21.14999999999999858, 13.98997548377052524, -210.4902890347897255 ) ) ;
#162712 = EDGE_CURVE ( 'NONE', #14945, #199652, #119991, .T. ) ;
#162713 = ORIENTED_EDGE ( 'NONE', *, *, #96140, .T. ) ;
#162714 = CARTESIAN_POINT ( 'NONE',  ( -22.39999999999999858, 0.3085173699977072914, -229.9658011520297691 ) ) ;
#162717 = EDGE_CURVE ( 'NONE', #77018, #252194, #41317, .T. ) ;
#162716 = ADVANCED_FACE ( 'NONE', ( #58674 ), #7984, .T. ) ;
#162715 = VERTEX_POINT ( 'NONE', #22162 ) ;
#162718 = CARTESIAN_POINT ( 'NONE',  ( -18.40000000000000213, 59.52583735386146202, -220.6583686759552734 ) ) ;
#162719 = DIRECTION ( 'NONE',  ( 6.938893903907991995E-14, 0.000000000000000000, -1.000000000000000000 ) ) ;
#162720 = CARTESIAN_POINT ( 'NONE',  ( 20.94999999999999929, 84.73084112150739600, -126.9250327655398962 ) ) ;
#162722 = VERTEX_POINT ( 'NONE', #161674 ) ;
#162721 = CARTESIAN_POINT ( 'NONE',  ( -16.94445028196808778, 9.992063609708889516, -146.6073301784184935 ) ) ;
#162723 = CARTESIAN_POINT ( 'NONE',  ( -21.05000000000000071, 11.65000000001115232, -174.2838656629781156 ) ) ;
#162724 = AXIS2_PLACEMENT_3D ( 'NONE', #26094, #67769, #148605 ) ;
#162725 = DIRECTION ( 'NONE',  ( 0.000000000000000000, 0.000000000000000000, -1.000000000000000000 ) ) ;
#162726 = EDGE_CURVE ( 'NONE', #13877, #189000, #181235, .T. ) ;
#162727 = CARTESIAN_POINT ( 'NONE',  ( 20.94999999999999929, -3.770473190032740174, -225.9805569534692324 ) ) ;
#162728 = VERTEX_POINT ( 'NONE', #2559 ) ;
#162729 = DIRECTION ( 'NONE',  ( 1.000000000000000000, 0.000000000000000000, 0.000000000000000000 ) ) ;
#162730 = DIRECTION ( 'NONE',  ( 0.000000000000000000, 0.4088369013363281068, -0.9126074666063770380 ) ) ;
#162732 = ORIENTED_EDGE ( 'NONE', *, *, #196100, .F. ) ;
#162731 = ADVANCED_FACE ( 'NONE', ( #198204 ), #138208, .T. ) ;
#162734 = EDGE_CURVE ( 'NONE', #186448, #68820, #82081, .T. ) ;
#162733 = CARTESIAN_POINT ( 'NONE',  ( -21.53752568622129004, 65.35928353582079353, -242.3794047578559514 ) ) ;
#162735 = AXIS2_PLACEMENT_3D ( 'NONE', #94394, #253464, #154421 ) ;
#162736 = EDGE_LOOP ( 'NONE', ( #212639, #229097, #172147, #93947 ) ) ;
#162737 = EDGE_CURVE ( 'NONE', #224643, #218145, #237106, .T. ) ;
#162739 = CARTESIAN_POINT ( 'NONE',  ( -18.59999999999999787, 11.65000000001115232, -141.0148057706540214 ) ) ;
#162738 = AXIS2_PLACEMENT_3D ( 'NONE', #242339, #59829, #23329 ) ;
#162740 = ORIENTED_EDGE ( 'NONE', *, *, #237408, .F. ) ;
#162742 = ORIENTED_EDGE ( 'NONE', *, *, #150030, .F. ) ;
#162741 = FACE_OUTER_BOUND ( 'NONE', #55311, .T. ) ;
#162743 = EDGE_CURVE ( 'NONE', #170736, #58594, #130709, .T. ) ;
#162746 = ORIENTED_EDGE ( 'NONE', *, *, #43392, .F. ) ;
#162745 = ORIENTED_EDGE ( 'NONE', *, *, #193242, .T. ) ;
#162744 = CARTESIAN_POINT ( 'NONE',  ( -15.55912972643740488, 12.73329240860610234, -219.5655768140866542 ) ) ;
#162747 = CIRCLE ( 'NONE', #179324, 0.09999999999999609201 ) ;
#162748 = DIRECTION ( 'NONE',  ( 0.000000000000000000, -6.982962677686266711E-15, 1.000000000000000000 ) ) ;
#162749 = FACE_OUTER_BOUND ( 'NONE', #140825, .T. ) ;
#162750 = DIRECTION ( 'NONE',  ( 1.000000000000000000, 0.000000000000000000, 0.000000000000000000 ) ) ;
#162752 = CARTESIAN_POINT ( 'NONE',  ( -16.92570016628983964, 9.958788957739857395, -20.87934932996099846 ) ) ;
#162751 = DIRECTION ( 'NONE',  ( 0.000000000000000000, 6.982962677686266711E-15, -1.000000000000000000 ) ) ;
#162753 = DIRECTION ( 'NONE',  ( 1.000000000000000000, 0.000000000000000000, 0.000000000000000000 ) ) ;
#162754 = CIRCLE ( 'NONE', #4320, 0.09999999999999939493 ) ;
#162755 = CARTESIAN_POINT ( 'NONE',  ( -22.59999999999999787, 25.89494711235935043, -254.2627752153468350 ) ) ;
#162756 = AXIS2_PLACEMENT_3D ( 'NONE', #77796, #256386, #119528 ) ;
#162757 = DIRECTION ( 'NONE',  ( 0.000000000000000000, 0.2617529984165033463, 0.9651348961777157509 ) ) ;
#162759 = DIRECTION ( 'NONE',  ( -0.000000000000000000, 1.000000000000000000, 6.982962677686266711E-15 ) ) ;
#162758 = CARTESIAN_POINT ( 'NONE',  ( 23.15000000000000213, 87.48912529308798014, -106.1231074845242262 ) ) ;
#162761 = VERTEX_POINT ( 'NONE', #242455 ) ;
#162760 = CIRCLE ( 'NONE', #25210, 0.09999999999998902822 ) ;
#162762 = ORIENTED_EDGE ( 'NONE', *, *, #102149, .F. ) ;
#162763 = CARTESIAN_POINT ( 'NONE',  ( -21.05315837410545043, 64.25000000001175238, -76.36475148275638958 ) ) ;
#162765 = ORIENTED_EDGE ( 'NONE', *, *, #158330, .T. ) ;
#162764 = DIRECTION ( 'NONE',  ( 1.000000000000000000, 0.000000000000000000, 0.000000000000000000 ) ) ;
#162766 = VERTEX_POINT ( 'NONE', #87228 ) ;
#162767 = DIRECTION ( 'NONE',  ( 1.000000000000000000, 0.000000000000000000, 0.000000000000000000 ) ) ;
#162768 = ORIENTED_EDGE ( 'NONE', *, *, #127284, .F. ) ;
#162769 = CARTESIAN_POINT ( 'NONE',  ( -21.09107601085562322, 69.63612202465165524, -136.5624146492413331 ) ) ;
#162770 = ORIENTED_EDGE ( 'NONE', *, *, #242838, .F. ) ;
#162771 = AXIS2_PLACEMENT_3D ( 'NONE', #144370, #160143, #100114 ) ;
#162772 = PLANE ( 'NONE',  #181165 ) ;
#162773 = DIRECTION ( 'NONE',  ( 1.000000000000000000, 0.000000000000000000, 0.000000000000000000 ) ) ;
#162775 = ORIENTED_EDGE ( 'NONE', *, *, #95046, .T. ) ;
#162774 = ORIENTED_EDGE ( 'NONE', *, *, #66657, .F. ) ;
#162776 = ORIENTED_EDGE ( 'NONE', *, *, #234230, .T. ) ;
#162777 = DIRECTION ( 'NONE',  ( 1.000000000000000000, 0.000000000000000000, 0.000000000000000000 ) ) ;
#162778 = ORIENTED_EDGE ( 'NONE', *, *, #221347, .F. ) ;
#162779 = ORIENTED_EDGE ( 'NONE', *, *, #110552, .F. ) ;
#162780 = DIRECTION ( 'NONE',  ( -1.000000000000000000, 0.000000000000000000, 0.000000000000000000 ) ) ;
#162781 = DIRECTION ( 'NONE',  ( 0.000000000000000000, 0.5907332058517377193, -0.8068669527896954463 ) ) ;
#162783 = ORIENTED_EDGE ( 'NONE', *, *, #243650, .T. ) ;
#162782 = DIRECTION ( 'NONE',  ( 1.000000000000000000, -0.000000000000000000, -0.000000000000000000 ) ) ;
#162784 = B_SPLINE_CURVE_WITH_KNOTS ( 'NONE', 3,
 ( #150831, #136364, #71320, #94699, #230366, #93414, #51701, #253763, #131265, #95973 ),
 .UNSPECIFIED., .F., .F.,
 ( 4, 2, 2, 2, 4 ),
 ( 0.000000000000000000, 0.0001660831991682683057, 0.0002491247987523607845, 0.0002906455985444082843, 0.0003321663983364558383 ),
 .UNSPECIFIED. ) ;
#162786 = DIRECTION ( 'NONE',  ( 0.000000000000000000, 0.8660254037844378194, 0.5000000000000016653 ) ) ;
#162785 = LINE ( 'NONE', #205734, #153237 ) ;
#162787 = LINE ( 'NONE', #47942, #61746 ) ;
#162788 = DIRECTION ( 'NONE',  ( 0.000000000000000000, 0.2128009952263609783, -0.9770955615653315052 ) ) ;
#162789 = CARTESIAN_POINT ( 'NONE',  ( -21.17356465864818205, 6.422803126252873973, -66.90108875898617669 ) ) ;
#162790 = ORIENTED_EDGE ( 'NONE', *, *, #105404, .T. ) ;
#162791 = VERTEX_POINT ( 'NONE', #182520 ) ;
#162793 = CIRCLE ( 'NONE', #195743, 0.09999999999998898659 ) ;
#162792 = CARTESIAN_POINT ( 'NONE',  ( -23.15000000000000213, 1.115600667400684642E-11, -100.5000000000000284 ) ) ;
#162795 = EDGE_CURVE ( 'NONE', #200485, #91017, #194865, .T. ) ;
#162794 = DIRECTION ( 'NONE',  ( 1.000000000000000000, 0.000000000000000000, 0.000000000000000000 ) ) ;
#162796 = AXIS2_PLACEMENT_3D ( 'NONE', #22060, #141980, #198110 ) ;
#162797 = VECTOR ( 'NONE', #27925, 1000.000000000000114 ) ;
#162798 = AXIS2_PLACEMENT_3D ( 'NONE', #55698, #75341, #114439 ) ;
#162799 = ORIENTED_EDGE ( 'NONE', *, *, #25832, .F. ) ;
#162800 = CARTESIAN_POINT ( 'NONE',  ( 22.24259225415828567, 0.09906588346399246292, -26.00806212943458817 ) ) ;
#162801 = ADVANCED_FACE ( 'NONE', ( #46814 ), #187238, .T. ) ;
#162802 = CARTESIAN_POINT ( 'NONE',  ( -20.54999999999999716, 9.614325556249161409, -211.5456030694648746 ) ) ;
#162803 = VECTOR ( 'NONE', #37172, 1000.000000000000000 ) ;
#162804 = PLANE ( 'NONE',  #85041 ) ;
#162805 = ORIENTED_EDGE ( 'NONE', *, *, #247800, .F. ) ;
#162806 = EDGE_LOOP ( 'NONE', ( #6352, #164206, #213018, #50466 ) ) ;
#162807 = EDGE_CURVE ( 'NONE', #670, #244528, #233021, .T. ) ;
#162808 = CARTESIAN_POINT ( 'NONE',  ( 20.94999999999999929, -9.400000000000000355, -23.60603087734755690 ) ) ;
#162810 = EDGE_CURVE ( 'NONE', #3259, #73651, #24929, .T. ) ;
#162809 = CARTESIAN_POINT ( 'NONE',  ( -21.64999999999999858, 7.349999999999998757, -12.34999999999999964 ) ) ;
#162811 = VERTEX_POINT ( 'NONE', #166821 ) ;
#162812 = DIRECTION ( 'NONE',  ( 3.469446951953635646E-14, -0.9126074666063771490, -0.4088369013363281623 ) ) ;
#162813 = EDGE_LOOP ( 'NONE', ( #92985, #57385, #48948, #165051, #90537, #178141, #137975, #126190, #151200, #106185, #194648, #4579, #60266, #97278 ) ) ;
#162814 = DIRECTION ( 'NONE',  ( 0.000000000000000000, -0.8814952561688430555, 0.4721928772777346239 ) ) ;
#162815 = CARTESIAN_POINT ( 'NONE',  ( 20.96077737575347300, 64.37609936600742344, -143.3823155274180294 ) ) ;
#162817 = LINE ( 'NONE', #205764, #191817 ) ;
#162816 = DIRECTION ( 'NONE',  ( 1.000000000000000000, 0.000000000000000000, 0.000000000000000000 ) ) ;
#162818 = AXIS2_PLACEMENT_3D ( 'NONE', #106746, #28561, #49356 ) ;
#162819 = DIRECTION ( 'NONE',  ( -1.000000000000000000, 0.000000000000000000, -0.000000000000000000 ) ) ;
#162820 = DIRECTION ( 'NONE',  ( 1.000000000000000000, 0.000000000000000000, 0.000000000000000000 ) ) ;
#162821 = ORIENTED_EDGE ( 'NONE', *, *, #133528, .F. ) ;
#162822 = CARTESIAN_POINT ( 'NONE',  ( -16.78805706634180339, 63.08588851766376848, -213.1337219450663270 ) ) ;
#162823 = EDGE_CURVE ( 'NONE', #165929, #66231, #253827, .T. ) ;
#162825 = ORIENTED_EDGE ( 'NONE', *, *, #31721, .F. ) ;
#162824 = VERTEX_POINT ( 'NONE', #63838 ) ;
#162826 = ORIENTED_EDGE ( 'NONE', *, *, #243245, .T. ) ;
#162827 = EDGE_CURVE ( 'NONE', #37616, #224306, #178884, .T. ) ;
#162828 = VERTEX_POINT ( 'NONE', #122538 ) ;
#162829 = FACE_OUTER_BOUND ( 'NONE', #165352, .T. ) ;
#162830 = CARTESIAN_POINT ( 'NONE',  ( -21.05000000000000071, 1.115600667400684642E-11, -67.00000000000004263 ) ) ;
#162832 = DIRECTION ( 'NONE',  ( 2.952720810173289112E-16, -1.000000000000000000, 0.000000000000000000 ) ) ;
#162831 =( BOUNDED_SURFACE ( )  B_SPLINE_SURFACE ( 3, 2, ( 
 ( #230060, #227476, #147956 ),
 ( #247035, #192234, #48846 ),
 ( #51383, #128394, #210502 ),
 ( #89250, #108815, #130960 ),
 ( #31889, #73587, #111402 ),
 ( #91833, #168848, #12321 ) ),
 .UNSPECIFIED., .F., .F., .F. ) 
 B_SPLINE_SURFACE_WITH_KNOTS ( ( 4, 2, 4 ),
 ( 3, 3 ),
 ( 0.0001342700090130013102, 0.0002909192928057331620, 0.0004475685765984649595 ),
 ( 0.000000000000000000, 1.000000000000000000 ),
 .UNSPECIFIED. ) 
 GEOMETRIC_REPRESENTATION_ITEM ( )  RATIONAL_B_SPLINE_SURFACE ( (
 ( 1.000000000000000000, 0.7250110520819876836, 1.000000000000000000),
 ( 1.000000000000000000, 0.7257599279134849812, 1.000000000000000000),
 ( 1.000000000000000000, 0.7137594617283078424, 1.000000000000000000),
 ( 1.000000000000000000, 0.6959270178811023388, 1.000000000000000000),
 ( 1.000000000000000000, 0.6919879549338179281, 1.000000000000000000),
 ( 1.000000000000000000, 0.7071067811865494601, 1.000000000000000000) ) ) 
 REPRESENTATION_ITEM ( '' )  SURFACE ( )  );
#162833 = CARTESIAN_POINT ( 'NONE',  ( -20.64999999999999858, 2.000000000011154189, -188.1753780772378946 ) ) ;
#162834 = DIRECTION ( 'NONE',  ( 0.000000000000000000, 0.000000000000000000, -1.000000000000000000 ) ) ;
#162835 = VECTOR ( 'NONE', #25331, 1000.000000000000227 ) ;
#162837 = CARTESIAN_POINT ( 'NONE',  ( -22.47071067811865319, 0.09909245471376178227, -159.7799252555018938 ) ) ;
#162836 = CARTESIAN_POINT ( 'NONE',  ( -23.25000000000000355, 10.04999999999998295, -12.75000000000000178 ) ) ;
#162839 = EDGE_LOOP ( 'NONE', ( #9194, #168556, #89445, #60424 ) ) ;
#162838 = CARTESIAN_POINT ( 'NONE',  ( 23.25000000000000000, 6.550000000011156231, -179.8499999999999943 ) ) ;
#162840 = CARTESIAN_POINT ( 'NONE',  ( -21.05000000000000071, 6.257814610492677510, -167.4022097086907763 ) ) ;
#162841 = EDGE_LOOP ( 'NONE', ( #163045, #249846, #206607, #105874 ) ) ;
#162842 = CARTESIAN_POINT ( 'NONE',  ( 20.94999999999999929, 11.65000000001115943, -160.6583993101029648 ) ) ;
#162843 = ORIENTED_EDGE ( 'NONE', *, *, #254845, .F. ) ;
#162844 = ORIENTED_EDGE ( 'NONE', *, *, #252795, .F. ) ;
#162845 = CARTESIAN_POINT ( 'NONE',  ( 21.05000000000000071, 69.52293297888738266, -136.4231074845243938 ) ) ;
#162846 = AXIS2_PLACEMENT_3D ( 'NONE', #148117, #244634, #28200 ) ;
#162847 = CARTESIAN_POINT ( 'NONE',  ( 21.04999999999999716, 6.304455821947667182, -0.02103547654011554344 ) ) ;
#162848 = LINE ( 'NONE', #183684, #233445 ) ;
#162849 = EDGE_CURVE ( 'NONE', #100804, #220045, #44284, .T. ) ;
#162850 = CARTESIAN_POINT ( 'NONE',  ( 21.05000000000000071, 1.115600667400684642E-11, -134.0000000000000000 ) ) ;
#162851 = TOROIDAL_SURFACE ( 'NONE', #158561, 0.2000000000000000111, 0.1000000000000000056 ) ;
#162852 = EDGE_CURVE ( 'NONE', #96731, #5980, #103977, .T. ) ;
#162853 = B_SPLINE_CURVE_WITH_KNOTS ( 'NONE', 3,
 ( #193277, #78445, #94154, #237539, #15948, #96699, #176297, #138400, #217943, #219240 ),
 .UNSPECIFIED., .F., .F.,
 ( 4, 2, 2, 2, 4 ),
 ( 0.000000000000000000, 0.0001660831991682082409, 0.0002491247987523123749, 0.0002906455985443822092, 0.0003321663983364520978 ),
 .UNSPECIFIED. ) ;
#162854 = FACE_OUTER_BOUND ( 'NONE', #256537, .T. ) ;
#162855 = EDGE_LOOP ( 'NONE', ( #32024, #44086, #219528, #159791 ) ) ;
#162856 = VERTEX_POINT ( 'NONE', #65111 ) ;
#162857 = AXIS2_PLACEMENT_3D ( 'NONE', #220578, #144873, #142308 ) ;
#162858 = VERTEX_POINT ( 'NONE', #144640 ) ;
#162859 = DIRECTION ( 'NONE',  ( 0.000000000000000000, 1.000000000000000000, 6.982962677686266711E-15 ) ) ;
#162860 = CARTESIAN_POINT ( 'NONE',  ( -16.89268316805466341, 9.951721813253341153, -46.14424752145445296 ) ) ;
#162861 = CARTESIAN_POINT ( 'NONE',  ( -18.59999999999999787, 9.250000000000001776, -21.25000000000000000 ) ) ;
#162862 = SPHERICAL_SURFACE ( 'NONE', #250261, 0.1000000000000000056 ) ;
#162863 = DIRECTION ( 'NONE',  ( -0.000000000000000000, -0.000000000000000000, 1.000000000000000000 ) ) ;
#162865 = EDGE_CURVE ( 'NONE', #38016, #237011, #226749, .T. ) ;
#162864 = CARTESIAN_POINT ( 'NONE',  ( -16.79814274880124358, 66.05072745733455974, -90.37067444747638945 ) ) ;
#162866 = DIRECTION ( 'NONE',  ( -1.000000000000000000, -0.000000000000000000, 0.000000000000000000 ) ) ;
#162867 = B_SPLINE_CURVE_WITH_KNOTS ( 'NONE', 3,
 ( #225294, #141926, #83208, #102776, #182358, #123664, #25848, #204462, #162800, #84475 ),
 .UNSPECIFIED., .F., .F.,
 ( 4, 3, 3, 4 ),
 ( 3.469446951953614189E-18, 0.0002000000000008561227, 0.001000000000082977483, 0.001967863649483317639 ),
 .UNSPECIFIED. ) ;
#162868 = DIRECTION ( 'NONE',  ( 0.000000000000000000, 0.000000000000000000, 1.000000000000000000 ) ) ;
#162869 = FACE_OUTER_BOUND ( 'NONE', #161750, .T. ) ;
#162870 = EDGE_CURVE ( 'NONE', #181475, #188424, #191336, .T. ) ;
#162871 = CARTESIAN_POINT ( 'NONE',  ( -21.05000000000000071, 6.390846877240203838, -199.6081416912452937 ) ) ;
#162872 = FACE_OUTER_BOUND ( 'NONE', #74026, .T. ) ;
#162874 = EDGE_CURVE ( 'NONE', #234687, #186652, #183131, .T. ) ;
#162873 = AXIS2_PLACEMENT_3D ( 'NONE', #43640, #20229, #159736 ) ;
#162875 = DIRECTION ( 'NONE',  ( -1.836970198721029934E-16, -1.000000000000000000, -6.982962677686266711E-15 ) ) ;
#162876 = CIRCLE ( 'NONE', #96367, 0.1000000000000028644 ) ;
#162878 = VERTEX_POINT ( 'NONE', #8993 ) ;
#162877 = AXIS2_PLACEMENT_3D ( 'NONE', #190887, #153060, #236397 ) ;
#162879 = AXIS2_PLACEMENT_3D ( 'NONE', #112218, #195612, #235982 ) ;
#162880 = DIRECTION ( 'NONE',  ( -1.000000000000000000, -0.000000000000000000, -0.000000000000000000 ) ) ;
#162881 = ORIENTED_EDGE ( 'NONE', *, *, #2294, .F. ) ;
#162882 = EDGE_CURVE ( 'NONE', #142859, #127785, #88500, .T. ) ;
#162883 = AXIS2_PLACEMENT_3D ( 'NONE', #226117, #127049, #25400 ) ;
#162884 = CARTESIAN_POINT ( 'NONE',  ( -23.25000000000000355, 70.35000000001160458, -60.27310748452436684 ) ) ;
#162885 = FACE_OUTER_BOUND ( 'NONE', #106337, .T. ) ;
#162886 = DIRECTION ( 'NONE',  ( 1.000000000000000000, 0.000000000000000000, 0.000000000000000000 ) ) ;
#162887 = ORIENTED_EDGE ( 'NONE', *, *, #72390, .T. ) ;
#162888 = DIRECTION ( 'NONE',  ( 1.000000000000000000, -0.000000000000000000, -0.000000000000000000 ) ) ;
#162889 = ADVANCED_FACE ( 'NONE', ( #126373 ), #95625, .F. ) ;
#162890 = DIRECTION ( 'NONE',  ( 2.952720810173289112E-16, -1.000000000000000000, 0.000000000000000000 ) ) ;
#162891 = FACE_OUTER_BOUND ( 'NONE', #93603, .T. ) ;
#162892 = FACE_OUTER_BOUND ( 'NONE', #203676, .T. ) ;
#162893 = VECTOR ( 'NONE', #134937, 1000.000000000000000 ) ;
#162894 = CARTESIAN_POINT ( 'NONE',  ( 23.14999999999999503, 11.65000000001116298, -179.6499999999999773 ) ) ;
#162895 = VECTOR ( 'NONE', #60020, 1000.000000000000000 ) ;
#162896 = AXIS2_PLACEMENT_3D ( 'NONE', #222479, #240790, #43873 ) ;
#162897 = CYLINDRICAL_SURFACE ( 'NONE', #48876, 1.749999999999998002 ) ;
#162898 = CIRCLE ( 'NONE', #53955, 0.09999999999999939493 ) ;
#162899 = ORIENTED_EDGE ( 'NONE', *, *, #145237, .T. ) ;
#162900 = DIRECTION ( 'NONE',  ( 0.000000000000000000, -0.1568667991644693838, -0.9876197685951279004 ) ) ;
#162902 = VERTEX_POINT ( 'NONE', #24741 ) ;
#162901 = CARTESIAN_POINT ( 'NONE',  ( -23.39999999999994529, 74.16448838626247664, -47.62760213295649692 ) ) ;
#162903 = CARTESIAN_POINT ( 'NONE',  ( 22.49999999999999645, 0.04562336060759585726, -122.3494956614463405 ) ) ;
#162904 = EDGE_CURVE ( 'NONE', #240326, #84962, #27315, .T. ) ;
#162905 = CYLINDRICAL_SURFACE ( 'NONE', #3787, 0.5000000000000004441 ) ;
#162906 = SURFACE_SIDE_STYLE ('',( #83306 ) ) ;
#162907 =( BOUNDED_SURFACE ( )  B_SPLINE_SURFACE ( 3, 2, ( 
 ( #177434, #256882, #78283 ),
 ( #219077, #58709, #138249 ),
 ( #36, #77008, #19621 ),
 ( #120028, #217784, #99122 ) ),
 .UNSPECIFIED., .F., .F., .F. ) 
 B_SPLINE_SURFACE_WITH_KNOTS ( ( 4, 4 ),
 ( 3, 3 ),
 ( 5.727910411845712702, 5.983100554402348337 ),
 ( 0.000000000000000000, 1.000000000000000000 ),
 .UNSPECIFIED. ) 
 GEOMETRIC_REPRESENTATION_ITEM ( )  RATIONAL_B_SPLINE_SURFACE ( (
 ( 1.000000000000000000, 0.8946697475932152699, 1.000000000000000000),
 ( 1.000000000000000000, 0.9035312726220557922, 1.000000000000000000),
 ( 1.000000000000000000, 0.9104333467450282935, 1.000000000000000000),
 ( 1.000000000000000000, 0.9152888060719359675, 1.000000000000000000) ) ) 
 REPRESENTATION_ITEM ( '' )  SURFACE ( )  );
#162908 = ORIENTED_EDGE ( 'NONE', *, *, #30563, .T. ) ;
#162909 = CYLINDRICAL_SURFACE ( 'NONE', #117929, 4.049999999999998046 ) ;
#162910 = VECTOR ( 'NONE', #106602, 1000.000000000000114 ) ;
#162911 = CARTESIAN_POINT ( 'NONE',  ( -20.85000000000000142, 1.115600667400684642E-11, -200.9999999999999432 ) ) ;
#162912 = ORIENTED_EDGE ( 'NONE', *, *, #177464, .F. ) ;
#162913 = DIRECTION ( 'NONE',  ( -0.000000000000000000, -6.982962677686266711E-15, 1.000000000000000000 ) ) ;
#162914 = LINE ( 'NONE', #119944, #59176 ) ;
#162915 = ORIENTED_EDGE ( 'NONE', *, *, #49005, .F. ) ;
#162916 = ORIENTED_EDGE ( 'NONE', *, *, #146571, .T. ) ;
#162917 = CARTESIAN_POINT ( 'NONE',  ( 23.14999999999999858, 5.600000000011153389, -179.9052660189130677 ) ) ;
#162918 = DIRECTION ( 'NONE',  ( 0.000000000000000000, 0.000000000000000000, 1.000000000000000000 ) ) ;
#162919 = AXIS2_PLACEMENT_3D ( 'NONE', #140564, #41498, #57162 ) ;
#162920 = CARTESIAN_POINT ( 'NONE',  ( -22.94999999999999929, 0.000000000000000000, 0.000000000000000000 ) ) ;
#162921 = DIRECTION ( 'NONE',  ( 1.000000000000000000, 0.000000000000000000, 0.000000000000000000 ) ) ;
#162922 = CARTESIAN_POINT ( 'NONE',  ( -18.40000000000000213, 64.52683809664910086, -56.91452884076171159 ) ) ;
#162923 = FACE_OUTER_BOUND ( 'NONE', #13512, .T. ) ;
#162925 = CARTESIAN_POINT ( 'NONE',  ( -18.42554971533677843, -9.497159669426592288, -74.03982691354869417 ) ) ;
#162924 = CARTESIAN_POINT ( 'NONE',  ( 21.07928932188134041, -1.250084634897252522, -194.7953894783236990 ) ) ;
#162926 = DIRECTION ( 'NONE',  ( 0.000000000000000000, 0.000000000000000000, 1.000000000000000000 ) ) ;
#162927 = DIRECTION ( 'NONE',  ( 1.000000000000000000, 0.000000000000000000, 0.000000000000000000 ) ) ;
#162928 = DIRECTION ( 'NONE',  ( 0.000000000000000000, -7.056502275159890832E-15, 1.000000000000000000 ) ) ;
#162929 = CYLINDRICAL_SURFACE ( 'NONE', #252909, 0.09999999999999771572 ) ;
#162930 = ORIENTED_EDGE ( 'NONE', *, *, #62629, .T. ) ;
#162931 = EDGE_LOOP ( 'NONE', ( #131674, #204197, #230741, #218156 ) ) ;
#162932 = CARTESIAN_POINT ( 'NONE',  ( -20.54999999999999716, -11.74999999998884448, -117.2500000000000284 ) ) ;
#162933 = CARTESIAN_POINT ( 'NONE',  ( 20.99999999999999645, 60.24242455067834356, -224.3755369822736156 ) ) ;
#162935 = CARTESIAN_POINT ( 'NONE',  ( -21.64999999999999858, 66.65000000001225544, -149.1731074845244223 ) ) ;
#162934 = DIRECTION ( 'NONE',  ( -1.000000000000000000, -2.952720810173289112E-16, 0.000000000000000000 ) ) ;
#162936 =( BOUNDED_SURFACE ( )  B_SPLINE_SURFACE ( 3, 2, ( 
 ( #191591, #109435, #170766 ),
 ( #52026, #212421, #169472 ),
 ( #10372, #32524, #11657 ),
 ( #194147, #15512, #248979 ) ),
 .UNSPECIFIED., .F., .F., .F. ) 
 B_SPLINE_SURFACE_WITH_KNOTS ( ( 4, 4 ),
 ( 3, 3 ),
 ( 5.727910411845712702, 5.983100554402349225 ),
 ( 0.000000000000000000, 1.000000000000000000 ),
 .UNSPECIFIED. ) 
 GEOMETRIC_REPRESENTATION_ITEM ( )  RATIONAL_B_SPLINE_SURFACE ( (
 ( 1.000000000000000000, 0.8946697475932183785, 1.000000000000000000),
 ( 1.000000000000000000, 0.9035312726220445789, 1.000000000000000000),
 ( 1.000000000000000000, 0.9104333467450315132, 1.000000000000000000),
 ( 1.000000000000000000, 0.9152888060719349683, 1.000000000000000000) ) ) 
 REPRESENTATION_ITEM ( '' )  SURFACE ( )  );
#162937 = AXIS2_PLACEMENT_3D ( 'NONE', #37130, #134890, #35841 ) ;
#162938 = CYLINDRICAL_SURFACE ( 'NONE', #176888, 0.09999999999999609201 ) ;
#162939 = DIRECTION ( 'NONE',  ( -1.000000000000000000, -1.541880601228652843E-16, -2.878400969107353907E-16 ) ) ;
#162941 = ADVANCED_FACE ( 'NONE', ( #42996 ), #224620, .F. ) ;
#162940 = CARTESIAN_POINT ( 'NONE',  ( -18.59999999999999787, 11.64999999999999680, -7.014805770654001016 ) ) ;
#162942 = ORIENTED_EDGE ( 'NONE', *, *, #147346, .F. ) ;
#162943 = ADVANCED_FACE ( 'NONE', ( #23458 ), #20641, .F. ) ;
#162944 = EDGE_CURVE ( 'NONE', #109224, #112914, #70721, .T. ) ;
#162945 = CARTESIAN_POINT ( 'NONE',  ( -18.34374000495059676, 64.52683809664972614, -145.7731074845244450 ) ) ;
#162946 = ORIENTED_EDGE ( 'NONE', *, *, #191884, .F. ) ;
#162947 = CARTESIAN_POINT ( 'NONE',  ( -21.65000000000000213, 7.250000000011138646, -109.7500000000000426 ) ) ;
#162948 = TOROIDAL_SURFACE ( 'NONE', #212824, 0.2000000000000000111, 0.1000000000000000056 ) ;
#162949 = CIRCLE ( 'NONE', #25562, 0.09999999999999990841 ) ;
#162950 = CARTESIAN_POINT ( 'NONE',  ( 18.37172112093850274, 85.57096165225516415, -29.20637303104079407 ) ) ;
#162951 = CIRCLE ( 'NONE', #83771, 1.899999999999999023 ) ;
#162952 = VERTEX_POINT ( 'NONE', #131502 ) ;
#162953 = FACE_OUTER_BOUND ( 'NONE', #109655, .T. ) ;
#162954 = EDGE_CURVE ( 'NONE', #129819, #145746, #70284, .T. ) ;
#162955 = VERTEX_POINT ( 'NONE', #31166 ) ;
#162956 = DIRECTION ( 'NONE',  ( -1.000000000000000000, 0.000000000000000000, -0.000000000000000000 ) ) ;
#162957 = LINE ( 'NONE', #61270, #220016 ) ;
#162958 = CARTESIAN_POINT ( 'NONE',  ( 21.14999999999999858, 76.00000000001156764, -57.37310748452432563 ) ) ;
#162959 = DIRECTION ( 'NONE',  ( 0.000000000000000000, 0.2617529984165180013, 0.9651348961777117541 ) ) ;
#162960 = CARTESIAN_POINT ( 'NONE',  ( -18.59999999999999787, 13.67914474873013475, -219.8713009340548865 ) ) ;
#162961 = CARTESIAN_POINT ( 'NONE',  ( -21.05000000000000071, 1.736257131608553550, -78.56865232901755292 ) ) ;
#162962 = AXIS2_PLACEMENT_3D ( 'NONE', #129951, #206948, #28347 ) ;
#162963 = DIRECTION ( 'NONE',  ( -1.000000000000000000, 0.000000000000000000, 0.000000000000000000 ) ) ;
#162965 = ORIENTED_EDGE ( 'NONE', *, *, #42323, .F. ) ;
#162964 = CARTESIAN_POINT ( 'NONE',  ( 21.12769345151713196, 65.28071232307203786, -191.2756271383269393 ) ) ;
#162967 = DIRECTION ( 'NONE',  ( 1.000000000000000000, 0.000000000000000000, 0.000000000000000000 ) ) ;
#162966 = CARTESIAN_POINT ( 'NONE',  ( -16.77779411440718604, 66.05389855290439982, -115.6861649015288975 ) ) ;
#162968 = ORIENTED_EDGE ( 'NONE', *, *, #191615, .T. ) ;
#162970 = EDGE_LOOP ( 'NONE', ( #236021, #218612, #87334, #25564, #204539 ) ) ;
#162969 = LINE ( 'NONE', #41739, #98264 ) ;
#162971 = ORIENTED_EDGE ( 'NONE', *, *, #26038, .F. ) ;
#162972 = CARTESIAN_POINT ( 'NONE',  ( 21.14999999999999503, 87.75000000001210765, -133.6231074845242119 ) ) ;
#162973 = DIRECTION ( 'NONE',  ( -0.000000000000000000, -0.000000000000000000, -1.000000000000000000 ) ) ;
#162974 = DIRECTION ( 'NONE',  ( 1.000000000000000000, -0.000000000000000000, -0.000000000000000000 ) ) ;
#162975 = VERTEX_POINT ( 'NONE', #192773 ) ;
#162976 = ADVANCED_FACE ( 'NONE', ( #111963 ), #216433, .F. ) ;
#162978 = EDGE_CURVE ( 'NONE', #124483, #100546, #245491, .T. ) ;
#162977 = CARTESIAN_POINT ( 'NONE',  ( 21.05000000000000071, -0.09999993529482809063, -127.5219217789050674 ) ) ;
#162979 = CARTESIAN_POINT ( 'NONE',  ( 21.05000000000000071, 10.91926294161915223, -235.7631306847335679 ) ) ;
#162980 = CARTESIAN_POINT ( 'NONE',  ( 18.49999999999998934, 38.23184963764531830, -261.0790774497031634 ) ) ;
#162981 = CARTESIAN_POINT ( 'NONE',  ( 21.14999999999999858, 76.00000000001195133, -103.0231074845243171 ) ) ;
#162982 = DIRECTION ( 'NONE',  ( 1.000000000000000000, 0.000000000000000000, 0.000000000000000000 ) ) ;
#162983 = B_SPLINE_CURVE_WITH_KNOTS ( 'NONE', 3,
 ( #68894, #168017, #166725, #84534, #24647, #105392, #104127 ),
 .UNSPECIFIED., .F., .F.,
 ( 4, 3, 4 ),
 ( 0.000000000000000000, 0.0007844235214594269838, 0.001767853679404345069 ),
 .UNSPECIFIED. ) ;
#162984 = AXIS2_PLACEMENT_3D ( 'NONE', #70185, #29785, #44189 ) ;
#162985 = AXIS2_PLACEMENT_3D ( 'NONE', #166494, #244697, #226407 ) ;
#162986 = EDGE_CURVE ( 'NONE', #61696, #49587, #78855, .T. ) ;
#162987 = CARTESIAN_POINT ( 'NONE',  ( 23.14999999999998437, 11.75000000001115552, -100.5000000000000284 ) ) ;
#162988 = ORIENTED_EDGE ( 'NONE', *, *, #1111, .F. ) ;
#162989 = ORIENTED_EDGE ( 'NONE', *, *, #20234, .T. ) ;
#162990 = CARTESIAN_POINT ( 'NONE',  ( 21.05000000000000071, 76.00000000001267608, -203.4231074845243654 ) ) ;
#162991 = ORIENTED_EDGE ( 'NONE', *, *, #253635, .T. ) ;
#162992 = DIRECTION ( 'NONE',  ( -0.000000000000000000, 0.8814952561688430555, -0.4721928772777346239 ) ) ;
#162993 = ORIENTED_EDGE ( 'NONE', *, *, #30509, .F. ) ;
#162994 = DIRECTION ( 'NONE',  ( 0.000000000000000000, -1.000000000000000000, -6.982962677686265922E-15 ) ) ;
#162995 = DIRECTION ( 'NONE',  ( 0.000000000000000000, -6.982962677686266711E-15, 1.000000000000000000 ) ) ;
#162996 = DIRECTION ( 'NONE',  ( 0.000000000000000000, 0.4721928772777346239, 0.8814952561688430555 ) ) ;
#162997 = CARTESIAN_POINT ( 'NONE',  ( 21.05000000000000071, 5.000000000011153745, -88.59473398108696074 ) ) ;
#162998 = CARTESIAN_POINT ( 'NONE',  ( -23.15000000000000213, -9.599999999988847676, -43.39396912265245021 ) ) ;
#162999 = ORIENTED_EDGE ( 'NONE', *, *, #153415, .T. ) ;
#163000 = CIRCLE ( 'NONE', #183824, 0.09999999999999939493 ) ;
#163001 = ADVANCED_FACE ( 'NONE', ( #194070 ), #109354, .T. ) ;
#163002 = CARTESIAN_POINT ( 'NONE',  ( 23.25000000000000000, 87.65000000001269598, -203.5231074845243029 ) ) ;
#163003 = CYLINDRICAL_SURFACE ( 'NONE', #158775, 0.09999999999999939493 ) ;
#163004 = CARTESIAN_POINT ( 'NONE',  ( 18.43473516226059417, 85.49494228276991237, -62.47720880117490339 ) ) ;
#163005 = LINE ( 'NONE', #122592, #10157 ) ;
#163006 = ORIENTED_EDGE ( 'NONE', *, *, #256578, .T. ) ;
#163008 = CARTESIAN_POINT ( 'NONE',  ( -20.54999999999999716, 84.66355140188136374, -146.0472086025916099 ) ) ;
#163007 = CARTESIAN_POINT ( 'NONE',  ( -20.94999999999999929, 86.45856254523214091, -209.4679346046102921 ) ) ;
#163009 = VERTEX_POINT ( 'NONE', #91097 ) ;
#163012 = ORIENTED_EDGE ( 'NONE', *, *, #13795, .F. ) ;
#163011 = CARTESIAN_POINT ( 'NONE',  ( -22.50000000000000000, 1.115600667400684642E-11, -155.8504291924551808 ) ) ;
#163010 = CARTESIAN_POINT ( 'NONE',  ( 23.14999999999998437, 3.558777552609279304, -231.8203201594644725 ) ) ;
#163013 = ORIENTED_EDGE ( 'NONE', *, *, #136756, .T. ) ;
#163014 = CARTESIAN_POINT ( 'NONE',  ( -20.94999999999999929, -1.164121893230052995, -74.91484808557160591 ) ) ;
#163015 = CYLINDRICAL_SURFACE ( 'NONE', #69407, 0.09999999999999939493 ) ;
#163016 = EDGE_CURVE ( 'NONE', #197879, #167673, #14155, .T. ) ;
#163017 = DIRECTION ( 'NONE',  ( 1.000000000000000000, 0.000000000000000000, 0.000000000000000000 ) ) ;
#163018 = VERTEX_POINT ( 'NONE', #72851 ) ;
#163019 = CARTESIAN_POINT ( 'NONE',  ( 19.83283456528358002, 16.76897757965512881, -222.7804130104206592 ) ) ;
#163020 = VECTOR ( 'NONE', #67652, 1000.000000000000000 ) ;
#163021 = LINE ( 'NONE', #221668, #52878 ) ;
#163022 = EDGE_CURVE ( 'NONE', #85729, #231733, #170515, .T. ) ;
#163024 = DIRECTION ( 'NONE',  ( 0.000000000000000000, 1.734723475976757554E-14, 1.000000000000000000 ) ) ;
#163023 = PLANE ( 'NONE',  #180333 ) ;
#163025 = EDGE_CURVE ( 'NONE', #158579, #190837, #248159, .T. ) ;
#163027 = ORIENTED_EDGE ( 'NONE', *, *, #230407, .T. ) ;
#163026 = DIRECTION ( 'NONE',  ( 0.000000000000000000, -1.000000000000000000, 0.000000000000000000 ) ) ;
#163028 = AXIS2_PLACEMENT_3D ( 'NONE', #47403, #126960, #227336 ) ;
#163029 = EDGE_LOOP ( 'NONE', ( #200847, #96861, #163738, #111798 ) ) ;
#163030 = TOROIDAL_SURFACE ( 'NONE', #158931, 0.2000000000000000111, 0.1000000000000000056 ) ;
#163031 = FACE_OUTER_BOUND ( 'NONE', #118361, .T. ) ;
#163032 = DIRECTION ( 'NONE',  ( 0.000000000000000000, 6.982962677686266711E-15, -1.000000000000000000 ) ) ;
#163033 = ADVANCED_FACE ( 'NONE', ( #171960 ), #87243, .T. ) ;
#163034 = DIRECTION ( 'NONE',  ( 0.000000000000000000, -0.8777080977375132376, 0.4791956752371582251 ) ) ;
#163037 = ADVANCED_FACE ( 'NONE', ( #148513 ), #231912, .T. ) ;
#163036 = VERTEX_POINT ( 'NONE', #188918 ) ;
#163035 = VECTOR ( 'NONE', #180189, 1000.000000000000000 ) ;
#163038 = DIRECTION ( 'NONE',  ( -2.578261006436899437E-14, -0.1350103645451973811, 0.9908441862701586889 ) ) ;
#163039 = VERTEX_POINT ( 'NONE', #53260 ) ;
#163040 = CARTESIAN_POINT ( 'NONE',  ( 20.95263205890665503, 18.81279984507908409, -229.8998340085670407 ) ) ;
#163041 = AXIS2_PLACEMENT_3D ( 'NONE', #23387, #102863, #5042 ) ;
#163042 = DIRECTION ( 'NONE',  ( -1.000000000000000000, -0.000000000000000000, -0.000000000000000000 ) ) ;
#163043 = CARTESIAN_POINT ( 'NONE',  ( -21.05000000000000071, 1.115600667400684642E-11, -167.4999999999999716 ) ) ;
#163044 = EDGE_CURVE ( 'NONE', #62395, #156950, #29042, .T. ) ;
#163045 = ORIENTED_EDGE ( 'NONE', *, *, #165140, .F. ) ;
#163046 = CARTESIAN_POINT ( 'NONE',  ( 21.14999999999999858, 65.28660755661240955, -157.7731074845244450 ) ) ;
#163047 = AXIS2_PLACEMENT_3D ( 'NONE', #198703, #163437, #61762 ) ;
#163048 = EDGE_CURVE ( 'NONE', #154309, #116247, #174799, .T. ) ;
#163049 = CIRCLE ( 'NONE', #4773, 7.799999999999993605 ) ;
#163050 = FACE_OUTER_BOUND ( 'NONE', #165916, .T. ) ;
#163051 = EDGE_CURVE ( 'NONE', #121523, #106796, #250178, .T. ) ;
#163052 = EDGE_CURVE ( 'NONE', #223845, #99386, #162287, .T. ) ;
#163053 = EDGE_LOOP ( 'NONE', ( #25054, #198896, #181558, #187757 ) ) ;
#163054 = ORIENTED_EDGE ( 'NONE', *, *, #99604, .F. ) ;
#163055 = CIRCLE ( 'NONE', #50585, 0.09999999999999990841 ) ;
#163056 = VERTEX_POINT ( 'NONE', #115797 ) ;
#163057 = EDGE_CURVE ( 'NONE', #182152, #231868, #83115, .T. ) ;
#163058 = FACE_OUTER_BOUND ( 'NONE', #88770, .T. ) ;
#163059 = ORIENTED_EDGE ( 'NONE', *, *, #152818, .T. ) ;
#163061 = VERTEX_POINT ( 'NONE', #178361 ) ;
#163060 = DIRECTION ( 'NONE',  ( 0.000000000000000000, 0.000000000000000000, -1.000000000000000000 ) ) ;
#163062 = AXIS2_PLACEMENT_3D ( 'NONE', #137308, #19961, #17381 ) ;
#163064 = EDGE_CURVE ( 'NONE', #31427, #134440, #228916, .T. ) ;
#163063 = VERTEX_POINT ( 'NONE', #117085 ) ;
#163065 = ADVANCED_FACE ( 'NONE', ( #40139 ), #4051, .T. ) ;
#163068 = ORIENTED_EDGE ( 'NONE', *, *, #121231, .F. ) ;
#163067 = ORIENTED_EDGE ( 'NONE', *, *, #97789, .F. ) ;
#163066 = DIRECTION ( 'NONE',  ( 1.000000000000000000, 0.000000000000000000, -0.000000000000000000 ) ) ;
#163069 = ADVANCED_FACE ( 'NONE', ( #75416 ), #154950, .F. ) ;
#163070 = VERTEX_POINT ( 'NONE', #235728 ) ;
#163071 = CARTESIAN_POINT ( 'NONE',  ( 20.73486653747088937, 68.25000000001183764, -90.37310748452435405 ) ) ;
#163072 = VECTOR ( 'NONE', #163523, 1000.000000000000000 ) ;
#163073 = CARTESIAN_POINT ( 'NONE',  ( 18.39999999999999503, 11.75000000001113953, -191.7499999999999716 ) ) ;
#163074 = AXIS2_PLACEMENT_3D ( 'NONE', #8652, #92033, #171613 ) ;
#163075 = CARTESIAN_POINT ( 'NONE',  ( -21.05000000000000071, 7.128833340093095217, -233.7327013124392749 ) ) ;
#163076 = ORIENTED_EDGE ( 'NONE', *, *, #226879, .F. ) ;
#163077 = CARTESIAN_POINT ( 'NONE',  ( -13.39999999999994529, 64.25000000001119815, -18.32310748452479388 ) ) ;
#163079 = ORIENTED_EDGE ( 'NONE', *, *, #186868, .T. ) ;
#163078 = LINE ( 'NONE', #197025, #111847 ) ;
#163080 = CARTESIAN_POINT ( 'NONE',  ( -16.77732147278574715, 9.945966932584589415, -180.1635087568757854 ) ) ;
#163082 = ORIENTED_EDGE ( 'NONE', *, *, #180474, .T. ) ;
#163081 = LINE ( 'NONE', #242580, #218883 ) ;
#163083 = ADVANCED_FACE ( 'NONE', ( #139179 ), #220719, .T. ) ;
#163084 = ORIENTED_EDGE ( 'NONE', *, *, #29780, .T. ) ;
#163085 = EDGE_LOOP ( 'NONE', ( #101773, #92406, #66931, #9238, #232328, #71462 ) ) ;
#163086 = VERTEX_POINT ( 'NONE', #256522 ) ;
#163087 = DIRECTION ( 'NONE',  ( -0.000000000000000000, 0.4791956752371485107, 0.8777080977375185666 ) ) ;
#163088 = CARTESIAN_POINT ( 'NONE',  ( -21.15000000000000213, 1.115526128501326264E-11, -160.9593430482987344 ) ) ;
#163090 = ORIENTED_EDGE ( 'NONE', *, *, #61961, .T. ) ;
#163089 = VERTEX_POINT ( 'NONE', #137905 ) ;
#163091 = ORIENTED_EDGE ( 'NONE', *, *, #174924, .F. ) ;
#163092 = DIRECTION ( 'NONE',  ( -3.265361837132813093E-16, -1.000000000000000000, -6.982962677686266711E-15 ) ) ;
#163093 = EDGE_LOOP ( 'NONE', ( #63614, #120775, #18837, #200003 ) ) ;
#163094 = ORIENTED_EDGE ( 'NONE', *, *, #165949, .T. ) ;
#163095 = DIRECTION ( 'NONE',  ( 0.000000000000000000, -1.000000000000000000, 0.000000000000000000 ) ) ;
#163097 = ORIENTED_EDGE ( 'NONE', *, *, #112237, .F. ) ;
#163096 = DIRECTION ( 'NONE',  ( 0.000000000000000000, 0.4088369013363281623, -0.9126074666063771490 ) ) ;
#163098 = CARTESIAN_POINT ( 'NONE',  ( -18.59999999999999787, 74.73821383144760944, -195.4366085209788935 ) ) ;
#163100 = CARTESIAN_POINT ( 'NONE',  ( 18.58703555224997928, -9.406336740777952343, -107.6249446412463726 ) ) ;
#163099 = CARTESIAN_POINT ( 'NONE',  ( 18.59999999999999076, 2.319530388122574394, -217.8268657444419887 ) ) ;
#163101 = VECTOR ( 'NONE', #38603, 1000.000000000000000 ) ;
#163102 = EDGE_LOOP ( 'NONE', ( #168570, #144878, #91546, #20703 ) ) ;
#163104 = EDGE_LOOP ( 'NONE', ( #89057, #54132, #201155, #225190, #217969 ) ) ;
#163103 = ORIENTED_EDGE ( 'NONE', *, *, #250849, .T. ) ;
#163105 = DIRECTION ( 'NONE',  ( 1.000000000000000000, 0.000000000000000000, 0.000000000000000000 ) ) ;
#163107 = EDGE_CURVE ( 'NONE', #126399, #115616, #12450, .T. ) ;
#163106 = CARTESIAN_POINT ( 'NONE',  ( -18.59999999999999787, -10.64999999999999325, 31.59999999999999787 ) ) ;
#163108 = ORIENTED_EDGE ( 'NONE', *, *, #250532, .F. ) ;
#163109 = EDGE_CURVE ( 'NONE', #106103, #37010, #135338, .T. ) ;
#163110 = B_SPLINE_CURVE_WITH_KNOTS ( 'NONE', 3,
 ( #29769, #145813, #225341, #212239, #214778, #153581, #92259, #133952, #15325, #171849, #250064, #72744, #190096, #90980, #173146, #170584, #34900, #113120, #231799 ),
 .UNSPECIFIED., .F., .F.,
 ( 4, 3, 3, 3, 3, 3, 4 ),
 ( 0.0001624081864585774811, 0.0001685232196531728874, 0.0001764526673566831365, 0.0001916878551483135532, 0.0002009890782182522111, 0.0002238845907555150493, 0.0002283406619926365698 ),
 .UNSPECIFIED. ) ;
#163111 = AXIS2_PLACEMENT_3D ( 'NONE', #52801, #72403, #150637 ) ;
#163112 = CARTESIAN_POINT ( 'NONE',  ( 23.14999999999999858, 6.650000000011155876, -45.85000000000000142 ) ) ;
#163113 = ORIENTED_EDGE ( 'NONE', *, *, #188454, .T. ) ;
#163114 = VERTEX_POINT ( 'NONE', #199186 ) ;
#163115 = DIRECTION ( 'NONE',  ( 0.000000000000000000, 0.9126074666063545004, 0.4088369013363783999 ) ) ;
#163116 = ORIENTED_EDGE ( 'NONE', *, *, #166898, .T. ) ;
#163117 = DIRECTION ( 'NONE',  ( 2.952720810173289112E-16, 1.000000000000000000, -6.088138035986627436E-46 ) ) ;
#163118 = CARTESIAN_POINT ( 'NONE',  ( 23.24999999999997513, 35.97645343225767789, -235.9694016464868298 ) ) ;
#163119 = ORIENTED_EDGE ( 'NONE', *, *, #81221, .F. ) ;
#163120 = CARTESIAN_POINT ( 'NONE',  ( 19.99999999738052026, 64.25000000001219291, -145.3359355348916040 ) ) ;
#163121 = CARTESIAN_POINT ( 'NONE',  ( -16.87036670365549540, 9.989418819312804843, -46.02043988269793573 ) ) ;
#163123 = CARTESIAN_POINT ( 'NONE',  ( -16.93710578446422943, 9.950000000011137047, -121.0811960162006926 ) ) ;
#163122 = DIRECTION ( 'NONE',  ( 0.000000000000000000, 0.4088369013363281068, -0.9126074666063770380 ) ) ;
#163124 = CYLINDRICAL_SURFACE ( 'NONE', #169143, 0.1000000000000028644 ) ;
#163125 = FACE_OUTER_BOUND ( 'NONE', #110493, .T. ) ;
#163126 = DIRECTION ( 'NONE',  ( -0.5932847527679298016, -0.3291107096594080295, 0.7346423231209709970 ) ) ;
#163127 = DIRECTION ( 'NONE',  ( -0.000000000000000000, -0.000000000000000000, -1.000000000000000000 ) ) ;
#163128 = LINE ( 'NONE', #237520, #139122 ) ;
#163129 = ADVANCED_FACE ( 'NONE', ( #175788 ), #217435, .T. ) ;
#163130 = VECTOR ( 'NONE', #72419, 1000.000000000000000 ) ;
#163131 = VERTEX_POINT ( 'NONE', #177078 ) ;
#163132 = CIRCLE ( 'NONE', #54766, 0.1000000000000124678 ) ;
#163133 = CIRCLE ( 'NONE', #88059, 0.1999999999999987899 ) ;
#163135 = ORIENTED_EDGE ( 'NONE', *, *, #250813, .T. ) ;
#163134 = ORIENTED_EDGE ( 'NONE', *, *, #257779, .F. ) ;
#163136 = EDGE_LOOP ( 'NONE', ( #167223, #199491, #39615 ) ) ;
#163137 = DIRECTION ( 'NONE',  ( 1.000000000000000000, 0.000000000000000000, 0.000000000000000000 ) ) ;
#163138 = DIRECTION ( 'NONE',  ( 0.000000000000000000, -0.9126074666063770380, -0.4088369013363281068 ) ) ;
#163140 = CARTESIAN_POINT ( 'NONE',  ( 21.05000000000000071, 11.60000000001116227, -194.0717967697244717 ) ) ;
#163139 = DIRECTION ( 'NONE',  ( 1.000000000000000000, 0.000000000000000000, 0.000000000000000000 ) ) ;
#163141 = CARTESIAN_POINT ( 'NONE',  ( 21.05000000000000071, 6.450000000011156587, -177.5170271704400022 ) ) ;
#163142 = ORIENTED_EDGE ( 'NONE', *, *, #249655, .T. ) ;
#163143 = CYLINDRICAL_SURFACE ( 'NONE', #9133, 0.09999999999999939493 ) ;
#163144 = DIRECTION ( 'NONE',  ( 0.000000000000000000, 1.000000000000000000, 0.000000000000000000 ) ) ;
#163146 = AXIS2_PLACEMENT_3D ( 'NONE', #21801, #139132, #240842 ) ;
#163145 = CARTESIAN_POINT ( 'NONE',  ( -16.97683809663753252, 66.05000000001190585, -89.75158271585443970 ) ) ;
#163147 = CARTESIAN_POINT ( 'NONE',  ( -16.92563707711778065, 9.968990694407935393, -87.88075829952403240 ) ) ;
#163148 = VERTEX_POINT ( 'NONE', #19258 ) ;
#163149 = CARTESIAN_POINT ( 'NONE',  ( 21.14999999999999858, 6.540656951712400691, -134.0000000000000000 ) ) ;
#163150 = DIRECTION ( 'NONE',  ( 0.000000000000000000, -0.9915357197604882655, 0.1298341882519793711 ) ) ;
#163151 = VERTEX_POINT ( 'NONE', #96219 ) ;
#163152 = CARTESIAN_POINT ( 'NONE',  ( -17.22361732159832215, 65.65484434141018255, -192.1523229586573223 ) ) ;
#163153 = DIRECTION ( 'NONE',  ( -1.000000000000000000, 0.000000000000000000, -0.000000000000000000 ) ) ;
#163154 = CARTESIAN_POINT ( 'NONE',  ( 21.05000000000000071, 1.115600667400684642E-11, -134.0000000000000000 ) ) ;
#163155 = CARTESIAN_POINT ( 'NONE',  ( -20.64999999999999858, 7.249999999999999112, -21.25000000000000000 ) ) ;
#163156 = DIRECTION ( 'NONE',  ( 1.000000000000000000, 0.000000000000000000, 0.000000000000000000 ) ) ;
#163157 = DIRECTION ( 'NONE',  ( -1.000000000000000000, 1.836970198721029934E-16, 1.282749433769087757E-30 ) ) ;
#163158 = ORIENTED_EDGE ( 'NONE', *, *, #30381, .T. ) ;
#163159 = LINE ( 'NONE', #223107, #240336 ) ;
#163161 = ADVANCED_FACE ( 'NONE', ( #136624 ), #236698, .T. ) ;
#163160 = CARTESIAN_POINT ( 'NONE',  ( -20.05000000000000426, 9.250000000011157297, -121.7500000000000426 ) ) ;
#163162 = CARTESIAN_POINT ( 'NONE',  ( 20.90000000000000213, 1.885425182446133885, -11.49641995933507843 ) ) ;
#163165 = DIRECTION ( 'NONE',  ( -1.387778780781259631E-13, 0.1675535138457220907, -0.9858629823651720026 ) ) ;
#163164 = CIRCLE ( 'NONE', #75676, 0.09999999999999939493 ) ;
#163163 = CARTESIAN_POINT ( 'NONE',  ( -21.05000000000000071, 4.273531877263400780, -211.9976340888692050 ) ) ;
#163167 = CARTESIAN_POINT ( 'NONE',  ( -18.47140463609787986, 85.67147468523329223, -163.3503470262502617 ) ) ;
#163166 = AXIS2_PLACEMENT_3D ( 'NONE', #183411, #4738, #106406 ) ;
#163168 = EDGE_CURVE ( 'NONE', #133775, #241262, #245660, .T. ) ;
#163169 = AXIS2_PLACEMENT_3D ( 'NONE', #38440, #59238, #252338 ) ;
#163170 = CARTESIAN_POINT ( 'NONE',  ( 20.04142135623730070, 11.65000000001115943, -121.7500000000000426 ) ) ;
#163171 = CARTESIAN_POINT ( 'NONE',  ( -20.54999999999999716, 4.350000000011156054, -50.25000000000000000 ) ) ;
#163173 = ORIENTED_EDGE ( 'NONE', *, *, #20913, .F. ) ;
#163172 = CARTESIAN_POINT ( 'NONE',  ( 18.52928932188133970, 54.95214567929435390, -230.0923768967488456 ) ) ;
#163174 = EDGE_CURVE ( 'NONE', #140969, #14771, #62241, .T. ) ;
#163175 = EDGE_CURVE ( 'NONE', #152513, #88951, #184737, .T. ) ;
#163176 = EDGE_CURVE ( 'NONE', #79382, #56413, #29225, .T. ) ;
#163177 = CIRCLE ( 'NONE', #246540, 0.1000000000000028644 ) ;
#163178 = CARTESIAN_POINT ( 'NONE',  ( 22.37643362114956247, 7.625789993969535274, -100.4009186263186564 ) ) ;
#163179 = DIRECTION ( 'NONE',  ( 1.000000000000000000, -0.000000000000000000, -0.000000000000000000 ) ) ;
#163180 = EDGE_CURVE ( 'NONE', #140913, #61591, #74998, .T. ) ;
#163181 = DIRECTION ( 'NONE',  ( 0.000000000000000000, 0.000000000000000000, -1.000000000000000000 ) ) ;
#163182 = ORIENTED_EDGE ( 'NONE', *, *, #9299, .F. ) ;
#163183 = CARTESIAN_POINT ( 'NONE',  ( 23.14999999999999503, 11.65000000001116298, -112.6500000000000341 ) ) ;
#163184 = FACE_OUTER_BOUND ( 'NONE', #165933, .T. ) ;
#163185 = CARTESIAN_POINT ( 'NONE',  ( -18.57399277249657032, 65.66887361445333227, -97.43298459182689442 ) ) ;
#163186 = ORIENTED_EDGE ( 'NONE', *, *, #151635, .F. ) ;
#163187 = CARTESIAN_POINT ( 'NONE',  ( -21.05000000000000071, 14.81796439977981272, -236.5325475414793743 ) ) ;
#163189 = VERTEX_POINT ( 'NONE', #143034 ) ;
#163188 = DIRECTION ( 'NONE',  ( 1.000000000000000000, 0.000000000000000000, -0.000000000000000000 ) ) ;
#163191 = CARTESIAN_POINT ( 'NONE',  ( 21.10257677756356287, 0.02495074956798263091, 6.398381742532735394 ) ) ;
#163190 = DIRECTION ( 'NONE',  ( -1.000000000000000000, 0.000000000000000000, 0.000000000000000000 ) ) ;
#163192 = ADVANCED_FACE ( 'NONE', ( #105162 ), #26989, .F. ) ;
#163193 = AXIS2_PLACEMENT_3D ( 'NONE', #61385, #178808, #197027 ) ;
#163194 = DIRECTION ( 'NONE',  ( 0.000000000000000000, 0.000000000000000000, -1.000000000000000000 ) ) ;
#163195 = ORIENTED_EDGE ( 'NONE', *, *, #118757, .T. ) ;
#163196 = AXIS2_PLACEMENT_3D ( 'NONE', #32670, #53473, #96424 ) ;
#163197 = CARTESIAN_POINT ( 'NONE',  ( 0.000000000000000000, 0.000000000000000000, 0.000000000000000000 ) ) ;
#163198 = DIRECTION ( 'NONE',  ( 1.000000000000000000, 0.000000000000000000, 0.000000000000000000 ) ) ;
#163199 = LINE ( 'NONE', #242711, #114910 ) ;
#163200 = VERTEX_POINT ( 'NONE', #84303 ) ;
#163201 = VECTOR ( 'NONE', #44547, 1000.000000000000000 ) ;
#163202 = CARTESIAN_POINT ( 'NONE',  ( 23.15000000000000213, 87.75000000001229239, -157.7731074845242745 ) ) ;
#163203 = CARTESIAN_POINT ( 'NONE',  ( 23.15000000000000213, 85.00000000001232081, -160.1291383618718385 ) ) ;
#163204 = VECTOR ( 'NONE', #30111, 1000.000000000000000 ) ;
#163206 = CARTESIAN_POINT ( 'NONE',  ( 22.39999999999999503, -3.275978944802467652, -228.2735455795363748 ) ) ;
#163205 = VECTOR ( 'NONE', #64732, 1000.000000000000000 ) ;
#163207 = DIRECTION ( 'NONE',  ( 1.000000000000000000, 0.000000000000000000, 0.000000000000000000 ) ) ;
#163208 = ORIENTED_EDGE ( 'NONE', *, *, #20559, .T. ) ;
#163209 = ORIENTED_EDGE ( 'NONE', *, *, #990, .F. ) ;
#163211 = AXIS2_PLACEMENT_3D ( 'NONE', #254497, #56310, #139372 ) ;
#163210 = DIRECTION ( 'NONE',  ( -2.952720810173289112E-16, -1.000000000000000000, -6.982962677686266711E-15 ) ) ;
#163213 = AXIS2_PLACEMENT_3D ( 'NONE', #4393, #124366, #46088 ) ;
#163212 = DIRECTION ( 'NONE',  ( 0.000000000000000000, 0.000000000000000000, -1.000000000000000000 ) ) ;
#163214 = DIRECTION ( 'NONE',  ( 0.000000000000000000, 0.000000000000000000, -1.000000000000000000 ) ) ;
#163215 = DIRECTION ( 'NONE',  ( 1.000000000000000000, 0.000000000000000000, 0.000000000000000000 ) ) ;
#163216 = FACE_OUTER_BOUND ( 'NONE', #49076, .T. ) ;
#163218 = CARTESIAN_POINT ( 'NONE',  ( 18.59999999999999432, -9.480686695267811714, -174.4411151687578752 ) ) ;
#163217 = CARTESIAN_POINT ( 'NONE',  ( -16.87683809663753109, 12.46404896785209537, -211.8723793542922067 ) ) ;
#163219 = VECTOR ( 'NONE', #204320, 1000.000000000000114 ) ;
#163220 = DIRECTION ( 'NONE',  ( 1.000000000000000000, 0.000000000000000000, -0.000000000000000000 ) ) ;
#163221 = CARTESIAN_POINT ( 'NONE',  ( -22.39999999999999858, 10.71943444926882449, -226.8179467668883547 ) ) ;
#163223 = CARTESIAN_POINT ( 'NONE',  ( -18.49719636458513961, 46.97455478271485418, -255.2808495583587103 ) ) ;
#163222 = CIRCLE ( 'NONE', #188163, 0.2000000000000057288 ) ;
#163224 = CARTESIAN_POINT ( 'NONE',  ( 20.94999999999999574, 7.128833340093095217, -233.7327013124392749 ) ) ;
#163225 = ADVANCED_FACE ( 'NONE', ( #63505 ), #64795, .T. ) ;
#163227 = VERTEX_POINT ( 'NONE', #122218 ) ;
#163226 = CYLINDRICAL_SURFACE ( 'NONE', #11397, 0.1000000000000053763 ) ;
#163228 = CARTESIAN_POINT ( 'NONE',  ( -21.12844524849339223, 64.25000000001209344, -129.6186940136819601 ) ) ;
#163229 = CARTESIAN_POINT ( 'NONE',  ( -23.15000000000000213, 74.00000000001259082, -190.2984855617622770 ) ) ;
#163231 = DIRECTION ( 'NONE',  ( -2.952720810173287633E-16, 0.9770955615653312831, 0.2128009952263610616 ) ) ;
#163230 = CARTESIAN_POINT ( 'NONE',  ( 21.53699400384887852, 75.99999999997994848, -109.8108192777622634 ) ) ;
#163232 = CIRCLE ( 'NONE', #71650, 0.09999999999999939493 ) ;
#163233 = ORIENTED_EDGE ( 'NONE', *, *, #113998, .T. ) ;
#163235 = CARTESIAN_POINT ( 'NONE',  ( -21.65000000000000213, 9.950000000011138823, -113.2500000000000284 ) ) ;
#163234 = CARTESIAN_POINT ( 'NONE',  ( -16.93710578446435733, 66.05000000001157900, -56.60430350072524419 ) ) ;
#163236 = CARTESIAN_POINT ( 'NONE',  ( 23.24999999999999289, 11.65000000001116298, -88.75000000000004263 ) ) ;
#163237 = LINE ( 'NONE', #64127, #101167 ) ;
#163238 = CARTESIAN_POINT ( 'NONE',  ( -23.49999999999994316, 76.00000000001119815, -36.02310748452479316 ) ) ;
#163241 = ADVANCED_FACE ( 'NONE', ( #123496 ), #50024, .F. ) ;
#163240 = CARTESIAN_POINT ( 'NONE',  ( -12.25000000000000178, 66.65000000001258229, -186.7731074845244166 ) ) ;
#163239 = AXIS2_PLACEMENT_3D ( 'NONE', #4422, #120555, #143937 ) ;
#163242 = ORIENTED_EDGE ( 'NONE', *, *, #10597, .F. ) ;
#163243 = VERTEX_POINT ( 'NONE', #3536 ) ;
#163244 = ADVANCED_FACE ( 'NONE', ( #24423 ), #101893, .T. ) ;
#163245 = EDGE_CURVE ( 'NONE', #236709, #25987, #179059, .T. ) ;
#163246 = DIRECTION ( 'NONE',  ( -0.7071067811865456854, 0.7071067811865493491, 0.000000000000000000 ) ) ;
#163247 = EDGE_LOOP ( 'NONE', ( #144024, #133883, #58989, #58516 ) ) ;
#163249 = CYLINDRICAL_SURFACE ( 'NONE', #105333, 0.8750000000000007772 ) ;
#163248 = AXIS2_PLACEMENT_3D ( 'NONE', #214275, #156895, #215545 ) ;
#163250 = CIRCLE ( 'NONE', #29984, 0.09999999999999939493 ) ;
#163251 = VERTEX_POINT ( 'NONE', #205579 ) ;
#163252 =( BOUNDED_CURVE ( )  B_SPLINE_CURVE ( 3, ( #156137, #133963, #213502, #256416 ),
 .UNSPECIFIED., .F., .T. ) 
 B_SPLINE_CURVE_WITH_KNOTS ( ( 4, 4 ),
 ( 3.141592653589793116, 4.712388980384689674 ),
 .UNSPECIFIED. ) 
 CURVE ( )  GEOMETRIC_REPRESENTATION_ITEM ( )  RATIONAL_B_SPLINE_CURVE ( ( 1.000000000000000000, 0.8047378541243649375, 0.8047378541243649375, 1.000000000000000000 ) ) 
 REPRESENTATION_ITEM ( '' )  );
#163253 = VECTOR ( 'NONE', #59288, 1000.000000000000114 ) ;
#163254 = CYLINDRICAL_SURFACE ( 'NONE', #247700, 7.899999999999990585 ) ;
#163255 = DIRECTION ( 'NONE',  ( 0.000000000000000000, -1.000000000000000000, 0.000000000000000000 ) ) ;
#163256 = VERTEX_POINT ( 'NONE', #106464 ) ;
#163257 = ADVANCED_FACE ( 'NONE', ( #240883 ), #7388, .F. ) ;
#163258 = EDGE_CURVE ( 'NONE', #56718, #230402, #47784, .T. ) ;
#163259 = DIRECTION ( 'NONE',  ( -1.000000000000000000, -0.000000000000000000, -0.000000000000000000 ) ) ;
#163260 = CARTESIAN_POINT ( 'NONE',  ( -17.11825945287481332, 66.05000000001201954, -115.7731074845243597 ) ) ;
#163261 = CARTESIAN_POINT ( 'NONE',  ( 20.99551997958415583, 11.75000000001125144, -160.6516591376888528 ) ) ;
#163262 = CARTESIAN_POINT ( 'NONE',  ( 18.39999999999998082, 58.57934086597919077, -223.9244941873113817 ) ) ;
#163263 = DIRECTION ( 'NONE',  ( -0.000000000000000000, 6.982962677686266711E-15, -1.000000000000000000 ) ) ;
#163264 = PRODUCT_DEFINITION ( 'UNKNOWN', '', #257000, #204299 ) ;
#163265 = CARTESIAN_POINT ( 'NONE',  ( 22.59999999999999787, 11.64957080755595520, -100.4000000000000483 ) ) ;
#163266 = CARTESIAN_POINT ( 'NONE',  ( 21.07199075132372101, 11.17301161084810168, -211.0664710372803938 ) ) ;
#163267 = VERTEX_POINT ( 'NONE', #212035 ) ;
#163268 = AXIS2_PLACEMENT_3D ( 'NONE', #219235, #141012, #101837 ) ;
#163270 = DIRECTION ( 'NONE',  ( 0.000000000000000000, -0.9916376685811618685, 0.1290532225514649800 ) ) ;
#163269 = DIRECTION ( 'NONE',  ( 0.000000000000000000, 0.9090645160164306793, 0.4166553800442435729 ) ) ;
#163271 = VERTEX_POINT ( 'NONE', #89485 ) ;
#163273 = ORIENTED_EDGE ( 'NONE', *, *, #173862, .T. ) ;
#163272 = CARTESIAN_POINT ( 'NONE',  ( 18.49999999999999289, 69.55000000001207638, -126.5060803140843291 ) ) ;
#163274 = ORIENTED_EDGE ( 'NONE', *, *, #136050, .F. ) ;
#163275 = DIRECTION ( 'NONE',  ( 0.000000000000000000, -0.4930308989875575865, -0.8700118002898125091 ) ) ;
#163276 = FACE_BOUND ( 'NONE', #214540, .T. ) ;
#163277 = DIRECTION ( 'NONE',  ( -7.304098846218134667E-16, -1.000000000000000000, -6.982962677686267499E-15 ) ) ;
#163278 = EDGE_CURVE ( 'NONE', #142984, #133447, #129147, .T. ) ;
#163279 = DIRECTION ( 'NONE',  ( -0.000000000000000000, 1.000000000000000000, -0.000000000000000000 ) ) ;
#163280 = VERTEX_POINT ( 'NONE', #153374 ) ;
#163281 = ADVANCED_FACE ( 'NONE', ( #170375 ), #110342, .F. ) ;
#163282 = EDGE_CURVE ( 'NONE', #208732, #240643, #83313, .T. ) ;
#163283 = DIRECTION ( 'NONE',  ( 0.000000000000000000, -6.454785026890510900E-15, 1.000000000000000000 ) ) ;
#163284 = ORIENTED_EDGE ( 'NONE', *, *, #183640, .T. ) ;
#163285 = CARTESIAN_POINT ( 'NONE',  ( -20.94983749550516450, 10.29766095124176850, -38.97436639332756414 ) ) ;
#163286 = DIRECTION ( 'NONE',  ( -1.000000000000000000, 0.000000000000000000, 0.000000000000000000 ) ) ;
#163287 = VERTEX_POINT ( 'NONE', #167786 ) ;
#163288 = DIRECTION ( 'NONE',  ( 0.000000000000000000, 0.9910465087640865089, -0.1335171055202867274 ) ) ;
#163289 = AXIS2_PLACEMENT_3D ( 'NONE', #148779, #225699, #206174 ) ;
#163290 = EDGE_LOOP ( 'NONE', ( #7487, #142515, #204144, #244840 ) ) ;
#163291 = DIRECTION ( 'NONE',  ( 1.000000000000000000, 0.000000000000000000, 0.000000000000000000 ) ) ;
#163292 = EDGE_LOOP ( 'NONE', ( #13396, #61393, #228266, #134221 ) ) ;
#163293 = LINE ( 'NONE', #139849, #33719 ) ;
#163294 = CARTESIAN_POINT ( 'NONE',  ( 18.59999999999997655, 79.19526988099229925, -196.1889237952725296 ) ) ;
#163295 = CARTESIAN_POINT ( 'NONE',  ( 19.97071067811864609, 16.69779891432240149, -222.5912266955230621 ) ) ;
#163296 =( BOUNDED_SURFACE ( )  B_SPLINE_SURFACE ( 3, 2, ( 
 ( #55781, #177079, #231913 ),
 ( #75417, #53262, #135339 ),
 ( #58356, #212351, #93663 ),
 ( #132810, #156235, #33743 ),
 ( #72852, #35017, #192774 ),
 ( #175789, #234445, #117086 ) ),
 .UNSPECIFIED., .F., .F., .F. ) 
 B_SPLINE_SURFACE_WITH_KNOTS ( ( 4, 2, 4 ),
 ( 3, 3 ),
 ( 0.0001381104793128061785, 0.0002947094729387726578, 0.0004513084665647390829 ),
 ( 0.000000000000000000, 1.000000000000000000 ),
 .UNSPECIFIED. ) 
 GEOMETRIC_REPRESENTATION_ITEM ( )  RATIONAL_B_SPLINE_SURFACE ( (
 ( 1.000000000000000000, 0.7071067811865494601, 1.000000000000000000),
 ( 1.000000000000000000, 0.6919563088092252068, 1.000000000000000000),
 ( 1.000000000000000000, 0.6959445945726553395, 1.000000000000000000),
 ( 1.000000000000000000, 0.7137882985304006001, 1.000000000000000000),
 ( 1.000000000000000000, 0.7257496306103440320, 1.000000000000000000),
 ( 1.000000000000000000, 0.7250110520819876836, 1.000000000000000000) ) ) 
 REPRESENTATION_ITEM ( '' )  SURFACE ( )  );
#163297 = DIRECTION ( 'NONE',  ( -2.827886303505249259E-16, -0.8660254037844378194, -0.5000000000000016653 ) ) ;
#163298 = EDGE_CURVE ( 'NONE', #72835, #60863, #252405, .T. ) ;
#163299 = CIRCLE ( 'NONE', #171510, 0.1000000000000028644 ) ;
#163300 = CARTESIAN_POINT ( 'NONE',  ( -21.45000000000000284, 68.29142135624952914, -148.7731074845244166 ) ) ;
#163301 = DIRECTION ( 'NONE',  ( 0.000000000000000000, 0.8887656589064600876, -0.4583618696494786149 ) ) ;
#163302 = LINE ( 'NONE', #207572, #14628 ) ;
#163304 = ORIENTED_EDGE ( 'NONE', *, *, #251615, .F. ) ;
#163303 = AXIS2_PLACEMENT_3D ( 'NONE', #130854, #210413, #31795 ) ;
#163306 = CARTESIAN_POINT ( 'NONE',  ( -20.85000000000000142, 68.97833521811203639, -132.6895420826271277 ) ) ;
#163305 = CARTESIAN_POINT ( 'NONE',  ( -21.14999999999999858, 69.45934304831114048, -170.0231074845243882 ) ) ;
#163307 = ORIENTED_EDGE ( 'NONE', *, *, #184364, .F. ) ;
#163308 = CARTESIAN_POINT ( 'NONE',  ( -20.64999999999999858, 85.40000000001178648, -79.41707660717668205 ) ) ;
#163309 = EDGE_CURVE ( 'NONE', #137749, #132077, #116660, .T. ) ;
#163310 = CARTESIAN_POINT ( 'NONE',  ( 21.05000000000000071, 10.39655183198268418, -207.4949966697317620 ) ) ;
#163312 = VERTEX_POINT ( 'NONE', #111632 ) ;
#163311 = DIRECTION ( 'NONE',  ( 0.000000000000000000, 1.000000000000000000, -2.775557561562888827E-14 ) ) ;
#163314 = ORIENTED_EDGE ( 'NONE', *, *, #239328, .F. ) ;
#163313 = CARTESIAN_POINT ( 'NONE',  ( 21.04999999999999716, 67.12872031401592210, -57.37310748452439668 ) ) ;
#163315 = LINE ( 'NONE', #204975, #193576 ) ;
#163316 = DIRECTION ( 'NONE',  ( -6.420062716055394467E-16, 0.1480365673253023484, -0.9889818879709282307 ) ) ;
#163317 = DIRECTION ( 'NONE',  ( -1.000000000000000000, 0.000000000000000000, 0.000000000000000000 ) ) ;
#163318 = EDGE_CURVE ( 'NONE', #121941, #21979, #224793, .T. ) ;
#163319 = LINE ( 'NONE', #142454, #238986 ) ;
#163321 = ORIENTED_EDGE ( 'NONE', *, *, #96920, .T. ) ;
#163320 = CARTESIAN_POINT ( 'NONE',  ( 21.09546886439534674, 67.12144688699737571, -157.7860136339689916 ) ) ;
#163322 = AXIS2_PLACEMENT_3D ( 'NONE', #146688, #188409, #26801 ) ;
#163323 = EDGE_CURVE ( 'NONE', #18030, #96167, #232891, .T. ) ;
#163325 = EDGE_CURVE ( 'NONE', #169137, #223322, #248571, .T. ) ;
#163324 = CARTESIAN_POINT ( 'NONE',  ( 21.13461538461538325, 10.61458296203669249, -179.8499999999999943 ) ) ;
#163327 = EDGE_CURVE ( 'NONE', #77399, #249368, #71243, .T. ) ;
#163326 = ORIENTED_EDGE ( 'NONE', *, *, #53994, .F. ) ;
#163328 = ORIENTED_EDGE ( 'NONE', *, *, #38561, .T. ) ;
#163329 = CARTESIAN_POINT ( 'NONE',  ( -18.54260524012588007, 85.62421939008548577, -62.78233443875351583 ) ) ;
#163330 = DIRECTION ( 'NONE',  ( -1.000000000000000000, -0.000000000000000000, -0.000000000000000000 ) ) ;
#163331 = ORIENTED_EDGE ( 'NONE', *, *, #97295, .F. ) ;
#163332 = CARTESIAN_POINT ( 'NONE',  ( -21.14999999999999858, 11.64999999999999680, 0.000000000000000000 ) ) ;
#163333 = B_SPLINE_CURVE_WITH_KNOTS ( 'NONE', 3,
 ( #170800, #247714, #226862, #230734, #48226, #229442 ),
 .UNSPECIFIED., .F., .F.,
 ( 4, 2, 4 ),
 ( 0.000000000000000000, 0.0001496588209255838274, 0.0002993176418511676548 ),
 .UNSPECIFIED. ) ;
#163334 = AXIS2_PLACEMENT_3D ( 'NONE', #104256, #22196, #183815 ) ;
#163335 = VECTOR ( 'NONE', #186983, 1000.000000000000000 ) ;
#163336 = CYLINDRICAL_SURFACE ( 'NONE', #120129, 0.1000000000000028644 ) ;
#163337 = AXIS2_PLACEMENT_3D ( 'NONE', #112556, #193385, #74743 ) ;
#163338 = EDGE_LOOP ( 'NONE', ( #7019, #219668, #104244, #109308 ) ) ;
#163340 = ADVANCED_FACE ( 'NONE', ( #149502 ), #9964, .F. ) ;
#163339 = LINE ( 'NONE', #164622, #23015 ) ;
#163341 = EDGE_CURVE ( 'NONE', #144138, #26148, #66606, .T. ) ;
#163342 = CARTESIAN_POINT ( 'NONE',  ( 23.40000000000005187, 77.75000000001119815, -47.64205752314703801 ) ) ;
#163343 = ORIENTED_EDGE ( 'NONE', *, *, #213756, .F. ) ;
#163344 = ORIENTED_EDGE ( 'NONE', *, *, #156813, .T. ) ;
#163345 = CARTESIAN_POINT ( 'NONE',  ( -21.44999999999999929, 68.65000000001187175, -90.77310748452435973 ) ) ;
#163346 = ORIENTED_EDGE ( 'NONE', *, *, #88699, .F. ) ;
#163347 = EDGE_CURVE ( 'NONE', #150529, #29621, #209441, .T. ) ;
#163348 = CARTESIAN_POINT ( 'NONE',  ( 17.74533788810830259, 10.81849979148194940, -177.8136226749475384 ) ) ;
#163349 = ORIENTED_EDGE ( 'NONE', *, *, #207150, .T. ) ;
#163350 = ORIENTED_EDGE ( 'NONE', *, *, #4562, .F. ) ;
#163351 = CIRCLE ( 'NONE', #117551, 0.09999999999999939493 ) ;
#163352 = CARTESIAN_POINT ( 'NONE',  ( -21.65000000000000213, 21.70314669089253812, -233.3151006027785286 ) ) ;
#163353 = ORIENTED_EDGE ( 'NONE', *, *, #215736, .F. ) ;
#163354 = CARTESIAN_POINT ( 'NONE',  ( 22.59999954896768770, -0.008828232233007798913, -88.74949132593202705 ) ) ;
#163356 = ORIENTED_EDGE ( 'NONE', *, *, #18120, .T. ) ;
#163355 = EDGE_CURVE ( 'NONE', #161543, #157067, #11254, .T. ) ;
#163358 = ORIENTED_EDGE ( 'NONE', *, *, #159415, .T. ) ;
#163357 = ORIENTED_EDGE ( 'NONE', *, *, #148291, .T. ) ;
#163359 = CARTESIAN_POINT ( 'NONE',  ( 21.05000000000000071, 69.58602111852371763, -136.4373083682503704 ) ) ;
#163360 = EDGE_CURVE ( 'NONE', #166838, #19374, #249861, .T. ) ;
#163361 = CARTESIAN_POINT ( 'NONE',  ( -20.99749315643147440, 56.02567684099302880, -227.9999002278294142 ) ) ;
#163362 = ORIENTED_EDGE ( 'NONE', *, *, #104740, .T. ) ;
#163363 = ADVANCED_FACE ( 'NONE', ( #32121 ), #191200, .F. ) ;
#163364 = ORIENTED_EDGE ( 'NONE', *, *, #219592, .T. ) ;
#163365 = DIRECTION ( 'NONE',  ( 0.000000000000000000, 0.000000000000000000, -1.000000000000000000 ) ) ;
#163367 = CARTESIAN_POINT ( 'NONE',  ( -16.27683809663750480, 66.65000000001182912, -82.07310748452438531 ) ) ;
#163366 = CIRCLE ( 'NONE', #42545, 4.049999999999998046 ) ;
#163369 = ORIENTED_EDGE ( 'NONE', *, *, #155374, .T. ) ;
#163368 = DIRECTION ( 'NONE',  ( 1.000000000000000000, 0.000000000000000000, 0.000000000000000000 ) ) ;
#163370 = DIRECTION ( 'NONE',  ( -0.000000000000000000, -1.000000000000000000, -1.734723475976807292E-15 ) ) ;
#163371 = EDGE_LOOP ( 'NONE', ( #63503, #155818, #231178, #154108 ) ) ;
#163372 = ADVANCED_FACE ( 'NONE', ( #8683 ), #20832, .F. ) ;
#163373 = CARTESIAN_POINT ( 'NONE',  ( -18.56579813702275672, 65.66974365629688748, -130.9360145562605169 ) ) ;
#163374 = EDGE_CURVE ( 'NONE', #42457, #140969, #208184, .T. ) ;
#163375 = TOROIDAL_SURFACE ( 'NONE', #200779, 0.2000000000000000111, 0.1000000000000000056 ) ;
#163376 = EDGE_LOOP ( 'NONE', ( #37209, #17150, #106106, #229418, #176127, #49910, #88841 ) ) ;
#163377 = DIRECTION ( 'NONE',  ( 0.000000000000000000, -1.000000000000000000, -6.982962677686266711E-15 ) ) ;
#163378 = DIRECTION ( 'NONE',  ( 1.000000000000000000, -0.000000000000000000, -0.000000000000000000 ) ) ;
#163379 = AXIS2_PLACEMENT_3D ( 'NONE', #231984, #7792, #112030 ) ;
#163380 = AXIS2_PLACEMENT_3D ( 'NONE', #1227, #160359, #61225 ) ;
#163382 = ORIENTED_EDGE ( 'NONE', *, *, #217194, .T. ) ;
#163381 = AXIS2_PLACEMENT_3D ( 'NONE', #133242, #157986, #116260 ) ;
#163383 = DIRECTION ( 'NONE',  ( 1.186688945009010077E-16, 0.4088369013363281623, -0.9126074666063771490 ) ) ;
#163384 = ORIENTED_EDGE ( 'NONE', *, *, #14430, .F. ) ;
#163385 = AXIS2_PLACEMENT_3D ( 'NONE', #160336, #19527, #181171 ) ;
#163387 = ORIENTED_EDGE ( 'NONE', *, *, #203713, .T. ) ;
#163386 = ORIENTED_EDGE ( 'NONE', *, *, #71757, .T. ) ;
#163388 = EDGE_LOOP ( 'NONE', ( #95755, #48222, #188934, #180340 ) ) ;
#163389 = CARTESIAN_POINT ( 'NONE',  ( -18.34374000495060386, 11.47316190337362585, -42.74999999999999289 ) ) ;
#163390 = VERTEX_POINT ( 'NONE', #88184 ) ;
#163391 = CARTESIAN_POINT ( 'NONE',  ( -20.64999999999999858, -8.999999999988844479, -191.1060308773475356 ) ) ;
#163392 = EDGE_LOOP ( 'NONE', ( #195467, #44693, #85143, #167681 ) ) ;
#163393 = CARTESIAN_POINT ( 'NONE',  ( -16.92973740335365562, 66.00749618554431208, -48.61704844932231850 ) ) ;
#163394 = AXIS2_PLACEMENT_3D ( 'NONE', #9840, #72405, #29449 ) ;
#163395 = DIRECTION ( 'NONE',  ( 0.000000000000000000, -7.172728831056617961E-15, 1.000000000000000000 ) ) ;
#163397 = ORIENTED_EDGE ( 'NONE', *, *, #180835, .F. ) ;
#163396 = AXIS2_PLACEMENT_3D ( 'NONE', #146170, #44524, #122789 ) ;
#163398 = ORIENTED_EDGE ( 'NONE', *, *, #186775, .F. ) ;
#163399 = CIRCLE ( 'NONE', #38498, 0.6000000000000005329 ) ;
#163400 = VECTOR ( 'NONE', #170262, 1000.000000000000000 ) ;
#163401 = ORIENTED_EDGE ( 'NONE', *, *, #6508, .T. ) ;
#163402 = EDGE_CURVE ( 'NONE', #95143, #249646, #99745, .T. ) ;
#163403 = CIRCLE ( 'NONE', #130638, 0.1999999999999987899 ) ;
#163404 = AXIS2_PLACEMENT_3D ( 'NONE', #196224, #253617, #213211 ) ;
#163405 = DIRECTION ( 'NONE',  ( 1.000000000000000000, 0.000000000000000000, 0.000000000000000000 ) ) ;
#163406 = VERTEX_POINT ( 'NONE', #39829 ) ;
#163407 = AXIS2_PLACEMENT_3D ( 'NONE', #185861, #129742, #132305 ) ;
#163408 = FACE_OUTER_BOUND ( 'NONE', #141924, .T. ) ;
#163409 = CARTESIAN_POINT ( 'NONE',  ( -20.54999999999999716, 85.00000000001188027, -93.12913836187181005 ) ) ;
#163410 = DIRECTION ( 'NONE',  ( 2.952720810173289112E-16, -1.000000000000000000, -0.000000000000000000 ) ) ;
#163411 = FACE_OUTER_BOUND ( 'NONE', #32011, .T. ) ;
#163412 = CARTESIAN_POINT ( 'NONE',  ( 18.69999999999999929, 9.511171963237318394, 1.617965922123942191 ) ) ;
#163413 = DIRECTION ( 'NONE',  ( -0.000000000000000000, 0.2128009952263603677, -0.9770955615653313941 ) ) ;
#163415 = CARTESIAN_POINT ( 'NONE',  ( 21.05000000000000071, 34.04174220360669523, -243.6657363632959914 ) ) ;
#163414 = CARTESIAN_POINT ( 'NONE',  ( -20.54999999999999716, 76.00000000001126921, -203.5231074845248997 ) ) ;
#163416 = DIRECTION ( 'NONE',  ( 0.000000000000000000, 0.000000000000000000, -1.000000000000000000 ) ) ;
#163417 = LINE ( 'NONE', #143828, #94598 ) ;
#163418 = FACE_OUTER_BOUND ( 'NONE', #147173, .T. ) ;
#163419 = EDGE_CURVE ( 'NONE', #1139, #68228, #121747, .T. ) ;
#163420 = FACE_OUTER_BOUND ( 'NONE', #120522, .T. ) ;
#163421 = VECTOR ( 'NONE', #62195, 1000.000000000000000 ) ;
#163423 = EDGE_LOOP ( 'NONE', ( #193347, #113401, #117518, #91902, #235881, #145475, #50082, #92866, #152807, #214148, #11401 ) ) ;
#163422 = AXIS2_PLACEMENT_3D ( 'NONE', #44291, #84641, #24747 ) ;
#163424 = AXIS2_PLACEMENT_3D ( 'NONE', #140374, #122116, #227617 ) ;
#163426 = VERTEX_POINT ( 'NONE', #78897 ) ;
#163425 = CARTESIAN_POINT ( 'NONE',  ( 21.05000000000000071, -1.360870587180885716, -142.0729979270909951 ) ) ;
#163427 = ORIENTED_EDGE ( 'NONE', *, *, #195148, .F. ) ;
#163428 = FACE_OUTER_BOUND ( 'NONE', #191337, .T. ) ;
#163429 = CARTESIAN_POINT ( 'NONE',  ( -16.92507428761700439, 9.950000000011138823, -54.28660254037843913 ) ) ;
#163430 = CARTESIAN_POINT ( 'NONE',  ( 20.94999999999999929, 67.23127455305835554, -235.8551265064784559 ) ) ;
#163431 = VERTEX_POINT ( 'NONE', #94625 ) ;
#163432 = SHAPE_REPRESENTATION_RELATIONSHIP ( 'NONE' , 'NONE' ,  #168659, #157328 ) ;
#163433 = CARTESIAN_POINT ( 'NONE',  ( -22.57320508075687115, 64.35000000001238618, -170.0231074845243882 ) ) ;
#163434 = CARTESIAN_POINT ( 'NONE',  ( 21.05000000000000071, 8.433899723187009201, -209.4150263691077782 ) ) ;
#163435 = ORIENTED_EDGE ( 'NONE', *, *, #241156, .F. ) ;
#163436 = CARTESIAN_POINT ( 'NONE',  ( 20.85000000000000142, 87.75000000001172396, -72.42310748452422331 ) ) ;
#163437 = DIRECTION ( 'NONE',  ( 0.000000000000000000, 0.9651348961777157509, -0.2617529984165031243 ) ) ;
#163438 = DIRECTION ( 'NONE',  ( 0.000000000000000000, 7.109473446599835262E-15, -1.000000000000000000 ) ) ;
#163439 = VECTOR ( 'NONE', #79801, 1000.000000000000000 ) ;
#163440 = DIRECTION ( 'NONE',  ( -3.035766082959430717E-14, 0.000000000000000000, -1.000000000000000000 ) ) ;
#163442 = VERTEX_POINT ( 'NONE', #175479 ) ;
#163441 = CARTESIAN_POINT ( 'NONE',  ( -20.85882249326303040, 67.49222854868494892, -195.4187676019683693 ) ) ;
#163443 = DIRECTION ( 'NONE',  ( 0.000000000000000000, -1.000000000000000000, 0.000000000000000000 ) ) ;
#163445 = VERTEX_POINT ( 'NONE', #76334 ) ;
#163444 = CARTESIAN_POINT ( 'NONE',  ( 18.59999999999999787, -10.64999999999999325, 32.89999999999999858 ) ) ;
#163446 = DIRECTION ( 'NONE',  ( 0.000000000000000000, -6.547589603894034005E-15, 1.000000000000000000 ) ) ;
#163447 = DIRECTION ( 'NONE',  ( 1.000000000000000000, -0.000000000000000000, -0.000000000000000000 ) ) ;
#163448 = EDGE_LOOP ( 'NONE', ( #173755, #192415, #80261, #32240 ) ) ;
#163449 = DIRECTION ( 'NONE',  ( 2.557131231893037478E-16, 0.8660254037844420383, -0.4999999999999942824 ) ) ;
#163450 = CARTESIAN_POINT ( 'NONE',  ( 22.39999999999999503, 59.68594599439719417, -233.9123800762197902 ) ) ;
#163452 = DIRECTION ( 'NONE',  ( 0.000000000000000000, -7.147358527629762208E-15, 1.000000000000000000 ) ) ;
#163451 = CARTESIAN_POINT ( 'NONE',  ( -16.94107738177414291, 63.04990807712500356, -213.0142932718104021 ) ) ;
#163453 = CARTESIAN_POINT ( 'NONE',  ( -18.79999999999999716, 1.885425182446133885, -11.49641995933507843 ) ) ;
#163455 = EDGE_CURVE ( 'NONE', #191031, #114960, #179334, .T. ) ;
#163454 = CARTESIAN_POINT ( 'NONE',  ( -16.87036670365549895, 65.91505003675732155, -190.9731074845244336 ) ) ;
#163456 = DIRECTION ( 'NONE',  ( 0.000000000000000000, 0.2128009952263403282, -0.9770955615653358350 ) ) ;
#163457 = CARTESIAN_POINT ( 'NONE',  ( -20.64999999999999858, 82.09643798151613225, -215.4278993322501208 ) ) ;
#163458 = FACE_OUTER_BOUND ( 'NONE', #56572, .T. ) ;
#163459 = ORIENTED_EDGE ( 'NONE', *, *, #183202, .F. ) ;
#163460 = DIRECTION ( 'NONE',  ( 0.000000000000000000, 0.9126074666063660468, 0.4088369013363524762 ) ) ;
#163461 = ORIENTED_EDGE ( 'NONE', *, *, #200132, .F. ) ;
#163462 = ORIENTED_EDGE ( 'NONE', *, *, #203143, .F. ) ;
#163463 = EDGE_CURVE ( 'NONE', #28696, #38071, #187408, .T. ) ;
#163464 = CARTESIAN_POINT ( 'NONE',  ( 20.77526135991773515, 67.06799098339033094, -94.55453894179980523 ) ) ;
#163465 = CARTESIAN_POINT ( 'NONE',  ( -20.15000000000000568, 30.24795051788250433, -235.5764561060020981 ) ) ;
#163466 = ORIENTED_EDGE ( 'NONE', *, *, #210429, .T. ) ;
#163467 = EDGE_CURVE ( 'NONE', #220244, #87859, #191824, .T. ) ;
#163468 = VERTEX_POINT ( 'NONE', #198868 ) ;
#163469 = AXIS2_PLACEMENT_3D ( 'NONE', #188530, #11186, #26923 ) ;
#163470 = EDGE_CURVE ( 'NONE', #365, #43729, #174217, .T. ) ;
#163471 = ORIENTED_EDGE ( 'NONE', *, *, #185670, .T. ) ;
#163472 = CARTESIAN_POINT ( 'NONE',  ( -18.59999999999999787, 11.75000000000000000, 30.00000000000000000 ) ) ;
#163473 = ORIENTED_EDGE ( 'NONE', *, *, #86271, .T. ) ;
#163474 = CIRCLE ( 'NONE', #138321, 0.09999999999999942268 ) ;
#163475 = CARTESIAN_POINT ( 'NONE',  ( -20.54999999999999716, 13.63658454968486389, -219.6758818217417968 ) ) ;
#163476 = CARTESIAN_POINT ( 'NONE',  ( 20.02499999999999858, 9.750000000011153745, -54.75000000000000711 ) ) ;
#163477 = DIRECTION ( 'NONE',  ( 0.000000000000000000, -0.2617529984165031243, -0.9651348961777158619 ) ) ;
#163478 = CARTESIAN_POINT ( 'NONE',  ( 21.05000000000000071, 64.40000000001218439, -143.4513107147999449 ) ) ;
#163479 = LINE ( 'NONE', #64382, #173487 ) ;
#163480 = AXIS2_PLACEMENT_3D ( 'NONE', #32317, #227922, #107976 ) ;
#163481 = CARTESIAN_POINT ( 'NONE',  ( 23.14999999999999503, 51.38014393322265505, -230.1906178717505327 ) ) ;
#163482 = DIRECTION ( 'NONE',  ( -0.000000000000000000, 0.000000000000000000, -1.000000000000000000 ) ) ;
#163484 = VERTEX_POINT ( 'NONE', #219708 ) ;
#163483 = CARTESIAN_POINT ( 'NONE',  ( 21.05000000000000071, 44.18296097254452803, -236.5637753386232589 ) ) ;
#163486 = DIRECTION ( 'NONE',  ( 0.000000000000000000, 0.000000000000000000, -1.000000000000000000 ) ) ;
#163485 = CARTESIAN_POINT ( 'NONE',  ( 20.94999999999999574, 65.52661458509869874, -61.94445302027585143 ) ) ;
#163487 = EDGE_CURVE ( 'NONE', #226829, #47866, #25112, .T. ) ;
#163488 = CARTESIAN_POINT ( 'NONE',  ( -22.39999999999999503, 76.00000000001170974, -77.31388708289772183 ) ) ;
#163489 = VERTEX_POINT ( 'NONE', #38522 ) ;
#163490 = LINE ( 'NONE', #26565, #27226 ) ;
#163491 = DIRECTION ( 'NONE',  ( 0.000000000000000000, 0.000000000000000000, -1.000000000000000000 ) ) ;
#163492 = ORIENTED_EDGE ( 'NONE', *, *, #171322, .F. ) ;
#163493 = VECTOR ( 'NONE', #35784, 1000.000000000000000 ) ;
#163496 = CARTESIAN_POINT ( 'NONE',  ( -21.07928932188134041, 6.328516656404449492, -33.40110485434561127 ) ) ;
#163495 = CIRCLE ( 'NONE', #67631, 0.1999999999999987899 ) ;
#163494 = DIRECTION ( 'NONE',  ( 1.000000000000000000, 0.000000000000000000, 0.000000000000000000 ) ) ;
#163497 = CYLINDRICAL_SURFACE ( 'NONE', #148113, 0.09999999999999939493 ) ;
#163498 = ORIENTED_EDGE ( 'NONE', *, *, #143065, .F. ) ;
#163499 = CARTESIAN_POINT ( 'NONE',  ( -20.64999999999999858, 1.115600667400684642E-11, -134.0000000000000000 ) ) ;
#163500 = DIRECTION ( 'NONE',  ( 0.000000000000000000, 0.000000000000000000, 1.000000000000000000 ) ) ;
#163501 = AXIS2_PLACEMENT_3D ( 'NONE', #202105, #140847, #196951 ) ;
#163502 = FACE_OUTER_BOUND ( 'NONE', #164564, .T. ) ;
#163503 = FACE_OUTER_BOUND ( 'NONE', #160269, .T. ) ;
#163504 = ORIENTED_EDGE ( 'NONE', *, *, #227044, .F. ) ;
#163505 = ORIENTED_EDGE ( 'NONE', *, *, #151561, .T. ) ;
#163506 = ADVANCED_FACE ( 'NONE', ( #154641 ), #58371, .F. ) ;
#163507 = VECTOR ( 'NONE', #214489, 1000.000000000000227 ) ;
#163508 = CIRCLE ( 'NONE', #51043, 4.299999999999969624 ) ;
#163509 = AXIS2_PLACEMENT_3D ( 'NONE', #79364, #155107, #257969 ) ;
#163510 = LINE ( 'NONE', #160955, #248324 ) ;
#163511 = CARTESIAN_POINT ( 'NONE',  ( -18.59999999999999787, 64.35000000001180354, -81.67310748452439384 ) ) ;
#163512 = FACE_OUTER_BOUND ( 'NONE', #90050, .T. ) ;
#163513 = DIRECTION ( 'NONE',  ( 1.000000000000000000, 0.000000000000000000, 0.000000000000000000 ) ) ;
#163514 = DIRECTION ( 'NONE',  ( 0.000000000000000000, -0.8814952561688437216, 0.4721928772777334582 ) ) ;
#163515 = CARTESIAN_POINT ( 'NONE',  ( -23.15000000000000213, 76.00000000001244871, -170.0231074845243597 ) ) ;
#163516 = EDGE_CURVE ( 'NONE', #44981, #245138, #58184, .T. ) ;
#163518 = ORIENTED_EDGE ( 'NONE', *, *, #223660, .T. ) ;
#163517 = DIRECTION ( 'NONE',  ( -1.000000000000000000, -0.000000000000000000, 0.000000000000000000 ) ) ;
#163519 = CARTESIAN_POINT ( 'NONE',  ( 15.74999999999999645, 66.65000000001204228, -119.7731074845243739 ) ) ;
#163520 = DIRECTION ( 'NONE',  ( 1.000000000000000000, -0.000000000000000000, -0.000000000000000000 ) ) ;
#163521 = CARTESIAN_POINT ( 'NONE',  ( -21.64999999999999858, 9.690755012883050412, -211.4266134137857023 ) ) ;
#163522 = CARTESIAN_POINT ( 'NONE',  ( 21.05000000000000426, 6.258817194692633201, -167.4663672646663599 ) ) ;
#163523 = DIRECTION ( 'NONE',  ( 0.000000000000000000, -0.2617529984165031243, -0.9651348961777157509 ) ) ;
#163525 = VERTEX_POINT ( 'NONE', #159754 ) ;
#163524 = CARTESIAN_POINT ( 'NONE',  ( 21.05543885634738643, 67.22422895316402958, -57.33872301380969816 ) ) ;
#163526 = DIRECTION ( 'NONE',  ( 0.000000000000000000, 0.2128009952263601179, -0.9770955615653315052 ) ) ;
#163527 = DIRECTION ( 'NONE',  ( 1.040834085586054469E-13, -1.000000000000000000, 0.000000000000000000 ) ) ;
#163528 = DIRECTION ( 'NONE',  ( 0.000000000000000000, -0.9654727137038715545, 0.2605042016806676242 ) ) ;
#163529 = DIRECTION ( 'NONE',  ( 0.000000000000000000, 0.000000000000000000, 1.000000000000000000 ) ) ;
#163530 = EDGE_CURVE ( 'NONE', #213938, #33839, #98437, .T. ) ;
#163531 = ORIENTED_EDGE ( 'NONE', *, *, #174718, .T. ) ;
#163532 = CARTESIAN_POINT ( 'NONE',  ( -15.66061380678751291, 66.63927620602623847, -152.7091802899176116 ) ) ;
#163533 = DIRECTION ( 'NONE',  ( 0.000000000000000000, 1.000000000000000000, 6.982962677686266711E-15 ) ) ;
#163534 = CARTESIAN_POINT ( 'NONE',  ( 18.54999999999999716, 11.24151875332161765, -211.4982501455723138 ) ) ;
#163535 = ADVANCED_FACE ( 'NONE', ( #193741 ), #77610, .F. ) ;
#163536 = CIRCLE ( 'NONE', #196841, 0.09999999999999543976 ) ;
#163537 = DIRECTION ( 'NONE',  ( 1.000000000000000000, 0.000000000000000000, -0.000000000000000000 ) ) ;
#163538 = ORIENTED_EDGE ( 'NONE', *, *, #42349, .F. ) ;
#163539 = CIRCLE ( 'NONE', #51066, 0.09999999999999939493 ) ;
#163540 = CARTESIAN_POINT ( 'NONE',  ( -21.44999999999999929, 68.65000000001199965, -115.3731074845243540 ) ) ;
#163541 = ORIENTED_EDGE ( 'NONE', *, *, #75946, .F. ) ;
#163542 = DIRECTION ( 'NONE',  ( 0.000000000000000000, -0.2128009952263604232, 0.9770955615653316162 ) ) ;
#163543 = CARTESIAN_POINT ( 'NONE',  ( -20.64999999999999858, 1.115625160336667635E-11, -69.00000000000000000 ) ) ;
#163544 = TOROIDAL_SURFACE ( 'NONE', #51072, 7.800000000000000711, 0.1000000000000000056 ) ;
#163545 = EDGE_CURVE ( 'NONE', #196505, #109895, #58054, .T. ) ;
#163546 = CARTESIAN_POINT ( 'NONE',  ( -21.05000000000000071, 1.115649653272650466E-11, -104.5000000000000568 ) ) ;
#163547 = CARTESIAN_POINT ( 'NONE',  ( 19.97071067811864609, 61.50763418579565212, -212.1815653095142693 ) ) ;
#163548 = EDGE_LOOP ( 'NONE', ( #134875, #51929, #87725, #201010 ) ) ;
#163549 = AXIS2_PLACEMENT_3D ( 'NONE', #50262, #129810, #209347 ) ;
#163550 = ADVANCED_FACE ( 'NONE', ( #118048 ), #197577, .T. ) ;
#163552 = ADVANCED_FACE ( 'NONE', ( #18939 ), #66783, .F. ) ;
#163551 = FACE_OUTER_BOUND ( 'NONE', #36392, .T. ) ;
#163553 = AXIS2_PLACEMENT_3D ( 'NONE', #162702, #3605, #4863 ) ;
#163554 = FACE_OUTER_BOUND ( 'NONE', #32870, .T. ) ;
#163555 = VECTOR ( 'NONE', #217556, 1000.000000000000000 ) ;
#163556 = AXIS2_PLACEMENT_3D ( 'NONE', #88644, #165664, #27461 ) ;
#163557 = CARTESIAN_POINT ( 'NONE',  ( 13.77030915526558275, 9.456007326069306274, -18.48863349414675383 ) ) ;
#163558 = CARTESIAN_POINT ( 'NONE',  ( -16.96982749440706328, 9.949999999999983302, -20.37522159118827858 ) ) ;
#163560 = CARTESIAN_POINT ( 'NONE',  ( 20.94999999999999929, -4.259020970815407203, -226.0869574510824123 ) ) ;
#163559 = VECTOR ( 'NONE', #163855, 1000.000000000000000 ) ;
#163561 = ORIENTED_EDGE ( 'NONE', *, *, #6731, .F. ) ;
#163563 = ORIENTED_EDGE ( 'NONE', *, *, #120714, .T. ) ;
#163562 = CARTESIAN_POINT ( 'NONE',  ( -20.85000000000000142, -1.164121893230052995, -74.81484808557161159 ) ) ;
#163564 = TOROIDAL_SURFACE ( 'NONE', #51097, 11.70000000000000639, 0.1000000000000000056 ) ;
#163565 = EDGE_CURVE ( 'NONE', #1366, #171058, #133475, .T. ) ;
#163566 = EDGE_LOOP ( 'NONE', ( #136378, #222254, #1967, #49435, #213265 ) ) ;
#163567 = CARTESIAN_POINT ( 'NONE',  ( 20.94999999999999574, 77.83534155023627932, -91.46795619196130644 ) ) ;
#163568 = ORIENTED_EDGE ( 'NONE', *, *, #84867, .T. ) ;
#163569 = CARTESIAN_POINT ( 'NONE',  ( -18.59999999999999787, 77.36242903720540198, -128.6342262366031548 ) ) ;
#163570 = DIRECTION ( 'NONE',  ( 1.000000000000000000, 0.000000000000000000, 0.000000000000000000 ) ) ;
#163571 = LINE ( 'NONE', #7051, #99827 ) ;
#163572 = ORIENTED_EDGE ( 'NONE', *, *, #212170, .F. ) ;
#163573 = ADVANCED_FACE ( 'NONE', ( #24116 ), #61937, .T. ) ;
#163574 = EDGE_CURVE ( 'NONE', #150597, #203670, #8512, .T. ) ;
#163575 = CARTESIAN_POINT ( 'NONE',  ( 18.59999999999999432, 68.58368164137472434, -224.2353459317783120 ) ) ;
#163576 = DIRECTION ( 'NONE',  ( 1.000000000000000000, 0.000000000000000000, 0.000000000000000000 ) ) ;
#163577 = AXIS2_PLACEMENT_3D ( 'NONE', #162218, #185607, #26549 ) ;
#163578 = ORIENTED_EDGE ( 'NONE', *, *, #96116, .T. ) ;
#163579 = CARTESIAN_POINT ( 'NONE',  ( 22.49999999999999645, 11.64957080755595520, -100.4000000000000483 ) ) ;
#163580 = CIRCLE ( 'NONE', #51109, 0.1000000000000028644 ) ;
#163582 = ORIENTED_EDGE ( 'NONE', *, *, #43507, .T. ) ;
#163581 = LINE ( 'NONE', #3191, #225753 ) ;
#163583 = DIRECTION ( 'NONE',  ( 1.000000000000000000, 0.000000000000000000, -0.000000000000000000 ) ) ;
#163584 = CARTESIAN_POINT ( 'NONE',  ( 23.14999999999999858, 36.65892442174935439, -249.5511627012433848 ) ) ;
#163585 = CIRCLE ( 'NONE', #34597, 0.09999999999999939493 ) ;
#163586 = AXIS2_PLACEMENT_3D ( 'NONE', #65208, #246426, #86025 ) ;
#163587 = VERTEX_POINT ( 'NONE', #123194 ) ;
#163588 = AXIS2_PLACEMENT_3D ( 'NONE', #134941, #179265, #35898 ) ;
#163589 = CIRCLE ( 'NONE', #85003, 0.1000000000000000472 ) ;
#163590 = CARTESIAN_POINT ( 'NONE',  ( -20.54999999999999716, 76.00000000001244871, -170.0231074845243597 ) ) ;
#163591 = DIRECTION ( 'NONE',  ( -1.000000000000000000, -0.000000000000000000, -0.000000000000000000 ) ) ;
#163592 = VECTOR ( 'NONE', #116782, 1000.000000000000000 ) ;
#163593 = CARTESIAN_POINT ( 'NONE',  ( 23.15000000000000213, 69.09936979046463534, -247.6075824278584889 ) ) ;
#163594 = ORIENTED_EDGE ( 'NONE', *, *, #153972, .F. ) ;
#163595 = LINE ( 'NONE', #138843, #29983 ) ;
#163596 = EDGE_CURVE ( 'NONE', #69817, #196984, #42369, .T. ) ;
#163597 = EDGE_CURVE ( 'NONE', #190383, #156526, #125054, .T. ) ;
#163598 = CARTESIAN_POINT ( 'NONE',  ( -18.79999999999999716, -1.467286812112899463, 32.89999999999999858 ) ) ;
#163599 = ORIENTED_EDGE ( 'NONE', *, *, #180822, .F. ) ;
#163600 = ADVANCED_FACE ( 'NONE', ( #204006 ), #121919, .F. ) ;
#163601 = VECTOR ( 'NONE', #100427, 1000.000000000000000 ) ;
#163602 = AXIS2_PLACEMENT_3D ( 'NONE', #33847, #212448, #12978 ) ;
#163603 = ORIENTED_EDGE ( 'NONE', *, *, #255063, .T. ) ;
#163604 = FACE_OUTER_BOUND ( 'NONE', #61894, .T. ) ;
#163605 = ORIENTED_EDGE ( 'NONE', *, *, #182684, .F. ) ;
#163606 = CARTESIAN_POINT ( 'NONE',  ( 18.50016250449482413, 10.29766095124067249, -38.97436639332788388 ) ) ;
#163607 = CARTESIAN_POINT ( 'NONE',  ( -16.77308656112215246, 66.05000000001254534, -182.6733006762267451 ) ) ;
#163610 = EDGE_LOOP ( 'NONE', ( #33774, #43415, #50442, #219980 ) ) ;
#163609 = DIRECTION ( 'NONE',  ( 0.000000000000000000, -0.2617529984164506107, -0.9651348961777299618 ) ) ;
#163608 =( BOUNDED_SURFACE ( )  B_SPLINE_SURFACE ( 3, 2, ( 
 ( #109996, #189556, #209101 ),
 ( #86558, #65741, #246934 ),
 ( #10919, #210407, #145260 ),
 ( #206537, #48736, #166164 ) ),
 .UNSPECIFIED., .F., .F., .F. ) 
 B_SPLINE_SURFACE_WITH_KNOTS ( ( 4, 4 ),
 ( 3, 3 ),
 ( 0.04058434257139457990, 0.04256401539001584966 ),
 ( 0.000000000000000000, 1.000000000000000000 ),
 .UNSPECIFIED. ) 
 GEOMETRIC_REPRESENTATION_ITEM ( )  RATIONAL_B_SPLINE_SURFACE ( (
 ( 1.000000000000000000, 0.7103081912007809251, 1.000000000000000000),
 ( 1.000000000000000000, 0.7104998333556791223, 1.000000000000000000),
 ( 1.000000000000000000, 0.7107238315753988678, 1.000000000000000000),
 ( 1.000000000000000000, 0.7110073749539779220, 1.000000000000000000) ) ) 
 REPRESENTATION_ITEM ( '' )  SURFACE ( )  );
#163611 = CARTESIAN_POINT ( 'NONE',  ( 21.05000000000000071, 11.75000000001115907, -126.9851942293460922 ) ) ;
#163612 = DIRECTION ( 'NONE',  ( -0.000000000000000000, -2.891205793294679805E-16, 1.000000000000000000 ) ) ;
#163613 = DIRECTION ( 'NONE',  ( -0.000000000000000000, 0.2493442905258256848, 0.9684149032218436481 ) ) ;
#163614 = CARTESIAN_POINT ( 'NONE',  ( -16.88853107394619357, 51.62118350788017551, -231.9444668182231339 ) ) ;
#163615 = DIRECTION ( 'NONE',  ( 0.000000000000000000, -0.8660254037844420383, 0.4999999999999942824 ) ) ;
#163616 = EDGE_CURVE ( 'NONE', #71227, #83974, #106172, .T. ) ;
#163617 = LINE ( 'NONE', #144030, #147211 ) ;
#163619 = ORIENTED_EDGE ( 'NONE', *, *, #233866, .T. ) ;
#163618 = DIRECTION ( 'NONE',  ( 1.000000000000000000, -2.952720810173289112E-16, -2.061873921506763405E-30 ) ) ;
#163621 = EDGE_LOOP ( 'NONE', ( #212092, #123363, #189969, #27894 ) ) ;
#163620 = CARTESIAN_POINT ( 'NONE',  ( 21.00000000000000000, 66.25000000001199396, -115.3731074845243683 ) ) ;
#163622 = CARTESIAN_POINT ( 'NONE',  ( 23.14999999999999858, 71.00000000001180922, -81.92837350343744163 ) ) ;
#163623 = ORIENTED_EDGE ( 'NONE', *, *, #55272, .F. ) ;
#163624 = EDGE_CURVE ( 'NONE', #225728, #235804, #33499, .T. ) ;
#163625 = DIRECTION ( 'NONE',  ( 0.000000000000000000, -0.2617529984165024026, -0.9651348961777158619 ) ) ;
#163626 = AXIS2_PLACEMENT_3D ( 'NONE', #170234, #249718, #172791 ) ;
#163627 = CARTESIAN_POINT ( 'NONE',  ( -23.15000000000000213, 11.75000000000000000, -21.35000000000000142 ) ) ;
#163629 = B_SPLINE_CURVE_WITH_KNOTS ( 'NONE', 3,
 ( #69363, #249279, #188018, #211425, #126750, #107176, #112338, #131889, #186743, #9357 ),
 .UNSPECIFIED., .F., .F.,
 ( 4, 3, 3, 4 ),
 ( 0.000000000000000000, 1.004626015991471073E-05, 1.831183478184062558E-05, 2.062343583996205056E-05 ),
 .UNSPECIFIED. ) ;
#163628 = AXIS2_PLACEMENT_3D ( 'NONE', #58018, #37216, #236667 ) ;
#163630 = FACE_OUTER_BOUND ( 'NONE', #231549, .T. ) ;
#163631 = EDGE_CURVE ( 'NONE', #68027, #110197, #145306, .T. ) ;
#163632 = CARTESIAN_POINT ( 'NONE',  ( 21.14999999999999858, 11.65000000000000391, -0.1000000000000028644 ) ) ;
#163633 = CARTESIAN_POINT ( 'NONE',  ( 23.14999999999999503, 69.35000000001151932, -48.37310748452436826 ) ) ;
#163634 = EDGE_CURVE ( 'NONE', #88477, #71888, #158395, .T. ) ;
#163635 = EDGE_LOOP ( 'NONE', ( #116527, #37512, #155281, #254832 ) ) ;
#163636 = DIRECTION ( 'NONE',  ( -0.000000000000000000, -0.4791956752371546169, -0.8777080977375152360 ) ) ;
#163637 =( NAMED_UNIT ( * ) PLANE_ANGLE_UNIT ( ) SI_UNIT ( $, .RADIAN. ) );
#163638 = ORIENTED_EDGE ( 'NONE', *, *, #195758, .F. ) ;
#163640 = EDGE_CURVE ( 'NONE', #4681, #173033, #233404, .T. ) ;
#163639 = DIRECTION ( 'NONE',  ( -0.000000000000000000, 1.000000000000000000, -0.000000000000000000 ) ) ;
#163641 = AXIS2_PLACEMENT_3D ( 'NONE', #51263, #128274, #133411 ) ;
#163642 = ADVANCED_FACE ( 'NONE', ( #7085 ), #4512, .F. ) ;
#163643 = LINE ( 'NONE', #222289, #155402 ) ;
#163644 = EDGE_LOOP ( 'NONE', ( #72303, #155255, #98050, #218336 ) ) ;
#163645 = CARTESIAN_POINT ( 'NONE',  ( -15.75000000000000355, 66.65000000001204228, -119.7731074845243739 ) ) ;
#163646 = EDGE_LOOP ( 'NONE', ( #197011, #169092, #230193, #50652 ) ) ;
#163647 = EDGE_CURVE ( 'NONE', #106553, #37051, #144023, .T. ) ;
#163648 = CARTESIAN_POINT ( 'NONE',  ( -14.45443560709636976, 9.450592112144857282, -48.55618831880839537 ) ) ;
#163649 = EDGE_LOOP ( 'NONE', ( #107931, #138966, #148626, #210406 ) ) ;
#163650 = CARTESIAN_POINT ( 'NONE',  ( -21.37071067811865532, 52.66096799524555649, -233.5388714123112095 ) ) ;
#163651 = CARTESIAN_POINT ( 'NONE',  ( 23.14999999999999858, 1.115600667400684642E-11, -67.00000000000000000 ) ) ;
#163652 = ORIENTED_EDGE ( 'NONE', *, *, #182856, .T. ) ;
#163654 = FACE_OUTER_BOUND ( 'NONE', #76234, .T. ) ;
#163653 = AXIS2_PLACEMENT_3D ( 'NONE', #209377, #226349, #245949 ) ;
#163656 = VERTEX_POINT ( 'NONE', #41110 ) ;
#163655 = DIRECTION ( 'NONE',  ( 0.000000000000000000, -7.429790795770644761E-15, 1.000000000000000000 ) ) ;
#163657 = EDGE_CURVE ( 'NONE', #217421, #89621, #71070, .T. ) ;
#163658 = DIRECTION ( 'NONE',  ( 1.000000000000000000, -0.000000000000000000, -0.000000000000000000 ) ) ;
#163659 = EDGE_CURVE ( 'NONE', #128551, #42653, #142675, .T. ) ;
#163660 = ORIENTED_EDGE ( 'NONE', *, *, #67626, .T. ) ;
#163661 = AXIS2_PLACEMENT_3D ( 'NONE', #53282, #187674, #208519 ) ;
#163662 = TOROIDAL_SURFACE ( 'NONE', #117856, 0.2000000000000000111, 0.1000000000000000056 ) ;
#163663 = EDGE_CURVE ( 'NONE', #112510, #173885, #190905, .T. ) ;
#163664 = ORIENTED_EDGE ( 'NONE', *, *, #1653, .F. ) ;
#163665 = CARTESIAN_POINT ( 'NONE',  ( 18.49999999999999645, 76.00000000001190870, -103.0231074845243029 ) ) ;
#163666 = DIRECTION ( 'NONE',  ( 0.000000000000000000, -0.2617529984164856383, -0.9651348961777204138 ) ) ;
#163668 = EDGE_CURVE ( 'NONE', #144042, #29656, #12631, .T. ) ;
#163667 = FACE_OUTER_BOUND ( 'NONE', #241719, .T. ) ;
#163669 = CARTESIAN_POINT ( 'NONE',  ( 18.69999999999999929, 6.841561409100513025, 9.675512259591560138 ) ) ;
#163670 = EDGE_CURVE ( 'NONE', #108752, #117253, #29394, .T. ) ;
#163671 = FACE_OUTER_BOUND ( 'NONE', #201120, .T. ) ;
#163672 = AXIS2_PLACEMENT_3D ( 'NONE', #172123, #157698, #237194 ) ;
#163673 = ORIENTED_EDGE ( 'NONE', *, *, #236961, .T. ) ;
#163674 = AXIS2_PLACEMENT_3D ( 'NONE', #188676, #10039, #89564 ) ;
#163675 = DIRECTION ( 'NONE',  ( 0.000000000000000000, 1.000000000000000000, 6.982962677686266711E-15 ) ) ;
#163676 = DIRECTION ( 'NONE',  ( -0.000000000000000000, -0.4791956752371546724, -0.8777080977375153470 ) ) ;
#163677 = DIRECTION ( 'NONE',  ( 1.000000000000000000, 0.000000000000000000, 0.000000000000000000 ) ) ;
#163678 = CIRCLE ( 'NONE', #105380, 7.900000000000000355 ) ;
#163679 = CARTESIAN_POINT ( 'NONE',  ( 23.14999999999999858, 3.999999999999999112, -33.50000000000000000 ) ) ;
#163680 = ORIENTED_EDGE ( 'NONE', *, *, #188343, .F. ) ;
#163681 = CARTESIAN_POINT ( 'NONE',  ( 23.24999999999999645, 1.115600667400684642E-11, -100.5000000000000426 ) ) ;
#163682 = ORIENTED_EDGE ( 'NONE', *, *, #144522, .T. ) ;
#163683 = DIRECTION ( 'NONE',  ( 0.000000000000000000, 1.000000000000000000, 0.000000000000000000 ) ) ;
#163684 = ORIENTED_EDGE ( 'NONE', *, *, #113019, .F. ) ;
#163685 = DIRECTION ( 'NONE',  ( 1.000000000000000000, 0.000000000000000000, 0.000000000000000000 ) ) ;
#163686 = CARTESIAN_POINT ( 'NONE',  ( -20.86777300164945004, 10.33200063080771969, -72.59316749566428939 ) ) ;
#163688 = ORIENTED_EDGE ( 'NONE', *, *, #106383, .F. ) ;
#163687 = AXIS2_PLACEMENT_3D ( 'NONE', #219881, #257662, #199044 ) ;
#163690 = ORIENTED_EDGE ( 'NONE', *, *, #235623, .F. ) ;
#163689 = CYLINDRICAL_SURFACE ( 'NONE', #77998, 0.09999999999999939493 ) ;
#163691 = EDGE_CURVE ( 'NONE', #64537, #113079, #191716, .T. ) ;
#163692 = CARTESIAN_POINT ( 'NONE',  ( 23.15000000000000213, -11.48912529306489994, -130.9000000000000341 ) ) ;
#163693 = VERTEX_POINT ( 'NONE', #90474 ) ;
#163694 = DIRECTION ( 'NONE',  ( 1.000000000000000000, -2.952720810173289112E-16, -2.061873921506763405E-30 ) ) ;
#163695 = AXIS2_PLACEMENT_3D ( 'NONE', #125663, #48691, #189508 ) ;
#163696 = AXIS2_PLACEMENT_3D ( 'NONE', #115510, #56793, #93378 ) ;
#163697 = AXIS2_PLACEMENT_3D ( 'NONE', #77925, #192765, #175778 ) ;
#163698 = FACE_OUTER_BOUND ( 'NONE', #154660, .T. ) ;
#163699 = AXIS2_PLACEMENT_3D ( 'NONE', #155839, #136218, #176684 ) ;
#163701 = ORIENTED_EDGE ( 'NONE', *, *, #96461, .T. ) ;
#163700 = ADVANCED_FACE ( 'NONE', ( #211736 ), #250828, .T. ) ;
#163702 = SPHERICAL_SURFACE ( 'NONE', #206094, 0.1000000000000000056 ) ;
#163703 = DIRECTION ( 'NONE',  ( -1.000000000000000000, -3.448943450116723568E-16, -6.438528483529607644E-16 ) ) ;
#163704 = ORIENTED_EDGE ( 'NONE', *, *, #100263, .F. ) ;
#163705 = VERTEX_POINT ( 'NONE', #110044 ) ;
#163706 = DIRECTION ( 'NONE',  ( 0.7071067811865474617, -0.6824534298470372740, 0.1850873201762209819 ) ) ;
#163707 =( BOUNDED_CURVE ( )  B_SPLINE_CURVE ( 3, ( #234796, #138238, #36629, #212674 ),
 .UNSPECIFIED., .F., .T. ) 
 B_SPLINE_CURVE_WITH_KNOTS ( ( 4, 4 ),
 ( 1.570796326794895448, 3.141592653589791784 ),
 .UNSPECIFIED. ) 
 CURVE ( )  GEOMETRIC_REPRESENTATION_ITEM ( )  RATIONAL_B_SPLINE_CURVE ( ( 1.000000000000000000, 0.8047378541243650485, 0.8047378541243650485, 1.000000000000000000 ) ) 
 REPRESENTATION_ITEM ( '' )  );
#163708 = EDGE_CURVE ( 'NONE', #248652, #120342, #93537, .T. ) ;
#163710 = ORIENTED_EDGE ( 'NONE', *, *, #224874, .F. ) ;
#163709 = FACE_OUTER_BOUND ( 'NONE', #10105, .T. ) ;
#163711 = DIRECTION ( 'NONE',  ( 1.000000000000000000, 0.000000000000000000, 0.000000000000000000 ) ) ;
#163712 = FACE_OUTER_BOUND ( 'NONE', #94193, .T. ) ;
#163713 = DIRECTION ( 'NONE',  ( -1.000000000000000000, 0.000000000000000000, 0.000000000000000000 ) ) ;
#163714 = AXIS2_PLACEMENT_3D ( 'NONE', #86242, #161984, #26306 ) ;
#163716 = CARTESIAN_POINT ( 'NONE',  ( -27.30103769104855971, 12.19999999999999574, -347.0000000000001137 ) ) ;
#163715 = CARTESIAN_POINT ( 'NONE',  ( -21.05000000000000071, 77.83534155023598089, -57.96795619196132776 ) ) ;
#163717 = FACE_OUTER_BOUND ( 'NONE', #25819, .T. ) ;
#163718 = CARTESIAN_POINT ( 'NONE',  ( -18.59999999999999787, 11.65000000001115232, -174.5148057706539930 ) ) ;
#163719 = CIRCLE ( 'NONE', #22086, 0.2000000000000057288 ) ;
#163720 = CARTESIAN_POINT ( 'NONE',  ( 23.14999999999998437, 1.115600667400684642E-11, -167.4999999999999716 ) ) ;
#163721 = B_SPLINE_CURVE_WITH_KNOTS ( 'NONE', 3,
 ( #222539, #123465, #183444, #4767, #58325, #119627, #38803, #118342 ),
 .UNSPECIFIED., .F., .F.,
 ( 4, 2, 2, 4 ),
 ( 0.000000000000000000, 0.0001094981963948479494, 0.0002189963927896958987, 0.0004379927855793917975 ),
 .UNSPECIFIED. ) ;
#163722 = EDGE_CURVE ( 'NONE', #144062, #91963, #187605, .T. ) ;
#163723 = DIRECTION ( 'NONE',  ( 1.000000000000000000, -0.000000000000000000, -0.000000000000000000 ) ) ;
#163724 = ORIENTED_EDGE ( 'NONE', *, *, #258032, .F. ) ;
#163725 = AXIS2_PLACEMENT_3D ( 'NONE', #20035, #79952, #38304 ) ;
#163726 = VERTEX_POINT ( 'NONE', #10958 ) ;
#163728 = DIRECTION ( 'NONE',  ( -1.073024830501117725E-15, 6.982962677686266711E-15, -1.000000000000000000 ) ) ;
#163727 = TOROIDAL_SURFACE ( 'NONE', #122026, 2.100000000000002309, 0.1000000000000000056 ) ;
#163729 = ORIENTED_EDGE ( 'NONE', *, *, #4582, .F. ) ;
#163730 = DIRECTION ( 'NONE',  ( 0.000000000000000000, -6.938893903907222067E-15, 1.000000000000000000 ) ) ;
#163731 = CIRCLE ( 'NONE', #51270, 4.000000000000003553 ) ;
#163732 = ORIENTED_EDGE ( 'NONE', *, *, #89019, .T. ) ;
#163734 = VECTOR ( 'NONE', #196111, 1000.000000000000114 ) ;
#163733 = SHAPE_REPRESENTATION_RELATIONSHIP ( 'NONE' , 'NONE' ,  #151872, #85670 ) ;
#163735 = CARTESIAN_POINT ( 'NONE',  ( 20.85882249326303040, 65.66751761918692409, -130.9282609406112670 ) ) ;
#163736 = CIRCLE ( 'NONE', #30483, 0.09999999999999939493 ) ;
#163737 = PRODUCT_DEFINITION_SHAPE ( 'NONE', 'NONE',  #21371 ) ;
#163738 = ORIENTED_EDGE ( 'NONE', *, *, #248168, .F. ) ;
#163739 = DIRECTION ( 'NONE',  ( 0.000000000000000000, -0.8660254037844377084, -0.5000000000000016653 ) ) ;
#163740 = ORIENTED_EDGE ( 'NONE', *, *, #214990, .F. ) ;
#163741 = EDGE_LOOP ( 'NONE', ( #244656, #58150, #191908, #22298, #65215, #27009, #8893, #61770, #200232, #31714, #215871, #103236, #179568, #155389, #55601, #254959 ) ) ;
#163742 = VECTOR ( 'NONE', #232931, 1000.000000000000000 ) ;
#163743 = CARTESIAN_POINT ( 'NONE',  ( 19.75857864376268935, 54.53338637621133955, -228.6684279704127789 ) ) ;
#163744 = DIRECTION ( 'NONE',  ( 1.000000000000000000, 0.000000000000000000, -0.000000000000000000 ) ) ;
#163746 = EDGE_LOOP ( 'NONE', ( #96329, #107250, #109135, #54921 ) ) ;
#163745 = CARTESIAN_POINT ( 'NONE',  ( -21.14999999999999858, -11.64999999998884483, -67.00000000000004263 ) ) ;
#163747 = CYLINDRICAL_SURFACE ( 'NONE', #140870, 0.1000000000000000472 ) ;
#163749 = ORIENTED_EDGE ( 'NONE', *, *, #22295, .T. ) ;
#163748 = DIRECTION ( 'NONE',  ( -1.000000000000000000, 0.000000000000000000, 0.000000000000000000 ) ) ;
#163750 = CARTESIAN_POINT ( 'NONE',  ( -20.64999999999999858, 6.878457983866232972, -212.1414458560986986 ) ) ;
#163751 = ORIENTED_EDGE ( 'NONE', *, *, #83939, .T. ) ;
#163752 = CARTESIAN_POINT ( 'NONE',  ( -18.50000000000000000, 76.00000000001213607, -136.5231074845242745 ) ) ;
#163753 = AXIS2_PLACEMENT_3D ( 'NONE', #89059, #112504, #192050 ) ;
#163755 = ORIENTED_EDGE ( 'NONE', *, *, #216639, .T. ) ;
#163754 = FACE_OUTER_BOUND ( 'NONE', #201224, .T. ) ;
#163756 = VECTOR ( 'NONE', #179354, 1000.000000000000000 ) ;
#163757 = CARTESIAN_POINT ( 'NONE',  ( 18.49999999999998934, 10.29288807859941457, -172.9580020160121592 ) ) ;
#163758 = CARTESIAN_POINT ( 'NONE',  ( -12.33960340485503693, 26.81162386565848621, -233.6570620184931215 ) ) ;
#163759 = ADVANCED_FACE ( 'NONE', ( #249575 ), #87886, .T. ) ;
#163760 = CARTESIAN_POINT ( 'NONE',  ( 21.05000000000000071, 8.776282895303632259, -75.55862899514100661 ) ) ;
#163761 = VERTEX_POINT ( 'NONE', #246981 ) ;
#163762 = VECTOR ( 'NONE', #246436, 1000.000000000000000 ) ;
#163763 = CARTESIAN_POINT ( 'NONE',  ( 23.14999999999999503, 13.96869538424789070, -210.3925794786331949 ) ) ;
#163764 = DIRECTION ( 'NONE',  ( 0.000000000000000000, -1.000000000000000000, 0.000000000000000000 ) ) ;
#163765 = CARTESIAN_POINT ( 'NONE',  ( -23.15000000000000213, 1.115648428625851357E-11, -163.6000000000000512 ) ) ;
#163766 = CARTESIAN_POINT ( 'NONE',  ( -20.05000000000000426, 9.250000000011157297, -79.35000000000005116 ) ) ;
#163767 = CARTESIAN_POINT ( 'NONE',  ( -17.11825945287483108, 44.13548170601893617, -235.2989316066074252 ) ) ;
#163769 = ORIENTED_EDGE ( 'NONE', *, *, #121231, .T. ) ;
#163768 = AXIS2_PLACEMENT_3D ( 'NONE', #118479, #257914, #98859 ) ;
#163770 = VERTEX_POINT ( 'NONE', #192175 ) ;
#163772 = ORIENTED_EDGE ( 'NONE', *, *, #34867, .T. ) ;
#163771 = AXIS2_PLACEMENT_3D ( 'NONE', #91814, #209187, #50108 ) ;
#163773 = DIRECTION ( 'NONE',  ( 0.000000000000000000, -0.2128009952272136851, 0.9770955615651456538 ) ) ;
#163774 = AXIS2_PLACEMENT_3D ( 'NONE', #178944, #2816, #164490 ) ;
#163775 = ORIENTED_EDGE ( 'NONE', *, *, #164804, .F. ) ;
#163776 = CARTESIAN_POINT ( 'NONE',  ( 21.05000000000000071, -11.64999999998883595, -134.0000000000000000 ) ) ;
#163777 = VERTEX_POINT ( 'NONE', #171358 ) ;
#163778 = ADVANCED_FACE ( 'NONE', ( #13527 ), #122, .T. ) ;
#163779 = CARTESIAN_POINT ( 'NONE',  ( -22.47071067811865674, 7.720074744509219045, -100.4009075452974429 ) ) ;
#163780 = DIRECTION ( 'NONE',  ( 1.000000000000000000, 0.000000000000000000, 0.000000000000000000 ) ) ;
#163781 = EDGE_CURVE ( 'NONE', #155087, #59363, #254204, .T. ) ;
#163782 = EDGE_LOOP ( 'NONE', ( #106830, #63611 ) ) ;
#163783 = DIRECTION ( 'NONE',  ( 0.000000000000000000, -1.000000000000000000, -6.982962677686265922E-15 ) ) ;
#163785 = EDGE_CURVE ( 'NONE', #221551, #141516, #229288, .T. ) ;
#163784 = AXIS2_PLACEMENT_3D ( 'NONE', #23201, #101373, #19325 ) ;
#163786 = AXIS2_PLACEMENT_3D ( 'NONE', #213295, #98447, #192465 ) ;
#163787 = EDGE_LOOP ( 'NONE', ( #121099, #108826, #5273, #25722 ) ) ;
#163788 = CIRCLE ( 'NONE', #217925, 0.09999999999999939493 ) ;
#163790 = ORIENTED_EDGE ( 'NONE', *, *, #255989, .F. ) ;
#163789 = CIRCLE ( 'NONE', #13948, 0.09999999999999892308 ) ;
#163791 = ORIENTED_EDGE ( 'NONE', *, *, #253867, .T. ) ;
#163792 = EDGE_CURVE ( 'NONE', #95961, #191338, #100066, .T. ) ;
#163793 = LINE ( 'NONE', #63378, #137763 ) ;
#163794 = SPHERICAL_SURFACE ( 'NONE', #61655, 0.1000000000000000056 ) ;
#163795 = DIRECTION ( 'NONE',  ( 1.000000000000000000, 7.304098846218134667E-16, 0.000000000000000000 ) ) ;
#163797 = EDGE_CURVE ( 'NONE', #3957, #242308, #79227, .T. ) ;
#163796 = CARTESIAN_POINT ( 'NONE',  ( 15.39170923737819585, 27.26819834643092477, -233.8689871410715853 ) ) ;
#163798 = CARTESIAN_POINT ( 'NONE',  ( -21.44999999999999929, 7.150000000011155876, -54.75000000000000000 ) ) ;
#163799 = CARTESIAN_POINT ( 'NONE',  ( -20.94999999999999929, 1.115600667400684642E-11, -67.00000000000004263 ) ) ;
#163800 = CARTESIAN_POINT ( 'NONE',  ( 20.94999999999999929, 76.00000000001190870, -103.0231074845243029 ) ) ;
#163801 = DIRECTION ( 'NONE',  ( -1.000000000000000000, 0.000000000000000000, 0.000000000000000000 ) ) ;
#163802 = VERTEX_POINT ( 'NONE', #113901 ) ;
#163804 = CARTESIAN_POINT ( 'NONE',  ( -16.90257928357875272, 12.41512770975328905, -211.2286145703175464 ) ) ;
#163803 = DIRECTION ( 'NONE',  ( 0.7071359030027302151, 0.2890794387707354418, -0.6452843503173697481 ) ) ;
#163805 = EDGE_CURVE ( 'NONE', #28235, #147882, #171069, .T. ) ;
#163806 = CARTESIAN_POINT ( 'NONE',  ( -20.94999999999999929, -1.362429037182149694, -208.8888812479211765 ) ) ;
#163807 = ORIENTED_EDGE ( 'NONE', *, *, #168544, .T. ) ;
#163808 = CARTESIAN_POINT ( 'NONE',  ( 20.95420533658165141, 10.54586447477073285, -74.56750602069328693 ) ) ;
#163809 = DIRECTION ( 'NONE',  ( 1.000000000000000000, -2.986185139342070877E-16, 6.665775143889692774E-16 ) ) ;
#163810 = DIRECTION ( 'NONE',  ( -1.836970198721029934E-16, 1.000000000000000000, 0.000000000000000000 ) ) ;
#163811 = ORIENTED_EDGE ( 'NONE', *, *, #244230, .T. ) ;
#163812 = EDGE_CURVE ( 'NONE', #125649, #189474, #223019, .T. ) ;
#163813 = CARTESIAN_POINT ( 'NONE',  ( 21.05000000000000071, 0.000000000000000000, -33.50000000000000000 ) ) ;
#163814 = CARTESIAN_POINT ( 'NONE',  ( 21.10320863425824811, 69.59972261355351009, -203.5481297357515302 ) ) ;
#163815 = CARTESIAN_POINT ( 'NONE',  ( 20.94999999999999574, 76.00000000001267608, -203.5231074845243597 ) ) ;
#163816 = ORIENTED_EDGE ( 'NONE', *, *, #38735, .F. ) ;
#163817 = ORIENTED_EDGE ( 'NONE', *, *, #135523, .F. ) ;
#163818 = AXIS2_PLACEMENT_3D ( 'NONE', #121605, #81143, #223224 ) ;
#163819 = ORIENTED_EDGE ( 'NONE', *, *, #215977, .F. ) ;
#163820 = DIRECTION ( 'NONE',  ( 0.000000000000000000, -6.982962677686266711E-15, 1.000000000000000000 ) ) ;
#163821 = CARTESIAN_POINT ( 'NONE',  ( -18.47130263965437180, -9.471155585952832467, -174.1834047654767801 ) ) ;
#163822 = CARTESIAN_POINT ( 'NONE',  ( 20.84999999999998721, 10.33248238083634440, -139.5948465439131780 ) ) ;
#163823 = EDGE_LOOP ( 'NONE', ( #182726, #164286, #119570, #225115 ) ) ;
#163824 = ADVANCED_FACE ( 'NONE', ( #35682 ), #173927, .T. ) ;
#163825 = CARTESIAN_POINT ( 'NONE',  ( 18.54999999999999716, 67.25000000001203659, -123.8731074845243683 ) ) ;
#163826 = CARTESIAN_POINT ( 'NONE',  ( 18.49999999999999289, 10.25000000263022493, -192.1871719496316473 ) ) ;
#163827 = DIRECTION ( 'NONE',  ( 0.000000000000000000, 0.2128009952263403282, -0.9770955615653358350 ) ) ;
#163828 = VECTOR ( 'NONE', #98798, 1000.000000000000114 ) ;
#163830 = ORIENTED_EDGE ( 'NONE', *, *, #222391, .F. ) ;
#163829 = VECTOR ( 'NONE', #109661, 1000.000000000000114 ) ;
#163831 = AXIS2_PLACEMENT_3D ( 'NONE', #92211, #12716, #70124 ) ;
#163832 = EDGE_CURVE ( 'NONE', #212622, #28415, #133421, .T. ) ;
#163834 = ORIENTED_EDGE ( 'NONE', *, *, #64624, .F. ) ;
#163833 = CARTESIAN_POINT ( 'NONE',  ( 20.94999999999999929, 0.000000000000000000, -33.50000000000000000 ) ) ;
#163835 = CARTESIAN_POINT ( 'NONE',  ( 21.07928932188134397, 6.328516656404459262, -33.40110485434561127 ) ) ;
#163836 = CARTESIAN_POINT ( 'NONE',  ( 18.43579564894478295, 78.24390728993300570, -231.6169759425274322 ) ) ;
#163837 = DIRECTION ( 'NONE',  ( 0.000000000000000000, -6.982962677686266711E-15, 1.000000000000000000 ) ) ;
#163838 = FACE_OUTER_BOUND ( 'NONE', #125225, .T. ) ;
#163839 = DIRECTION ( 'NONE',  ( 1.000000000000000000, 0.000000000000000000, 0.000000000000000000 ) ) ;
#163840 = CARTESIAN_POINT ( 'NONE',  ( -20.94999999999999929, 77.83534155023627932, -91.46795619196132066 ) ) ;
#163841 = ORIENTED_EDGE ( 'NONE', *, *, #198714, .T. ) ;
#163842 = CARTESIAN_POINT ( 'NONE',  ( 20.95512820512820440, 61.84489010471549619, -221.8053782964821039 ) ) ;
#163843 = FACE_OUTER_BOUND ( 'NONE', #227535, .T. ) ;
#163844 = FACE_OUTER_BOUND ( 'NONE', #174001, .T. ) ;
#163845 = CIRCLE ( 'NONE', #180411, 0.09999999999999939493 ) ;
#163846 = DIRECTION ( 'NONE',  ( 1.000000000000000000, 0.000000000000000000, 0.000000000000000000 ) ) ;
#163848 = CARTESIAN_POINT ( 'NONE',  ( -21.55000000000000071, 68.85000000001200249, -115.2731074845243455 ) ) ;
#163847 = AXIS2_PLACEMENT_3D ( 'NONE', #188613, #129917, #131206 ) ;
#163849 = EDGE_CURVE ( 'NONE', #21530, #101771, #19955, .T. ) ;
#163851 = ORIENTED_EDGE ( 'NONE', *, *, #230407, .F. ) ;
#163850 = AXIS2_PLACEMENT_3D ( 'NONE', #59573, #218668, #38773 ) ;
#163852 = VERTEX_POINT ( 'NONE', #74817 ) ;
#163853 = DIRECTION ( 'NONE',  ( 0.000000000000000000, -0.03181660087583042251, 0.9994937237965568766 ) ) ;
#163855 = DIRECTION ( 'NONE',  ( 0.7071067811865463515, 0.7071067811865487940, 4.937700262164540154E-15 ) ) ;
#163854 = AXIS2_PLACEMENT_3D ( 'NONE', #132892, #96296, #234541 ) ;
#163856 = CARTESIAN_POINT ( 'NONE',  ( 22.49436431346199683, 11.64995094765345840, 0.06690352972225574457 ) ) ;
#163857 = FACE_BOUND ( 'NONE', #29406, .T. ) ;
#163858 = EDGE_CURVE ( 'NONE', #243059, #21979, #77326, .T. ) ;
#163859 = ORIENTED_EDGE ( 'NONE', *, *, #153470, .T. ) ;
#163860 = CARTESIAN_POINT ( 'NONE',  ( -23.15000000000000213, 11.36448785225375602, -246.7787679937655980 ) ) ;
#163861 = CARTESIAN_POINT ( 'NONE',  ( -23.15000000000000213, 2.000000000011154189, -113.7246219227621395 ) ) ;
#163862 = EDGE_CURVE ( 'NONE', #107596, #77200, #156911, .T. ) ;
#163863 = CIRCLE ( 'NONE', #209655, 0.09999999999999939493 ) ;
#163865 = EDGE_CURVE ( 'NONE', #67070, #235804, #57763, .T. ) ;
#163864 = CARTESIAN_POINT ( 'NONE',  ( 23.15000000000000213, 85.50000000001261924, -193.6291383618718385 ) ) ;
#163866 = AXIS2_PLACEMENT_3D ( 'NONE', #168759, #248241, #107440 ) ;
#163867 = CARTESIAN_POINT ( 'NONE',  ( 23.24999999999997513, 11.75000000001116263, -93.48519422934610645 ) ) ;
#163868 = ORIENTED_EDGE ( 'NONE', *, *, #46105, .F. ) ;
#163869 = CARTESIAN_POINT ( 'NONE',  ( -20.94999999999999929, 18.24178995542692050, -237.7003448530951459 ) ) ;
#163870 = ADVANCED_FACE ( 'NONE', ( #235138 ), #34393, .F. ) ;
#163871 = VECTOR ( 'NONE', #149360, 1000.000000000000000 ) ;
#163872 = ORIENTED_EDGE ( 'NONE', *, *, #198879, .T. ) ;
#163873 = DIRECTION ( 'NONE',  ( 0.000000000000000000, 1.000000000000000000, -6.308085367188393199E-16 ) ) ;
#163874 = DIRECTION ( 'NONE',  ( 2.952720810173289112E-16, 1.000000000000000000, 6.938893903907229955E-15 ) ) ;
#163875 = CARTESIAN_POINT ( 'NONE',  ( -21.05000000000000071, 10.23276890377598036, -228.1195043774102658 ) ) ;
#163876 = LINE ( 'NONE', #30479, #3330 ) ;
#163878 = AXIS2_PLACEMENT_3D ( 'NONE', #25009, #246589, #168400 ) ;
#163877 = DIRECTION ( 'NONE',  ( 1.000000000000000000, 0.000000000000000000, 0.000000000000000000 ) ) ;
#163879 = CARTESIAN_POINT ( 'NONE',  ( -20.65000000000000568, 68.75000000001189449, -93.77310748452435973 ) ) ;
#163881 = LINE ( 'NONE', #162599, #207929 ) ;
#163880 = CIRCLE ( 'NONE', #9743, 4.049999999999998934 ) ;
#163882 = CIRCLE ( 'NONE', #180627, 0.09999999999999971412 ) ;
#163883 = FACE_OUTER_BOUND ( 'NONE', #71711, .T. ) ;
#163885 = CARTESIAN_POINT ( 'NONE',  ( -22.39999999999999858, 7.790779598384559357, -67.00000000000004263 ) ) ;
#163884 = TOROIDAL_SURFACE ( 'NONE', #47328, 0.2000000000000000111, 0.1000000000000000056 ) ;
#163886 = DIRECTION ( 'NONE',  ( 0.000000000000000000, 1.000000000000000000, 0.000000000000000000 ) ) ;
#163887 = DIRECTION ( 'NONE',  ( 0.000000000000000000, -0.2818822000686317941, 0.9594490217226071538 ) ) ;
#163888 = FACE_OUTER_BOUND ( 'NONE', #208888, .T. ) ;
#163889 = DIRECTION ( 'NONE',  ( -1.000000000000000000, 0.000000000000000000, 0.000000000000000000 ) ) ;
#163890 = DIRECTION ( 'NONE',  ( 1.000000000000000000, 0.000000000000000000, 0.000000000000000000 ) ) ;
#163891 = EDGE_LOOP ( 'NONE', ( #139275, #55041, #89305, #132690 ) ) ;
#163892 = CARTESIAN_POINT ( 'NONE',  ( 23.14999999999999503, 64.35000000001178933, -81.67310748452439384 ) ) ;
#163893 = DIRECTION ( 'NONE',  ( 1.186688945009009831E-16, -1.000000000000000000, 0.000000000000000000 ) ) ;
#163894 = EDGE_CURVE ( 'NONE', #220397, #147164, #241743, .T. ) ;
#163895 = ADVANCED_FACE ( 'NONE', ( #233854 ), #175091, .F. ) ;
#163896 = ORIENTED_EDGE ( 'NONE', *, *, #134287, .F. ) ;
#163897 = CARTESIAN_POINT ( 'NONE',  ( -21.14999999999999858, 11.75000000001115552, -73.78386566297820082 ) ) ;
#163898 = DIRECTION ( 'NONE',  ( 1.000000000000000000, -0.000000000000000000, -0.000000000000000000 ) ) ;
#163899 = ORIENTED_EDGE ( 'NONE', *, *, #144300, .T. ) ;
#163900 = CARTESIAN_POINT ( 'NONE',  ( 20.87155475150661132, 64.25000000001146816, -42.92752095536695833 ) ) ;
#163901 = CARTESIAN_POINT ( 'NONE',  ( 22.49544290803790147, 31.79553970091822990, -238.8548453295647391 ) ) ;
#163902 = VECTOR ( 'NONE', #67881, 1000.000000000000000 ) ;
#163903 = EDGE_CURVE ( 'NONE', #77606, #156170, #129322, .T. ) ;
#163905 = EDGE_LOOP ( 'NONE', ( #234555, #162398, #133436, #240028 ) ) ;
#163904 = AXIS2_PLACEMENT_3D ( 'NONE', #220660, #204924, #100668 ) ;
#163907 = FACE_OUTER_BOUND ( 'NONE', #53372, .T. ) ;
#163906 = CIRCLE ( 'NONE', #51441, 0.09999999999999528710 ) ;
#163908 = CIRCLE ( 'NONE', #168055, 0.1000000000000028644 ) ;
#163909 = VERTEX_POINT ( 'NONE', #104578 ) ;
#163910 = CARTESIAN_POINT ( 'NONE',  ( -21.65000000000000213, 9.775875410973588586, -211.8174516384118817 ) ) ;
#163911 = DIRECTION ( 'NONE',  ( -0.000000000000000000, -0.000000000000000000, -1.000000000000000000 ) ) ;
#163912 = FACE_OUTER_BOUND ( 'NONE', #237957, .T. ) ;
#163913 = CIRCLE ( 'NONE', #130589, 0.1000000000000028644 ) ;
#163914 = CARTESIAN_POINT ( 'NONE',  ( -18.59999999999999787, 7.128833340093095217, -233.7327013124392749 ) ) ;
#163915 = DIRECTION ( 'NONE',  ( 1.000000000000000000, 7.492892343619937423E-30, -1.073024830501117725E-15 ) ) ;
#163916 = CARTESIAN_POINT ( 'NONE',  ( -16.94445028196807002, 9.992063609708893068, -87.89266982158160602 ) ) ;
#163917 = AXIS2_PLACEMENT_3D ( 'NONE', #257266, #40875, #82504 ) ;
#163918 = FACE_OUTER_BOUND ( 'NONE', #174954, .T. ) ;
#163919 = CARTESIAN_POINT ( 'NONE',  ( -21.05000000000000071, 76.00000000001213607, -136.5231074845242745 ) ) ;
#163920 = CIRCLE ( 'NONE', #255454, 0.1000000000000028644 ) ;
#163922 = ORIENTED_EDGE ( 'NONE', *, *, #184979, .F. ) ;
#163921 = CARTESIAN_POINT ( 'NONE',  ( -18.46946985241261174, -9.509317228700407298, -40.48666256549965681 ) ) ;
#163923 = ORIENTED_EDGE ( 'NONE', *, *, #122018, .F. ) ;
#163925 = FACE_OUTER_BOUND ( 'NONE', #225334, .T. ) ;
#163924 = CARTESIAN_POINT ( 'NONE',  ( -20.54999999999999716, 73.50000000001254818, -183.2477294072864709 ) ) ;
#163926 = AXIS2_PLACEMENT_3D ( 'NONE', #78428, #32937, #73334 ) ;
#163928 = ORIENTED_EDGE ( 'NONE', *, *, #232307, .F. ) ;
#163927 = DIRECTION ( 'NONE',  ( -0.000000000000000000, -0.000000000000000000, -1.000000000000000000 ) ) ;
#163929 = EDGE_CURVE ( 'NONE', #192537, #162084, #21015, .T. ) ;
#163930 = ORIENTED_EDGE ( 'NONE', *, *, #126187, .T. ) ;
#163931 = CARTESIAN_POINT ( 'NONE',  ( 18.49999999999999289, 6.450000000011156587, -177.5170271704400022 ) ) ;
#163932 = AXIS2_PLACEMENT_3D ( 'NONE', #210475, #70986, #94355 ) ;
#163933 = FACE_OUTER_BOUND ( 'NONE', #228253, .T. ) ;
#163934 = CARTESIAN_POINT ( 'NONE',  ( -21.14999999999994174, 76.00000000001119815, -3.123107484524795474 ) ) ;
#163935 = EDGE_CURVE ( 'NONE', #102830, #64347, #125228, .T. ) ;
#163936 = LINE ( 'NONE', #160104, #39791 ) ;
#163937 = CARTESIAN_POINT ( 'NONE',  ( 21.05000000000000071, 36.65892442174935439, -249.5511627012433848 ) ) ;
#163938 = EDGE_CURVE ( 'NONE', #90057, #178217, #191897, .T. ) ;
#163939 = DIRECTION ( 'NONE',  ( -1.000000000000000000, 0.000000000000000000, 0.000000000000000000 ) ) ;
#163940 = AXIS2_PLACEMENT_3D ( 'NONE', #151194, #31281, #173366 ) ;
#163941 = ORIENTED_EDGE ( 'NONE', *, *, #247830, .F. ) ;
#163942 = ORIENTED_EDGE ( 'NONE', *, *, #9594, .T. ) ;
#163943 = EDGE_CURVE ( 'NONE', #173457, #145606, #125418, .T. ) ;
#163944 = CARTESIAN_POINT ( 'NONE',  ( -18.59999999999999787, 67.75954444190071513, -227.8703747234148693 ) ) ;
#163945 = ORIENTED_EDGE ( 'NONE', *, *, #233241, .F. ) ;
#163946 = CARTESIAN_POINT ( 'NONE',  ( 21.14999999999999858, 1.115486826172573664E-11, -26.95934304829875927 ) ) ;
#163947 = ORIENTED_EDGE ( 'NONE', *, *, #198490, .F. ) ;
#163948 = CIRCLE ( 'NONE', #51481, 0.09999999999999693856 ) ;
#163949 = CIRCLE ( 'NONE', #134871, 0.09999999999999939493 ) ;
#163950 = EDGE_CURVE ( 'NONE', #67839, #232210, #203715, .T. ) ;
#163951 = AXIS2_PLACEMENT_3D ( 'NONE', #105757, #86193, #66668 ) ;
#163953 = EDGE_CURVE ( 'NONE', #180993, #174426, #241912, .T. ) ;
#163952 = ADVANCED_FACE ( 'NONE', ( #202427 ), #96164, .T. ) ;
#163954 = DIRECTION ( 'NONE',  ( -0.000000000000000000, 0.000000000000000000, 1.000000000000000000 ) ) ;
#163955 = CARTESIAN_POINT ( 'NONE',  ( -18.59999999999999787, 74.26374286841466699, -124.9544551555068068 ) ) ;
#163956 = DIRECTION ( 'NONE',  ( -0.4999999999999799050, 0.000000000000000000, -0.8660254037844502539 ) ) ;
#163957 = ORIENTED_EDGE ( 'NONE', *, *, #90468, .F. ) ;
#163958 = APPLICATION_CONTEXT ( 'automotive_design' ) ;
#163959 = SPHERICAL_SURFACE ( 'NONE', #121357, 0.1000000000000000056 ) ;
#163960 = ORIENTED_EDGE ( 'NONE', *, *, #8759, .F. ) ;
#163961 = DIRECTION ( 'NONE',  ( 0.000000000000000000, 0.000000000000000000, -1.000000000000000000 ) ) ;
#163962 = DIRECTION ( 'NONE',  ( 1.000000000000000000, 0.000000000000000000, 0.000000000000000000 ) ) ;
#163963 = FACE_OUTER_BOUND ( 'NONE', #78693, .T. ) ;
#163964 = DIRECTION ( 'NONE',  ( 0.000000000000000000, -1.000000000000000000, -6.982962677686265922E-15 ) ) ;
#163965 = ORIENTED_EDGE ( 'NONE', *, *, #17806, .T. ) ;
#163966 = DIRECTION ( 'NONE',  ( 0.000000000000000000, 0.1335171055202901413, 0.9910465087640860649 ) ) ;
#163967 = CIRCLE ( 'NONE', #159328, 0.09999999999999939493 ) ;
#163968 = ORIENTED_EDGE ( 'NONE', *, *, #195071, .T. ) ;
#163971 = ORIENTED_EDGE ( 'NONE', *, *, #195472, .F. ) ;
#163970 = CARTESIAN_POINT ( 'NONE',  ( 21.00000000000000000, 9.749999999999998224, -12.35000000000000320 ) ) ;
#163969 = DIRECTION ( 'NONE',  ( 0.000000000000000000, 0.9446535261619708468, -0.3280696808755038663 ) ) ;
#163972 = AXIS2_PLACEMENT_3D ( 'NONE', #62924, #43370, #120369 ) ;
#163974 = EDGE_CURVE ( 'NONE', #94251, #18434, #129509, .T. ) ;
#163973 = AXIS2_PLACEMENT_3D ( 'NONE', #158542, #61991, #221041 ) ;
#163975 = DIRECTION ( 'NONE',  ( 1.000000000000000000, 0.000000000000000000, 0.000000000000000000 ) ) ;
#163976 = VECTOR ( 'NONE', #57855, 1000.000000000000000 ) ;
#163977 = ADVANCED_FACE ( 'NONE', ( #105866 ), #219402, .F. ) ;
#163978 = VERTEX_POINT ( 'NONE', #62916 ) ;
#163979 = DIRECTION ( 'NONE',  ( 0.000000000000000000, 1.000000000000000000, 0.000000000000000000 ) ) ;
#163980 = VERTEX_POINT ( 'NONE', #142446 ) ;
#163981 = CARTESIAN_POINT ( 'NONE',  ( 21.00023020733504708, 76.00000000001219291, -142.9139767297926653 ) ) ;
#163982 = EDGE_CURVE ( 'NONE', #38302, #133775, #216959, .T. ) ;
#163983 = CARTESIAN_POINT ( 'NONE',  ( -16.93826681692523550, 10.01142872029886810, -54.44545846735943684 ) ) ;
#163984 = CARTESIAN_POINT ( 'NONE',  ( 22.39999999999999503, 31.94635157770351341, -238.7871412784868710 ) ) ;
#163985 = CARTESIAN_POINT ( 'NONE',  ( -16.87383368123029825, 9.949999999999983302, -12.65000000000000213 ) ) ;
#163986 = EDGE_CURVE ( 'NONE', #4154, #256392, #66959, .T. ) ;
#163987 = ORIENTED_EDGE ( 'NONE', *, *, #138846, .F. ) ;
#163988 = ADVANCED_FACE ( 'NONE', ( #120361 ), #137857, .F. ) ;
#163989 = DIRECTION ( 'NONE',  ( 1.000000000000000000, 0.000000000000000000, 0.000000000000000000 ) ) ;
#163990 = CARTESIAN_POINT ( 'NONE',  ( -18.31572283045123939, -9.548437830874796362, -140.8506256510583796 ) ) ;
#163991 = B_SPLINE_CURVE_WITH_KNOTS ( 'NONE', 3,
 ( #123590, #23231, #238397, #4892, #79304, #223954 ),
 .UNSPECIFIED., .F., .F.,
 ( 4, 2, 4 ),
 ( 0.000000000000000000, 0.0001496588209255839358, 0.0002993176418511678716 ),
 .UNSPECIFIED. ) ;
#163992 = VERTEX_POINT ( 'NONE', #180299 ) ;
#163993 = VERTEX_POINT ( 'NONE', #181598 ) ;
#163994 = LINE ( 'NONE', #143116, #68923 ) ;
#163995 = CIRCLE ( 'NONE', #109999, 0.5000000000000004441 ) ;
#163996 = CARTESIAN_POINT ( 'NONE',  ( 21.05000000000000071, -8.663551401858002876, -143.5241011180673070 ) ) ;
#163997 = CARTESIAN_POINT ( 'NONE',  ( 20.94999999999999929, 36.18002604163306302, -236.0784499204090991 ) ) ;
#163999 = EDGE_LOOP ( 'NONE', ( #187174, #238644, #27596, #252400, #54642, #63648, #195222, #142744, #8869, #164967, #251194, #168602 ) ) ;
#163998 = FACE_OUTER_BOUND ( 'NONE', #222924, .T. ) ;
#164000 = ADVANCED_FACE ( 'NONE', ( #103306 ), #79416, .F. ) ;
#164001 = CARTESIAN_POINT ( 'NONE',  ( -20.94999999999999929, 11.60000000001115161, -174.4282032302755283 ) ) ;
#164002 = CARTESIAN_POINT ( 'NONE',  ( -15.73854595235691534, 62.65055472571233253, -217.0190438104121995 ) ) ;
#164003 = CARTESIAN_POINT ( 'NONE',  ( -20.00857864376270001, 66.85000000001228670, -157.6731074845244223 ) ) ;
#164004 = ORIENTED_EDGE ( 'NONE', *, *, #256442, .T. ) ;
#164005 = ADVANCED_FACE ( 'NONE', ( #242829 ), #139975, .T. ) ;
#164006 = CYLINDRICAL_SURFACE ( 'NONE', #226537, 0.1000000000000000056 ) ;
#164007 = CARTESIAN_POINT ( 'NONE',  ( -23.25000000000000000, 1.627786319807483340, -244.0021210468063089 ) ) ;
#164008 = ORIENTED_EDGE ( 'NONE', *, *, #232101, .T. ) ;
#164010 = CARTESIAN_POINT ( 'NONE',  ( -16.94445028196808778, 9.992063609708889516, -146.6073301784184935 ) ) ;
#164009 = CIRCLE ( 'NONE', #5570, 0.09999999999999939493 ) ;
#164011 = CIRCLE ( 'NONE', #193062, 0.5000000000000007772 ) ;
#164012 = ORIENTED_EDGE ( 'NONE', *, *, #171923, .F. ) ;
#164013 = AXIS2_PLACEMENT_3D ( 'NONE', #173759, #17217, #18486 ) ;
#164014 = CARTESIAN_POINT ( 'NONE',  ( 18.39999999999999503, 5.650000000011139001, -79.65000000000004832 ) ) ;
#164016 = ORIENTED_EDGE ( 'NONE', *, *, #47769, .F. ) ;
#164015 = DIRECTION ( 'NONE',  ( -0.7071067811865475727, 0.7071067811865475727, 4.937700262164531476E-15 ) ) ;
#164017 = EDGE_CURVE ( 'NONE', #170250, #241192, #233251, .T. ) ;
#164020 = VERTEX_POINT ( 'NONE', #246679 ) ;
#164019 = ORIENTED_EDGE ( 'NONE', *, *, #208584, .T. ) ;
#164018 = DIRECTION ( 'NONE',  ( 1.000000000000000000, 0.000000000000000000, 0.000000000000000000 ) ) ;
#164021 = DIRECTION ( 'NONE',  ( 0.000000000000000000, 0.2617529984164357892, 0.9651348961777339586 ) ) ;
#164022 = CARTESIAN_POINT ( 'NONE',  ( -20.94999999999999929, 87.75000000001266187, -200.4231074845242802 ) ) ;
#164023 = DIRECTION ( 'NONE',  ( 0.000000000000000000, 0.9651348961777379554, -0.2617529984164210233 ) ) ;
#164025 = DIRECTION ( 'NONE',  ( 1.000000000000000000, 0.000000000000000000, 0.000000000000000000 ) ) ;
#164024 = CYLINDRICAL_SURFACE ( 'NONE', #98239, 0.09999999999998898659 ) ;
#164026 = FACE_OUTER_BOUND ( 'NONE', #233031, .T. ) ;
#164027 = CARTESIAN_POINT ( 'NONE',  ( -18.59999999999999787, -9.499999999988842703, -146.1500000000000341 ) ) ;
#164028 = AXIS2_PLACEMENT_3D ( 'NONE', #179561, #180832, #101231 ) ;
#164029 = DIRECTION ( 'NONE',  ( 0.000000000000000000, 0.9126074666063780372, 0.4088369013363259419 ) ) ;
#164030 = DIRECTION ( 'NONE',  ( -0.000000000000000000, 6.982962677686266711E-15, -1.000000000000000000 ) ) ;
#164031 = AXIS2_PLACEMENT_3D ( 'NONE', #131228, #15146, #109089 ) ;
#164032 = ORIENTED_EDGE ( 'NONE', *, *, #32555, .F. ) ;
#164033 = ORIENTED_EDGE ( 'NONE', *, *, #97102, .T. ) ;
#164034 = AXIS2_PLACEMENT_3D ( 'NONE', #118472, #153784, #12964 ) ;
#164035 = DIRECTION ( 'NONE',  ( 1.000000000000000000, 3.265361837132813093E-16, -0.000000000000000000 ) ) ;
#164037 = ORIENTED_EDGE ( 'NONE', *, *, #69252, .T. ) ;
#164036 = CARTESIAN_POINT ( 'NONE',  ( -18.50000000000000000, 59.50933445848280456, -243.9217804674669310 ) ) ;
#164038 = EDGE_LOOP ( 'NONE', ( #78384, #206317, #70104, #69106 ) ) ;
#164039 = DIRECTION ( 'NONE',  ( -1.000000000000000000, -0.000000000000000000, -0.000000000000000000 ) ) ;
#164040 = ORIENTED_EDGE ( 'NONE', *, *, #39894, .F. ) ;
#164041 = DIRECTION ( 'NONE',  ( 0.000000000000000000, -0.2965989261549489275, -0.9550021345545417484 ) ) ;
#164042 = AXIS2_PLACEMENT_3D ( 'NONE', #162194, #100859, #141323 ) ;
#164043 = VECTOR ( 'NONE', #122333, 1000.000000000000000 ) ;
#164044 = ORIENTED_EDGE ( 'NONE', *, *, #226605, .T. ) ;
#164045 = AXIS2_PLACEMENT_3D ( 'NONE', #117410, #237361, #75728 ) ;
#164046 = DIRECTION ( 'NONE',  ( 0.000000000000000000, 1.776356839400308446E-15, -1.000000000000000000 ) ) ;
#164047 = CARTESIAN_POINT ( 'NONE',  ( -20.94999999999999929, 14.05000000000000071, -27.98630492923908619 ) ) ;
#164048 = TOROIDAL_SURFACE ( 'NONE', #234972, 0.2000000000000000111, 0.1000000000000000056 ) ;
#164050 = ORIENTED_EDGE ( 'NONE', *, *, #170791, .F. ) ;
#164049 = VERTEX_POINT ( 'NONE', #114561 ) ;
#164051 = ORIENTED_EDGE ( 'NONE', *, *, #197105, .T. ) ;
#164052 = FACE_OUTER_BOUND ( 'NONE', #9399, .T. ) ;
#164053 = ORIENTED_EDGE ( 'NONE', *, *, #239702, .T. ) ;
#164054 = ORIENTED_EDGE ( 'NONE', *, *, #225314, .T. ) ;
#164056 = CARTESIAN_POINT ( 'NONE',  ( 20.94999999999999574, 4.184122562697137226, -245.3714803909117279 ) ) ;
#164055 = CIRCLE ( 'NONE', #255581, 0.2000000000000005107 ) ;
#164057 = CARTESIAN_POINT ( 'NONE',  ( 21.00000000000000000, 66.25000000001186606, -90.67310748452437963 ) ) ;
#164059 = ORIENTED_EDGE ( 'NONE', *, *, #53258, .F. ) ;
#164058 = CARTESIAN_POINT ( 'NONE',  ( 18.46163235739467368, -9.480150806907140293, -107.1576105398775240 ) ) ;
#164060 = DIRECTION ( 'NONE',  ( 0.000000000000000000, -6.982962677686266711E-15, 1.000000000000000000 ) ) ;
#164061 = CARTESIAN_POINT ( 'NONE',  ( 23.14999999999999858, 1.115600667400684642E-11, -167.5000000000000284 ) ) ;
#164063 = ORIENTED_EDGE ( 'NONE', *, *, #6017, .T. ) ;
#164062 = DIRECTION ( 'NONE',  ( 0.000000000000000000, 0.000000000000000000, -1.000000000000000000 ) ) ;
#164064 = CARTESIAN_POINT ( 'NONE',  ( 23.14999999999999503, 69.35000000001200249, -115.1731074845243512 ) ) ;
#164065 = ORIENTED_EDGE ( 'NONE', *, *, #177727, .T. ) ;
#164066 = CIRCLE ( 'NONE', #189007, 0.1000000000000028644 ) ;
#164067 = CARTESIAN_POINT ( 'NONE',  ( 23.04999999999999716, 62.02748777246247869, -221.3368380802343722 ) ) ;
#164068 = TOROIDAL_SURFACE ( 'NONE', #72491, 4.099999999999999645, 0.1000000000000000056 ) ;
#164069 = ORIENTED_EDGE ( 'NONE', *, *, #55510, .T. ) ;
#164070 = AXIS2_PLACEMENT_3D ( 'NONE', #183436, #62203, #81720 ) ;
#164071 = CARTESIAN_POINT ( 'NONE',  ( -21.05000000000000071, 18.65704504850842227, -226.5784250989226223 ) ) ;
#164072 = DIRECTION ( 'NONE',  ( 1.000000000000000000, 0.000000000000000000, 0.000000000000000000 ) ) ;
#164073 = EDGE_CURVE ( 'NONE', #151096, #143707, #42039, .T. ) ;
#164074 = ORIENTED_EDGE ( 'NONE', *, *, #56746, .F. ) ;
#164075 = CARTESIAN_POINT ( 'NONE',  ( 18.59999999999999076, 68.87972903831452243, -132.8635444426850825 ) ) ;
#164076 = PLANE ( 'NONE',  #5947 ) ;
#164077 = ORIENTED_EDGE ( 'NONE', *, *, #200362, .F. ) ;
#164078 = ORIENTED_EDGE ( 'NONE', *, *, #125000, .T. ) ;
#164079 = DIRECTION ( 'NONE',  ( -0.7070776581708965169, 0.7071359030027827286, 4.937903618720407826E-15 ) ) ;
#164080 = DIRECTION ( 'NONE',  ( 0.5932847527679310229, 0.8049926720990042694, 6.257843056355992909E-15 ) ) ;
#164081 = ORIENTED_EDGE ( 'NONE', *, *, #45412, .T. ) ;
#164082 = VERTEX_POINT ( 'NONE', #154994 ) ;
#164083 = CARTESIAN_POINT ( 'NONE',  ( 22.88900146558018989, 41.54206602352874000, -237.8261728628838512 ) ) ;
#164084 = FACE_OUTER_BOUND ( 'NONE', #249262, .T. ) ;
#164085 = ADVANCED_FACE ( 'NONE', ( #112007 ), #126741, .F. ) ;
#164086 = ADVANCED_FACE ( 'NONE', ( #12922 ), #234495, .F. ) ;
#164087 = CYLINDRICAL_SURFACE ( 'NONE', #82468, 0.4999999999999944489 ) ;
#164088 = DIRECTION ( 'NONE',  ( -1.000000000000000000, 0.000000000000000000, 0.000000000000000000 ) ) ;
#164089 = CIRCLE ( 'NONE', #80670, 0.1000000000000035028 ) ;
#164090 = CIRCLE ( 'NONE', #5833, 0.09999999999999993616 ) ;
#164091 = ORIENTED_EDGE ( 'NONE', *, *, #172204, .F. ) ;
#164092 = CARTESIAN_POINT ( 'NONE',  ( 18.49999999999999289, 54.30302133219453964, -244.5233354669909431 ) ) ;
#164093 = VECTOR ( 'NONE', #26005, 1000.000000000000000 ) ;
#164095 = ORIENTED_EDGE ( 'NONE', *, *, #106748, .T. ) ;
#164094 = ORIENTED_EDGE ( 'NONE', *, *, #218440, .F. ) ;
#164096 = EDGE_LOOP ( 'NONE', ( #129420, #209975, #186691, #220384 ) ) ;
#164097 = ORIENTED_EDGE ( 'NONE', *, *, #171447, .F. ) ;
#164098 = EDGE_CURVE ( 'NONE', #146114, #71159, #54575, .T. ) ;
#164099 = CARTESIAN_POINT ( 'NONE',  ( 21.30740335185486245, 6.556657922039159203, -33.40106547422415417 ) ) ;
#164100 = CARTESIAN_POINT ( 'NONE',  ( 18.49999999999999645, 77.86671491006887891, -57.77043223824230722 ) ) ;
#164101 = AXIS2_PLACEMENT_3D ( 'NONE', #107952, #64965, #66264 ) ;
#164102 = DIRECTION ( 'NONE',  ( 1.000000000000000000, 0.000000000000000000, 0.000000000000000000 ) ) ;
#164104 = EDGE_CURVE ( 'NONE', #256568, #7935, #206283, .T. ) ;
#164103 = CARTESIAN_POINT ( 'NONE',  ( -18.50000000000000000, 13.96869538424787649, -210.3925794786331949 ) ) ;
#164105 = CYLINDRICAL_SURFACE ( 'NONE', #234191, 0.09999999999999691080 ) ;
#164107 = CARTESIAN_POINT ( 'NONE',  ( 21.05000000000097771, 58.96901243545040927, -225.7107919458293850 ) ) ;
#164106 = CARTESIAN_POINT ( 'NONE',  ( -18.59999999999999787, 7.783179459866045313, -245.3643104511423303 ) ) ;
#164109 = VERTEX_POINT ( 'NONE', #214938 ) ;
#164108 = CARTESIAN_POINT ( 'NONE',  ( 18.52326479938732362, 77.30136670619768324, -241.9095796805263205 ) ) ;
#164110 = PLANE ( 'NONE',  #95595 ) ;
#164111 = ORIENTED_EDGE ( 'NONE', *, *, #216170, .T. ) ;
#164112 = AXIS2_PLACEMENT_3D ( 'NONE', #205529, #66030, #145561 ) ;
#164113 = ADVANCED_FACE ( 'NONE', ( #252770 ), #50365, .F. ) ;
#164114 = FACE_OUTER_BOUND ( 'NONE', #62145, .T. ) ;
#164115 = EDGE_LOOP ( 'NONE', ( #196862, #75540, #62959, #216469 ) ) ;
#164116 = VERTEX_POINT ( 'NONE', #213660 ) ;
#164117 = CARTESIAN_POINT ( 'NONE',  ( -21.05000000000000071, 74.75000000001261924, -195.5231074845243597 ) ) ;
#164118 = CIRCLE ( 'NONE', #151664, 0.1000000000000033362 ) ;
#164119 = CYLINDRICAL_SURFACE ( 'NONE', #35239, 0.1000000000000024342 ) ;
#164120 = CARTESIAN_POINT ( 'NONE',  ( -16.82542659449985223, 66.06550010858410360, -48.76774308455063078 ) ) ;
#164121 = VECTOR ( 'NONE', #37522, 1000.000000000000227 ) ;
#164122 = CARTESIAN_POINT ( 'NONE',  ( 15.52844286134407525, 9.375669526436928081, -82.86779000938595630 ) ) ;
#164123 = EDGE_CURVE ( 'NONE', #242008, #158190, #74187, .T. ) ;
#164124 = AXIS2_PLACEMENT_3D ( 'NONE', #73988, #34854, #93507 ) ;
#164125 = DIRECTION ( 'NONE',  ( 1.000000000000000000, 0.000000000000000000, 0.000000000000000000 ) ) ;
#164126 = ORIENTED_EDGE ( 'NONE', *, *, #253362, .T. ) ;
#164128 = EDGE_LOOP ( 'NONE', ( #149111, #186462, #140306, #120431, #177799, #221453, #239054, #252351, #83093, #67654, #129890 ) ) ;
#164127 = EDGE_CURVE ( 'NONE', #110138, #125075, #92079, .T. ) ;
#164129 = CARTESIAN_POINT ( 'NONE',  ( -21.05000000000000071, 74.83729825007408465, -128.6231074845242972 ) ) ;
#164130 = VERTEX_POINT ( 'NONE', #136671 ) ;
#164131 = CARTESIAN_POINT ( 'NONE',  ( -23.15000000000000213, 1.115600667400684642E-11, -134.0000000000000284 ) ) ;
#164132 = DIRECTION ( 'NONE',  ( 2.940209281316621016E-16, 1.000000000000000000, 7.056502275159890832E-15 ) ) ;
#164133 = DIRECTION ( 'NONE',  ( -0.000000000000000000, 0.9908441862701591329, 0.1350103645451946055 ) ) ;
#164135 = AXIS2_PLACEMENT_3D ( 'NONE', #243686, #144571, #33340 ) ;
#164134 = CARTESIAN_POINT ( 'NONE',  ( 21.12642695952774119, -1.260108817593847519, -194.7493242710371248 ) ) ;
#164136 = CARTESIAN_POINT ( 'NONE',  ( -18.59999999999999787, 77.83585931145526615, -58.01866831572577610 ) ) ;
#164137 = DIRECTION ( 'NONE',  ( 0.000000000000000000, -1.776356839400188145E-15, 1.000000000000000000 ) ) ;
#164138 = CARTESIAN_POINT ( 'NONE',  ( 22.59999999999999432, 75.90000000001276703, -215.1726782920691505 ) ) ;
#164139 = CARTESIAN_POINT ( 'NONE',  ( 21.97500000000000497, 66.25000000001199396, -115.3731074845243683 ) ) ;
#164140 = LINE ( 'NONE', #3769, #141681 ) ;
#164141 = EDGE_CURVE ( 'NONE', #230224, #211628, #87785, .T. ) ;
#164142 = CARTESIAN_POINT ( 'NONE',  ( -21.05000000000000071, 6.412126976762841046, -199.7058512474018244 ) ) ;
#164143 = AXIS2_PLACEMENT_3D ( 'NONE', #150578, #245824, #108873 ) ;
#164144 = CARTESIAN_POINT ( 'NONE',  ( -18.52139480978223318, 85.48135884507880178, -95.99855091740519697 ) ) ;
#164145 = CARTESIAN_POINT ( 'NONE',  ( 18.50000000000000000, 77.35494420175977837, -241.6200040285045532 ) ) ;
#164146 = CIRCLE ( 'NONE', #51666, 0.09999999999999938105 ) ;
#164147 = VECTOR ( 'NONE', #35426, 1000.000000000000114 ) ;
#164148 = ORIENTED_EDGE ( 'NONE', *, *, #242689, .T. ) ;
#164149 = CIRCLE ( 'NONE', #205621, 11.90000000000000568 ) ;
#164150 = DIRECTION ( 'NONE',  ( 0.000000000000000000, 0.2128009952263603677, -0.9770955615653313941 ) ) ;
#164151 = ORIENTED_EDGE ( 'NONE', *, *, #30392, .F. ) ;
#164152 = CYLINDRICAL_SURFACE ( 'NONE', #6426, 2.000000000000001776 ) ;
#164153 = VERTEX_POINT ( 'NONE', #119705 ) ;
#164154 = DIRECTION ( 'NONE',  ( -1.000000000000000000, -3.265361837132813093E-16, 0.000000000000000000 ) ) ;
#164155 = FACE_OUTER_BOUND ( 'NONE', #108840, .T. ) ;
#164156 = DIRECTION ( 'NONE',  ( 0.000000000000000000, -0.2868887416115947775, 0.9579639084728169829 ) ) ;
#164157 = DIRECTION ( 'NONE',  ( -1.000000000000000000, 0.000000000000000000, 0.000000000000000000 ) ) ;
#164158 = AXIS2_PLACEMENT_3D ( 'NONE', #224247, #48182, #105556 ) ;
#164159 = CIRCLE ( 'NONE', #189100, 0.1000000000000028644 ) ;
#164161 = DIRECTION ( 'NONE',  ( -1.836970198721029934E-16, -1.000000000000000000, -6.982962677686266711E-15 ) ) ;
#164160 = CIRCLE ( 'NONE', #51687, 0.09999999999998898659 ) ;
#164162 = CARTESIAN_POINT ( 'NONE',  ( 22.50000000000000000, 75.90000000001245439, -181.6726782920691505 ) ) ;
#164163 = ADVANCED_FACE ( 'NONE', ( #140519 ), #80527, .F. ) ;
#164164 = EDGE_CURVE ( 'NONE', #135639, #148274, #246032, .T. ) ;
#164165 = EDGE_LOOP ( 'NONE', ( #25409, #112264, #156444, #239699 ) ) ;
#164166 = DIRECTION ( 'NONE',  ( -0.000000000000000000, -0.000000000000000000, -1.000000000000000000 ) ) ;
#164168 = ORIENTED_EDGE ( 'NONE', *, *, #184861, .F. ) ;
#164167 = CARTESIAN_POINT ( 'NONE',  ( 20.94999999999999929, 67.23127455305841238, -235.8551265064783991 ) ) ;
#164169 = CARTESIAN_POINT ( 'NONE',  ( -40.23850191057533010, 65.35000000001120668, -4.523107484524794053 ) ) ;
#164170 = LINE ( 'NONE', #243695, #107826 ) ;
#164171 = ADVANCED_FACE ( 'NONE', ( #175836 ), #2284, .T. ) ;
#164172 = EDGE_CURVE ( 'NONE', #120661, #256898, #121172, .T. ) ;
#164173 = ORIENTED_EDGE ( 'NONE', *, *, #65339, .F. ) ;
#164174 = DIRECTION ( 'NONE',  ( 0.000000000000000000, -0.2128009952263585913, 0.9770955615653319493 ) ) ;
#164175 = ITEM_DEFINED_TRANSFORMATION ( 'NONE', 'NONE', #111123,  #2425 ) ;
#164176 = CARTESIAN_POINT ( 'NONE',  ( 20.94999999999999929, 1.115600667400684642E-11, -167.5000000000000284 ) ) ;
#164177 = EDGE_CURVE ( 'NONE', #77989, #177651, #20611, .T. ) ;
#164178 = VERTEX_POINT ( 'NONE', #257863 ) ;
#164179 = DIRECTION ( 'NONE',  ( 0.000000000000000000, -1.000000000000000000, 0.000000000000000000 ) ) ;
#164180 = CARTESIAN_POINT ( 'NONE',  ( 18.49999999999999289, 10.49142135624846439, -91.85000000000003695 ) ) ;
#164181 = ADVANCED_FACE ( 'NONE', ( #220075 ), #16760, .F. ) ;
#164182 = EDGE_CURVE ( 'NONE', #235820, #63414, #41461, .T. ) ;
#164183 = VECTOR ( 'NONE', #28635, 1000.000000000000000 ) ;
#164184 = LINE ( 'NONE', #200733, #203666 ) ;
#164185 = VERTEX_POINT ( 'NONE', #139224 ) ;
#164186 = ADVANCED_FACE ( 'NONE', ( #179676 ), #187779, .F. ) ;
#164187 = VERTEX_POINT ( 'NONE', #983 ) ;
#164188 = DIRECTION ( 'NONE',  ( 0.000000000000000000, 0.000000000000000000, 1.000000000000000000 ) ) ;
#164189 = CARTESIAN_POINT ( 'NONE',  ( 18.39999999999999503, 64.52683809664910086, -56.87310748452440379 ) ) ;
#164190 = CARTESIAN_POINT ( 'NONE',  ( 20.85000000000000142, 64.35000000001249987, -176.8069731475025321 ) ) ;
#164191 = CARTESIAN_POINT ( 'NONE',  ( 18.49999999999999645, -1.637172712959225507, -112.0821533654720383 ) ) ;
#164192 = EDGE_CURVE ( 'NONE', #164153, #128716, #75368, .T. ) ;
#164193 = DIRECTION ( 'NONE',  ( 0.000000000000000000, -0.9126074666064055707, -0.4088369013362648241 ) ) ;
#164194 = CARTESIAN_POINT ( 'NONE',  ( -20.64999999999999858, 4.350000000011156054, -188.6499999999999488 ) ) ;
#164196 = CARTESIAN_POINT ( 'NONE',  ( 20.94999999999999574, 10.52493806863738079, -207.3780514093641330 ) ) ;
#164195 = CARTESIAN_POINT ( 'NONE',  ( 21.05000000000000071, -1.300607522999445820, -194.8777000085252666 ) ) ;
#164197 = CARTESIAN_POINT ( 'NONE',  ( 20.12500000000000355, 40.50633771312144660, -237.6829562735682657 ) ) ;
#164199 = EDGE_CURVE ( 'NONE', #121611, #2705, #175319, .T. ) ;
#164198 = DIRECTION ( 'NONE',  ( 1.000000000000000000, 0.000000000000000000, 0.000000000000000000 ) ) ;
#164200 = FACE_OUTER_BOUND ( 'NONE', #121535, .T. ) ;
#164203 = EDGE_CURVE ( 'NONE', #249539, #207750, #37950, .T. ) ;
#164202 = CARTESIAN_POINT ( 'NONE',  ( 20.94999999999999929, 70.60000000001198828, -112.9170766071767815 ) ) ;
#164201 = VECTOR ( 'NONE', #1357, 1000.000000000000000 ) ;
#164204 = EDGE_LOOP ( 'NONE', ( #96945, #26016, #178950, #68565 ) ) ;
#164205 = AXIS2_PLACEMENT_3D ( 'NONE', #105152, #85597, #253685 ) ;
#164206 = ORIENTED_EDGE ( 'NONE', *, *, #47757, .F. ) ;
#164207 = CARTESIAN_POINT ( 'NONE',  ( -20.64999999999999858, 84.73084112150691283, -59.92503276553993175 ) ) ;
#164208 = DIRECTION ( 'NONE',  ( -0.000000000000000000, 1.000000000000000000, 6.982962677686266711E-15 ) ) ;
#164210 = DIRECTION ( 'NONE',  ( 0.000000000000000000, -0.9126074666063545004, -0.4088369013363783999 ) ) ;
#164209 = AXIS2_PLACEMENT_3D ( 'NONE', #190419, #229533, #27517 ) ;
#164211 = CIRCLE ( 'NONE', #51730, 0.09999999999999986677 ) ;
#164212 = EDGE_CURVE ( 'NONE', #132946, #41194, #158842, .T. ) ;
#164213 = FACE_OUTER_BOUND ( 'NONE', #117120, .T. ) ;
#164214 = CARTESIAN_POINT ( 'NONE',  ( 23.24999999999999289, 71.23658437219593509, -236.9414014499068912 ) ) ;
#164215 = CARTESIAN_POINT ( 'NONE',  ( -21.14999999999999858, -0.09999999998884338825, -21.85042919245520210 ) ) ;
#164216 = ADVANCED_FACE ( 'NONE', ( #197929 ), #162851, .F. ) ;
#164217 = ADVANCED_FACE ( 'NONE', ( #221331 ), #3664, .T. ) ;
#164218 = ORIENTED_EDGE ( 'NONE', *, *, #257197, .T. ) ;
#164220 = AXIS2_PLACEMENT_3D ( 'NONE', #94002, #118734, #174894 ) ;
#164219 = DIRECTION ( 'NONE',  ( -0.000000000000000000, -0.4721928772777330696, -0.8814952561688438326 ) ) ;
#164221 = EDGE_LOOP ( 'NONE', ( #21820, #207813, #193031, #250521 ) ) ;
#164222 = CARTESIAN_POINT ( 'NONE',  ( -18.59999999999999787, -9.480686695267820596, -73.94111516875784673 ) ) ;
#164223 = AXIS2_PLACEMENT_3D ( 'NONE', #183400, #167707, #204228 ) ;
#164225 = CARTESIAN_POINT ( 'NONE',  ( 18.60000000000000142, 85.48068669529034480, -29.08199231576639576 ) ) ;
#164224 = AXIS2_PLACEMENT_3D ( 'NONE', #216565, #173651, #114902 ) ;
#164226 = CIRCLE ( 'NONE', #210017, 0.1000000000000028644 ) ;
#164227 = CIRCLE ( 'NONE', #214104, 11.70000000000000284 ) ;
#164228 = ORIENTED_EDGE ( 'NONE', *, *, #77146, .T. ) ;
#164229 = CARTESIAN_POINT ( 'NONE',  ( -21.45000000000000284, 52.80902093404626640, -233.8693558107618173 ) ) ;
#164230 = ORIENTED_EDGE ( 'NONE', *, *, #186124, .T. ) ;
#164231 = CARTESIAN_POINT ( 'NONE',  ( -20.94999999999999929, 76.00000000001244871, -170.0231074845243597 ) ) ;
#164232 = CARTESIAN_POINT ( 'NONE',  ( -18.40000000000000213, 11.47316190337362940, -46.10857864376269077 ) ) ;
#164233 = CARTESIAN_POINT ( 'NONE',  ( -18.34804628011471195, 64.52683809664921455, -60.27310748452440947 ) ) ;
#164234 = AXIS2_PLACEMENT_3D ( 'NONE', #240133, #138425, #78467 ) ;
#164236 = CARTESIAN_POINT ( 'NONE',  ( 18.43579564894478295, -9.519327535281362884, -140.9729766438603633 ) ) ;
#164235 = VECTOR ( 'NONE', #83992, 1000.000000000000000 ) ;
#164237 = DIRECTION ( 'NONE',  ( -0.000000000000000000, -0.1298341882519737922, -0.9915357197604890427 ) ) ;
#164239 = CIRCLE ( 'NONE', #1884, 0.09999999999999939493 ) ;
#164238 = DIRECTION ( 'NONE',  ( 1.000000000000000000, 0.000000000000000000, 0.000000000000000000 ) ) ;
#164240 = FACE_OUTER_BOUND ( 'NONE', #249322, .T. ) ;
#164241 = CARTESIAN_POINT ( 'NONE',  ( -23.15000000000000213, 5.950000000011163692, -190.6942976949651438 ) ) ;
#164243 = ORIENTED_EDGE ( 'NONE', *, *, #132353, .F. ) ;
#164242 = CARTESIAN_POINT ( 'NONE',  ( -18.59999999999999787, 64.25000000001222134, -148.2731074845243882 ) ) ;
#164245 = DIRECTION ( 'NONE',  ( 1.000000000000000000, 0.000000000000000000, 0.000000000000000000 ) ) ;
#164244 = CYLINDRICAL_SURFACE ( 'NONE', #220345, 0.1000000000000028644 ) ;
#164246 = AXIS2_PLACEMENT_3D ( 'NONE', #28553, #7664, #246270 ) ;
#164247 = VERTEX_POINT ( 'NONE', #67413 ) ;
#164249 = ORIENTED_EDGE ( 'NONE', *, *, #85742, .F. ) ;
#164248 = CARTESIAN_POINT ( 'NONE',  ( 21.05000000000005400, 77.36076146337680370, -43.99645795275012006 ) ) ;
#164250 = EDGE_LOOP ( 'NONE', ( #3895, #128728, #200372, #161006 ) ) ;
#164251 = DIRECTION ( 'NONE',  ( -0.8660254037844653530, 0.000000000000000000, -0.4999999999999539257 ) ) ;
#164252 = DIRECTION ( 'NONE',  ( 0.000000000000000000, 0.9856811345164800953, 0.1686199900910462790 ) ) ;
#164253 = AXIS2_PLACEMENT_3D ( 'NONE', #179704, #16789, #200533 ) ;
#164254 = EDGE_LOOP ( 'NONE', ( #72455, #86635, #63358, #37831 ) ) ;
#164255 = CARTESIAN_POINT ( 'NONE',  ( 18.49999999999998934, 69.35000000001228670, -157.6731074845243938 ) ) ;
#164256 = CARTESIAN_POINT ( 'NONE',  ( 20.94999999999999929, 87.65000000001246860, -172.9231074845242802 ) ) ;
#164257 = CARTESIAN_POINT ( 'NONE',  ( 18.41416235934318735, 37.99112772578903474, -261.0419300540665404 ) ) ;
#164258 = AXIS2_PLACEMENT_3D ( 'NONE', #173004, #34761, #73893 ) ;
#164259 = ORIENTED_EDGE ( 'NONE', *, *, #126082, .F. ) ;
#164260 = CYLINDRICAL_SURFACE ( 'NONE', #98352, 0.09999999999999895084 ) ;
#164261 = AXIS2_PLACEMENT_3D ( 'NONE', #183141, #41074, #4476 ) ;
#164262 = EDGE_CURVE ( 'NONE', #8702, #163445, #24467, .T. ) ;
#164263 = DIRECTION ( 'NONE',  ( 1.000000000000000000, -7.304098846218134667E-16, -5.100424963727256530E-30 ) ) ;
#164264 = ORIENTED_EDGE ( 'NONE', *, *, #112094, .T. ) ;
#164265 = ORIENTED_EDGE ( 'NONE', *, *, #73763, .F. ) ;
#164266 = EDGE_CURVE ( 'NONE', #117589, #58504, #8730, .T. ) ;
#164267 = DIRECTION ( 'NONE',  ( 0.000000000000000000, 0.4999999999999949485, -0.8660254037844415942 ) ) ;
#164268 = VERTEX_POINT ( 'NONE', #86946 ) ;
#164269 = DIRECTION ( 'NONE',  ( 1.000000000000000000, 0.000000000000000000, 0.000000000000000000 ) ) ;
#164270 = ORIENTED_EDGE ( 'NONE', *, *, #200770, .T. ) ;
#164271 = SPHERICAL_SURFACE ( 'NONE', #130166, 0.1000000000000000056 ) ;
#164272 = ADVANCED_FACE ( 'NONE', ( #226463 ), #163959, .T. ) ;
#164273 = EDGE_CURVE ( 'NONE', #123641, #118795, #58918, .T. ) ;
#164274 = CARTESIAN_POINT ( 'NONE',  ( -17.11825945287482753, 9.950000000011138823, -180.2499999999999716 ) ) ;
#164275 = DIRECTION ( 'NONE',  ( 1.000000000000000000, 0.000000000000000000, 0.000000000000000000 ) ) ;
#164276 = CARTESIAN_POINT ( 'NONE',  ( -2.995603634470891112E-16, 6.650000000011155876, -121.6500000000000341 ) ) ;
#164277 = EDGE_LOOP ( 'NONE', ( #42417, #126600, #69979, #218067, #180438 ) ) ;
#164278 = DIRECTION ( 'NONE',  ( -0.000000000000000000, 0.4721928772777345684, 0.8814952561688429444 ) ) ;
#164279 = DIRECTION ( 'NONE',  ( 1.000000000000000000, 0.000000000000000000, 0.000000000000000000 ) ) ;
#164280 = CARTESIAN_POINT ( 'NONE',  ( 18.47073956224755165, 85.47172941248341260, -62.41442173170622709 ) ) ;
#164281 = CYLINDRICAL_SURFACE ( 'NONE', #243182, 0.09999999999999939493 ) ;
#164282 = VECTOR ( 'NONE', #163915, 1000.000000000000000 ) ;
#164283 = ORIENTED_EDGE ( 'NONE', *, *, #60927, .T. ) ;
#164285 = FACE_OUTER_BOUND ( 'NONE', #128904, .T. ) ;
#164284 = CARTESIAN_POINT ( 'NONE',  ( -22.39999999999999503, 7.790779598384560245, -134.0000000000000000 ) ) ;
#164286 = ORIENTED_EDGE ( 'NONE', *, *, #229883, .T. ) ;
#164288 = VERTEX_POINT ( 'NONE', #85651 ) ;
#164287 =( LENGTH_UNIT ( ) NAMED_UNIT ( * ) SI_UNIT ( .MILLI., .METRE. ) );
#164289 = VERTEX_POINT ( 'NONE', #127394 ) ;
#164290 = CARTESIAN_POINT ( 'NONE',  ( -18.59999999999999787, 11.75000000001115197, -155.7499999999999716 ) ) ;
#164291 = ADVANCED_FACE ( 'NONE', ( #6141 ), #223902, .T. ) ;
#164292 = AXIS2_PLACEMENT_3D ( 'NONE', #175237, #130926, #153103 ) ;
#164293 = DIRECTION ( 'NONE',  ( -0.000000000000000000, 0.8874830700839094755, -0.4608403197577646826 ) ) ;
#164294 = CARTESIAN_POINT ( 'NONE',  ( -20.94999999999999929, 7.128833340093095217, -233.7327013124392749 ) ) ;
#164295 = AXIS2_PLACEMENT_3D ( 'NONE', #206742, #122080, #25553 ) ;
#164296 = ORIENTED_EDGE ( 'NONE', *, *, #104860, .T. ) ;
#164297 = CARTESIAN_POINT ( 'NONE',  ( -20.54999999999999716, 74.00000000001254818, -182.8477294072864652 ) ) ;
#164298 = DIRECTION ( 'NONE',  ( 0.000000000000000000, -0.2617529984165033463, -0.9651348961777157509 ) ) ;
#164299 = CIRCLE ( 'NONE', #160027, 0.1000000000000128147 ) ;
#164300 = CARTESIAN_POINT ( 'NONE',  ( 18.59999999999999076, 69.35000000001254250, -182.3731074845244109 ) ) ;
#164302 = ORIENTED_EDGE ( 'NONE', *, *, #80473, .T. ) ;
#164301 = CARTESIAN_POINT ( 'NONE',  ( 22.24259225415828567, 0.09906588345283645625, 7.491937870565415380 ) ) ;
#164303 = AXIS2_PLACEMENT_3D ( 'NONE', #214723, #36109, #33575 ) ;
#164304 = ADVANCED_FACE ( 'NONE', ( #183517 ), #45286, .F. ) ;
#164305 = AXIS2_PLACEMENT_3D ( 'NONE', #29418, #54073, #151922 ) ;
#164306 = EDGE_LOOP ( 'NONE', ( #247637, #48680, #226053, #128776, #76690, #100145 ) ) ;
#164308 = EDGE_CURVE ( 'NONE', #124696, #123531, #166698, .T. ) ;
#164307 = CARTESIAN_POINT ( 'NONE',  ( -20.07928932188135107, 9.220710678129810489, -112.8500000000000369 ) ) ;
#164309 = CARTESIAN_POINT ( 'NONE',  ( -18.34374000495060386, 11.47316190337362585, -176.7499999999999716 ) ) ;
#164310 = CARTESIAN_POINT ( 'NONE',  ( 23.24999999999999289, 52.91185528119409298, -244.1460391050142675 ) ) ;
#164311 = ORIENTED_EDGE ( 'NONE', *, *, #3323, .F. ) ;
#164312 = ORIENTED_EDGE ( 'NONE', *, *, #175032, .F. ) ;
#164313 = CARTESIAN_POINT ( 'NONE',  ( 21.05000000000000071, 18.75470391387417024, -230.0042304569477380 ) ) ;
#164314 = DIRECTION ( 'NONE',  ( 1.000000000000000000, -0.000000000000000000, -0.000000000000000000 ) ) ;
#164315 = DIRECTION ( 'NONE',  ( 0.000000000000000000, 0.000000000000000000, -1.000000000000000000 ) ) ;
#164316 = CIRCLE ( 'NONE', #85144, 0.1000000000000028644 ) ;
#164317 = ORIENTED_EDGE ( 'NONE', *, *, #53518, .F. ) ;
#164318 = EDGE_CURVE ( 'NONE', #71479, #173939, #206930, .T. ) ;
#164319 = DIRECTION ( 'NONE',  ( 0.000000000000000000, 0.1071148137998806232, 0.9942466578594150173 ) ) ;
#164320 = EDGE_CURVE ( 'NONE', #55464, #199951, #203068, .T. ) ;
#164321 = AXIS2_PLACEMENT_3D ( 'NONE', #113999, #193559, #96971 ) ;
#164322 = EDGE_CURVE ( 'NONE', #240054, #112979, #7432, .T. ) ;
#164323 = CARTESIAN_POINT ( 'NONE',  ( -20.64999999999999858, 4.350000000011156054, -121.6500000000000341 ) ) ;
#164324 = VECTOR ( 'NONE', #100192, 1000.000000000000000 ) ;
#164325 = AXIS2_PLACEMENT_3D ( 'NONE', #256657, #78066, #134188 ) ;
#164326 = EDGE_LOOP ( 'NONE', ( #39308, #63791, #221471, #52343 ) ) ;
#164327 = CIRCLE ( 'NONE', #93383, 0.1999999999999987899 ) ;
#164328 = ORIENTED_EDGE ( 'NONE', *, *, #218705, .T. ) ;
#164329 = VERTEX_POINT ( 'NONE', #167832 ) ;
#164330 = DIRECTION ( 'NONE',  ( 0.000000000000000000, -0.9910465087640861759, -0.1335171055202901691 ) ) ;
#164331 = VERTEX_POINT ( 'NONE', #247328 ) ;
#164333 = ORIENTED_EDGE ( 'NONE', *, *, #215239, .T. ) ;
#164332 = CARTESIAN_POINT ( 'NONE',  ( -23.25000000000000000, 11.65000000000000036, -21.25000000000000000 ) ) ;
#164334 = EDGE_CURVE ( 'NONE', #144252, #119824, #254552, .T. ) ;
#164335 = ORIENTED_EDGE ( 'NONE', *, *, #197483, .T. ) ;
#164338 = ORIENTED_EDGE ( 'NONE', *, *, #68489, .F. ) ;
#164337 = EDGE_LOOP ( 'NONE', ( #91884, #20943, #49239, #4563 ) ) ;
#164336 = CARTESIAN_POINT ( 'NONE',  ( -16.77902162784673834, 9.946419257218996890, -113.1619912440693838 ) ) ;
#164339 = EDGE_CURVE ( 'NONE', #245998, #79677, #15153, .T. ) ;
#164340 = CARTESIAN_POINT ( 'NONE',  ( 22.39999999999999503, 10.80758397488569500, -226.8651660546161395 ) ) ;
#164341 = ORIENTED_EDGE ( 'NONE', *, *, #124172, .T. ) ;
#164342 = DIRECTION ( 'NONE',  ( 0.000000000000000000, 0.4088369013363281068, -0.9126074666063770380 ) ) ;
#164343 = AXIS2_PLACEMENT_3D ( 'NONE', #169871, #129409, #208946 ) ;
#164344 = CARTESIAN_POINT ( 'NONE',  ( 21.05000000000000071, 67.12338541492552224, -195.1380270056797599 ) ) ;
#164345 = CARTESIAN_POINT ( 'NONE',  ( -18.48408745364672967, 87.07669050450563475, -199.6027005069816198 ) ) ;
#164346 = ORIENTED_EDGE ( 'NONE', *, *, #60837, .F. ) ;
#164347 = DIRECTION ( 'NONE',  ( -1.000000000000000000, 0.000000000000000000, 0.000000000000000000 ) ) ;
#164348 = CIRCLE ( 'NONE', #22887, 0.09999999999999767408 ) ;
#164349 =( BOUNDED_SURFACE ( )  B_SPLINE_SURFACE ( 3, 2, ( 
 ( #255106, #32292, #191370 ),
 ( #12729, #251296, #212203 ),
 ( #173110, #73995, #58222 ),
 ( #179497, #200325, #159937 ),
 ( #240742, #201600, #180769 ),
 ( #76513, #60797, #41282 ) ),
 .UNSPECIFIED., .F., .F., .F. ) 
 B_SPLINE_SURFACE_WITH_KNOTS ( ( 4, 2, 4 ),
 ( 3, 3 ),
 ( 0.0001792624049599564567, 0.0003686986002124703144, 0.0005581347954649841991 ),
 ( 0.000000000000000000, 1.000000000000000000 ),
 .UNSPECIFIED. ) 
 GEOMETRIC_REPRESENTATION_ITEM ( )  RATIONAL_B_SPLINE_SURFACE ( (
 ( 1.000000000000000000, 0.9238795325112719725, 1.000000000000000000),
 ( 1.000000000000000000, 0.9229318695243835524, 1.000000000000000000),
 ( 1.000000000000000000, 0.8926288119223798612, 1.000000000000000000),
 ( 1.000000000000000000, 0.8123777807278315111, 1.000000000000000000),
 ( 1.000000000000000000, 0.7629087100926418286, 1.000000000000000000),
 ( 1.000000000000000000, 0.7071067811865597852, 1.000000000000000000) ) ) 
 REPRESENTATION_ITEM ( '' )  SURFACE ( )  );
#164351 = ORIENTED_EDGE ( 'NONE', *, *, #61793, .T. ) ;
#164350 = CARTESIAN_POINT ( 'NONE',  ( -20.85000000000000142, 45.99141771592758943, -256.5205054824189119 ) ) ;
#164352 = DIRECTION ( 'NONE',  ( 0.000000000000000000, -0.9893560106964500722, 0.1455152366551550613 ) ) ;
#164354 = ORIENTED_EDGE ( 'NONE', *, *, #94076, .T. ) ;
#164353 = DIRECTION ( 'NONE',  ( 1.000000000000000000, 0.000000000000000000, 0.000000000000000000 ) ) ;
#164355 = ORIENTED_EDGE ( 'NONE', *, *, #209843, .T. ) ;
#164356 = CARTESIAN_POINT ( 'NONE',  ( -18.59999999999999787, -1.736705739456431807, -112.0174225876237699 ) ) ;
#164357 = ORIENTED_EDGE ( 'NONE', *, *, #27452, .F. ) ;
#164358 = ORIENTED_EDGE ( 'NONE', *, *, #257148, .T. ) ;
#164359 = CARTESIAN_POINT ( 'NONE',  ( -23.25000000000000000, 77.14957036958777792, -128.7071950000224092 ) ) ;
#164360 = LINE ( 'NONE', #246452, #186031 ) ;
#164362 = ORIENTED_EDGE ( 'NONE', *, *, #160949, .F. ) ;
#164361 = VERTEX_POINT ( 'NONE', #109095 ) ;
#164363 = CIRCLE ( 'NONE', #185016, 0.09999999999999642508 ) ;
#164364 = VERTEX_POINT ( 'NONE', #171687 ) ;
#164365 = LINE ( 'NONE', #243882, #206986 ) ;
#164366 = EDGE_LOOP ( 'NONE', ( #30506, #181419 ) ) ;
#164367 = ORIENTED_EDGE ( 'NONE', *, *, #105025, .F. ) ;
#164368 = CARTESIAN_POINT ( 'NONE',  ( 18.50000000000000711, 85.41907808086196496, -163.1931821343160323 ) ) ;
#164370 = ORIENTED_EDGE ( 'NONE', *, *, #158316, .T. ) ;
#164369 = CARTESIAN_POINT ( 'NONE',  ( 20.94999999999999929, 1.115600667400684642E-11, -67.00000000000000000 ) ) ;
#164371 = DIRECTION ( 'NONE',  ( 0.000000000000000000, 0.9126074666063844765, 0.4088369013363114535 ) ) ;
#164373 = CARTESIAN_POINT ( 'NONE',  ( 18.49999999999998579, -9.321008403350155902, -107.7359382490778614 ) ) ;
#164372 = CARTESIAN_POINT ( 'NONE',  ( -16.89268316805466341, 22.97380970494227626, -230.9308293615217451 ) ) ;
#164374 = ORIENTED_EDGE ( 'NONE', *, *, #164768, .F. ) ;
#164375 = VERTEX_POINT ( 'NONE', #189935 ) ;
#164376 = DIRECTION ( 'NONE',  ( 0.000000000000000000, -0.2128009952263603954, 0.9770955615653315052 ) ) ;
#164377 = CARTESIAN_POINT ( 'NONE',  ( 20.94999999999999929, 76.00000000001142553, -36.02310748452432421 ) ) ;
#164378 = EDGE_CURVE ( 'NONE', #241724, #119487, #183854, .T. ) ;
#164379 = VECTOR ( 'NONE', #136709, 1000.000000000000114 ) ;
#164380 = ORIENTED_EDGE ( 'NONE', *, *, #115968, .F. ) ;
#164381 = CIRCLE ( 'NONE', #139217, 0.09999999999999939493 ) ;
#164382 = CIRCLE ( 'NONE', #243474, 0.09999999999999799327 ) ;
#164383 = DIRECTION ( 'NONE',  ( -1.000000000000000000, -0.000000000000000000, -0.000000000000000000 ) ) ;
#164384 = ORIENTED_EDGE ( 'NONE', *, *, #243724, .T. ) ;
#164385 = ORIENTED_EDGE ( 'NONE', *, *, #41904, .T. ) ;
#164386 = MECHANICAL_DESIGN_GEOMETRIC_PRESENTATION_REPRESENTATION (  '', ( #180948 ), #176868 ) ;
#164387 = CARTESIAN_POINT ( 'NONE',  ( -20.94999999999999929, 76.00000000001126921, -203.5231074845248997 ) ) ;
#164388 = EDGE_CURVE ( 'NONE', #147060, #148919, #138038, .T. ) ;
#164389 = VERTEX_POINT ( 'NONE', #132530 ) ;
#164390 = CARTESIAN_POINT ( 'NONE',  ( -20.95613430942474054, 11.75000000001078604, -107.3571626482198695 ) ) ;
#164391 = CARTESIAN_POINT ( 'NONE',  ( 18.39999999999999503, 53.37686160793744961, -235.8706811220569932 ) ) ;
#164392 = ORIENTED_EDGE ( 'NONE', *, *, #17896, .T. ) ;
#164393 = CARTESIAN_POINT ( 'NONE',  ( 19.86930884467584590, 64.31308993304128307, -145.2838848455857317 ) ) ;
#164394 = DIRECTION ( 'NONE',  ( -1.000000000000000000, -0.000000000000000000, -0.000000000000000000 ) ) ;
#164396 = CARTESIAN_POINT ( 'NONE',  ( 23.14999999999999503, 64.35000000001245724, -181.7731074845244450 ) ) ;
#164395 = CARTESIAN_POINT ( 'NONE',  ( -18.50000000000000000, 9.250000000000001776, -21.35000000000000142 ) ) ;
#164397 = CARTESIAN_POINT ( 'NONE',  ( -23.15000000000000213, 85.00000000001159606, -59.62913836187181715 ) ) ;
#164398 = EDGE_CURVE ( 'NONE', #187157, #139949, #34735, .T. ) ;
#164400 = EDGE_CURVE ( 'NONE', #165343, #105902, #100436, .T. ) ;
#164399 = CARTESIAN_POINT ( 'NONE',  ( -20.85000000000000142, -1.835859311432481045, -145.5044391687985694 ) ) ;
#164401 = DIRECTION ( 'NONE',  ( 0.000000000000000000, -0.9126074666063660468, -0.4088369013363524762 ) ) ;
#164402 = DIRECTION ( 'NONE',  ( 0.000000000000000000, -0.9893560106964500722, 0.1455152366551550613 ) ) ;
#164403 = CIRCLE ( 'NONE', #51937, 11.75000000000001066 ) ;
#164404 = ORIENTED_EDGE ( 'NONE', *, *, #74526, .T. ) ;
#164405 = AXIS2_PLACEMENT_3D ( 'NONE', #103022, #163038, #239993 ) ;
#164406 = AXIS2_PLACEMENT_3D ( 'NONE', #67161, #87977, #244505 ) ;
#164408 = ORIENTED_EDGE ( 'NONE', *, *, #57861, .T. ) ;
#164407 = ORIENTED_EDGE ( 'NONE', *, *, #162852, .F. ) ;
#164409 = ORIENTED_EDGE ( 'NONE', *, *, #145332, .F. ) ;
#164410 = ADVANCED_FACE ( 'NONE', ( #149547 ), #170423, .T. ) ;
#164411 = CARTESIAN_POINT ( 'NONE',  ( -18.59999999999999787, 76.00000000001213607, -136.5231074845243313 ) ) ;
#164412 = SPHERICAL_SURFACE ( 'NONE', #16159, 0.1000000000000000056 ) ;
#164413 =( BOUNDED_SURFACE ( )  B_SPLINE_SURFACE ( 3, 2, ( 
 ( #66844, #129380, #185506 ),
 ( #6863, #146357, #10724 ),
 ( #246746, #90229, #190664 ),
 ( #30294, #225879, #47252 ),
 ( #126814, #169836, #250600 ),
 ( #68126, #210219, #27750 ) ),
 .UNSPECIFIED., .F., .F., .F. ) 
 B_SPLINE_SURFACE_WITH_KNOTS ( ( 4, 2, 4 ),
 ( 3, 3 ),
 ( 4.712388980384689674, 5.497787143782137953, 6.283185307179586232 ),
 ( 0.000000000000000000, 1.000000000000000000 ),
 .UNSPECIFIED. ) 
 GEOMETRIC_REPRESENTATION_ITEM ( )  RATIONAL_B_SPLINE_SURFACE ( (
 ( 1.000000000000000000, 0.7071067811865898722, 1.000000000000000000),
 ( 1.000000000000000000, 0.7727932973488216284, 1.000000000000000000),
 ( 1.000000000000000000, 0.8282379607654585252, 1.000000000000000000),
 ( 1.000000000000000000, 0.9038128468034328789, 1.000000000000000000),
 ( 1.000000000000000000, 0.9240297172247350366, 1.000000000000000000),
 ( 1.000000000000000000, 0.9238795325113333679, 1.000000000000000000) ) ) 
 REPRESENTATION_ITEM ( '' )  SURFACE ( )  );
#164415 = CARTESIAN_POINT ( 'NONE',  ( 21.70464131381650219, 7.095358018967851343, 0.000000000000000000 ) ) ;
#164414 = CARTESIAN_POINT ( 'NONE',  ( -23.15000000000000213, 2.600000000011156054, -122.2500000000000284 ) ) ;
#164416 = CARTESIAN_POINT ( 'NONE',  ( 20.95429402530550433, 67.12380584891013768, -161.5000207865867026 ) ) ;
#164417 = ORIENTED_EDGE ( 'NONE', *, *, #177624, .T. ) ;
#164418 = CIRCLE ( 'NONE', #243505, 3.970710678118653636 ) ;
#164419 = CARTESIAN_POINT ( 'NONE',  ( -20.89192007715127986, 10.32898536001801304, -106.0826683222764899 ) ) ;
#164420 = AXIS2_PLACEMENT_3D ( 'NONE', #10292, #151075, #89795 ) ;
#164422 = AXIS2_PLACEMENT_3D ( 'NONE', #176464, #113899, #235135 ) ;
#164421 = DIRECTION ( 'NONE',  ( 0.000000000000000000, -1.000000000000000000, -6.982962677686265922E-15 ) ) ;
#164423 = DIRECTION ( 'NONE',  ( -1.000000000000000000, -1.418437941187492324E-14, 3.166243193347622926E-14 ) ) ;
#164424 = DIRECTION ( 'NONE',  ( 0.000000000000000000, 0.000000000000000000, -1.000000000000000000 ) ) ;
#164426 = ORIENTED_EDGE ( 'NONE', *, *, #9600, .T. ) ;
#164425 = VECTOR ( 'NONE', #207435, 1000.000000000000000 ) ;
#164427 = LINE ( 'NONE', #143568, #163902 ) ;
#164428 = AXIS2_PLACEMENT_3D ( 'NONE', #78959, #178115, #114268 ) ;
#164429 = CARTESIAN_POINT ( 'NONE',  ( 18.54999999999999716, 23.65833333334447985, -184.2499999999999716 ) ) ;
#164430 = ORIENTED_EDGE ( 'NONE', *, *, #249208, .T. ) ;
#164432 = ORIENTED_EDGE ( 'NONE', *, *, #22227, .F. ) ;
#164431 = EDGE_CURVE ( 'NONE', #217380, #109970, #232935, .T. ) ;
#164433 = CARTESIAN_POINT ( 'NONE',  ( -20.94999999999999929, 7.939498413483247141, -209.7295111514051200 ) ) ;
#164434 = VECTOR ( 'NONE', #21805, 1000.000000000000000 ) ;
#164435 = CARTESIAN_POINT ( 'NONE',  ( -20.54999999999999716, 2.000000000011154189, -46.22462192276210402 ) ) ;
#164436 = EDGE_CURVE ( 'NONE', #216709, #239387, #129935, .T. ) ;
#164437 = CARTESIAN_POINT ( 'NONE',  ( -21.00000000000000000, 0.000000000000000000, 0.000000000000000000 ) ) ;
#164438 = CARTESIAN_POINT ( 'NONE',  ( 20.94999999999999929, 70.15000000001198543, -113.1556047088022581 ) ) ;
#164439 = CARTESIAN_POINT ( 'NONE',  ( 21.97500000000000497, 66.25000000001223555, -148.7731074845244450 ) ) ;
#164440 = VECTOR ( 'NONE', #174958, 1000.000000000000000 ) ;
#164441 = DIRECTION ( 'NONE',  ( 0.000000000000000000, 1.000000000000000000, 0.000000000000000000 ) ) ;
#164443 = EDGE_LOOP ( 'NONE', ( #3346, #96635, #189753, #205313 ) ) ;
#164442 = AXIS2_PLACEMENT_3D ( 'NONE', #3564, #139205, #63538 ) ;
#164444 = DIRECTION ( 'NONE',  ( -1.000000000000000000, -7.304098846218134667E-16, 0.000000000000000000 ) ) ;
#164445 = CARTESIAN_POINT ( 'NONE',  ( 20.95595012432479365, 11.97768371613162586, -206.1652126091303785 ) ) ;
#164447 = CARTESIAN_POINT ( 'NONE',  ( 18.59999999999999432, 5.699452464332755319, -154.9577260434301422 ) ) ;
#164446 = DIRECTION ( 'NONE',  ( 0.000000000000000000, 0.000000000000000000, 1.000000000000000000 ) ) ;
#164448 = DIRECTION ( 'NONE',  ( 1.000000000000000000, 0.000000000000000000, 0.000000000000000000 ) ) ;
#164449 = EDGE_CURVE ( 'NONE', #24875, #134102, #171419, .T. ) ;
#164450 = DIRECTION ( 'NONE',  ( 1.000000000000000000, 0.000000000000000000, 0.000000000000000000 ) ) ;
#164451 = DIRECTION ( 'NONE',  ( 1.000000000000000000, 0.000000000000000000, 0.000000000000000000 ) ) ;
#164453 = ORIENTED_EDGE ( 'NONE', *, *, #72698, .T. ) ;
#164452 = LINE ( 'NONE', #224403, #40379 ) ;
#164454 =( BOUNDED_CURVE ( )  B_SPLINE_CURVE ( 3, ( #204275, #8658, #225113, #46482 ),
 .UNSPECIFIED., .F., .F. ) 
 B_SPLINE_CURVE_WITH_KNOTS ( ( 4, 4 ),
 ( 4.712388980384689674, 6.283185307179586232 ),
 .UNSPECIFIED. ) 
 CURVE ( )  GEOMETRIC_REPRESENTATION_ITEM ( )  RATIONAL_B_SPLINE_CURVE ( ( 1.000000000000000000, 0.8047378541243649375, 0.8047378541243649375, 1.000000000000000000 ) ) 
 REPRESENTATION_ITEM ( '' )  );
#164455 = DIRECTION ( 'NONE',  ( 0.000000000000000000, -1.000000000000000000, 0.000000000000000000 ) ) ;
#164456 = CIRCLE ( 'NONE', #152007, 11.74999999999999645 ) ;
#164457 = CIRCLE ( 'NONE', #176947, 0.1000000000000028644 ) ;
#164458 = CARTESIAN_POINT ( 'NONE',  ( -20.05000000000000426, 9.250000000000001776, -21.15000000000000213 ) ) ;
#164459 = VECTOR ( 'NONE', #241852, 1000.000000000000000 ) ;
#164460 = CARTESIAN_POINT ( 'NONE',  ( 15.74999999999999645, 9.350000000011139178, -150.7500000000000284 ) ) ;
#164461 = ORIENTED_EDGE ( 'NONE', *, *, #8475, .F. ) ;
#164462 = DIRECTION ( 'NONE',  ( 0.000000000000000000, -6.982962677686266711E-15, 1.000000000000000000 ) ) ;
#164463 = DIRECTION ( 'NONE',  ( -0.000000000000000000, -1.000000000000000000, -6.982962677686266711E-15 ) ) ;
#164464 = CARTESIAN_POINT ( 'NONE',  ( -20.54999999999999716, 73.60000000001251408, -179.9170766071768242 ) ) ;
#164465 = CIRCLE ( 'NONE', #64672, 11.70000000000000284 ) ;
#164466 = EDGE_CURVE ( 'NONE', #255696, #57112, #131236, .T. ) ;
#164467 = AXIS2_PLACEMENT_3D ( 'NONE', #67891, #249118, #45757 ) ;
#164468 = EDGE_CURVE ( 'NONE', #60368, #152543, #92263, .T. ) ;
#164469 = ORIENTED_EDGE ( 'NONE', *, *, #228610, .T. ) ;
#164470 = DIRECTION ( 'NONE',  ( 0.000000000000000000, 0.8814952561688429444, -0.4721928772777349015 ) ) ;
#164472 = ORIENTED_EDGE ( 'NONE', *, *, #155726, .T. ) ;
#164471 = CARTESIAN_POINT ( 'NONE',  ( -18.59999999999999787, 1.750000000011155743, -179.1695115579016147 ) ) ;
#164474 = CARTESIAN_POINT ( 'NONE',  ( -16.77683809663752257, 66.05416425680765258, -82.18705650362858250 ) ) ;
#164473 = CARTESIAN_POINT ( 'NONE',  ( 21.10257677756355932, -1.337202735977050638, -194.7428600538324019 ) ) ;
#164476 = ADVANCED_FACE ( 'NONE', ( #231639 ), #33872, .T. ) ;
#164475 = DIRECTION ( 'NONE',  ( -1.000000000000000000, 0.000000000000000000, 0.000000000000000000 ) ) ;
#164477 = EDGE_CURVE ( 'NONE', #22057, #214167, #108823, .T. ) ;
#164478 = ORIENTED_EDGE ( 'NONE', *, *, #5267, .F. ) ;
#164479 = CARTESIAN_POINT ( 'NONE',  ( 23.15000000000000213, -11.48912529306489994, -63.89999999999999858 ) ) ;
#164480 = AXIS2_PLACEMENT_3D ( 'NONE', #137432, #98283, #141305 ) ;
#164481 = DIRECTION ( 'NONE',  ( 1.000000000000000000, 0.000000000000000000, 0.000000000000000000 ) ) ;
#164482 = DIRECTION ( 'NONE',  ( 1.000000000000000000, 0.000000000000000000, 0.000000000000000000 ) ) ;
#164483 = DIRECTION ( 'NONE',  ( 0.000000000000000000, -6.982962677686266711E-15, 1.000000000000000000 ) ) ;
#164484 = CARTESIAN_POINT ( 'NONE',  ( 20.95512820512820440, 8.876151316299271343, -179.6499999999999773 ) ) ;
#164485 = VECTOR ( 'NONE', #43070, 1000.000000000000000 ) ;
#164486 = VERTEX_POINT ( 'NONE', #30892 ) ;
#164487 = CARTESIAN_POINT ( 'NONE',  ( 18.49999999999999289, 69.35000000001200249, -115.3731074845243398 ) ) ;
#164488 = CIRCLE ( 'NONE', #110297, 0.1000000000000028644 ) ;
#164489 = ADVANCED_FACE ( 'NONE', ( #49129 ), #200418, .F. ) ;
#164490 = DIRECTION ( 'NONE',  ( 0.000000000000000000, 0.4088369013363345461, -0.9126074666063741514 ) ) ;
#164492 = ADVANCED_FACE ( 'NONE', ( #252451 ), #21373, .F. ) ;
#164491 = EDGE_CURVE ( 'NONE', #118720, #86236, #154659, .T. ) ;
#164493 = CYLINDRICAL_SURFACE ( 'NONE', #53345, 0.09999999999999881206 ) ;
#164494 = CARTESIAN_POINT ( 'NONE',  ( -23.15000000000000213, 2.000000000011154189, -113.2246219227621395 ) ) ;
#164495 = ORIENTED_EDGE ( 'NONE', *, *, #22727, .T. ) ;
#164497 = EDGE_CURVE ( 'NONE', #179358, #116282, #128688, .T. ) ;
#164496 = CIRCLE ( 'NONE', #135429, 11.65000000000000036 ) ;
#164498 = VERTEX_POINT ( 'NONE', #179374 ) ;
#164499 = CARTESIAN_POINT ( 'NONE',  ( 22.40000000000020819, 76.10085836911140689, -81.27267460801402876 ) ) ;
#164500 = DIRECTION ( 'NONE',  ( 1.000000000000000000, 0.000000000000000000, 0.000000000000000000 ) ) ;
#164501 = CARTESIAN_POINT ( 'NONE',  ( 18.59999999999999432, 77.83585931145600512, -158.5186683157258187 ) ) ;
#164502 = EDGE_CURVE ( 'NONE', #140279, #27375, #200207, .T. ) ;
#164503 = DIRECTION ( 'NONE',  ( 0.7071359030027593029, -0.7070776581709197206, 0.000000000000000000 ) ) ;
#164504 = CARTESIAN_POINT ( 'NONE',  ( 21.09787244211752011, 8.775370707348422172, -146.2392533843176352 ) ) ;
#164505 = CARTESIAN_POINT ( 'NONE',  ( -12.25000000000000178, 62.59162599727320497, -217.2417264603073477 ) ) ;
#164506 = DIRECTION ( 'NONE',  ( -0.000000000000000000, -0.4721928772777330696, -0.8814952561688438326 ) ) ;
#164508 = EDGE_CURVE ( 'NONE', #184497, #18470, #167137, .T. ) ;
#164507 = DIRECTION ( 'NONE',  ( 0.000000000000000000, 0.000000000000000000, 1.000000000000000000 ) ) ;
#164510 = EDGE_CURVE ( 'NONE', #126171, #63693, #96340, .T. ) ;
#164509 = DIRECTION ( 'NONE',  ( 0.000000000000000000, 1.000000000000000000, 6.982962677686266711E-15 ) ) ;
#164511 = AXIS2_PLACEMENT_3D ( 'NONE', #99859, #179452, #80292 ) ;
#164513 = ORIENTED_EDGE ( 'NONE', *, *, #60221, .F. ) ;
#164512 = CARTESIAN_POINT ( 'NONE',  ( 15.07585980824112681, 62.89253001998300618, -215.8738493471900597 ) ) ;
#164514 = CIRCLE ( 'NONE', #43691, 4.099999999999992539 ) ;
#164515 = CARTESIAN_POINT ( 'NONE',  ( -20.97625342178408658, 64.39999999919190543, -129.5949042547223655 ) ) ;
#164516 = DIRECTION ( 'NONE',  ( -1.000000000000000000, 0.000000000000000000, 0.000000000000000000 ) ) ;
#164518 = CARTESIAN_POINT ( 'NONE',  ( -18.50000000000000000, 64.35000000001222986, -148.2731074845243882 ) ) ;
#164517 = CARTESIAN_POINT ( 'NONE',  ( -20.64999999999999858, 4.350000000011156054, -188.6499999999999488 ) ) ;
#164519 = EDGE_CURVE ( 'NONE', #214929, #2240, #101040, .T. ) ;
#164520 = ORIENTED_EDGE ( 'NONE', *, *, #133605, .T. ) ;
#164521 = DIRECTION ( 'NONE',  ( -1.000000000000000000, 0.000000000000000000, 0.000000000000000000 ) ) ;
#164522 = CARTESIAN_POINT ( 'NONE',  ( 20.94999999999999574, 8.926614585098251453, -41.97168301922312850 ) ) ;
#164523 = CARTESIAN_POINT ( 'NONE',  ( -21.00000000000000000, 6.726092018229619995, 9.512212474619552438 ) ) ;
#164524 = DIRECTION ( 'NONE',  ( 1.000000000000000000, -0.000000000000000000, -0.000000000000000000 ) ) ;
#164525 = CARTESIAN_POINT ( 'NONE',  ( -12.68215100488890634, 66.60336962369484581, -185.6160500917061142 ) ) ;
#164526 = ORIENTED_EDGE ( 'NONE', *, *, #99099, .T. ) ;
#164527 = ADVANCED_FACE ( 'NONE', ( #135070 ), #163030, .T. ) ;
#164528 = VERTEX_POINT ( 'NONE', #76380 ) ;
#164529 = ADVANCED_FACE ( 'NONE', ( #218458 ), #155968, .T. ) ;
#164530 = CARTESIAN_POINT ( 'NONE',  ( 23.24999999999999645, 59.20211495293902715, -220.5705723384363637 ) ) ;
#164531 = VERTEX_POINT ( 'NONE', #120692 ) ;
#164532 = DIRECTION ( 'NONE',  ( 0.000000000000000000, 0.000000000000000000, -1.000000000000000000 ) ) ;
#164533 = AXIS2_PLACEMENT_3D ( 'NONE', #98590, #101148, #119496 ) ;
#164534 = ORIENTED_EDGE ( 'NONE', *, *, #146181, .T. ) ;
#164535 = CARTESIAN_POINT ( 'NONE',  ( -21.05000000000000071, 7.128833340093095217, -233.7327013124392749 ) ) ;
#164536 = DIRECTION ( 'NONE',  ( 0.000000000000000000, 1.000000000000000000, 0.000000000000000000 ) ) ;
#164537 = CIRCLE ( 'NONE', #81278, 0.09999999999999681366 ) ;
#164538 = CARTESIAN_POINT ( 'NONE',  ( -21.05000000000000071, 62.86885547537412577, -207.0505773246642036 ) ) ;
#164539 = EDGE_LOOP ( 'NONE', ( #165469, #181712, #245490, #198939 ) ) ;
#164540 = ADVANCED_FACE ( 'NONE', ( #77660 ), #246619, .T. ) ;
#164541 = DIRECTION ( 'NONE',  ( 0.000000000000000000, 0.4088369013363281068, -0.9126074666063770380 ) ) ;
#164542 = CARTESIAN_POINT ( 'NONE',  ( -16.87331047859649757, 66.05000000001201954, -115.6731074845243796 ) ) ;
#164543 = CARTESIAN_POINT ( 'NONE',  ( 20.94999999999999929, 11.65000000001115943, -160.7161343370219129 ) ) ;
#164544 = FACE_OUTER_BOUND ( 'NONE', #4932, .T. ) ;
#164545 = CARTESIAN_POINT ( 'NONE',  ( -16.92989143108098204, 44.34764822598747713, -235.2038836196412603 ) ) ;
#164546 = DIRECTION ( 'NONE',  ( 0.000000000000000000, 0.2128009952263485993, -0.9770955615653341697 ) ) ;
#164547 = CARTESIAN_POINT ( 'NONE',  ( 15.39793903038207823, 62.27137470634864513, -218.2709398499965801 ) ) ;
#164548 = ORIENTED_EDGE ( 'NONE', *, *, #250664, .T. ) ;
#164550 = CARTESIAN_POINT ( 'NONE',  ( 20.94999999999999574, 76.00000000001213607, -136.5231074845242745 ) ) ;
#164549 = DIRECTION ( 'NONE',  ( -6.938893903907222067E-15, 1.000000000000000000, 2.891205793294679805E-16 ) ) ;
#164551 = EDGE_LOOP ( 'NONE', ( #163563, #224699, #249657, #51052, #102689 ) ) ;
#164553 = VERTEX_POINT ( 'NONE', #17695 ) ;
#164552 = DIRECTION ( 'NONE',  ( 0.000000000000000000, 0.000000000000000000, 1.000000000000000000 ) ) ;
#164554 = AXIS2_PLACEMENT_3D ( 'NONE', #184830, #144400, #123587 ) ;
#164555 = VERTEX_POINT ( 'NONE', #119387 ) ;
#164556 = AXIS2_PLACEMENT_3D ( 'NONE', #20802, #19510, #98999 ) ;
#164557 = CARTESIAN_POINT ( 'NONE',  ( -21.14999999999999858, 76.10000000001272724, -209.7731074845243597 ) ) ;
#164558 = CARTESIAN_POINT ( 'NONE',  ( 18.50000324121758055, 10.29307482169091692, -72.45864214669397541 ) ) ;
#164559 = DIRECTION ( 'NONE',  ( -1.000000000000000000, 0.000000000000000000, -0.000000000000000000 ) ) ;
#164560 = DIRECTION ( 'NONE',  ( 0.000000000000000000, -0.9999631594459053030, -0.008583690987162452199 ) ) ;
#164561 = ORIENTED_EDGE ( 'NONE', *, *, #219762, .T. ) ;
#164562 = CARTESIAN_POINT ( 'NONE',  ( -16.27683809663750480, 9.350000000011133849, -143.2500000000000284 ) ) ;
#164563 = CARTESIAN_POINT ( 'NONE',  ( -21.05000000000000071, 76.00000000001165290, -69.52310748452431710 ) ) ;
#164564 = EDGE_LOOP ( 'NONE', ( #126666, #44272, #195487, #121966 ) ) ;
#164565 = CARTESIAN_POINT ( 'NONE',  ( 21.05000000000000071, 71.14953271029267512, -157.9888400755227167 ) ) ;
#164566 = ADVANCED_FACE ( 'NONE', ( #239333 ), #176806, .T. ) ;
#164568 = VECTOR ( 'NONE', #7475, 1000.000000000000227 ) ;
#164567 = CARTESIAN_POINT ( 'NONE',  ( -22.59999999999999787, 76.00000000001237765, -170.0231074845243597 ) ) ;
#164569 = ORIENTED_EDGE ( 'NONE', *, *, #237694, .T. ) ;
#164570 = EDGE_CURVE ( 'NONE', #216880, #208882, #79598, .T. ) ;
#164572 = CARTESIAN_POINT ( 'NONE',  ( -16.92280123533699054, 9.950000000011137047, -146.8506323140851180 ) ) ;
#164571 = TOROIDAL_SURFACE ( 'NONE', #235272, 11.65000000000000036, 0.1000000000000000056 ) ;
#164573 = ORIENTED_EDGE ( 'NONE', *, *, #203042, .T. ) ;
#164574 = CARTESIAN_POINT ( 'NONE',  ( -20.64999999999999858, 85.00000000001222134, -146.4170766071767389 ) ) ;
#164575 = EDGE_LOOP ( 'NONE', ( #89757, #48606, #75220, #63369 ) ) ;
#164576 = DIRECTION ( 'NONE',  ( 0.000000000000000000, 0.000000000000000000, -1.000000000000000000 ) ) ;
#164577 =( GEOMETRIC_REPRESENTATION_CONTEXT ( 3 ) GLOBAL_UNCERTAINTY_ASSIGNED_CONTEXT ( ( #165191 ) ) GLOBAL_UNIT_ASSIGNED_CONTEXT ( ( #74644, #155466, #36798 ) ) REPRESENTATION_CONTEXT ( 'NONE', 'WORKASPACE' ) );
#164578 = EDGE_CURVE ( 'NONE', #232481, #175607, #175528, .T. ) ;
#164579 = ADVANCED_FACE ( 'NONE', ( #78936 ), #1981, .T. ) ;
#164580 = FACE_OUTER_BOUND ( 'NONE', #126504, .T. ) ;
#164581 = CARTESIAN_POINT ( 'NONE',  ( 21.05000000000000071, 85.40000000001198543, -112.9170766071766820 ) ) ;
#164582 = CARTESIAN_POINT ( 'NONE',  ( -22.47071067811865674, 7.522163794833024220, -199.2603376134759117 ) ) ;
#164583 = FACE_OUTER_BOUND ( 'NONE', #181699, .T. ) ;
#164584 = DIRECTION ( 'NONE',  ( -0.000000000000000000, -1.000000000000000000, 0.000000000000000000 ) ) ;
#164585 = AXIS2_PLACEMENT_3D ( 'NONE', #78022, #121042, #239678 ) ;
#164586 = ORIENTED_EDGE ( 'NONE', *, *, #220639, .T. ) ;
#164588 = DIRECTION ( 'NONE',  ( 0.000000000000000000, -0.1298341882520022694, -0.9915357197604853789 ) ) ;
#164587 = CARTESIAN_POINT ( 'NONE',  ( 18.39999999999997371, 11.47316190336247388, -24.25000000000001066 ) ) ;
#164589 = AXIS2_PLACEMENT_3D ( 'NONE', #16845, #238441, #134192 ) ;
#164590 = ADVANCED_FACE ( 'NONE', ( #137635 ), #238032, .F. ) ;
#164591 = CIRCLE ( 'NONE', #97903, 0.09999999999999939493 ) ;
#164592 = ORIENTED_EDGE ( 'NONE', *, *, #187158, .F. ) ;
#164593 = CARTESIAN_POINT ( 'NONE',  ( -18.59999999999999787, 74.83729825007408465, -128.4231074845243086 ) ) ;
#164594 = CARTESIAN_POINT ( 'NONE',  ( -23.15000000000000213, 74.00000000001186606, -89.79848556176222019 ) ) ;
#164596 = ORIENTED_EDGE ( 'NONE', *, *, #240703, .F. ) ;
#164595 = CARTESIAN_POINT ( 'NONE',  ( -18.50000000000000000, -9.399999999988850163, -207.8820418481726335 ) ) ;
#164598 = ORIENTED_EDGE ( 'NONE', *, *, #201594, .T. ) ;
#164597 = SPHERICAL_SURFACE ( 'NONE', #8082, 0.1000000000000000056 ) ;
#164599 = DIRECTION ( 'NONE',  ( -1.000000000000000000, -0.000000000000000000, -0.000000000000000000 ) ) ;
#164600 = DIRECTION ( 'NONE',  ( 0.000000000000000000, -0.3738317757008748909, -0.9274965247785733613 ) ) ;
#164601 = CARTESIAN_POINT ( 'NONE',  ( 23.15000000000000213, 12.29073439453116201, -249.8274140313476437 ) ) ;
#164602 = TOROIDAL_SURFACE ( 'NONE', #181361, 0.2000000000000000111, 0.1000000000000000056 ) ;
#164603 = DIRECTION ( 'NONE',  ( 1.000000000000000000, 0.000000000000000000, 0.000000000000000000 ) ) ;
#164604 = AXIS2_PLACEMENT_3D ( 'NONE', #121619, #101992, #347 ) ;
#164605 = ORIENTED_EDGE ( 'NONE', *, *, #240103, .T. ) ;
#164606 = EDGE_CURVE ( 'NONE', #56789, #234281, #158754, .T. ) ;
#164607 = CARTESIAN_POINT ( 'NONE',  ( 23.14999999999999147, 4.150000000011154988, -167.4999999999999716 ) ) ;
#164608 = AXIS2_PLACEMENT_3D ( 'NONE', #18716, #98209, #257272 ) ;
#164609 = ORIENTED_EDGE ( 'NONE', *, *, #79475, .T. ) ;
#164610 = VERTEX_POINT ( 'NONE', #46249 ) ;
#164611 = VECTOR ( 'NONE', #77241, 1000.000000000000000 ) ;
#164612 = DIRECTION ( 'NONE',  ( 0.000000000000000000, -1.000000000000000000, 0.000000000000000000 ) ) ;
#164613 = CYLINDRICAL_SURFACE ( 'NONE', #188952, 0.09999999999998898659 ) ;
#164614 = CIRCLE ( 'NONE', #177106, 0.09999999999998898659 ) ;
#164616 = EDGE_LOOP ( 'NONE', ( #133122, #56685, #75469, #159811 ) ) ;
#164615 = AXIS2_PLACEMENT_3D ( 'NONE', #48809, #207914, #146607 ) ;
#164617 = ADVANCED_FACE ( 'NONE', ( #124525 ), #46275, .T. ) ;
#164618 = CYLINDRICAL_SURFACE ( 'NONE', #108370, 0.1000000000000028644 ) ;
#164619 = EDGE_CURVE ( 'NONE', #123853, #191279, #187957, .T. ) ;
#164620 = DIRECTION ( 'NONE',  ( 8.775271659896538527E-15, -0.1686199900910279881, 0.9856811345164833149 ) ) ;
#164621 = ORIENTED_EDGE ( 'NONE', *, *, #35870, .T. ) ;
#164622 = CARTESIAN_POINT ( 'NONE',  ( 20.27550659511089037, 9.216043722519994930, -188.3499999999999659 ) ) ;
#164623 = EDGE_CURVE ( 'NONE', #197944, #9728, #201326, .T. ) ;
#164624 = ORIENTED_EDGE ( 'NONE', *, *, #21198, .F. ) ;
#164625 = ORIENTED_EDGE ( 'NONE', *, *, #43733, .T. ) ;
#164626 = DIRECTION ( 'NONE',  ( 1.000000000000000000, 0.000000000000000000, 0.000000000000000000 ) ) ;
#164627 = ORIENTED_EDGE ( 'NONE', *, *, #63600, .T. ) ;
#164628 = CARTESIAN_POINT ( 'NONE',  ( -16.85939591225058720, 23.23024940989758136, -231.1209430754783796 ) ) ;
#164629 = EDGE_LOOP ( 'NONE', ( #177591, #49515, #91766, #93389 ) ) ;
#164631 = VERTEX_POINT ( 'NONE', #5827 ) ;
#164630 = DIRECTION ( 'NONE',  ( -1.000000000000000000, 0.000000000000000000, 0.000000000000000000 ) ) ;
#164632 = EDGE_CURVE ( 'NONE', #116802, #75446, #196312, .T. ) ;
#164633 = ADVANCED_FACE ( 'NONE', ( #141503 ), #47522, .F. ) ;
#164634 = LINE ( 'NONE', #205009, #148450 ) ;
#164635 = EDGE_LOOP ( 'NONE', ( #55906, #143762, #221820, #123558 ) ) ;
#164636 = CIRCLE ( 'NONE', #218586, 0.1000000000000028644 ) ;
#164638 = B_SPLINE_CURVE_WITH_KNOTS ( 'NONE', 3,
 ( #58534, #132975, #16879, #53420, #35185, #13037, #174705, #39008, #237199, #232079, #191686, #192940, #36455 ),
 .UNSPECIFIED., .F., .F.,
 ( 4, 3, 3, 3, 4 ),
 ( 1.084445006577768341E-16, 1.946463881814499081E-05, 3.922356109944648083E-05, 4.215060953239448225E-05, 4.415117091092920593E-05 ),
 .UNSPECIFIED. ) ;
#164637 = CARTESIAN_POINT ( 'NONE',  ( 18.59999999999999787, 87.75000000001149658, -48.17310748452423752 ) ) ;
#164639 = ORIENTED_EDGE ( 'NONE', *, *, #236638, .F. ) ;
#164640 = VECTOR ( 'NONE', #197632, 999.9999999999998863 ) ;
#164642 = ORIENTED_EDGE ( 'NONE', *, *, #147066, .T. ) ;
#164641 = ORIENTED_EDGE ( 'NONE', *, *, #179550, .F. ) ;
#164643 = CARTESIAN_POINT ( 'NONE',  ( 21.05000000000000071, 69.45934304831089889, -136.4231074845243654 ) ) ;
#164644 = EDGE_CURVE ( 'NONE', #102761, #100166, #8426, .T. ) ;
#164645 = CIRCLE ( 'NONE', #31398, 1.749999999999999778 ) ;
#164646 = CARTESIAN_POINT ( 'NONE',  ( -23.25000000000000000, -11.74999999998884448, -67.00000000000000000 ) ) ;
#164647 = ORIENTED_EDGE ( 'NONE', *, *, #128538, .F. ) ;
#164648 = CIRCLE ( 'NONE', #44017, 1.900000000000005906 ) ;
#164649 = CIRCLE ( 'NONE', #252115, 0.09999999999999939493 ) ;
#164650 = ORIENTED_EDGE ( 'NONE', *, *, #157185, .F. ) ;
#164651 = CARTESIAN_POINT ( 'NONE',  ( -21.05000000000046967, 69.55922910635128176, -203.5055102975169348 ) ) ;
#164652 = ADVANCED_FACE ( 'NONE', ( #202763 ), #24151, .T. ) ;
#164653 = CARTESIAN_POINT ( 'NONE',  ( -18.50000000000000000, 9.350000000011156942, -79.15000000000003411 ) ) ;
#164655 = VERTEX_POINT ( 'NONE', #240610 ) ;
#164654 = CARTESIAN_POINT ( 'NONE',  ( -23.15000000000000213, -8.596261682231835621, -176.9501275171502641 ) ) ;
#164656 = DIRECTION ( 'NONE',  ( 0.000000000000000000, -1.000000000000000000, 0.000000000000000000 ) ) ;
#164657 = ORIENTED_EDGE ( 'NONE', *, *, #175616, .F. ) ;
#164658 = CARTESIAN_POINT ( 'NONE',  ( 21.97500000000000497, 52.06567329910104291, -231.9654557484363409 ) ) ;
#164659 = CARTESIAN_POINT ( 'NONE',  ( 20.94999999999999929, 5.500000000011153745, -146.4052660189131245 ) ) ;
#164660 = AXIS2_PLACEMENT_3D ( 'NONE', #17226, #176306, #255773 ) ;
#164661 = VERTEX_POINT ( 'NONE', #61982 ) ;
#164662 = DIRECTION ( 'NONE',  ( -1.000000000000000000, -1.646408749285562691E-14, 1.073024830501117725E-15 ) ) ;
#164663 = DIRECTION ( 'NONE',  ( 0.000000000000000000, -1.000000000000000000, 0.000000000000000000 ) ) ;
#164664 = ORIENTED_EDGE ( 'NONE', *, *, #107211, .T. ) ;
#164665 = LINE ( 'NONE', #145078, #242951 ) ;
#164666 = VERTEX_POINT ( 'NONE', #85352 ) ;
#164668 = VERTEX_POINT ( 'NONE', #244450 ) ;
#164667 = ORIENTED_EDGE ( 'NONE', *, *, #29050, .T. ) ;
#164669 = ORIENTED_EDGE ( 'NONE', *, *, #81416, .T. ) ;
#164670 = CARTESIAN_POINT ( 'NONE',  ( -21.05000000000000071, 4.252251777740764460, -211.8999245327126744 ) ) ;
#164671 = ORIENTED_EDGE ( 'NONE', *, *, #10457, .T. ) ;
#164672 = CARTESIAN_POINT ( 'NONE',  ( 20.85000000000000142, 43.02787096365918984, -254.3959382439171577 ) ) ;
#164673 = AXIS2_PLACEMENT_3D ( 'NONE', #36395, #196715, #115912 ) ;
#164674 = EDGE_LOOP ( 'NONE', ( #149744, #186196, #109111, #54940 ) ) ;
#164675 = CARTESIAN_POINT ( 'NONE',  ( -16.92778301347278003, 65.99905508317625902, -48.59458937655572441 ) ) ;
#164676 = CARTESIAN_POINT ( 'NONE',  ( 21.03670563405601968, 43.56349054571641233, -234.8157308747548484 ) ) ;
#164677 = ORIENTED_EDGE ( 'NONE', *, *, #91517, .F. ) ;
#164678 = ORIENTED_EDGE ( 'NONE', *, *, #135682, .F. ) ;
#164679 = ORIENTED_EDGE ( 'NONE', *, *, #33333, .F. ) ;
#164680 = CIRCLE ( 'NONE', #98013, 0.1000000000000028644 ) ;
#164681 = ADVANCED_FACE ( 'NONE', ( #103640 ), #184475, .T. ) ;
#164682 = CIRCLE ( 'NONE', #177183, 3.970710678118653636 ) ;
#164683 = DIRECTION ( 'NONE',  ( -1.000000000000000000, 0.000000000000000000, 0.000000000000000000 ) ) ;
#164684 = ORIENTED_EDGE ( 'NONE', *, *, #3886, .F. ) ;
#164685 = CARTESIAN_POINT ( 'NONE',  ( 21.56666275994540172, 76.00000000001219291, -143.4804758914176261 ) ) ;
#164686 = EDGE_CURVE ( 'NONE', #92384, #229005, #213062, .T. ) ;
#164688 = ORIENTED_EDGE ( 'NONE', *, *, #102012, .F. ) ;
#164687 = DIRECTION ( 'NONE',  ( 1.000000000000000000, 0.000000000000000000, 0.000000000000000000 ) ) ;
#164689 = DIRECTION ( 'NONE',  ( 0.000000000000000000, -1.000000000000000000, 0.000000000000000000 ) ) ;
#164690 = CARTESIAN_POINT ( 'NONE',  ( -21.04386569057559697, 11.75000000001104539, -127.1428373517806421 ) ) ;
#164691 = DIRECTION ( 'NONE',  ( -1.000000000000000000, -0.000000000000000000, -0.000000000000000000 ) ) ;
#164692 = DIRECTION ( 'NONE',  ( 0.000000000000000000, 0.000000000000000000, -1.000000000000000000 ) ) ;
#164693 = FACE_OUTER_BOUND ( 'NONE', #84895, .T. ) ;
#164694 = EDGE_CURVE ( 'NONE', #104833, #83651, #9695, .T. ) ;
#164696 = CARTESIAN_POINT ( 'NONE',  ( 21.08134388332232234, 6.334680580529114202, -100.4241810824930070 ) ) ;
#164695 = DIRECTION ( 'NONE',  ( 0.000000000000000000, 0.000000000000000000, -1.000000000000000000 ) ) ;
#164698 = EDGE_CURVE ( 'NONE', #42134, #41545, #21549, .T. ) ;
#164697 = DIRECTION ( 'NONE',  ( 1.000000000000000000, 0.000000000000000000, 0.000000000000000000 ) ) ;
#164699 = CARTESIAN_POINT ( 'NONE',  ( 20.00000000000000711, 4.645987002755569861, 21.91686199900910736 ) ) ;
#164700 = LINE ( 'NONE', #99550, #226432 ) ;
#164701 = CARTESIAN_POINT ( 'NONE',  ( -23.25000000000000000, 67.74990736105834799, -227.9721689390126755 ) ) ;
#164702 = AXIS2_PLACEMENT_3D ( 'NONE', #202863, #125886, #185869 ) ;
#164703 = ORIENTED_EDGE ( 'NONE', *, *, #214250, .T. ) ;
#164704 = TOROIDAL_SURFACE ( 'NONE', #206397, 0.2000000000000000111, 0.1000000000000000056 ) ;
#164706 = ORIENTED_EDGE ( 'NONE', *, *, #57890, .T. ) ;
#164705 = FACE_BOUND ( 'NONE', #129064, .T. ) ;
#164707 = VERTEX_POINT ( 'NONE', #247015 ) ;
#164708 = ADVANCED_FACE ( 'NONE', ( #91809 ), #210481, .T. ) ;
#164709 = LINE ( 'NONE', #244218, #7710 ) ;
#164710 = FACE_OUTER_BOUND ( 'NONE', #118523, .T. ) ;
#164711 = ADVANCED_FACE ( 'NONE', ( #69697 ), #4928, .T. ) ;
#164712 =( LENGTH_UNIT ( ) NAMED_UNIT ( * ) SI_UNIT ( .MILLI., .METRE. ) );
#164713 = B_SPLINE_CURVE_WITH_KNOTS ( 'NONE', 3,
 ( #43807, #223701, #102452, #119499, #163758, #243268, #123345, #202866, #45084, #4651, #60781, #3369, #24260, #25534, #241997, #161189, #787, #105006, #122061, #21680, #199028, #219863, #180752, #85455, #141612, #103740, #184588, #240723, #221139, #5931 ),
 .UNSPECIFIED., .F., .F.,
 ( 4, 2, 2, 2, 2, 2, 2, 2, 2, 2, 2, 2, 2, 2, 4 ),
 ( 3.469446951953614189E-18, 0.0003422764154113311212, 0.0006845528308226587729, 0.001026829246233986479, 0.001369105661645314076, 0.002053658492467989004, 0.002738211323290663714, 0.003080487738701998685, 0.003422764154113333221, 0.003765040569524669058, 0.004107316984936004028, 0.004449593400347338565, 0.004791869815758673101, 0.005134146231170011974, 0.005476422646581350848 ),
 .UNSPECIFIED. ) ;
#164714 = ORIENTED_EDGE ( 'NONE', *, *, #241162, .F. ) ;
#164715 = CARTESIAN_POINT ( 'NONE',  ( 21.05000000000000071, 85.00000000001232081, -160.1291383618718385 ) ) ;
#164716 = CARTESIAN_POINT ( 'NONE',  ( -20.94999999999999929, 1.835341550235569663, -45.05515129256298223 ) ) ;
#164717 = ORIENTED_EDGE ( 'NONE', *, *, #247730, .F. ) ;
#164719 = DIRECTION ( 'NONE',  ( 1.000000000000000000, 0.000000000000000000, 0.000000000000000000 ) ) ;
#164718 = AXIS2_PLACEMENT_3D ( 'NONE', #108844, #12346, #207973 ) ;
#164720 =( GEOMETRIC_REPRESENTATION_CONTEXT ( 3 ) GLOBAL_UNCERTAINTY_ASSIGNED_CONTEXT ( ( #52937 ) ) GLOBAL_UNIT_ASSIGNED_CONTEXT ( ( #226677, #166754, #247539 ) ) REPRESENTATION_CONTEXT ( 'NONE', 'WORKASPACE' ) );
#164721 = DIRECTION ( 'NONE',  ( -1.000000000000000000, 0.000000000000000000, 0.000000000000000000 ) ) ;
#164722 = DIRECTION ( 'NONE',  ( 0.000000000000000000, 1.000000000000000000, -0.000000000000000000 ) ) ;
#164723 = EDGE_CURVE ( 'NONE', #160723, #212737, #93080, .T. ) ;
#164724 = EDGE_CURVE ( 'NONE', #74170, #201487, #190935, .T. ) ;
#164725 = FACE_OUTER_BOUND ( 'NONE', #140648, .T. ) ;
#164727 = EDGE_LOOP ( 'NONE', ( #92115, #164461, #66653 ) ) ;
#164726 = CARTESIAN_POINT ( 'NONE',  ( -16.84421487269769102, 66.05000000001230376, -157.3536053620794632 ) ) ;
#164728 = EDGE_CURVE ( 'NONE', #125620, #184131, #31863, .T. ) ;
#164729 = DIRECTION ( 'NONE',  ( 1.000000000000000000, 0.000000000000000000, 0.000000000000000000 ) ) ;
#164730 = CARTESIAN_POINT ( 'NONE',  ( 20.94999999999999929, 5.500000000011153745, -188.5947339810868755 ) ) ;
#164731 = DIRECTION ( 'NONE',  ( -0.000000000000000000, -0.8660254037844377084, -0.5000000000000016653 ) ) ;
#164732 = ORIENTED_EDGE ( 'NONE', *, *, #142126, .T. ) ;
#164733 = CARTESIAN_POINT ( 'NONE',  ( -16.93970660449832621, 65.98715860837673119, -157.4708257487299363 ) ) ;
#164734 = DIRECTION ( 'NONE',  ( 0.000000000000000000, 1.000000000000000000, -6.308085367188393199E-16 ) ) ;
#164736 = CARTESIAN_POINT ( 'NONE',  ( 23.24999999999999645, 70.35000000001207354, -123.8731074845243398 ) ) ;
#164735 = DIRECTION ( 'NONE',  ( -1.000000000000000000, 0.000000000000000000, -0.000000000000000000 ) ) ;
#164737 = DIRECTION ( 'NONE',  ( 0.000000000000000000, 0.2128009952263485993, -0.9770955615653341697 ) ) ;
#164738 = FACE_OUTER_BOUND ( 'NONE', #97892, .T. ) ;
#164739 = ADVANCED_FACE ( 'NONE', ( #149238 ), #50102, .F. ) ;
#164740 = VECTOR ( 'NONE', #165641, 1000.000000000000000 ) ;
#164741 = DIRECTION ( 'NONE',  ( 0.000000000000000000, 0.9910465087640866200, -0.1335171055202867274 ) ) ;
#164742 = DIRECTION ( 'NONE',  ( 0.000000000000000000, -1.000000000000000000, -0.000000000000000000 ) ) ;
#164743 = VECTOR ( 'NONE', #143069, 1000.000000000000000 ) ;
#164744 = DIRECTION ( 'NONE',  ( 1.000000000000000000, 0.000000000000000000, 0.000000000000000000 ) ) ;
#164745 = AXIS2_PLACEMENT_3D ( 'NONE', #217991, #39416, #226676 ) ;
#164746 = ORIENTED_EDGE ( 'NONE', *, *, #23437, .T. ) ;
#164747 = AXIS2_PLACEMENT_3D ( 'NONE', #108212, #31277, #33852 ) ;
#164748 = CARTESIAN_POINT ( 'NONE',  ( -21.05000000000000071, 1.261786168576181755, -142.0864989635454947 ) ) ;
#164749 = ORIENTED_EDGE ( 'NONE', *, *, #175511, .T. ) ;
#164750 = ORIENTED_EDGE ( 'NONE', *, *, #239539, .F. ) ;
#164751 = CARTESIAN_POINT ( 'NONE',  ( -20.87155475150660777, 11.74999999999999645, -26.59558652915735522 ) ) ;
#164752 = CARTESIAN_POINT ( 'NONE',  ( 18.49999999999999645, 70.30054753569015702, -82.06538144109418909 ) ) ;
#164753 = ORIENTED_EDGE ( 'NONE', *, *, #222955, .T. ) ;
#164755 = EDGE_CURVE ( 'NONE', #165951, #147926, #129851, .T. ) ;
#164754 = ORIENTED_EDGE ( 'NONE', *, *, #243784, .T. ) ;
#164756 = FILL_AREA_STYLE ('',( #68222 ) ) ;
#164757 = EDGE_LOOP ( 'NONE', ( #235245, #24135, #96973 ) ) ;
#164758 = DIRECTION ( 'NONE',  ( 0.000000000000000000, -0.9126074666063770380, -0.4088369013363281068 ) ) ;
#164759 = VECTOR ( 'NONE', #42439, 1000.000000000000000 ) ;
#164760 = ORIENTED_EDGE ( 'NONE', *, *, #83538, .F. ) ;
#164761 =( BOUNDED_CURVE ( )  B_SPLINE_CURVE ( 3, ( #240829, #101255, #102555, #2190 ),
 .UNSPECIFIED., .F., .F. ) 
 B_SPLINE_CURVE_WITH_KNOTS ( ( 4, 4 ),
 ( 0.3000847527772375622, 0.5517402753107888413 ),
 .UNSPECIFIED. ) 
 CURVE ( )  GEOMETRIC_REPRESENTATION_ITEM ( )  RATIONAL_B_SPLINE_CURVE ( ( 1.000000000000000000, 0.9947294176030464508, 0.9947294176030464508, 1.000000000000000000 ) ) 
 REPRESENTATION_ITEM ( '' )  );
#164762 = CARTESIAN_POINT ( 'NONE',  ( 23.25000000000000000, -8.999999999988842703, -124.1060308773475924 ) ) ;
#164763 = CARTESIAN_POINT ( 'NONE',  ( -23.25000000000000000, -8.999999999988846255, -177.3939691226524076 ) ) ;
#164764 = DIRECTION ( 'NONE',  ( 0.000000000000000000, -0.4930308989875170078, -0.8700118002898356018 ) ) ;
#164765 = VECTOR ( 'NONE', #16755, 999.9999999999998863 ) ;
#164766 = CARTESIAN_POINT ( 'NONE',  ( -16.85312964099708921, 29.97125116805203859, -234.7224086421056199 ) ) ;
#164767 = CARTESIAN_POINT ( 'NONE',  ( 18.39999999999999858, -9.599999999988845900, -73.60018939122203108 ) ) ;
#164768 = EDGE_CURVE ( 'NONE', #182942, #147024, #188130, .T. ) ;
#164769 = CARTESIAN_POINT ( 'NONE',  ( 21.87500000000000355, 9.750000000011153745, -112.8500000000000369 ) ) ;
#164770 = CARTESIAN_POINT ( 'NONE',  ( 20.94999999999999929, 19.92792862942048870, -235.1286901285539841 ) ) ;
#164772 = ORIENTED_EDGE ( 'NONE', *, *, #100688, .F. ) ;
#164771 = AXIS2_PLACEMENT_3D ( 'NONE', #219366, #82402, #64161 ) ;
#164773 = CARTESIAN_POINT ( 'NONE',  ( -20.54999999999999716, -8.730841121484173684, -43.09807471898433562 ) ) ;
#164774 = DIRECTION ( 'NONE',  ( 0.000000000000000000, -7.116814260417660624E-15, 1.000000000000000000 ) ) ;
#164775 = ORIENTED_EDGE ( 'NONE', *, *, #244267, .T. ) ;
#164776 = DIRECTION ( 'NONE',  ( 0.000000000000000000, 0.000000000000000000, -1.000000000000000000 ) ) ;
#164777 = CYLINDRICAL_SURFACE ( 'NONE', #23109, 0.5000000000000004441 ) ;
#164779 = EDGE_CURVE ( 'NONE', #99810, #211247, #209180, .T. ) ;
#164778 = CARTESIAN_POINT ( 'NONE',  ( 18.59999999999999076, 10.20857864376269575, -21.35000000000000142 ) ) ;
#164781 = ORIENTED_EDGE ( 'NONE', *, *, #239815, .T. ) ;
#164780 = AXIS2_PLACEMENT_3D ( 'NONE', #3005, #90243, #91553 ) ;
#164783 = CARTESIAN_POINT ( 'NONE',  ( 21.53752568622133623, 75.90102553874103819, -76.30991535907283208 ) ) ;
#164782 = FACE_OUTER_BOUND ( 'NONE', #233928, .T. ) ;
#164784 = DIRECTION ( 'NONE',  ( 0.000000000000000000, 0.8814952561688436106, -0.4721928772777334027 ) ) ;
#164785 = ORIENTED_EDGE ( 'NONE', *, *, #70932, .T. ) ;
#164786 = ADVANCED_FACE ( 'NONE', ( #189635 ), #173566, .F. ) ;
#164787 =( NAMED_UNIT ( * ) PLANE_ANGLE_UNIT ( ) SI_UNIT ( $, .RADIAN. ) );
#164789 = EDGE_CURVE ( 'NONE', #223504, #170630, #144899, .T. ) ;
#164788 = DIRECTION ( 'NONE',  ( -1.000000000000000000, 0.000000000000000000, -0.000000000000000000 ) ) ;
#164790 = CIRCLE ( 'NONE', #119014, 0.09999999999999939493 ) ;
#164791 = CARTESIAN_POINT ( 'NONE',  ( -22.39999999999999858, 1.115137594488420878E-11, -21.74956710754139522 ) ) ;
#164792 = CARTESIAN_POINT ( 'NONE',  ( -20.94999999999999929, 1.162701749949165642, -175.3999999999999773 ) ) ;
#164793 = ORIENTED_EDGE ( 'NONE', *, *, #16092, .F. ) ;
#164794 = VECTOR ( 'NONE', #75695, 1000.000000000000000 ) ;
#164795 = CIRCLE ( 'NONE', #202397, 0.09999999999999939493 ) ;
#164796 = ORIENTED_EDGE ( 'NONE', *, *, #5191, .T. ) ;
#164797 = CARTESIAN_POINT ( 'NONE',  ( -16.93388492042257454, 66.01145817749663536, -182.6225623613382538 ) ) ;
#164798 = CARTESIAN_POINT ( 'NONE',  ( -20.64999999999999858, 9.690755012883057518, -211.4266134137857023 ) ) ;
#164799 = EDGE_CURVE ( 'NONE', #86933, #213725, #107066, .T. ) ;
#164800 = CARTESIAN_POINT ( 'NONE',  ( -23.15000000000000213, 11.60000000001115517, -160.5717967697245285 ) ) ;
#164801 = CARTESIAN_POINT ( 'NONE',  ( 20.94999999999999929, 76.00000000001237765, -170.0231074845243597 ) ) ;
#164802 = CARTESIAN_POINT ( 'NONE',  ( 21.14250536705908345, 6.518172176891879666, -167.4999999999999716 ) ) ;
#164804 = EDGE_CURVE ( 'NONE', #230504, #994, #84024, .T. ) ;
#164803 = FACE_OUTER_BOUND ( 'NONE', #474, .T. ) ;
#164805 = VERTEX_POINT ( 'NONE', #64101 ) ;
#164806 = LINE ( 'NONE', #26592, #136818 ) ;
#164808 = ORIENTED_EDGE ( 'NONE', *, *, #242378, .T. ) ;
#164807 = FACE_OUTER_BOUND ( 'NONE', #131769, .T. ) ;
#164809 = DIRECTION ( 'NONE',  ( 0.000000000000000000, 0.000000000000000000, -1.000000000000000000 ) ) ;
#164810 = CARTESIAN_POINT ( 'NONE',  ( -16.77308656112214535, 66.05000000001189164, -90.37291429282207389 ) ) ;
#164811 = DIRECTION ( 'NONE',  ( 0.000000000000000000, 0.000000000000000000, -1.000000000000000000 ) ) ;
#164812 = CARTESIAN_POINT ( 'NONE',  ( 23.14999999999999858, 76.00000000001190870, -103.0231074845243029 ) ) ;
#164813 = EDGE_CURVE ( 'NONE', #180362, #199601, #233918, .T. ) ;
#164814 = CARTESIAN_POINT ( 'NONE',  ( 21.14999999999999858, 76.00000000001260503, -191.3731074845243540 ) ) ;
#164816 = EDGE_LOOP ( 'NONE', ( #170439, #23613, #233521, #215455 ) ) ;
#164815 = DIRECTION ( 'NONE',  ( -1.000000000000000000, -0.000000000000000000, -0.000000000000000000 ) ) ;
#164817 = DIRECTION ( 'NONE',  ( 1.000000000000000000, 0.000000000000000000, 0.000000000000000000 ) ) ;
#164818 = CARTESIAN_POINT ( 'NONE',  ( 21.05000000000000071, 10.72371710471867701, -179.6611902941274082 ) ) ;
#164819 = CARTESIAN_POINT ( 'NONE',  ( 18.39999999999997371, 11.47316190337362940, -191.7499999999999716 ) ) ;
#164820 = CARTESIAN_POINT ( 'NONE',  ( 21.14999999999999858, 6.540656951712400691, -33.50000000000000000 ) ) ;
#164821 =( BOUNDED_SURFACE ( )  B_SPLINE_SURFACE ( 3, 2, ( 
 ( #122563, #145946, #23482 ),
 ( #241226, #24762, #162977 ),
 ( #165538, #224200, #205927 ),
 ( #144661, #203373, #204631 ),
 ( #7742, #66425, #87247 ),
 ( #187675, #166843, #246346 ) ),
 .UNSPECIFIED., .F., .F., .T. ) 
 B_SPLINE_SURFACE_WITH_KNOTS ( ( 4, 2, 4 ),
 ( 3, 3 ),
 ( 0.0001300404313046571046, 0.0003183318589266508720, 0.0005066232865486446123 ),
 ( 0.000000000000000000, 1.000000000000000000 ),
 .UNSPECIFIED. ) 
 GEOMETRIC_REPRESENTATION_ITEM ( )  RATIONAL_B_SPLINE_SURFACE ( (
 ( 1.000000000000000000, 0.7071067811865597852, 1.000000000000000000),
 ( 1.000000000000000000, 0.7625113560538043789, 1.000000000000000000),
 ( 1.000000000000000000, 0.8126073484691690441, 1.000000000000000000),
 ( 1.000000000000000000, 0.8923049332729230398, 1.000000000000000000),
 ( 1.000000000000000000, 0.9231914937772274232, 1.000000000000000000),
 ( 1.000000000000000000, 0.9238795325112714174, 1.000000000000000000) ) ) 
 REPRESENTATION_ITEM ( '' )  SURFACE ( )  );
#164822 = ORIENTED_EDGE ( 'NONE', *, *, #113093, .T. ) ;
#164823 = DIRECTION ( 'NONE',  ( -1.000000000000000000, -3.265361837132813093E-16, 0.000000000000000000 ) ) ;
#164824 = AXIS2_PLACEMENT_3D ( 'NONE', #105541, #62612, #3916 ) ;
#164825 = CARTESIAN_POINT ( 'NONE',  ( -16.85697194749126027, 66.09145628588836985, -115.9581117521381657 ) ) ;
#164826 = EDGE_CURVE ( 'NONE', #50561, #64218, #208971, .T. ) ;
#164828 = AXIS2_PLACEMENT_3D ( 'NONE', #76102, #159514, #139912 ) ;
#164827 = DIRECTION ( 'NONE',  ( 1.000000000000000000, 0.000000000000000000, 0.000000000000000000 ) ) ;
#164829 = AXIS2_PLACEMENT_3D ( 'NONE', #206933, #127398, #186087 ) ;
#164830 = ADVANCED_FACE ( 'NONE', ( #186628 ), #26267, .T. ) ;
#164831 = FACE_OUTER_BOUND ( 'NONE', #153732, .T. ) ;
#164832 = EDGE_LOOP ( 'NONE', ( #73813, #124372, #90588, #160837 ) ) ;
#164833 = CARTESIAN_POINT ( 'NONE',  ( -16.89935556175728948, 9.950000000011137047, -87.36032363711532867 ) ) ;
#164834 = ORIENTED_EDGE ( 'NONE', *, *, #144665, .F. ) ;
#164835 = AXIS2_PLACEMENT_3D ( 'NONE', #170781, #228144, #88598 ) ;
#164836 = CARTESIAN_POINT ( 'NONE',  ( 22.14074124539698829, 60.07292514105704129, -234.0163508767828660 ) ) ;
#164837 = DIRECTION ( 'NONE',  ( 1.000000000000000000, 0.000000000000000000, 0.000000000000000000 ) ) ;
#164838 = SURFACE_SIDE_STYLE ('',( #241794 ) ) ;
#164839 = DIRECTION ( 'NONE',  ( 1.000000000000000000, -3.265361837132813093E-16, -2.280189983783949500E-30 ) ) ;
#164840 = ORIENTED_EDGE ( 'NONE', *, *, #145094, .F. ) ;
#164841 = EDGE_CURVE ( 'NONE', #12431, #222371, #125762, .T. ) ;
#164842 = VECTOR ( 'NONE', #15920, 1000.000000000000000 ) ;
#164843 = EDGE_CURVE ( 'NONE', #11451, #193738, #9067, .T. ) ;
#164844 = AXIS2_PLACEMENT_3D ( 'NONE', #63389, #24302, #202912 ) ;
#164845 = AXIS2_PLACEMENT_3D ( 'NONE', #24019, #174464, #135264 ) ;
#164846 = CARTESIAN_POINT ( 'NONE',  ( 21.05000000000000071, 13.06921230367881037, -210.6153319958218617 ) ) ;
#164847 = DIRECTION ( 'NONE',  ( 0.000000000000000000, 0.2128009952263485993, -0.9770955615653341697 ) ) ;
#164848 = CYLINDRICAL_SURFACE ( 'NONE', #28118, 11.80000000000000959 ) ;
#164849 = DIRECTION ( 'NONE',  ( 3.469446951953498700E-14, -0.7899159663865300551, -0.6132151058540831201 ) ) ;
#164850 = ORIENTED_EDGE ( 'NONE', *, *, #121678, .T. ) ;
#164852 = ORIENTED_EDGE ( 'NONE', *, *, #89182, .T. ) ;
#164851 = CARTESIAN_POINT ( 'NONE',  ( 20.90851465518106167, 10.32532329027886320, -106.0699343018359997 ) ) ;
#164853 = ORIENTED_EDGE ( 'NONE', *, *, #144022, .T. ) ;
#164854 = DIRECTION ( 'NONE',  ( 1.000000000000000000, 0.000000000000000000, 0.000000000000000000 ) ) ;
#164855 = VERTEX_POINT ( 'NONE', #28875 ) ;
#164856 = CARTESIAN_POINT ( 'NONE',  ( -18.59999999999999787, -9.749999999999994671, 30.09999999999999076 ) ) ;
#164857 = DIRECTION ( 'NONE',  ( 1.000000000000000000, 0.000000000000000000, 0.000000000000000000 ) ) ;
#164858 = DIRECTION ( 'NONE',  ( 0.000000000000000000, 0.000000000000000000, 1.000000000000000000 ) ) ;
#164860 = ORIENTED_EDGE ( 'NONE', *, *, #79647, .T. ) ;
#164859 = AXIS2_PLACEMENT_3D ( 'NONE', #199303, #23251, #220149 ) ;
#164861 = CARTESIAN_POINT ( 'NONE',  ( 23.15000000000000213, 87.65000000001275282, -215.2731074845242745 ) ) ;
#164862 = PLANE ( 'NONE',  #55431 ) ;
#164863 = CARTESIAN_POINT ( 'NONE',  ( 20.84451136049629838, 10.62014191481791059, -40.99392455952863656 ) ) ;
#164864 = ORIENTED_EDGE ( 'NONE', *, *, #188753, .T. ) ;
#164866 = ORIENTED_EDGE ( 'NONE', *, *, #89303, .F. ) ;
#164865 = DIRECTION ( 'NONE',  ( 1.186688945009009831E-16, 1.000000000000000000, 6.982962677686266711E-15 ) ) ;
#164867 = PLANE ( 'NONE',  #102487 ) ;
#164868 = AXIS2_PLACEMENT_3D ( 'NONE', #234664, #55994, #30073 ) ;
#164869 = AXIS2_PLACEMENT_3D ( 'NONE', #212208, #173116, #252587 ) ;
#164870 = EDGE_CURVE ( 'NONE', #32118, #96541, #167306, .T. ) ;
#164871 = AXIS2_PLACEMENT_3D ( 'NONE', #35661, #194724, #76031 ) ;
#164872 = VECTOR ( 'NONE', #97667, 1000.000000000000000 ) ;
#164873 = ORIENTED_EDGE ( 'NONE', *, *, #9682, .F. ) ;
#164874 = CARTESIAN_POINT ( 'NONE',  ( -21.14999999999999858, 87.75000000001267608, -203.5231074845243029 ) ) ;
#164875 = CARTESIAN_POINT ( 'NONE',  ( 21.05933563467872105, 10.72452471209247626, -79.19364774895599624 ) ) ;
#164876 = DIRECTION ( 'NONE',  ( -1.000000000000000000, 0.000000000000000000, 0.000000000000000000 ) ) ;
#164877 = ORIENTED_EDGE ( 'NONE', *, *, #237068, .T. ) ;
#164878 = CARTESIAN_POINT ( 'NONE',  ( 20.94999999999999574, 62.00000000001210054, -131.0960149541418502 ) ) ;
#164879 = DIRECTION ( 'NONE',  ( 0.000000000000000000, -1.000000000000000000, 0.000000000000000000 ) ) ;
#164880 = ORIENTED_EDGE ( 'NONE', *, *, #251111, .T. ) ;
#164881 = AXIS2_PLACEMENT_3D ( 'NONE', #43212, #186587, #203566 ) ;
#164882 = ADVANCED_FACE ( 'NONE', ( #67949 ), #23724, .T. ) ;
#164883 = AXIS2_PLACEMENT_3D ( 'NONE', #130730, #167319, #188145 ) ;
#164884 = ORIENTED_EDGE ( 'NONE', *, *, #236932, .T. ) ;
#164885 = CARTESIAN_POINT ( 'NONE',  ( 22.39999999999999503, 0.1000000000111554016, -94.25000000000002842 ) ) ;
#164886 = VECTOR ( 'NONE', #46187, 1000.000000000000000 ) ;
#164887 = ORIENTED_EDGE ( 'NONE', *, *, #19330, .T. ) ;
#164888 = FACE_OUTER_BOUND ( 'NONE', #142482, .T. ) ;
#164889 = LINE ( 'NONE', #108762, #121308 ) ;
#164891 = ORIENTED_EDGE ( 'NONE', *, *, #120961, .T. ) ;
#164890 = DIRECTION ( 'NONE',  ( 1.000000000000000000, 7.304098846218134667E-16, -0.000000000000000000 ) ) ;
#164892 = DIRECTION ( 'NONE',  ( -1.000000000000000000, -0.000000000000000000, 0.000000000000000000 ) ) ;
#164893 = CARTESIAN_POINT ( 'NONE',  ( -21.55000000000000071, 68.75000000001185185, -90.67310748452436542 ) ) ;
#164894 = LINE ( 'NONE', #167485, #135106 ) ;
#164895 = CARTESIAN_POINT ( 'NONE',  ( -23.25000000000000000, 4.350000000011156054, -88.15000000000004832 ) ) ;
#164896 = CARTESIAN_POINT ( 'NONE',  ( -23.15000000000000213, 11.65000000001115588, -93.48519422934610645 ) ) ;
#164897 = CARTESIAN_POINT ( 'NONE',  ( -18.46856557590793457, 85.47421590779860878, -129.4211212436419487 ) ) ;
#164898 = DIRECTION ( 'NONE',  ( 0.000000000000000000, 7.162729191130010591E-15, -1.000000000000000000 ) ) ;
#164899 = CARTESIAN_POINT ( 'NONE',  ( -18.41799967126731730, -9.499999999988851584, -107.5320698132558306 ) ) ;
#164901 = EDGE_LOOP ( 'NONE', ( #106996, #252673, #242781, #84047 ) ) ;
#164900 = DIRECTION ( 'NONE',  ( -7.304098846218201720E-16, 1.000000000000000000, 0.000000000000000000 ) ) ;
#164902 = FACE_OUTER_BOUND ( 'NONE', #46993, .T. ) ;
#164903 = ORIENTED_EDGE ( 'NONE', *, *, #176330, .F. ) ;
#164904 = CARTESIAN_POINT ( 'NONE',  ( 21.08489834409762054, 65.37767610527633622, -90.67310748452440805 ) ) ;
#164905 = TOROIDAL_SURFACE ( 'NONE', #44095, 0.2000000000000000111, 0.1000000000000000056 ) ;
#164906 = FACE_OUTER_BOUND ( 'NONE', #235768, .T. ) ;
#164907 = CARTESIAN_POINT ( 'NONE',  ( 22.49806830649814060, 11.64988965485023620, -66.92253568367453909 ) ) ;
#164908 = CARTESIAN_POINT ( 'NONE',  ( 20.54374330479327426, 65.49498968578961922, -195.7974238496363455 ) ) ;
#164909 = LINE ( 'NONE', #979, #163828 ) ;
#164910 = ORIENTED_EDGE ( 'NONE', *, *, #186226, .F. ) ;
#164911 = DIRECTION ( 'NONE',  ( 0.000000000000000000, 0.2617529984164506107, 0.9651348961777299618 ) ) ;
#164912 = CARTESIAN_POINT ( 'NONE',  ( -21.05000000000000071, 6.400000000011158541, -177.4304246300615375 ) ) ;
#164913 = EDGE_CURVE ( 'NONE', #77760, #75529, #221859, .T. ) ;
#164914 = AXIS2_PLACEMENT_3D ( 'NONE', #182179, #163898, #46492 ) ;
#164915 = CIRCLE ( 'NONE', #39496, 1.749999999999998002 ) ;
#164916 = ORIENTED_EDGE ( 'NONE', *, *, #50824, .F. ) ;
#164917 = CIRCLE ( 'NONE', #73381, 0.1000000000000028644 ) ;
#164918 = CARTESIAN_POINT ( 'NONE',  ( 21.11825140030062897, 75.99279637937966925, -209.9685150499435906 ) ) ;
#164919 = DIRECTION ( 'NONE',  ( 0.000000000000000000, -0.4930308989874980785, -0.8700118002898462599 ) ) ;
#164920 =( GEOMETRIC_REPRESENTATION_CONTEXT ( 3 ) GLOBAL_UNCERTAINTY_ASSIGNED_CONTEXT ( ( #157535 ) ) GLOBAL_UNIT_ASSIGNED_CONTEXT ( ( #111505, #228888, #171508 ) ) REPRESENTATION_CONTEXT ( 'NONE', 'WORKASPACE' ) );
#164921 = ADVANCED_FACE ( 'NONE', ( #225711 ), #113356, .T. ) ;
#164922 = ORIENTED_EDGE ( 'NONE', *, *, #27489, .T. ) ;
#164923 = DIRECTION ( 'NONE',  ( 0.000000000000000000, -0.2128009952263604232, 0.9770955615653316162 ) ) ;
#164924 = ORIENTED_EDGE ( 'NONE', *, *, #123903, .F. ) ;
#164925 = CARTESIAN_POINT ( 'NONE',  ( 18.59999999999999432, 70.30054753569086756, -182.5653814410942459 ) ) ;
#164926 = ORIENTED_EDGE ( 'NONE', *, *, #199696, .T. ) ;
#164927 = ADVANCED_FACE ( 'NONE', ( #11854 ), #13352, .T. ) ;
#164928 = CARTESIAN_POINT ( 'NONE',  ( 15.70340296795548163, 9.355888454513701546, -183.7886428967779864 ) ) ;
#164929 = ORIENTED_EDGE ( 'NONE', *, *, #193481, .T. ) ;
#164930 = CARTESIAN_POINT ( 'NONE',  ( 20.94999999999999574, 65.52661458509942349, -162.4444530202758870 ) ) ;
#164931 = EDGE_CURVE ( 'NONE', #152772, #55017, #254717, .T. ) ;
#164933 = ORIENTED_EDGE ( 'NONE', *, *, #43001, .F. ) ;
#164932 = CARTESIAN_POINT ( 'NONE',  ( 12.47034474403012716, 9.375538102059159939, -49.36987588099082558 ) ) ;
#164934 = CARTESIAN_POINT ( 'NONE',  ( -22.45437739390952814, 76.00000000001276135, -215.1726782961185620 ) ) ;
#164936 = ORIENTED_EDGE ( 'NONE', *, *, #213074, .T. ) ;
#164935 = VECTOR ( 'NONE', #153146, 1000.000000000000000 ) ;
#164937 = CIRCLE ( 'NONE', #169073, 0.1000000000000028644 ) ;
#164938 = ORIENTED_EDGE ( 'NONE', *, *, #250642, .F. ) ;
#164939 = CIRCLE ( 'NONE', #27619, 0.09999999999999939493 ) ;
#164940 = DIRECTION ( 'NONE',  ( 1.000000000000000000, 0.000000000000000000, 0.000000000000000000 ) ) ;
#164941 = ADVANCED_FACE ( 'NONE', ( #70553 ), #242278, .F. ) ;
#164942 = CARTESIAN_POINT ( 'NONE',  ( 0.9000000000000547562, 67.75000000001118394, -10.02310748452479139 ) ) ;
#164943 = FACE_OUTER_BOUND ( 'NONE', #195734, .T. ) ;
#164944 = AXIS2_PLACEMENT_3D ( 'NONE', #192798, #134083, #32470 ) ;
#164945 = DIRECTION ( 'NONE',  ( -1.000000000000000000, 0.000000000000000000, 0.000000000000000000 ) ) ;
#164946 = AXIS2_PLACEMENT_3D ( 'NONE', #80297, #215038, #93799 ) ;
#164947 = CYLINDRICAL_SURFACE ( 'NONE', #252081, 4.049999999999998046 ) ;
#164948 = CARTESIAN_POINT ( 'NONE',  ( 21.05000000000000071, 76.00000000001142553, -36.02310748452432421 ) ) ;
#164949 = ORIENTED_EDGE ( 'NONE', *, *, #208596, .F. ) ;
#164950 = CARTESIAN_POINT ( 'NONE',  ( -16.93301857435208291, 66.02369064527707110, -182.6373319133629423 ) ) ;
#164951 = CARTESIAN_POINT ( 'NONE',  ( 23.14999999999999858, 0.000000000000000000, -12.87500000000000178 ) ) ;
#164952 = DIRECTION ( 'NONE',  ( 0.000000000000000000, 0.4088369013363281623, -0.9126074666063771490 ) ) ;
#164953 = CYLINDRICAL_SURFACE ( 'NONE', #42767, 0.1000000000000055844 ) ;
#164954 = ORIENTED_EDGE ( 'NONE', *, *, #221902, .F. ) ;
#164955 = CARTESIAN_POINT ( 'NONE',  ( 20.89878130938411616, 68.09900309800710261, -224.1499508721967970 ) ) ;
#164956 = ORIENTED_EDGE ( 'NONE', *, *, #153470, .F. ) ;
#164957 = CARTESIAN_POINT ( 'NONE',  ( -20.54999999999999361, 64.35000000001222986, -148.6731074845244507 ) ) ;
#164958 = ORIENTED_EDGE ( 'NONE', *, *, #206618, .F. ) ;
#164959 = TOROIDAL_SURFACE ( 'NONE', #110788, 0.2000000000000000111, 0.1000000000000000056 ) ;
#164960 = AXIS2_PLACEMENT_3D ( 'NONE', #71106, #172801, #208050 ) ;
#164961 = AXIS2_PLACEMENT_3D ( 'NONE', #199141, #239554, #204256 ) ;
#164962 = CARTESIAN_POINT ( 'NONE',  ( 21.05000000000000071, -11.64999999998883595, -97.40000000000004832 ) ) ;
#164963 = CARTESIAN_POINT ( 'NONE',  ( -20.94999999999999929, -1.835341550224411922, -11.55515129256298046 ) ) ;
#164964 = ORIENTED_EDGE ( 'NONE', *, *, #180357, .T. ) ;
#164965 = VERTEX_POINT ( 'NONE', #69251 ) ;
#164967 = ORIENTED_EDGE ( 'NONE', *, *, #63063, .F. ) ;
#164966 = LINE ( 'NONE', #104952, #86348 ) ;
#164968 = DIRECTION ( 'NONE',  ( 0.000000000000000000, -0.4088369013363280513, 0.9126074666063769270 ) ) ;
#164969 = VERTEX_POINT ( 'NONE', #150079 ) ;
#164970 = CIRCLE ( 'NONE', #15136, 6.329289321881370611 ) ;
#164971 = DIRECTION ( 'NONE',  ( 2.694716079187274425E-16, 0.4088369013363281623, -0.9126074666063770380 ) ) ;
#164972 = DIRECTION ( 'NONE',  ( 0.000000000000000000, 0.000000000000000000, -1.000000000000000000 ) ) ;
#164973 = ORIENTED_EDGE ( 'NONE', *, *, #39666, .T. ) ;
#164974 = DIRECTION ( 'NONE',  ( 0.000000000000000000, 0.2617529984165031243, 0.9651348961777157509 ) ) ;
#164975 = AXIS2_PLACEMENT_3D ( 'NONE', #1398, #240039, #13941 ) ;
#164976 = CARTESIAN_POINT ( 'NONE',  ( 23.24999999999999289, 21.15538238767524604, -233.7023398932965108 ) ) ;
#164977 = EDGE_LOOP ( 'NONE', ( #220494, #193312, #131463, #106131 ) ) ;
#164978 = EDGE_CURVE ( 'NONE', #12568, #40580, #109002, .T. ) ;
#164979 = LINE ( 'NONE', #127139, #63990 ) ;
#164980 = EDGE_CURVE ( 'NONE', #220391, #44347, #46634, .T. ) ;
#164981 = DIRECTION ( 'NONE',  ( 0.000000000000000000, 0.000000000000000000, 1.000000000000000000 ) ) ;
#164983 = ORIENTED_EDGE ( 'NONE', *, *, #196914, .F. ) ;
#164982 = CARTESIAN_POINT ( 'NONE',  ( -23.49999999999994316, 78.47315729244128590, -52.27034697567518862 ) ) ;
#164984 = TOROIDAL_SURFACE ( 'NONE', #60729, 0.2000000000000000111, 0.1000000000000000056 ) ;
#164985 = DIRECTION ( 'NONE',  ( 1.000000000000000000, -0.000000000000000000, -0.000000000000000000 ) ) ;
#164986 = CARTESIAN_POINT ( 'NONE',  ( -18.50000000000000000, 11.65000000001115232, -100.6000000000000369 ) ) ;
#164987 = CIRCLE ( 'NONE', #127588, 2.100000000000004530 ) ;
#164988 = DIRECTION ( 'NONE',  ( 0.7071359030028113724, 0.000000000000000000, -0.7070776581708677622 ) ) ;
#164989 = EDGE_CURVE ( 'NONE', #200341, #123360, #113494, .T. ) ;
#164990 = CYLINDRICAL_SURFACE ( 'NONE', #215177, 0.1000000000000028644 ) ;
#164993 = EDGE_CURVE ( 'NONE', #16468, #212431, #75716, .T. ) ;
#164992 = CIRCLE ( 'NONE', #102415, 0.1000000000000035444 ) ;
#164991 = CARTESIAN_POINT ( 'NONE',  ( 20.94999999999999574, 74.16465844978765176, -124.8679561919613263 ) ) ;
#164994 = CIRCLE ( 'NONE', #127403, 0.1000000000000028644 ) ;
#164995 = DIRECTION ( 'NONE',  ( 0.000000000000000000, 0.000000000000000000, 1.000000000000000000 ) ) ;
#164996 = DIRECTION ( 'NONE',  ( -1.000000000000000000, 0.000000000000000000, 0.000000000000000000 ) ) ;
#164997 = CARTESIAN_POINT ( 'NONE',  ( 20.94999999999999929, 36.65892442174935439, -249.5511627012433848 ) ) ;
#164999 = EDGE_LOOP ( 'NONE', ( #75731, #236330, #72445, #126855 ) ) ;
#164998 = VECTOR ( 'NONE', #199283, 1000.000000000000000 ) ;
#165000 = ORIENTED_EDGE ( 'NONE', *, *, #52789, .F. ) ;
#165001 = DIRECTION ( 'NONE',  ( 1.000000000000000000, -0.000000000000000000, -0.000000000000000000 ) ) ;
#165002 = ADVANCED_FACE ( 'NONE', ( #131774 ), #171592, .F. ) ;
#165003 = EDGE_LOOP ( 'NONE', ( #119617, #76371, #73211, #110650 ) ) ;
#165004 = EDGE_CURVE ( 'NONE', #171663, #42537, #151362, .T. ) ;
#165005 = FACE_OUTER_BOUND ( 'NONE', #93327, .T. ) ;
#165006 = EDGE_CURVE ( 'NONE', #165926, #113603, #200599, .T. ) ;
#165007 = AXIS2_PLACEMENT_3D ( 'NONE', #69579, #126967, #149117 ) ;
#165008 = ORIENTED_EDGE ( 'NONE', *, *, #106759, .F. ) ;
#165009 = AXIS2_PLACEMENT_3D ( 'NONE', #25001, #245314, #207481 ) ;
#165010 = FACE_OUTER_BOUND ( 'NONE', #27726, .T. ) ;
#165011 = ORIENTED_EDGE ( 'NONE', *, *, #70471, .T. ) ;
#165012 = CARTESIAN_POINT ( 'NONE',  ( 18.59999999999999787, -1.835341550213255957, -145.5551512925629822 ) ) ;
#165013 = EDGE_LOOP ( 'NONE', ( #114608, #24543, #113365, #228765 ) ) ;
#165014 = VERTEX_POINT ( 'NONE', #114782 ) ;
#165015 = EDGE_CURVE ( 'NONE', #175330, #79626, #15713, .T. ) ;
#165016 = CARTESIAN_POINT ( 'NONE',  ( -18.39999999999999858, 85.51932773110452501, -129.5501311079648872 ) ) ;
#165017 = DIRECTION ( 'NONE',  ( 0.000000000000000000, 0.000000000000000000, -1.000000000000000000 ) ) ;
#165019 = VERTEX_POINT ( 'NONE', #211319 ) ;
#165018 = CARTESIAN_POINT ( 'NONE',  ( -23.25000000000000000, 8.751106741858205140, -220.7398867978735950 ) ) ;
#165020 = EDGE_CURVE ( 'NONE', #76430, #206635, #152656, .T. ) ;
#165021 = AXIS2_PLACEMENT_3D ( 'NONE', #226206, #127150, #227523 ) ;
#165022 = EDGE_CURVE ( 'NONE', #26818, #98813, #251723, .T. ) ;
#165023 = CARTESIAN_POINT ( 'NONE',  ( 19.75857864376269291, 11.65000000001116476, -158.7500000000000284 ) ) ;
#165025 = EDGE_LOOP ( 'NONE', ( #218151, #81922, #255616, #101503 ) ) ;
#165024 = DIRECTION ( 'NONE',  ( 0.000000000000000000, 0.000000000000000000, 1.000000000000000000 ) ) ;
#165026 = DIRECTION ( 'NONE',  ( 1.000000000000000000, 7.304098846218134667E-16, 0.000000000000000000 ) ) ;
#165027 = EDGE_CURVE ( 'NONE', #105902, #41142, #31432, .T. ) ;
#165028 = DIRECTION ( 'NONE',  ( 1.000000000000000000, 0.000000000000000000, 0.000000000000000000 ) ) ;
#165030 = EDGE_LOOP ( 'NONE', ( #199824, #4116, #195830, #177404 ) ) ;
#165029 = CARTESIAN_POINT ( 'NONE',  ( -23.25000000000000000, -2.576749817950531707, -189.6385361693310756 ) ) ;
#165031 = DIRECTION ( 'NONE',  ( -1.000000000000000000, -0.000000000000000000, -0.000000000000000000 ) ) ;
#165032 = DIRECTION ( 'NONE',  ( 0.000000000000000000, 0.000000000000000000, 1.000000000000000000 ) ) ;
#165033 = CARTESIAN_POINT ( 'NONE',  ( 23.14999999999999858, 79.90000000001171543, -69.52310748452428868 ) ) ;
#165035 = CYLINDRICAL_SURFACE ( 'NONE', #228968, 0.1000000000000026007 ) ;
#165034 = DIRECTION ( 'NONE',  ( 1.000000000000000000, 0.000000000000000000, 0.000000000000000000 ) ) ;
#165036 = CARTESIAN_POINT ( 'NONE',  ( -23.25000000000000000, 4.350000000011156054, -121.6500000000000341 ) ) ;
#165037 = CARTESIAN_POINT ( 'NONE',  ( 18.60000000000000142, 85.48068669529135377, -163.0819923157664562 ) ) ;
#165038 = CIRCLE ( 'NONE', #27710, 0.1000000000000028644 ) ;
#165039 = TOROIDAL_SURFACE ( 'NONE', #181793, 2.100000000000002309, 0.1000000000000000056 ) ;
#165040 = CARTESIAN_POINT ( 'NONE',  ( -20.64999999999999858, 4.250000000011156409, -188.6499999999999488 ) ) ;
#165041 = CIRCLE ( 'NONE', #131735, 12.97500000000001208 ) ;
#165043 = FACE_OUTER_BOUND ( 'NONE', #189205, .T. ) ;
#165042 = AXIS2_PLACEMENT_3D ( 'NONE', #72715, #15298, #94808 ) ;
#165044 = ORIENTED_EDGE ( 'NONE', *, *, #88853, .F. ) ;
#165045 = ORIENTED_EDGE ( 'NONE', *, *, #131979, .T. ) ;
#165046 = ORIENTED_EDGE ( 'NONE', *, *, #151014, .F. ) ;
#165047 = CARTESIAN_POINT ( 'NONE',  ( -21.05000000000000071, 86.27712145182582049, -209.5223386573213702 ) ) ;
#165049 = EDGE_LOOP ( 'NONE', ( #69426, #105323, #215516, #149210 ) ) ;
#165048 = EDGE_CURVE ( 'NONE', #102370, #207654, #252998, .T. ) ;
#165050 = DIRECTION ( 'NONE',  ( 0.000000000000000000, -1.000000000000000000, 0.000000000000000000 ) ) ;
#165051 = ORIENTED_EDGE ( 'NONE', *, *, #52191, .F. ) ;
#165052 = EDGE_CURVE ( 'NONE', #130647, #17019, #192589, .T. ) ;
#165053 = CARTESIAN_POINT ( 'NONE',  ( -17.29838795458563183, 14.83790627693142383, -220.3913684649999709 ) ) ;
#165055 = EDGE_CURVE ( 'NONE', #52860, #154991, #54790, .T. ) ;
#165054 = VERTEX_POINT ( 'NONE', #170957 ) ;
#165056 = CIRCLE ( 'NONE', #85718, 11.74999999999999645 ) ;
#165057 = CARTESIAN_POINT ( 'NONE',  ( 20.94999999999999574, -1.349084418627015447, -7.986498963545480834 ) ) ;
#165058 = PRESENTATION_STYLE_ASSIGNMENT (( #5959 ) ) ;
#165059 = AXIS2_PLACEMENT_3D ( 'NONE', #168328, #190433, #247815 ) ;
#165060 = ORIENTED_EDGE ( 'NONE', *, *, #22759, .T. ) ;
#165061 = ORIENTED_EDGE ( 'NONE', *, *, #107189, .F. ) ;
#165062 = ORIENTED_EDGE ( 'NONE', *, *, #128820, .F. ) ;
#165063 = CARTESIAN_POINT ( 'NONE',  ( -18.50000000000000000, 74.83729825007431202, -161.9231074845243654 ) ) ;
#165064 = DIRECTION ( 'NONE',  ( -3.265361837132813093E-16, 1.000000000000000000, 0.000000000000000000 ) ) ;
#165065 = VECTOR ( 'NONE', #113874, 1000.000000000000000 ) ;
#165066 = LINE ( 'NONE', #82926, #26028 ) ;
#165067 = DIRECTION ( 'NONE',  ( 0.000000000000000000, 0.8814952561688437216, -0.4721928772777334582 ) ) ;
#165068 = DIRECTION ( 'NONE',  ( 0.000000000000000000, 0.9889818879709272315, 0.1480365673253073999 ) ) ;
#165069 = CARTESIAN_POINT ( 'NONE',  ( 21.05000000000000071, -1.360870587180885716, -175.5729979270909382 ) ) ;
#165071 = DIRECTION ( 'NONE',  ( 0.7071067811865474617, 0.7071067811865474617, 0.000000000000000000 ) ) ;
#165070 = DIRECTION ( 'NONE',  ( 1.000000000000000000, 0.000000000000000000, 0.000000000000000000 ) ) ;
#165073 = ORIENTED_EDGE ( 'NONE', *, *, #217690, .F. ) ;
#165072 = DIRECTION ( 'NONE',  ( 0.000000000000000000, 0.000000000000000000, -1.000000000000000000 ) ) ;
#165075 = CARTESIAN_POINT ( 'NONE',  ( 21.08035267497491105, 69.66829316022892726, -103.1057961093004849 ) ) ;
#165074 = DIRECTION ( 'NONE',  ( 0.000000000000000000, 0.000000000000000000, -1.000000000000000000 ) ) ;
#165076 = CARTESIAN_POINT ( 'NONE',  ( -21.05000000000000071, -1.360870587180885716, -108.5729979270909951 ) ) ;
#165077 = ORIENTED_EDGE ( 'NONE', *, *, #73665, .T. ) ;
#165078 = DIRECTION ( 'NONE',  ( 1.000000000000000000, 0.000000000000000000, 0.000000000000000000 ) ) ;
#165079 = DIRECTION ( 'NONE',  ( 1.186688945009009831E-16, -1.000000000000000000, 0.000000000000000000 ) ) ;
#165081 = EDGE_CURVE ( 'NONE', #110495, #42521, #34224, .T. ) ;
#165080 = CARTESIAN_POINT ( 'NONE',  ( 19.99999999738052381, 64.25000000001148237, -44.83593553489200900 ) ) ;
#165082 = ORIENTED_EDGE ( 'NONE', *, *, #22894, .T. ) ;
#165083 = DIRECTION ( 'NONE',  ( -0.7071067811865475727, -0.7071067811865475727, -0.000000000000000000 ) ) ;
#165084 = EDGE_CURVE ( 'NONE', #187409, #13140, #157806, .T. ) ;
#165085 = CIRCLE ( 'NONE', #85946, 0.09999999999999939493 ) ;
#165086 = CARTESIAN_POINT ( 'NONE',  ( -15.55912972643741199, 8.490870273573719373, -79.55000000000005400 ) ) ;
#165087 = CARTESIAN_POINT ( 'NONE',  ( 20.85000000000000142, 7.128833340094563376, -233.7327013124401276 ) ) ;
#165088 = ORIENTED_EDGE ( 'NONE', *, *, #156998, .T. ) ;
#165089 = ORIENTED_EDGE ( 'NONE', *, *, #80500, .F. ) ;
#165090 = EDGE_CURVE ( 'NONE', #142271, #120254, #159298, .T. ) ;
#165092 = ADVANCED_FACE ( 'NONE', ( #156515 ), #100323, .T. ) ;
#165091 = DIRECTION ( 'NONE',  ( 0.000000000000000000, 0.000000000000000000, -1.000000000000000000 ) ) ;
#165093 = VERTEX_POINT ( 'NONE', #139463 ) ;
#165094 = DIRECTION ( 'NONE',  ( 1.000000000000000000, -0.000000000000000000, -0.000000000000000000 ) ) ;
#165095 = DIRECTION ( 'NONE',  ( -2.952720810173288619E-16, 1.000000000000000000, 0.000000000000000000 ) ) ;
#165096 = CARTESIAN_POINT ( 'NONE',  ( 18.50000000000000355, 85.41907808086121179, -62.69318213431594700 ) ) ;
#165097 = DIRECTION ( 'NONE',  ( 0.000000000000000000, 0.9889818879709274535, 0.1480365673253065395 ) ) ;
#165098 = VERTEX_POINT ( 'NONE', #99039 ) ;
#165099 = EDGE_CURVE ( 'NONE', #67969, #151223, #96697, .T. ) ;
#165100 = CIRCLE ( 'NONE', #132336, 0.09999999999999939493 ) ;
#165101 = CARTESIAN_POINT ( 'NONE',  ( -14.77538296656415007, 9.436662931810239741, -118.8230367322948808 ) ) ;
#165102 = CARTESIAN_POINT ( 'NONE',  ( -20.85000000000000142, -1.164121893230052995, -108.4148480855716485 ) ) ;
#165103 = AXIS2_PLACEMENT_3D ( 'NONE', #244014, #165802, #87502 ) ;
#165104 = CARTESIAN_POINT ( 'NONE',  ( -16.77683809663752257, 9.945835743215303282, -87.83605098089584828 ) ) ;
#165105 = CARTESIAN_POINT ( 'NONE',  ( -21.14999999999999858, -11.64999999998884483, -103.4000000000000341 ) ) ;
#165106 = AXIS2_PLACEMENT_3D ( 'NONE', #188531, #205517, #67301 ) ;
#165107 = AXIS2_PLACEMENT_3D ( 'NONE', #58163, #118164, #79003 ) ;
#165108 = EDGE_CURVE ( 'NONE', #99384, #127304, #38470, .T. ) ;
#165109 = ORIENTED_EDGE ( 'NONE', *, *, #156547, .T. ) ;
#165111 = EDGE_CURVE ( 'NONE', #84718, #233154, #59267, .T. ) ;
#165110 = CARTESIAN_POINT ( 'NONE',  ( -18.59999999999999787, 2.953700692300310848, -208.6327728934509764 ) ) ;
#165113 = ORIENTED_EDGE ( 'NONE', *, *, #148533, .T. ) ;
#165112 = CARTESIAN_POINT ( 'NONE',  ( 22.50000000000000000, 68.25000000001165290, -69.62310748452438247 ) ) ;
#165114 = CARTESIAN_POINT ( 'NONE',  ( 21.00000000000000000, 61.02768354592784306, -221.4801322937404393 ) ) ;
#165115 = CARTESIAN_POINT ( 'NONE',  ( 18.48536876927954964, 78.20985190841274459, -231.5293656822601918 ) ) ;
#165116 = EDGE_CURVE ( 'NONE', #241204, #114637, #250841, .T. ) ;
#165117 = FACE_OUTER_BOUND ( 'NONE', #20728, .T. ) ;
#165118 = DIRECTION ( 'NONE',  ( 1.000000000000000000, 0.000000000000000000, 0.000000000000000000 ) ) ;
#165119 = CARTESIAN_POINT ( 'NONE',  ( -14.00000000000000178, 9.850000000011133849, -184.2499999999999716 ) ) ;
#165120 = FACE_OUTER_BOUND ( 'NONE', #47467, .T. ) ;
#165121 = ORIENTED_EDGE ( 'NONE', *, *, #49755, .F. ) ;
#165122 = LINE ( 'NONE', #166439, #80217 ) ;
#165123 = DIRECTION ( 'NONE',  ( 1.186688945009009831E-16, -0.9770955615653313941, -0.2128009952263603677 ) ) ;
#165124 = CARTESIAN_POINT ( 'NONE',  ( -14.00000000000000178, 9.849999999999978328, -16.75000000000000355 ) ) ;
#165125 = ADVANCED_FACE ( 'NONE', ( #58635 ), #150891, .T. ) ;
#165126 = CARTESIAN_POINT ( 'NONE',  ( -18.59999999999999787, 11.75000000001115197, -107.5148057706540357 ) ) ;
#165127 = VECTOR ( 'NONE', #155535, 1000.000000000000000 ) ;
#165128 = DIRECTION ( 'NONE',  ( -1.020425574104004196E-15, -0.2617529984165031243, -0.9651348961777157509 ) ) ;
#165129 = CIRCLE ( 'NONE', #23523, 0.1000000000000028644 ) ;
#165130 = ORIENTED_EDGE ( 'NONE', *, *, #193976, .T. ) ;
#165131 = ORIENTED_EDGE ( 'NONE', *, *, #125972, .T. ) ;
#165132 = LINE ( 'NONE', #47731, #42752 ) ;
#165133 = EDGE_CURVE ( 'NONE', #18074, #60562, #225696, .T. ) ;
#165134 = AXIS2_PLACEMENT_3D ( 'NONE', #30687, #230140, #51470 ) ;
#165135 = DIRECTION ( 'NONE',  ( 0.000000000000000000, -0.4088369013363281068, 0.9126074666063770380 ) ) ;
#165136 = PLANE ( 'NONE',  #149743 ) ;
#165137 = CIRCLE ( 'NONE', #152695, 12.77500000000000924 ) ;
#165138 =( BOUNDED_SURFACE ( )  B_SPLINE_SURFACE ( 3, 2, ( 
 ( #251363, #193978, #234362 ),
 ( #92287, #113143, #135253 ),
 ( #149733, #233118, #192690 ),
 ( #173168, #248817, #70196 ),
 ( #51861, #72769, #152297 ),
 ( #231824, #252637, #77851 ) ),
 .UNSPECIFIED., .F., .F., .T. ) 
 B_SPLINE_SURFACE_WITH_KNOTS ( ( 4, 2, 4 ),
 ( 3, 3 ),
 ( 1.570796326794895448, 2.356194490192343505, 3.141592653589791784 ),
 ( 0.000000000000000000, 1.000000000000000000 ),
 .UNSPECIFIED. ) 
 GEOMETRIC_REPRESENTATION_ITEM ( )  RATIONAL_B_SPLINE_SURFACE ( (
 ( 1.000000000000000000, 0.7071067811865475727, 1.000000000000000000),
 ( 1.000000000000000000, 0.6611148371775555921, 1.000000000000000000),
 ( 1.000000000000000000, 0.6092287576700941010, 1.000000000000000000),
 ( 1.000000000000000000, 0.5278258667053719044, 1.000000000000000000),
 ( 1.000000000000000000, 0.4993418825339194789, 1.000000000000000000),
 ( 1.000000000000000000, 0.5000000000000545120, 1.000000000000000000) ) ) 
 REPRESENTATION_ITEM ( '' )  SURFACE ( )  );
#165140 = EDGE_CURVE ( 'NONE', #55132, #128766, #246567, .T. ) ;
#165139 = DIRECTION ( 'NONE',  ( -1.000000000000000000, -0.000000000000000000, -0.000000000000000000 ) ) ;
#165141 = CIRCLE ( 'NONE', #73584, 0.1000000000000028644 ) ;
#165142 = AXIS2_PLACEMENT_3D ( 'NONE', #51446, #213119, #34510 ) ;
#165143 = ADVANCED_FACE ( 'NONE', ( #135613 ), #234089, .T. ) ;
#165144 = CARTESIAN_POINT ( 'NONE',  ( -20.85000000000000142, 67.49222854868494892, -195.4187676019683408 ) ) ;
#165145 = DIRECTION ( 'NONE',  ( 1.000000000000000000, 0.000000000000000000, 0.000000000000000000 ) ) ;
#165146 = LINE ( 'NONE', #163867, #224573 ) ;
#165147 = AXIS2_PLACEMENT_3D ( 'NONE', #51131, #12059, #228528 ) ;
#165148 = AXIS2_PLACEMENT_3D ( 'NONE', #140020, #40976, #120514 ) ;
#165149 = EDGE_LOOP ( 'NONE', ( #206139, #255388, #9983 ) ) ;
#165151 = DIRECTION ( 'NONE',  ( -0.000000000000000000, 0.2253241261139106999, -0.9742838591452712693 ) ) ;
#165150 = AXIS2_PLACEMENT_3D ( 'NONE', #245664, #108722, #68318 ) ;
#165152 = ORIENTED_EDGE ( 'NONE', *, *, #56690, .T. ) ;
#165153 = EDGE_CURVE ( 'NONE', #188280, #19024, #50915, .T. ) ;
#165154 = CARTESIAN_POINT ( 'NONE',  ( -21.65000000000000213, 10.16011026985487398, -211.4267369781599939 ) ) ;
#165155 = FACE_OUTER_BOUND ( 'NONE', #212767, .T. ) ;
#165156 = CARTESIAN_POINT ( 'NONE',  ( 22.59999999999999432, 0.09999999999999939493, 11.64957080754479968 ) ) ;
#165157 = CARTESIAN_POINT ( 'NONE',  ( -20.85000000000000497, 11.75000000001115019, -194.0808527540412456 ) ) ;
#165158 = CARTESIAN_POINT ( 'NONE',  ( 18.52928932188133970, 65.72071067813116940, -178.8731074845244109 ) ) ;
#165159 = CYLINDRICAL_SURFACE ( 'NONE', #222523, 0.09999999999999939493 ) ;
#165160 = FACE_OUTER_BOUND ( 'NONE', #157735, .T. ) ;
#165161 = DIRECTION ( 'NONE',  ( -1.000000000000000000, 0.000000000000000000, 0.000000000000000000 ) ) ;
#165162 = DIRECTION ( 'NONE',  ( 0.000000000000000000, 0.000000000000000000, 1.000000000000000000 ) ) ;
#165163 = AXIS2_PLACEMENT_3D ( 'NONE', #234247, #162448, #146685 ) ;
#165164 = PLANE ( 'NONE',  #118836 ) ;
#165165 = FACE_OUTER_BOUND ( 'NONE', #91701, .T. ) ;
#165166 = DIRECTION ( 'NONE',  ( -1.000000000000000000, 0.000000000000000000, 0.000000000000000000 ) ) ;
#165167 = ORIENTED_EDGE ( 'NONE', *, *, #219033, .T. ) ;
#165168 = CARTESIAN_POINT ( 'NONE',  ( 18.41416235934317669, 85.50000000001209344, -129.9229180933022860 ) ) ;
#165169 = PLANE ( 'NONE',  #204331 ) ;
#165170 = EDGE_CURVE ( 'NONE', #181858, #61516, #26009, .T. ) ;
#165171 = ORIENTED_EDGE ( 'NONE', *, *, #147124, .T. ) ;
#165172 = CARTESIAN_POINT ( 'NONE',  ( 18.39999999999999858, -9.499999999988842703, -107.1001893912220879 ) ) ;
#165173 = CARTESIAN_POINT ( 'NONE',  ( 21.13461538461538680, 11.30999384151885856, -211.1763045966511356 ) ) ;
#165174 = CIRCLE ( 'NONE', #48464, 0.9750000000000036415 ) ;
#165175 = CIRCLE ( 'NONE', #115283, 0.09999999999998898659 ) ;
#165176 = DIRECTION ( 'NONE',  ( 0.000000000000000000, 0.8700118002898321601, -0.4930308989875230030 ) ) ;
#165177 = ORIENTED_EDGE ( 'NONE', *, *, #195117, .T. ) ;
#165179 = AXIS2_PLACEMENT_3D ( 'NONE', #151611, #130728, #48620 ) ;
#165178 = CARTESIAN_POINT ( 'NONE',  ( 18.36493879433247756, -9.500000806178645618, -174.4221486603523488 ) ) ;
#165180 = DIRECTION ( 'NONE',  ( 0.000000000000000000, 0.000000000000000000, -1.000000000000000000 ) ) ;
#165181 = AXIS2_PLACEMENT_3D ( 'NONE', #182921, #222002, #122941 ) ;
#165182 = ADVANCED_FACE ( 'NONE', ( #256799 ), #16984, .F. ) ;
#165183 = VERTEX_POINT ( 'NONE', #20842 ) ;
#165184 = TOROIDAL_SURFACE ( 'NONE', #52745, 0.2000000000000000111, 0.1000000000000000056 ) ;
#165185 = LINE ( 'NONE', #126039, #22959 ) ;
#165186 = VERTEX_POINT ( 'NONE', #36568 ) ;
#165187 = FACE_OUTER_BOUND ( 'NONE', #158236, .T. ) ;
#165189 = AXIS2_PLACEMENT_3D ( 'NONE', #184284, #185574, #89033 ) ;
#165188 = CARTESIAN_POINT ( 'NONE',  ( 22.50927854361889047, -0.1008580735143522616, -21.75043287397308944 ) ) ;
#165190 = LINE ( 'NONE', #187338, #149106 ) ;
#165192 = FACE_OUTER_BOUND ( 'NONE', #28370, .T. ) ;
#165191 = UNCERTAINTY_MEASURE_WITH_UNIT (LENGTH_MEASURE( 1.000000000000000082E-05 ), #74644, 'distance_accuracy_value', 'NONE');
#165193 = FACE_OUTER_BOUND ( 'NONE', #174127, .T. ) ;
#165194 = AXIS2_PLACEMENT_3D ( 'NONE', #226901, #185213, #6570 ) ;
#165195 = CARTESIAN_POINT ( 'NONE',  ( -16.83233564386414116, 66.06977820342760310, -157.2476281480000182 ) ) ;
#165196 = FACE_OUTER_BOUND ( 'NONE', #110791, .T. ) ;
#165197 = CARTESIAN_POINT ( 'NONE',  ( 20.94999999999999574, 70.65782965956557859, -228.4198064469268559 ) ) ;
#165198 = CARTESIAN_POINT ( 'NONE',  ( 20.99999999999999645, 66.25000000001210765, -127.2731074845243597 ) ) ;
#165200 = ORIENTED_EDGE ( 'NONE', *, *, #139756, .T. ) ;
#165199 = CARTESIAN_POINT ( 'NONE',  ( 18.50000000000001776, 86.96699927712943179, -199.3055931863049466 ) ) ;
#165201 = ORIENTED_EDGE ( 'NONE', *, *, #1666, .F. ) ;
#165203 = CARTESIAN_POINT ( 'NONE',  ( 21.05000000000000071, 1.115600667400684642E-11, -135.9000000000000625 ) ) ;
#165202 = FACE_OUTER_BOUND ( 'NONE', #48911, .T. ) ;
#165205 = ORIENTED_EDGE ( 'NONE', *, *, #200492, .T. ) ;
#165204 = CARTESIAN_POINT ( 'NONE',  ( -23.15000000000000213, 26.38661631484795578, -241.7796963509253203 ) ) ;
#165206 = VERTEX_POINT ( 'NONE', #254269 ) ;
#165207 = DIRECTION ( 'NONE',  ( 1.000000000000000000, 0.000000000000000000, 0.000000000000000000 ) ) ;
#165208 = CARTESIAN_POINT ( 'NONE',  ( 20.51284917709620359, 10.31088662285602275, -175.1724731855919686 ) ) ;
#165209 = DIRECTION ( 'NONE',  ( 0.000000000000000000, 0.9770955615653313941, 0.2128009952263603677 ) ) ;
#165211 = CARTESIAN_POINT ( 'NONE',  ( -20.94999999999999929, 10.29270135741298731, -172.9573618871519614 ) ) ;
#165210 = AXIS2_PLACEMENT_3D ( 'NONE', #50164, #129715, #159561 ) ;
#165212 = CARTESIAN_POINT ( 'NONE',  ( -23.25000000000000000, -1.835859311432481045, -78.50443916879852679 ) ) ;
#165213 = CARTESIAN_POINT ( 'NONE',  ( -18.50000000000000000, 67.85909929089923764, -227.8797997985275856 ) ) ;
#165214 = EDGE_CURVE ( 'NONE', #217842, #47981, #97752, .T. ) ;
#165215 = DIRECTION ( 'NONE',  ( 0.000000000000000000, 0.4999999999999799605, -0.8660254037844502539 ) ) ;
#165216 = VERTEX_POINT ( 'NONE', #176068 ) ;
#165217 = ORIENTED_EDGE ( 'NONE', *, *, #12872, .F. ) ;
#165218 = DIRECTION ( 'NONE',  ( 0.000000000000000000, 0.000000000000000000, 1.000000000000000000 ) ) ;
#165219 = VECTOR ( 'NONE', #74692, 1000.000000000000000 ) ;
#165220 = CIRCLE ( 'NONE', #136149, 0.09999999999999939493 ) ;
#165221 = ORIENTED_EDGE ( 'NONE', *, *, #166898, .F. ) ;
#165222 = AXIS2_PLACEMENT_3D ( 'NONE', #162348, #241859, #63207 ) ;
#165223 = DIRECTION ( 'NONE',  ( 1.000000000000000000, 0.000000000000000000, 0.000000000000000000 ) ) ;
#165224 = ORIENTED_EDGE ( 'NONE', *, *, #256305, .T. ) ;
#165225 = CARTESIAN_POINT ( 'NONE',  ( -23.15000000000000213, 87.65000000001215597, -139.6231074845242688 ) ) ;
#165226 = LINE ( 'NONE', #166543, #230372 ) ;
#165227 = EDGE_CURVE ( 'NONE', #129700, #53755, #20759, .T. ) ;
#165228 = DIRECTION ( 'NONE',  ( 0.000000000000000000, 0.000000000000000000, 1.000000000000000000 ) ) ;
#165229 = CARTESIAN_POINT ( 'NONE',  ( -21.09813707148783735, 75.96864850048329743, -209.9081695902610534 ) ) ;
#165230 = ORIENTED_EDGE ( 'NONE', *, *, #212802, .T. ) ;
#165231 = CARTESIAN_POINT ( 'NONE',  ( 19.97071067811864609, 11.72071067812981404, -125.1500000000000341 ) ) ;
#165232 = ORIENTED_EDGE ( 'NONE', *, *, #243223, .F. ) ;
#165233 = EDGE_CURVE ( 'NONE', #102935, #174819, #205038, .T. ) ;
#165234 = CARTESIAN_POINT ( 'NONE',  ( 18.39999999999999503, 64.25000000001179501, -78.77310748452438816 ) ) ;
#165235 = DIRECTION ( 'NONE',  ( 0.000000000000000000, -0.9651348961777157509, 0.2617529984165031243 ) ) ;
#165236 = DIRECTION ( 'NONE',  ( -1.000000000000000000, 0.000000000000000000, 0.000000000000000000 ) ) ;
#165237 = AXIS2_PLACEMENT_3D ( 'NONE', #94518, #253590, #73715 ) ;
#165238 = CARTESIAN_POINT ( 'NONE',  ( -21.65000000000000213, 66.05000000001224691, -149.2731074845244450 ) ) ;
#165239 = ORIENTED_EDGE ( 'NONE', *, *, #117924, .F. ) ;
#165240 = CIRCLE ( 'NONE', #52796, 0.1000000000000024342 ) ;
#165242 = CARTESIAN_POINT ( 'NONE',  ( -21.03922262424652345, 64.37609936600713922, -96.16389944163073267 ) ) ;
#165241 = AXIS2_PLACEMENT_3D ( 'NONE', #49769, #172340, #129310 ) ;
#165243 = EDGE_CURVE ( 'NONE', #40333, #198131, #138398, .T. ) ;
#165244 = ORIENTED_EDGE ( 'NONE', *, *, #165449, .T. ) ;
#165247 = VERTEX_POINT ( 'NONE', #173686 ) ;
#165246 = CARTESIAN_POINT ( 'NONE',  ( 18.59999999999996945, 46.46967969402478360, -243.0849751855955674 ) ) ;
#165245 = CARTESIAN_POINT ( 'NONE',  ( -21.00000000000000000, -11.65000000000000036, 0.000000000000000000 ) ) ;
#165248 = CARTESIAN_POINT ( 'NONE',  ( -13.39999999999994529, 64.35000000001120668, -21.02310748452479316 ) ) ;
#165249 = ORIENTED_EDGE ( 'NONE', *, *, #230156, .F. ) ;
#165250 = CIRCLE ( 'NONE', #248635, 0.09999999999999935330 ) ;
#165251 = ORIENTED_EDGE ( 'NONE', *, *, #164694, .F. ) ;
#165252 = DIRECTION ( 'NONE',  ( 0.000000000000000000, -1.000000000000000000, 0.000000000000000000 ) ) ;
#165253 = LINE ( 'NONE', #247349, #61636 ) ;
#165254 = ADVANCED_FACE ( 'NONE', ( #215316 ), #30122, .T. ) ;
#165255 = CARTESIAN_POINT ( 'NONE',  ( 21.05000000000000071, 70.50000000001199396, -115.4283735034374274 ) ) ;
#165256 = CARTESIAN_POINT ( 'NONE',  ( -17.78043020864321022, 65.14640788800610949, -79.86005831880416395 ) ) ;
#165257 = CARTESIAN_POINT ( 'NONE',  ( -20.94999999999999929, 1.835341550235569663, -112.0551512925630249 ) ) ;
#165258 = ADVANCED_FACE ( 'NONE', ( #130643 ), #134473, .F. ) ;
#165259 = ORIENTED_EDGE ( 'NONE', *, *, #244230, .F. ) ;
#165260 = DIRECTION ( 'NONE',  ( 1.000000000000000000, 0.000000000000000000, 0.000000000000000000 ) ) ;
#165261 = CARTESIAN_POINT ( 'NONE',  ( -15.75000000000000355, 66.65000000001228386, -153.2731074845243882 ) ) ;
#165262 = AXIS2_PLACEMENT_3D ( 'NONE', #102766, #161505, #48904 ) ;
#165263 = EDGE_LOOP ( 'NONE', ( #163350, #116229, #76251, #4915 ) ) ;
#165264 = DIRECTION ( 'NONE',  ( -0.000000000000000000, 1.000000000000000000, 7.272083257015735086E-15 ) ) ;
#165265 = ORIENTED_EDGE ( 'NONE', *, *, #77061, .F. ) ;
#165266 = DIRECTION ( 'NONE',  ( 0.000000000000000000, 1.000000000000000000, 0.000000000000000000 ) ) ;
#165267 = CARTESIAN_POINT ( 'NONE',  ( -23.15000000000000213, 71.65000000001180069, -81.87310748452433984 ) ) ;
#165268 = CARTESIAN_POINT ( 'NONE',  ( 20.94999999999999929, 36.14042471737574402, -236.0721279892244411 ) ) ;
#165270 = VERTEX_POINT ( 'NONE', #31583 ) ;
#165269 = DIRECTION ( 'NONE',  ( 0.000000000000000000, 0.000000000000000000, -1.000000000000000000 ) ) ;
#165271 = CARTESIAN_POINT ( 'NONE',  ( 23.14999999999999858, 71.00000000001199396, -115.4283735034374274 ) ) ;
#165272 = AXIS2_PLACEMENT_3D ( 'NONE', #250103, #27237, #8925 ) ;
#165273 = EDGE_CURVE ( 'NONE', #23667, #56249, #231056, .T. ) ;
#165274 = DIRECTION ( 'NONE',  ( 1.000000000000000000, -0.000000000000000000, -0.000000000000000000 ) ) ;
#165275 = CARTESIAN_POINT ( 'NONE',  ( -18.69999999999999929, -2.462484827400499565, -15.77971343137458682 ) ) ;
#165276 = ORIENTED_EDGE ( 'NONE', *, *, #75259, .F. ) ;
#165277 = VECTOR ( 'NONE', #115428, 1000.000000000000000 ) ;
#165278 = FACE_OUTER_BOUND ( 'NONE', #101800, .T. ) ;
#165279 = DIRECTION ( 'NONE',  ( -1.000000000000000000, 1.335000415235278971E-16, -2.979993593738921214E-16 ) ) ;
#165280 = ORIENTED_EDGE ( 'NONE', *, *, #131233, .T. ) ;
#165281 = CARTESIAN_POINT ( 'NONE',  ( -22.47007471830798764, 65.21035539001040604, -243.3066537799435878 ) ) ;
#165282 = AXIS2_PLACEMENT_3D ( 'NONE', #98780, #158824, #177109 ) ;
#165283 = AXIS2_PLACEMENT_3D ( 'NONE', #132967, #213772, #6893 ) ;
#165284 = ORIENTED_EDGE ( 'NONE', *, *, #44046, .T. ) ;
#165285 = AXIS2_PLACEMENT_3D ( 'NONE', #187897, #241449, #185318 ) ;
#165286 = ADVANCED_FACE ( 'NONE', ( #95374 ), #175863, .T. ) ;
#165287 = DIRECTION ( 'NONE',  ( 1.000000000000000000, -7.304098846218134667E-16, 0.000000000000000000 ) ) ;
#165290 = EDGE_LOOP ( 'NONE', ( #13705, #136884, #201661, #140087 ) ) ;
#165289 = LINE ( 'NONE', #124884, #67907 ) ;
#165288 = AXIS2_PLACEMENT_3D ( 'NONE', #35155, #212482, #52089 ) ;
#165291 = CIRCLE ( 'NONE', #107022, 0.09999999999999939493 ) ;
#165292 = EDGE_CURVE ( 'NONE', #31563, #121315, #111083, .T. ) ;
#165295 = ORIENTED_EDGE ( 'NONE', *, *, #79042, .T. ) ;
#165294 = ORIENTED_EDGE ( 'NONE', *, *, #172912, .F. ) ;
#165293 = CARTESIAN_POINT ( 'NONE',  ( 20.94999999999999929, 6.550000000011156231, -112.7500000000000284 ) ) ;
#165296 = DIRECTION ( 'NONE',  ( 0.000000000000000000, -0.8814952561688449428, 0.4721928772777310157 ) ) ;
#165297 = FACE_BOUND ( 'NONE', #53123, .T. ) ;
#165298 = LINE ( 'NONE', #66203, #44238 ) ;
#165300 = FACE_OUTER_BOUND ( 'NONE', #96042, .T. ) ;
#165299 = CARTESIAN_POINT ( 'NONE',  ( 22.44352723754029810, 0.009277095054436620969, -88.85027865465131924 ) ) ;
#165302 = ADVANCED_FACE ( 'NONE', ( #174965 ), #152816, .T. ) ;
#165301 = CARTESIAN_POINT ( 'NONE',  ( -23.25000000000000000, 1.115650265596050101E-11, -29.45000000000000284 ) ) ;
#165303 = DIRECTION ( 'NONE',  ( 1.000000000000000000, 0.000000000000000000, 0.000000000000000000 ) ) ;
#165304 = CONICAL_SURFACE ( 'NONE', #152876, 4.049999999999998046, 0.7853981633974604915 ) ;
#165305 = CARTESIAN_POINT ( 'NONE',  ( -17.22767730083113946, 65.65075578754417052, -58.16553617509497087 ) ) ;
#165306 = EDGE_CURVE ( 'NONE', #74683, #82237, #21734, .T. ) ;
#165307 = DIRECTION ( 'NONE',  ( -1.000000000000000000, 0.000000000000000000, -0.000000000000000000 ) ) ;
#165308 = CARTESIAN_POINT ( 'NONE',  ( 21.05000000000000071, 77.25000000001189449, -95.12310748452429721 ) ) ;
#165309 = AXIS2_PLACEMENT_3D ( 'NONE', #128721, #169159, #109134 ) ;
#165310 = ORIENTED_EDGE ( 'NONE', *, *, #25477, .T. ) ;
#165311 = ORIENTED_EDGE ( 'NONE', *, *, #215394, .T. ) ;
#165313 = CARTESIAN_POINT ( 'NONE',  ( 21.72449340488910252, 60.61704490885460217, -220.9543136786127491 ) ) ;
#165312 = CIRCLE ( 'NONE', #82075, 0.09999999999999484301 ) ;
#165315 = ORIENTED_EDGE ( 'NONE', *, *, #242760, .F. ) ;
#165314 = FACE_OUTER_BOUND ( 'NONE', #215597, .T. ) ;
#165316 = VERTEX_POINT ( 'NONE', #52374 ) ;
#165317 = PLANE ( 'NONE',  #101924 ) ;
#165318 = EDGE_CURVE ( 'NONE', #239491, #161272, #135768, .T. ) ;
#165319 = ORIENTED_EDGE ( 'NONE', *, *, #185100, .T. ) ;
#165320 = CARTESIAN_POINT ( 'NONE',  ( -21.11825140030087411, 69.55459243459270624, -136.5303111051574376 ) ) ;
#165321 = AXIS2_PLACEMENT_3D ( 'NONE', #159179, #97857, #17094 ) ;
#165322 = AXIS2_PLACEMENT_3D ( 'NONE', #255755, #17209, #100540 ) ;
#165323 = ADVANCED_FACE ( 'NONE', ( #90214 ), #133218, .F. ) ;
#165324 = EDGE_CURVE ( 'NONE', #71372, #47133, #232340, .T. ) ;
#165325 = ORIENTED_EDGE ( 'NONE', *, *, #103152, .T. ) ;
#165326 = CARTESIAN_POINT ( 'NONE',  ( -23.15000000000000213, -11.48912529306489816, -63.89999999999999858 ) ) ;
#165327 = DIRECTION ( 'NONE',  ( 0.000000000000000000, -0.5000000000000004441, -0.8660254037844384856 ) ) ;
#165329 = ORIENTED_EDGE ( 'NONE', *, *, #139697, .F. ) ;
#165328 = ORIENTED_EDGE ( 'NONE', *, *, #231874, .F. ) ;
#165330 = ORIENTED_EDGE ( 'NONE', *, *, #87499, .F. ) ;
#165331 = CARTESIAN_POINT ( 'NONE',  ( 21.05563370358598263, 10.72423035585766549, -45.68309081596307664 ) ) ;
#165332 = TOROIDAL_SURFACE ( 'NONE', #165536, 12.77499999999999858, 0.1000000000000000056 ) ;
#165333 = ORIENTED_EDGE ( 'NONE', *, *, #75123, .T. ) ;
#165334 = ORIENTED_EDGE ( 'NONE', *, *, #252105, .F. ) ;
#165335 = EDGE_CURVE ( 'NONE', #66273, #141610, #109180, .T. ) ;
#165336 = DIRECTION ( 'NONE',  ( -1.000000000000000000, -0.000000000000000000, -0.000000000000000000 ) ) ;
#165337 = LINE ( 'NONE', #143185, #169840 ) ;
#165339 = VERTEX_POINT ( 'NONE', #199634 ) ;
#165338 = CARTESIAN_POINT ( 'NONE',  ( 21.05000000000000071, -4.892732937820623462, -233.2805462221312496 ) ) ;
#165340 = DIRECTION ( 'NONE',  ( 0.000000000000000000, 0.000000000000000000, 1.000000000000000000 ) ) ;
#165341 = DIRECTION ( 'NONE',  ( 0.000000000000000000, 0.3994087351226822125, 0.9167729611565227366 ) ) ;
#165343 = VERTEX_POINT ( 'NONE', #77086 ) ;
#165342 = FACE_OUTER_BOUND ( 'NONE', #43949, .T. ) ;
#165344 = LINE ( 'NONE', #244865, #230142 ) ;
#165346 = EDGE_CURVE ( 'NONE', #221121, #247770, #92625, .T. ) ;
#165345 = EDGE_LOOP ( 'NONE', ( #176901, #37927 ) ) ;
#165347 = CARTESIAN_POINT ( 'NONE',  ( 20.94999999999999574, 10.47338541492405994, -74.57865446424858646 ) ) ;
#165348 = ORIENTED_EDGE ( 'NONE', *, *, #65716, .F. ) ;
#165349 = DIRECTION ( 'NONE',  ( 1.000000000000000000, 0.000000000000000000, 0.000000000000000000 ) ) ;
#165350 = CARTESIAN_POINT ( 'NONE',  ( -23.25000000000000000, -1.835859311432481045, -112.0044391687985694 ) ) ;
#165351 = CIRCLE ( 'NONE', #40489, 0.1000000000000028644 ) ;
#165352 = EDGE_LOOP ( 'NONE', ( #192681, #30855, #14977, #174086, #118745 ) ) ;
#165354 = DIRECTION ( 'NONE',  ( 1.000000000000000000, 3.265361837132813093E-16, -0.000000000000000000 ) ) ;
#165353 = CARTESIAN_POINT ( 'NONE',  ( 20.95512840106819752, 10.62384869378447583, -45.70247922079902025 ) ) ;
#165355 = DIRECTION ( 'NONE',  ( -1.000000000000000000, 7.304098846218163263E-16, -4.217023435051627211E-16 ) ) ;
#165356 = CARTESIAN_POINT ( 'NONE',  ( -16.87036670365549895, 22.88247411645692253, -230.8391385443351282 ) ) ;
#165357 = ORIENTED_EDGE ( 'NONE', *, *, #146318, .F. ) ;
#165358 = ORIENTED_EDGE ( 'NONE', *, *, #53608, .T. ) ;
#165359 = VECTOR ( 'NONE', #227526, 1000.000000000000000 ) ;
#165360 = FACE_OUTER_BOUND ( 'NONE', #116600, .T. ) ;
#165361 = CYLINDRICAL_SURFACE ( 'NONE', #127592, 0.5000000000000004441 ) ;
#165363 = ORIENTED_EDGE ( 'NONE', *, *, #92768, .F. ) ;
#165362 = ADVANCED_FACE ( 'NONE', ( #41845 ), #33420, .F. ) ;
#165364 = FACE_OUTER_BOUND ( 'NONE', #89697, .T. ) ;
#165365 = VERTEX_POINT ( 'NONE', #80923 ) ;
#165366 = EDGE_CURVE ( 'NONE', #202204, #117904, #62675, .T. ) ;
#165367 = CARTESIAN_POINT ( 'NONE',  ( -21.05000000000000071, 1.851028230140860487, -11.65391326942249606 ) ) ;
#165368 = ORIENTED_EDGE ( 'NONE', *, *, #65366, .T. ) ;
#165369 = CARTESIAN_POINT ( 'NONE',  ( -23.49999999999994316, 64.35000000001120668, -51.02310748452479316 ) ) ;
#165370 = TOROIDAL_SURFACE ( 'NONE', #127771, 0.2000000000000000111, 0.1000000000000000056 ) ;
#165371 = DIRECTION ( 'NONE',  ( 0.000000000000000000, 0.000000000000000000, -1.000000000000000000 ) ) ;
#165372 = AXIS2_PLACEMENT_3D ( 'NONE', #134792, #223323, #81237 ) ;
#165373 = DIRECTION ( 'NONE',  ( -1.000000000000000000, -0.000000000000000000, -0.000000000000000000 ) ) ;
#165374 = AXIS2_PLACEMENT_3D ( 'NONE', #9198, #109571, #211256 ) ;
#165375 = VECTOR ( 'NONE', #50535, 1000.000000000000000 ) ;
#165377 = ADVANCED_FACE ( 'NONE', ( #180053 ), #140926, .T. ) ;
#165376 = ORIENTED_EDGE ( 'NONE', *, *, #176999, .F. ) ;
#165378 = CARTESIAN_POINT ( 'NONE',  ( -18.50000000000000000, 65.70729864260985664, -64.06574559737244101 ) ) ;
#165379 = VECTOR ( 'NONE', #72985, 1000.000000000000000 ) ;
#165380 = VERTEX_POINT ( 'NONE', #219153 ) ;
#165381 = EDGE_LOOP ( 'NONE', ( #134128, #71169, #191958, #66543 ) ) ;
#165382 = ORIENTED_EDGE ( 'NONE', *, *, #215171, .F. ) ;
#165383 = DIRECTION ( 'NONE',  ( 1.000000000000000000, 0.000000000000000000, -0.000000000000000000 ) ) ;
#165384 = CARTESIAN_POINT ( 'NONE',  ( -21.05000000000000071, 1.115600667400684642E-11, -167.5000000000000284 ) ) ;
#165385 = PLANE ( 'NONE',  #96542 ) ;
#165386 = FACE_OUTER_BOUND ( 'NONE', #89880, .T. ) ;
#165387 = CARTESIAN_POINT ( 'NONE',  ( -18.50000000000000000, 66.65000000001253966, -182.3731074845244393 ) ) ;
#165389 = CARTESIAN_POINT ( 'NONE',  ( 21.05000000000000071, 59.13236860818125251, -225.8959333647716505 ) ) ;
#165388 = DIRECTION ( 'NONE',  ( 0.000000000000000000, 6.608470384673558123E-15, -1.000000000000000000 ) ) ;
#165391 = VERTEX_POINT ( 'NONE', #101753 ) ;
#165390 = DIRECTION ( 'NONE',  ( 1.000000000000000000, 0.000000000000000000, 0.000000000000000000 ) ) ;
#165392 = CARTESIAN_POINT ( 'NONE',  ( 18.59999999999999787, 76.00000000001165290, -69.52310748452431710 ) ) ;
#165393 = ORIENTED_EDGE ( 'NONE', *, *, #140214, .T. ) ;
#165394 = CARTESIAN_POINT ( 'NONE',  ( 21.13461538461538325, 8.885417037985616773, -79.35000000000005116 ) ) ;
#165395 = CIRCLE ( 'NONE', #77883, 0.1000000000000074440 ) ;
#165396 = ORIENTED_EDGE ( 'NONE', *, *, #213163, .T. ) ;
#165397 = ORIENTED_EDGE ( 'NONE', *, *, #126438, .F. ) ;
#165398 = CARTESIAN_POINT ( 'NONE',  ( 21.05000000000000071, 0.000000000000000000, 0.000000000000000000 ) ) ;
#165399 = VECTOR ( 'NONE', #42634, 1000.000000000000227 ) ;
#165400 = CARTESIAN_POINT ( 'NONE',  ( 23.14999999999999503, 11.75000000000000711, -12.15000000000000036 ) ) ;
#165402 = EDGE_CURVE ( 'NONE', #94150, #161837, #146595, .T. ) ;
#165401 = CARTESIAN_POINT ( 'NONE',  ( -16.97683810757273193, 66.05000000001153637, -49.28668419698479397 ) ) ;
#165403 = CARTESIAN_POINT ( 'NONE',  ( 21.05000000000000071, 4.850467289719620823, -21.46573259099832498 ) ) ;
#165404 = EDGE_CURVE ( 'NONE', #211140, #186900, #256961, .T. ) ;
#165405 = VECTOR ( 'NONE', #142695, 1000.000000000000227 ) ;
#165406 = CARTESIAN_POINT ( 'NONE',  ( 23.14999999999998437, 87.75000000001193712, -103.0231074845242318 ) ) ;
#165407 = ORIENTED_EDGE ( 'NONE', *, *, #161221, .T. ) ;
#165408 = VERTEX_POINT ( 'NONE', #40575 ) ;
#165410 = ADVANCED_FACE ( 'NONE', ( #237451 ), #19702, .T. ) ;
#165409 = LINE ( 'NONE', #208400, #128143 ) ;
#165411 = ORIENTED_EDGE ( 'NONE', *, *, #10517, .T. ) ;
#165412 = CARTESIAN_POINT ( 'NONE',  ( 18.59999999999999787, 77.83534155023598089, -57.96795619196132776 ) ) ;
#165413 = CARTESIAN_POINT ( 'NONE',  ( 23.24999999999999289, 69.55000000001150795, -48.37310748452436826 ) ) ;
#165414 = FACE_OUTER_BOUND ( 'NONE', #184329, .T. ) ;
#165415 = CARTESIAN_POINT ( 'NONE',  ( -23.25000000000000000, 8.882751598337867094, -187.0399955572217721 ) ) ;
#165416 = PLANE ( 'NONE',  #223760 ) ;
#165417 = DIRECTION ( 'NONE',  ( 1.000000000000000000, 0.000000000000000000, 0.000000000000000000 ) ) ;
#165418 = ORIENTED_EDGE ( 'NONE', *, *, #108168, .F. ) ;
#165419 = FACE_OUTER_BOUND ( 'NONE', #243162, .T. ) ;
#165420 = EDGE_CURVE ( 'NONE', #5211, #211434, #17146, .T. ) ;
#165421 = CARTESIAN_POINT ( 'NONE',  ( 23.25000000000000355, 90.68298050906625463, -235.1761083729927861 ) ) ;
#165422 = CARTESIAN_POINT ( 'NONE',  ( 21.05000000000000071, -1.736257131597395809, -11.56865232901749785 ) ) ;
#165423 = DIRECTION ( 'NONE',  ( 1.000000000000000000, 2.952720810173289112E-16, -0.000000000000000000 ) ) ;
#165425 = ADVANCED_FACE ( 'NONE', ( #118800 ), #182629, .T. ) ;
#165424 = DIRECTION ( 'NONE',  ( 0.000000000000000000, -0.4999999999999478195, -0.8660254037844686836 ) ) ;
#165426 = VECTOR ( 'NONE', #67613, 1000.000000000000000 ) ;
#165428 = TOROIDAL_SURFACE ( 'NONE', #219557, 0.2000000000000000111, 0.1000000000000000056 ) ;
#165427 = CYLINDRICAL_SURFACE ( 'NONE', #36448, 0.09999999999999990841 ) ;
#165429 = CIRCLE ( 'NONE', #57046, 0.09999999999999939493 ) ;
#165430 = VECTOR ( 'NONE', #117308, 1000.000000000000000 ) ;
#165431 = EDGE_CURVE ( 'NONE', #5236, #156221, #87343, .T. ) ;
#165432 = ORIENTED_EDGE ( 'NONE', *, *, #225449, .T. ) ;
#165434 = EDGE_CURVE ( 'NONE', #23607, #148851, #192782, .T. ) ;
#165433 = ADVANCED_FACE ( 'NONE', ( #148637 ), #3971, .T. ) ;
#165435 = SPHERICAL_SURFACE ( 'NONE', #157936, 0.1000000000000000056 ) ;
#165436 = EDGE_LOOP ( 'NONE', ( #65505, #33587, #182133, #113357 ) ) ;
#165437 = FACE_BOUND ( 'NONE', #79712, .T. ) ;
#165438 = CARTESIAN_POINT ( 'NONE',  ( -11.59999999999994458, 63.75000000001119815, -21.02310748452479316 ) ) ;
#165439 = DIRECTION ( 'NONE',  ( 1.000000000000000000, -0.000000000000000000, -0.000000000000000000 ) ) ;
#165440 = ORIENTED_EDGE ( 'NONE', *, *, #228087, .F. ) ;
#165441 = CARTESIAN_POINT ( 'NONE',  ( -20.05000000000000426, 9.250000000011157297, -54.75000000000000000 ) ) ;
#165442 = DIRECTION ( 'NONE',  ( 1.000000000000000000, 0.000000000000000000, 0.000000000000000000 ) ) ;
#165443 = AXIS2_PLACEMENT_3D ( 'NONE', #185115, #85978, #165567 ) ;
#165444 = CARTESIAN_POINT ( 'NONE',  ( -20.54999999999999716, 68.96522873961046685, -235.0783363939394235 ) ) ;
#165445 = DIRECTION ( 'NONE',  ( 0.000000000000000000, -0.1568667991644355497, -0.9876197685951332295 ) ) ;
#165446 = VECTOR ( 'NONE', #111241, 1000.000000000000000 ) ;
#165447 = ADVANCED_FACE ( 'NONE', ( #86040 ), #228167, .T. ) ;
#165448 = DIRECTION ( 'NONE',  ( -0.000000000000000000, -0.8700118002898356018, 0.4930308989875170078 ) ) ;
#165449 = EDGE_CURVE ( 'NONE', #155241, #179129, #242655, .T. ) ;
#165450 = DIRECTION ( 'NONE',  ( 0.000000000000000000, 0.000000000000000000, 1.000000000000000000 ) ) ;
#165451 = VECTOR ( 'NONE', #214582, 1000.000000000000000 ) ;
#165452 = ORIENTED_EDGE ( 'NONE', *, *, #172491, .T. ) ;
#165453 = VERTEX_POINT ( 'NONE', #242573 ) ;
#165454 = DIRECTION ( 'NONE',  ( 0.000000000000000000, -6.982962677686266711E-15, 1.000000000000000000 ) ) ;
#165456 = ORIENTED_EDGE ( 'NONE', *, *, #222477, .T. ) ;
#165455 = CARTESIAN_POINT ( 'NONE',  ( -21.59142135623730852, 52.84246341164006822, -233.6994099349884380 ) ) ;
#165457 = FACE_OUTER_BOUND ( 'NONE', #71637, .T. ) ;
#165458 = EDGE_CURVE ( 'NONE', #199798, #132306, #121871, .T. ) ;
#165459 = DIRECTION ( 'NONE',  ( 1.000000000000000000, -0.000000000000000000, -0.000000000000000000 ) ) ;
#165460 = ORIENTED_EDGE ( 'NONE', *, *, #236139, .F. ) ;
#165461 = CARTESIAN_POINT ( 'NONE',  ( 22.59999985501178799, 11.74986979301414181, -33.43440133020061467 ) ) ;
#165462 = CONTEXT_DEPENDENT_SHAPE_REPRESENTATION ( #112555, #255639 ) ;
#165463 = EDGE_CURVE ( 'NONE', #226856, #138091, #111834, .T. ) ;
#165464 = FACE_OUTER_BOUND ( 'NONE', #134140, .T. ) ;
#165465 = ORIENTED_EDGE ( 'NONE', *, *, #88603, .T. ) ;
#165466 = CARTESIAN_POINT ( 'NONE',  ( -23.25000000000000000, -11.74999999998884448, -164.4000000000000057 ) ) ;
#165467 = AXIS2_PLACEMENT_3D ( 'NONE', #3043, #166021, #4329 ) ;
#165468 = FACE_OUTER_BOUND ( 'NONE', #84777, .T. ) ;
#165469 = ORIENTED_EDGE ( 'NONE', *, *, #77261, .F. ) ;
#165470 = ORIENTED_EDGE ( 'NONE', *, *, #214819, .T. ) ;
#165471 = EDGE_CURVE ( 'NONE', #239767, #160025, #226059, .T. ) ;
#165472 = CARTESIAN_POINT ( 'NONE',  ( -22.59999970745345976, 76.00935637733951467, -114.7736206921935320 ) ) ;
#165473 = CARTESIAN_POINT ( 'NONE',  ( 18.79999999999999716, 1.250000000000000000, 0.000000000000000000 ) ) ;
#165474 = AXIS2_PLACEMENT_3D ( 'NONE', #124712, #25614, #146819 ) ;
#165475 = CARTESIAN_POINT ( 'NONE',  ( -23.25000000000000000, -9.599999999988838795, -57.10603087734755690 ) ) ;
#165476 = CARTESIAN_POINT ( 'NONE',  ( -23.25000000000000000, 7.804459559388685186, -245.4620200072988325 ) ) ;
#165477 = LINE ( 'NONE', #186319, #244299 ) ;
#165478 = DIRECTION ( 'NONE',  ( -1.000000000000000000, -0.000000000000000000, -0.000000000000000000 ) ) ;
#165479 = CARTESIAN_POINT ( 'NONE',  ( -16.93658211146646408, 9.994108662341188776, -12.59570493004432379 ) ) ;
#165482 = CARTESIAN_POINT ( 'NONE',  ( -23.25000000000000000, 1.115600667400684642E-11, -208.8999999999999488 ) ) ;
#165481 = AXIS2_PLACEMENT_3D ( 'NONE', #138521, #182842, #100671 ) ;
#165480 = FACE_OUTER_BOUND ( 'NONE', #197606, .T. ) ;
#165483 = ADVANCED_FACE ( 'NONE', ( #187764 ), #156791, .T. ) ;
#165484 = DIRECTION ( 'NONE',  ( 0.000000000000000000, -6.938893903907234689E-15, 1.000000000000000000 ) ) ;
#165485 = LINE ( 'NONE', #245006, #158747 ) ;
#165486 = DIRECTION ( 'NONE',  ( 0.000000000000000000, -0.8660254037844377084, -0.5000000000000016653 ) ) ;
#165487 = CIRCLE ( 'NONE', #194537, 0.1000000000000017958 ) ;
#165488 = ORIENTED_EDGE ( 'NONE', *, *, #178243, .T. ) ;
#165489 = CIRCLE ( 'NONE', #53031, 0.1000000000000028644 ) ;
#165490 = VERTEX_POINT ( 'NONE', #229445 ) ;
#165491 = CARTESIAN_POINT ( 'NONE',  ( -18.59999999999999787, 77.25000000001159606, -61.52310748452431710 ) ) ;
#165492 = DIRECTION ( 'NONE',  ( 1.000000000000000000, 0.000000000000000000, 0.000000000000000000 ) ) ;
#165494 = CARTESIAN_POINT ( 'NONE',  ( -12.30589683808040924, 12.80332707393613134, -215.8182015632437185 ) ) ;
#165493 = CARTESIAN_POINT ( 'NONE',  ( -21.05000000000000426, 69.72991413632281876, -103.0579754875374476 ) ) ;
#165495 = PRODUCT_DEFINITION_FORMATION_WITH_SPECIFIED_SOURCE ( 'ANY', '', #147169, .NOT_KNOWN. ) ;
#165496 = AXIS2_PLACEMENT_3D ( 'NONE', #61086, #161498, #241025 ) ;
#165497 = CARTESIAN_POINT ( 'NONE',  ( 20.95539060131842746, 39.30035216274485776, -236.7266179559437091 ) ) ;
#165498 = CARTESIAN_POINT ( 'NONE',  ( 18.57071067811864040, 10.17928932189250091, -188.7499999999999716 ) ) ;
#165499 = ADVANCED_FACE ( 'NONE', ( #170806 ), #171970, .T. ) ;
#165500 = AXIS2_PLACEMENT_3D ( 'NONE', #20453, #63393, #157416 ) ;
#165501 = CARTESIAN_POINT ( 'NONE',  ( -21.33487959338958362, 6.571513019293445446, -199.5687945318220500 ) ) ;
#165502 = ORIENTED_EDGE ( 'NONE', *, *, #204550, .T. ) ;
#165503 = ORIENTED_EDGE ( 'NONE', *, *, #43457, .F. ) ;
#165504 = B_SPLINE_CURVE_WITH_KNOTS ( 'NONE', 3,
 ( #104874, #198875, #102308, #5790 ),
 .UNSPECIFIED., .F., .F.,
 ( 4, 4 ),
 ( 7.757919228897728493E-18, 0.0001058379652594506807 ),
 .UNSPECIFIED. ) ;
#165505 = DIRECTION ( 'NONE',  ( 1.000000000000000000, 0.000000000000000000, 0.000000000000000000 ) ) ;
#165506 = ORIENTED_EDGE ( 'NONE', *, *, #146286, .F. ) ;
#165507 = DIRECTION ( 'NONE',  ( 1.000000000000000000, 0.000000000000000000, 0.000000000000000000 ) ) ;
#165508 = AXIS2_PLACEMENT_3D ( 'NONE', #77900, #211014, #12831 ) ;
#165509 = CIRCLE ( 'NONE', #82254, 0.1999999999999987899 ) ;
#165510 = CARTESIAN_POINT ( 'NONE',  ( -18.40000000000000213, 53.37686160793744961, -235.8706811220569932 ) ) ;
#165511 = AXIS2_PLACEMENT_3D ( 'NONE', #254149, #75558, #195506 ) ;
#165513 = ORIENTED_EDGE ( 'NONE', *, *, #25968, .T. ) ;
#165512 = CIRCLE ( 'NONE', #169821, 2.600000000000001421 ) ;
#165514 = CARTESIAN_POINT ( 'NONE',  ( 23.14999999999998437, -4.049999999988842525, -33.50000000000000000 ) ) ;
#165515 = ORIENTED_EDGE ( 'NONE', *, *, #226275, .F. ) ;
#165516 = TOROIDAL_SURFACE ( 'NONE', #61454, 0.6000000000000009770, 0.1000000000000000056 ) ;
#165517 = DIRECTION ( 'NONE',  ( -0.7071067811865389130, 8.659560562355038861E-17, -0.7071067811865561215 ) ) ;
#165518 = DIRECTION ( 'NONE',  ( -1.000000000000000000, 0.000000000000000000, 0.000000000000000000 ) ) ;
#165519 = DIRECTION ( 'NONE',  ( -1.000000000000000000, 0.000000000000000000, 0.000000000000000000 ) ) ;
#165520 = CARTESIAN_POINT ( 'NONE',  ( 18.58703555224998638, -9.406336740777428318, -141.1249446412470547 ) ) ;
#165521 = DIRECTION ( 'NONE',  ( 0.000000000000000000, -0.9651348961777158619, 0.2617529984165032353 ) ) ;
#165522 = LINE ( 'NONE', #126378, #174997 ) ;
#165523 = DIRECTION ( 'NONE',  ( -0.000000000000000000, 0.2617529984165031243, 0.9651348961777157509 ) ) ;
#165524 = DIRECTION ( 'NONE',  ( 0.5735764363510460484, 0.8191520442889919096, -0.000000000000000000 ) ) ;
#165526 = ORIENTED_EDGE ( 'NONE', *, *, #77941, .T. ) ;
#165525 = CARTESIAN_POINT ( 'NONE',  ( 18.50000000000000000, -0.6242021414292636683, -242.4056766684517186 ) ) ;
#165528 = CARTESIAN_POINT ( 'NONE',  ( 13.99999999999999822, 66.15000000001155911, -52.77310748452440237 ) ) ;
#165527 = CARTESIAN_POINT ( 'NONE',  ( -16.80939487329394666, 66.05000000001201954, -115.6731074845234843 ) ) ;
#165529 = ORIENTED_EDGE ( 'NONE', *, *, #253996, .F. ) ;
#165531 = ORIENTED_EDGE ( 'NONE', *, *, #187097, .T. ) ;
#165530 = CARTESIAN_POINT ( 'NONE',  ( -23.15000000000000213, 87.65000000001246860, -173.1231074845242688 ) ) ;
#165532 = AXIS2_PLACEMENT_3D ( 'NONE', #257990, #238479, #160259 ) ;
#165533 = ORIENTED_EDGE ( 'NONE', *, *, #193182, .F. ) ;
#165534 = FACE_OUTER_BOUND ( 'NONE', #232458, .T. ) ;
#165535 = AXIS2_PLACEMENT_3D ( 'NONE', #180225, #257126, #158127 ) ;
#165536 = AXIS2_PLACEMENT_3D ( 'NONE', #192684, #55684, #131405 ) ;
#165537 = LINE ( 'NONE', #101657, #171701 ) ;
#165538 = CARTESIAN_POINT ( 'NONE',  ( 21.11825140030063253, 0.007203620644165132682, -127.5545924345806412 ) ) ;
#165539 = CARTESIAN_POINT ( 'NONE',  ( -18.59999999999999787, 72.02722222756958104, -225.1832529173024398 ) ) ;
#165540 = CARTESIAN_POINT ( 'NONE',  ( -18.59999999999999787, 11.64999999999999680, -7.014805770654001016 ) ) ;
#165541 = CARTESIAN_POINT ( 'NONE',  ( 21.05000000000000071, 5.000000000011153745, -79.40526601891313874 ) ) ;
#165542 = ADVANCED_FACE ( 'NONE', ( #92489 ), #191636, .F. ) ;
#165543 = AXIS2_PLACEMENT_3D ( 'NONE', #170871, #228228, #129122 ) ;
#165544 = CARTESIAN_POINT ( 'NONE',  ( 21.09813707148777340, 69.61493789427564138, -136.5544589840538663 ) ) ;
#165545 = ORIENTED_EDGE ( 'NONE', *, *, #228281, .F. ) ;
#165546 = ORIENTED_EDGE ( 'NONE', *, *, #41055, .T. ) ;
#165547 = DIRECTION ( 'NONE',  ( -1.836970198721029934E-16, 1.000000000000000000, 0.000000000000000000 ) ) ;
#165548 = AXIS2_PLACEMENT_3D ( 'NONE', #233443, #235971, #138145 ) ;
#165549 = ORIENTED_EDGE ( 'NONE', *, *, #75642, .T. ) ;
#165550 = PLANE ( 'NONE',  #17559 ) ;
#165551 = ORIENTED_EDGE ( 'NONE', *, *, #146012, .F. ) ;
#165552 = CARTESIAN_POINT ( 'NONE',  ( -18.50000000000000000, 61.43991280424057777, -221.4883200034892923 ) ) ;
#165553 = AXIS2_PLACEMENT_3D ( 'NONE', #96968, #38337, #1745 ) ;
#165554 = CARTESIAN_POINT ( 'NONE',  ( -21.64999999999999858, 7.250000000011148416, -79.25000000000004263 ) ) ;
#165555 = CARTESIAN_POINT ( 'NONE',  ( 19.97071067811864609, 11.72071067811865674, -21.35000000000000142 ) ) ;
#165556 = EDGE_CURVE ( 'NONE', #179132, #152685, #12988, .T. ) ;
#165557 = DIRECTION ( 'NONE',  ( -0.000000000000000000, 0.000000000000000000, -1.000000000000000000 ) ) ;
#165558 = CARTESIAN_POINT ( 'NONE',  ( -21.05000000000000071, 1.360870587203197646, -108.5729979270909951 ) ) ;
#165559 = EDGE_LOOP ( 'NONE', ( #115852, #145781, #167894, #79907 ) ) ;
#165560 = VECTOR ( 'NONE', #147636, 1000.000000000000000 ) ;
#165561 = ADVANCED_FACE ( 'NONE', ( #172072 ), #21910, .T. ) ;
#165562 = AXIS2_PLACEMENT_3D ( 'NONE', #205700, #220480, #21010 ) ;
#165563 = DIRECTION ( 'NONE',  ( 0.000000000000000000, 0.000000000000000000, 1.000000000000000000 ) ) ;
#165564 = VECTOR ( 'NONE', #85826, 1000.000000000000000 ) ;
#165565 = VECTOR ( 'NONE', #82927, 1000.000000000000114 ) ;
#165566 = CARTESIAN_POINT ( 'NONE',  ( -18.59999999999999787, 74.13328508995498112, -158.2704322382423641 ) ) ;
#165567 = DIRECTION ( 'NONE',  ( 0.000000000000000000, -0.6324589521315897578, 0.7745938767306462802 ) ) ;
#165568 = DIRECTION ( 'NONE',  ( -0.000000000000000000, -6.982962677686266711E-15, 1.000000000000000000 ) ) ;
#165569 = ORIENTED_EDGE ( 'NONE', *, *, #35526, .T. ) ;
#165571 = CARTESIAN_POINT ( 'NONE',  ( -20.64999999999999858, 85.00000000001232081, -160.6291383618718385 ) ) ;
#165570 = CARTESIAN_POINT ( 'NONE',  ( -20.94999999999999929, 68.97833521811179480, -99.18954208262705663 ) ) ;
#165572 = ORIENTED_EDGE ( 'NONE', *, *, #102586, .F. ) ;
#165575 = EDGE_LOOP ( 'NONE', ( #152382, #133156, #113842, #35445 ) ) ;
#165574 = DIRECTION ( 'NONE',  ( 0.000000000000000000, -0.2128009952263602012, 0.9770955615653315052 ) ) ;
#165573 = CARTESIAN_POINT ( 'NONE',  ( 21.70464131381650219, 68.90464198104409377, -103.0231074845243739 ) ) ;
#165576 = AXIS2_PLACEMENT_3D ( 'NONE', #169207, #210867, #70102 ) ;
#165577 = EDGE_LOOP ( 'NONE', ( #210616, #182706, #118869, #253162, #126660 ) ) ;
#165578 = CARTESIAN_POINT ( 'NONE',  ( -17.04295772865494740, 10.02489942527117783, -113.1500000000000483 ) ) ;
#165579 = CARTESIAN_POINT ( 'NONE',  ( -21.11825140030084214, 34.01722988687274096, -243.6719807376591689 ) ) ;
#165580 = EDGE_CURVE ( 'NONE', #86132, #77947, #230187, .T. ) ;
#165581 = CARTESIAN_POINT ( 'NONE',  ( 18.59999999999999787, 1.148907358139439339E-11, -201.0000000000015064 ) ) ;
#165582 = ORIENTED_EDGE ( 'NONE', *, *, #209131, .T. ) ;
#165583 = CYLINDRICAL_SURFACE ( 'NONE', #172018, 0.09999999999999939493 ) ;
#165584 = ADVANCED_FACE ( 'NONE', ( #93770 ), #41797, .T. ) ;
#165585 = FACE_OUTER_BOUND ( 'NONE', #146248, .T. ) ;
#165586 = EDGE_CURVE ( 'NONE', #7150, #38262, #255059, .T. ) ;
#165588 = CARTESIAN_POINT ( 'NONE',  ( 18.79999999999999716, 1.885425182446133885, -11.49641995933507843 ) ) ;
#165587 = CARTESIAN_POINT ( 'NONE',  ( -18.59999999999999787, 44.52640028187936849, -247.3006740988509193 ) ) ;
#165590 = ORIENTED_EDGE ( 'NONE', *, *, #99118, .F. ) ;
#165589 = CARTESIAN_POINT ( 'NONE',  ( 20.94999999999999929, 11.65000000001116298, -93.71613433702195550 ) ) ;
#165591 = AXIS2_PLACEMENT_3D ( 'NONE', #235387, #159723, #20216 ) ;
#165592 = EDGE_CURVE ( 'NONE', #210104, #95143, #213419, .T. ) ;
#165593 = VERTEX_POINT ( 'NONE', #251563 ) ;
#165594 = CARTESIAN_POINT ( 'NONE',  ( 19.86930884467576419, 64.31308993304064359, -78.28388484558554694 ) ) ;
#165595 = B_SPLINE_CURVE_WITH_KNOTS ( 'NONE', 3,
 ( #114755, #237274, #198135, #74381, #18222, #177331, #59884, #213849, #99005, #255491, #254239, #116053, #97720, #174776, #139425, #195596 ),
 .UNSPECIFIED., .F., .F.,
 ( 4, 3, 3, 3, 3, 4 ),
 ( 0.000000000000000000, 2.209833635978076120E-05, 5.595056164119271882E-05, 8.979992002655370561E-05, 0.0001236482757198912198, 0.0001574984039362985287 ),
 .UNSPECIFIED. ) ;
#165596 = DIRECTION ( 'NONE',  ( 0.000000000000000000, 0.000000000000000000, 1.000000000000000000 ) ) ;
#165597 = VECTOR ( 'NONE', #122864, 1000.000000000000000 ) ;
#165598 = CARTESIAN_POINT ( 'NONE',  ( 20.94999999999999574, 77.83534155023646406, -124.9679561919613064 ) ) ;
#165599 = ORIENTED_EDGE ( 'NONE', *, *, #140713, .F. ) ;
#165600 = CARTESIAN_POINT ( 'NONE',  ( 20.94999999999999929, 64.35000000001249987, -176.8069731475025321 ) ) ;
#165601 = ADVANCED_FACE ( 'NONE', ( #54639 ), #149926, .T. ) ;
#165602 = ORIENTED_EDGE ( 'NONE', *, *, #77361, .T. ) ;
#165603 = DIRECTION ( 'NONE',  ( -0.000000000000000000, 1.000000000000000000, 6.982962677686266711E-15 ) ) ;
#165604 = CARTESIAN_POINT ( 'NONE',  ( 20.94999999999999574, 44.29184115892635987, -259.0069060397277667 ) ) ;
#165605 = CARTESIAN_POINT ( 'NONE',  ( 22.47007471830798764, 7.720710651937610081, -33.50000000000001421 ) ) ;
#165606 = ORIENTED_EDGE ( 'NONE', *, *, #92770, .T. ) ;
#165607 = FACE_OUTER_BOUND ( 'NONE', #104934, .T. ) ;
#165608 = EDGE_CURVE ( 'NONE', #53948, #156004, #233318, .T. ) ;
#165609 = ORIENTED_EDGE ( 'NONE', *, *, #61730, .T. ) ;
#165610 = AXIS2_PLACEMENT_3D ( 'NONE', #223801, #242083, #6034 ) ;
#165611 = VECTOR ( 'NONE', #183382, 1000.000000000000000 ) ;
#165612 = CARTESIAN_POINT ( 'NONE',  ( -20.94999999999999929, -11.64999999998884483, -136.9000000000000341 ) ) ;
#165613 = DIRECTION ( 'NONE',  ( 0.000000000000000000, 0.000000000000000000, -1.000000000000000000 ) ) ;
#165614 = CIRCLE ( 'NONE', #53169, 0.09999999999999967248 ) ;
#165615 = ORIENTED_EDGE ( 'NONE', *, *, #42097, .F. ) ;
#165616 = ORIENTED_EDGE ( 'NONE', *, *, #217147, .T. ) ;
#165617 = ORIENTED_EDGE ( 'NONE', *, *, #188842, .F. ) ;
#165618 = DIRECTION ( 'NONE',  ( 0.000000000000000000, 0.9126074666063660468, 0.4088369013363524762 ) ) ;
#165619 = ORIENTED_EDGE ( 'NONE', *, *, #234342, .F. ) ;
#165621 = VERTEX_POINT ( 'NONE', #211162 ) ;
#165620 = CARTESIAN_POINT ( 'NONE',  ( 18.59999999999999432, 77.16270174995064224, -195.4231074845243370 ) ) ;
#165622 = ORIENTED_EDGE ( 'NONE', *, *, #83930, .F. ) ;
#165624 = VERTEX_POINT ( 'NONE', #209891 ) ;
#165623 = ORIENTED_EDGE ( 'NONE', *, *, #91095, .T. ) ;
#165625 = CIRCLE ( 'NONE', #149062, 0.1000000000000028644 ) ;
#165626 = CARTESIAN_POINT ( 'NONE',  ( -18.49372193242250972, -9.442484523346742264, -107.2647812600345816 ) ) ;
#165627 = AXIS2_PLACEMENT_3D ( 'NONE', #87199, #23426, #166791 ) ;
#165628 = ORIENTED_EDGE ( 'NONE', *, *, #73020, .T. ) ;
#165629 = DIRECTION ( 'NONE',  ( -1.000000000000000000, 0.000000000000000000, 0.000000000000000000 ) ) ;
#165630 = CARTESIAN_POINT ( 'NONE',  ( -20.64999999999999858, 2.000000000011154189, -53.77537807723790309 ) ) ;
#165631 = DIRECTION ( 'NONE',  ( 0.000000000000000000, 0.2128009952263604510, -0.9770955615653315052 ) ) ;
#165632 = EDGE_CURVE ( 'NONE', #202498, #249506, #201689, .T. ) ;
#165633 = AXIS2_PLACEMENT_3D ( 'NONE', #76896, #14394, #113459 ) ;
#165634 = DIRECTION ( 'NONE',  ( -1.000000000000000000, -0.000000000000000000, -0.000000000000000000 ) ) ;
#165635 = EDGE_LOOP ( 'NONE', ( #249113, #83034, #244066, #75227, #177810 ) ) ;
#165636 = VERTEX_POINT ( 'NONE', #35131 ) ;
#165637 = CARTESIAN_POINT ( 'NONE',  ( 20.94999999999999574, 1.115600667400684642E-11, -167.4999999999999716 ) ) ;
#165639 = VERTEX_POINT ( 'NONE', #112076 ) ;
#165638 = CARTESIAN_POINT ( 'NONE',  ( -16.93589915522259304, 65.99137474131667602, -182.5825473825641438 ) ) ;
#165640 = CARTESIAN_POINT ( 'NONE',  ( -16.81095280782810875, 9.950000000011138823, -180.1499999999990962 ) ) ;
#165642 = ORIENTED_EDGE ( 'NONE', *, *, #195277, .T. ) ;
#165641 = DIRECTION ( 'NONE',  ( 1.000000000000000000, -0.000000000000000000, -0.000000000000000000 ) ) ;
#165643 = EDGE_CURVE ( 'NONE', #166612, #258034, #109475, .T. ) ;
#165644 = EDGE_CURVE ( 'NONE', #70458, #235860, #96877, .T. ) ;
#165645 = EDGE_LOOP ( 'NONE', ( #109107, #93116, #136355 ) ) ;
#165646 = CARTESIAN_POINT ( 'NONE',  ( -13.39999999999994529, 63.75000000001119815, -21.02310748452479316 ) ) ;
#165647 = EDGE_CURVE ( 'NONE', #165365, #152028, #130216, .T. ) ;
#165648 = EDGE_CURVE ( 'NONE', #221652, #120417, #161478, .T. ) ;
#165649 = ORIENTED_EDGE ( 'NONE', *, *, #99994, .F. ) ;
#165650 = ORIENTED_EDGE ( 'NONE', *, *, #201933, .F. ) ;
#165651 = CARTESIAN_POINT ( 'NONE',  ( 20.94999999999999929, 6.846123162363745074, -204.7377262668498190 ) ) ;
#165653 = EDGE_CURVE ( 'NONE', #187418, #165014, #238567, .T. ) ;
#165652 = DIRECTION ( 'NONE',  ( -1.000000000000000000, -0.000000000000000000, -0.000000000000000000 ) ) ;
#165654 = CIRCLE ( 'NONE', #236366, 0.09999999999999939493 ) ;
#165655 = ADVANCED_FACE ( 'NONE', ( #21960 ), #88510, .F. ) ;
#165656 = AXIS2_PLACEMENT_3D ( 'NONE', #110100, #127100, #9713 ) ;
#165658 = VERTEX_POINT ( 'NONE', #41532 ) ;
#165657 = ORIENTED_EDGE ( 'NONE', *, *, #162944, .F. ) ;
#165659 = ORIENTED_EDGE ( 'NONE', *, *, #222109, .T. ) ;
#165660 = CARTESIAN_POINT ( 'NONE',  ( -16.81744102076748959, 9.950000000011138823, -54.35000000000000142 ) ) ;
#165661 = ORIENTED_EDGE ( 'NONE', *, *, #247347, .T. ) ;
#165662 = ORIENTED_EDGE ( 'NONE', *, *, #138596, .T. ) ;
#165663 = ADVANCED_FACE ( 'NONE', ( #81878 ), #159469, .T. ) ;
#165664 = DIRECTION ( 'NONE',  ( 1.000000000000000000, -0.000000000000000000, -0.000000000000000000 ) ) ;
#165666 = ORIENTED_EDGE ( 'NONE', *, *, #115883, .T. ) ;
#165665 = CARTESIAN_POINT ( 'NONE',  ( 20.94999999999999929, 76.00000000001165290, -69.52310748452431710 ) ) ;
#165667 = CARTESIAN_POINT ( 'NONE',  ( 21.05000000000000071, -9.399999999988844834, -191.1060308773475072 ) ) ;
#165668 = CIRCLE ( 'NONE', #53216, 0.09999999999998898659 ) ;
#165670 = DIRECTION ( 'NONE',  ( 1.000000000000000000, 0.000000000000000000, 0.000000000000000000 ) ) ;
#165669 = DIRECTION ( 'NONE',  ( -1.000000000000000000, -0.000000000000000000, 0.000000000000000000 ) ) ;
#165671 = CYLINDRICAL_SURFACE ( 'NONE', #36660, 4.049999999999998046 ) ;
#165672 = CARTESIAN_POINT ( 'NONE',  ( -12.93407622233967658, 62.16167874586912490, -218.5680441376359795 ) ) ;
#165673 = ORIENTED_EDGE ( 'NONE', *, *, #40930, .T. ) ;
#165674 = ORIENTED_EDGE ( 'NONE', *, *, #175412, .F. ) ;
#165675 = AXIS2_PLACEMENT_3D ( 'NONE', #148521, #26010, #185070 ) ;
#165676 = DIRECTION ( 'NONE',  ( 0.000000000000000000, -0.4088369013363281068, 0.9126074666063770380 ) ) ;
#165677 = CARTESIAN_POINT ( 'NONE',  ( -23.49999999999994316, 87.50449464844290048, -37.85861909827351468 ) ) ;
#165678 = ORIENTED_EDGE ( 'NONE', *, *, #101379, .T. ) ;
#165679 = VECTOR ( 'NONE', #181908, 1000.000000000000000 ) ;
#165680 = AXIS2_PLACEMENT_3D ( 'NONE', #14965, #73667, #94471 ) ;
#165681 = AXIS2_PLACEMENT_3D ( 'NONE', #37254, #214574, #15112 ) ;
#165682 = EDGE_CURVE ( 'NONE', #133293, #161458, #221787, .T. ) ;
#165683 = CARTESIAN_POINT ( 'NONE',  ( 23.24999999999999289, 6.450000000011156587, -88.15000000000004832 ) ) ;
#165684 = CIRCLE ( 'NONE', #44858, 12.87499999999999822 ) ;
#165685 = VERTEX_POINT ( 'NONE', #36402 ) ;
#165686 = ORIENTED_EDGE ( 'NONE', *, *, #252058, .F. ) ;
#165687 = DIRECTION ( 'NONE',  ( 0.000000000000000000, -6.853228547068871147E-15, 1.000000000000000000 ) ) ;
#165688 = AXIS2_PLACEMENT_3D ( 'NONE', #231483, #52815, #132366 ) ;
#165689 = FACE_OUTER_BOUND ( 'NONE', #56121, .T. ) ;
#165691 = ADVANCED_FACE ( 'NONE', ( #136743 ), #118496, .T. ) ;
#165690 = VERTEX_POINT ( 'NONE', #98878 ) ;
#165692 = CARTESIAN_POINT ( 'NONE',  ( -21.12844524849339223, 11.75000000001115197, -107.4044134708428260 ) ) ;
#165693 = LINE ( 'NONE', #129113, #93599 ) ;
#165694 = VERTEX_POINT ( 'NONE', #1068 ) ;
#165695 = EDGE_CURVE ( 'NONE', #61015, #117533, #193332, .T. ) ;
#165696 = DIRECTION ( 'NONE',  ( 0.000000000000000000, -0.1575844902526579161, -0.9875055080513779338 ) ) ;
#165697 = DIRECTION ( 'NONE',  ( 0.000000000000000000, 0.000000000000000000, 1.000000000000000000 ) ) ;
#165698 = CARTESIAN_POINT ( 'NONE',  ( 23.14999999999998437, -4.049999999988842525, -134.0000000000000000 ) ) ;
#165699 = DIRECTION ( 'NONE',  ( -1.000000000000000000, 0.000000000000000000, 0.000000000000000000 ) ) ;
#165700 = CARTESIAN_POINT ( 'NONE',  ( -21.05000000000000071, -1.249999999988843369, -142.0000000000000284 ) ) ;
#165701 = DIRECTION ( 'NONE',  ( 0.000000000000000000, -1.000000000000000000, 0.000000000000000000 ) ) ;
#165702 = TOROIDAL_SURFACE ( 'NONE', #124178, 0.6000000000000004219, 0.1000000000000000056 ) ;
#165703 = ORIENTED_EDGE ( 'NONE', *, *, #104116, .T. ) ;
#165704 = AXIS2_PLACEMENT_3D ( 'NONE', #77401, #156986, #137381 ) ;
#165707 = ORIENTED_EDGE ( 'NONE', *, *, #46479, .F. ) ;
#165706 = ORIENTED_EDGE ( 'NONE', *, *, #213221, .T. ) ;
#165705 = CIRCLE ( 'NONE', #61627, 0.2000000000000057288 ) ;
#165708 = VERTEX_POINT ( 'NONE', #76776 ) ;
#165709 = PRESENTATION_LAYER_ASSIGNMENT (  '', '', ( #15689 ) ) ;
#165710 = CIRCLE ( 'NONE', #111516, 0.1000000000000013933 ) ;
#165711 = FACE_OUTER_BOUND ( 'NONE', #233346, .T. ) ;
#165712 = CARTESIAN_POINT ( 'NONE',  ( 18.50000000000000000, 85.40000000001263913, -196.5238218066854472 ) ) ;
#165713 = AXIS2_PLACEMENT_3D ( 'NONE', #10029, #132549, #153440 ) ;
#165714 = CARTESIAN_POINT ( 'NONE',  ( -17.11825945287482753, 10.05000000001113847, -146.6500000000000341 ) ) ;
#165715 = CARTESIAN_POINT ( 'NONE',  ( 21.05000000000000071, 67.12338541492520960, -161.6380270056797599 ) ) ;
#165716 = ORIENTED_EDGE ( 'NONE', *, *, #220957, .F. ) ;
#165717 = CYLINDRICAL_SURFACE ( 'NONE', #63462, 0.09999999999999781286 ) ;
#165718 = CARTESIAN_POINT ( 'NONE',  ( -21.09096482362056690, 0.03944827877415432726, 6.363544365404331771 ) ) ;
#165719 = CARTESIAN_POINT ( 'NONE',  ( -16.90137573187934095, 66.05000000001189164, -90.23469006042749641 ) ) ;
#165720 = CARTESIAN_POINT ( 'NONE',  ( -16.90987985657661596, 9.957807518190884721, -87.86928708888368078 ) ) ;
#165721 = ORIENTED_EDGE ( 'NONE', *, *, #14037, .T. ) ;
#165722 = VECTOR ( 'NONE', #239130, 1000.000000000000000 ) ;
#165723 = AXIS2_PLACEMENT_3D ( 'NONE', #28431, #3679, #6240 ) ;
#165724 = CIRCLE ( 'NONE', #53281, 0.09999999999999939493 ) ;
#165725 = DIRECTION ( 'NONE',  ( 0.000000000000000000, 0.000000000000000000, 1.000000000000000000 ) ) ;
#165726 = DIRECTION ( 'NONE',  ( -1.000000000000000000, -0.000000000000000000, -0.000000000000000000 ) ) ;
#165727 = ORIENTED_EDGE ( 'NONE', *, *, #84352, .T. ) ;
#165728 = ORIENTED_EDGE ( 'NONE', *, *, #229780, .T. ) ;
#165729 = LINE ( 'NONE', #67887, #58169 ) ;
#165730 = CARTESIAN_POINT ( 'NONE',  ( -20.94999999999999929, 64.35000000001176090, -76.30697314750248950 ) ) ;
#165731 = CARTESIAN_POINT ( 'NONE',  ( -23.25000000000000000, 76.00000000001168132, -73.57310748452432847 ) ) ;
#165732 = DIRECTION ( 'NONE',  ( -1.000000000000000000, -0.000000000000000000, -0.000000000000000000 ) ) ;
#165733 = FACE_OUTER_BOUND ( 'NONE', #430, .T. ) ;
#165734 = CARTESIAN_POINT ( 'NONE',  ( 20.85000000000000142, 87.75000000001246292, -172.9231074845242802 ) ) ;
#165735 = ORIENTED_EDGE ( 'NONE', *, *, #143369, .F. ) ;
#165736 = CARTESIAN_POINT ( 'NONE',  ( 20.94999999999999574, 77.36087058720364951, -61.45010955743335046 ) ) ;
#165737 = CARTESIAN_POINT ( 'NONE',  ( 20.95512820512820085, 12.01161663143393454, -206.2285874551107554 ) ) ;
#165738 = CIRCLE ( 'NONE', #111543, 0.4000000000000010214 ) ;
#165739 = EDGE_CURVE ( 'NONE', #32893, #56802, #63584, .T. ) ;
#165741 = CARTESIAN_POINT ( 'NONE',  ( -21.00448002041607864, 11.75000000001115552, -174.3483408623104935 ) ) ;
#165740 = DIRECTION ( 'NONE',  ( 1.000000000000000000, 0.000000000000000000, 0.000000000000000000 ) ) ;
#165742 = DIRECTION ( 'NONE',  ( 1.000000000000000000, -0.000000000000000000, -0.000000000000000000 ) ) ;
#165743 = CARTESIAN_POINT ( 'NONE',  ( -20.85000000000000142, 67.49222854868494892, -195.4187676019683693 ) ) ;
#165745 = EDGE_CURVE ( 'NONE', #212748, #147427, #146775, .T. ) ;
#165744 = CARTESIAN_POINT ( 'NONE',  ( -23.15000000000000213, 11.65000000001115588, -155.3500000000000227 ) ) ;
#165747 = DIRECTION ( 'NONE',  ( -1.000000000000000000, 3.389981217840264988E-14, 7.383017642607961770E-15 ) ) ;
#165746 = CIRCLE ( 'NONE', #182293, 0.4000000000000114575 ) ;
#165749 = ORIENTED_EDGE ( 'NONE', *, *, #142869, .T. ) ;
#165748 = CARTESIAN_POINT ( 'NONE',  ( 21.53752568622180874, 30.42476846892407139, -252.2355353702193668 ) ) ;
#165750 = TOROIDAL_SURFACE ( 'NONE', #219878, 11.65000000000000036, 0.1000000000000000056 ) ;
#165751 = EDGE_CURVE ( 'NONE', #38916, #217539, #17777, .T. ) ;
#165752 = ADVANCED_FACE ( 'NONE', ( #40253 ), #117761, .T. ) ;
#165753 = AXIS2_PLACEMENT_3D ( 'NONE', #161134, #24201, #5883 ) ;
#165754 = CARTESIAN_POINT ( 'NONE',  ( 23.15000000000000213, -8.999999999988844479, -177.3939691226524076 ) ) ;
#165755 = AXIS2_PLACEMENT_3D ( 'NONE', #7292, #125950, #106376 ) ;
#165756 = CIRCLE ( 'NONE', #182311, 4.150000000000001243 ) ;
#165757 = CARTESIAN_POINT ( 'NONE',  ( 21.07928932188134397, 65.47931918658503037, -241.9371126717015841 ) ) ;
#165758 = AXIS2_PLACEMENT_3D ( 'NONE', #73527, #213001, #192178 ) ;
#165759 = CARTESIAN_POINT ( 'NONE',  ( 21.07016717457010202, 65.57674933587217936, -241.9556870860043603 ) ) ;
#165760 = ORIENTED_EDGE ( 'NONE', *, *, #187616, .F. ) ;
#165761 = EDGE_CURVE ( 'NONE', #137090, #193211, #58477, .T. ) ;
#165762 = CARTESIAN_POINT ( 'NONE',  ( -20.64999999999999858, 76.00000000001213607, -136.5231074845242745 ) ) ;
#165763 = EDGE_CURVE ( 'NONE', #29920, #227881, #101428, .T. ) ;
#165764 = CARTESIAN_POINT ( 'NONE',  ( -20.85000000000000142, 76.00000000001213607, -136.5231074845243313 ) ) ;
#165765 = CARTESIAN_POINT ( 'NONE',  ( 18.59999999999998721, 6.933893972126341509, -37.28564583437357527 ) ) ;
#165766 = ORIENTED_EDGE ( 'NONE', *, *, #69756, .F. ) ;
#165767 = CARTESIAN_POINT ( 'NONE',  ( 21.05000000000000071, 67.63082410804655353, -211.8415745842588649 ) ) ;
#165769 = ORIENTED_EDGE ( 'NONE', *, *, #17112, .T. ) ;
#165768 = LINE ( 'NONE', #203585, #63418 ) ;
#165771 = DIRECTION ( 'NONE',  ( 1.000000000000000000, 0.000000000000000000, 0.000000000000000000 ) ) ;
#165770 = CARTESIAN_POINT ( 'NONE',  ( -20.54999999999999716, -8.999999999988846255, -143.3939691226524644 ) ) ;
#165772 = CARTESIAN_POINT ( 'NONE',  ( -17.71734398241073905, 10.84235722847571814, -144.2748617469944463 ) ) ;
#165773 = ORIENTED_EDGE ( 'NONE', *, *, #216960, .T. ) ;
#165774 = CARTESIAN_POINT ( 'NONE',  ( -16.87683809663750623, 66.05000000001261640, -190.1207434663279230 ) ) ;
#165775 = AXIS2_PLACEMENT_3D ( 'NONE', #187008, #227388, #116121 ) ;
#165776 = DIRECTION ( 'NONE',  ( 0.000000000000000000, 0.000000000000000000, 1.000000000000000000 ) ) ;
#165777 = DIRECTION ( 'NONE',  ( 0.000000000000000000, 0.000000000000000000, 1.000000000000000000 ) ) ;
#165778 = ADVANCED_FACE ( 'NONE', ( #235845 ), #42745, .T. ) ;
#165779 = DIRECTION ( 'NONE',  ( -3.890533409366484652E-14, 0.1298341882520054891, 0.9915357197604850459 ) ) ;
#165780 = LINE ( 'NONE', #218315, #150421 ) ;
#165781 = ORIENTED_EDGE ( 'NONE', *, *, #52830, .T. ) ;
#165782 = CARTESIAN_POINT ( 'NONE',  ( -14.00000000000000178, 66.15000000001204228, -119.7731074845243739 ) ) ;
#165783 = DIRECTION ( 'NONE',  ( 0.7071067811865388020, -0.7071067811865561215, 0.000000000000000000 ) ) ;
#165784 = ADVANCED_FACE ( 'NONE', ( #42795 ), #189686, .T. ) ;
#165785 = CIRCLE ( 'NONE', #86619, 0.09999999999998898659 ) ;
#165786 = CARTESIAN_POINT ( 'NONE',  ( -22.49756042579671700, 0.07804633702833754794, -122.3501350388976903 ) ) ;
#165787 = ORIENTED_EDGE ( 'NONE', *, *, #22693, .F. ) ;
#165788 = ORIENTED_EDGE ( 'NONE', *, *, #203704, .T. ) ;
#165789 = ADVANCED_FACE ( 'NONE', ( #226200 ), #151087, .T. ) ;
#165790 = DIRECTION ( 'NONE',  ( -1.000000000000000000, 2.952720810173289112E-16, 2.061873921506763405E-30 ) ) ;
#165791 = ADVANCED_FACE ( 'NONE', ( #188394 ), #201864, .F. ) ;
#165792 = DIRECTION ( 'NONE',  ( 1.000000000000000000, -7.304098846218134667E-16, -0.000000000000000000 ) ) ;
#165793 = DIRECTION ( 'NONE',  ( 0.000000000000000000, -0.1350103645451807555, -0.9908441862701609093 ) ) ;
#165794 = CARTESIAN_POINT ( 'NONE',  ( 21.05000000000000071, 10.47338541492405284, -141.5786544642485580 ) ) ;
#165795 = CARTESIAN_POINT ( 'NONE',  ( 20.97462148592277842, 8.874737576461731337, -146.2546443317310434 ) ) ;
#165797 = CARTESIAN_POINT ( 'NONE',  ( -20.94999999999999929, 64.35000000001195986, -109.8069731475024753 ) ) ;
#165796 = CARTESIAN_POINT ( 'NONE',  ( -20.54999999999999716, 85.00000000001197975, -112.5170766071766764 ) ) ;
#165798 = EDGE_CURVE ( 'NONE', #27481, #493, #5304, .T. ) ;
#165799 = AXIS2_PLACEMENT_3D ( 'NONE', #220631, #61556, #103221 ) ;
#165800 = CIRCLE ( 'NONE', #132078, 0.9750000000000036415 ) ;
#165802 = DIRECTION ( 'NONE',  ( 0.000000000000000000, -0.9651348961777157509, 0.2617529984165031243 ) ) ;
#165801 = AXIS2_PLACEMENT_3D ( 'NONE', #175581, #236809, #38626 ) ;
#165803 = CARTESIAN_POINT ( 'NONE',  ( -16.91247567987037570, 9.959082683680399839, -113.1287244585373770 ) ) ;
#165804 = VECTOR ( 'NONE', #243038, 1000.000000000000000 ) ;
#165805 = FACE_OUTER_BOUND ( 'NONE', #62593, .T. ) ;
#165806 = CARTESIAN_POINT ( 'NONE',  ( -18.59999999999999787, 77.83534155023700407, -191.9679561919613491 ) ) ;
#165807 = ORIENTED_EDGE ( 'NONE', *, *, #7650, .T. ) ;
#165808 = CARTESIAN_POINT ( 'NONE',  ( -20.94999999999999929, 1.115600667400684642E-11, -108.4000000000000341 ) ) ;
#165809 = DIRECTION ( 'NONE',  ( 0.000000000000000000, -1.000000000000000000, 0.000000000000000000 ) ) ;
#165811 = DIRECTION ( 'NONE',  ( -0.000000000000000000, 0.9770955615653313941, 0.2128009952263603677 ) ) ;
#165810 = CARTESIAN_POINT ( 'NONE',  ( -16.98495255085917321, 14.21656675727647468, -219.2582788632799975 ) ) ;
#165812 = VERTEX_POINT ( 'NONE', #50156 ) ;
#165813 = LINE ( 'NONE', #110951, #151767 ) ;
#165814 = DIRECTION ( 'NONE',  ( 1.000000000000000000, 0.000000000000000000, 0.000000000000000000 ) ) ;
#165815 = EDGE_CURVE ( 'NONE', #155635, #68804, #38846, .T. ) ;
#165816 = DIRECTION ( 'NONE',  ( -1.000000000000000000, 0.000000000000000000, 0.000000000000000000 ) ) ;
#165817 = DIRECTION ( 'NONE',  ( 0.000000000000000000, 0.000000000000000000, 1.000000000000000000 ) ) ;
#165818 = CARTESIAN_POINT ( 'NONE',  ( 22.49533356619858182, 12.57247511773154258, -223.4325311539369068 ) ) ;
#165819 = ORIENTED_EDGE ( 'NONE', *, *, #83952, .F. ) ;
#165820 = ORIENTED_EDGE ( 'NONE', *, *, #238648, .F. ) ;
#165821 = ADVANCED_FACE ( 'NONE', ( #128427 ), #159646, .T. ) ;
#165822 = TOROIDAL_SURFACE ( 'NONE', #95050, 0.4000000000000012990, 0.1000000000000000056 ) ;
#165824 = AXIS2_PLACEMENT_3D ( 'NONE', #67025, #190861, #167435 ) ;
#165823 = CARTESIAN_POINT ( 'NONE',  ( -15.55912972643740488, 8.490870273573721150, -154.9500000000000455 ) ) ;
#165825 = VERTEX_POINT ( 'NONE', #87985 ) ;
#165826 = CARTESIAN_POINT ( 'NONE',  ( 21.14999999999999858, 64.35000000001164722, -69.42310748452440805 ) ) ;
#165827 = ORIENTED_EDGE ( 'NONE', *, *, #110011, .F. ) ;
#165829 = CARTESIAN_POINT ( 'NONE',  ( 20.94999999999999929, 10.72371710471868056, -179.6499999999999773 ) ) ;
#165828 = AXIS2_PLACEMENT_3D ( 'NONE', #110803, #212493, #213757 ) ;
#165830 = FACE_OUTER_BOUND ( 'NONE', #228980, .T. ) ;
#165831 = CARTESIAN_POINT ( 'NONE',  ( -21.05315837191484363, 62.86884414000814303, -207.0506191381281837 ) ) ;
#165832 = ORIENTED_EDGE ( 'NONE', *, *, #200142, .T. ) ;
#165833 = DIRECTION ( 'NONE',  ( 0.000000000000000000, -8.338584948901395817E-15, 1.000000000000000000 ) ) ;
#165834 = CARTESIAN_POINT ( 'NONE',  ( -23.49999999999994316, 74.83745509109094485, -43.92310748452479885 ) ) ;
#165835 = DIRECTION ( 'NONE',  ( 1.000000000000000000, 0.000000000000000000, 0.000000000000000000 ) ) ;
#165836 = DIRECTION ( 'NONE',  ( 1.000000000000000000, -0.000000000000000000, -0.000000000000000000 ) ) ;
#165837 = DIRECTION ( 'NONE',  ( 0.000000000000000000, -0.7071067811865472397, -0.7071067811865479058 ) ) ;
#165838 = DIRECTION ( 'NONE',  ( -1.000000000000000000, 0.000000000000000000, 0.000000000000000000 ) ) ;
#165839 = CARTESIAN_POINT ( 'NONE',  ( 21.13920837816993270, 11.18888390033836266, -211.1003369155923224 ) ) ;
#165840 = AXIS2_PLACEMENT_3D ( 'NONE', #152264, #250054, #231788 ) ;
#165841 = EDGE_LOOP ( 'NONE', ( #18049, #247372, #121944, #183406 ) ) ;
#165843 = DIRECTION ( 'NONE',  ( 0.000000000000000000, 0.000000000000000000, 1.000000000000000000 ) ) ;
#165842 = DIRECTION ( 'NONE',  ( 1.000000000000000000, 0.000000000000000000, 0.000000000000000000 ) ) ;
#165844 = ORIENTED_EDGE ( 'NONE', *, *, #117955, .F. ) ;
#165845 = VERTEX_POINT ( 'NONE', #89286 ) ;
#165846 = ORIENTED_EDGE ( 'NONE', *, *, #200111, .T. ) ;
#165847 = CARTESIAN_POINT ( 'NONE',  ( 21.14999999999999503, 1.115600667400684642E-11, -27.25000000000000355 ) ) ;
#165848 = CARTESIAN_POINT ( 'NONE',  ( -23.25000000000000000, 70.85002333954264486, -215.2140597723681879 ) ) ;
#165849 = CARTESIAN_POINT ( 'NONE',  ( 18.49999999999999289, 65.74999999739273449, -78.33593553489180294 ) ) ;
#165850 = CARTESIAN_POINT ( 'NONE',  ( 21.05000000000000071, 76.00000000001170974, -69.52310748452431710 ) ) ;
#165851 = ORIENTED_EDGE ( 'NONE', *, *, #159680, .F. ) ;
#165852 = LINE ( 'NONE', #244076, #72238 ) ;
#165853 = AXIS2_PLACEMENT_3D ( 'NONE', #178980, #177686, #17313 ) ;
#165854 = CARTESIAN_POINT ( 'NONE',  ( 18.52928932188133970, 10.27928932189250055, -158.6500000000000057 ) ) ;
#165855 = ORIENTED_EDGE ( 'NONE', *, *, #96995, .T. ) ;
#165856 = CARTESIAN_POINT ( 'NONE',  ( 18.59999999999999076, 6.450000000011156587, -177.5170271704400022 ) ) ;
#165857 = ADVANCED_FACE ( 'NONE', ( #9754 ), #246928, .T. ) ;
#165858 = DIRECTION ( 'NONE',  ( 1.000000000000000000, 0.000000000000000000, 0.000000000000000000 ) ) ;
#165859 = AXIS2_PLACEMENT_3D ( 'NONE', #116210, #58756, #176184 ) ;
#165860 = ORIENTED_EDGE ( 'NONE', *, *, #198572, .F. ) ;
#165861 = VECTOR ( 'NONE', #72068, 1000.000000000000000 ) ;
#165862 = DIRECTION ( 'NONE',  ( 1.000000000000000000, 0.000000000000000000, 0.000000000000000000 ) ) ;
#165863 = AXIS2_PLACEMENT_3D ( 'NONE', #240572, #63197, #141466 ) ;
#165864 = VERTEX_POINT ( 'NONE', #3654 ) ;
#165865 = PLANE ( 'NONE',  #42345 ) ;
#165867 = EDGE_LOOP ( 'NONE', ( #158613, #209483, #243842, #57833 ) ) ;
#165866 = AXIS2_PLACEMENT_3D ( 'NONE', #79788, #117658, #95524 ) ;
#165868 = DIRECTION ( 'NONE',  ( -0.7071067811865562325, -0.7071067811865388020, 0.000000000000000000 ) ) ;
#165869 = ADVANCED_FACE ( 'NONE', ( #248373 ), #83158, .T. ) ;
#165870 = DIRECTION ( 'NONE',  ( -1.000000000000000000, 0.000000000000000000, -0.000000000000000000 ) ) ;
#165872 = CARTESIAN_POINT ( 'NONE',  ( 19.75857864376268935, 16.64998792410002793, -222.7039835543563981 ) ) ;
#165871 = APPLICATION_CONTEXT ( 'automotive_design' ) ;
#165873 = DIRECTION ( 'NONE',  ( 0.000000000000000000, 0.5000000000000209832, -0.8660254037844264952 ) ) ;
#165874 = EDGE_CURVE ( 'NONE', #231942, #213725, #255255, .T. ) ;
#165875 = EDGE_CURVE ( 'NONE', #219246, #146247, #32759, .T. ) ;
#165876 = AXIS2_PLACEMENT_3D ( 'NONE', #83664, #22476, #100667 ) ;
#165877 = DIRECTION ( 'NONE',  ( -1.000000000000000000, 0.000000000000000000, 0.000000000000000000 ) ) ;
#165878 = DIRECTION ( 'NONE',  ( 0.000000000000000000, 0.1575844902526876978, 0.9875055080513731598 ) ) ;
#165880 = CARTESIAN_POINT ( 'NONE',  ( 20.94999675878240808, 10.29307482169070909, -72.45864214669403225 ) ) ;
#165879 = AXIS2_PLACEMENT_3D ( 'NONE', #43133, #97928, #22301 ) ;
#165881 = EDGE_LOOP ( 'NONE', ( #213337, #195624, #182928, #138045 ) ) ;
#165883 = CARTESIAN_POINT ( 'NONE',  ( 20.94999999999999929, 68.48451787451661232, -224.2224406095231757 ) ) ;
#165882 = CARTESIAN_POINT ( 'NONE',  ( -21.05000000000000071, 64.23744694032046709, -224.5446448091673233 ) ) ;
#165884 = VECTOR ( 'NONE', #186856, 1000.000000000000000 ) ;
#165885 = ORIENTED_EDGE ( 'NONE', *, *, #19837, .T. ) ;
#165886 = AXIS2_PLACEMENT_3D ( 'NONE', #137078, #216610, #217871 ) ;
#165887 = CIRCLE ( 'NONE', #136817, 0.09999999999999867328 ) ;
#165888 = FACE_OUTER_BOUND ( 'NONE', #40064, .T. ) ;
#165889 = FACE_OUTER_BOUND ( 'NONE', #200398, .T. ) ;
#165890 = ADVANCED_FACE ( 'NONE', ( #230091 ), #241000, .F. ) ;
#165891 = CARTESIAN_POINT ( 'NONE',  ( -16.94445028196808778, 60.88759175473954599, -221.0718995934454938 ) ) ;
#165894 = ORIENTED_EDGE ( 'NONE', *, *, #122605, .T. ) ;
#165893 = DIRECTION ( 'NONE',  ( 0.000000000000000000, -0.000000000000000000, 1.000000000000000000 ) ) ;
#165892 =( BOUNDED_CURVE ( )  B_SPLINE_CURVE ( 3, ( #129861, #109012, #251088, #167747 ),
 .UNSPECIFIED., .F., .F. ) 
 B_SPLINE_CURVE_WITH_KNOTS ( ( 4, 4 ),
 ( 3.141592653589793116, 4.712388980384689674 ),
 .UNSPECIFIED. ) 
 CURVE ( )  GEOMETRIC_REPRESENTATION_ITEM ( )  RATIONAL_B_SPLINE_CURVE ( ( 1.000000000000000000, 0.8047378541243649375, 0.8047378541243649375, 1.000000000000000000 ) ) 
 REPRESENTATION_ITEM ( '' )  );
#165896 = ORIENTED_EDGE ( 'NONE', *, *, #67359, .F. ) ;
#165895 = CARTESIAN_POINT ( 'NONE',  ( -23.25000000000000000, 7.668827189579289438, -241.6142244293585009 ) ) ;
#165897 = ADVANCED_FACE ( 'NONE', ( #215649 ), #73618, .T. ) ;
#165898 = AXIS2_PLACEMENT_3D ( 'NONE', #142830, #24219, #103706 ) ;
#165899 = FILL_AREA_STYLE ('',( #105870 ) ) ;
#165900 = CARTESIAN_POINT ( 'NONE',  ( -20.10000000000000142, 5.572697453181475247, 16.49970471148372297 ) ) ;
#165901 = CARTESIAN_POINT ( 'NONE',  ( 19.97071067811865319, 64.27928932189354327, -145.3145288407617386 ) ) ;
#165903 = ORIENTED_EDGE ( 'NONE', *, *, #33345, .T. ) ;
#165902 = DIRECTION ( 'NONE',  ( 0.000000000000000000, -6.789366196018718420E-15, 1.000000000000000000 ) ) ;
#165904 = PRODUCT_DEFINITION_SHAPE ( 'NONE', 'NONE',  #179166 ) ;
#165905 = CIRCLE ( 'NONE', #53459, 0.3999999999999975797 ) ;
#165906 = VECTOR ( 'NONE', #64407, 1000.000000000000000 ) ;
#165907 = CARTESIAN_POINT ( 'NONE',  ( 22.49999999999999645, 11.64957080755595520, -167.3999999999999773 ) ) ;
#165909 = AXIS2_PLACEMENT_3D ( 'NONE', #222920, #183805, #63860 ) ;
#165908 = DIRECTION ( 'NONE',  ( 0.000000000000000000, 0.9964539953858966292, 0.08413937888696132461 ) ) ;
#165910 = ORIENTED_EDGE ( 'NONE', *, *, #223347, .F. ) ;
#165911 = CARTESIAN_POINT ( 'NONE',  ( -20.54999999999999716, 74.00000000001199396, -116.2477294072864140 ) ) ;
#165912 = EDGE_CURVE ( 'NONE', #70728, #76759, #52726, .T. ) ;
#165913 = ORIENTED_EDGE ( 'NONE', *, *, #93029, .F. ) ;
#165914 = CARTESIAN_POINT ( 'NONE',  ( 20.85000000000000142, 76.00000000001213607, -136.5231074845243313 ) ) ;
#165915 = DIRECTION ( 'NONE',  ( 0.000000000000000000, 0.000000000000000000, -1.000000000000000000 ) ) ;
#165916 = EDGE_LOOP ( 'NONE', ( #69953, #236495, #147246, #116049 ) ) ;
#165917 = DIRECTION ( 'NONE',  ( 1.000000000000000000, 0.000000000000000000, 0.000000000000000000 ) ) ;
#165918 = AXIS2_PLACEMENT_3D ( 'NONE', #53125, #234324, #115675 ) ;
#165919 = CIRCLE ( 'NONE', #232568, 11.74999999999999645 ) ;
#165921 = EDGE_CURVE ( 'NONE', #95915, #201984, #72175, .T. ) ;
#165920 = LINE ( 'NONE', #62939, #228441 ) ;
#165923 = VERTEX_POINT ( 'NONE', #132272 ) ;
#165922 = AXIS2_PLACEMENT_3D ( 'NONE', #99366, #281, #235062 ) ;
#165924 = CARTESIAN_POINT ( 'NONE',  ( -20.94999999999999929, -1.851028230129704522, -112.1539132694225316 ) ) ;
#165925 = AXIS2_PLACEMENT_3D ( 'NONE', #221764, #5282, #123993 ) ;
#165926 = VERTEX_POINT ( 'NONE', #236503 ) ;
#165927 = ORIENTED_EDGE ( 'NONE', *, *, #23608, .T. ) ;
#165928 = DIRECTION ( 'NONE',  ( 1.000000000000000000, 0.000000000000000000, 0.000000000000000000 ) ) ;
#165929 = VERTEX_POINT ( 'NONE', #35770 ) ;
#165930 = CARTESIAN_POINT ( 'NONE',  ( -16.81453046979150301, 23.02733327219609905, -230.9738165231199218 ) ) ;
#165931 = ORIENTED_EDGE ( 'NONE', *, *, #71599, .F. ) ;
#165933 = EDGE_LOOP ( 'NONE', ( #9063, #137690, #17517, #28108 ) ) ;
#165932 = CARTESIAN_POINT ( 'NONE',  ( -21.65000000000000213, 68.75000000001161027, -60.27310748452437394 ) ) ;
#165934 = CIRCLE ( 'NONE', #232583, 0.09999999999998898659 ) ;
#165935 = CARTESIAN_POINT ( 'NONE',  ( -20.94684162602228028, 11.75000000001115374, -73.84164399907105292 ) ) ;
#165936 = EDGE_LOOP ( 'NONE', ( #66891, #141075, #138009, #176544, #252921, #241409, #255724 ) ) ;
#165937 = EDGE_CURVE ( 'NONE', #120222, #58764, #176229, .T. ) ;
#165938 = DIRECTION ( 'NONE',  ( 1.000000000000000000, 0.000000000000000000, 0.000000000000000000 ) ) ;
#165939 = AXIS2_PLACEMENT_3D ( 'NONE', #219605, #82640, #60531 ) ;
#165940 = CIRCLE ( 'NONE', #161850, 0.09999999999999520384 ) ;
#165941 = ORIENTED_EDGE ( 'NONE', *, *, #227253, .T. ) ;
#165943 = ORIENTED_EDGE ( 'NONE', *, *, #5792, .F. ) ;
#165942 = EDGE_LOOP ( 'NONE', ( #161594, #125204, #217136, #21602 ) ) ;
#165944 = CARTESIAN_POINT ( 'NONE',  ( -21.05000000000000071, 47.95459712139159336, -246.5019368548292675 ) ) ;
#165945 = AXIS2_PLACEMENT_3D ( 'NONE', #120708, #82795, #222312 ) ;
#165946 = DIRECTION ( 'NONE',  ( 0.000000000000000000, 0.000000000000000000, -1.000000000000000000 ) ) ;
#165947 = ORIENTED_EDGE ( 'NONE', *, *, #54977, .T. ) ;
#165948 = VECTOR ( 'NONE', #240351, 1000.000000000000000 ) ;
#165949 = EDGE_CURVE ( 'NONE', #45034, #240562, #38326, .T. ) ;
#165950 = EDGE_CURVE ( 'NONE', #237061, #148456, #47190, .T. ) ;
#165951 = VERTEX_POINT ( 'NONE', #94423 ) ;
#165952 = CARTESIAN_POINT ( 'NONE',  ( 21.05000000000000071, -11.74999999999999112, -30.39999999999999858 ) ) ;
#165953 = DIRECTION ( 'NONE',  ( 0.000000000000000000, 0.000000000000000000, 1.000000000000000000 ) ) ;
#165955 = VERTEX_POINT ( 'NONE', #95704 ) ;
#165954 = CARTESIAN_POINT ( 'NONE',  ( -18.59999999999999787, 38.23914636435921466, -236.1324109481172968 ) ) ;
#165956 = CYLINDRICAL_SURFACE ( 'NONE', #127184, 0.09999999999999868716 ) ;
#165957 = ORIENTED_EDGE ( 'NONE', *, *, #35205, .F. ) ;
#165958 = ADVANCED_FACE ( 'NONE', ( #115277 ), #153168, .T. ) ;
#165960 = ADVANCED_FACE ( 'NONE', ( #192268 ), #13619, .F. ) ;
#165959 = CARTESIAN_POINT ( 'NONE',  ( 21.72449340488910252, 10.28395627750227526, -109.7500000000000426 ) ) ;
#165961 = DIRECTION ( 'NONE',  ( 0.000000000000000000, -1.000000000000000000, 0.000000000000000000 ) ) ;
#165962 = CIRCLE ( 'NONE', #107666, 11.74999999999999645 ) ;
#165963 = ORIENTED_EDGE ( 'NONE', *, *, #156553, .T. ) ;
#165964 = DIRECTION ( 'NONE',  ( 0.000000000000000000, -0.9126074666063660468, -0.4088369013363524762 ) ) ;
#165965 = CARTESIAN_POINT ( 'NONE',  ( 20.94999999999999574, 46.45388641681647357, -243.1520440498138385 ) ) ;
#165966 = EDGE_CURVE ( 'NONE', #194066, #172696, #133557, .T. ) ;
#165967 = ORIENTED_EDGE ( 'NONE', *, *, #97070, .T. ) ;
#165968 = CARTESIAN_POINT ( 'NONE',  ( -22.50000000000000000, 76.00000000001213607, -136.5231074845242745 ) ) ;
#165969 = EDGE_LOOP ( 'NONE', ( #51635, #220816, #102388, #136841, #105505 ) ) ;
#165970 = EDGE_CURVE ( 'NONE', #85340, #71686, #172166, .T. ) ;
#165972 = EDGE_CURVE ( 'NONE', #15940, #108252, #242844, .T. ) ;
#165971 = EDGE_CURVE ( 'NONE', #100336, #62026, #130414, .T. ) ;
#165973 = B_SPLINE_CURVE_WITH_KNOTS ( 'NONE', 3,
 ( #42486, #43782, #125870, #102430, #185854, #7202, #161167, #3344 ),
 .UNSPECIFIED., .F., .F.,
 ( 4, 2, 2, 4 ),
 ( 0.000000000000000000, 9.550056980125360177E-05, 0.0001910011396025072035, 0.0003820022792049716353 ),
 .UNSPECIFIED. ) ;
#165975 = EDGE_LOOP ( 'NONE', ( #256148, #240664 ) ) ;
#165974 = EDGE_LOOP ( 'NONE', ( #156923, #2994, #240528, #120427, #239283 ) ) ;
#165976 = VERTEX_POINT ( 'NONE', #193547 ) ;
#165977 = CARTESIAN_POINT ( 'NONE',  ( 20.94999999999999929, -1.164121893230052995, -74.91484808557160591 ) ) ;
#165978 = ORIENTED_EDGE ( 'NONE', *, *, #69228, .T. ) ;
#165979 = CARTESIAN_POINT ( 'NONE',  ( -20.94999999999999929, 46.53760404070597900, -243.0973507280067167 ) ) ;
#165980 = ORIENTED_EDGE ( 'NONE', *, *, #245685, .F. ) ;
#165981 = FACE_OUTER_BOUND ( 'NONE', #34378, .T. ) ;
#165982 = CARTESIAN_POINT ( 'NONE',  ( -21.05000000000000071, 87.41227409416181615, -133.5231074845242176 ) ) ;
#165983 = ORIENTED_EDGE ( 'NONE', *, *, #237694, .F. ) ;
#165984 = EDGE_CURVE ( 'NONE', #65772, #190642, #192976, .T. ) ;
#165985 = ORIENTED_EDGE ( 'NONE', *, *, #228314, .T. ) ;
#165986 = CIRCLE ( 'NONE', #36988, 0.1000000000000028644 ) ;
#165987 = AXIS2_PLACEMENT_3D ( 'NONE', #99541, #179143, #454 ) ;
#165988 = EDGE_CURVE ( 'NONE', #237460, #234652, #5493, .T. ) ;
#165989 = VECTOR ( 'NONE', #37163, 1000.000000000000000 ) ;
#165990 = EDGE_CURVE ( 'NONE', #37772, #156163, #9606, .T. ) ;
#165991 = ORIENTED_EDGE ( 'NONE', *, *, #45912, .F. ) ;
#165992 =( BOUNDED_CURVE ( )  B_SPLINE_CURVE ( 3, ( #252218, #230097, #112726, #209247 ),
 .UNSPECIFIED., .F., .F. ) 
 B_SPLINE_CURVE_WITH_KNOTS ( ( 4, 4 ),
 ( 1.570796326794901665, 3.141592653589802886 ),
 .UNSPECIFIED. ) 
 CURVE ( )  GEOMETRIC_REPRESENTATION_ITEM ( )  RATIONAL_B_SPLINE_CURVE ( ( 1.000000000000000000, 0.8047378541243639383, 0.8047378541243639383, 1.000000000000000000 ) ) 
 REPRESENTATION_ITEM ( '' )  );
#165993 = EDGE_CURVE ( 'NONE', #212664, #5080, #96960, .T. ) ;
#165994 = AXIS2_PLACEMENT_3D ( 'NONE', #235302, #256091, #200046 ) ;
#165995 = CARTESIAN_POINT ( 'NONE',  ( -18.50000000000000000, 7.120270961708746960, -204.6595630418393057 ) ) ;
#165996 = EDGE_LOOP ( 'NONE', ( #206823, #155963, #173143, #38850 ) ) ;
#165997 = DIRECTION ( 'NONE',  ( 1.000000000000000000, 0.000000000000000000, 0.000000000000000000 ) ) ;
#165999 = EDGE_LOOP ( 'NONE', ( #236919, #10783, #67989, #175941 ) ) ;
#165998 = LINE ( 'NONE', #72016, #54407 ) ;
#166000 = DIRECTION ( 'NONE',  ( -0.000000000000000000, 0.8660254037844411501, 0.4999999999999956701 ) ) ;
#166001 = EDGE_CURVE ( 'NONE', #144129, #257328, #117839, .T. ) ;
#166002 = CARTESIAN_POINT ( 'NONE',  ( -16.87242674293850797, 12.41380142168690526, -211.2418236764092683 ) ) ;
#166003 = CARTESIAN_POINT ( 'NONE',  ( 15.48841904831874849, 8.561580951692381092, -180.1499999999999773 ) ) ;
#166004 = CARTESIAN_POINT ( 'NONE',  ( 23.24999999999999645, 2.971323450867608518, -188.3274415783412508 ) ) ;
#166007 = CARTESIAN_POINT ( 'NONE',  ( -23.15000000000000213, 64.25000000001222134, -148.6731074845244507 ) ) ;
#166006 = CIRCLE ( 'NONE', #53554, 0.09999999999999939493 ) ;
#166005 = CARTESIAN_POINT ( 'NONE',  ( -17.11825945287481332, 30.25354784785470486, -234.7188954791831748 ) ) ;
#166009 = CARTESIAN_POINT ( 'NONE',  ( -18.34374000495060386, 13.17878477875124688, -207.5966336730521391 ) ) ;
#166008 = VECTOR ( 'NONE', #79403, 1000.000000000000000 ) ;
#166010 = DIRECTION ( 'NONE',  ( 0.000000000000000000, 0.000000000000000000, 1.000000000000000000 ) ) ;
#166011 = AXIS2_PLACEMENT_3D ( 'NONE', #148839, #104528, #28929 ) ;
#166012 = DIRECTION ( 'NONE',  ( -1.000000000000000000, -0.000000000000000000, -0.000000000000000000 ) ) ;
#166013 = B_SPLINE_CURVE_WITH_KNOTS ( 'NONE', 3,
 ( #230915, #87509, #32736, #130497, #170972, #186646, #228334, #107083, #225729, #71838, #28892, #30146, #191797, #112247, #67964, #31446, #168404, #129229, #9274 ),
 .UNSPECIFIED., .F., .F.,
 ( 4, 3, 3, 3, 3, 3, 4 ),
 ( 0.000000000000000000, 7.110282409889357531E-05, 0.0001508797727291297914, 0.0002027344179858282824, 0.0002343294522349063957, 0.0002454816334821210652, 0.0002619873080085486088 ),
 .UNSPECIFIED. ) ;
#166014 = DIRECTION ( 'NONE',  ( -1.000000000000000000, -0.000000000000000000, -0.000000000000000000 ) ) ;
#166015 = VERTEX_POINT ( 'NONE', #72321 ) ;
#166016 = CIRCLE ( 'NONE', #53561, 0.1000000000000099282 ) ;
#166018 = ORIENTED_EDGE ( 'NONE', *, *, #115913, .T. ) ;
#166017 = CARTESIAN_POINT ( 'NONE',  ( -23.49999999999994316, 76.00000000001119815, -40.07310748452479032 ) ) ;
#166019 = ORIENTED_EDGE ( 'NONE', *, *, #212160, .F. ) ;
#166020 = FACE_OUTER_BOUND ( 'NONE', #183692, .T. ) ;
#166021 = DIRECTION ( 'NONE',  ( 1.000000000000000000, 2.952720810173289112E-16, -0.000000000000000000 ) ) ;
#166022 = ORIENTED_EDGE ( 'NONE', *, *, #109352, .T. ) ;
#166023 = VECTOR ( 'NONE', #124670, 1000.000000000000000 ) ;
#166024 = FACE_OUTER_BOUND ( 'NONE', #47173, .T. ) ;
#166025 = VERTEX_POINT ( 'NONE', #63001 ) ;
#166026 = VECTOR ( 'NONE', #208616, 1000.000000000000000 ) ;
#166027 = VECTOR ( 'NONE', #191157, 1000.000000000000000 ) ;
#166028 = CARTESIAN_POINT ( 'NONE',  ( 22.39999999999999503, 64.27847795353595473, -247.1247091181747066 ) ) ;
#166029 = DIRECTION ( 'NONE',  ( 0.000000000000000000, 0.000000000000000000, 1.000000000000000000 ) ) ;
#166030 = CARTESIAN_POINT ( 'NONE',  ( 20.95595624212443653, 65.37610879691743548, -61.89347457039733769 ) ) ;
#166031 = DIRECTION ( 'NONE',  ( 0.000000000000000000, 0.8660254037844377084, 0.5000000000000016653 ) ) ;
#166033 = ORIENTED_EDGE ( 'NONE', *, *, #143188, .T. ) ;
#166032 = LINE ( 'NONE', #23948, #31246 ) ;
#166034 = AXIS2_PLACEMENT_3D ( 'NONE', #24571, #4948, #104056 ) ;
#166035 = CYLINDRICAL_SURFACE ( 'NONE', #223424, 0.09999999999999939493 ) ;
#166036 = CARTESIAN_POINT ( 'NONE',  ( 18.49999999999999645, 76.00000000001142553, -36.02310748452432421 ) ) ;
#166037 = CARTESIAN_POINT ( 'NONE',  ( 18.42595409746844837, 85.49999981257613513, -96.02374513277639778 ) ) ;
#166038 = EDGE_LOOP ( 'NONE', ( #216505, #80245, #26281, #36630 ) ) ;
#166039 = CARTESIAN_POINT ( 'NONE',  ( 18.59999999999998366, 76.00000000001244871, -170.0231074845243597 ) ) ;
#166040 = FACE_OUTER_BOUND ( 'NONE', #103353, .T. ) ;
#166041 = EDGE_CURVE ( 'NONE', #225390, #7237, #198665, .T. ) ;
#166043 = CARTESIAN_POINT ( 'NONE',  ( -18.59999999999999787, 16.44800918141279311, -240.8068063186265135 ) ) ;
#166042 = LINE ( 'NONE', #10799, #228395 ) ;
#166044 = FACE_OUTER_BOUND ( 'NONE', #12769, .T. ) ;
#166045 = CARTESIAN_POINT ( 'NONE',  ( 18.49999999999999289, 10.25000000001115552, -155.3500000000000227 ) ) ;
#166046 = CARTESIAN_POINT ( 'NONE',  ( -20.97625342178412566, 64.39999999919187701, -163.0949042547225645 ) ) ;
#166047 = LINE ( 'NONE', #60481, #185321 ) ;
#166048 = AXIS2_PLACEMENT_3D ( 'NONE', #238053, #16474, #93409 ) ;
#166049 = VECTOR ( 'NONE', #32673, 1000.000000000000000 ) ;
#166051 = ADVANCED_FACE ( 'NONE', ( #162130 ), #155267, .T. ) ;
#166050 = CARTESIAN_POINT ( 'NONE',  ( -20.94999999999999929, 87.65000000001144542, -39.12310748452424747 ) ) ;
#166052 = DIRECTION ( 'NONE',  ( 0.000000000000000000, 2.891205793294679805E-16, -1.000000000000000000 ) ) ;
#166053 = TOROIDAL_SURFACE ( 'NONE', #12115, 0.2000000000000000111, 0.1000000000000000056 ) ;
#166054 = EDGE_LOOP ( 'NONE', ( #124661, #205221, #157874, #167440 ) ) ;
#166055 = DIRECTION ( 'NONE',  ( -1.000000000000000000, 0.000000000000000000, 0.000000000000000000 ) ) ;
#166056 = VECTOR ( 'NONE', #49376, 1000.000000000000000 ) ;
#166057 = ORIENTED_EDGE ( 'NONE', *, *, #3900, .T. ) ;
#166058 = ORIENTED_EDGE ( 'NONE', *, *, #244241, .T. ) ;
#166059 = ADVANCED_FACE ( 'NONE', ( #237802 ), #59121, .T. ) ;
#166060 = DIRECTION ( 'NONE',  ( 1.000000000000000000, -0.000000000000000000, 0.000000000000000000 ) ) ;
#166061 = ADVANCED_FACE ( 'NONE', ( #79974 ), #238750, .T. ) ;
#166062 = DIRECTION ( 'NONE',  ( -1.000000000000000000, 0.000000000000000000, 0.000000000000000000 ) ) ;
#166063 = ORIENTED_EDGE ( 'NONE', *, *, #152773, .F. ) ;
#166064 = CIRCLE ( 'NONE', #154177, 0.1000000000000013933 ) ;
#166065 = B_SPLINE_CURVE_WITH_KNOTS ( 'NONE', 3,
 ( #254729, #39620, #197363, #196094, #16192, #134804, #154434, #436, #214366, #35757, #79956, #116555, #115267, #17446, #232668, #54006 ),
 .UNSPECIFIED., .F., .F.,
 ( 4, 3, 3, 3, 3, 4 ),
 ( 0.000000000000000000, 1.810570668010836920E-05, 2.740575833572790496E-05, 4.256816319437009604E-05, 5.213463471025706227E-05, 6.641585710718375028E-05 ),
 .UNSPECIFIED. ) ;
#166066 = CIRCLE ( 'NONE', #53614, 0.09999999999999939493 ) ;
#166067 = ORIENTED_EDGE ( 'NONE', *, *, #197138, .F. ) ;
#166068 = VECTOR ( 'NONE', #137906, 1000.000000000000000 ) ;
#166069 = ORIENTED_EDGE ( 'NONE', *, *, #165214, .T. ) ;
#166070 = CARTESIAN_POINT ( 'NONE',  ( 20.94999999999999929, -3.444512620907435263, -226.2123967847655308 ) ) ;
#166071 = EDGE_LOOP ( 'NONE', ( #27636, #147566, #102694, #201990 ) ) ;
#166072 = EDGE_CURVE ( 'NONE', #146933, #167205, #113849, .T. ) ;
#166074 = CYLINDRICAL_SURFACE ( 'NONE', #213153, 0.09999999999999939493 ) ;
#166073 = TOROIDAL_SURFACE ( 'NONE', #182825, 11.70000000000000107, 0.1000000000000000056 ) ;
#166075 = CARTESIAN_POINT ( 'NONE',  ( 22.39999999999999503, 11.65000000001116298, -167.5999999999999659 ) ) ;
#166076 = CARTESIAN_POINT ( 'NONE',  ( -16.94107738177414291, 30.32481141862675145, -234.7976376674202186 ) ) ;
#166078 = EDGE_CURVE ( 'NONE', #82680, #131402, #159554, .T. ) ;
#166077 = AXIS2_PLACEMENT_3D ( 'NONE', #143634, #244013, #245319 ) ;
#166079 = CIRCLE ( 'NONE', #207760, 0.09999999999999950595 ) ;
#166080 = CARTESIAN_POINT ( 'NONE',  ( 21.05000000000000071, 4.850467289730776344, -121.9657325909983570 ) ) ;
#166081 = CARTESIAN_POINT ( 'NONE',  ( -21.09316766718153247, 1.532113312989072496, -230.6901497882401202 ) ) ;
#166082 = CIRCLE ( 'NONE', #182830, 0.1000000000000028644 ) ;
#166083 = DIRECTION ( 'NONE',  ( 0.000000000000000000, -0.9887567792719341719, -0.1495327102803664099 ) ) ;
#166084 = FACE_OUTER_BOUND ( 'NONE', #136635, .T. ) ;
#166086 = ORIENTED_EDGE ( 'NONE', *, *, #80450, .F. ) ;
#166085 = DIRECTION ( 'NONE',  ( 0.000000000000000000, 0.000000000000000000, -1.000000000000000000 ) ) ;
#166088 = DIRECTION ( 'NONE',  ( 1.000000000000000000, 0.000000000000000000, 0.000000000000000000 ) ) ;
#166087 = CARTESIAN_POINT ( 'NONE',  ( 20.95566103547454517, 65.38175234906454136, -61.89126729154380513 ) ) ;
#166089 = TOROIDAL_SURFACE ( 'NONE', #53635, 7.800000000000000711, 0.1000000000000000056 ) ;
#166090 = DIRECTION ( 'NONE',  ( 0.000000000000000000, -6.982962677686266711E-15, 1.000000000000000000 ) ) ;
#166091 = ORIENTED_EDGE ( 'NONE', *, *, #171954, .F. ) ;
#166092 = DIRECTION ( 'NONE',  ( -1.000000000000000000, -1.646408749285562691E-14, 0.000000000000000000 ) ) ;
#166093 = DIRECTION ( 'NONE',  ( 4.336808689942128177E-15, -0.7049548389604990417, 0.7092521942343054109 ) ) ;
#166094 = DIRECTION ( 'NONE',  ( 0.000000000000000000, 0.9999631594459056361, -0.008583690987128059571 ) ) ;
#166095 = ORIENTED_EDGE ( 'NONE', *, *, #177290, .T. ) ;
#166096 = CARTESIAN_POINT ( 'NONE',  ( 21.53699400384725493, 76.00000000001170974, -76.31081927776408236 ) ) ;
#166097 = EDGE_CURVE ( 'NONE', #210872, #227765, #23318, .T. ) ;
#166098 = CARTESIAN_POINT ( 'NONE',  ( -23.15000000000000213, 82.57900542960499024, -215.5587758314583482 ) ) ;
#166099 = ADVANCED_FACE ( 'NONE', ( #4301 ), #40268, .T. ) ;
#166100 = VECTOR ( 'NONE', #171417, 1000.000000000000227 ) ;
#166102 = ORIENTED_EDGE ( 'NONE', *, *, #255365, .T. ) ;
#166101 = CIRCLE ( 'NONE', #132768, 0.5000000000000004441 ) ;
#166103 = CARTESIAN_POINT ( 'NONE',  ( 21.05000000000000071, 71.00000000001199396, -115.4283735034374274 ) ) ;
#166104 = VECTOR ( 'NONE', #106819, 1000.000000000000000 ) ;
#166105 = CARTESIAN_POINT ( 'NONE',  ( -20.64999999999999858, 66.26558728512915764, -222.7970849955717938 ) ) ;
#166106 = DIRECTION ( 'NONE',  ( 0.000000000000000000, 0.000000000000000000, -1.000000000000000000 ) ) ;
#166107 = CARTESIAN_POINT ( 'NONE',  ( 21.05000000000000071, 76.10000000001241460, -176.5637644362255969 ) ) ;
#166108 = ORIENTED_EDGE ( 'NONE', *, *, #24502, .F. ) ;
#166109 = ORIENTED_EDGE ( 'NONE', *, *, #98846, .T. ) ;
#166110 = EDGE_CURVE ( 'NONE', #255597, #184002, #223353, .T. ) ;
#166111 = CIRCLE ( 'NONE', #232724, 0.1000000000000028644 ) ;
#166112 = EDGE_CURVE ( 'NONE', #144573, #93396, #180311, .T. ) ;
#166113 = AXIS2_PLACEMENT_3D ( 'NONE', #38913, #140550, #117161 ) ;
#166114 = CARTESIAN_POINT ( 'NONE',  ( 21.04105312098505109, 67.12466737696824737, -90.69460073731197269 ) ) ;
#166115 = CARTESIAN_POINT ( 'NONE',  ( 21.05000000000000426, 10.72371710470752149, -7.594417391613111690 ) ) ;
#166116 = DIRECTION ( 'NONE',  ( -1.000000000000000000, 0.000000000000000000, 0.000000000000000000 ) ) ;
#166117 = DIRECTION ( 'NONE',  ( -0.000000000000000000, 0.4721928772777347905, 0.8814952561688430555 ) ) ;
#166118 = VECTOR ( 'NONE', #239893, 1000.000000000000000 ) ;
#166119 = EDGE_CURVE ( 'NONE', #66990, #158029, #230363, .T. ) ;
#166120 = CARTESIAN_POINT ( 'NONE',  ( 21.08884785362045378, 6.357193367436396514, -167.4502169049331144 ) ) ;
#166121 = CARTESIAN_POINT ( 'NONE',  ( 20.94999999999999574, 4.288595810029049993, -211.9930862808554934 ) ) ;
#166122 = ORIENTED_EDGE ( 'NONE', *, *, #143004, .F. ) ;
#166123 = CARTESIAN_POINT ( 'NONE',  ( 23.15000000000000213, 87.65000000001144542, -39.12310748452424747 ) ) ;
#166124 = AXIS2_PLACEMENT_3D ( 'NONE', #40963, #98295, #162188 ) ;
#166125 = EDGE_CURVE ( 'NONE', #132946, #167562, #42942, .T. ) ;
#166127 = ORIENTED_EDGE ( 'NONE', *, *, #257460, .T. ) ;
#166126 = DIRECTION ( 'NONE',  ( 0.000000000000000000, 0.000000000000000000, 1.000000000000000000 ) ) ;
#166128 = DIRECTION ( 'NONE',  ( -1.836970198721029934E-16, -1.000000000000000000, -6.982962677686266711E-15 ) ) ;
#166129 = CARTESIAN_POINT ( 'NONE',  ( -16.79270642812297609, 66.05375578307368301, -90.36204076308727906 ) ) ;
#166130 = CARTESIAN_POINT ( 'NONE',  ( -21.64999999999999858, 7.250000000011148416, -88.15000000000004832 ) ) ;
#166131 = CARTESIAN_POINT ( 'NONE',  ( -23.25000000000000000, 76.00000000001195133, -103.0231074845243171 ) ) ;
#166133 = ORIENTED_EDGE ( 'NONE', *, *, #217062, .T. ) ;
#166132 = DIRECTION ( 'NONE',  ( 1.000000000000000000, -3.469446951953718318E-14, 2.003086131649645455E-14 ) ) ;
#166134 = CARTESIAN_POINT ( 'NONE',  ( -21.45000000000000284, 68.29142135624915966, -90.67310748452436542 ) ) ;
#166135 = ADVANCED_FACE ( 'NONE', ( #208941 ), #129403, .T. ) ;
#166136 = CARTESIAN_POINT ( 'NONE',  ( -16.93388492042257809, 63.06176463275114941, -213.0687502871022616 ) ) ;
#166137 = CARTESIAN_POINT ( 'NONE',  ( 21.05000000000000071, -11.74999999998883560, -69.90000000000004832 ) ) ;
#166138 = ORIENTED_EDGE ( 'NONE', *, *, #157827, .T. ) ;
#166139 = CARTESIAN_POINT ( 'NONE',  ( 23.14999999999999503, 62.94620731560446103, -207.1474054025217697 ) ) ;
#166140 = CARTESIAN_POINT ( 'NONE',  ( 20.94999999999999574, 72.06821323333463170, -225.0920403225231610 ) ) ;
#166141 = TOROIDAL_SURFACE ( 'NONE', #57753, 0.2000000000000000111, 0.1000000000000000056 ) ;
#166142 = AXIS2_PLACEMENT_3D ( 'NONE', #88747, #11833, #87469 ) ;
#166143 = CARTESIAN_POINT ( 'NONE',  ( -20.85000000000000142, 18.60970618848720903, -231.2322896185303875 ) ) ;
#166144 = EDGE_CURVE ( 'NONE', #70011, #183119, #90254, .T. ) ;
#166145 = AXIS2_PLACEMENT_3D ( 'NONE', #83773, #44706, #160818 ) ;
#166146 = B_SPLINE_CURVE_WITH_KNOTS ( 'NONE', 3,
 ( #214762, #131376, #12748, #255123, #195239, #71430, #152258, #156113, #31037, #212224, #231781, #250048, #113104, #150952, #110527, #32314, #133938, #111830, #191391, #92242, #251316, #192651, #252600, #74016, #54409, #99924 ),
 .UNSPECIFIED., .F., .F.,
 ( 4, 2, 2, 2, 2, 2, 2, 2, 2, 2, 2, 2, 4 ),
 ( 0.005476422646581343909, 0.006160811967703539241, 0.006845201288825734573, 0.007187395949386840913, 0.007529590609947948120, 0.007871785270509055327, 0.008213979931070161666, 0.008556174591631268006, 0.008898369252192374346, 0.009240563912753480685, 0.009582758573314588760, 0.01026714789443680838, 0.01095153721555902800 ),
 .UNSPECIFIED. ) ;
#166147 = CARTESIAN_POINT ( 'NONE',  ( -18.60000000000000142, 78.12133356376092763, -231.3112718935514920 ) ) ;
#166148 = ORIENTED_EDGE ( 'NONE', *, *, #4044, .F. ) ;
#166149 = CARTESIAN_POINT ( 'NONE',  ( 23.14999999999999858, 4.999999999999997335, -21.09473398108690390 ) ) ;
#166150 = ORIENTED_EDGE ( 'NONE', *, *, #100793, .F. ) ;
#166151 = CARTESIAN_POINT ( 'NONE',  ( -18.59999999999999787, -1.162701749926853712, -108.6000000000000227 ) ) ;
#166152 = FACE_OUTER_BOUND ( 'NONE', #58224, .T. ) ;
#166153 = EDGE_CURVE ( 'NONE', #98643, #242104, #116577, .T. ) ;
#166154 = SPHERICAL_SURFACE ( 'NONE', #49724, 0.1000000000000000056 ) ;
#166155 = DIRECTION ( 'NONE',  ( 0.000000000000000000, 6.982962677686266711E-15, -1.000000000000000000 ) ) ;
#166156 = ORIENTED_EDGE ( 'NONE', *, *, #94560, .F. ) ;
#166157 = CIRCLE ( 'NONE', #211925, 0.1000000000000028644 ) ;
#166158 = CARTESIAN_POINT ( 'NONE',  ( -21.10000000000000142, 0.000000000000000000, -4.000000000000000000 ) ) ;
#166159 = DIRECTION ( 'NONE',  ( 1.000000000000000000, 0.000000000000000000, 0.000000000000000000 ) ) ;
#166160 = FACE_OUTER_BOUND ( 'NONE', #199294, .T. ) ;
#166161 = CARTESIAN_POINT ( 'NONE',  ( -16.77431908686106610, 9.945805754517978770, -20.83583921765024982 ) ) ;
#166162 = CARTESIAN_POINT ( 'NONE',  ( -21.05000000000000071, 1.250000000011155299, -41.50000000000000000 ) ) ;
#166163 = EDGE_LOOP ( 'NONE', ( #42438, #155676, #212607, #92512, #203078, #104474, #116403, #177091, #199059, #9824, #34802, #148425 ) ) ;
#166165 = VERTEX_POINT ( 'NONE', #167278 ) ;
#166164 = CARTESIAN_POINT ( 'NONE',  ( -21.07094088545304089, 6.320167221927643020, -167.4011062974477682 ) ) ;
#166166 = ORIENTED_EDGE ( 'NONE', *, *, #38869, .T. ) ;
#166167 = CARTESIAN_POINT ( 'NONE',  ( -15.75000000000000355, 66.15000000001228386, -153.2731074845244166 ) ) ;
#166168 = ORIENTED_EDGE ( 'NONE', *, *, #24957, .F. ) ;
#166169 = CARTESIAN_POINT ( 'NONE',  ( 21.15000000000000213, 60.91865828504416669, -234.1430899377568551 ) ) ;
#166170 = DIRECTION ( 'NONE',  ( 1.000000000000000000, 0.000000000000000000, 0.000000000000000000 ) ) ;
#166171 = CARTESIAN_POINT ( 'NONE',  ( -16.77683809663752257, 9.950000000011138823, -188.3499999999999659 ) ) ;
#166172 = ORIENTED_EDGE ( 'NONE', *, *, #199187, .T. ) ;
#166173 = CARTESIAN_POINT ( 'NONE',  ( 20.94999999999999929, 1.115600667400684642E-11, -200.9999999999999432 ) ) ;
#166174 = CARTESIAN_POINT ( 'NONE',  ( 19.97071067811865674, 11.72071067812981759, -91.70857864376274904 ) ) ;
#166175 = CARTESIAN_POINT ( 'NONE',  ( 20.97217846901852312, 8.875441724720827708, -42.00122768393723760 ) ) ;
#166176 = ORIENTED_EDGE ( 'NONE', *, *, #145352, .F. ) ;
#166177 = DIRECTION ( 'NONE',  ( 0.000000000000000000, -0.9126074666063771490, -0.4088369013363281623 ) ) ;
#166179 = ORIENTED_EDGE ( 'NONE', *, *, #32302, .T. ) ;
#166178 = DIRECTION ( 'NONE',  ( 1.000000000000000000, 0.000000000000000000, 0.000000000000000000 ) ) ;
#166180 = LINE ( 'NONE', #44919, #156731 ) ;
#166181 = DIRECTION ( 'NONE',  ( 1.000000000000000000, 0.000000000000000000, 0.000000000000000000 ) ) ;
#166182 = AXIS2_PLACEMENT_3D ( 'NONE', #243394, #64758, #3492 ) ;
#166183 = CIRCLE ( 'NONE', #170285, 4.049999999999998046 ) ;
#166184 = AXIS2_PLACEMENT_3D ( 'NONE', #100622, #195931, #116385 ) ;
#166185 = CIRCLE ( 'NONE', #228709, 0.1000000000000028644 ) ;
#166186 = EDGE_LOOP ( 'NONE', ( #134774, #191081, #220112, #36838 ) ) ;
#166187 = DIRECTION ( 'NONE',  ( 0.000000000000000000, 0.8814952561688476074, -0.4721928772777262417 ) ) ;
#166188 = DIRECTION ( 'NONE',  ( 1.000000000000000000, 0.000000000000000000, 0.000000000000000000 ) ) ;
#166189 = AXIS2_PLACEMENT_3D ( 'NONE', #64073, #185308, #241441 ) ;
#166190 = CARTESIAN_POINT ( 'NONE',  ( -17.11825945287481332, 30.16539832223782369, -234.6716761914553899 ) ) ;
#166191 = ORIENTED_EDGE ( 'NONE', *, *, #238430, .F. ) ;
#166192 = CARTESIAN_POINT ( 'NONE',  ( -20.54999999999999716, 1.940186915899004161, -121.1708807889467039 ) ) ;
#166193 = EDGE_CURVE ( 'NONE', #153545, #206475, #30320, .T. ) ;
#166194 = DIRECTION ( 'NONE',  ( 0.000000000000000000, -0.8814952561688429444, 0.4721928772777345684 ) ) ;
#166195 = EDGE_CURVE ( 'NONE', #89895, #46953, #234453, .T. ) ;
#166196 = ORIENTED_EDGE ( 'NONE', *, *, #254682, .T. ) ;
#166197 = AXIS2_PLACEMENT_3D ( 'NONE', #167895, #150864, #227830 ) ;
#166199 = EDGE_CURVE ( 'NONE', #112286, #47002, #122035, .T. ) ;
#166198 = VECTOR ( 'NONE', #9213, 1000.000000000000000 ) ;
#166200 = AXIS2_PLACEMENT_3D ( 'NONE', #39173, #118704, #198213 ) ;
#166201 = VECTOR ( 'NONE', #168922, 1000.000000000000000 ) ;
#166202 = VERTEX_POINT ( 'NONE', #168585 ) ;
#166203 = CARTESIAN_POINT ( 'NONE',  ( 20.85000000000000142, 77.83585931145498193, -24.51866831572578675 ) ) ;
#166204 = ORIENTED_EDGE ( 'NONE', *, *, #16147, .T. ) ;
#166205 = CARTESIAN_POINT ( 'NONE',  ( 18.50596464788227280, 10.30632246270533159, -39.00418367788959273 ) ) ;
#166206 = EDGE_CURVE ( 'NONE', #36652, #204355, #213812, .T. ) ;
#166207 = CARTESIAN_POINT ( 'NONE',  ( -16.85697194749129224, 66.09145628588886723, -182.9581117521382509 ) ) ;
#166209 = ORIENTED_EDGE ( 'NONE', *, *, #22894, .F. ) ;
#166208 = DIRECTION ( 'NONE',  ( 0.000000000000000000, 0.000000000000000000, -1.000000000000000000 ) ) ;
#166210 = DIRECTION ( 'NONE',  ( -1.000000000000000000, 0.000000000000000000, 0.000000000000000000 ) ) ;
#166211 = CARTESIAN_POINT ( 'NONE',  ( 23.14999999999999503, 6.550000000011156231, -188.6499999999999488 ) ) ;
#166212 = DIRECTION ( 'NONE',  ( 3.469446951953622393E-14, 0.9684149032218615227, -0.2493442905257554076 ) ) ;
#166213 = DIRECTION ( 'NONE',  ( 2.952720810173289112E-16, 1.000000000000000000, -6.088138035986627436E-46 ) ) ;
#166214 = DIRECTION ( 'NONE',  ( 0.000000000000000000, -0.4088369013363280513, 0.9126074666063769270 ) ) ;
#166215 = CARTESIAN_POINT ( 'NONE',  ( 23.15000000000000213, -6.688413578037176066, -212.5825622730469036 ) ) ;
#166216 = CARTESIAN_POINT ( 'NONE',  ( -18.46093223321773635, -9.480682968263376864, -107.5845505139267146 ) ) ;
#166218 = ORIENTED_EDGE ( 'NONE', *, *, #28442, .F. ) ;
#166217 = DIRECTION ( 'NONE',  ( 0.000000000000000000, -6.982962677686266711E-15, 1.000000000000000000 ) ) ;
#166219 = CARTESIAN_POINT ( 'NONE',  ( 22.57856590037848932, -0.004128330053174996891, -55.24994153732460944 ) ) ;
#166220 = VERTEX_POINT ( 'NONE', #165995 ) ;
#166221 = AXIS2_PLACEMENT_3D ( 'NONE', #140807, #156552, #79522 ) ;
#166222 = CARTESIAN_POINT ( 'NONE',  ( -22.50000000000000000, 1.115600667400684642E-11, -161.2499999999999716 ) ) ;
#166223 = PLANE ( 'NONE',  #6910 ) ;
#166224 = EDGE_CURVE ( 'NONE', #11972, #58156, #6881, .T. ) ;
#166225 = EDGE_CURVE ( 'NONE', #58960, #6078, #126835, .T. ) ;
#166226 = AXIS2_PLACEMENT_3D ( 'NONE', #33246, #110166, #31951 ) ;
#166227 = CARTESIAN_POINT ( 'NONE',  ( -20.64999999999999858, -3.770473190032741062, -225.9805569534692324 ) ) ;
#166228 = DIRECTION ( 'NONE',  ( 0.000000000000000000, 0.000000000000000000, -1.000000000000000000 ) ) ;
#166229 = EDGE_LOOP ( 'NONE', ( #36403, #65722, #136091, #143430 ) ) ;
#166230 = FACE_BOUND ( 'NONE', #9328, .T. ) ;
#166231 = CARTESIAN_POINT ( 'NONE',  ( -22.39999999999999858, 75.90000000001170122, -77.31388708289772183 ) ) ;
#166232 = ADVANCED_FACE ( 'NONE', ( #206379 ), #27770, .T. ) ;
#166233 = VECTOR ( 'NONE', #213183, 1000.000000000000000 ) ;
#166234 = EDGE_LOOP ( 'NONE', ( #194125, #50518, #56132, #82712 ) ) ;
#166235 = TOROIDAL_SURFACE ( 'NONE', #232862, 0.2000000000000000111, 0.1000000000000000056 ) ;
#166236 = CARTESIAN_POINT ( 'NONE',  ( 21.05000000000005400, 87.75000000001119815, -3.123107484524795474 ) ) ;
#166237 = CONICAL_SURFACE ( 'NONE', #203625, 4.049999999999998046, 0.7853981633974604915 ) ;
#166238 = CARTESIAN_POINT ( 'NONE',  ( 22.45305468355010703, -0.1008583690885486023, -21.75043287651027768 ) ) ;
#166239 = VERTEX_POINT ( 'NONE', #227213 ) ;
#166240 = LINE ( 'NONE', #116511, #177632 ) ;
#166241 = ORIENTED_EDGE ( 'NONE', *, *, #182222, .T. ) ;
#166242 = CARTESIAN_POINT ( 'NONE',  ( -13.22483237240078324, 9.436674251854009654, -48.67686193099922320 ) ) ;
#166243 = VERTEX_POINT ( 'NONE', #26465 ) ;
#166244 = VECTOR ( 'NONE', #219259, 1000.000000000000000 ) ;
#166245 = AXIS2_PLACEMENT_3D ( 'NONE', #248858, #164193, #203313 ) ;
#166246 = DIRECTION ( 'NONE',  ( 0.000000000000000000, 0.000000000000000000, 1.000000000000000000 ) ) ;
#166247 = ADVANCED_FACE ( 'NONE', ( #25190 ), #168065, .T. ) ;
#166248 = DIRECTION ( 'NONE',  ( 0.000000000000000000, -0.9908441862701605762, 0.1350103645451835310 ) ) ;
#166249 = ORIENTED_EDGE ( 'NONE', *, *, #162322, .T. ) ;
#166250 = ORIENTED_EDGE ( 'NONE', *, *, #92089, .F. ) ;
#166251 = DIRECTION ( 'NONE',  ( 1.000000000000000000, -0.000000000000000000, 0.000000000000000000 ) ) ;
#166253 = EDGE_LOOP ( 'NONE', ( #51358, #97438, #175069, #123734 ) ) ;
#166252 = DIRECTION ( 'NONE',  ( 0.000000000000000000, -0.000000000000000000, -1.000000000000000000 ) ) ;
#166254 = DIRECTION ( 'NONE',  ( 4.026293107431335207E-15, -0.8454177738465953329, -0.5341055959866617409 ) ) ;
#166255 = EDGE_LOOP ( 'NONE', ( #204073, #33251, #134480, #104990 ) ) ;
#166256 = AXIS2_PLACEMENT_3D ( 'NONE', #199397, #157732, #178559 ) ;
#166257 = AXIS2_PLACEMENT_3D ( 'NONE', #136913, #159078, #255525 ) ;
#166258 = AXIS2_PLACEMENT_3D ( 'NONE', #116621, #198719, #140010 ) ;
#166259 = EDGE_CURVE ( 'NONE', #171197, #163151, #22288, .T. ) ;
#166260 = ORIENTED_EDGE ( 'NONE', *, *, #8409, .F. ) ;
#166262 = AXIS2_PLACEMENT_3D ( 'NONE', #114363, #208350, #188756 ) ;
#166261 = DIRECTION ( 'NONE',  ( 1.000000000000000000, 0.000000000000000000, 0.000000000000000000 ) ) ;
#166263 = CARTESIAN_POINT ( 'NONE',  ( 20.94999999999999929, 62.33780030268293615, -247.9091949332902516 ) ) ;
#166264 = CARTESIAN_POINT ( 'NONE',  ( -18.44448725179915627, 38.02117248346215206, -261.0467725487098392 ) ) ;
#166265 = ADVANCED_FACE ( 'NONE', ( #9451 ), #246544, .T. ) ;
#166267 = EDGE_CURVE ( 'NONE', #84692, #184180, #167474, .T. ) ;
#166266 = CARTESIAN_POINT ( 'NONE',  ( -16.77779411440718604, 9.946101447107603022, -20.83694258299546576 ) ) ;
#166268 = CYLINDRICAL_SURFACE ( 'NONE', #23156, 0.5000000000000004441 ) ;
#166269 = DIRECTION ( 'NONE',  ( -0.5735764363510466035, -0.8191520442889914655, -0.000000000000000000 ) ) ;
#166270 = ORIENTED_EDGE ( 'NONE', *, *, #104444, .F. ) ;
#166271 = DIRECTION ( 'NONE',  ( 0.000000000000000000, -0.5773469543544729188, -0.8164989248600478255 ) ) ;
#166272 = DIRECTION ( 'NONE',  ( 1.000000000000000000, 0.000000000000000000, 0.000000000000000000 ) ) ;
#166273 = CARTESIAN_POINT ( 'NONE',  ( 20.95483826173899899, 67.12383379524210625, -127.9768319316248437 ) ) ;
#166274 = CYLINDRICAL_SURFACE ( 'NONE', #201346, 0.5000000000000007772 ) ;
#166275 = VERTEX_POINT ( 'NONE', #14616 ) ;
#166276 = FACE_OUTER_BOUND ( 'NONE', #179835, .T. ) ;
#166277 = ORIENTED_EDGE ( 'NONE', *, *, #65009, .T. ) ;
#166279 = AXIS2_PLACEMENT_3D ( 'NONE', #79481, #234727, #56059 ) ;
#166278 = CARTESIAN_POINT ( 'NONE',  ( -23.25000000000000000, 1.115600667400684642E-11, -167.4999999999999716 ) ) ;
#166280 = EDGE_LOOP ( 'NONE', ( #159624, #21128, #224561, #28129 ) ) ;
#166281 = EDGE_CURVE ( 'NONE', #131047, #31458, #94120, .T. ) ;
#166282 = EDGE_CURVE ( 'NONE', #135784, #156438, #134115, .T. ) ;
#166283 = FACE_OUTER_BOUND ( 'NONE', #29387, .T. ) ;
#166284 = CARTESIAN_POINT ( 'NONE',  ( -18.40000000000000213, 64.51332499825454647, -145.7731074845244450 ) ) ;
#166285 = ORIENTED_EDGE ( 'NONE', *, *, #127673, .F. ) ;
#166286 = ORIENTED_EDGE ( 'NONE', *, *, #1985, .F. ) ;
#166288 = ORIENTED_EDGE ( 'NONE', *, *, #170963, .T. ) ;
#166287 = LINE ( 'NONE', #28055, #194741 ) ;
#166289 = DIRECTION ( 'NONE',  ( 0.000000000000000000, -0.9654727137038715545, 0.2605042016806676242 ) ) ;
#166290 = ORIENTED_EDGE ( 'NONE', *, *, #252110, .T. ) ;
#166291 = ADVANCED_FACE ( 'NONE', ( #214077 ), #101314, .F. ) ;
#166292 = CARTESIAN_POINT ( 'NONE',  ( -23.15000000000000213, 36.65892442174935439, -249.5511627012433848 ) ) ;
#166293 = AXIS2_PLACEMENT_3D ( 'NONE', #24659, #138132, #241129 ) ;
#166294 = FACE_OUTER_BOUND ( 'NONE', #112463, .T. ) ;
#166295 = CIRCLE ( 'NONE', #108011, 0.1000000000000055844 ) ;
#166296 = ORIENTED_EDGE ( 'NONE', *, *, #239586, .F. ) ;
#166297 = ADVANCED_FACE ( 'NONE', ( #194541 ), #211513, .T. ) ;
#166298 = DIRECTION ( 'NONE',  ( 0.000000000000000000, 0.000000000000000000, -1.000000000000000000 ) ) ;
#166299 = AXIS2_PLACEMENT_3D ( 'NONE', #3509, #83021, #21813 ) ;
#166300 = CARTESIAN_POINT ( 'NONE',  ( 18.69999999999999929, -8.150000000000007461, 10.52591260281975138 ) ) ;
#166301 = EDGE_CURVE ( 'NONE', #100439, #76299, #232379, .T. ) ;
#166302 = EDGE_CURVE ( 'NONE', #16283, #175979, #12049, .T. ) ;
#166303 = ORIENTED_EDGE ( 'NONE', *, *, #158884, .F. ) ;
#166304 = AXIS2_PLACEMENT_3D ( 'NONE', #193593, #114035, #170230 ) ;
#166305 = FACE_OUTER_BOUND ( 'NONE', #27100, .T. ) ;
#166306 = EDGE_CURVE ( 'NONE', #41677, #4874, #191974, .T. ) ;
#166307 = DIRECTION ( 'NONE',  ( 0.000000000000000000, 1.897661533703519897E-16, -1.000000000000000000 ) ) ;
#166309 = EDGE_LOOP ( 'NONE', ( #189639, #65601, #113382, #136697, #238061 ) ) ;
#166308 = DIRECTION ( 'NONE',  ( 0.000000000000000000, 0.4088369013363576943, -0.9126074666063638263 ) ) ;
#166310 = EDGE_CURVE ( 'NONE', #216286, #14895, #215352, .T. ) ;
#166311 = PLANE ( 'NONE',  #240973 ) ;
#166312 = CIRCLE ( 'NONE', #137243, 12.87499999999998579 ) ;
#166313 = LINE ( 'NONE', #161147, #52521 ) ;
#166314 = EDGE_CURVE ( 'NONE', #23846, #128626, #117562, .T. ) ;
#166315 = CARTESIAN_POINT ( 'NONE',  ( -16.91256925476569251, 9.985731158139330432, -121.4676424890052999 ) ) ;
#166316 = VECTOR ( 'NONE', #202179, 1000.000000000000000 ) ;
#166318 = DIRECTION ( 'NONE',  ( 1.000000000000000000, 0.000000000000000000, 0.000000000000000000 ) ) ;
#166317 = CARTESIAN_POINT ( 'NONE',  ( -23.15000000000000213, 4.768403829798271154, -213.4961173936592331 ) ) ;
#166319 = CARTESIAN_POINT ( 'NONE',  ( 21.05000000000000071, 39.26973050389061370, -236.6309188891183055 ) ) ;
#166321 = EDGE_CURVE ( 'NONE', #148976, #65207, #71794, .T. ) ;
#166320 = CARTESIAN_POINT ( 'NONE',  ( 6.099999999999987210, -11.75000000000000000, -15.00000000000001243 ) ) ;
#166322 = DIRECTION ( 'NONE',  ( -3.440080580676165868E-14, 0.1298341882520054891, 0.9915357197604850459 ) ) ;
#166323 = DIRECTION ( 'NONE',  ( 0.000000000000000000, -0.9656312546561486299, -0.2599159095384356855 ) ) ;
#166324 = ORIENTED_EDGE ( 'NONE', *, *, #229568, .T. ) ;
#166325 = ORIENTED_EDGE ( 'NONE', *, *, #154429, .F. ) ;
#166326 = DIRECTION ( 'NONE',  ( 1.000000000000000000, 0.000000000000000000, 0.000000000000000000 ) ) ;
#166327 = ORIENTED_EDGE ( 'NONE', *, *, #25132, .T. ) ;
#166328 = EDGE_CURVE ( 'NONE', #56261, #161130, #109740, .T. ) ;
#166329 = CARTESIAN_POINT ( 'NONE',  ( -33.72168855820451938, 9.950000000011156587, -87.85000000000009379 ) ) ;
#166330 = ORIENTED_EDGE ( 'NONE', *, *, #11698, .T. ) ;
#166331 = SHAPE_REPRESENTATION_RELATIONSHIP ( 'NONE' , 'NONE' ,  #206680, #73277 ) ;
#166332 = CARTESIAN_POINT ( 'NONE',  ( 21.05000000000000071, 6.650000000011155876, -146.1500000000000341 ) ) ;
#166334 = CARTESIAN_POINT ( 'NONE',  ( -22.39999999999999858, 11.75000000001115552, -167.5999999999999659 ) ) ;
#166333 = CIRCLE ( 'NONE', #253764, 0.5000000000000004441 ) ;
#166335 = EDGE_LOOP ( 'NONE', ( #181073, #44116, #7433 ) ) ;
#166336 = DIRECTION ( 'NONE',  ( 1.000000000000000000, 0.000000000000000000, -0.000000000000000000 ) ) ;
#166337 = ORIENTED_EDGE ( 'NONE', *, *, #28911, .F. ) ;
#166338 = EDGE_LOOP ( 'NONE', ( #219588, #253571, #106577, #7396, #72088 ) ) ;
#166339 = CARTESIAN_POINT ( 'NONE',  ( -20.94999999999999929, 7.128833340094563376, -233.7327013124401276 ) ) ;
#166340 = CARTESIAN_POINT ( 'NONE',  ( -11.59999999999994458, 67.72071067812984779, -17.05239680640613642 ) ) ;
#166342 = ORIENTED_EDGE ( 'NONE', *, *, #169503, .F. ) ;
#166341 = CARTESIAN_POINT ( 'NONE',  ( 21.08804582317324972, 67.12183383291966265, -57.17310765511903270 ) ) ;
#166344 = ORIENTED_EDGE ( 'NONE', *, *, #185360, .F. ) ;
#166343 = CYLINDRICAL_SURFACE ( 'NONE', #31054, 0.5000000000000004441 ) ;
#166345 = DIRECTION ( 'NONE',  ( -0.000000000000000000, 1.000000000000000000, -0.000000000000000000 ) ) ;
#166346 = CARTESIAN_POINT ( 'NONE',  ( -16.88005004766534967, 9.950100503332199864, -121.3503361119487920 ) ) ;
#166348 = ORIENTED_EDGE ( 'NONE', *, *, #123972, .F. ) ;
#166347 = DIRECTION ( 'NONE',  ( 0.000000000000000000, 0.000000000000000000, -1.000000000000000000 ) ) ;
#166349 = CYLINDRICAL_SURFACE ( 'NONE', #188958, 0.8750000000000007772 ) ;
#166350 = CARTESIAN_POINT ( 'NONE',  ( -18.56579813702275672, 10.33025634372637391, -72.58709292826389969 ) ) ;
#166351 = DIRECTION ( 'NONE',  ( 2.952720810173289112E-16, -1.000000000000000000, 0.000000000000000000 ) ) ;
#166352 = CIRCLE ( 'NONE', #37341, 0.09999999999999971412 ) ;
#166353 = ADVANCED_FACE ( 'NONE', ( #31621 ), #88301, .T. ) ;
#166356 = CARTESIAN_POINT ( 'NONE',  ( -18.40000000000000213, 11.47316190336248809, -24.17405393319204876 ) ) ;
#166355 = CIRCLE ( 'NONE', #28996, 0.09999999999999976963 ) ;
#166354 = CARTESIAN_POINT ( 'NONE',  ( -21.05000000000000071, 1.115600667400684642E-11, -100.5000000000000426 ) ) ;
#166357 = CARTESIAN_POINT ( 'NONE',  ( 18.52928932188133970, 10.27928932189250055, -91.65000000000004832 ) ) ;
#166358 = AXIS2_PLACEMENT_3D ( 'NONE', #156187, #212300, #152340 ) ;
#166359 = CIRCLE ( 'NONE', #70864, 0.09999999999999986677 ) ;
#166360 = CARTESIAN_POINT ( 'NONE',  ( 18.59999996954842771, 85.52320413787099085, -163.1400657726075565 ) ) ;
#166361 = ADVANCED_FACE ( 'NONE', ( #96657 ), #155009, .T. ) ;
#166362 = DIRECTION ( 'NONE',  ( -1.000000000000000000, 0.000000000000000000, 0.000000000000000000 ) ) ;
#166363 = DIRECTION ( 'NONE',  ( 0.000000000000000000, 0.000000000000000000, 1.000000000000000000 ) ) ;
#166364 = VERTEX_POINT ( 'NONE', #52416 ) ;
#166365 = EDGE_LOOP ( 'NONE', ( #38531, #32567, #97887 ) ) ;
#166366 = ORIENTED_EDGE ( 'NONE', *, *, #77030, .T. ) ;
#166367 = CARTESIAN_POINT ( 'NONE',  ( 18.59999999999999432, 74.83729825007408465, -128.4231074845243086 ) ) ;
#166368 = CIRCLE ( 'NONE', #195584, 4.300000000000039790 ) ;
#166369 = ORIENTED_EDGE ( 'NONE', *, *, #166640, .T. ) ;
#166370 = CARTESIAN_POINT ( 'NONE',  ( -20.94999999999999929, 77.83585931145600512, -158.5186683157258187 ) ) ;
#166371 = ORIENTED_EDGE ( 'NONE', *, *, #217799, .T. ) ;
#166372 = CARTESIAN_POINT ( 'NONE',  ( -18.52139480978223318, -7.769361016604765524, -209.8813056420265752 ) ) ;
#166373 = CARTESIAN_POINT ( 'NONE',  ( 18.58685178364169488, -9.406733083793096029, -40.62442046908773818 ) ) ;
#166374 = CIRCLE ( 'NONE', #195018, 0.09999999999999939493 ) ;
#166375 = ORIENTED_EDGE ( 'NONE', *, *, #124916, .F. ) ;
#166376 = CIRCLE ( 'NONE', #66394, 0.1000000000000028644 ) ;
#166377 = CYLINDRICAL_SURFACE ( 'NONE', #148679, 0.1000000000000028644 ) ;
#166378 =( NAMED_UNIT ( * ) PLANE_ANGLE_UNIT ( ) SI_UNIT ( $, .RADIAN. ) );
#166379 = EDGE_CURVE ( 'NONE', #70455, #61914, #111125, .T. ) ;
#166380 = ORIENTED_EDGE ( 'NONE', *, *, #27939, .F. ) ;
#166381 = CIRCLE ( 'NONE', #149620, 0.09999999999999939493 ) ;
#166382 = EDGE_LOOP ( 'NONE', ( #74789, #192647, #17231, #207281, #32740 ) ) ;
#166383 = VERTEX_POINT ( 'NONE', #251913 ) ;
#166384 = DIRECTION ( 'NONE',  ( -1.000000000000000000, -0.000000000000000000, -0.000000000000000000 ) ) ;
#166385 = DIRECTION ( 'NONE',  ( -1.000000000000000000, -0.000000000000000000, -0.000000000000000000 ) ) ;
#166386 = PLANE ( 'NONE',  #155041 ) ;
#166387 = CARTESIAN_POINT ( 'NONE',  ( 18.55857864376268296, 65.63284271248683410, -145.2731074845244450 ) ) ;
#166388 = DIRECTION ( 'NONE',  ( 0.000000000000000000, -1.565658005757035267E-14, 1.000000000000000000 ) ) ;
#166389 = DIRECTION ( 'NONE',  ( -2.840903330521631775E-16, 0.8700118002898321601, -0.4930308989875230030 ) ) ;
#166390 = DIRECTION ( 'NONE',  ( 1.186688945009010077E-16, -1.000000000000000000, -0.000000000000000000 ) ) ;
#166391 = CARTESIAN_POINT ( 'NONE',  ( 23.14999999999999503, 64.35000000001221565, -148.2731074845243882 ) ) ;
#166393 = VERTEX_POINT ( 'NONE', #73317 ) ;
#166392 = DIRECTION ( 'NONE',  ( 0.000000000000000000, 0.000000000000000000, -1.000000000000000000 ) ) ;
#166395 = CARTESIAN_POINT ( 'NONE',  ( 20.94999999999999574, 77.83534155023700407, -191.9679561919613491 ) ) ;
#166394 = CARTESIAN_POINT ( 'NONE',  ( 20.22516295850462598, 9.899364295460458152, -74.91006571209143772 ) ) ;
#166396 = DIRECTION ( 'NONE',  ( -0.000000000000000000, 1.000000000000000000, 6.352154140967427193E-15 ) ) ;
#166397 = ORIENTED_EDGE ( 'NONE', *, *, #56408, .F. ) ;
#166398 = CARTESIAN_POINT ( 'NONE',  ( -22.59999999999999787, 64.25043287652275126, -136.6239658536230763 ) ) ;
#166399 = DIRECTION ( 'NONE',  ( 0.000000000000000000, 0.000000000000000000, 1.000000000000000000 ) ) ;
#166400 = DIRECTION ( 'NONE',  ( 0.000000000000000000, 0.000000000000000000, 1.000000000000000000 ) ) ;
#166401 = ORIENTED_EDGE ( 'NONE', *, *, #198069, .T. ) ;
#166402 = DIRECTION ( 'NONE',  ( 0.000000000000000000, 0.000000000000000000, -1.000000000000000000 ) ) ;
#166403 = AXIS2_PLACEMENT_3D ( 'NONE', #12870, #134060, #190210 ) ;
#166404 = CARTESIAN_POINT ( 'NONE',  ( 20.85000000000000142, 77.26327546522934142, -128.6212428177779543 ) ) ;
#166405 = DIRECTION ( 'NONE',  ( -0.000000000000000000, 0.000000000000000000, -1.000000000000000000 ) ) ;
#166406 = VERTEX_POINT ( 'NONE', #152856 ) ;
#166407 = ORIENTED_EDGE ( 'NONE', *, *, #196709, .F. ) ;
#166408 = DIRECTION ( 'NONE',  ( 1.000000000000000000, 0.000000000000000000, 0.000000000000000000 ) ) ;
#166409 = ORIENTED_EDGE ( 'NONE', *, *, #203595, .T. ) ;
#166410 = PLANE ( 'NONE',  #35649 ) ;
#166412 = CARTESIAN_POINT ( 'NONE',  ( -18.37151313414829801, -9.571014125766513558, -174.3166629092390281 ) ) ;
#166411 = VECTOR ( 'NONE', #122744, 1000.000000000000000 ) ;
#166413 = CARTESIAN_POINT ( 'NONE',  ( -23.15000000000000213, 76.00000000001264766, -199.4731074845243484 ) ) ;
#166414 = ORIENTED_EDGE ( 'NONE', *, *, #139095, .F. ) ;
#166415 = EDGE_CURVE ( 'NONE', #162455, #15440, #30103, .T. ) ;
#166416 = CARTESIAN_POINT ( 'NONE',  ( -12.25000000000000355, 9.350000000011135626, -117.3657431672739619 ) ) ;
#166417 = DIRECTION ( 'NONE',  ( -1.000000000000000000, 2.952720810173289112E-16, 2.061873921506763405E-30 ) ) ;
#166418 = EDGE_CURVE ( 'NONE', #97655, #170518, #50957, .T. ) ;
#166419 = DIRECTION ( 'NONE',  ( 0.000000000000000000, 0.2128009952263601734, -0.9770955615653316162 ) ) ;
#166420 = DIRECTION ( 'NONE',  ( -3.265361837132813093E-16, 1.000000000000000000, 0.000000000000000000 ) ) ;
#166421 = CIRCLE ( 'NONE', #83135, 4.150000000000001243 ) ;
#166422 = ORIENTED_EDGE ( 'NONE', *, *, #137755, .T. ) ;
#166424 = DIRECTION ( 'NONE',  ( 1.000000000000000000, -7.304098846218135653E-16, -2.111765289898286048E-31 ) ) ;
#166423 = AXIS2_PLACEMENT_3D ( 'NONE', #230951, #172283, #211371 ) ;
#166425 = EDGE_CURVE ( 'NONE', #156311, #157579, #200933, .T. ) ;
#166427 = EDGE_LOOP ( 'NONE', ( #158038, #47864, #101486, #205718 ) ) ;
#166426 = DIRECTION ( 'NONE',  ( -7.304098846218490641E-16, -0.9651348961777379554, 0.2617529984164210233 ) ) ;
#166428 = DIRECTION ( 'NONE',  ( 1.000000000000000000, 0.000000000000000000, 0.000000000000000000 ) ) ;
#166429 = LINE ( 'NONE', #63430, #210012 ) ;
#166430 = CARTESIAN_POINT ( 'NONE',  ( 21.00000000000000000, 66.25000000001151079, -48.37310748452438958 ) ) ;
#166431 = DIRECTION ( 'NONE',  ( -0.000000000000000000, 0.4088369013363276072, -0.9126074666063772600 ) ) ;
#166432 = EDGE_CURVE ( 'NONE', #211815, #68317, #155586, .T. ) ;
#166433 = LINE ( 'NONE', #132412, #54799 ) ;
#166434 = CIRCLE ( 'NONE', #170557, 11.80000000000000426 ) ;
#166435 = DIRECTION ( 'NONE',  ( -1.000000000000000000, -2.952720810173289112E-16, 0.000000000000000000 ) ) ;
#166436 = FACE_OUTER_BOUND ( 'NONE', #178089, .T. ) ;
#166437 = CIRCLE ( 'NONE', #62174, 11.89999999999999858 ) ;
#166438 = EDGE_LOOP ( 'NONE', ( #152323, #197373, #111763, #24237, #21432, #213133, #197792, #245052, #86094, #76014, #165903, #52366, #204290, #233054 ) ) ;
#166439 = CARTESIAN_POINT ( 'NONE',  ( 18.39999999999999503, 9.957490673325212427, -220.1701168356097469 ) ) ;
#166440 = DIRECTION ( 'NONE',  ( 1.000000000000000000, -0.000000000000000000, 0.000000000000000000 ) ) ;
#166441 = CARTESIAN_POINT ( 'NONE',  ( -18.50000000000000000, 66.65000000001205649, -124.3731074845243683 ) ) ;
#166442 = EDGE_CURVE ( 'NONE', #18925, #2008, #146, .T. ) ;
#166443 = CARTESIAN_POINT ( 'NONE',  ( -18.79999999999999716, 7.900000000000000355, 1.300000000000000044 ) ) ;
#166444 = CARTESIAN_POINT ( 'NONE',  ( -1.739115166359751801E-14, 64.35000000001255671, -182.1731074845244507 ) ) ;
#166445 = CIRCLE ( 'NONE', #108160, 7.720710678118692272 ) ;
#166446 = CIRCLE ( 'NONE', #70587, 0.1000000000000000472 ) ;
#166448 = ORIENTED_EDGE ( 'NONE', *, *, #230760, .F. ) ;
#166447 = VECTOR ( 'NONE', #215, 1000.000000000000000 ) ;
#166449 = VERTEX_POINT ( 'NONE', #1436 ) ;
#166450 = AXIS2_PLACEMENT_3D ( 'NONE', #19096, #98593, #79047 ) ;
#166451 = CIRCLE ( 'NONE', #49881, 0.09999999999999939493 ) ;
#166452 = LINE ( 'NONE', #222510, #163559 ) ;
#166453 = CARTESIAN_POINT ( 'NONE',  ( 21.07016717457009491, 1.115540062193308597E-11, -127.6790591618991186 ) ) ;
#166454 = CARTESIAN_POINT ( 'NONE',  ( -18.50000000000000000, 67.49463558145298236, -195.5618716440587548 ) ) ;
#166455 = CIRCLE ( 'NONE', #145560, 0.1000000000000009492 ) ;
#166456 = EDGE_CURVE ( 'NONE', #171197, #165098, #63963, .T. ) ;
#166457 = DIRECTION ( 'NONE',  ( 0.000000000000000000, 0.000000000000000000, -1.000000000000000000 ) ) ;
#166458 = CARTESIAN_POINT ( 'NONE',  ( 21.30740335185486245, 6.556657922028002794, 0.09893452577585087893 ) ) ;
#166459 = CARTESIAN_POINT ( 'NONE',  ( -33.72168855820452649, 23.65833333334447985, -83.75000000000004263 ) ) ;
#166460 = B_SPLINE_CURVE_WITH_KNOTS ( 'NONE', 3,
 ( #171190, #128168, #31663, #246814, #250665, #32962, #227254, #109866 ),
 .UNSPECIFIED., .F., .F.,
 ( 4, 2, 2, 4 ),
 ( 0.000000000000000000, 0.0001049670497870086627, 0.0002099340995740173253, 0.0004198681991480253265 ),
 .UNSPECIFIED. ) ;
#166461 = CIRCLE ( 'NONE', #91427, 0.09999999999999939493 ) ;
#166462 = ORIENTED_EDGE ( 'NONE', *, *, #5726, .F. ) ;
#166463 = CARTESIAN_POINT ( 'NONE',  ( 18.49999999999999645, 77.29973367124280514, -112.9949779616549108 ) ) ;
#166464 = ORIENTED_EDGE ( 'NONE', *, *, #198574, .F. ) ;
#166465 = DIRECTION ( 'NONE',  ( 0.000000000000000000, 6.308085367188394185E-16, 1.000000000000000000 ) ) ;
#166466 = DIRECTION ( 'NONE',  ( 0.000000000000000000, -0.8741572761215371523, 0.4856429311786332748 ) ) ;
#166467 = CARTESIAN_POINT ( 'NONE',  ( -21.05000000000000071, 10.27588520313136300, -228.0695253486332490 ) ) ;
#166468 = CARTESIAN_POINT ( 'NONE',  ( -16.79814274880124358, 9.949272542688458287, -46.15243303704799871 ) ) ;
#166469 = DIRECTION ( 'NONE',  ( 1.000000000000000000, 0.000000000000000000, -0.000000000000000000 ) ) ;
#166470 = CARTESIAN_POINT ( 'NONE',  ( 18.52928932188134326, 65.72071067813118361, -178.8145288407617386 ) ) ;
#166471 = CARTESIAN_POINT ( 'NONE',  ( -16.97092634996643667, 65.99911103366365239, -82.15325025082218247 ) ) ;
#166472 = EDGE_LOOP ( 'NONE', ( #198833, #141894, #83968 ) ) ;
#166473 = CARTESIAN_POINT ( 'NONE',  ( -21.05000000000000071, 0.2561057921033771945, -133.9651035583277121 ) ) ;
#166474 = SPHERICAL_SURFACE ( 'NONE', #188003, 0.1000000000000000056 ) ;
#166475 = TOROIDAL_SURFACE ( 'NONE', #91445, 0.2000000000000000111, 0.1000000000000000056 ) ;
#166476 = CARTESIAN_POINT ( 'NONE',  ( -23.15000000000000213, 85.50000000001261924, -193.6291383618718385 ) ) ;
#166477 = CARTESIAN_POINT ( 'NONE',  ( 18.41416235934318735, -9.499999999999998224, -40.10018939122204529 ) ) ;
#166478 = CARTESIAN_POINT ( 'NONE',  ( 23.14999999999999858, 4.999999999999997335, -12.40526601891309788 ) ) ;
#166479 = DIRECTION ( 'NONE',  ( 0.000000000000000000, 0.8034013718071717491, -0.5954378521544919645 ) ) ;
#166480 = AXIS2_PLACEMENT_3D ( 'NONE', #228572, #215414, #41942 ) ;
#166481 = EDGE_CURVE ( 'NONE', #36208, #118151, #175849, .T. ) ;
#166482 = EDGE_LOOP ( 'NONE', ( #126517, #128900, #257237, #22314, #104649 ) ) ;
#166483 = SPHERICAL_SURFACE ( 'NONE', #110404, 0.1000000000000000056 ) ;
#166484 = LINE ( 'NONE', #132462, #166792 ) ;
#166485 = EDGE_CURVE ( 'NONE', #107516, #3690, #42534, .T. ) ;
#166486 = ORIENTED_EDGE ( 'NONE', *, *, #150147, .F. ) ;
#166487 = DIRECTION ( 'NONE',  ( 1.000000000000000000, 0.000000000000000000, 0.000000000000000000 ) ) ;
#166488 = PLANE ( 'NONE',  #102332 ) ;
#166489 = AXIS2_PLACEMENT_3D ( 'NONE', #145558, #49032, #12502 ) ;
#166490 = DIRECTION ( 'NONE',  ( 0.000000000000000000, 0.000000000000000000, -1.000000000000000000 ) ) ;
#166491 = CIRCLE ( 'NONE', #137407, 0.09999999999999641120 ) ;
#166492 = EDGE_CURVE ( 'NONE', #82377, #7289, #209132, .T. ) ;
#166493 = ORIENTED_EDGE ( 'NONE', *, *, #59987, .T. ) ;
#166495 = EDGE_CURVE ( 'NONE', #91388, #32792, #241359, .T. ) ;
#166494 = CARTESIAN_POINT ( 'NONE',  ( -22.94999999999999929, 3.461118860469513336, 28.84309995045515507 ) ) ;
#166496 = DIRECTION ( 'NONE',  ( 1.000000000000000000, -0.000000000000000000, -0.000000000000000000 ) ) ;
#166497 = ORIENTED_EDGE ( 'NONE', *, *, #202681, .T. ) ;
#166498 = CIRCLE ( 'NONE', #208178, 0.1000000000000054040 ) ;
#166499 = LINE ( 'NONE', #205573, #239603 ) ;
#166500 = ORIENTED_EDGE ( 'NONE', *, *, #179550, .T. ) ;
#166501 = EDGE_CURVE ( 'NONE', #108178, #91017, #237499, .T. ) ;
#166502 = DIRECTION ( 'NONE',  ( -0.000000000000000000, 0.000000000000000000, -1.000000000000000000 ) ) ;
#166503 = DIRECTION ( 'NONE',  ( 0.000000000000000000, 6.982962677686266711E-15, -1.000000000000000000 ) ) ;
#166504 = CARTESIAN_POINT ( 'NONE',  ( 18.59999999999999787, 87.75000000001251976, -182.1731074845242802 ) ) ;
#166505 = ADVANCED_FACE ( 'NONE', ( #40618 ), #38451, .T. ) ;
#166506 = CARTESIAN_POINT ( 'NONE',  ( -21.00023020733438628, 69.60913075474496736, -203.5231074845244166 ) ) ;
#166507 = DIRECTION ( 'NONE',  ( -0.000000000000000000, 1.000000000000000000, -1.224646799147352961E-16 ) ) ;
#166508 = CARTESIAN_POINT ( 'NONE',  ( -16.77683809663752257, 66.05416425680844839, -190.8591584654202222 ) ) ;
#166509 = DIRECTION ( 'NONE',  ( -6.938893903907224433E-15, 1.000000000000000000, 0.000000000000000000 ) ) ;
#166510 = CARTESIAN_POINT ( 'NONE',  ( -33.30000000000001137, 3.332938107839112263, -347.0000000000001137 ) ) ;
#166512 = ORIENTED_EDGE ( 'NONE', *, *, #16461, .F. ) ;
#166511 = CARTESIAN_POINT ( 'NONE',  ( -23.15000000000000213, 87.48912529308749697, -39.12310748452424747 ) ) ;
#166513 = VERTEX_POINT ( 'NONE', #22324 ) ;
#166516 = CARTESIAN_POINT ( 'NONE',  ( -15.66061380678752535, 9.360723793997191677, -84.31392719460676233 ) ) ;
#166515 = CARTESIAN_POINT ( 'NONE',  ( 20.94999999999999929, 8.776282895292474961, -12.15000000000000036 ) ) ;
#166514 = AXIS2_PLACEMENT_3D ( 'NONE', #94636, #160757, #235422 ) ;
#166517 = AXIS2_PLACEMENT_3D ( 'NONE', #185433, #102007, #66774 ) ;
#166519 = ORIENTED_EDGE ( 'NONE', *, *, #22907, .T. ) ;
#166518 = DIRECTION ( 'NONE',  ( 2.952720810173289112E-16, 1.000000000000000000, 7.086529944415894657E-15 ) ) ;
#166520 = EDGE_LOOP ( 'NONE', ( #165599, #86066, #241039, #37006 ) ) ;
#166521 = DIRECTION ( 'NONE',  ( 1.000000000000000000, -7.125593699324843413E-30, 1.020425574104004196E-15 ) ) ;
#166522 = CARTESIAN_POINT ( 'NONE',  ( 20.95512820512820440, 67.12384868372375024, -90.82293462539561801 ) ) ;
#166524 = ADVANCED_FACE ( 'NONE', ( #138364 ), #188285, .T. ) ;
#166523 = DIRECTION ( 'NONE',  ( 0.000000000000000000, 0.2617529984164506107, 0.9651348961777299618 ) ) ;
#166525 = DIRECTION ( 'NONE',  ( 0.000000000000000000, -1.000000000000000000, 0.000000000000000000 ) ) ;
#166526 = EDGE_CURVE ( 'NONE', #209971, #56225, #75870, .T. ) ;
#166527 = ADVANCED_FACE ( 'NONE', ( #43154 ), #202222, .F. ) ;
#166528 = DIRECTION ( 'NONE',  ( -0.000000000000000000, 1.000000000000000000, 0.000000000000000000 ) ) ;
#166529 = DIRECTION ( 'NONE',  ( 0.000000000000000000, -0.9126074666065445706, -0.4088369013359539617 ) ) ;
#166530 = FACE_OUTER_BOUND ( 'NONE', #193686, .T. ) ;
#166531 = AXIS2_PLACEMENT_3D ( 'NONE', #220675, #23789, #44609 ) ;
#166532 = ORIENTED_EDGE ( 'NONE', *, *, #176756, .T. ) ;
#166533 = ORIENTED_EDGE ( 'NONE', *, *, #166631, .T. ) ;
#166534 = VECTOR ( 'NONE', #4351, 1000.000000000000000 ) ;
#166535 = CARTESIAN_POINT ( 'NONE',  ( -20.64999999999999858, 19.28991295610541812, -237.9781866380819793 ) ) ;
#166536 = CIRCLE ( 'NONE', #70678, 0.2000000000000057288 ) ;
#166537 = AXIS2_PLACEMENT_3D ( 'NONE', #256728, #157734, #237225 ) ;
#166538 = ORIENTED_EDGE ( 'NONE', *, *, #48272, .T. ) ;
#166539 = CARTESIAN_POINT ( 'NONE',  ( 20.94999999999999929, 85.00000000001251976, -179.5170766071767332 ) ) ;
#166540 = EDGE_LOOP ( 'NONE', ( #140405, #110795, #167918, #49471 ) ) ;
#166541 = CARTESIAN_POINT ( 'NONE',  ( -21.44999999999999929, 7.250000000011155521, -88.15000000000004832 ) ) ;
#166542 = VECTOR ( 'NONE', #79154, 1000.000000000000000 ) ;
#166543 = CARTESIAN_POINT ( 'NONE',  ( -18.69999999999999929, 7.799999999999999822, -15.00000000000000000 ) ) ;
#166544 = CARTESIAN_POINT ( 'NONE',  ( 21.14999999999999503, 64.25000000001237765, -170.0231074845244166 ) ) ;
#166545 = CARTESIAN_POINT ( 'NONE',  ( -21.08884785362073089, 75.95021690494600364, -209.8803008519499826 ) ) ;
#166546 = ORIENTED_EDGE ( 'NONE', *, *, #189330, .F. ) ;
#166547 = CARTESIAN_POINT ( 'NONE',  ( -21.00250684356850783, 11.74999999999999645, -7.014805768759292626 ) ) ;
#166548 = ORIENTED_EDGE ( 'NONE', *, *, #197449, .F. ) ;
#166549 = DIRECTION ( 'NONE',  ( -1.186688945009010077E-16, 1.000000000000000000, 0.000000000000000000 ) ) ;
#166550 = VECTOR ( 'NONE', #94531, 1000.000000000000000 ) ;
#166551 = FACE_OUTER_BOUND ( 'NONE', #14942, .T. ) ;
#166552 = ADVANCED_FACE ( 'NONE', ( #100511 ), #50893, .T. ) ;
#166554 = AXIS2_PLACEMENT_3D ( 'NONE', #27373, #126422, #108153 ) ;
#166553 = CARTESIAN_POINT ( 'NONE',  ( 20.73486653747088937, 21.93924312953142319, -232.8743529746940624 ) ) ;
#166555 = VERTEX_POINT ( 'NONE', #240069 ) ;
#166556 = CARTESIAN_POINT ( 'NONE',  ( 20.94999999999999929, 62.44369217491800583, -212.5390448563743746 ) ) ;
#166557 = EDGE_LOOP ( 'NONE', ( #57948, #203861, #7913, #54092, #215159 ) ) ;
#166560 = ORIENTED_EDGE ( 'NONE', *, *, #201590, .T. ) ;
#166559 = CARTESIAN_POINT ( 'NONE',  ( -18.59999999999999787, 72.10920423909969657, -225.0008277277438822 ) ) ;
#166558 = DIRECTION ( 'NONE',  ( 0.000000000000000000, 0.000000000000000000, 1.000000000000000000 ) ) ;
#166561 = AXIS2_PLACEMENT_3D ( 'NONE', #249115, #247810, #225646 ) ;
#166562 = CYLINDRICAL_SURFACE ( 'NONE', #243740, 0.09999999999999939493 ) ;
#166563 = EDGE_LOOP ( 'NONE', ( #120773, #47099, #223624, #126343, #147557 ) ) ;
#166564 = DIRECTION ( 'NONE',  ( -0.000000000000000000, -0.2617529984165031243, -0.9651348961777157509 ) ) ;
#166565 = EDGE_LOOP ( 'NONE', ( #69483, #234525, #23776, #5334 ) ) ;
#166566 = EDGE_CURVE ( 'NONE', #13993, #236185, #229987, .T. ) ;
#166567 = DIRECTION ( 'NONE',  ( -0.000000000000000000, -0.000000000000000000, -1.000000000000000000 ) ) ;
#166568 = CYLINDRICAL_SURFACE ( 'NONE', #9603, 0.09999999999999939493 ) ;
#166569 = CARTESIAN_POINT ( 'NONE',  ( -21.05000000000000071, 87.65000000001212754, -133.5231074845242176 ) ) ;
#166570 = EDGE_CURVE ( 'NONE', #111449, #64043, #243901, .T. ) ;
#166571 = DIRECTION ( 'NONE',  ( -1.000000000000000000, 0.000000000000000000, 0.000000000000000000 ) ) ;
#166572 = ORIENTED_EDGE ( 'NONE', *, *, #7670, .T. ) ;
#166573 = EDGE_CURVE ( 'NONE', #11117, #164187, #113462, .T. ) ;
#166574 = SPHERICAL_SURFACE ( 'NONE', #223245, 0.1000000000000000056 ) ;
#166575 = CARTESIAN_POINT ( 'NONE',  ( -16.85312964099708566, 14.07083882076682713, -219.0212948398784647 ) ) ;
#166576 = CARTESIAN_POINT ( 'NONE',  ( 18.59999999999999076, 74.16465844978745281, -91.36795619196134055 ) ) ;
#166577 = AXIS2_PLACEMENT_3D ( 'NONE', #72525, #92060, #171645 ) ;
#166578 = ORIENTED_EDGE ( 'NONE', *, *, #15009, .T. ) ;
#166579 = CARTESIAN_POINT ( 'NONE',  ( -21.05000000000000071, 64.35000000001190301, -96.23924182154622997 ) ) ;
#166580 = VERTEX_POINT ( 'NONE', #89960 ) ;
#166581 = DIRECTION ( 'NONE',  ( 0.000000000000000000, 0.000000000000000000, -1.000000000000000000 ) ) ;
#166582 = ADVANCED_FACE ( 'NONE', ( #105658, #189078 ), #207369, .T. ) ;
#166583 = EDGE_CURVE ( 'NONE', #195224, #155749, #30278, .T. ) ;
#166584 = DIRECTION ( 'NONE',  ( 0.000000000000000000, 0.000000000000000000, 1.000000000000000000 ) ) ;
#166585 = CARTESIAN_POINT ( 'NONE',  ( 20.09999999999999787, 61.13238474529445909, -221.0940783352693586 ) ) ;
#166586 = AXIS2_PLACEMENT_3D ( 'NONE', #65308, #144834, #22360 ) ;
#166588 = ORIENTED_EDGE ( 'NONE', *, *, #151668, .F. ) ;
#166587 = CARTESIAN_POINT ( 'NONE',  ( 21.14999999999999858, 6.550000000011156231, -179.6499999999999773 ) ) ;
#166589 = DIRECTION ( 'NONE',  ( 1.000000000000000000, 0.000000000000000000, 0.000000000000000000 ) ) ;
#166590 = CIRCLE ( 'NONE', #145696, 0.1000000000000052097 ) ;
#166591 = DIRECTION ( 'NONE',  ( 0.000000000000000000, 0.000000000000000000, 1.000000000000000000 ) ) ;
#166592 = DIRECTION ( 'NONE',  ( 0.000000000000000000, -7.272083257015735086E-15, 1.000000000000000000 ) ) ;
#166593 = ORIENTED_EDGE ( 'NONE', *, *, #227709, .F. ) ;
#166594 = CARTESIAN_POINT ( 'NONE',  ( 22.39999999999999147, 68.20922040163929978, -203.5231074845244166 ) ) ;
#166595 = CARTESIAN_POINT ( 'NONE',  ( 18.43565242384934066, 85.51932773110476660, -163.0501311079649724 ) ) ;
#166596 = ORIENTED_EDGE ( 'NONE', *, *, #89086, .F. ) ;
#166597 = DIRECTION ( 'NONE',  ( 0.000000000000000000, 0.000000000000000000, -1.000000000000000000 ) ) ;
#166598 = VECTOR ( 'NONE', #142058, 1000.000000000000114 ) ;
#166599 = ADVANCED_FACE ( 'NONE', ( #28769 ), #59251, .T. ) ;
#166601 = EDGE_CURVE ( 'NONE', #43292, #84007, #129107, .T. ) ;
#166600 = AXIS2_PLACEMENT_3D ( 'NONE', #173262, #50666, #209774 ) ;
#166602 = ORIENTED_EDGE ( 'NONE', *, *, #49607, .F. ) ;
#166603 = DIRECTION ( 'NONE',  ( 0.000000000000000000, 0.2128009952263603677, -0.9770955615653313941 ) ) ;
#166605 = ORIENTED_EDGE ( 'NONE', *, *, #34144, .T. ) ;
#166604 = CARTESIAN_POINT ( 'NONE',  ( -21.59142135623730852, 68.15000000001222702, -148.8731074845244393 ) ) ;
#166606 = CIRCLE ( 'NONE', #198778, 0.09999999999999939493 ) ;
#166607 = EDGE_CURVE ( 'NONE', #189305, #218866, #188467, .T. ) ;
#166608 = AXIS2_PLACEMENT_3D ( 'NONE', #39067, #238525, #140705 ) ;
#166609 = TOROIDAL_SURFACE ( 'NONE', #149854, 11.70000000000000107, 0.1000000000000000056 ) ;
#166612 = VERTEX_POINT ( 'NONE', #168276 ) ;
#166611 = ORIENTED_EDGE ( 'NONE', *, *, #86941, .F. ) ;
#166610 = DIRECTION ( 'NONE',  ( -1.000000000000000000, -0.000000000000000000, -0.000000000000000000 ) ) ;
#166613 = CARTESIAN_POINT ( 'NONE',  ( 21.14999999999999858, 6.650000000011155876, -112.7500000000000284 ) ) ;
#166614 = DIRECTION ( 'NONE',  ( -1.000000000000000000, 7.166229603267618227E-16, 4.447280054184918885E-16 ) ) ;
#166615 = EDGE_CURVE ( 'NONE', #137667, #137151, #134294, .T. ) ;
#166616 = DIRECTION ( 'NONE',  ( 1.000000000000000000, -0.000000000000000000, -0.000000000000000000 ) ) ;
#166618 = CARTESIAN_POINT ( 'NONE',  ( -21.45000000000000284, 7.708578643762696636, -12.34999999999999964 ) ) ;
#166617 = LINE ( 'NONE', #210849, #189865 ) ;
#166619 = LINE ( 'NONE', #24534, #152919 ) ;
#166621 = EDGE_CURVE ( 'NONE', #253940, #109684, #208656, .T. ) ;
#166620 = CARTESIAN_POINT ( 'NONE',  ( 21.05000000000000071, 1.115625160336667635E-11, -198.9999999999999432 ) ) ;
#166622 = CARTESIAN_POINT ( 'NONE',  ( 20.85000000000000142, 74.73788286442776041, -233.7359682632885267 ) ) ;
#166623 = VECTOR ( 'NONE', #42914, 1000.000000000000000 ) ;
#166624 = CARTESIAN_POINT ( 'NONE',  ( 16.27683809663749770, 19.69766786220171539, -229.8585047820796490 ) ) ;
#166625 = DIRECTION ( 'NONE',  ( 0.000000000000000000, 0.000000000000000000, -1.000000000000000000 ) ) ;
#166626 = CIRCLE ( 'NONE', #224838, 0.1000000000000028644 ) ;
#166627 = VECTOR ( 'NONE', #196828, 1000.000000000000000 ) ;
#166628 = VERTEX_POINT ( 'NONE', #225600 ) ;
#166630 = ORIENTED_EDGE ( 'NONE', *, *, #17407, .F. ) ;
#166629 = AXIS2_PLACEMENT_3D ( 'NONE', #187869, #112183, #13084 ) ;
#166631 = EDGE_CURVE ( 'NONE', #171429, #121586, #184373, .T. ) ;
#166632 = DIRECTION ( 'NONE',  ( 0.000000000000000000, 3.469446951953514729E-13, -1.000000000000000000 ) ) ;
#166634 = ORIENTED_EDGE ( 'NONE', *, *, #244498, .F. ) ;
#166633 = DIRECTION ( 'NONE',  ( 0.000000000000000000, -1.000000000000000000, -0.000000000000000000 ) ) ;
#166635 = EDGE_LOOP ( 'NONE', ( #141918, #247422, #128360, #249958 ) ) ;
#166636 = AXIS2_PLACEMENT_3D ( 'NONE', #94472, #224689, #140007 ) ;
#166637 = CYLINDRICAL_SURFACE ( 'NONE', #135255, 0.1000000000000013933 ) ;
#166638 = VERTEX_POINT ( 'NONE', #45708 ) ;
#166639 = DIRECTION ( 'NONE',  ( 1.000000000000000000, -2.952720810173289112E-16, -2.061873921506763405E-30 ) ) ;
#166640 = EDGE_CURVE ( 'NONE', #57578, #223215, #92601, .T. ) ;
#166641 = ORIENTED_EDGE ( 'NONE', *, *, #70967, .T. ) ;
#166642 = CARTESIAN_POINT ( 'NONE',  ( -23.25000000000000000, 56.06656052939784018, -228.0911609752645290 ) ) ;
#166643 = CARTESIAN_POINT ( 'NONE',  ( -18.59999999999999787, -9.480686695267820596, -174.4411151687578752 ) ) ;
#166645 = ORIENTED_EDGE ( 'NONE', *, *, #233704, .T. ) ;
#166644 = VERTEX_POINT ( 'NONE', #86086 ) ;
#166646 = ORIENTED_EDGE ( 'NONE', *, *, #82594, .F. ) ;
#166647 = DIRECTION ( 'NONE',  ( -2.952720810173289605E-16, -1.000000000000000000, -7.086529944415894657E-15 ) ) ;
#166648 = ORIENTED_EDGE ( 'NONE', *, *, #130908, .T. ) ;
#166649 = ORIENTED_EDGE ( 'NONE', *, *, #221347, .T. ) ;
#166650 = CARTESIAN_POINT ( 'NONE',  ( -21.65000000000000213, 68.75000000001207923, -123.8731074845243540 ) ) ;
#166651 = LINE ( 'NONE', #183619, #182469 ) ;
#166653 = ORIENTED_EDGE ( 'NONE', *, *, #81158, .F. ) ;
#166652 = CARTESIAN_POINT ( 'NONE',  ( -20.85000000000000142, 17.16609282392353819, -224.6038045889790453 ) ) ;
#166654 = CARTESIAN_POINT ( 'NONE',  ( 21.05000000000000071, 1.115600667400684642E-11, -67.00000000000004263 ) ) ;
#166655 = CARTESIAN_POINT ( 'NONE',  ( -23.25000000000000000, 4.350000000011156054, -45.85000000000000142 ) ) ;
#166657 = ORIENTED_EDGE ( 'NONE', *, *, #35368, .T. ) ;
#166656 = CARTESIAN_POINT ( 'NONE',  ( -21.37071067811865532, 29.67153963045800324, -236.6525067779183189 ) ) ;
#166658 = DIRECTION ( 'NONE',  ( 1.000000000000000000, 0.000000000000000000, 0.000000000000000000 ) ) ;
#166659 = ORIENTED_EDGE ( 'NONE', *, *, #138023, .T. ) ;
#166660 = DIRECTION ( 'NONE',  ( 1.000000000000000000, 0.000000000000000000, 0.000000000000000000 ) ) ;
#166661 = CIRCLE ( 'NONE', #45818, 0.9000000000000014655 ) ;
#166662 = ORIENTED_EDGE ( 'NONE', *, *, #189210, .T. ) ;
#166663 = CARTESIAN_POINT ( 'NONE',  ( -21.14999999999999858, 18.65704504850842227, -226.5784250989226507 ) ) ;
#166664 = EDGE_LOOP ( 'NONE', ( #47654, #147865, #230434 ) ) ;
#166666 = DIRECTION ( 'NONE',  ( 0.000000000000000000, -1.000000000000000000, -0.000000000000000000 ) ) ;
#166665 = CARTESIAN_POINT ( 'NONE',  ( 21.05000012384953223, 10.62872029888669978, -45.67797733003531135 ) ) ;
#166667 = AXIS2_PLACEMENT_3D ( 'NONE', #70507, #150029, #229557 ) ;
#166668 = PLANE ( 'NONE',  #134788 ) ;
#166669 = LINE ( 'NONE', #124951, #239199 ) ;
#166670 = ORIENTED_EDGE ( 'NONE', *, *, #97825, .T. ) ;
#166671 = EDGE_LOOP ( 'NONE', ( #188735, #97781, #27839, #252852 ) ) ;
#166672 = DIRECTION ( 'NONE',  ( 0.000000000000000000, 0.000000000000000000, -1.000000000000000000 ) ) ;
#166673 = ADVANCED_FACE ( 'NONE', ( #125254 ), #106955, .T. ) ;
#166674 = CARTESIAN_POINT ( 'NONE',  ( 21.05000000000000071, 71.00000000001253397, -182.0283735034374786 ) ) ;
#166675 = VERTEX_POINT ( 'NONE', #165683 ) ;
#166676 = DIRECTION ( 'NONE',  ( 0.000000000000000000, -0.008583690987162452199, 0.9999631594459053030 ) ) ;
#166677 = ORIENTED_EDGE ( 'NONE', *, *, #46727, .T. ) ;
#166678 = DIRECTION ( 'NONE',  ( 1.000000000000000000, -0.000000000000000000, -0.000000000000000000 ) ) ;
#166679 = ORIENTED_EDGE ( 'NONE', *, *, #212022, .F. ) ;
#166680 = AXIS2_PLACEMENT_3D ( 'NONE', #35627, #135958, #115131 ) ;
#166681 = SPHERICAL_SURFACE ( 'NONE', #94968, 0.1000000000000000056 ) ;
#166682 = CARTESIAN_POINT ( 'NONE',  ( -21.05000000000000071, 7.128833340094563376, -233.7327013124401276 ) ) ;
#166683 = VECTOR ( 'NONE', #30969, 1000.000000000000114 ) ;
#166684 = ORIENTED_EDGE ( 'NONE', *, *, #99129, .F. ) ;
#166685 = DIRECTION ( 'NONE',  ( -1.000000000000000000, -1.836970198721029934E-16, 0.000000000000000000 ) ) ;
#166686 = SURFACE_STYLE_FILL_AREA ( #72716 ) ;
#166687 = EDGE_CURVE ( 'NONE', #235587, #191384, #143520, .T. ) ;
#166688 = AXIS2_PLACEMENT_3D ( 'NONE', #75883, #177594, #138395 ) ;
#166690 = ORIENTED_EDGE ( 'NONE', *, *, #160864, .F. ) ;
#166689 = TOROIDAL_SURFACE ( 'NONE', #162580, 7.800000000000000711, 0.1000000000000000056 ) ;
#166691 = ORIENTED_EDGE ( 'NONE', *, *, #120426, .T. ) ;
#166692 = ORIENTED_EDGE ( 'NONE', *, *, #31674, .T. ) ;
#166693 = DIRECTION ( 'NONE',  ( 0.000000000000000000, -0.9915357197604792727, 0.1298341882520475943 ) ) ;
#166694 = DIRECTION ( 'NONE',  ( 0.7071067811865474617, -0.7071067811865474617, -4.937700262164531476E-15 ) ) ;
#166695 = CARTESIAN_POINT ( 'NONE',  ( -18.59999999999999787, 64.25000000001254818, -182.1731074845244507 ) ) ;
#166696 = DIRECTION ( 'NONE',  ( -0.000000000000000000, -1.897661533703519897E-16, 1.000000000000000000 ) ) ;
#166697 = CARTESIAN_POINT ( 'NONE',  ( 21.05000000000005400, 83.97335046823651794, -37.38386894789040582 ) ) ;
#166698 =( BOUNDED_CURVE ( )  B_SPLINE_CURVE ( 3, ( #165231, #66130, #145655, #126086 ),
 .UNSPECIFIED., .F., .F. ) 
 B_SPLINE_CURVE_WITH_KNOTS ( ( 4, 4 ),
 ( 0.000000000000000000, 1.570796326794916320 ),
 .UNSPECIFIED. ) 
 CURVE ( )  GEOMETRIC_REPRESENTATION_ITEM ( )  RATIONAL_B_SPLINE_CURVE ( ( 1.000000000000000000, 0.8047378541243603856, 0.8047378541243603856, 1.000000000000000000 ) ) 
 REPRESENTATION_ITEM ( '' )  );
#166700 = CYLINDRICAL_SURFACE ( 'NONE', #194870, 0.09999999999999553690 ) ;
#166699 = DIRECTION ( 'NONE',  ( 0.000000000000000000, 0.000000000000000000, 1.000000000000000000 ) ) ;
#166702 = EDGE_LOOP ( 'NONE', ( #61145, #212906, #201255, #1439 ) ) ;
#166701 = CARTESIAN_POINT ( 'NONE',  ( -23.25000000000000000, 12.67709964810647882, -223.3751320524553705 ) ) ;
#166703 = CARTESIAN_POINT ( 'NONE',  ( 21.04999999999998650, 45.11960049378627247, -238.4740710069430349 ) ) ;
#166704 = ORIENTED_EDGE ( 'NONE', *, *, #64894, .F. ) ;
#166705 = CARTESIAN_POINT ( 'NONE',  ( 21.03675099975491136, 8.875180032795967122, -79.32554213677809685 ) ) ;
#166706 = VERTEX_POINT ( 'NONE', #123978 ) ;
#166707 = ORIENTED_EDGE ( 'NONE', *, *, #106982, .F. ) ;
#166708 = DIRECTION ( 'NONE',  ( 0.000000000000000000, 0.000000000000000000, -1.000000000000000000 ) ) ;
#166709 = LINE ( 'NONE', #226633, #151927 ) ;
#166710 = CARTESIAN_POINT ( 'NONE',  ( -21.04999999999999716, 75.98514436511885606, -209.8674665265682791 ) ) ;
#166711 = DIRECTION ( 'NONE',  ( -1.000000000000000000, -0.000000000000000000, -0.000000000000000000 ) ) ;
#166712 = CIRCLE ( 'NONE', #25221, 0.09999999999998898659 ) ;
#166713 = LINE ( 'NONE', #246221, #109047 ) ;
#166714 = ORIENTED_EDGE ( 'NONE', *, *, #73878, .T. ) ;
#166715 = ORIENTED_EDGE ( 'NONE', *, *, #87606, .F. ) ;
#166716 =( BOUNDED_CURVE ( )  B_SPLINE_CURVE ( 3, ( #203088, #24485, #243501, #223920 ),
 .UNSPECIFIED., .F., .F. ) 
 B_SPLINE_CURVE_WITH_KNOTS ( ( 4, 4 ),
 ( 0.3000847527772370071, 0.5497968875596834781 ),
 .UNSPECIFIED. ) 
 CURVE ( )  GEOMETRIC_REPRESENTATION_ITEM ( )  RATIONAL_B_SPLINE_CURVE ( ( 1.000000000000000000, 0.9948104011409417691, 0.9948104011409417691, 1.000000000000000000 ) ) 
 REPRESENTATION_ITEM ( '' )  );
#166717 = DIRECTION ( 'NONE',  ( -3.265361837132813093E-16, 1.000000000000000000, 0.000000000000000000 ) ) ;
#166718 = ORIENTED_EDGE ( 'NONE', *, *, #244057, .T. ) ;
#166719 = CARTESIAN_POINT ( 'NONE',  ( -21.76363531954647357, 0.09900187431060442078, -126.9870634521282966 ) ) ;
#166720 = DIRECTION ( 'NONE',  ( -1.000000000000000000, -0.000000000000000000, 0.000000000000000000 ) ) ;
#166721 = ORIENTED_EDGE ( 'NONE', *, *, #207253, .T. ) ;
#166722 = CARTESIAN_POINT ( 'NONE',  ( 21.05000000000000071, 68.19849547655701372, -211.6586561550524834 ) ) ;
#166723 = FACE_OUTER_BOUND ( 'NONE', #195349, .T. ) ;
#166724 = DIRECTION ( 'NONE',  ( 0.000000000000000000, 0.000000000000000000, 1.000000000000000000 ) ) ;
#166725 = CARTESIAN_POINT ( 'NONE',  ( 21.51976009735019346, 6.910458441670357388, -67.00000000000004263 ) ) ;
#166726 = ORIENTED_EDGE ( 'NONE', *, *, #179441, .F. ) ;
#166727 = CARTESIAN_POINT ( 'NONE',  ( -21.14999999999999858, 76.10085836911075319, -114.7726746080137019 ) ) ;
#166728 = FACE_OUTER_BOUND ( 'NONE', #212724, .T. ) ;
#166729 = CARTESIAN_POINT ( 'NONE',  ( 20.94999999999999574, 1.148907358139439339E-11, -201.0000000000015064 ) ) ;
#166730 = LINE ( 'NONE', #147123, #162691 ) ;
#166731 = CIRCLE ( 'NONE', #166531, 11.74999999999999645 ) ;
#166732 = CIRCLE ( 'NONE', #233360, 0.1000000000000018374 ) ;
#166733 = CARTESIAN_POINT ( 'NONE',  ( -16.87036670365548474, 10.08494996326643189, -54.44999999999999574 ) ) ;
#166734 = EDGE_CURVE ( 'NONE', #89898, #49355, #151072, .T. ) ;
#166735 = AXIS2_PLACEMENT_3D ( 'NONE', #157363, #175624, #79043 ) ;
#166736 = CIRCLE ( 'NONE', #204090, 0.1000000000000024342 ) ;
#166737 = CARTESIAN_POINT ( 'NONE',  ( 21.14999999999999858, -11.64999999998883595, -167.4999999999999432 ) ) ;
#166738 =( BOUNDED_SURFACE ( )  B_SPLINE_SURFACE ( 3, 2, ( 
 ( #238480, #156418, #235901 ),
 ( #117259, #179811, #58541 ),
 ( #217608, #119844, #196776 ),
 ( #18149, #177260, #97661 ) ),
 .UNSPECIFIED., .F., .F., .F. ) 
 B_SPLINE_SURFACE_WITH_KNOTS ( ( 4, 4 ),
 ( 3, 3 ),
 ( 0.0006461284895274125748, 0.0007503702773986283599 ),
 ( 0.000000000000000000, 1.000000000000000000 ),
 .UNSPECIFIED. ) 
 GEOMETRIC_REPRESENTATION_ITEM ( )  RATIONAL_B_SPLINE_SURFACE ( (
 ( 1.000000000000000000, 0.7071067811865475727, 1.000000000000000000),
 ( 1.000000000000000000, 0.7076476444649285602, 1.000000000000000000),
 ( 1.000000000000000000, 0.7075727925191765966, 1.000000000000000000),
 ( 1.000000000000000000, 0.7071067811865670016, 1.000000000000000000) ) ) 
 REPRESENTATION_ITEM ( '' )  SURFACE ( )  );
#166739 = ORIENTED_EDGE ( 'NONE', *, *, #234663, .F. ) ;
#166740 = AXIS2_PLACEMENT_3D ( 'NONE', #150401, #172570, #149116 ) ;
#166741 = EDGE_CURVE ( 'NONE', #209763, #227236, #7889, .T. ) ;
#166742 = DIRECTION ( 'NONE',  ( 2.465190328815661345E-32, -0.8814952561688430555, 0.4721928772777344574 ) ) ;
#166743 = ORIENTED_EDGE ( 'NONE', *, *, #64967, .F. ) ;
#166744 = CYLINDRICAL_SURFACE ( 'NONE', #183532, 14.30833333333335133 ) ;
#166745 = EDGE_CURVE ( 'NONE', #211171, #48243, #67838, .T. ) ;
#166746 = CARTESIAN_POINT ( 'NONE',  ( -20.85000000000000142, 7.788796164756791818, -245.4641525896719543 ) ) ;
#166747 = CARTESIAN_POINT ( 'NONE',  ( 21.04105312098488056, 61.89240493045525682, -221.6333095009565284 ) ) ;
#166748 = CARTESIAN_POINT ( 'NONE',  ( 20.97250901189795513, 65.37543196631044395, -162.3585617675574326 ) ) ;
#166749 = VECTOR ( 'NONE', #55378, 1000.000000000000000 ) ;
#166750 = EDGE_LOOP ( 'NONE', ( #3816, #160314, #111976, #53985 ) ) ;
#166752 = AXIS2_PLACEMENT_3D ( 'NONE', #115633, #213440, #116915 ) ;
#166751 = DIRECTION ( 'NONE',  ( 0.000000000000000000, -6.938893903907222067E-15, 1.000000000000000000 ) ) ;
#166753 = DIRECTION ( 'NONE',  ( 1.000000000000000000, 0.000000000000000000, 0.000000000000000000 ) ) ;
#166754 =( NAMED_UNIT ( * ) PLANE_ANGLE_UNIT ( ) SI_UNIT ( $, .RADIAN. ) );
#166755 = DIRECTION ( 'NONE',  ( 1.000000000000000000, 0.000000000000000000, 0.000000000000000000 ) ) ;
#166756 = EDGE_CURVE ( 'NONE', #126916, #226829, #48275, .T. ) ;
#166757 = LINE ( 'NONE', #54133, #180873 ) ;
#166758 = CARTESIAN_POINT ( 'NONE',  ( 22.39999999999999503, 76.00000000001246292, -181.6726782920691505 ) ) ;
#166759 = ORIENTED_EDGE ( 'NONE', *, *, #199017, .F. ) ;
#166760 = ORIENTED_EDGE ( 'NONE', *, *, #35184, .T. ) ;
#166761 = CARTESIAN_POINT ( 'NONE',  ( 22.50000000000000000, 25.89490299898616854, -254.2637355452866927 ) ) ;
#166762 = CARTESIAN_POINT ( 'NONE',  ( 22.49806830649814060, 11.64988965485023620, -167.4225356836744538 ) ) ;
#166763 = CARTESIAN_POINT ( 'NONE',  ( 18.39999999999999147, 8.822561741677553471, -176.7499999999999716 ) ) ;
#166764 = CARTESIAN_POINT ( 'NONE',  ( -23.15000000000000213, 1.115600667400684642E-11, -67.00000000000004263 ) ) ;
#166765 = DIRECTION ( 'NONE',  ( 0.000000000000000000, 0.8814952561688437216, -0.4721928772777334582 ) ) ;
#166766 = EDGE_CURVE ( 'NONE', #203688, #217036, #38634, .T. ) ;
#166767 = ORIENTED_EDGE ( 'NONE', *, *, #242295, .T. ) ;
#166768 = LINE ( 'NONE', #29824, #155581 ) ;
#166769 = DIRECTION ( 'NONE',  ( 0.000000000000000000, -1.000000000000000000, 0.000000000000000000 ) ) ;
#166770 = ORIENTED_EDGE ( 'NONE', *, *, #122796, .T. ) ;
#166771 = CARTESIAN_POINT ( 'NONE',  ( -21.64999999999999858, 9.349999999999978328, -12.65000000000000213 ) ) ;
#166772 = VECTOR ( 'NONE', #146579, 1000.000000000000000 ) ;
#166773 = B_SPLINE_CURVE_WITH_KNOTS ( 'NONE', 3,
 ( #188338, #106208, #130931, #8424, #167519, #69693, #170105, #210478, #247012, #249607 ),
 .UNSPECIFIED., .F., .F.,
 ( 4, 3, 3, 4 ),
 ( 0.000000000000000000, 4.874959354404207151E-05, 9.785140065121151641E-05, 0.0001360444631936073986 ),
 .UNSPECIFIED. ) ;
#166774 = ORIENTED_EDGE ( 'NONE', *, *, #190035, .F. ) ;
#166775 = VERTEX_POINT ( 'NONE', #31324 ) ;
#166776 = CIRCLE ( 'NONE', #158400, 0.09999999999999939493 ) ;
#166777 = ORIENTED_EDGE ( 'NONE', *, *, #35868, .F. ) ;
#166778 = CARTESIAN_POINT ( 'NONE',  ( 21.05000000000000071, 10.60832956796507531, -74.59168501329543233 ) ) ;
#166779 = LINE ( 'NONE', #65072, #142275 ) ;
#166780 = CARTESIAN_POINT ( 'NONE',  ( 18.49999999999999289, 65.50857864377520912, -178.6731074845244223 ) ) ;
#166781 = EDGE_CURVE ( 'NONE', #252297, #250592, #91268, .T. ) ;
#166782 = CARTESIAN_POINT ( 'NONE',  ( 18.47688499308724985, -9.464855950272976770, -140.7013477531374406 ) ) ;
#166783 = FACE_OUTER_BOUND ( 'NONE', #95655, .T. ) ;
#166784 = CARTESIAN_POINT ( 'NONE',  ( -23.15000000000000213, 76.00000000001195133, -103.0231074845243171 ) ) ;
#166785 = DIRECTION ( 'NONE',  ( 0.000000000000000000, 0.000000000000000000, 1.000000000000000000 ) ) ;
#166787 = DIRECTION ( 'NONE',  ( -0.000000000000000000, 0.4791956752371485107, 0.8777080977375185666 ) ) ;
#166786 = CARTESIAN_POINT ( 'NONE',  ( 20.95017935633852346, 10.47548927963648246, -108.0774397973905252 ) ) ;
#166788 = CARTESIAN_POINT ( 'NONE',  ( -23.15000000000000213, 41.46275801244657799, -260.2743004338703940 ) ) ;
#166789 = CARTESIAN_POINT ( 'NONE',  ( -16.87331047859651179, 9.950000000011142376, -113.1500000000000341 ) ) ;
#166790 = CARTESIAN_POINT ( 'NONE',  ( -18.59999999999999787, 64.35000000001150511, -48.17310748452440095 ) ) ;
#166791 = DIRECTION ( 'NONE',  ( 0.000000000000000000, 0.000000000000000000, -1.000000000000000000 ) ) ;
#166792 = VECTOR ( 'NONE', #33399, 1000.000000000000000 ) ;
#166793 = ORIENTED_EDGE ( 'NONE', *, *, #203534, .T. ) ;
#166794 = EDGE_LOOP ( 'NONE', ( #136943, #101394, #105885, #109748 ) ) ;
#166795 = CARTESIAN_POINT ( 'NONE',  ( -23.25000000000000000, 76.00000000001190870, -103.0231074845243029 ) ) ;
#166796 = TOROIDAL_SURFACE ( 'NONE', #212573, 1.900000000000002576, 0.1000000000000000056 ) ;
#166797 = DIRECTION ( 'NONE',  ( -3.265361837132813093E-16, -1.000000000000000000, -6.938893903907222067E-15 ) ) ;
#166799 = CARTESIAN_POINT ( 'NONE',  ( -15.57281606413133090, 12.88553809045803611, -216.1303193953969526 ) ) ;
#166798 = DIRECTION ( 'NONE',  ( 1.000000000000000000, 0.000000000000000000, 0.000000000000000000 ) ) ;
#166800 = EDGE_CURVE ( 'NONE', #206320, #123343, #52114, .T. ) ;
#166801 = AXIS2_PLACEMENT_3D ( 'NONE', #232473, #113778, #214174 ) ;
#166802 = CARTESIAN_POINT ( 'NONE',  ( 20.95203847575071521, 39.27146918321979996, -236.8741184434562683 ) ) ;
#166803 = CARTESIAN_POINT ( 'NONE',  ( 20.94999999999999929, 70.50000000001180922, -81.92837350343744163 ) ) ;
#166804 = CARTESIAN_POINT ( 'NONE',  ( -22.39999999999999858, 7.612336166715881092, -199.3421143478784359 ) ) ;
#166805 = VERTEX_POINT ( 'NONE', #55959 ) ;
#166807 = EDGE_CURVE ( 'NONE', #187777, #59145, #138384, .T. ) ;
#166806 = AXIS2_PLACEMENT_3D ( 'NONE', #109359, #127670, #106800 ) ;
#166808 = ORIENTED_EDGE ( 'NONE', *, *, #130190, .F. ) ;
#166809 = ORIENTED_EDGE ( 'NONE', *, *, #98752, .F. ) ;
#166810 = EDGE_CURVE ( 'NONE', #34173, #103882, #125916, .T. ) ;
#166811 = CARTESIAN_POINT ( 'NONE',  ( -21.05000000000000071, 11.65000000001115588, -193.9851942293460070 ) ) ;
#166812 = CIRCLE ( 'NONE', #233439, 0.4000000000000114575 ) ;
#166813 = VECTOR ( 'NONE', #190814, 1000.000000000000000 ) ;
#166814 = CARTESIAN_POINT ( 'NONE',  ( -20.64999999999999858, 85.00000000001261924, -193.6291383618718385 ) ) ;
#166815 = VECTOR ( 'NONE', #51165, 1000.000000000000000 ) ;
#166816 = AXIS2_PLACEMENT_3D ( 'NONE', #10507, #88719, #54745 ) ;
#166817 = EDGE_LOOP ( 'NONE', ( #218702, #211540, #224818, #174396, #141930 ) ) ;
#166818 = CARTESIAN_POINT ( 'NONE',  ( -18.59999999999999787, 1.261786168576181755, -142.0864989635454947 ) ) ;
#166819 = ADVANCED_FACE ( 'NONE', ( #54695 ), #242638, .T. ) ;
#166820 = VERTEX_POINT ( 'NONE', #251618 ) ;
#166821 = CARTESIAN_POINT ( 'NONE',  ( -18.79999999999999716, 4.513204987021263825, 22.00000000000000355 ) ) ;
#166822 = DIRECTION ( 'NONE',  ( -1.000000000000000000, 0.000000000000000000, 0.000000000000000000 ) ) ;
#166823 = CARTESIAN_POINT ( 'NONE',  ( -22.50000000000000000, 75.90000000001194280, -103.0231074845243171 ) ) ;
#166824 = ADVANCED_FACE ( 'NONE', ( #50818 ), #191681, .F. ) ;
#166825 = DIRECTION ( 'NONE',  ( 0.000000000000000000, 0.000000000000000000, -1.000000000000000000 ) ) ;
#166826 = EDGE_CURVE ( 'NONE', #61931, #82879, #173419, .T. ) ;
#166827 = DIRECTION ( 'NONE',  ( 0.000000000000000000, 0.000000000000000000, 1.000000000000000000 ) ) ;
#166828 = CIRCLE ( 'NONE', #75232, 0.1000000000000028644 ) ;
#166829 = CARTESIAN_POINT ( 'NONE',  ( -16.98495255085917321, 10.00556436599476129, -20.86538279377949578 ) ) ;
#166830 = DIRECTION ( 'NONE',  ( 2.465190328815662439E-32, -0.9126074666063770380, -0.4088369013363282178 ) ) ;
#166831 = CARTESIAN_POINT ( 'NONE',  ( -22.39999999999999858, -3.140208063160686791, -228.2318569537739847 ) ) ;
#166833 = ORIENTED_EDGE ( 'NONE', *, *, #124172, .F. ) ;
#166832 = CARTESIAN_POINT ( 'NONE',  ( -18.50000000000000000, -1.637172712959223952, -145.5821533654720383 ) ) ;
#166835 = DIRECTION ( 'NONE',  ( 1.000000000000000000, 0.000000000000000000, 0.000000000000000000 ) ) ;
#166834 = CARTESIAN_POINT ( 'NONE',  ( -16.77732147262506146, 66.05403306739336244, -115.6866162412485011 ) ) ;
#166836 = ORIENTED_EDGE ( 'NONE', *, *, #224514, .T. ) ;
#166838 = VERTEX_POINT ( 'NONE', #92528 ) ;
#166837 = CARTESIAN_POINT ( 'NONE',  ( -18.59999999999999787, 64.25000000001179501, -81.77310748452438816 ) ) ;
#166839 = ORIENTED_EDGE ( 'NONE', *, *, #201949, .F. ) ;
#166840 = CARTESIAN_POINT ( 'NONE',  ( -20.64999999999999858, 74.00000000001151079, -49.24772940728643533 ) ) ;
#166841 = DIRECTION ( 'NONE',  ( 0.000000000000000000, -1.000000000000000000, -6.982962677686265922E-15 ) ) ;
#166842 = EDGE_CURVE ( 'NONE', #45318, #31293, #13519, .T. ) ;
#166843 = CARTESIAN_POINT ( 'NONE',  ( 21.04999999999999716, 0.09843750001147472117, -127.7007690899077090 ) ) ;
#166844 = CARTESIAN_POINT ( 'NONE',  ( -22.57320508075687115, 11.48087284840413425, -198.4995883060917663 ) ) ;
#166845 = CARTESIAN_POINT ( 'NONE',  ( -15.75000000000000355, 47.91805600923872532, -233.7139610577891631 ) ) ;
#166846 = ADVANCED_FACE ( 'NONE', ( #115970 ), #73018, .T. ) ;
#166847 = EDGE_CURVE ( 'NONE', #14291, #16570, #195523, .T. ) ;
#166848 = CARTESIAN_POINT ( 'NONE',  ( 20.73486653747088937, 7.750000000011182166, -79.65000000000004832 ) ) ;
#166849 = DIRECTION ( 'NONE',  ( -0.000000000000000000, -6.982962677686266711E-15, 1.000000000000000000 ) ) ;
#166850 = AXIS2_PLACEMENT_3D ( 'NONE', #140900, #156644, #220440 ) ;
#166851 = DIRECTION ( 'NONE',  ( 1.000000000000000000, 2.885090398161910739E-16, 6.283419270304611573E-17 ) ) ;
#166852 = VECTOR ( 'NONE', #80587, 1000.000000000000000 ) ;
#166853 = CARTESIAN_POINT ( 'NONE',  ( -21.04999999999994387, 83.97335046823651794, -37.38386894789040582 ) ) ;
#166854 = VERTEX_POINT ( 'NONE', #212511 ) ;
#166855 = VERTEX_POINT ( 'NONE', #16874 ) ;
#166856 = DIRECTION ( 'NONE',  ( 0.000000000000000000, -1.000000000000000000, -7.272083257015735086E-15 ) ) ;
#166857 = CIRCLE ( 'NONE', #25188, 0.1000000000000000749 ) ;
#166858 = EDGE_LOOP ( 'NONE', ( #156426, #208790, #171816, #216548, #236662, #250641 ) ) ;
#166859 = CARTESIAN_POINT ( 'NONE',  ( 20.94999999999999929, 65.61821452928744236, -30.51526212064022303 ) ) ;
#166860 = ORIENTED_EDGE ( 'NONE', *, *, #65183, .F. ) ;
#166861 = DIRECTION ( 'NONE',  ( -1.000000000000000000, -0.000000000000000000, -0.000000000000000000 ) ) ;
#166862 = TOROIDAL_SURFACE ( 'NONE', #88246, 0.4000000000000012990, 0.1000000000000000056 ) ;
#166863 = EDGE_CURVE ( 'NONE', #12698, #149927, #233368, .T. ) ;
#166864 = CARTESIAN_POINT ( 'NONE',  ( -22.47120815636973745, -2.450875325420101447, -189.6107523991855146 ) ) ;
#166865 = EDGE_CURVE ( 'NONE', #160419, #28788, #46808, .T. ) ;
#166866 = CARTESIAN_POINT ( 'NONE',  ( -23.15000000000000213, 11.65000000001115588, -121.8500000000000227 ) ) ;
#166867 = DIRECTION ( 'NONE',  ( 0.000000000000000000, 0.8814952561688429444, -0.4721928772777348460 ) ) ;
#166868 = ORIENTED_EDGE ( 'NONE', *, *, #135944, .T. ) ;
#166869 = DIRECTION ( 'NONE',  ( 1.000000000000000000, 0.000000000000000000, 0.000000000000000000 ) ) ;
#166870 = CIRCLE ( 'NONE', #229, 0.1000000000000028644 ) ;
#166871 = EDGE_CURVE ( 'NONE', #156138, #167773, #75575, .T. ) ;
#166872 = CARTESIAN_POINT ( 'NONE',  ( -23.25000000000000000, -1.149570369564537842, -175.3159124845019790 ) ) ;
#166873 = FACE_OUTER_BOUND ( 'NONE', #249639, .T. ) ;
#166874 = CARTESIAN_POINT ( 'NONE',  ( -23.15000000000000213, 1.910280373842936141, -79.63136785519898808 ) ) ;
#166875 = VERTEX_POINT ( 'NONE', #70453 ) ;
#166878 = CARTESIAN_POINT ( 'NONE',  ( -20.94999999999999929, 1.835341550235569663, -112.0551512925630249 ) ) ;
#166877 = DIRECTION ( 'NONE',  ( 0.000000000000000000, -6.982962677686267499E-15, 1.000000000000000000 ) ) ;
#166876 = AXIS2_PLACEMENT_3D ( 'NONE', #84516, #3747, #83254 ) ;
#166879 = ORIENTED_EDGE ( 'NONE', *, *, #155351, .T. ) ;
#166881 = ORIENTED_EDGE ( 'NONE', *, *, #146510, .F. ) ;
#166880 = CARTESIAN_POINT ( 'NONE',  ( -17.78043020864320667, 10.85359211201684637, -56.66304916572023131 ) ) ;
#166882 = AXIS2_PLACEMENT_3D ( 'NONE', #10144, #213470, #131365 ) ;
#166883 = VERTEX_POINT ( 'NONE', #74299 ) ;
#166884 = CARTESIAN_POINT ( 'NONE',  ( 18.49999999999999645, 22.88260507592945814, -249.4775442468528013 ) ) ;
#166885 = AXIS2_PLACEMENT_3D ( 'NONE', #103396, #65575, #64298 ) ;
#166886 = DIRECTION ( 'NONE',  ( 0.000000000000000000, 1.000000000000000000, -6.308085367188393199E-16 ) ) ;
#166887 = CARTESIAN_POINT ( 'NONE',  ( -18.41418431465367789, 85.50000000001210765, -96.42291809330278340 ) ) ;
#166888 = ORIENTED_EDGE ( 'NONE', *, *, #180062, .T. ) ;
#166889 = CARTESIAN_POINT ( 'NONE',  ( -23.25000000000000000, 76.00000000001240608, -174.1731074845243654 ) ) ;
#166890 = FACE_OUTER_BOUND ( 'NONE', #155754, .T. ) ;
#166892 = CARTESIAN_POINT ( 'NONE',  ( -18.50000000000000000, 1.115600667400684642E-11, -167.5000000000000284 ) ) ;
#166891 = DIRECTION ( 'NONE',  ( 0.000000000000000000, 0.008583690987124100932, -0.9999631594459055250 ) ) ;
#166894 = VERTEX_POINT ( 'NONE', #149975 ) ;
#166893 = DIRECTION ( 'NONE',  ( -1.000000000000000000, 0.000000000000000000, 0.000000000000000000 ) ) ;
#166895 = EDGE_CURVE ( 'NONE', #168194, #208880, #180122, .T. ) ;
#166896 = CIRCLE ( 'NONE', #208575, 0.09999999999999939493 ) ;
#166897 = VERTEX_POINT ( 'NONE', #170855 ) ;
#166898 = EDGE_CURVE ( 'NONE', #43405, #104735, #80102, .T. ) ;
#166899 = DIRECTION ( 'NONE',  ( 0.000000000000000000, 0.2128009952263403282, -0.9770955615653358350 ) ) ;
#166900 = DIRECTION ( 'NONE',  ( 0.000000000000000000, 0.000000000000000000, 1.000000000000000000 ) ) ;
#166901 = DIRECTION ( 'NONE',  ( -0.7070776581709311559, 0.000000000000000000, 0.7071359030027479786 ) ) ;
#166902 = ORIENTED_EDGE ( 'NONE', *, *, #156874, .T. ) ;
#166903 = DIRECTION ( 'NONE',  ( -1.000000000000000000, -0.000000000000000000, 0.000000000000000000 ) ) ;
#166904 = EDGE_CURVE ( 'NONE', #86370, #8189, #117245, .T. ) ;
#166905 = DIRECTION ( 'NONE',  ( -0.000000000000000000, -0.8700118002898321601, 0.4930308989875230030 ) ) ;
#166906 = DIRECTION ( 'NONE',  ( -0.000000000000000000, 0.8700118002898356018, -0.4930308989875170078 ) ) ;
#166907 = EDGE_LOOP ( 'NONE', ( #210466, #235866, #208375, #250304 ) ) ;
#166908 = DIRECTION ( 'NONE',  ( 0.000000000000000000, -1.000000000000000000, 0.000000000000000000 ) ) ;
#166909 = EDGE_CURVE ( 'NONE', #55547, #165825, #237195, .T. ) ;
#166910 = VECTOR ( 'NONE', #220260, 1000.000000000000000 ) ;
#166911 = EDGE_CURVE ( 'NONE', #18090, #184441, #142666, .T. ) ;
#166912 = VERTEX_POINT ( 'NONE', #181084 ) ;
#166913 = AXIS2_PLACEMENT_3D ( 'NONE', #140043, #22718, #81342 ) ;
#166914 = CARTESIAN_POINT ( 'NONE',  ( -11.60000000000000320, -8.350000000000004974, 19.04142135623731491 ) ) ;
#166915 = CARTESIAN_POINT ( 'NONE',  ( 20.94999999999999929, 4.898587196589411843E-16, -29.50000000000000355 ) ) ;
#166916 = EDGE_CURVE ( 'NONE', #158102, #235411, #42729, .T. ) ;
#166917 = ORIENTED_EDGE ( 'NONE', *, *, #250128, .F. ) ;
#166918 = VECTOR ( 'NONE', #52548, 1000.000000000000000 ) ;
#166919 = ORIENTED_EDGE ( 'NONE', *, *, #192417, .F. ) ;
#166921 = EDGE_CURVE ( 'NONE', #81149, #183114, #98926, .T. ) ;
#166920 = EDGE_CURVE ( 'NONE', #20048, #156829, #163539, .T. ) ;
#166922 = DIRECTION ( 'NONE',  ( 1.000000000000000000, 0.000000000000000000, -0.000000000000000000 ) ) ;
#166923 = EDGE_LOOP ( 'NONE', ( #186941, #255319, #77753, #216581, #228721, #193901 ) ) ;
#166925 = ORIENTED_EDGE ( 'NONE', *, *, #218763, .T. ) ;
#166924 = CARTESIAN_POINT ( 'NONE',  ( -22.50000000000094147, 0.1000000000110504439, -155.8504291924551524 ) ) ;
#166926 = VERTEX_POINT ( 'NONE', #175959 ) ;
#166927 = CIRCLE ( 'NONE', #162619, 0.9750000000000036415 ) ;
#166929 = EDGE_LOOP ( 'NONE', ( #151434, #116926, #133650, #184282 ) ) ;
#166928 = ORIENTED_EDGE ( 'NONE', *, *, #171541, .F. ) ;
#166930 = CARTESIAN_POINT ( 'NONE',  ( 20.99999999999999645, 66.25000000001233502, -160.7731074845244166 ) ) ;
#166931 = ORIENTED_EDGE ( 'NONE', *, *, #64242, .T. ) ;
#166932 = CARTESIAN_POINT ( 'NONE',  ( -23.15000000000000213, 76.00000000001142553, -36.02310748452432421 ) ) ;
#166933 = DIRECTION ( 'NONE',  ( -1.000000000000000000, 0.000000000000000000, 0.000000000000000000 ) ) ;
#166934 = EDGE_CURVE ( 'NONE', #203964, #6496, #230163, .T. ) ;
#166935 = EDGE_CURVE ( 'NONE', #193788, #214956, #214075, .T. ) ;
#166936 = CARTESIAN_POINT ( 'NONE',  ( 21.05000000000000071, 69.52293297888719792, -102.9231074845243654 ) ) ;
#166937 = DIRECTION ( 'NONE',  ( 0.000000000000000000, -6.982962677686266711E-15, 1.000000000000000000 ) ) ;
#166938 = ORIENTED_EDGE ( 'NONE', *, *, #127580, .F. ) ;
#166939 = ORIENTED_EDGE ( 'NONE', *, *, #194246, .T. ) ;
#166940 = EDGE_CURVE ( 'NONE', #24198, #188307, #39316, .T. ) ;
#166941 = FACE_OUTER_BOUND ( 'NONE', #157868, .T. ) ;
#166943 = ORIENTED_EDGE ( 'NONE', *, *, #91634, .T. ) ;
#166942 = FACE_OUTER_BOUND ( 'NONE', #74245, .T. ) ;
#166944 = CARTESIAN_POINT ( 'NONE',  ( -16.86733706339143879, 14.18592885272122217, -219.3035684813490320 ) ) ;
#166946 = VERTEX_POINT ( 'NONE', #220199 ) ;
#166945 = CARTESIAN_POINT ( 'NONE',  ( -23.25000000000000000, 41.46275801244657799, -260.2743004338703940 ) ) ;
#166947 = CIRCLE ( 'NONE', #71063, 0.1000000000000028644 ) ;
#166948 = ORIENTED_EDGE ( 'NONE', *, *, #64638, .F. ) ;
#166949 = ADVANCED_FACE ( 'NONE', ( #81920 ), #140646, .F. ) ;
#166950 = CARTESIAN_POINT ( 'NONE',  ( -23.25000000000000000, 47.66483718802935954, -241.7716698398223514 ) ) ;
#166951 = EDGE_CURVE ( 'NONE', #86948, #202965, #251681, .T. ) ;
#166952 = AXIS2_PLACEMENT_3D ( 'NONE', #184661, #8607, #6018 ) ;
#166953 = ORIENTED_EDGE ( 'NONE', *, *, #223244, .F. ) ;
#166954 = ORIENTED_EDGE ( 'NONE', *, *, #111394, .T. ) ;
#166956 = AXIS2_PLACEMENT_3D ( 'NONE', #53305, #165893, #36325 ) ;
#166955 = DIRECTION ( 'NONE',  ( -0.000000000000000000, 1.000000000000000000, -0.000000000000000000 ) ) ;
#166957 = DIRECTION ( 'NONE',  ( 0.000000000000000000, 0.000000000000000000, 1.000000000000000000 ) ) ;
#166959 = VERTEX_POINT ( 'NONE', #198054 ) ;
#166958 = VERTEX_POINT ( 'NONE', #40308 ) ;
#166960 = ORIENTED_EDGE ( 'NONE', *, *, #66518, .T. ) ;
#166961 = CARTESIAN_POINT ( 'NONE',  ( -18.59999999999999787, -1.164121893230052995, -141.7148480855716457 ) ) ;
#166962 = ORIENTED_EDGE ( 'NONE', *, *, #211279, .T. ) ;
#166963 = ORIENTED_EDGE ( 'NONE', *, *, #253966, .F. ) ;
#166964 = DIRECTION ( 'NONE',  ( 0.000000000000000000, 0.000000000000000000, -1.000000000000000000 ) ) ;
#166966 = ORIENTED_EDGE ( 'NONE', *, *, #210423, .T. ) ;
#166965 = FACE_OUTER_BOUND ( 'NONE', #100384, .T. ) ;
#166967 = EDGE_CURVE ( 'NONE', #177256, #113573, #147616, .T. ) ;
#166968 = LINE ( 'NONE', #10432, #94212 ) ;
#166969 = EDGE_CURVE ( 'NONE', #119125, #202859, #53727, .T. ) ;
#166971 = CARTESIAN_POINT ( 'NONE',  ( 21.14999999999999503, 11.65000000001116298, -33.60000000000000142 ) ) ;
#166970 = CARTESIAN_POINT ( 'NONE',  ( 21.14999999999999858, 6.650000000011155876, -45.75000000000000711 ) ) ;
#166972 = CARTESIAN_POINT ( 'NONE',  ( 18.59999999999999787, 80.78317333349157536, -192.9003134612049166 ) ) ;
#166973 = CARTESIAN_POINT ( 'NONE',  ( -18.59999999999999787, 66.75000000001185185, -90.67310748452436542 ) ) ;
#166974 = ORIENTED_EDGE ( 'NONE', *, *, #257181, .T. ) ;
#166975 = EDGE_LOOP ( 'NONE', ( #154471, #28713, #123188, #48151, #58188, #32536, #150888 ) ) ;
#166976 = EDGE_CURVE ( 'NONE', #189647, #39898, #1056, .T. ) ;
#166977 = DIRECTION ( 'NONE',  ( 0.000000000000000000, -0.6728971962616792091, 0.7397360091702790408 ) ) ;
#166978 =( LENGTH_UNIT ( ) NAMED_UNIT ( * ) SI_UNIT ( .MILLI., .METRE. ) );
#166980 = ORIENTED_EDGE ( 'NONE', *, *, #183820, .F. ) ;
#166979 = CIRCLE ( 'NONE', #237849, 0.09999999999999939493 ) ;
#166981 = AXIS2_PLACEMENT_3D ( 'NONE', #94005, #95304, #146586 ) ;
#166982 = TOROIDAL_SURFACE ( 'NONE', #29599, 11.65000000000000036, 0.1000000000000000056 ) ;
#166983 = CARTESIAN_POINT ( 'NONE',  ( 20.94999999999999574, 77.36087058720467269, -195.4501095574333931 ) ) ;
#166984 = EDGE_LOOP ( 'NONE', ( #77659, #105634, #228648, #139914, #23328 ) ) ;
#166985 = ORIENTED_EDGE ( 'NONE', *, *, #74370, .F. ) ;
#166986 = AXIS2_PLACEMENT_3D ( 'NONE', #33989, #95202, #75661 ) ;
#166987 = LINE ( 'NONE', #89963, #9267 ) ;
#166988 = EDGE_CURVE ( 'NONE', #89559, #108947, #183422, .T. ) ;
#166989 = DIRECTION ( 'NONE',  ( 0.000000000000000000, -0.8700118002898354908, 0.4930308989875170078 ) ) ;
#166990 = VERTEX_POINT ( 'NONE', #207051 ) ;
#166991 = CARTESIAN_POINT ( 'NONE',  ( -23.25000000000000000, 82.67551891922275331, -215.5849511313000164 ) ) ;
#166992 = ORIENTED_EDGE ( 'NONE', *, *, #87337, .F. ) ;
#166993 = CARTESIAN_POINT ( 'NONE',  ( 19.75857864376269291, 64.35000000001220144, -145.2731074845244166 ) ) ;
#166995 = TOROIDAL_SURFACE ( 'NONE', #200264, 0.2000000000000000111, 0.1000000000000000056 ) ;
#166994 = CARTESIAN_POINT ( 'NONE',  ( -21.05000000000000071, 70.10000000001213039, -126.3040077198679398 ) ) ;
#166997 = FACE_OUTER_BOUND ( 'NONE', #82760, .T. ) ;
#166996 = LINE ( 'NONE', #28780, #186379 ) ;
#166998 = CARTESIAN_POINT ( 'NONE',  ( 19.75857864376269291, 11.65000000001116476, -91.75000000000005684 ) ) ;
#166999 = CARTESIAN_POINT ( 'NONE',  ( -18.50000000000000000, 85.50000000001161027, -61.42310748452425884 ) ) ;
#167000 = CARTESIAN_POINT ( 'NONE',  ( -23.25000000000000000, 1.115600667400684642E-11, -171.5499999999999829 ) ) ;
#167001 = CARTESIAN_POINT ( 'NONE',  ( -20.94999999999999929, 11.65000000001115588, -141.0148057706540214 ) ) ;
#167002 = ORIENTED_EDGE ( 'NONE', *, *, #162944, .T. ) ;
#167003 = EDGE_CURVE ( 'NONE', #146896, #14013, #66256, .T. ) ;
#167004 = AXIS2_PLACEMENT_3D ( 'NONE', #84694, #83420, #221658 ) ;
#167005 = CIRCLE ( 'NONE', #129361, 0.09999999999999481526 ) ;
#167006 = CIRCLE ( 'NONE', #225197, 0.5000000000000004441 ) ;
#167007 = CIRCLE ( 'NONE', #200281, 0.09999999999998898659 ) ;
#167009 = ORIENTED_EDGE ( 'NONE', *, *, #171731, .F. ) ;
#167008 = ORIENTED_EDGE ( 'NONE', *, *, #115294, .F. ) ;
#167010 = ORIENTED_EDGE ( 'NONE', *, *, #170635, .T. ) ;
#167011 = DIRECTION ( 'NONE',  ( 3.616040088954497272E-32, -1.224646799147352961E-16, 1.000000000000000000 ) ) ;
#167012 = DIRECTION ( 'NONE',  ( 0.000000000000000000, -6.982962677686266711E-15, 1.000000000000000000 ) ) ;
#167014 = CARTESIAN_POINT ( 'NONE',  ( -15.75000000000000355, 9.349999999999983658, -16.52151937182510366 ) ) ;
#167013 = CARTESIAN_POINT ( 'NONE',  ( -20.64999999999999858, 74.00000000001229239, -156.7984855617622770 ) ) ;
#167015 = DIRECTION ( 'NONE',  ( 0.000000000000000000, 0.000000000000000000, -1.000000000000000000 ) ) ;
#167016 = ORIENTED_EDGE ( 'NONE', *, *, #66852, .T. ) ;
#167017 = CARTESIAN_POINT ( 'NONE',  ( -22.59999985501179154, 11.74986979301414358, -100.4344013302006857 ) ) ;
#167018 = CIRCLE ( 'NONE', #75421, 0.5000000000000008882 ) ;
#167019 = CARTESIAN_POINT ( 'NONE',  ( -20.85000000000000142, -1.149570369564537842, -175.3159124845019790 ) ) ;
#167020 = DIRECTION ( 'NONE',  ( -1.000000000000000000, 0.000000000000000000, 0.000000000000000000 ) ) ;
#167021 = DIRECTION ( 'NONE',  ( 1.000000000000000000, 1.394253735153569469E-16, 2.602809386958778209E-16 ) ) ;
#167022 = VERTEX_POINT ( 'NONE', #128804 ) ;
#167023 = FACE_OUTER_BOUND ( 'NONE', #219920, .T. ) ;
#167024 = DIRECTION ( 'NONE',  ( -1.000000000000000000, 0.000000000000000000, 0.000000000000000000 ) ) ;
#167025 = ORIENTED_EDGE ( 'NONE', *, *, #7748, .T. ) ;
#167026 = ORIENTED_EDGE ( 'NONE', *, *, #131697, .F. ) ;
#167027 = FACE_OUTER_BOUND ( 'NONE', #94932, .T. ) ;
#167028 = CARTESIAN_POINT ( 'NONE',  ( 18.59999999999999432, -1.162701749926853712, -142.0000000000000284 ) ) ;
#167029 = DIRECTION ( 'NONE',  ( 0.000000000000000000, 0.000000000000000000, 1.000000000000000000 ) ) ;
#167030 = DIRECTION ( 'NONE',  ( -0.000000000000000000, -1.000000000000000000, 6.308085367188393199E-16 ) ) ;
#167031 = CARTESIAN_POINT ( 'NONE',  ( -18.59999999999999787, 11.65000000001115232, -88.25000000000005684 ) ) ;
#167032 = FACE_OUTER_BOUND ( 'NONE', #184507, .T. ) ;
#167033 = ORIENTED_EDGE ( 'NONE', *, *, #160278, .F. ) ;
#167034 = DIRECTION ( 'NONE',  ( -1.000000000000000000, 0.000000000000000000, -0.000000000000000000 ) ) ;
#167035 = CIRCLE ( 'NONE', #54558, 0.8750000000000007772 ) ;
#167036 = DIRECTION ( 'NONE',  ( -0.000000000000000000, -0.000000000000000000, 1.000000000000000000 ) ) ;
#167038 = CARTESIAN_POINT ( 'NONE',  ( -18.79999999999999716, 7.900000000000000355, -1.212568896937008089 ) ) ;
#167037 = CYLINDRICAL_SURFACE ( 'NONE', #32789, 0.09999999999999868716 ) ;
#167040 = EDGE_CURVE ( 'NONE', #87043, #193316, #247377, .T. ) ;
#167039 = FACE_OUTER_BOUND ( 'NONE', #222952, .T. ) ;
#167041 = DIRECTION ( 'NONE',  ( 1.000000000000000000, 0.000000000000000000, 0.000000000000000000 ) ) ;
#167042 = CYLINDRICAL_SURFACE ( 'NONE', #7955, 7.900000000000007461 ) ;
#167043 = DIRECTION ( 'NONE',  ( 0.000000000000000000, 0.000000000000000000, -1.000000000000000000 ) ) ;
#167046 = EDGE_LOOP ( 'NONE', ( #96452, #22569, #21118, #8464, #85746 ) ) ;
#167045 = AXIS2_PLACEMENT_3D ( 'NONE', #198637, #99510, #60403 ) ;
#167044 = CARTESIAN_POINT ( 'NONE',  ( -20.85000000000000142, -1.835859311432481045, -112.1044391687985780 ) ) ;
#167047 = AXIS2_PLACEMENT_3D ( 'NONE', #162520, #202902, #242027 ) ;
#167048 = EDGE_CURVE ( 'NONE', #121064, #231796, #47641, .T. ) ;
#167049 = DIRECTION ( 'NONE',  ( -1.000000000000000000, -3.265361837132813093E-16, 0.000000000000000000 ) ) ;
#167050 = ADVANCED_FACE ( 'NONE', ( #46669 ), #89170, .T. ) ;
#167051 = LINE ( 'NONE', #71792, #217428 ) ;
#167052 = DIRECTION ( 'NONE',  ( 0.000000000000000000, -1.756682000989173806E-15, 1.000000000000000000 ) ) ;
#167053 = AXIS2_PLACEMENT_3D ( 'NONE', #191405, #92257, #231798 ) ;
#167054 = EDGE_CURVE ( 'NONE', #155390, #154949, #139218, .T. ) ;
#167055 = ORIENTED_EDGE ( 'NONE', *, *, #92457, .F. ) ;
#167056 = CIRCLE ( 'NONE', #200339, 11.89999999999999325 ) ;
#167057 = DIRECTION ( 'NONE',  ( -1.000000000000000000, 0.000000000000000000, -0.000000000000000000 ) ) ;
#167058 = CYLINDRICAL_SURFACE ( 'NONE', #61872, 0.09999999999999939493 ) ;
#167060 = DIRECTION ( 'NONE',  ( 1.000000000000000000, 0.000000000000000000, 0.000000000000000000 ) ) ;
#167059 = AXIS2_PLACEMENT_3D ( 'NONE', #76733, #196679, #40213 ) ;
#167061 = EDGE_CURVE ( 'NONE', #217530, #183920, #172625, .T. ) ;
#167063 = VERTEX_POINT ( 'NONE', #123666 ) ;
#167062 = EDGE_CURVE ( 'NONE', #202918, #210551, #49252, .T. ) ;
#167064 = DIRECTION ( 'NONE',  ( 1.000000000000000000, 0.000000000000000000, 0.000000000000000000 ) ) ;
#167066 = ORIENTED_EDGE ( 'NONE', *, *, #179878, .T. ) ;
#167065 = LINE ( 'NONE', #164471, #242489 ) ;
#167067 = CARTESIAN_POINT ( 'NONE',  ( 21.14999999999999503, 76.10000000001245724, -181.6726782920691505 ) ) ;
#167068 = ADVANCED_FACE ( 'NONE', ( #247451, #106635, #148359 ), #162804, .F. ) ;
#167069 = DIRECTION ( 'NONE',  ( -1.000000000000000000, 0.000000000000000000, 0.000000000000000000 ) ) ;
#167070 = EDGE_LOOP ( 'NONE', ( #32750, #3906, #96409, #112096 ) ) ;
#167071 = CARTESIAN_POINT ( 'NONE',  ( -16.88705144915421030, 66.05000000001261640, -190.5921288898123009 ) ) ;
#167072 = CARTESIAN_POINT ( 'NONE',  ( 0.000000000000000000, 0.000000000000000000, 0.000000000000000000 ) ) ;
#167073 = CARTESIAN_POINT ( 'NONE',  ( -20.86777300164945004, 65.66799936921512426, -63.92993998886009877 ) ) ;
#167074 = CARTESIAN_POINT ( 'NONE',  ( 21.00000000000000000, 9.750000000011153745, -54.75000000000000000 ) ) ;
#167076 = EDGE_CURVE ( 'NONE', #62297, #201338, #186205, .T. ) ;
#167075 = CARTESIAN_POINT ( 'NONE',  ( -21.14999999999994174, 87.50449464844290048, -37.85861909827351468 ) ) ;
#167077 = AXIS2_PLACEMENT_3D ( 'NONE', #14560, #88916, #247998 ) ;
#167078 = ORIENTED_EDGE ( 'NONE', *, *, #226393, .T. ) ;
#167079 = DIRECTION ( 'NONE',  ( 0.000000000000000000, 0.000000000000000000, 1.000000000000000000 ) ) ;
#167080 = DIRECTION ( 'NONE',  ( -0.000000000000000000, -0.9126074666063771490, -0.4088369013363281623 ) ) ;
#167081 = SPHERICAL_SURFACE ( 'NONE', #188898, 0.1000000000000000056 ) ;
#167082 = CARTESIAN_POINT ( 'NONE',  ( 21.05000000000000071, 1.115600667400684642E-11, -67.00000000000000000 ) ) ;
#167083 = ORIENTED_EDGE ( 'NONE', *, *, #82052, .F. ) ;
#167084 = EDGE_LOOP ( 'NONE', ( #192156, #248604, #142116, #255753 ) ) ;
#167085 = CARTESIAN_POINT ( 'NONE',  ( 18.59999999999998721, 6.846123162363745074, -204.7377262668498190 ) ) ;
#167086 = ADVANCED_FACE ( 'NONE', ( #102778 ), #164076, .F. ) ;
#167087 = B_SPLINE_CURVE_WITH_KNOTS ( 'NONE', 3,
 ( #180579, #38505, #155902, #18922, #1914, #78879 ),
 .UNSPECIFIED., .F., .F.,
 ( 4, 2, 4 ),
 ( 0.000000000000000000, 0.0001497467027049226784, 0.0002994934054098453567 ),
 .UNSPECIFIED. ) ;
#167088 = CARTESIAN_POINT ( 'NONE',  ( 23.15000000000000213, -8.663551401857999323, -90.97589888193273566 ) ) ;
#167089 = FACE_OUTER_BOUND ( 'NONE', #174122, .T. ) ;
#167090 = AXIS2_PLACEMENT_3D ( 'NONE', #37251, #97152, #183179 ) ;
#167091 = CARTESIAN_POINT ( 'NONE',  ( 23.14999999999999858, 4.999999999999997335, -21.09473398108690390 ) ) ;
#167093 = CARTESIAN_POINT ( 'NONE',  ( 21.15000000000000213, 8.786607556611267356, -146.2500000000000568 ) ) ;
#167092 = CIRCLE ( 'NONE', #33830, 12.97499999999998721 ) ;
#167094 = AXIS2_PLACEMENT_3D ( 'NONE', #93653, #175780, #54523 ) ;
#167097 = FACE_OUTER_BOUND ( 'NONE', #208447, .T. ) ;
#167096 = CIRCLE ( 'NONE', #17056, 0.1000000000000028644 ) ;
#167095 = CARTESIAN_POINT ( 'NONE',  ( -17.11825945287482753, 12.53302308287915245, -211.3193184079345883 ) ) ;
#167098 = DIRECTION ( 'NONE',  ( -1.000000000000000000, 2.952720810173289112E-16, 2.061873921506763405E-30 ) ) ;
#167099 = CARTESIAN_POINT ( 'NONE',  ( -18.59999999999999787, 43.57568952063339651, -245.1784935019914826 ) ) ;
#167100 = DIRECTION ( 'NONE',  ( 1.000000000000000000, 0.000000000000000000, 0.000000000000000000 ) ) ;
#167101 = DIRECTION ( 'NONE',  ( -0.7071067811865475727, -0.7071067811865475727, -0.000000000000000000 ) ) ;
#167103 = ORIENTED_EDGE ( 'NONE', *, *, #202893, .T. ) ;
#167102 = CYLINDRICAL_SURFACE ( 'NONE', #115619, 1.749999999999998002 ) ;
#167104 = DIRECTION ( 'NONE',  ( -1.000000000000000000, 0.000000000000000000, 0.000000000000000000 ) ) ;
#167106 = DIRECTION ( 'NONE',  ( 0.000000000000000000, 0.000000000000000000, 1.000000000000000000 ) ) ;
#167105 = CARTESIAN_POINT ( 'NONE',  ( -18.40000000000000213, 11.75000000001113953, -79.65000000000004832 ) ) ;
#167107 = EDGE_CURVE ( 'NONE', #34471, #132760, #166669, .T. ) ;
#167108 = ORIENTED_EDGE ( 'NONE', *, *, #37917, .F. ) ;
#167109 = CARTESIAN_POINT ( 'NONE',  ( 23.14999999999999147, 1.115600667400684642E-11, -100.5000000000000284 ) ) ;
#167110 = DIRECTION ( 'NONE',  ( -0.000000000000000000, -0.2605042016806452532, -0.9654727137038777718 ) ) ;
#167111 = CARTESIAN_POINT ( 'NONE',  ( -20.94999999999999929, 1.115600667400684642E-11, -200.9999999999999432 ) ) ;
#167112 = CARTESIAN_POINT ( 'NONE',  ( -23.15000000000000213, 67.23127455305841238, -235.8551265064783991 ) ) ;
#167113 = FACE_OUTER_BOUND ( 'NONE', #62738, .T. ) ;
#167114 = EDGE_LOOP ( 'NONE', ( #188593, #215527, #226569, #125907 ) ) ;
#167116 = ORIENTED_EDGE ( 'NONE', *, *, #106507, .T. ) ;
#167115 = AXIS2_PLACEMENT_3D ( 'NONE', #159062, #177352, #79478 ) ;
#167117 = CYLINDRICAL_SURFACE ( 'NONE', #167623, 0.1000000000000024342 ) ;
#167118 = ORIENTED_EDGE ( 'NONE', *, *, #26444, .T. ) ;
#167119 = DIRECTION ( 'NONE',  ( 0.000000000000000000, -0.4999999999999689138, -0.8660254037844565822 ) ) ;
#167120 = ORIENTED_EDGE ( 'NONE', *, *, #67982, .T. ) ;
#167121 = EDGE_CURVE ( 'NONE', #145277, #77509, #25854, .T. ) ;
#167122 = DIRECTION ( 'NONE',  ( 1.000000000000000000, 0.000000000000000000, 0.000000000000000000 ) ) ;
#167123 = LINE ( 'NONE', #66712, #48411 ) ;
#167124 = DIRECTION ( 'NONE',  ( -0.000000000000000000, 0.1350103645451626311, 0.9908441862701635738 ) ) ;
#167125 = ORIENTED_EDGE ( 'NONE', *, *, #240476, .T. ) ;
#167126 = AXIS2_PLACEMENT_3D ( 'NONE', #32415, #108074, #111938 ) ;
#167127 = EDGE_CURVE ( 'NONE', #203294, #104543, #101613, .T. ) ;
#167128 = PLANE ( 'NONE',  #78681 ) ;
#167129 = CARTESIAN_POINT ( 'NONE',  ( -21.05000000000000071, 65.63226930301911466, -242.1330134503736247 ) ) ;
#167130 = CARTESIAN_POINT ( 'NONE',  ( -21.04999999999999716, -0.08574093702224822033, -161.0861737111870013 ) ) ;
#167131 = AXIS2_PLACEMENT_3D ( 'NONE', #218327, #200077, #61854 ) ;
#167132 = EDGE_CURVE ( 'NONE', #71001, #18309, #135191, .T. ) ;
#167133 = DIRECTION ( 'NONE',  ( 0.000000000000000000, -6.982962677686266711E-15, 1.000000000000000000 ) ) ;
#167134 = EDGE_CURVE ( 'NONE', #208162, #207792, #122518, .T. ) ;
#167135 = CARTESIAN_POINT ( 'NONE',  ( 23.15000000000000213, 87.48912529308779540, -72.62310748452422615 ) ) ;
#167136 = DIRECTION ( 'NONE',  ( 1.000000000000000000, 0.000000000000000000, 0.000000000000000000 ) ) ;
#167138 = DIRECTION ( 'NONE',  ( 0.000000000000000000, 0.000000000000000000, 1.000000000000000000 ) ) ;
#167137 = CIRCLE ( 'NONE', #13172, 0.09999999999998898659 ) ;
#167139 = EDGE_LOOP ( 'NONE', ( #48455, #7100, #8527, #51047 ) ) ;
#167142 = EDGE_CURVE ( 'NONE', #22985, #43643, #15284, .T. ) ;
#167141 = CARTESIAN_POINT ( 'NONE',  ( -22.44366136229477249, 75.99065843052669322, -215.1728260419982917 ) ) ;
#167140 = SPHERICAL_SURFACE ( 'NONE', #207514, 0.1000000000000000056 ) ;
#167143 = EDGE_LOOP ( 'NONE', ( #93886, #166649, #8419, #80263 ) ) ;
#167145 = VERTEX_POINT ( 'NONE', #89650 ) ;
#167144 = DIRECTION ( 'NONE',  ( 0.9880948137434723000, -0.1538461538461484146, -1.074301950413233906E-15 ) ) ;
#167146 = ORIENTED_EDGE ( 'NONE', *, *, #23480, .F. ) ;
#167147 = DIRECTION ( 'NONE',  ( 0.000000000000000000, -0.8700118002898357128, 0.4930308989875171188 ) ) ;
#167148 = VECTOR ( 'NONE', #218292, 1000.000000000000227 ) ;
#167149 = CARTESIAN_POINT ( 'NONE',  ( -18.59999999999999787, -1.835859311432484375, -212.5044391687984842 ) ) ;
#167150 = DIRECTION ( 'NONE',  ( 1.000000000000000000, 0.000000000000000000, 0.000000000000000000 ) ) ;
#167151 = EDGE_CURVE ( 'NONE', #167521, #117799, #252578, .T. ) ;
#167152 = CIRCLE ( 'NONE', #171428, 0.2000000000000057288 ) ;
#167153 = ORIENTED_EDGE ( 'NONE', *, *, #92629, .T. ) ;
#167154 = CARTESIAN_POINT ( 'NONE',  ( -21.44999999999999929, 7.250000000011155521, -54.65000000000000568 ) ) ;
#167155 = CARTESIAN_POINT ( 'NONE',  ( 18.49999999999999289, 10.37342005529114886, -158.7657881246250895 ) ) ;
#167156 = ORIENTED_EDGE ( 'NONE', *, *, #32886, .T. ) ;
#167157 = VECTOR ( 'NONE', #201264, 1000.000000000000000 ) ;
#167158 = FACE_OUTER_BOUND ( 'NONE', #9394, .T. ) ;
#167159 = DIRECTION ( 'NONE',  ( -1.000000000000000000, 0.000000000000000000, 0.000000000000000000 ) ) ;
#167160 = AXIS2_PLACEMENT_3D ( 'NONE', #185086, #6439, #88528 ) ;
#167161 = ORIENTED_EDGE ( 'NONE', *, *, #152020, .F. ) ;
#167162 = FACE_OUTER_BOUND ( 'NONE', #243635, .T. ) ;
#167163 = VECTOR ( 'NONE', #87275, 1000.000000000000000 ) ;
#167164 = ADVANCED_FACE ( 'NONE', ( #212198 ), #10134, .T. ) ;
#167165 = ORIENTED_EDGE ( 'NONE', *, *, #35478, .F. ) ;
#167166 = DIRECTION ( 'NONE',  ( 0.000000000000000000, -0.9126074666063771490, -0.4088369013363281623 ) ) ;
#167167 = EDGE_LOOP ( 'NONE', ( #218565, #83676, #127774, #156569 ) ) ;
#167168 = CARTESIAN_POINT ( 'NONE',  ( 18.49999999999999289, 10.20857864377385127, -122.2500000000000284 ) ) ;
#167169 = AXIS2_PLACEMENT_3D ( 'NONE', #72458, #189826, #247215 ) ;
#167170 = EDGE_CURVE ( 'NONE', #68348, #75696, #189144, .T. ) ;
#167171 = CARTESIAN_POINT ( 'NONE',  ( 20.96077737575347300, 64.37609936600699712, -76.38231552741797259 ) ) ;
#167172 = CARTESIAN_POINT ( 'NONE',  ( 21.05000000000000071, 75.90220970870291239, -75.78092209500044873 ) ) ;
#167173 = EDGE_CURVE ( 'NONE', #154279, #152534, #255722, .T. ) ;
#167174 = TOROIDAL_SURFACE ( 'NONE', #196169, 0.6000000000000006439, 0.1000000000000000056 ) ;
#167175 = DIRECTION ( 'NONE',  ( 0.000000000000000000, -0.1568667991644355497, -0.9876197685951332295 ) ) ;
#167176 = EDGE_CURVE ( 'NONE', #140280, #225193, #35240, .T. ) ;
#167177 = DIRECTION ( 'NONE',  ( 0.000000000000000000, 0.000000000000000000, -1.000000000000000000 ) ) ;
#167178 = CARTESIAN_POINT ( 'NONE',  ( -19.99999999999999645, 4.645987002755569861, 21.91686199900910736 ) ) ;
#167179 = CIRCLE ( 'NONE', #154696, 0.09999999999999939493 ) ;
#167181 = CARTESIAN_POINT ( 'NONE',  ( 20.94999999999999929, 10.29270135741298731, -72.45736188715193293 ) ) ;
#167180 = CIRCLE ( 'NONE', #204554, 0.09999999999999939493 ) ;
#167182 = AXIS2_PLACEMENT_3D ( 'NONE', #116671, #196210, #219612 ) ;
#167183 = ORIENTED_EDGE ( 'NONE', *, *, #144288, .T. ) ;
#167185 = CARTESIAN_POINT ( 'NONE',  ( 21.14999999999999858, 64.35000000001228670, -157.8731074845244393 ) ) ;
#167184 = DIRECTION ( 'NONE',  ( 0.000000000000000000, 0.9126074666063770380, 0.4088369013363281068 ) ) ;
#167186 = CIRCLE ( 'NONE', #254418, 1.749999999999998002 ) ;
#167187 = ORIENTED_EDGE ( 'NONE', *, *, #177525, .F. ) ;
#167188 = CARTESIAN_POINT ( 'NONE',  ( -23.25000000000000355, 13.44928205424795564, -207.5377222505711075 ) ) ;
#167189 = CARTESIAN_POINT ( 'NONE',  ( -17.11825945287482753, 60.84284427644114146, -221.0155524357444108 ) ) ;
#167191 = ORIENTED_EDGE ( 'NONE', *, *, #19117, .F. ) ;
#167190 = CARTESIAN_POINT ( 'NONE',  ( -18.33981767444319289, -9.569575789792956755, -207.8191618437251407 ) ) ;
#167193 = ORIENTED_EDGE ( 'NONE', *, *, #233088, .T. ) ;
#167192 = DIRECTION ( 'NONE',  ( 0.000000000000000000, 0.000000000000000000, 1.000000000000000000 ) ) ;
#167194 = CARTESIAN_POINT ( 'NONE',  ( -20.64999999999999858, 84.73084112150753811, -146.1211822035086243 ) ) ;
#167195 = CARTESIAN_POINT ( 'NONE',  ( -18.40000000000000213, 51.03393957836610184, -230.5394855108573040 ) ) ;
#167198 = EDGE_CURVE ( 'NONE', #151746, #116136, #160118, .T. ) ;
#167197 = ORIENTED_EDGE ( 'NONE', *, *, #42809, .T. ) ;
#167196 = DIRECTION ( 'NONE',  ( 1.476360405086644309E-16, 1.000000000000000000, 1.445602896647339410E-16 ) ) ;
#167199 = ORIENTED_EDGE ( 'NONE', *, *, #5267, .T. ) ;
#167200 = EDGE_CURVE ( 'NONE', #136324, #180198, #193916, .T. ) ;
#167201 = CARTESIAN_POINT ( 'NONE',  ( 21.03670563405603033, 10.62482368933940258, -179.8255468862091959 ) ) ;
#167202 = DIRECTION ( 'NONE',  ( 0.000000000000000000, -0.9999631594459057471, 0.008583690987121077309 ) ) ;
#167203 = ORIENTED_EDGE ( 'NONE', *, *, #142242, .F. ) ;
#167204 = CARTESIAN_POINT ( 'NONE',  ( 21.14999999999999503, 64.35000000001267040, -203.4231074845244507 ) ) ;
#167205 = VERTEX_POINT ( 'NONE', #191366 ) ;
#167206 = EDGE_CURVE ( 'NONE', #41950, #89935, #80964, .T. ) ;
#167207 = DIRECTION ( 'NONE',  ( 1.000000000000000000, 0.000000000000000000, 0.000000000000000000 ) ) ;
#167208 = DIRECTION ( 'NONE',  ( 1.000000000000000000, 0.000000000000000000, 0.000000000000000000 ) ) ;
#167209 = ORIENTED_EDGE ( 'NONE', *, *, #42533, .T. ) ;
#167210 = CARTESIAN_POINT ( 'NONE',  ( -18.59999999999999787, 77.16270174994961906, -61.42310748452431568 ) ) ;
#167211 = CIRCLE ( 'NONE', #21452, 0.1000000000000002554 ) ;
#167212 = EDGE_CURVE ( 'NONE', #138584, #203751, #151753, .T. ) ;
#167213 = DIRECTION ( 'NONE',  ( 1.000000000000000000, 0.000000000000000000, 0.000000000000000000 ) ) ;
#167214 = EDGE_CURVE ( 'NONE', #24890, #133820, #97515, .T. ) ;
#167215 = ORIENTED_EDGE ( 'NONE', *, *, #35282, .F. ) ;
#167216 = CARTESIAN_POINT ( 'NONE',  ( -21.45000000000000284, 7.708578643773852157, -45.85000000000000142 ) ) ;
#167217 = ADVANCED_FACE ( 'NONE', ( #149663 ), #253856, .F. ) ;
#167219 = ORIENTED_EDGE ( 'NONE', *, *, #182391, .T. ) ;
#167218 = AXIS2_PLACEMENT_3D ( 'NONE', #64378, #103474, #205144 ) ;
#167220 = ORIENTED_EDGE ( 'NONE', *, *, #87222, .F. ) ;
#167222 = EDGE_CURVE ( 'NONE', #46071, #52417, #222416, .T. ) ;
#167221 = FACE_OUTER_BOUND ( 'NONE', #202621, .T. ) ;
#167223 = ORIENTED_EDGE ( 'NONE', *, *, #28530, .F. ) ;
#167224 = VERTEX_POINT ( 'NONE', #210897 ) ;
#167226 = ORIENTED_EDGE ( 'NONE', *, *, #121762, .T. ) ;
#167225 = DIRECTION ( 'NONE',  ( 2.952720810173289112E-16, 1.000000000000000000, 6.982962677686266711E-15 ) ) ;
#167227 = DIRECTION ( 'NONE',  ( 1.713247197920696616E-14, 0.9983803033886531342, 0.05689261644169053833 ) ) ;
#167228 = VERTEX_POINT ( 'NONE', #32288 ) ;
#167229 = CARTESIAN_POINT ( 'NONE',  ( 20.94999999999999929, 63.62814136979439184, -224.4990371885399441 ) ) ;
#167230 = ORIENTED_EDGE ( 'NONE', *, *, #233542, .T. ) ;
#167233 = ORIENTED_EDGE ( 'NONE', *, *, #183217, .F. ) ;
#167232 = ORIENTED_EDGE ( 'NONE', *, *, #231383, .F. ) ;
#167231 = CARTESIAN_POINT ( 'NONE',  ( 21.05000000000000071, 7.128833340094563376, -233.7327013124401276 ) ) ;
#167234 = DIRECTION ( 'NONE',  ( 0.000000000000000000, 0.000000000000000000, -1.000000000000000000 ) ) ;
#167235 = CARTESIAN_POINT ( 'NONE',  ( 20.99999999999999645, 66.25000000001256240, -182.6731074845244223 ) ) ;
#167236 = AXIS2_PLACEMENT_3D ( 'NONE', #118920, #198434, #99312 ) ;
#167237 = ORIENTED_EDGE ( 'NONE', *, *, #242805, .T. ) ;
#167238 = EDGE_CURVE ( 'NONE', #119881, #131987, #210085, .T. ) ;
#167239 = EDGE_CURVE ( 'NONE', #210898, #187411, #66887, .T. ) ;
#167240 = CIRCLE ( 'NONE', #71556, 11.80000000000000426 ) ;
#167241 = B_SPLINE_CURVE_WITH_KNOTS ( 'NONE', 3,
 ( #149858, #213664, #130261, #71607, #229389, #35068, #209820, #151135 ),
 .UNSPECIFIED., .F., .F.,
 ( 4, 2, 2, 4 ),
 ( 0.000000000000000000, 9.550056980125525518E-05, 0.0001910011396025105104, 0.0003820022792049782489 ),
 .UNSPECIFIED. ) ;
#167242 = EDGE_LOOP ( 'NONE', ( #59974, #203623, #71415 ) ) ;
#167243 = CARTESIAN_POINT ( 'NONE',  ( 5.900000000000061640, 64.75000000001119815, -22.12310748452479103 ) ) ;
#167244 = DIRECTION ( 'NONE',  ( 0.000000000000000000, -0.5000000000000144329, -0.8660254037844302699 ) ) ;
#167246 = VERTEX_POINT ( 'NONE', #195216 ) ;
#167245 = LINE ( 'NONE', #47241, #11713 ) ;
#167247 = LINE ( 'NONE', #126802, #177295 ) ;
#167248 = ORIENTED_EDGE ( 'NONE', *, *, #197824, .T. ) ;
#167249 = DIRECTION ( 'NONE',  ( 1.000000000000000000, 0.000000000000000000, 0.000000000000000000 ) ) ;
#167250 = DIRECTION ( 'NONE',  ( -1.000000000000000000, -0.000000000000000000, -0.000000000000000000 ) ) ;
#167251 = ORIENTED_EDGE ( 'NONE', *, *, #3065, .T. ) ;
#167253 = ADVANCED_FACE ( 'NONE', ( #239453 ), #118217, .T. ) ;
#167252 = CARTESIAN_POINT ( 'NONE',  ( 18.50000000000000000, 85.40000000001160174, -62.22584772486096227 ) ) ;
#167254 = DIRECTION ( 'NONE',  ( -0.000000000000000000, 0.9875055080513808203, -0.1575844902526395142 ) ) ;
#167255 = AXIS2_PLACEMENT_3D ( 'NONE', #40101, #20526, #98714 ) ;
#167256 = VERTEX_POINT ( 'NONE', #799 ) ;
#167257 = EDGE_CURVE ( 'NONE', #62787, #57087, #37413, .T. ) ;
#167259 = ORIENTED_EDGE ( 'NONE', *, *, #257013, .F. ) ;
#167258 = CARTESIAN_POINT ( 'NONE',  ( -16.97683809663752186, 66.05000000001257376, -183.4254715027207681 ) ) ;
#167260 = DIRECTION ( 'NONE',  ( 0.000000000000000000, 0.000000000000000000, 1.000000000000000000 ) ) ;
#167262 = ORIENTED_EDGE ( 'NONE', *, *, #153159, .T. ) ;
#167261 = ORIENTED_EDGE ( 'NONE', *, *, #125653, .F. ) ;
#167263 = ORIENTED_EDGE ( 'NONE', *, *, #242159, .F. ) ;
#167264 = DIRECTION ( 'NONE',  ( 0.000000000000000000, 0.000000000000000000, -1.000000000000000000 ) ) ;
#167265 = ORIENTED_EDGE ( 'NONE', *, *, #217282, .F. ) ;
#167266 = DIRECTION ( 'NONE',  ( 1.000000000000000000, 0.000000000000000000, 0.000000000000000000 ) ) ;
#167267 = ORIENTED_EDGE ( 'NONE', *, *, #133328, .F. ) ;
#167268 = EDGE_CURVE ( 'NONE', #247975, #214743, #68344, .T. ) ;
#167269 = CARTESIAN_POINT ( 'NONE',  ( 21.00000000000000000, 5.021051876504148371E-16, 4.100000000000000533 ) ) ;
#167270 = DIRECTION ( 'NONE',  ( 0.000000000000000000, -8.717686153663073805E-15, 1.000000000000000000 ) ) ;
#167271 = ORIENTED_EDGE ( 'NONE', *, *, #240851, .F. ) ;
#167272 = CIRCLE ( 'NONE', #54794, 0.1000000000000021289 ) ;
#167273 = AXIS2_PLACEMENT_3D ( 'NONE', #228578, #49922, #186892 ) ;
#167274 = EDGE_LOOP ( 'NONE', ( #182066, #237197, #43393, #255998 ) ) ;
#167275 = VECTOR ( 'NONE', #6023, 1000.000000000000114 ) ;
#167276 = EDGE_CURVE ( 'NONE', #172562, #2694, #226820, .T. ) ;
#167277 = ORIENTED_EDGE ( 'NONE', *, *, #257941, .F. ) ;
#167278 = CARTESIAN_POINT ( 'NONE',  ( -22.50000000000000000, 11.36146383068193444, -198.4232501820394816 ) ) ;
#167279 = ORIENTED_EDGE ( 'NONE', *, *, #137294, .F. ) ;
#167280 = FACE_OUTER_BOUND ( 'NONE', #194829, .T. ) ;
#167281 = EDGE_CURVE ( 'NONE', #157564, #59508, #30948, .T. ) ;
#167283 = EDGE_LOOP ( 'NONE', ( #32051, #88800 ) ) ;
#167282 = DIRECTION ( 'NONE',  ( 0.000000000000000000, 7.056502275159890832E-15, -1.000000000000000000 ) ) ;
#167284 = CARTESIAN_POINT ( 'NONE',  ( 23.14999999999999858, 3.220451093833237355, -234.5839052933455378 ) ) ;
#167285 = CARTESIAN_POINT ( 'NONE',  ( 23.14999999999999147, 76.00000000001195133, -103.0231074845243171 ) ) ;
#167286 = CARTESIAN_POINT ( 'NONE',  ( 21.14999999999999858, 65.28660755661240955, -157.6731074845244223 ) ) ;
#167287 = AXIS2_PLACEMENT_3D ( 'NONE', #91050, #233155, #54480 ) ;
#167288 = CARTESIAN_POINT ( 'NONE',  ( -18.50000000000000711, 85.41920341803927386, -196.2753216740956077 ) ) ;
#167290 = DIRECTION ( 'NONE',  ( -0.000000000000000000, 0.2617529984165031243, 0.9651348961777157509 ) ) ;
#167289 = DIRECTION ( 'NONE',  ( -1.000000000000000000, 0.000000000000000000, 0.000000000000000000 ) ) ;
#167291 = CARTESIAN_POINT ( 'NONE',  ( -21.05000000000000071, 11.65000000001115588, -93.48519422934610645 ) ) ;
#167292 = CARTESIAN_POINT ( 'NONE',  ( -23.25000000000000000, 68.97833521811233481, -166.1895420826271277 ) ) ;
#167293 = CARTESIAN_POINT ( 'NONE',  ( 18.59999999999999787, 0.6656436123793491033, -212.6810495496487476 ) ) ;
#167294 = EDGE_LOOP ( 'NONE', ( #111034, #151065, #187074, #242229 ) ) ;
#167295 = VERTEX_POINT ( 'NONE', #39997 ) ;
#167297 = ORIENTED_EDGE ( 'NONE', *, *, #9540, .T. ) ;
#167296 = DIRECTION ( 'NONE',  ( 1.073024830501117725E-15, 0.000000000000000000, 1.000000000000000000 ) ) ;
#167298 = ORIENTED_EDGE ( 'NONE', *, *, #247209, .T. ) ;
#167299 = CARTESIAN_POINT ( 'NONE',  ( -18.44085059012131822, 64.48598750652809031, -93.76341280364593445 ) ) ;
#167300 = AXIS2_PLACEMENT_3D ( 'NONE', #75818, #73283, #54941 ) ;
#167301 = CARTESIAN_POINT ( 'NONE',  ( 20.30531438145591139, 10.09690106110208596, -141.7960178072733584 ) ) ;
#167302 = DIRECTION ( 'NONE',  ( 0.000000000000000000, -0.9126074666063770380, -0.4088369013363281068 ) ) ;
#167303 = ORIENTED_EDGE ( 'NONE', *, *, #187633, .T. ) ;
#167304 = AXIS2_PLACEMENT_3D ( 'NONE', #52172, #33956, #131722 ) ;
#167305 = DIRECTION ( 'NONE',  ( 1.000000000000000000, 0.000000000000000000, 0.000000000000000000 ) ) ;
#167306 = CIRCLE ( 'NONE', #25813, 0.09999999999999363565 ) ;
#167307 = CARTESIAN_POINT ( 'NONE',  ( -18.59999999999999787, 9.783112580922244561, -245.9316685519929422 ) ) ;
#167308 = ORIENTED_EDGE ( 'NONE', *, *, #148300, .T. ) ;
#167309 = CARTESIAN_POINT ( 'NONE',  ( -20.64999999999999858, 53.03738849591485405, -234.3791188517465400 ) ) ;
#167310 = DIRECTION ( 'NONE',  ( 1.000000000000000000, -0.000000000000000000, -0.000000000000000000 ) ) ;
#167311 = AXIS2_PLACEMENT_3D ( 'NONE', #113470, #15695, #76908 ) ;
#167312 = CARTESIAN_POINT ( 'NONE',  ( -23.15000000000000213, 87.75000000001173817, -72.62310748452422615 ) ) ;
#167313 = CARTESIAN_POINT ( 'NONE',  ( -2.995603634470829482E-16, 64.04979281095441479, -250.1555871257962735 ) ) ;
#167314 = AXIS2_PLACEMENT_3D ( 'NONE', #206817, #149434, #50289 ) ;
#167315 = DIRECTION ( 'NONE',  ( 1.000000000000000000, 0.000000000000000000, 0.000000000000000000 ) ) ;
#167317 = EDGE_LOOP ( 'NONE', ( #127175, #201295, #174381, #125491 ) ) ;
#167316 = CARTESIAN_POINT ( 'NONE',  ( -20.89878130938411616, 67.49249915771264341, -195.4369143829851510 ) ) ;
#167318 = DIRECTION ( 'NONE',  ( -1.000000000000000000, 1.186688945009010077E-16, 8.286604613020808509E-31 ) ) ;
#167319 = DIRECTION ( 'NONE',  ( -0.000000000000000000, 0.8127272543711080433, -0.5826443254700077734 ) ) ;
#167320 = DIRECTION ( 'NONE',  ( 0.000000000000000000, 0.000000000000000000, -1.000000000000000000 ) ) ;
#167322 = VECTOR ( 'NONE', #74652, 1000.000000000000000 ) ;
#167321 = DIRECTION ( 'NONE',  ( 0.000000000000000000, -0.9126074666063660468, -0.4088369013363524762 ) ) ;
#167323 = EDGE_LOOP ( 'NONE', ( #3277, #216613, #15140, #220462 ) ) ;
#167324 = CARTESIAN_POINT ( 'NONE',  ( -16.93255653858138388, 66.00154854603513854, -157.4414641165347462 ) ) ;
#167325 = CARTESIAN_POINT ( 'NONE',  ( -23.25000000000000000, 1.115600667400684642E-11, -134.0000000000000284 ) ) ;
#167326 = CIRCLE ( 'NONE', #138242, 11.89999999999999325 ) ;
#167328 = DIRECTION ( 'NONE',  ( 5.421010862427554711E-16, -1.000000000000000000, -3.252606517456533024E-15 ) ) ;
#167327 = DIRECTION ( 'NONE',  ( 0.000000000000000000, 0.000000000000000000, -1.000000000000000000 ) ) ;
#167330 = EDGE_CURVE ( 'NONE', #216617, #197652, #216013, .T. ) ;
#167329 = DIRECTION ( 'NONE',  ( -1.000000000000000000, 0.000000000000000000, 0.000000000000000000 ) ) ;
#167331 = DIRECTION ( 'NONE',  ( -1.000000000000000000, -3.265361837132813093E-16, 0.000000000000000000 ) ) ;
#167333 = CARTESIAN_POINT ( 'NONE',  ( -20.94999999999999929, -11.48912529307605901, -3.100000000000000533 ) ) ;
#167332 = CIRCLE ( 'NONE', #200628, 0.1000000000000028644 ) ;
#167334 = CARTESIAN_POINT ( 'NONE',  ( -23.25000000000000355, 11.75000000001113953, -42.75000000000000000 ) ) ;
#167335 = DIRECTION ( 'NONE',  ( -0.000000000000000000, 1.000000000000000000, 6.982962677686266711E-15 ) ) ;
#167336 = DIRECTION ( 'NONE',  ( -0.000000000000000000, -0.4088369013363281068, 0.9126074666063770380 ) ) ;
#167337 = AXIS2_PLACEMENT_3D ( 'NONE', #36013, #155971, #38566 ) ;
#167338 = ORIENTED_EDGE ( 'NONE', *, *, #249521, .T. ) ;
#167339 = VERTEX_POINT ( 'NONE', #236870 ) ;
#167340 = VECTOR ( 'NONE', #66014, 1000.000000000000000 ) ;
#167341 = VERTEX_POINT ( 'NONE', #19110 ) ;
#167342 = CARTESIAN_POINT ( 'NONE',  ( 21.14999999999999858, -1.489567864901280680, -194.6304332222954372 ) ) ;
#167343 = CARTESIAN_POINT ( 'NONE',  ( 21.97500000000000497, 9.750000000011153745, -54.75000000000000711 ) ) ;
#167344 = VERTEX_POINT ( 'NONE', #257657 ) ;
#167345 = AXIS2_PLACEMENT_3D ( 'NONE', #241557, #206288, #66778 ) ;
#167346 = EDGE_CURVE ( 'NONE', #77430, #180046, #99897, .T. ) ;
#167347 = ORIENTED_EDGE ( 'NONE', *, *, #92104, .T. ) ;
#167349 = ORIENTED_EDGE ( 'NONE', *, *, #162628, .T. ) ;
#167348 = AXIS2_PLACEMENT_3D ( 'NONE', #115173, #96851, #91756 ) ;
#167350 = FACE_OUTER_BOUND ( 'NONE', #22256, .T. ) ;
#167351 = CIRCLE ( 'NONE', #242141, 0.09999999999999939493 ) ;
#167352 = ORIENTED_EDGE ( 'NONE', *, *, #4415, .T. ) ;
#167353 = VECTOR ( 'NONE', #34659, 1000.000000000000000 ) ;
#167354 = DIRECTION ( 'NONE',  ( 1.000000000000000000, 0.000000000000000000, 0.000000000000000000 ) ) ;
#167356 = DIRECTION ( 'NONE',  ( 0.000000000000000000, 0.000000000000000000, -1.000000000000000000 ) ) ;
#167355 = CIRCLE ( 'NONE', #233960, 7.899999999999990585 ) ;
#167357 = FACE_OUTER_BOUND ( 'NONE', #127395, .T. ) ;
#167358 = CARTESIAN_POINT ( 'NONE',  ( -21.08134388332232589, 1.580643611831310302, -230.6746762463788514 ) ) ;
#167359 = EDGE_CURVE ( 'NONE', #239499, #71039, #164211, .T. ) ;
#167360 = DIRECTION ( 'NONE',  ( 1.000000000000000000, 0.000000000000000000, 0.000000000000000000 ) ) ;
#167361 = EDGE_CURVE ( 'NONE', #134395, #240778, #199039, .T. ) ;
#167362 = DIRECTION ( 'NONE',  ( 0.000000000000000000, 0.000000000000000000, 1.000000000000000000 ) ) ;
#167364 = ORIENTED_EDGE ( 'NONE', *, *, #150414, .T. ) ;
#167363 = CARTESIAN_POINT ( 'NONE',  ( 21.05000000000000071, 44.15903683684982894, -236.5744930507153470 ) ) ;
#167366 = DIRECTION ( 'NONE',  ( 0.000000000000000000, -0.2617529984164506107, -0.9651348961777299618 ) ) ;
#167365 = CARTESIAN_POINT ( 'NONE',  ( 21.05000000000000071, 11.75000000000000355, -26.65839931010293995 ) ) ;
#167367 = DIRECTION ( 'NONE',  ( 1.000000000000000000, -0.000000000000000000, -0.000000000000000000 ) ) ;
#167368 = EDGE_LOOP ( 'NONE', ( #255901, #143056, #140914, #9775 ) ) ;
#167369 = FACE_OUTER_BOUND ( 'NONE', #78430, .T. ) ;
#167371 = ADVANCED_FACE ( 'NONE', ( #238148 ), #59483, .F. ) ;
#167370 = CARTESIAN_POINT ( 'NONE',  ( -14.23072895065543086, 9.455987233623901034, -115.5115311668978961 ) ) ;
#167372 = CARTESIAN_POINT ( 'NONE',  ( 21.05000000000000071, 69.35000000001231513, -160.1792853948412869 ) ) ;
#167373 = ORIENTED_EDGE ( 'NONE', *, *, #200702, .T. ) ;
#167374 = DIRECTION ( 'NONE',  ( 0.000000000000000000, -1.000000000000000000, -6.982962677686265922E-15 ) ) ;
#167375 = EDGE_CURVE ( 'NONE', #5545, #118409, #250900, .T. ) ;
#167376 = CARTESIAN_POINT ( 'NONE',  ( -16.80070461187904840, 66.05000000001183480, -82.17007131368336559 ) ) ;
#167377 = CIRCLE ( 'NONE', #209043, 7.799999999999993605 ) ;
#167378 = ORIENTED_EDGE ( 'NONE', *, *, #61366, .T. ) ;
#167379 = DIRECTION ( 'NONE',  ( 0.000000000000000000, 0.000000000000000000, -1.000000000000000000 ) ) ;
#167380 = CARTESIAN_POINT ( 'NONE',  ( 20.85000000000000142, 14.80545736607782814, -235.9842437978701639 ) ) ;
#167381 = EDGE_CURVE ( 'NONE', #179279, #129546, #255100, .T. ) ;
#167382 = CARTESIAN_POINT ( 'NONE',  ( -23.25000000000000000, 71.85000000001205933, -124.1731074845243228 ) ) ;
#167383 = LINE ( 'NONE', #8294, #249110 ) ;
#167384 = VERTEX_POINT ( 'NONE', #214742 ) ;
#167385 = EDGE_LOOP ( 'NONE', ( #178281, #160169, #158785, #204852 ) ) ;
#167386 = EDGE_CURVE ( 'NONE', #152802, #86042, #218576, .T. ) ;
#167387 = CARTESIAN_POINT ( 'NONE',  ( 21.05000000000000071, -8.999999999988842703, -191.1060308773475072 ) ) ;
#167388 = CARTESIAN_POINT ( 'NONE',  ( 23.24999999999999289, 9.125777775466493935, -211.6520035670780544 ) ) ;
#167389 = SPHERICAL_SURFACE ( 'NONE', #170286, 0.1000000000000000056 ) ;
#167390 = FACE_BOUND ( 'NONE', #25784, .T. ) ;
#167391 = CARTESIAN_POINT ( 'NONE',  ( 21.08134388332232234, 6.334680580529113314, -167.4241810824929360 ) ) ;
#167392 = CARTESIAN_POINT ( 'NONE',  ( 13.77030915526558452, 9.456007326080461795, -51.98863349414676094 ) ) ;
#167393 = CARTESIAN_POINT ( 'NONE',  ( 20.84999999999999432, -1.164121893230052995, -108.4148480855716485 ) ) ;
#167394 = VERTEX_POINT ( 'NONE', #176933 ) ;
#167395 = DIRECTION ( 'NONE',  ( 1.000000000000000000, 0.000000000000000000, 0.000000000000000000 ) ) ;
#167396 = VECTOR ( 'NONE', #147729, 1000.000000000000000 ) ;
#167398 = VERTEX_POINT ( 'NONE', #101162 ) ;
#167397 = FACE_OUTER_BOUND ( 'NONE', #53278, .T. ) ;
#167399 = CARTESIAN_POINT ( 'NONE',  ( 22.39999999999999147, 68.20922040163900135, -170.0231074845244166 ) ) ;
#167400 = DIRECTION ( 'NONE',  ( 0.000000000000000000, 0.000000000000000000, 1.000000000000000000 ) ) ;
#167401 = CARTESIAN_POINT ( 'NONE',  ( -23.15000000000000213, 0.000000000000000000, 0.000000000000000000 ) ) ;
#167402 = CARTESIAN_POINT ( 'NONE',  ( -16.83558968593870020, 66.05000000001207638, -123.8608022969078775 ) ) ;
#167404 = ORIENTED_EDGE ( 'NONE', *, *, #205034, .F. ) ;
#167403 = FACE_OUTER_BOUND ( 'NONE', #154539, .T. ) ;
#167405 = FACE_OUTER_BOUND ( 'NONE', #146949, .T. ) ;
#167406 = CARTESIAN_POINT ( 'NONE',  ( -18.50000972452446035, 65.70673848567030007, -164.5638252334829303 ) ) ;
#167407 = FACE_OUTER_BOUND ( 'NONE', #237744, .T. ) ;
#167408 = CARTESIAN_POINT ( 'NONE',  ( 23.14999999999999503, 64.35000000001275566, -215.2731074845244450 ) ) ;
#167409 = ORIENTED_EDGE ( 'NONE', *, *, #196171, .F. ) ;
#167410 = CARTESIAN_POINT ( 'NONE',  ( -23.25000000000000000, 64.35000000001166143, -69.52310748452440237 ) ) ;
#167411 = CARTESIAN_POINT ( 'NONE',  ( -16.80891096016330977, 66.05000000001201954, -115.6554446772562272 ) ) ;
#167412 = DIRECTION ( 'NONE',  ( 0.000000000000000000, 0.2128009952263604232, -0.9770955615653316162 ) ) ;
#167414 = VECTOR ( 'NONE', #87462, 1000.000000000000000 ) ;
#167413 = LINE ( 'NONE', #246914, #121652 ) ;
#167415 = VERTEX_POINT ( 'NONE', #77784 ) ;
#167417 = AXIS2_PLACEMENT_3D ( 'NONE', #24612, #80680, #258002 ) ;
#167416 = CYLINDRICAL_SURFACE ( 'NONE', #163641, 4.049999999999998046 ) ;
#167418 = VERTEX_POINT ( 'NONE', #217290 ) ;
#167419 = AXIS2_PLACEMENT_3D ( 'NONE', #93012, #170035, #34355 ) ;
#167420 = ADVANCED_FACE ( 'NONE', ( #36129 ), #188551, .T. ) ;
#167421 = LINE ( 'NONE', #171304, #172563 ) ;
#167423 = EDGE_CURVE ( 'NONE', #148456, #255325, #46893, .T. ) ;
#167422 = CARTESIAN_POINT ( 'NONE',  ( -20.94999999999999929, 76.00000000001170974, -69.52310748452431710 ) ) ;
#167424 =( BOUNDED_CURVE ( )  B_SPLINE_CURVE ( 3, ( #17258, #96747, #14710, #75940 ),
 .UNSPECIFIED., .F., .F. ) 
 B_SPLINE_CURVE_WITH_KNOTS ( ( 4, 4 ),
 ( 1.570796326794896558, 3.141592653589793116 ),
 .UNSPECIFIED. ) 
 CURVE ( )  GEOMETRIC_REPRESENTATION_ITEM ( )  RATIONAL_B_SPLINE_CURVE ( ( 1.000000000000000000, 0.8047378541243649375, 0.8047378541243649375, 1.000000000000000000 ) ) 
 REPRESENTATION_ITEM ( '' )  );
#167425 = CARTESIAN_POINT ( 'NONE',  ( -23.25000000000000355, 5.650000000011139001, -188.3499999999999659 ) ) ;
#167426 = EDGE_LOOP ( 'NONE', ( #34307, #85353, #66639, #168537 ) ) ;
#167427 = EDGE_CURVE ( 'NONE', #26051, #5207, #155278, .T. ) ;
#167428 = EDGE_CURVE ( 'NONE', #110088, #194795, #80188, .T. ) ;
#167429 = DIRECTION ( 'NONE',  ( 1.000000000000000000, 0.000000000000000000, 0.000000000000000000 ) ) ;
#167430 = EDGE_CURVE ( 'NONE', #253904, #71080, #184269, .T. ) ;
#167431 = LINE ( 'NONE', #68312, #179026 ) ;
#167432 = CARTESIAN_POINT ( 'NONE',  ( 22.39999999999999503, -0.1008583690987139431, 11.74956712348939192 ) ) ;
#167433 = CARTESIAN_POINT ( 'NONE',  ( -16.77308656112214891, 9.949999999999983302, -20.84980680829769994 ) ) ;
#167434 = ADVANCED_FACE ( 'NONE', ( #63357 ), #182045, .F. ) ;
#167437 = EDGE_CURVE ( 'NONE', #68342, #102259, #9483, .T. ) ;
#167436 = ADVANCED_FACE ( 'NONE', ( #106323 ), #184597, .T. ) ;
#167435 = DIRECTION ( 'NONE',  ( -3.469446951953515108E-14, -1.000000000000000000, 0.000000000000000000 ) ) ;
#167438 = ORIENTED_EDGE ( 'NONE', *, *, #103608, .T. ) ;
#167440 = ORIENTED_EDGE ( 'NONE', *, *, #153482, .F. ) ;
#167439 = CARTESIAN_POINT ( 'NONE',  ( 20.94999999999999929, 10.29270135741298731, -105.9573618871519756 ) ) ;
#167441 = ORIENTED_EDGE ( 'NONE', *, *, #216208, .T. ) ;
#167442 = CARTESIAN_POINT ( 'NONE',  ( -14.00000000000000178, 9.850000000011133849, -50.25000000000000711 ) ) ;
#167443 = EDGE_LOOP ( 'NONE', ( #23192, #255245, #54774, #5376 ) ) ;
#167444 = CARTESIAN_POINT ( 'NONE',  ( -20.65000000000000568, 7.250000000011138646, -154.8500000000000227 ) ) ;
#167445 = CARTESIAN_POINT ( 'NONE',  ( -23.25000000000000000, -11.74999999998884448, -200.9999999999999432 ) ) ;
#167446 = EDGE_CURVE ( 'NONE', #74847, #169204, #127203, .T. ) ;
#167447 = CARTESIAN_POINT ( 'NONE',  ( 21.05000000000000071, 82.09643798151613225, -215.4278993322501208 ) ) ;
#167448 = VERTEX_POINT ( 'NONE', #242006 ) ;
#167449 = FACE_OUTER_BOUND ( 'NONE', #24187, .T. ) ;
#167450 = CARTESIAN_POINT ( 'NONE',  ( -16.86578989773640913, 66.01519019875270544, -48.55844259790215744 ) ) ;
#167451 = CYLINDRICAL_SURFACE ( 'NONE', #48061, 0.1000000000000028644 ) ;
#167452 = ORIENTED_EDGE ( 'NONE', *, *, #67992, .T. ) ;
#167453 = CARTESIAN_POINT ( 'NONE',  ( -20.64999999999999858, 85.00000000001159606, -59.62913836187181715 ) ) ;
#167454 = EDGE_CURVE ( 'NONE', #223317, #140520, #202878, .T. ) ;
#167455 = ORIENTED_EDGE ( 'NONE', *, *, #222109, .F. ) ;
#167456 = AXIS2_PLACEMENT_3D ( 'NONE', #128987, #111997, #188955 ) ;
#167457 = VECTOR ( 'NONE', #133408, 1000.000000000000114 ) ;
#167458 = DIRECTION ( 'NONE',  ( 0.000000000000000000, -1.000000000000000000, 0.000000000000000000 ) ) ;
#167459 = CARTESIAN_POINT ( 'NONE',  ( -18.59999999999999787, -10.64999999999999325, 31.50000000000000000 ) ) ;
#167460 = AXIS2_PLACEMENT_3D ( 'NONE', #250763, #90401, #130818 ) ;
#167461 = EDGE_CURVE ( 'NONE', #164375, #32344, #206736, .T. ) ;
#167462 = EDGE_CURVE ( 'NONE', #106375, #4212, #28125, .T. ) ;
#167463 = ORIENTED_EDGE ( 'NONE', *, *, #119874, .F. ) ;
#167464 = CARTESIAN_POINT ( 'NONE',  ( -18.50000000000000000, 11.75000000001115197, -134.1000000000000227 ) ) ;
#167466 = EDGE_CURVE ( 'NONE', #2598, #48110, #167632, .T. ) ;
#167465 = CARTESIAN_POINT ( 'NONE',  ( -14.45443560709636444, 66.54940788787834549, -121.4669191657159644 ) ) ;
#167467 = CARTESIAN_POINT ( 'NONE',  ( -21.05000000000000071, 74.14897176987119565, -124.8691942151018139 ) ) ;
#167468 = ORIENTED_EDGE ( 'NONE', *, *, #207983, .F. ) ;
#167469 = CARTESIAN_POINT ( 'NONE',  ( -20.54999999999999716, 63.76951449014745066, -212.8986194275075832 ) ) ;
#167470 = ADVANCED_FACE ( 'NONE', ( #102463 ), #183328, .T. ) ;
#167471 = CARTESIAN_POINT ( 'NONE',  ( 20.99749315643150638, 64.25000000001249134, -177.0379132532823974 ) ) ;
#167472 = ADVANCED_FACE ( 'NONE', ( #67221 ), #209397, .F. ) ;
#167473 = EDGE_LOOP ( 'NONE', ( #116608, #87975, #22152, #250621 ) ) ;
#167474 = CIRCLE ( 'NONE', #201332, 0.09999999999999939493 ) ;
#167475 = EDGE_LOOP ( 'NONE', ( #178443, #175928, #3034, #178393 ) ) ;
#167476 = DIRECTION ( 'NONE',  ( 0.000000000000000000, -1.000000000000000000, -6.982962677686266711E-15 ) ) ;
#167477 = ORIENTED_EDGE ( 'NONE', *, *, #65801, .T. ) ;
#167478 = CARTESIAN_POINT ( 'NONE',  ( -16.92209698673681473, 9.950000000011138823, -188.2893644329461438 ) ) ;
#167479 = CARTESIAN_POINT ( 'NONE',  ( -16.85722902420161518, 66.05000000001255955, -182.7886549582941598 ) ) ;
#167480 = AXIS2_PLACEMENT_3D ( 'NONE', #148643, #228174, #129070 ) ;
#167482 = ORIENTED_EDGE ( 'NONE', *, *, #217162, .F. ) ;
#167481 = CARTESIAN_POINT ( 'NONE',  ( 23.14999999999999503, 6.450000000011156587, -55.25000000000004974 ) ) ;
#167483 = CARTESIAN_POINT ( 'NONE',  ( -20.00857864376270001, 9.350000000011156942, -146.3500000000000227 ) ) ;
#167484 = DIRECTION ( 'NONE',  ( 1.000000000000000000, -7.304098846218134667E-16, -5.100424963727256530E-30 ) ) ;
#167485 = CARTESIAN_POINT ( 'NONE',  ( -22.50000000000000000, -2.479040261793999722, -189.6172560698084624 ) ) ;
#167486 = CARTESIAN_POINT ( 'NONE',  ( 21.14999999999999858, 76.00000000001169553, -76.06376443622556849 ) ) ;
#167487 = CARTESIAN_POINT ( 'NONE',  ( 23.14999999999999503, 6.550000000011156231, -54.65000000000000568 ) ) ;
#167488 = AXIS2_PLACEMENT_3D ( 'NONE', #23364, #20781, #220262 ) ;
#167489 = DIRECTION ( 'NONE',  ( 1.000000000000000000, 0.000000000000000000, 0.000000000000000000 ) ) ;
#167490 = CARTESIAN_POINT ( 'NONE',  ( 23.24999999999999645, 71.00000000001199396, -115.4283735034374274 ) ) ;
#167492 = EDGE_LOOP ( 'NONE', ( #223754, #182963, #87584, #80368 ) ) ;
#167491 = PLANE ( 'NONE',  #169372 ) ;
#167493 = CARTESIAN_POINT ( 'NONE',  ( 21.05000000000000071, 55.99424519013661694, -234.9720658648265896 ) ) ;
#167494 = AXIS2_PLACEMENT_3D ( 'NONE', #131577, #129024, #50727 ) ;
#167495 = ORIENTED_EDGE ( 'NONE', *, *, #10904, .F. ) ;
#167496 = AXIS2_PLACEMENT_3D ( 'NONE', #22120, #159068, #174807 ) ;
#167497 = CIRCLE ( 'NONE', #88318, 0.09999999999999134581 ) ;
#167498 = AXIS2_PLACEMENT_3D ( 'NONE', #138153, #1207, #237284 ) ;
#167499 = DIRECTION ( 'NONE',  ( 0.000000000000000000, 0.000000000000000000, -1.000000000000000000 ) ) ;
#167500 = CARTESIAN_POINT ( 'NONE',  ( -20.64999999999999858, 2.000000000011154189, -87.27537807723794572 ) ) ;
#167501 = DIRECTION ( 'NONE',  ( 0.000000000000000000, -1.000000000000000000, 0.000000000000000000 ) ) ;
#167502 = CARTESIAN_POINT ( 'NONE',  ( -5.900000000000002132, -11.75000000000000000, 13.90000000000000213 ) ) ;
#167503 = CIRCLE ( 'NONE', #159138, 0.09999999999999939493 ) ;
#167504 = ORIENTED_EDGE ( 'NONE', *, *, #98597, .T. ) ;
#167505 = CARTESIAN_POINT ( 'NONE',  ( 18.49999999999999289, 39.24721131055453327, -235.5164460677962666 ) ) ;
#167506 = AXIS2_PLACEMENT_3D ( 'NONE', #194327, #212592, #150058 ) ;
#167507 = ADVANCED_FACE ( 'NONE', ( #165043 ), #120244, .T. ) ;
#167508 = CARTESIAN_POINT ( 'NONE',  ( 23.14999999999998792, 12.62988036037870643, -223.4632815780722410 ) ) ;
#167509 = AXIS2_PLACEMENT_3D ( 'NONE', #234160, #39848, #138875 ) ;
#167510 = EDGE_CURVE ( 'NONE', #106852, #163267, #113547, .T. ) ;
#167511 = ORIENTED_EDGE ( 'NONE', *, *, #238565, .T. ) ;
#167512 = CIRCLE ( 'NONE', #192434, 0.09999999999999939493 ) ;
#167513 = CARTESIAN_POINT ( 'NONE',  ( 20.94999999999999574, 18.27574494880468592, -237.6039235467692947 ) ) ;
#167515 =( BOUNDED_SURFACE ( )  B_SPLINE_SURFACE ( 3, 2, ( 
 ( #49474, #186432, #7791 ),
 ( #69059, #45631, #106865 ),
 ( #148584, #26074, #207284 ),
 ( #129023, #28679, #87300 ) ),
 .UNSPECIFIED., .F., .F., .F. ) 
 B_SPLINE_SURFACE_WITH_KNOTS ( ( 4, 4 ),
 ( 3, 3 ),
 ( 0.0006461284895273937097, 0.0007503702773986277094 ),
 ( 0.000000000000000000, 1.000000000000000000 ),
 .UNSPECIFIED. ) 
 GEOMETRIC_REPRESENTATION_ITEM ( )  RATIONAL_B_SPLINE_SURFACE ( (
 ( 1.000000000000000000, 0.7071067811865475727, 1.000000000000000000),
 ( 1.000000000000000000, 0.7076476444648727160, 1.000000000000000000),
 ( 1.000000000000000000, 0.7075727925191928058, 1.000000000000000000),
 ( 1.000000000000000000, 0.7071067811865471286, 1.000000000000000000) ) ) 
 REPRESENTATION_ITEM ( '' )  SURFACE ( )  );
#167514 = CIRCLE ( 'NONE', #117612, 0.1000000000000028644 ) ;
#167516 = CARTESIAN_POINT ( 'NONE',  ( 22.60000000000000142, 0.04781839071596404728, -21.74997758095277334 ) ) ;
#167517 = ADVANCED_FACE ( 'NONE', ( #189743 ), #208040, .F. ) ;
#167518 = ORIENTED_EDGE ( 'NONE', *, *, #53905, .T. ) ;
#167520 = EDGE_CURVE ( 'NONE', #256608, #209103, #112775, .T. ) ;
#167519 = CARTESIAN_POINT ( 'NONE',  ( -16.86422026484316916, 66.02955263915194450, -190.9408942588514151 ) ) ;
#167521 = VERTEX_POINT ( 'NONE', #250978 ) ;
#167523 = VECTOR ( 'NONE', #223466, 1000.000000000000000 ) ;
#167522 = CARTESIAN_POINT ( 'NONE',  ( 21.06089410995835109, 65.27470446788846914, -124.3207267534811677 ) ) ;
#167524 = EDGE_LOOP ( 'NONE', ( #43364, #6795 ) ) ;
#167525 = DIRECTION ( 'NONE',  ( 0.000000000000000000, -1.000000000000000000, -6.982962677686266711E-15 ) ) ;
#167526 = DIRECTION ( 'NONE',  ( -1.000000000000000000, 0.000000000000000000, 0.000000000000000000 ) ) ;
#167527 = ORIENTED_EDGE ( 'NONE', *, *, #73235, .T. ) ;
#167528 = VERTEX_POINT ( 'NONE', #29420 ) ;
#167529 = FACE_OUTER_BOUND ( 'NONE', #71283, .T. ) ;
#167531 = ORIENTED_EDGE ( 'NONE', *, *, #30136, .F. ) ;
#167530 = SURFACE_SIDE_STYLE ('',( #50113 ) ) ;
#167532 = CARTESIAN_POINT ( 'NONE',  ( -20.94999999999999929, 7.128833340094563376, -233.7327013124401276 ) ) ;
#167534 = ORIENTED_EDGE ( 'NONE', *, *, #196255, .T. ) ;
#167533 = AXIS2_PLACEMENT_3D ( 'NONE', #226694, #126313, #32393 ) ;
#167535 = CIRCLE ( 'NONE', #71668, 0.1000000000000028644 ) ;
#167536 = ADVANCED_FACE ( 'NONE', ( #150619 ), #21978, .F. ) ;
#167537 = AXIS2_PLACEMENT_3D ( 'NONE', #6308, #227939, #49295 ) ;
#167538 = EDGE_CURVE ( 'NONE', #194460, #60767, #209297, .T. ) ;
#167539 = ORIENTED_EDGE ( 'NONE', *, *, #206142, .F. ) ;
#167540 = DIRECTION ( 'NONE',  ( 0.000000000000000000, 0.9126074666064696306, 0.4088369013361213278 ) ) ;
#167541 = LINE ( 'NONE', #48841, #142847 ) ;
#167542 = CARTESIAN_POINT ( 'NONE',  ( -20.54999999999999716, 56.74893307810339849, -253.4262823364869064 ) ) ;
#167543 = DIRECTION ( 'NONE',  ( -1.000000000000000000, 0.000000000000000000, 0.000000000000000000 ) ) ;
#167544 = CARTESIAN_POINT ( 'NONE',  ( -12.25000000000000533, 66.65000000001259650, -187.0045385271218379 ) ) ;
#167545 = FACE_OUTER_BOUND ( 'NONE', #231202, .T. ) ;
#167546 = ORIENTED_EDGE ( 'NONE', *, *, #215678, .F. ) ;
#167547 = CARTESIAN_POINT ( 'NONE',  ( -16.91776028072577631, 66.03659960638279358, -182.6480834698222964 ) ) ;
#167549 = EDGE_CURVE ( 'NONE', #150422, #200055, #153218, .T. ) ;
#167548 = CARTESIAN_POINT ( 'NONE',  ( -23.15000000000000213, 71.75000000001259082, -191.2731074845243882 ) ) ;
#167550 = LINE ( 'NONE', #67136, #132767 ) ;
#167551 = CARTESIAN_POINT ( 'NONE',  ( -23.15000000000000213, 71.65000000001207070, -124.2731074845243313 ) ) ;
#167552 = ORIENTED_EDGE ( 'NONE', *, *, #172456, .T. ) ;
#167553 = ADVANCED_FACE ( 'NONE', ( #192315 ), #110191, .T. ) ;
#167555 = CARTESIAN_POINT ( 'NONE',  ( -20.94999999999999929, 4.459011116736869340, -245.2267018908137857 ) ) ;
#167554 = CIRCLE ( 'NONE', #230067, 0.09999999999998898659 ) ;
#167556 = VERTEX_POINT ( 'NONE', #231452 ) ;
#167557 = CARTESIAN_POINT ( 'NONE',  ( 12.60053434924909865, 9.389534562357859215, -116.1748093043900099 ) ) ;
#167558 = EDGE_LOOP ( 'NONE', ( #131011, #104255, #49302, #156380 ) ) ;
#167559 = DIRECTION ( 'NONE',  ( 0.000000000000000000, 0.000000000000000000, 1.000000000000000000 ) ) ;
#167560 = DIRECTION ( 'NONE',  ( 1.000000000000000000, 0.000000000000000000, 0.000000000000000000 ) ) ;
#167561 = ORIENTED_EDGE ( 'NONE', *, *, #181974, .F. ) ;
#167562 = VERTEX_POINT ( 'NONE', #89337 ) ;
#167564 = EDGE_LOOP ( 'NONE', ( #6224, #23898, #192099, #70118 ) ) ;
#167563 = FACE_OUTER_BOUND ( 'NONE', #7081, .T. ) ;
#167565 = CARTESIAN_POINT ( 'NONE',  ( -18.59999999999999787, -1.637172712959223952, -45.08215336547201701 ) ) ;
#167566 = ORIENTED_EDGE ( 'NONE', *, *, #74192, .F. ) ;
#167567 = EDGE_CURVE ( 'NONE', #35976, #150904, #193599, .T. ) ;
#167568 = FACE_OUTER_BOUND ( 'NONE', #136745, .T. ) ;
#167569 = DIRECTION ( 'NONE',  ( 0.000000000000000000, 0.5000000000000078826, 0.8660254037844340447 ) ) ;
#167570 = EDGE_CURVE ( 'NONE', #163189, #68733, #132328, .T. ) ;
#167571 = ORIENTED_EDGE ( 'NONE', *, *, #175334, .F. ) ;
#167572 = CARTESIAN_POINT ( 'NONE',  ( -21.44999999999999929, 68.85000000001151932, -48.37310748452436826 ) ) ;
#167573 = CARTESIAN_POINT ( 'NONE',  ( 20.94999999999999929, 5.400000000011154988, -57.10603087734755690 ) ) ;
#167574 = EDGE_CURVE ( 'NONE', #47181, #3363, #255141, .T. ) ;
#167575 = ORIENTED_EDGE ( 'NONE', *, *, #104717, .F. ) ;
#167576 = AXIS2_PLACEMENT_3D ( 'NONE', #166149, #245648, #22768 ) ;
#167577 = LINE ( 'NONE', #245808, #226454 ) ;
#167578 = EDGE_CURVE ( 'NONE', #74752, #188576, #109436, .T. ) ;
#167579 = DIRECTION ( 'NONE',  ( 0.000000000000000000, -0.2617529984165152257, -0.9651348961777124202 ) ) ;
#167581 = VERTEX_POINT ( 'NONE', #108911 ) ;
#167580 = DIRECTION ( 'NONE',  ( 0.000000000000000000, 0.9126074666063660468, 0.4088369013363524762 ) ) ;
#167582 = DIRECTION ( 'NONE',  ( 0.000000000000000000, 0.9968797965484670343, 0.07893460099023182075 ) ) ;
#167583 = CARTESIAN_POINT ( 'NONE',  ( -22.59080734064477625, 11.75000000001115907, -133.9692502919030233 ) ) ;
#167584 = CARTESIAN_POINT ( 'NONE',  ( -16.92570016628983254, 9.958788957751014692, -121.3793493299610446 ) ) ;
#167585 = EDGE_CURVE ( 'NONE', #55890, #118463, #34470, .T. ) ;
#167587 = CARTESIAN_POINT ( 'NONE',  ( -23.25000000000000000, 1.115600667400684642E-11, -134.0000000000000000 ) ) ;
#167586 = CARTESIAN_POINT ( 'NONE',  ( 23.40000000000004476, 84.00000000001119815, -34.86056257560453986 ) ) ;
#167588 = CARTESIAN_POINT ( 'NONE',  ( 23.14999999999999503, 6.649999999999999467, -12.15000000000000036 ) ) ;
#167589 = DIRECTION ( 'NONE',  ( 1.000000000000000000, 0.000000000000000000, 0.000000000000000000 ) ) ;
#167590 = CIRCLE ( 'NONE', #55111, 0.1999999999999987899 ) ;
#167591 = DIRECTION ( 'NONE',  ( 0.000000000000000000, 0.2617529984165031243, 0.9651348961777157509 ) ) ;
#167592 = DIRECTION ( 'NONE',  ( -1.000000000000000000, -0.000000000000000000, -0.000000000000000000 ) ) ;
#167593 = AXIS2_PLACEMENT_3D ( 'NONE', #205924, #160416, #239936 ) ;
#167594 = VERTEX_POINT ( 'NONE', #188451 ) ;
#167596 = ORIENTED_EDGE ( 'NONE', *, *, #29137, .T. ) ;
#167595 = AXIS2_PLACEMENT_3D ( 'NONE', #117275, #57267, #238495 ) ;
#167597 = ORIENTED_EDGE ( 'NONE', *, *, #17504, .T. ) ;
#167598 = CARTESIAN_POINT ( 'NONE',  ( -20.94560253601877164, 64.25000000001220712, -143.5130239720093925 ) ) ;
#167599 = CARTESIAN_POINT ( 'NONE',  ( 21.05000000000000071, -9.499999999988844479, -191.1060308773475072 ) ) ;
#167600 = ORIENTED_EDGE ( 'NONE', *, *, #241486, .T. ) ;
#167601 = AXIS2_PLACEMENT_3D ( 'NONE', #86716, #8503, #68474 ) ;
#167602 = AXIS2_PLACEMENT_3D ( 'NONE', #247684, #78019, #58438 ) ;
#167603 = DIRECTION ( 'NONE',  ( 0.000000000000000000, 1.000000000000000000, 0.000000000000000000 ) ) ;
#167604 = CARTESIAN_POINT ( 'NONE',  ( 20.85882249326303040, 10.33248238083634796, -206.5948465439131496 ) ) ;
#167605 = DIRECTION ( 'NONE',  ( 1.186688945009010077E-16, -1.000000000000000000, -0.000000000000000000 ) ) ;
#167606 = ORIENTED_EDGE ( 'NONE', *, *, #9940, .T. ) ;
#167607 = ORIENTED_EDGE ( 'NONE', *, *, #203822, .F. ) ;
#167608 = CARTESIAN_POINT ( 'NONE',  ( 20.04142135623730070, 11.65000000001115943, -158.6500000000000057 ) ) ;
#167609 = PLANE ( 'NONE',  #71850 ) ;
#167610 = ORIENTED_EDGE ( 'NONE', *, *, #99079, .T. ) ;
#167611 = AXIS2_PLACEMENT_3D ( 'NONE', #233240, #170729, #194110 ) ;
#167612 = CARTESIAN_POINT ( 'NONE',  ( -23.39999999999994529, 79.88763423575340994, -7.282924647898262549 ) ) ;
#167614 = EDGE_LOOP ( 'NONE', ( #37575, #41672, #27639, #84124 ) ) ;
#167613 = DIRECTION ( 'NONE',  ( 1.000000000000000000, 1.541880601228652843E-16, 2.878400969107353907E-16 ) ) ;
#167615 = CARTESIAN_POINT ( 'NONE',  ( 23.24999999999999289, 11.75000000001116263, -21.75000000000000355 ) ) ;
#167616 = CARTESIAN_POINT ( 'NONE',  ( -20.94999999999999929, 64.35000000001191722, -103.0231074845243882 ) ) ;
#167618 = ORIENTED_EDGE ( 'NONE', *, *, #47881, .F. ) ;
#167617 = CARTESIAN_POINT ( 'NONE',  ( 21.05000000000000071, 71.00000000001205080, -124.1178414656112352 ) ) ;
#167619 = AXIS2_PLACEMENT_3D ( 'NONE', #68581, #148116, #127266 ) ;
#167620 = CARTESIAN_POINT ( 'NONE',  ( 21.14999999999999858, 8.786607556611267356, -146.3500000000000227 ) ) ;
#167622 = CARTESIAN_POINT ( 'NONE',  ( 21.05000000000000071, 64.40000000001218439, -143.4513107147999165 ) ) ;
#167621 = VECTOR ( 'NONE', #119694, 1000.000000000000000 ) ;
#167623 = AXIS2_PLACEMENT_3D ( 'NONE', #126670, #187939, #32748 ) ;
#167624 = CARTESIAN_POINT ( 'NONE',  ( 18.50000000000000000, 85.50000000001263345, -196.4910380878246201 ) ) ;
#167625 = CARTESIAN_POINT ( 'NONE',  ( -16.94225986326250677, 12.47717560563228822, -211.5328121362375953 ) ) ;
#167626 = VECTOR ( 'NONE', #158137, 1000.000000000000000 ) ;
#167628 = CARTESIAN_POINT ( 'NONE',  ( 21.06086055315971350, 8.774707514967413857, -179.7023221551538938 ) ) ;
#167627 = DIRECTION ( 'NONE',  ( 0.000000000000000000, -1.000000000000000000, -6.982962677686266711E-15 ) ) ;
#167629 = CARTESIAN_POINT ( 'NONE',  ( 21.14999999999999858, 11.65000000001115943, -134.1000000000000227 ) ) ;
#167630 = FACE_OUTER_BOUND ( 'NONE', #3707, .T. ) ;
#167631 = CARTESIAN_POINT ( 'NONE',  ( -20.54999999999999716, 76.00000000001267608, -203.5231074845243597 ) ) ;
#167632 = LINE ( 'NONE', #103753, #213496 ) ;
#167633 = ORIENTED_EDGE ( 'NONE', *, *, #232511, .T. ) ;
#167634 = ORIENTED_EDGE ( 'NONE', *, *, #53518, .T. ) ;
#167635 = EDGE_LOOP ( 'NONE', ( #190672, #120438, #214621, #70261 ) ) ;
#167636 = DIRECTION ( 'NONE',  ( 1.000000000000000000, 0.000000000000000000, 0.000000000000000000 ) ) ;
#167637 = ORIENTED_EDGE ( 'NONE', *, *, #39485, .F. ) ;
#167638 = DIRECTION ( 'NONE',  ( 0.000000000000000000, -1.000000000000000000, -6.352154140967427193E-15 ) ) ;
#167639 = EDGE_LOOP ( 'NONE', ( #163965, #40384, #111165, #132429, #246775, #58535, #43937, #14476, #29711, #158177, #27718 ) ) ;
#167640 = CARTESIAN_POINT ( 'NONE',  ( 20.12500000000000000, 30.37633856152204359, -235.1250019192171408 ) ) ;
#167641 = ADVANCED_FACE ( 'NONE', ( #210588 ), #128485, .T. ) ;
#167642 = DIRECTION ( 'NONE',  ( 1.000000000000000000, 0.000000000000000000, 0.000000000000000000 ) ) ;
#167643 = ADVANCED_FACE ( 'NONE', ( #174075 ), #91913, .F. ) ;
#167644 = ADVANCED_FACE ( 'NONE', ( #211890 ), #114039, .F. ) ;
#167645 = ORIENTED_EDGE ( 'NONE', *, *, #83706, .F. ) ;
#167646 = DIRECTION ( 'NONE',  ( 0.000000000000000000, -0.8777080977375715243, 0.4791956752370512551 ) ) ;
#167647 = FILL_AREA_STYLE ('',( #127218 ) ) ;
#167648 = AXIS2_PLACEMENT_3D ( 'NONE', #159448, #2910, #79866 ) ;
#167649 = VECTOR ( 'NONE', #44444, 1000.000000000000000 ) ;
#167650 = ORIENTED_EDGE ( 'NONE', *, *, #103644, .T. ) ;
#167651 = ORIENTED_EDGE ( 'NONE', *, *, #233229, .F. ) ;
#167652 = ORIENTED_EDGE ( 'NONE', *, *, #235089, .F. ) ;
#167653 = CARTESIAN_POINT ( 'NONE',  ( -18.50000000000000000, 30.14024212288317628, -235.5657495473015501 ) ) ;
#167654 = SURFACE_STYLE_USAGE ( .BOTH. , #65965 ) ;
#167655 = LINE ( 'NONE', #171517, #117595 ) ;
#167656 = FACE_BOUND ( 'NONE', #216738, .T. ) ;
#167657 = DIRECTION ( 'NONE',  ( 0.000000000000000000, 0.1298341882519953583, 0.9915357197604862671 ) ) ;
#167658 = EDGE_CURVE ( 'NONE', #5646, #105369, #84450, .T. ) ;
#167659 = AXIS2_PLACEMENT_3D ( 'NONE', #174021, #93141, #253497 ) ;
#167661 = DIRECTION ( 'NONE',  ( 0.000000000000000000, -0.1298341882520022694, -0.9915357197604853789 ) ) ;
#167660 = LINE ( 'NONE', #189767, #16584 ) ;
#167662 = CARTESIAN_POINT ( 'NONE',  ( -14.45443560709636621, 9.450592112144860835, -82.05618831880845221 ) ) ;
#167664 = ORIENTED_EDGE ( 'NONE', *, *, #168008, .F. ) ;
#167663 = DIRECTION ( 'NONE',  ( -1.000000000000000000, 0.000000000000000000, 0.000000000000000000 ) ) ;
#167666 = CARTESIAN_POINT ( 'NONE',  ( 20.93284271247462414, 11.75000000001116085, -126.9851942293461065 ) ) ;
#167665 = CARTESIAN_POINT ( 'NONE',  ( -18.59999999999999787, 74.83729825007388570, -94.92310748452432279 ) ) ;
#167667 = DIRECTION ( 'NONE',  ( -4.336808689941751890E-15, -0.8660254037844445918, -0.4999999999999897304 ) ) ;
#167668 = EDGE_LOOP ( 'NONE', ( #216463, #162323, #82193, #175166 ) ) ;
#167669 = CARTESIAN_POINT ( 'NONE',  ( -20.94999999999999929, 1.115600667400684642E-11, -200.9999999999999432 ) ) ;
#167670 = AXIS2_PLACEMENT_3D ( 'NONE', #144227, #29474, #67276 ) ;
#167671 = CARTESIAN_POINT ( 'NONE',  ( 22.49544290803778424, 64.25012976215489857, -103.0884194437818167 ) ) ;
#167672 = CARTESIAN_POINT ( 'NONE',  ( -20.64999999999999858, 70.60134440767087938, -223.4290147181903308 ) ) ;
#167673 = VERTEX_POINT ( 'NONE', #39368 ) ;
#167674 = TOROIDAL_SURFACE ( 'NONE', #176057, 0.6000000000000009770, 0.1000000000000000056 ) ;
#167676 = CARTESIAN_POINT ( 'NONE',  ( 23.14999999999998437, 1.115600667400684642E-11, -100.5000000000000284 ) ) ;
#167675 = AXIS2_PLACEMENT_3D ( 'NONE', #163075, #165634, #203466 ) ;
#167677 = CIRCLE ( 'NONE', #88513, 0.1000000000000054040 ) ;
#167678 = LINE ( 'NONE', #85508, #60995 ) ;
#167679 = CARTESIAN_POINT ( 'NONE',  ( -21.44999999999999929, 68.65000000001222702, -148.8731074845244109 ) ) ;
#167680 = VECTOR ( 'NONE', #136563, 1000.000000000000000 ) ;
#167681 = ORIENTED_EDGE ( 'NONE', *, *, #130757, .T. ) ;
#167682 = VERTEX_POINT ( 'NONE', #121472 ) ;
#167683 = VECTOR ( 'NONE', #71597, 1000.000000000000000 ) ;
#167684 = CARTESIAN_POINT ( 'NONE',  ( -16.87331047859649757, 51.61886293219124155, -231.9464690156495692 ) ) ;
#167686 = ORIENTED_EDGE ( 'NONE', *, *, #146269, .T. ) ;
#167685 = EDGE_CURVE ( 'NONE', #178841, #99053, #5369, .T. ) ;
#167687 = ADVANCED_FACE ( 'NONE', ( #141018 ), #202266, .T. ) ;
#167688 = CARTESIAN_POINT ( 'NONE',  ( -17.22767730084089166, 65.65075578754372998, -158.6655361750987936 ) ) ;
#167689 = DIRECTION ( 'NONE',  ( -1.836970198721029934E-16, 1.000000000000000000, 0.000000000000000000 ) ) ;
#167690 = CARTESIAN_POINT ( 'NONE',  ( -23.25000000000000000, 70.02906482874161043, -215.6060937950565233 ) ) ;
#167691 = ORIENTED_EDGE ( 'NONE', *, *, #190414, .T. ) ;
#167692 = CIRCLE ( 'NONE', #109202, 0.9000000000000014655 ) ;
#167694 = AXIS2_PLACEMENT_3D ( 'NONE', #207146, #28551, #87169 ) ;
#167693 = CARTESIAN_POINT ( 'NONE',  ( -23.25000000000000000, 1.115600667400684642E-11, -104.4000000000000483 ) ) ;
#167695 = DIRECTION ( 'NONE',  ( -1.000000000000000000, 0.000000000000000000, 0.000000000000000000 ) ) ;
#167696 = EDGE_CURVE ( 'NONE', #115956, #144144, #180202, .T. ) ;
#167697 = CARTESIAN_POINT ( 'NONE',  ( 22.01447462590973814, 0.09903700007069084210, -126.7361997987701017 ) ) ;
#167698 = TOROIDAL_SURFACE ( 'NONE', #196696, 0.2000000000000000111, 0.1000000000000000056 ) ;
#167699 = DIRECTION ( 'NONE',  ( 1.000000000000000000, 3.265361837132813093E-16, -0.000000000000000000 ) ) ;
#167700 = ORIENTED_EDGE ( 'NONE', *, *, #102890, .F. ) ;
#167701 = CARTESIAN_POINT ( 'NONE',  ( -18.39999999999999858, -7.792952876741447987, -209.8605804245960655 ) ) ;
#167702 = CIRCLE ( 'NONE', #163586, 0.2000000000000057288 ) ;
#167703 = TOROIDAL_SURFACE ( 'NONE', #63615, 0.2000000000000000111, 0.1000000000000000056 ) ;
#167705 = ORIENTED_EDGE ( 'NONE', *, *, #163168, .F. ) ;
#167704 = DIRECTION ( 'NONE',  ( 1.000000000000000000, 0.000000000000000000, 0.000000000000000000 ) ) ;
#167706 = DIRECTION ( 'NONE',  ( 1.000000000000000000, 0.000000000000000000, 0.000000000000000000 ) ) ;
#167707 = DIRECTION ( 'NONE',  ( 1.000000000000000000, -0.000000000000000000, -0.000000000000000000 ) ) ;
#167708 = DIRECTION ( 'NONE',  ( 1.000000000000000000, 0.000000000000000000, 0.000000000000000000 ) ) ;
#167709 = VECTOR ( 'NONE', #248410, 1000.000000000000000 ) ;
#167710 = CARTESIAN_POINT ( 'NONE',  ( 23.15000000000000213, -11.48912529307605546, -30.39999999999999503 ) ) ;
#167711 = FACE_OUTER_BOUND ( 'NONE', #240871, .T. ) ;
#167712 = CARTESIAN_POINT ( 'NONE',  ( -20.85000000000000142, 87.75000000001215028, -136.5231074845242745 ) ) ;
#167713 = CARTESIAN_POINT ( 'NONE',  ( 23.14999999999999147, 76.00000000001267608, -203.5231074845243597 ) ) ;
#167714 = ORIENTED_EDGE ( 'NONE', *, *, #77061, .T. ) ;
#167715 = ADVANCED_FACE ( 'NONE', ( #24932 ), #241401, .F. ) ;
#167716 = CARTESIAN_POINT ( 'NONE',  ( -20.64999999999999858, 38.42191493408704872, -250.4955484557988541 ) ) ;
#167717 = DIRECTION ( 'NONE',  ( 0.000000000000000000, -1.000000000000000000, 0.000000000000000000 ) ) ;
#167718 = CARTESIAN_POINT ( 'NONE',  ( -20.90000000000000213, 1.410778198689825347, -7.973296578895943121 ) ) ;
#167719 = DIRECTION ( 'NONE',  ( 0.000000000000000000, 0.000000000000000000, -1.000000000000000000 ) ) ;
#167720 = CARTESIAN_POINT ( 'NONE',  ( 21.14999999999999858, -11.64999999998883595, -100.5000000000000284 ) ) ;
#167721 = CIRCLE ( 'NONE', #146825, 0.1000000000000024342 ) ;
#167722 = AXIS2_PLACEMENT_3D ( 'NONE', #215533, #116450, #17352 ) ;
#167723 = AXIS2_PLACEMENT_3D ( 'NONE', #90671, #234037, #32021 ) ;
#167724 = ORIENTED_EDGE ( 'NONE', *, *, #177675, .T. ) ;
#167725 = VERTEX_POINT ( 'NONE', #200982 ) ;
#167726 = CARTESIAN_POINT ( 'NONE',  ( -20.64999999999999858, -9.499999999988848032, -177.3939691226524076 ) ) ;
#167727 = EDGE_CURVE ( 'NONE', #184131, #195135, #104416, .T. ) ;
#167728 = CARTESIAN_POINT ( 'NONE',  ( -23.15000000000000213, 2.000000000011154189, -53.77537807723790309 ) ) ;
#167730 = EDGE_CURVE ( 'NONE', #46377, #204366, #146458, .T. ) ;
#167729 = DIRECTION ( 'NONE',  ( 1.301042606982683418E-14, -0.8660254037844330455, 0.5000000000000096589 ) ) ;
#167731 = DIRECTION ( 'NONE',  ( 1.000000000000000000, 0.000000000000000000, 0.000000000000000000 ) ) ;
#167732 = ADVANCED_FACE ( 'NONE', ( #19791 ), #86657, .T. ) ;
#167733 = EDGE_CURVE ( 'NONE', #56292, #62202, #38176, .T. ) ;
#167734 = CYLINDRICAL_SURFACE ( 'NONE', #21954, 0.1000000000000028644 ) ;
#167735 = CARTESIAN_POINT ( 'NONE',  ( -20.94999999999999929, 2.923777413779037548, -208.5507632484912222 ) ) ;
#167736 = CARTESIAN_POINT ( 'NONE',  ( -16.94445028196808778, 9.992063609697733995, -12.60733017841845438 ) ) ;
#167737 = EDGE_CURVE ( 'NONE', #256663, #43421, #126181, .T. ) ;
#167738 = ADVANCED_FACE ( 'NONE', ( #44486 ), #4796, .T. ) ;
#167739 = ORIENTED_EDGE ( 'NONE', *, *, #87299, .F. ) ;
#167740 = CARTESIAN_POINT ( 'NONE',  ( -18.58671080940899145, 85.40693285883820352, -62.39895301961955454 ) ) ;
#167741 = AXIS2_PLACEMENT_3D ( 'NONE', #62833, #182804, #144918 ) ;
#167742 = ORIENTED_EDGE ( 'NONE', *, *, #209811, .T. ) ;
#167743 = DIRECTION ( 'NONE',  ( -0.000000000000000000, 0.8164390028469705740, -0.5774316882803059992 ) ) ;
#167744 = DIRECTION ( 'NONE',  ( 0.000000000000000000, -0.9126074666063771490, -0.4088369013363281623 ) ) ;
#167746 = EDGE_CURVE ( 'NONE', #3631, #172600, #253551, .T. ) ;
#167745 = DIRECTION ( 'NONE',  ( -0.000000000000000000, -0.8490545835447252943, -0.5283051335749947564 ) ) ;
#167747 = CARTESIAN_POINT ( 'NONE',  ( -21.05000000000000071, 64.35000000001264198, -196.7392418215462726 ) ) ;
#167748 = CARTESIAN_POINT ( 'NONE',  ( -21.05000000000000071, 77.16270174994961906, -61.52310748452431710 ) ) ;
#167749 = CARTESIAN_POINT ( 'NONE',  ( 23.14999999999999503, 64.14229051353817113, -222.2212283990554624 ) ) ;
#167750 = CARTESIAN_POINT ( 'NONE',  ( -17.01764560440361507, 66.05000000001182059, -82.27310748373757576 ) ) ;
#167751 = ORIENTED_EDGE ( 'NONE', *, *, #89371, .F. ) ;
#167752 = CARTESIAN_POINT ( 'NONE',  ( -18.50000000000000000, 9.150000000011157653, -179.8499999999999943 ) ) ;
#167753 = EDGE_CURVE ( 'NONE', #152240, #84905, #167355, .T. ) ;
#167754 = DIRECTION ( 'NONE',  ( 0.000000000000000000, 0.1350103645451904977, 0.9908441862701596881 ) ) ;
#167755 = DIRECTION ( 'NONE',  ( -3.265361837132813093E-16, -1.000000000000000000, -6.982962677686266711E-15 ) ) ;
#167756 = CARTESIAN_POINT ( 'NONE',  ( -16.92507428761700439, 66.05000000001230376, -157.3097100249028699 ) ) ;
#167757 = ADVANCED_FACE ( 'NONE', ( #249112 ), #87434, .F. ) ;
#167758 = ADVANCED_FACE ( 'NONE', ( #47015 ), #50861, .F. ) ;
#167759 = DIRECTION ( 'NONE',  ( 1.186688945009010077E-16, -1.000000000000000000, -0.000000000000000000 ) ) ;
#167760 = DIRECTION ( 'NONE',  ( -1.000000000000000000, 0.000000000000000000, 0.000000000000000000 ) ) ;
#167761 = CIRCLE ( 'NONE', #26279, 11.75000000000000711 ) ;
#167762 = VERTEX_POINT ( 'NONE', #148722 ) ;
#167763 = DIRECTION ( 'NONE',  ( 1.000000000000000000, 0.000000000000000000, 0.000000000000000000 ) ) ;
#167765 = EDGE_CURVE ( 'NONE', #126928, #64660, #105306, .T. ) ;
#167764 = PLANE ( 'NONE',  #71092 ) ;
#167766 = ORIENTED_EDGE ( 'NONE', *, *, #72597, .T. ) ;
#167767 = ORIENTED_EDGE ( 'NONE', *, *, #158161, .F. ) ;
#167768 = CARTESIAN_POINT ( 'NONE',  ( 18.49999999999999289, 11.75000000001115552, -158.8500000000000227 ) ) ;
#167769 = CARTESIAN_POINT ( 'NONE',  ( 21.05000000000000071, 11.38316329224760892, -198.5208684056144079 ) ) ;
#167770 = EDGE_CURVE ( 'NONE', #72258, #152104, #34101, .T. ) ;
#167771 = EDGE_CURVE ( 'NONE', #2973, #44901, #58970, .T. ) ;
#167772 = DIRECTION ( 'NONE',  ( 1.000000000000000000, -0.000000000000000000, -0.000000000000000000 ) ) ;
#167773 = VERTEX_POINT ( 'NONE', #207415 ) ;
#167774 = DIRECTION ( 'NONE',  ( 1.000000000000000000, 0.000000000000000000, 0.000000000000000000 ) ) ;
#167775 = CARTESIAN_POINT ( 'NONE',  ( -21.64999999999999858, 68.75000000001230660, -157.7731074845244166 ) ) ;
#167776 = EDGE_CURVE ( 'NONE', #164965, #15694, #208703, .T. ) ;
#167777 = CIRCLE ( 'NONE', #59373, 0.09999999999999939493 ) ;
#167778 = VERTEX_POINT ( 'NONE', #204810 ) ;
#167779 = CIRCLE ( 'NONE', #105352, 12.87499999999999645 ) ;
#167780 = DIRECTION ( 'NONE',  ( 0.000000000000000000, 1.224646799142185182E-16, 1.000000000000000000 ) ) ;
#167781 = CIRCLE ( 'NONE', #51200, 0.09999999999998898659 ) ;
#167782 = ORIENTED_EDGE ( 'NONE', *, *, #16767, .F. ) ;
#167783 = CARTESIAN_POINT ( 'NONE',  ( -21.05000000000000071, 30.73075574124490572, -252.3164853687435709 ) ) ;
#167784 = ADVANCED_FACE ( 'NONE', ( #187856 ), #238633, .F. ) ;
#167785 = DIRECTION ( 'NONE',  ( 1.000000000000000000, 0.000000000000000000, 0.000000000000000000 ) ) ;
#167786 = CARTESIAN_POINT ( 'NONE',  ( -20.94999999999999929, 17.06838326776700399, -224.6250846885016870 ) ) ;
#167787 = CARTESIAN_POINT ( 'NONE',  ( 20.94999999999999929, 6.450000000011156587, -144.0170271704400307 ) ) ;
#167789 = LINE ( 'NONE', #186041, #70287 ) ;
#167788 = UNCERTAINTY_MEASURE_WITH_UNIT (LENGTH_MEASURE( 1.000000000000000082E-05 ), #231420, 'distance_accuracy_value', 'NONE');
#167790 = CARTESIAN_POINT ( 'NONE',  ( -21.07016717456945898, 69.67905916191242000, -203.5231074845244450 ) ) ;
#167791 = CARTESIAN_POINT ( 'NONE',  ( -16.82542659449973144, 66.06550010858485678, -157.2784718844984013 ) ) ;
#167792 = CARTESIAN_POINT ( 'NONE',  ( 20.94999999999999929, -11.48912529306489994, -164.4000000000000057 ) ) ;
#167793 = AXIS2_PLACEMENT_3D ( 'NONE', #257980, #217595, #123665 ) ;
#167794 = CARTESIAN_POINT ( 'NONE',  ( -23.25000000000000355, 34.05335961020092128, -234.8258093264404351 ) ) ;
#167796 = LINE ( 'NONE', #52942, #162403 ) ;
#167795 = AXIS2_PLACEMENT_3D ( 'NONE', #68738, #72604, #148269 ) ;
#167798 = EDGE_LOOP ( 'NONE', ( #212425, #210777, #131419, #155431 ) ) ;
#167797 = DIRECTION ( 'NONE',  ( -0.000000000000000000, 1.000000000000000000, 0.000000000000000000 ) ) ;
#167799 = ORIENTED_EDGE ( 'NONE', *, *, #45508, .T. ) ;
#167801 = CARTESIAN_POINT ( 'NONE',  ( -15.69373346032659811, 9.356790025057039273, -84.20482650861393381 ) ) ;
#167800 = DIRECTION ( 'NONE',  ( 1.000000000000000000, 0.000000000000000000, 0.000000000000000000 ) ) ;
#167803 = ORIENTED_EDGE ( 'NONE', *, *, #181939, .T. ) ;
#167802 = DIRECTION ( 'NONE',  ( -1.000000000000000000, 0.000000000000000000, -0.000000000000000000 ) ) ;
#167804 = EDGE_LOOP ( 'NONE', ( #62825, #94892, #217267, #61712, #236944 ) ) ;
#167805 = CARTESIAN_POINT ( 'NONE',  ( -16.79363873026997922, 66.05114977059410819, -182.6769537030789650 ) ) ;
#167806 = DIRECTION ( 'NONE',  ( 1.000000000000000000, 0.000000000000000000, 0.000000000000000000 ) ) ;
#167807 = DIRECTION ( 'NONE',  ( 1.000000000000000000, 0.000000000000000000, 0.000000000000000000 ) ) ;
#167808 = VECTOR ( 'NONE', #44133, 1000.000000000000000 ) ;
#167809 = DIRECTION ( 'NONE',  ( 1.000000000000000000, -3.265361837132813093E-16, -2.280189983783949500E-30 ) ) ;
#167810 = DIRECTION ( 'NONE',  ( -1.000000000000000000, 0.000000000000000000, 0.000000000000000000 ) ) ;
#167811 = DIRECTION ( 'NONE',  ( -1.000000000000000000, 7.304098846218135653E-16, 0.000000000000000000 ) ) ;
#167812 = AXIS2_PLACEMENT_3D ( 'NONE', #75021, #154559, #136208 ) ;
#167813 = AXIS2_PLACEMENT_3D ( 'NONE', #59355, #215877, #73862 ) ;
#167814 = VECTOR ( 'NONE', #57060, 1000.000000000000114 ) ;
#167816 = AXIS2_PLACEMENT_3D ( 'NONE', #217585, #74286, #153842 ) ;
#167815 = FACE_OUTER_BOUND ( 'NONE', #122650, .T. ) ;
#167818 = ORIENTED_EDGE ( 'NONE', *, *, #147637, .T. ) ;
#167817 = ADVANCED_FACE ( 'NONE', ( #48318 ), #185269, .T. ) ;
#167819 = VERTEX_POINT ( 'NONE', #169605 ) ;
#167820 = LINE ( 'NONE', #68693, #123052 ) ;
#167821 = EDGE_CURVE ( 'NONE', #20356, #192641, #9193, .T. ) ;
#167822 = ORIENTED_EDGE ( 'NONE', *, *, #184120, .T. ) ;
#167823 = CARTESIAN_POINT ( 'NONE',  ( -20.54999999999999716, 68.75000000001179501, -81.77310748452435973 ) ) ;
#167824 = ORIENTED_EDGE ( 'NONE', *, *, #45193, .F. ) ;
#167825 = DIRECTION ( 'NONE',  ( 1.000000000000000000, 2.952720810173289112E-16, -0.000000000000000000 ) ) ;
#167826 = CARTESIAN_POINT ( 'NONE',  ( 20.85000000000000142, 64.35000000001170406, -69.52310748452438816 ) ) ;
#167827 = EDGE_CURVE ( 'NONE', #188929, #52766, #159534, .T. ) ;
#167829 = EDGE_CURVE ( 'NONE', #96547, #51183, #88178, .T. ) ;
#167828 = DIRECTION ( 'NONE',  ( 1.000000000000000000, -3.265361837132813093E-16, -2.280189983783949500E-30 ) ) ;
#167830 = DIRECTION ( 'NONE',  ( -1.000000000000000000, 0.000000000000000000, 0.000000000000000000 ) ) ;
#167831 = ORIENTED_EDGE ( 'NONE', *, *, #155993, .F. ) ;
#167832 = CARTESIAN_POINT ( 'NONE',  ( -20.64999999999999858, 85.00000000001197975, -112.4170766071766678 ) ) ;
#167833 = EDGE_LOOP ( 'NONE', ( #137681, #153819, #29410, #175266 ) ) ;
#167834 = CARTESIAN_POINT ( 'NONE',  ( -23.25000000000000000, -1.736705739456431807, -78.51742258762372728 ) ) ;
#167835 = DIRECTION ( 'NONE',  ( 1.000000000000000000, 0.000000000000000000, -0.000000000000000000 ) ) ;
#167836 = CARTESIAN_POINT ( 'NONE',  ( 18.43473516226070075, 8.856315488830345473, -245.4294710645858117 ) ) ;
#167837 = EDGE_LOOP ( 'NONE', ( #201921, #218351, #114450, #154981 ) ) ;
#167838 = AXIS2_PLACEMENT_3D ( 'NONE', #155473, #150306, #211558 ) ;
#167839 = CARTESIAN_POINT ( 'NONE',  ( 23.25000000000000000, 87.75000000001222134, -148.2731074845242176 ) ) ;
#167840 = ORIENTED_EDGE ( 'NONE', *, *, #68491, .T. ) ;
#167843 = ORIENTED_EDGE ( 'NONE', *, *, #14562, .T. ) ;
#167842 = DIRECTION ( 'NONE',  ( -0.7071067811865463515, -0.7071067811865487940, 7.587431340288849180E-16 ) ) ;
#167841 = CARTESIAN_POINT ( 'NONE',  ( 18.49999999999999289, 64.25000000001149658, -44.67310748452440095 ) ) ;
#167844 = DIRECTION ( 'NONE',  ( -0.7071067811865475727, -0.7071067811865475727, -0.000000000000000000 ) ) ;
#167845 = VERTEX_POINT ( 'NONE', #69198 ) ;
#167846 = DIRECTION ( 'NONE',  ( -1.000000000000000000, -0.000000000000000000, -0.000000000000000000 ) ) ;
#167847 = VERTEX_POINT ( 'NONE', #109566 ) ;
#167848 = AXIS2_PLACEMENT_3D ( 'NONE', #116849, #3296, #198942 ) ;
#167849 = CIRCLE ( 'NONE', #234441, 3.899999999999999023 ) ;
#167850 = CARTESIAN_POINT ( 'NONE',  ( -21.05000000000000071, 74.83729825007462466, -195.4231074845243654 ) ) ;
#167851 = CARTESIAN_POINT ( 'NONE',  ( 20.12500000000000000, 66.25000000001189449, -94.91133620241009794 ) ) ;
#167852 = CARTESIAN_POINT ( 'NONE',  ( -16.91256925476569961, 51.71161613007731006, -231.8657639032808504 ) ) ;
#167853 = CIRCLE ( 'NONE', #88694, 0.09999999999999939493 ) ;
#167854 = FACE_OUTER_BOUND ( 'NONE', #252886, .T. ) ;
#167855 = VECTOR ( 'NONE', #251187, 1000.000000000000000 ) ;
#167856 = ORIENTED_EDGE ( 'NONE', *, *, #78727, .T. ) ;
#167857 = AXIS2_PLACEMENT_3D ( 'NONE', #162758, #69757, #149298 ) ;
#167858 = CIRCLE ( 'NONE', #130415, 0.09999999999998712696 ) ;
#167859 = LINE ( 'NONE', #49159, #40128 ) ;
#167860 = CARTESIAN_POINT ( 'NONE',  ( 18.50016250449482413, 10.29766095125186354, -139.4743663933279265 ) ) ;
#167861 = ORIENTED_EDGE ( 'NONE', *, *, #227057, .T. ) ;
#167862 = EDGE_CURVE ( 'NONE', #198292, #109096, #121584, .T. ) ;
#167863 = DIRECTION ( 'NONE',  ( 0.000000000000000000, -1.000000000000000000, -6.860497997771531562E-15 ) ) ;
#167864 = EDGE_LOOP ( 'NONE', ( #105697, #167441, #5312, #1951 ) ) ;
#167865 = LINE ( 'NONE', #24497, #197880 ) ;
#167866 = AXIS2_PLACEMENT_3D ( 'NONE', #118090, #161081, #240606 ) ;
#167867 = LINE ( 'NONE', #107856, #251588 ) ;
#167868 = CARTESIAN_POINT ( 'NONE',  ( 20.94999999999999929, -1.162701749938009677, -7.900000000000000355 ) ) ;
#167870 = ORIENTED_EDGE ( 'NONE', *, *, #200286, .T. ) ;
#167869 = DIRECTION ( 'NONE',  ( 1.836970198721029934E-16, -0.9770955615653316162, -0.2128009952263604232 ) ) ;
#167871 = AXIS2_PLACEMENT_3D ( 'NONE', #200041, #82614, #83891 ) ;
#167872 = EDGE_CURVE ( 'NONE', #162117, #189189, #204725, .T. ) ;
#167873 = CARTESIAN_POINT ( 'NONE',  ( 20.85000000000000142, 76.00000000001190870, -103.0231074845243029 ) ) ;
#167874 = AXIS2_PLACEMENT_3D ( 'NONE', #221012, #101025, #21556 ) ;
#167875 = DIRECTION ( 'NONE',  ( -1.000000000000000000, -0.000000000000000000, -0.000000000000000000 ) ) ;
#167876 = ADVANCED_FACE ( 'NONE', ( #229540 ), #31368, .F. ) ;
#167877 = VERTEX_POINT ( 'NONE', #6619 ) ;
#167878 = CARTESIAN_POINT ( 'NONE',  ( 12.25000000000000000, 66.15000000001258229, -186.7731074845244450 ) ) ;
#167879 = FACE_OUTER_BOUND ( 'NONE', #185597, .T. ) ;
#167880 = ORIENTED_EDGE ( 'NONE', *, *, #153026, .T. ) ;
#167881 = DIRECTION ( 'NONE',  ( 0.000000000000000000, -6.982962677686266711E-15, 1.000000000000000000 ) ) ;
#167882 = AXIS2_PLACEMENT_3D ( 'NONE', #227824, #146990, #89586 ) ;
#167883 = ORIENTED_EDGE ( 'NONE', *, *, #33030, .F. ) ;
#167884 = AXIS2_PLACEMENT_3D ( 'NONE', #187932, #107092, #54494 ) ;
#167885 = VECTOR ( 'NONE', #250873, 1000.000000000000000 ) ;
#167886 = EDGE_CURVE ( 'NONE', #54060, #141666, #150584, .T. ) ;
#167887 = CARTESIAN_POINT ( 'NONE',  ( -20.54999999999999716, -3.770473190032741062, -225.9805569534692324 ) ) ;
#167888 = AXIS2_PLACEMENT_3D ( 'NONE', #33027, #72117, #168687 ) ;
#167889 = FACE_OUTER_BOUND ( 'NONE', #42911, .T. ) ;
#167890 = ADVANCED_FACE ( 'NONE', ( #134258 ), #229699, .T. ) ;
#167891 = EDGE_CURVE ( 'NONE', #167448, #14564, #250375, .T. ) ;
#167894 = ORIENTED_EDGE ( 'NONE', *, *, #189723, .F. ) ;
#167893 = VERTEX_POINT ( 'NONE', #252930 ) ;
#167892 = CARTESIAN_POINT ( 'NONE',  ( 21.14999999999999858, 11.75000000001116263, -88.75000000000004263 ) ) ;
#167895 = CARTESIAN_POINT ( 'NONE',  ( 20.85000000000000142, 1.115600667400684642E-11, -134.0000000000000284 ) ) ;
#167896 = CARTESIAN_POINT ( 'NONE',  ( 18.59999999999999076, 61.95000000001160601, -64.00941241376344237 ) ) ;
#167897 = DIRECTION ( 'NONE',  ( -1.000000000000000000, 0.000000000000000000, 0.000000000000000000 ) ) ;
#167898 = ADVANCED_FACE ( 'NONE', ( #151296 ), #83890, .F. ) ;
#167900 = DIRECTION ( 'NONE',  ( 0.000000000000000000, -1.000000000000000000, 0.000000000000000000 ) ) ;
#167899 = CARTESIAN_POINT ( 'NONE',  ( 23.14999999999999503, 6.649999999999999467, -21.25000000000000000 ) ) ;
#167901 = LINE ( 'NONE', #27108, #207447 ) ;
#167902 = CARTESIAN_POINT ( 'NONE',  ( 22.50000000000000000, 36.65892442174472876, -249.5511627012454596 ) ) ;
#167903 = VECTOR ( 'NONE', #117464, 1000.000000000000000 ) ;
#167905 = B_SPLINE_CURVE_WITH_KNOTS ( 'NONE', 3,
 ( #21335, #159546, #18738, #180391, #1727, #257291 ),
 .UNSPECIFIED., .F., .F.,
 ( 4, 2, 4 ),
 ( 0.000000000000000000, 0.0001569047307838623796, 0.0003138094615677247592 ),
 .UNSPECIFIED. ) ;
#167904 = CARTESIAN_POINT ( 'NONE',  ( -18.40000000000000213, 50.88295650978584206, -230.3037755757580953 ) ) ;
#167906 = AXIS2_PLACEMENT_3D ( 'NONE', #42679, #221295, #6103 ) ;
#167907 = CARTESIAN_POINT ( 'NONE',  ( -22.50000000000000000, 11.64957080755595520, -33.40000000000000568 ) ) ;
#167908 = CIRCLE ( 'NONE', #9656, 0.1999999999999987899 ) ;
#167909 = AXIS2_PLACEMENT_3D ( 'NONE', #20145, #37150, #197474 ) ;
#167910 = ORIENTED_EDGE ( 'NONE', *, *, #168743, .T. ) ;
#167911 = VERTEX_POINT ( 'NONE', #131712 ) ;
#167912 = DIRECTION ( 'NONE',  ( -1.000000000000000000, -0.000000000000000000, -0.000000000000000000 ) ) ;
#167914 = ORIENTED_EDGE ( 'NONE', *, *, #216392, .F. ) ;
#167913 = CYLINDRICAL_SURFACE ( 'NONE', #141886, 0.09999999999998898659 ) ;
#167915 = VERTEX_POINT ( 'NONE', #75616 ) ;
#167916 = ADVANCED_FACE ( 'NONE', ( #234666 ), #79825, .T. ) ;
#167917 = CARTESIAN_POINT ( 'NONE',  ( 23.24999999999999645, 76.00000000001126921, -203.5231074845248997 ) ) ;
#167918 = ORIENTED_EDGE ( 'NONE', *, *, #101821, .F. ) ;
#167919 = CARTESIAN_POINT ( 'NONE',  ( -21.13435531349801266, 69.50627893641960497, -136.5231074845243313 ) ) ;
#167920 = ORIENTED_EDGE ( 'NONE', *, *, #48442, .T. ) ;
#167921 = CYLINDRICAL_SURFACE ( 'NONE', #118989, 0.09999999999999939493 ) ;
#167922 = DIRECTION ( 'NONE',  ( 1.000000000000000000, 0.000000000000000000, 0.000000000000000000 ) ) ;
#167924 = ORIENTED_EDGE ( 'NONE', *, *, #56339, .F. ) ;
#167923 = VERTEX_POINT ( 'NONE', #213818 ) ;
#167925 = ORIENTED_EDGE ( 'NONE', *, *, #147689, .F. ) ;
#167926 = CARTESIAN_POINT ( 'NONE',  ( 21.14261333020286671, 10.71569264926606202, -45.75000000000021316 ) ) ;
#167927 = VERTEX_POINT ( 'NONE', #114720 ) ;
#167928 = ORIENTED_EDGE ( 'NONE', *, *, #55553, .T. ) ;
#167929 = DIRECTION ( 'NONE',  ( -2.978066053179067258E-16, -0.4088369013363278293, 0.9126074666063771490 ) ) ;
#167930 = SPHERICAL_SURFACE ( 'NONE', #232358, 0.1000000000000000056 ) ;
#167931 = TOROIDAL_SURFACE ( 'NONE', #130295, 11.70000000000000107, 0.1000000000000000056 ) ;
#167932 = CARTESIAN_POINT ( 'NONE',  ( -15.75000000000000355, 9.350000000011140955, -184.2499999999999716 ) ) ;
#167934 = ORIENTED_EDGE ( 'NONE', *, *, #164993, .F. ) ;
#167933 = DIRECTION ( 'NONE',  ( -3.265361837132813093E-16, 1.000000000000000000, 0.000000000000000000 ) ) ;
#167935 = CARTESIAN_POINT ( 'NONE',  ( -21.65000000000000213, 7.750000000011155521, -45.85000000000000142 ) ) ;
#167936 = CARTESIAN_POINT ( 'NONE',  ( 20.73486653747088582, 68.75000000001183764, -90.37310748452435405 ) ) ;
#167938 = EDGE_LOOP ( 'NONE', ( #195319, #214327, #163097 ) ) ;
#167937 = CYLINDRICAL_SURFACE ( 'NONE', #5855, 0.5000000000000004441 ) ;
#167939 = ORIENTED_EDGE ( 'NONE', *, *, #170791, .T. ) ;
#167940 = CARTESIAN_POINT ( 'NONE',  ( -21.05000000000000071, 69.70076908991968878, -103.1215449845246468 ) ) ;
#167941 = VERTEX_POINT ( 'NONE', #155164 ) ;
#167942 = CARTESIAN_POINT ( 'NONE',  ( 21.76363531954645936, 68.98706345214066005, -170.1221093588238489 ) ) ;
#167943 = DIRECTION ( 'NONE',  ( -1.000000000000000000, -0.000000000000000000, -0.000000000000000000 ) ) ;
#167944 = ORIENTED_EDGE ( 'NONE', *, *, #50252, .F. ) ;
#167946 = CARTESIAN_POINT ( 'NONE',  ( 18.59999999999999076, 64.35000000001147669, -44.67310748452440095 ) ) ;
#167945 = DIRECTION ( 'NONE',  ( -1.000000000000000000, 0.000000000000000000, 0.000000000000000000 ) ) ;
#167947 = CIRCLE ( 'NONE', #147052, 0.09999999999998898659 ) ;
#167948 = DIRECTION ( 'NONE',  ( 0.000000000000000000, -0.2128009952263403282, 0.9770955615653358350 ) ) ;
#167949 = EDGE_CURVE ( 'NONE', #89549, #64826, #217757, .T. ) ;
#167950 = AXIS2_PLACEMENT_3D ( 'NONE', #234759, #19575, #117383 ) ;
#167951 = DIRECTION ( 'NONE',  ( 1.000000000000000000, 0.000000000000000000, 0.000000000000000000 ) ) ;
#167952 = CARTESIAN_POINT ( 'NONE',  ( -20.65000000000000568, 68.75000000001182343, -82.17310748452436542 ) ) ;
#167953 = EDGE_LOOP ( 'NONE', ( #61300, #166033, #149263, #203177 ) ) ;
#167954 = VERTEX_POINT ( 'NONE', #153898 ) ;
#167955 = PLANE ( 'NONE',  #205355 ) ;
#167956 = DIRECTION ( 'NONE',  ( -1.000000000000000000, -2.885090398161910739E-16, -6.283419270304611573E-17 ) ) ;
#167957 = ORIENTED_EDGE ( 'NONE', *, *, #156572, .F. ) ;
#167958 = DIRECTION ( 'NONE',  ( 1.000000000000000000, 3.265361837132813093E-16, -0.000000000000000000 ) ) ;
#167959 = VERTEX_POINT ( 'NONE', #212551 ) ;
#167960 = DIRECTION ( 'NONE',  ( 1.000000000000000000, -0.000000000000000000, 0.000000000000000000 ) ) ;
#167961 = ADVANCED_FACE ( 'NONE', ( #71759 ), #60032, .T. ) ;
#167962 = ORIENTED_EDGE ( 'NONE', *, *, #7479, .T. ) ;
#167963 = FACE_OUTER_BOUND ( 'NONE', #199903, .T. ) ;
#167964 = DIRECTION ( 'NONE',  ( -1.000000000000000000, 0.000000000000000000, 0.000000000000000000 ) ) ;
#167965 = DIRECTION ( 'NONE',  ( 1.000000000000000000, 0.000000000000000000, 0.000000000000000000 ) ) ;
#167966 = EDGE_CURVE ( 'NONE', #174912, #113945, #73064, .T. ) ;
#167967 = EDGE_CURVE ( 'NONE', #82879, #63155, #221469, .T. ) ;
#167968 = ORIENTED_EDGE ( 'NONE', *, *, #205494, .T. ) ;
#167969 = CIRCLE ( 'NONE', #130512, 1.749999999999999778 ) ;
#167970 = CARTESIAN_POINT ( 'NONE',  ( -16.80939487329395021, 63.08573235307446225, -213.1276215869279724 ) ) ;
#167971 = SHAPE_REPRESENTATION_RELATIONSHIP ( 'NONE' , 'NONE' ,  #135069, #48300 ) ;
#167972 = AXIS2_PLACEMENT_3D ( 'NONE', #214592, #76358, #33443 ) ;
#167973 = B_SPLINE_CURVE_WITH_KNOTS ( 'NONE', 3,
 ( #199884, #1644, #42099, #39543, #121636, #81176, #56479, #100721 ),
 .UNSPECIFIED., .F., .F.,
 ( 4, 2, 2, 4 ),
 ( 0.000000000000000000, 0.0001306511400391193183, 0.0001959767100587024775, 0.0002613022800782856367 ),
 .UNSPECIFIED. ) ;
#167974 = ORIENTED_EDGE ( 'NONE', *, *, #59349, .T. ) ;
#167975 = ORIENTED_EDGE ( 'NONE', *, *, #85638, .F. ) ;
#167976 = ORIENTED_EDGE ( 'NONE', *, *, #130674, .F. ) ;
#167977 = CIRCLE ( 'NONE', #192894, 3.999999999999996447 ) ;
#167978 = CARTESIAN_POINT ( 'NONE',  ( 22.49533356619859603, 64.34999999370803891, -136.5882300648470959 ) ) ;
#167979 = FACE_OUTER_BOUND ( 'NONE', #221366, .T. ) ;
#167980 = DIRECTION ( 'NONE',  ( 0.000000000000000000, -0.8660254037844377084, -0.5000000000000016653 ) ) ;
#167981 = DIRECTION ( 'NONE',  ( 0.000000000000000000, -6.853228547068871147E-15, 1.000000000000000000 ) ) ;
#167982 = CARTESIAN_POINT ( 'NONE',  ( 19.75857864376268935, 64.25000000001176659, -78.17310748452439384 ) ) ;
#167983 = EDGE_CURVE ( 'NONE', #87673, #17147, #135546, .T. ) ;
#167985 = CARTESIAN_POINT ( 'NONE',  ( 20.94999999999999929, -11.29603075032412995, -170.5478991596638423 ) ) ;
#167984 = CARTESIAN_POINT ( 'NONE',  ( 21.14999999999999858, 1.115488181425289271E-11, -160.9593430482987344 ) ) ;
#167987 = ORIENTED_EDGE ( 'NONE', *, *, #181744, .T. ) ;
#167986 = LINE ( 'NONE', #247483, #218799 ) ;
#167988 = PLANE ( 'NONE',  #212504 ) ;
#167989 = ORIENTED_EDGE ( 'NONE', *, *, #144288, .F. ) ;
#167990 = EDGE_CURVE ( 'NONE', #44800, #206460, #250531, .T. ) ;
#167991 = DIRECTION ( 'NONE',  ( 0.000000000000000000, -0.9651348961777157509, 0.2617529984165031243 ) ) ;
#167992 = ORIENTED_EDGE ( 'NONE', *, *, #27988, .T. ) ;
#167993 = ORIENTED_EDGE ( 'NONE', *, *, #18461, .F. ) ;
#167994 = CARTESIAN_POINT ( 'NONE',  ( -17.11825945287481332, 65.95000000001181206, -82.17310748452439384 ) ) ;
#167996 = TOROIDAL_SURFACE ( 'NONE', #34901, 0.2000000000000000111, 0.1000000000000000056 ) ;
#167995 = CARTESIAN_POINT ( 'NONE',  ( 23.24999999999999289, 6.649999999999999467, -12.15000000000000036 ) ) ;
#167997 = CARTESIAN_POINT ( 'NONE',  ( -21.04999999999999716, 76.01465611852667337, -210.0197940702928463 ) ) ;
#167998 = VECTOR ( 'NONE', #150247, 1000.000000000000000 ) ;
#167999 = PLANE ( 'NONE',  #29238 ) ;
#168000 = PRODUCT_DEFINITION ( 'UNKNOWN', '', #140510, #81763 ) ;
#168001 = AXIS2_PLACEMENT_3D ( 'NONE', #127995, #206243, #66737 ) ;
#168002 = DIRECTION ( 'NONE',  ( 0.000000000000000000, 0.6728971962617172897, -0.7397360091702445128 ) ) ;
#168003 = ORIENTED_EDGE ( 'NONE', *, *, #145036, .F. ) ;
#168004 = VERTEX_POINT ( 'NONE', #255458 ) ;
#168005 = EDGE_CURVE ( 'NONE', #160572, #45962, #215100, .T. ) ;
#168006 = CIRCLE ( 'NONE', #97175, 0.09999999999999609201 ) ;
#168007 = DIRECTION ( 'NONE',  ( 0.000000000000000000, 0.000000000000000000, -1.000000000000000000 ) ) ;
#168009 = EDGE_LOOP ( 'NONE', ( #60763, #225306, #145508, #114247 ) ) ;
#168008 = EDGE_CURVE ( 'NONE', #214060, #125402, #91310, .T. ) ;
#168010 = DIRECTION ( 'NONE',  ( 0.000000000000000000, 0.2128009952263678062, -0.9770955615653298398 ) ) ;
#168011 = DIRECTION ( 'NONE',  ( 0.000000000000000000, 0.000000000000000000, 1.000000000000000000 ) ) ;
#168012 = EDGE_LOOP ( 'NONE', ( #168003, #15599, #33411, #236107 ) ) ;
#168013 = EDGE_CURVE ( 'NONE', #173624, #220140, #138636, .T. ) ;
#168014 = CARTESIAN_POINT ( 'NONE',  ( 21.05000000000000071, 85.40000000001252545, -179.9170766071767389 ) ) ;
#168015 = CARTESIAN_POINT ( 'NONE',  ( 18.39999999999999858, 85.50000000001233502, -162.9910380878246201 ) ) ;
#168016 = CARTESIAN_POINT ( 'NONE',  ( -16.91049119928363353, 66.05000000001209060, -123.9048278777151921 ) ) ;
#168017 = CARTESIAN_POINT ( 'NONE',  ( 21.33487959338958362, 6.725558151922348848, -67.00000000000004263 ) ) ;
#168018 = ORIENTED_EDGE ( 'NONE', *, *, #20406, .T. ) ;
#168019 = DIRECTION ( 'NONE',  ( 0.000000000000000000, 0.000000000000000000, -1.000000000000000000 ) ) ;
#168020 = AXIS2_PLACEMENT_3D ( 'NONE', #38430, #60546, #18859 ) ;
#168022 = CARTESIAN_POINT ( 'NONE',  ( 20.90000000000000213, 11.49641995933507843, -1.885425182446133885 ) ) ;
#168021 = AXIS2_PLACEMENT_3D ( 'NONE', #221679, #66481, #43071 ) ;
#168024 = LINE ( 'NONE', #231820, #229186 ) ;
#168023 = CIRCLE ( 'NONE', #97181, 0.09999999999998898659 ) ;
#168025 = AXIS2_PLACEMENT_3D ( 'NONE', #232809, #213205, #157123 ) ;
#168026 = FACE_OUTER_BOUND ( 'NONE', #80792, .T. ) ;
#168027 = CARTESIAN_POINT ( 'NONE',  ( 23.14999999999999503, 14.10000000001115694, -128.3997023888606748 ) ) ;
#168028 = EDGE_CURVE ( 'NONE', #43598, #151638, #198100, .T. ) ;
#168029 = DIRECTION ( 'NONE',  ( 1.000000000000000000, -0.000000000000000000, -0.000000000000000000 ) ) ;
#168030 = VERTEX_POINT ( 'NONE', #23351 ) ;
#168031 = LINE ( 'NONE', #186280, #170405 ) ;
#168032 = VERTEX_POINT ( 'NONE', #80703 ) ;
#168033 = CARTESIAN_POINT ( 'NONE',  ( -23.25000000000000000, -11.64999999998884483, -164.4000000000000057 ) ) ;
#168034 = DIRECTION ( 'NONE',  ( -0.000000000000000000, 0.1350103645451807555, 0.9908441862701610203 ) ) ;
#168035 = CARTESIAN_POINT ( 'NONE',  ( -20.64999999999999858, 76.00000000001213607, -136.5231074845242745 ) ) ;
#168036 = DIRECTION ( 'NONE',  ( 1.000000000000000000, 2.952720810173289112E-16, -0.000000000000000000 ) ) ;
#168037 = ORIENTED_EDGE ( 'NONE', *, *, #185984, .F. ) ;
#168038 = EDGE_CURVE ( 'NONE', #156961, #14219, #13231, .T. ) ;
#168039 = CARTESIAN_POINT ( 'NONE',  ( -20.54999999999999361, 51.38014393322265505, -230.1906178717505611 ) ) ;
#168040 = AXIS2_PLACEMENT_3D ( 'NONE', #237016, #177063, #49711 ) ;
#168041 = FACE_OUTER_BOUND ( 'NONE', #206256, .T. ) ;
#168042 = DIRECTION ( 'NONE',  ( 0.000000000000000000, 0.000000000000000000, 1.000000000000000000 ) ) ;
#168044 = AXIS2_PLACEMENT_3D ( 'NONE', #73357, #36805, #14665 ) ;
#168043 = DIRECTION ( 'NONE',  ( 1.186688945009010077E-16, 0.9651348961777157509, -0.2617529984165031243 ) ) ;
#168045 = AXIS2_PLACEMENT_3D ( 'NONE', #28923, #49718, #169711 ) ;
#168046 = CARTESIAN_POINT ( 'NONE',  ( 22.47809213839789066, 75.96246293238394287, -181.6730808193121618 ) ) ;
#168047 = ORIENTED_EDGE ( 'NONE', *, *, #231577, .F. ) ;
#168048 = ORIENTED_EDGE ( 'NONE', *, *, #134514, .T. ) ;
#168049 = CARTESIAN_POINT ( 'NONE',  ( 20.94999999999999929, 5.000000000011153745, -146.4052660189131245 ) ) ;
#168050 = DIRECTION ( 'NONE',  ( 1.000000000000000000, 0.000000000000000000, 0.000000000000000000 ) ) ;
#168051 = TOROIDAL_SURFACE ( 'NONE', #226218, 11.65000000000000036, 0.1000000000000000056 ) ;
#168052 = LINE ( 'NONE', #183731, #121704 ) ;
#168054 = EDGE_CURVE ( 'NONE', #7052, #245185, #97689, .T. ) ;
#168053 = DIRECTION ( 'NONE',  ( 0.000000000000000000, 0.000000000000000000, -1.000000000000000000 ) ) ;
#168055 = AXIS2_PLACEMENT_3D ( 'NONE', #41891, #101805, #142243 ) ;
#168056 = DIRECTION ( 'NONE',  ( 1.000000000000000000, 0.000000000000000000, 0.000000000000000000 ) ) ;
#168057 = VERTEX_POINT ( 'NONE', #201964 ) ;
#168058 = CARTESIAN_POINT ( 'NONE',  ( 23.14999999999999858, 1.115600667400684642E-11, -67.00000000000000000 ) ) ;
#168059 = AXIS2_PLACEMENT_3D ( 'NONE', #97424, #180858, #177030 ) ;
#168060 = EDGE_CURVE ( 'NONE', #64537, #124804, #78139, .T. ) ;
#168061 = CONTEXT_DEPENDENT_SHAPE_REPRESENTATION ( #149119, #222525 ) ;
#168063 = AXIS2_PLACEMENT_3D ( 'NONE', #197335, #21311, #242892 ) ;
#168062 = DIRECTION ( 'NONE',  ( -1.000000000000000000, 0.000000000000000000, 0.000000000000000000 ) ) ;
#168064 = ORIENTED_EDGE ( 'NONE', *, *, #56276, .T. ) ;
#168065 = TOROIDAL_SURFACE ( 'NONE', #55538, 4.149999999999999467, 0.1000000000000000056 ) ;
#168066 = CARTESIAN_POINT ( 'NONE',  ( -20.54999999999999716, 1.115600667400684642E-11, -198.9999999999999432 ) ) ;
#168067 = AXIS2_PLACEMENT_3D ( 'NONE', #175911, #71669, #211161 ) ;
#168068 = PRODUCT ( 'Snap Open Cable Crossbars 6', 'Snap Open Cable Crossbars 6', '', ( #96462 ) ) ;
#168069 = EDGE_CURVE ( 'NONE', #11383, #218506, #113163, .T. ) ;
#168070 = EDGE_CURVE ( 'NONE', #229370, #207268, #146834, .T. ) ;
#168071 = VERTEX_POINT ( 'NONE', #81970 ) ;
#168072 = ORIENTED_EDGE ( 'NONE', *, *, #92631, .F. ) ;
#168073 = ORIENTED_EDGE ( 'NONE', *, *, #86116, .F. ) ;
#168074 = CARTESIAN_POINT ( 'NONE',  ( 21.05000000000000071, 10.48459288120634270, -74.45671357058543549 ) ) ;
#168075 = DIRECTION ( 'NONE',  ( 0.000000000000000000, 0.000000000000000000, 1.000000000000000000 ) ) ;
#168076 = CARTESIAN_POINT ( 'NONE',  ( 20.97468175916186084, 10.62526516438217605, -112.7547614354131724 ) ) ;
#168077 = CARTESIAN_POINT ( 'NONE',  ( -23.25000000000000000, 14.70949956575304185, -235.9560995168023112 ) ) ;
#168078 = DIRECTION ( 'NONE',  ( 0.000000000000000000, -0.9856811345164829818, -0.1686199900910294314 ) ) ;
#168079 = CARTESIAN_POINT ( 'NONE',  ( 20.94999999999999929, 8.876614585087098774, -8.385080478844676222 ) ) ;
#168080 = DIRECTION ( 'NONE',  ( 0.000000000000000000, 0.2128009952263485993, -0.9770955615653341697 ) ) ;
#168082 = DIRECTION ( 'NONE',  ( -0.000000000000000000, 0.2128009952263604232, -0.9770955615653316162 ) ) ;
#168081 = CARTESIAN_POINT ( 'NONE',  ( 20.95512820512820440, 65.37615131630001031, -95.35819391543677170 ) ) ;
#168083 = VECTOR ( 'NONE', #53368, 1000.000000000000000 ) ;
#168084 = CARTESIAN_POINT ( 'NONE',  ( 21.05000000000000071, -1.236118717437887371, -194.8647072476926212 ) ) ;
#168085 = DIRECTION ( 'NONE',  ( 1.000000000000000000, -0.000000000000000000, -0.000000000000000000 ) ) ;
#168086 = CARTESIAN_POINT ( 'NONE',  ( 22.49436431346199683, 0.06690352973341695542, -155.8500490523465203 ) ) ;
#168087 = CARTESIAN_POINT ( 'NONE',  ( 20.95132126680579532, 18.75531812006552457, -228.0605135901855647 ) ) ;
#168088 = ORIENTED_EDGE ( 'NONE', *, *, #102492, .T. ) ;
#168089 = ORIENTED_EDGE ( 'NONE', *, *, #236088, .T. ) ;
#168090 = CARTESIAN_POINT ( 'NONE',  ( -18.43459694179558639, -9.494210124998035738, -40.11700520266107617 ) ) ;
#168091 = ADVANCED_FACE ( 'NONE', ( #256739 ), #13401, .T. ) ;
#168092 = VECTOR ( 'NONE', #19047, 1000.000000000000000 ) ;
#168093 = DIRECTION ( 'NONE',  ( 1.000000000000000000, 0.000000000000000000, 0.000000000000000000 ) ) ;
#168095 = CARTESIAN_POINT ( 'NONE',  ( -14.11361717019516249, 13.17763673189382345, -217.0637590370182011 ) ) ;
#168094 = DIRECTION ( 'NONE',  ( -1.000000000000000000, 0.000000000000000000, 0.000000000000000000 ) ) ;
#168096 = AXIS2_PLACEMENT_3D ( 'NONE', #164637, #65516, #145054 ) ;
#168097 = AXIS2_PLACEMENT_3D ( 'NONE', #200409, #37500, #117022 ) ;
#168098 = CARTESIAN_POINT ( 'NONE',  ( 20.95420533658165141, 39.25354836604451947, -236.8330523274166808 ) ) ;
#168100 = EDGE_CURVE ( 'NONE', #164116, #34456, #161569, .T. ) ;
#168099 = FACE_OUTER_BOUND ( 'NONE', #216809, .T. ) ;
#168101 = CARTESIAN_POINT ( 'NONE',  ( -23.15000000000000213, 64.25000000001173817, -72.62310748452439668 ) ) ;
#168102 = ORIENTED_EDGE ( 'NONE', *, *, #70752, .F. ) ;
#168103 = VERTEX_POINT ( 'NONE', #121173 ) ;
#168104 = ADVANCED_FACE ( 'NONE', ( #218939 ), #241106, .T. ) ;
#168105 = DIRECTION ( 'NONE',  ( 1.000000000000000000, -0.000000000000000000, 0.000000000000000000 ) ) ;
#168106 = ORIENTED_EDGE ( 'NONE', *, *, #105248, .T. ) ;
#168107 = DIRECTION ( 'NONE',  ( 1.000000000000000000, 0.000000000000000000, 0.000000000000000000 ) ) ;
#168108 = ADVANCED_FACE ( 'NONE', ( #2454 ), #39051, .T. ) ;
#168109 = AXIS2_PLACEMENT_3D ( 'NONE', #257246, #78645, #198605 ) ;
#168110 = AXIS2_PLACEMENT_3D ( 'NONE', #103606, #22841, #241855 ) ;
#168111 = CIRCLE ( 'NONE', #155627, 9.500000000000001776 ) ;
#168112 = VECTOR ( 'NONE', #36066, 1000.000000000000000 ) ;
#168113 = CARTESIAN_POINT ( 'NONE',  ( 18.59999999999998366, 1.115600667400684642E-11, -134.0000000000000284 ) ) ;
#168114 = VERTEX_POINT ( 'NONE', #118589 ) ;
#168115 = CARTESIAN_POINT ( 'NONE',  ( 20.94999999999999574, 68.49522935589659767, -224.1230159437372436 ) ) ;
#168116 = ORIENTED_EDGE ( 'NONE', *, *, #201857, .T. ) ;
#168117 = ADVANCED_FACE ( 'NONE', ( #119879 ), #109235, .F. ) ;
#168118 = DIRECTION ( 'NONE',  ( 0.000000000000000000, 0.000000000000000000, 1.000000000000000000 ) ) ;
#168119 = ADVANCED_FACE ( 'NONE', ( #162854 ), #42887, .F. ) ;
#168120 = DIRECTION ( 'NONE',  ( 1.000000000000000000, 0.000000000000000000, 0.000000000000000000 ) ) ;
#168121 = DIRECTION ( 'NONE',  ( 1.000000000000000000, 0.000000000000000000, 0.000000000000000000 ) ) ;
#168122 = DIRECTION ( 'NONE',  ( -0.7071067811865388020, 0.7071067811865561215, 0.000000000000000000 ) ) ;
#168123 = CARTESIAN_POINT ( 'NONE',  ( 20.94999999999999929, 7.128833340094563376, -233.7327013124401276 ) ) ;
#168124 = CARTESIAN_POINT ( 'NONE',  ( -21.07016717457011268, 1.115057211061726283E-11, -60.67905916189913995 ) ) ;
#168125 = DIRECTION ( 'NONE',  ( 0.000000000000000000, -5.551115123125777653E-14, 1.000000000000000000 ) ) ;
#168126 = CARTESIAN_POINT ( 'NONE',  ( 28.12018973533754362, 11.62642356364896123, -347.0000000000001137 ) ) ;
#168128 = ORIENTED_EDGE ( 'NONE', *, *, #42349, .T. ) ;
#168127 = CARTESIAN_POINT ( 'NONE',  ( 18.41815437325345073, -0.7469876510888040499, -242.2067223904661830 ) ) ;
#168130 = DIRECTION ( 'NONE',  ( 1.000000000000000000, 0.000000000000000000, 0.000000000000000000 ) ) ;
#168129 = DIRECTION ( 'NONE',  ( 1.000000000000000000, 0.000000000000000000, 0.000000000000000000 ) ) ;
#168131 = VERTEX_POINT ( 'NONE', #83260 ) ;
#168133 = EDGE_LOOP ( 'NONE', ( #224625, #232521, #92144, #120508, #201986 ) ) ;
#168132 = DIRECTION ( 'NONE',  ( -3.265361837132813093E-16, 1.000000000000000000, -0.000000000000000000 ) ) ;
#168134 = VERTEX_POINT ( 'NONE', #20773 ) ;
#168135 = CARTESIAN_POINT ( 'NONE',  ( 20.94999999999999929, 36.65892442174935439, -249.5511627012433848 ) ) ;
#168136 = FACE_OUTER_BOUND ( 'NONE', #174094, .T. ) ;
#168137 = AXIS2_PLACEMENT_3D ( 'NONE', #38203, #139838, #98121 ) ;
#168138 = CARTESIAN_POINT ( 'NONE',  ( -21.00000000000000000, -11.65000000000000036, 11.89999999999999858 ) ) ;
#168139 = FACE_OUTER_BOUND ( 'NONE', #23952, .T. ) ;
#168140 = FACE_OUTER_BOUND ( 'NONE', #234885, .T. ) ;
#168141 = CARTESIAN_POINT ( 'NONE',  ( 20.94999999999999929, 85.00000000001159606, -59.62913836187181715 ) ) ;
#168142 = DIRECTION ( 'NONE',  ( 0.000000000000000000, 0.000000000000000000, 1.000000000000000000 ) ) ;
#168143 = CARTESIAN_POINT ( 'NONE',  ( 23.15000000000000213, -8.999999999988844479, -76.89396912265249284 ) ) ;
#168144 = DIRECTION ( 'NONE',  ( 0.000000000000000000, -0.9126074666063771490, -0.4088369013363281623 ) ) ;
#168145 = ORIENTED_EDGE ( 'NONE', *, *, #195454, .T. ) ;
#168146 = ORIENTED_EDGE ( 'NONE', *, *, #201003, .F. ) ;
#168147 = DIRECTION ( 'NONE',  ( 0.000000000000000000, 0.4088369013363205573, -0.9126074666063803686 ) ) ;
#168148 = CIRCLE ( 'NONE', #251288, 0.09999999999999939493 ) ;
#168149 = EDGE_CURVE ( 'NONE', #199921, #4454, #22051, .T. ) ;
#168150 = VECTOR ( 'NONE', #88491, 1000.000000000000000 ) ;
#168151 = ORIENTED_EDGE ( 'NONE', *, *, #150667, .F. ) ;
#168152 = CARTESIAN_POINT ( 'NONE',  ( 21.05000000000000071, 78.93126476241668854, -235.8702625865613243 ) ) ;
#168153 = ORIENTED_EDGE ( 'NONE', *, *, #158042, .T. ) ;
#168154 = CARTESIAN_POINT ( 'NONE',  ( -23.25000000000000000, 28.00279607545604321, -239.9795148779844283 ) ) ;
#168155 = AXIS2_PLACEMENT_3D ( 'NONE', #85454, #165031, #145453 ) ;
#168156 = CARTESIAN_POINT ( 'NONE',  ( -18.69999999999999929, 3.362550747017870378, 28.82623795144604983 ) ) ;
#168157 = LINE ( 'NONE', #71598, #68531 ) ;
#168158 = CARTESIAN_POINT ( 'NONE',  ( -20.00857864376270001, 9.250000000011157297, -54.65000000000000568 ) ) ;
#168159 = DIRECTION ( 'NONE',  ( -0.000000000000000000, 0.9651348961777161950, -0.2617529984165014589 ) ) ;
#168160 = EDGE_LOOP ( 'NONE', ( #126561, #67367, #255083, #93237 ) ) ;
#168161 = DIRECTION ( 'NONE',  ( 0.000000000000000000, 0.000000000000000000, -1.000000000000000000 ) ) ;
#168163 = AXIS2_PLACEMENT_3D ( 'NONE', #242812, #240269, #101993 ) ;
#168162 = CARTESIAN_POINT ( 'NONE',  ( 19.99999999999998934, 51.33926024308902925, -230.0993571250899379 ) ) ;
#168164 = DIRECTION ( 'NONE',  ( -0.000000000000000000, -0.000000000000000000, 1.000000000000000000 ) ) ;
#168166 = EDGE_CURVE ( 'NONE', #230635, #113629, #125802, .T. ) ;
#168165 = PLANE ( 'NONE',  #64315 ) ;
#168167 = ORIENTED_EDGE ( 'NONE', *, *, #140149, .F. ) ;
#168169 = FACE_OUTER_BOUND ( 'NONE', #216947, .T. ) ;
#168168 = CARTESIAN_POINT ( 'NONE',  ( 21.09813707148777340, 61.06062195154343897, -234.2140757814696883 ) ) ;
#168171 = ORIENTED_EDGE ( 'NONE', *, *, #123794, .T. ) ;
#168170 = AXIS2_PLACEMENT_3D ( 'NONE', #140397, #216085, #62166 ) ;
#168174 = ORIENTED_EDGE ( 'NONE', *, *, #115851, .T. ) ;
#168173 = CARTESIAN_POINT ( 'NONE',  ( -18.38817693311004575, 64.51850848411221762, -112.2731074845243739 ) ) ;
#168172 = DIRECTION ( 'NONE',  ( -1.000000000000000000, -0.000000000000000000, -0.000000000000000000 ) ) ;
#168175 = EDGE_LOOP ( 'NONE', ( #152398, #75905, #202731, #220158 ) ) ;
#168176 = LINE ( 'NONE', #164290, #114376 ) ;
#168177 = TOROIDAL_SURFACE ( 'NONE', #55650, 11.65000000000000036, 0.1000000000000000056 ) ;
#168179 = CARTESIAN_POINT ( 'NONE',  ( -1.739115166359751170E-14, 23.42819724844703089, -229.2476443247245186 ) ) ;
#168178 = AXIS2_PLACEMENT_3D ( 'NONE', #216254, #92463, #113318 ) ;
#168180 = DIRECTION ( 'NONE',  ( 0.000000000000000000, 0.000000000000000000, -1.000000000000000000 ) ) ;
#168181 = ORIENTED_EDGE ( 'NONE', *, *, #39920, .T. ) ;
#168182 = FACE_OUTER_BOUND ( 'NONE', #6124, .T. ) ;
#168183 = CARTESIAN_POINT ( 'NONE',  ( -18.59999999999999787, 9.150000000000002132, -21.15000000000000213 ) ) ;
#168184 = CARTESIAN_POINT ( 'NONE',  ( -18.59999999999999787, 1.148907358139439339E-11, -201.0000000000015064 ) ) ;
#168186 = EDGE_LOOP ( 'NONE', ( #45156, #68287, #52088, #12006 ) ) ;
#168185 = CARTESIAN_POINT ( 'NONE',  ( 20.94999999999999929, 11.63687328911539787, -93.67824078667517540 ) ) ;
#168187 = AXIS2_PLACEMENT_3D ( 'NONE', #36128, #17812, #191365 ) ;
#168188 = VECTOR ( 'NONE', #179749, 1000.000000000000114 ) ;
#168189 = TOROIDAL_SURFACE ( 'NONE', #168001, 4.100000000000000533, 0.1000000000000000056 ) ;
#168190 = ORIENTED_EDGE ( 'NONE', *, *, #142834, .T. ) ;
#168191 = CARTESIAN_POINT ( 'NONE',  ( 23.15000000000000213, -7.176961358819842651, -212.6889627706600834 ) ) ;
#168192 = DIRECTION ( 'NONE',  ( -1.000000000000000000, -0.000000000000000000, 0.000000000000000000 ) ) ;
#168193 = DIRECTION ( 'NONE',  ( 1.000000000000000000, 0.000000000000000000, 0.000000000000000000 ) ) ;
#168194 = VERTEX_POINT ( 'NONE', #126257 ) ;
#168195 = DIRECTION ( 'NONE',  ( 0.000000000000000000, -1.000000000000000000, -0.000000000000000000 ) ) ;
#168196 = VECTOR ( 'NONE', #203859, 1000.000000000000000 ) ;
#168197 = CARTESIAN_POINT ( 'NONE',  ( -18.59999999999999787, -1.162701749926853712, -75.00000000000004263 ) ) ;
#168198 = DIRECTION ( 'NONE',  ( 0.000000000000000000, 0.000000000000000000, 1.000000000000000000 ) ) ;
#168199 = VERTEX_POINT ( 'NONE', #165406 ) ;
#168200 = VECTOR ( 'NONE', #2529, 1000.000000000000000 ) ;
#168201 = AXIS2_PLACEMENT_3D ( 'NONE', #10624, #111003, #91447 ) ;
#168202 = AXIS2_PLACEMENT_3D ( 'NONE', #111922, #70243, #14108 ) ;
#168203 = EDGE_CURVE ( 'NONE', #250167, #202762, #63260, .T. ) ;
#168204 = ORIENTED_EDGE ( 'NONE', *, *, #3641, .F. ) ;
#168205 = CARTESIAN_POINT ( 'NONE',  ( -20.94999999999999929, 18.18127959618848877, -237.5711165786817389 ) ) ;
#168206 = CARTESIAN_POINT ( 'NONE',  ( -23.15000000000000213, 28.42524210734032053, -258.3567845160494585 ) ) ;
#168207 = ORIENTED_EDGE ( 'NONE', *, *, #77039, .F. ) ;
#168208 = ORIENTED_EDGE ( 'NONE', *, *, #193726, .F. ) ;
#168209 = ADVANCED_FACE ( 'NONE', ( #127555 ), #159173, .T. ) ;
#168210 = DIRECTION ( 'NONE',  ( 0.000000000000000000, 0.1335171055202867274, -0.9910465087640866200 ) ) ;
#168211 = ORIENTED_EDGE ( 'NONE', *, *, #245827, .T. ) ;
#168213 = ORIENTED_EDGE ( 'NONE', *, *, #181101, .T. ) ;
#168212 = CARTESIAN_POINT ( 'NONE',  ( 20.27550659511089037, 61.64772458173430181, -221.2338429919259966 ) ) ;
#168214 = EDGE_CURVE ( 'NONE', #167819, #15533, #7607, .T. ) ;
#168215 = ORIENTED_EDGE ( 'NONE', *, *, #125835, .T. ) ;
#168217 = ORIENTED_EDGE ( 'NONE', *, *, #93471, .F. ) ;
#168216 = ORIENTED_EDGE ( 'NONE', *, *, #250511, .T. ) ;
#168218 = CIRCLE ( 'NONE', #189024, 7.800000000000001599 ) ;
#168219 = AXIS2_PLACEMENT_3D ( 'NONE', #82753, #249263, #163625 ) ;
#168220 = DIRECTION ( 'NONE',  ( 0.000000000000000000, 0.000000000000000000, -1.000000000000000000 ) ) ;
#168222 = EDGE_CURVE ( 'NONE', #38945, #204755, #186255, .T. ) ;
#168221 = VERTEX_POINT ( 'NONE', #27205 ) ;
#168223 = PLANE ( 'NONE',  #177432 ) ;
#168224 = CIRCLE ( 'NONE', #230554, 1.749999999999998002 ) ;
#168225 = DIRECTION ( 'NONE',  ( -0.000000000000000000, -0.9651348961777157509, 0.2617529984165028467 ) ) ;
#168226 = CARTESIAN_POINT ( 'NONE',  ( -18.49999999999999645, 86.87898763699993765, -199.4031916457581985 ) ) ;
#168227 = ORIENTED_EDGE ( 'NONE', *, *, #92732, .T. ) ;
#168229 = ORIENTED_EDGE ( 'NONE', *, *, #53830, .F. ) ;
#168228 = CIRCLE ( 'NONE', #172339, 0.1000000000000004496 ) ;
#168230 = CARTESIAN_POINT ( 'NONE',  ( 23.14999999999999858, 17.01923898301590654, -224.3994341343041867 ) ) ;
#168231 = VECTOR ( 'NONE', #85781, 1000.000000000000000 ) ;
#168233 = VERTEX_POINT ( 'NONE', #87126 ) ;
#168232 = CARTESIAN_POINT ( 'NONE',  ( 18.52928932304084242, 63.76945704520649372, -209.3485784096579891 ) ) ;
#168234 = DIRECTION ( 'NONE',  ( -4.336808689942053235E-15, 0.9667078373770151556, 0.2558827019433999594 ) ) ;
#168236 = ORIENTED_EDGE ( 'NONE', *, *, #228184, .F. ) ;
#168235 = DIRECTION ( 'NONE',  ( 0.000000000000000000, -7.116814260417668513E-15, 1.000000000000000000 ) ) ;
#168237 = EDGE_CURVE ( 'NONE', #59716, #130077, #886, .T. ) ;
#168238 =( BOUNDED_SURFACE ( )  B_SPLINE_SURFACE ( 3, 2, ( 
 ( #108905, #188446, #89331 ),
 ( #37107, #119192, #16261 ),
 ( #253543, #98293, #74951 ),
 ( #175335, #138704, #236549 ),
 ( #154495, #232731, #235266 ),
 ( #57904, #153209, #114033 ),
 ( #78753, #197426, #54066 ),
 ( #254787, #174066, #214419 ),
 ( #233985, #116615, #196149 ),
 ( #194889, #134864, #157042 ) ),
 .UNSPECIFIED., .F., .F., .F. ) 
 B_SPLINE_SURFACE_WITH_KNOTS ( ( 4, 2, 2, 2, 4 ),
 ( 3, 3 ),
 ( 0.002161241639767248670, 0.002579950749615825267, 0.002789305304540113349, 0.002893982582002257390, 0.002998659859464401431 ),
 ( 0.000000000000000000, 1.000000000000000000 ),
 .UNSPECIFIED. ) 
 GEOMETRIC_REPRESENTATION_ITEM ( )  RATIONAL_B_SPLINE_SURFACE ( (
 ( 1.000000000000000000, 0.7071067811865536790, 1.000000000000000000),
 ( 1.000000000000000000, 0.7632447400664924553, 1.000000000000000000),
 ( 1.000000000000000000, 0.8158073005109215403, 1.000000000000000000),
 ( 1.000000000000000000, 0.8906973462396327035, 1.000000000000000000),
 ( 1.000000000000000000, 0.9149408947798607361, 1.000000000000000000),
 ( 1.000000000000000000, 0.9493368785276657951, 1.000000000000000000),
 ( 1.000000000000000000, 0.9605194247158186371, 1.000000000000000000),
 ( 1.000000000000000000, 0.9803630264779832348, 1.000000000000000000),
 ( 1.000000000000000000, 0.9900844824272205802, 1.000000000000000000),
 ( 1.000000000000000000, 0.9894588281429248511, 1.000000000000000000) ) ) 
 REPRESENTATION_ITEM ( '' )  SURFACE ( )  );
#168239 = ORIENTED_EDGE ( 'NONE', *, *, #129144, .T. ) ;
#168240 = CARTESIAN_POINT ( 'NONE',  ( 0.8999999999999993561, -11.65000000000000036, 28.60000000000000142 ) ) ;
#168241 = AXIS2_PLACEMENT_3D ( 'NONE', #102245, #219654, #594 ) ;
#168242 = AXIS2_PLACEMENT_3D ( 'NONE', #25835, #46652, #110490 ) ;
#168243 = VECTOR ( 'NONE', #101274, 1000.000000000000000 ) ;
#168244 = VERTEX_POINT ( 'NONE', #203236 ) ;
#168245 = CIRCLE ( 'NONE', #84960, 7.800000000000000711 ) ;
#168246 = DIRECTION ( 'NONE',  ( 1.000000000000000000, 0.000000000000000000, 0.000000000000000000 ) ) ;
#168247 = CARTESIAN_POINT ( 'NONE',  ( -21.64999999999999858, 12.51174298335651791, -211.2216088517780292 ) ) ;
#168248 = CIRCLE ( 'NONE', #89088, 0.09999999999998898659 ) ;
#168250 = ORIENTED_EDGE ( 'NONE', *, *, #217303, .T. ) ;
#168249 = EDGE_LOOP ( 'NONE', ( #230279, #193565, #36289, #199557 ) ) ;
#168251 = VERTEX_POINT ( 'NONE', #104115 ) ;
#168252 = CARTESIAN_POINT ( 'NONE',  ( -16.97683809663754317, 9.950000000011135270, -53.72847083211058106 ) ) ;
#168253 = ORIENTED_EDGE ( 'NONE', *, *, #114999, .F. ) ;
#168254 =( BOUNDED_SURFACE ( )  B_SPLINE_SURFACE ( 3, 2, ( 
 ( #32807, #232274, #212698 ),
 ( #95306, #174900, #135698 ),
 ( #255610, #14514, #130568 ),
 ( #191872, #151448, #94006 ),
 ( #194431, #230987, #52303 ),
 ( #17073, #133154, #75755 ),
 ( #155314, #96562, #233550 ),
 ( #156604, #73205, #234818 ),
 ( #91462, #56158, #92723 ),
 ( #215255, #131863, #213976 ) ),
 .UNSPECIFIED., .F., .F., .F. ) 
 B_SPLINE_SURFACE_WITH_KNOTS ( ( 4, 2, 2, 2, 4 ),
 ( 3, 3 ),
 ( 0.0001701955120502369480, 0.0002247052511886125372, 0.0002792149903269881264, 0.0003882344686037392505, 0.0006062734251572414988 ),
 ( 0.000000000000000000, 1.000000000000000000 ),
 .UNSPECIFIED. ) 
 GEOMETRIC_REPRESENTATION_ITEM ( )  RATIONAL_B_SPLINE_SURFACE ( (
 ( 1.000000000000000000, 0.2966190024560417804, 1.000000000000000000),
 ( 1.000000000000000000, 0.2964522492711926804, 1.000000000000000000),
 ( 1.000000000000000000, 0.3059923531883286807, 1.000000000000000000),
 ( 1.000000000000000000, 0.3355751146944992436, 1.000000000000000000),
 ( 1.000000000000000000, 0.3550672384964260742, 1.000000000000000000),
 ( 1.000000000000000000, 0.4157034672179444335, 1.000000000000000000),
 ( 1.000000000000000000, 0.4588031877653836466, 1.000000000000000000),
 ( 1.000000000000000000, 0.5771441759660936865, 1.000000000000000000),
 ( 1.000000000000000000, 0.6469377121771874295, 1.000000000000000000),
 ( 1.000000000000000000, 0.7071067811865376918, 1.000000000000000000) ) ) 
 REPRESENTATION_ITEM ( '' )  SURFACE ( )  );
#168255 = ORIENTED_EDGE ( 'NONE', *, *, #240476, .F. ) ;
#168256 = CARTESIAN_POINT ( 'NONE',  ( 20.94999999999999929, -11.64999999999999147, -33.49999999999998579 ) ) ;
#168258 = ORIENTED_EDGE ( 'NONE', *, *, #1790, .F. ) ;
#168257 = CARTESIAN_POINT ( 'NONE',  ( -18.59999999999999787, 67.23127455305835554, -235.8551265064784559 ) ) ;
#168259 = DIRECTION ( 'NONE',  ( 0.000000000000000000, -1.000000000000000000, -6.982962677686266711E-15 ) ) ;
#168260 = AXIS2_PLACEMENT_3D ( 'NONE', #183723, #119922, #179879 ) ;
#168262 = CARTESIAN_POINT ( 'NONE',  ( 20.94999999999999929, 77.36242903720516040, -95.13422623660308375 ) ) ;
#168261 = CARTESIAN_POINT ( 'NONE',  ( -23.15000000000000213, 1.115649653272650466E-11, -138.0000000000000284 ) ) ;
#168263 = DIRECTION ( 'NONE',  ( -1.000000000000000000, -2.671448610905051031E-14, -6.406987848362951272E-14 ) ) ;
#168264 = DIRECTION ( 'NONE',  ( 0.000000000000000000, 0.2716869542551192951, -0.9623856809447951521 ) ) ;
#168265 = ORIENTED_EDGE ( 'NONE', *, *, #252186, .F. ) ;
#168266 = ORIENTED_EDGE ( 'NONE', *, *, #96685, .F. ) ;
#168267 = CIRCLE ( 'NONE', #238970, 0.09999999999999939493 ) ;
#168268 = CARTESIAN_POINT ( 'NONE',  ( 19.90000000000000568, 5.488301202077012775, 16.50000000000000000 ) ) ;
#168269 = DIRECTION ( 'NONE',  ( -1.000000000000000000, 2.952720810173289112E-16, 2.061873921506763405E-30 ) ) ;
#168270 = ORIENTED_EDGE ( 'NONE', *, *, #232612, .T. ) ;
#168271 = VECTOR ( 'NONE', #30632, 1000.000000000000000 ) ;
#168272 =( BOUNDED_SURFACE ( )  B_SPLINE_SURFACE ( 3, 2, ( 
 ( #156290, #136675, #23184 ),
 ( #243483, #122265, #124836 ),
 ( #44003, #105211, #45291 ),
 ( #244757, #40187, #6144 ) ),
 .UNSPECIFIED., .F., .F., .T. ) 
 B_SPLINE_SURFACE_WITH_KNOTS ( ( 4, 4 ),
 ( 3, 3 ),
 ( -8.673617379884035472E-18, 0.001979672783031562362 ),
 ( 0.000000000000000000, 1.000000000000000000 ),
 .UNSPECIFIED. ) 
 GEOMETRIC_REPRESENTATION_ITEM ( )  RATIONAL_B_SPLINE_SURFACE ( (
 ( 1.000000000000000000, 0.7103081912007771503, 1.000000000000000000),
 ( 1.000000000000000000, 0.7104998333560409440, 1.000000000000000000),
 ( 1.000000000000000000, 0.7107238315753027225, 1.000000000000000000),
 ( 1.000000000000000000, 0.7110073749539924659, 1.000000000000000000) ) ) 
 REPRESENTATION_ITEM ( '' )  SURFACE ( )  );
#168273 = CIRCLE ( 'NONE', #105656, 12.87499999999999822 ) ;
#168274 = EDGE_CURVE ( 'NONE', #55246, #237061, #166713, .T. ) ;
#168275 = VECTOR ( 'NONE', #141403, 1000.000000000000000 ) ;
#168276 = CARTESIAN_POINT ( 'NONE',  ( 18.59999999999999076, 70.15623657602074559, -198.0563205710787713 ) ) ;
#168277 = VERTEX_POINT ( 'NONE', #67576 ) ;
#168278 = ORIENTED_EDGE ( 'NONE', *, *, #184921, .T. ) ;
#168279 = DIRECTION ( 'NONE',  ( 0.000000000000000000, 0.000000000000000000, -1.000000000000000000 ) ) ;
#168280 = CYLINDRICAL_SURFACE ( 'NONE', #94070, 0.1000000000000124678 ) ;
#168281 = ORIENTED_EDGE ( 'NONE', *, *, #134483, .F. ) ;
#168282 = CARTESIAN_POINT ( 'NONE',  ( -20.94999999999999574, 11.75000000001115552, -107.3416006898971631 ) ) ;
#168283 = CARTESIAN_POINT ( 'NONE',  ( 21.05000000000000071, 8.776282895303632259, -112.6500000000000341 ) ) ;
#168284 = ORIENTED_EDGE ( 'NONE', *, *, #169667, .T. ) ;
#168285 = DIRECTION ( 'NONE',  ( 0.000000000000000000, 0.8660254037844420383, -0.4999999999999943379 ) ) ;
#168287 = EDGE_CURVE ( 'NONE', #98189, #17866, #104923, .T. ) ;
#168286 = DIRECTION ( 'NONE',  ( 1.000000000000000000, 0.000000000000000000, 0.000000000000000000 ) ) ;
#168289 = CARTESIAN_POINT ( 'NONE',  ( 20.94999999999999574, 76.00000000001195133, -103.0231074845243171 ) ) ;
#168288 = CYLINDRICAL_SURFACE ( 'NONE', #169660, 0.1000000000000055844 ) ;
#168290 = B_SPLINE_CURVE_WITH_KNOTS ( 'NONE', 3,
 ( #238351, #41466, #235781, #178416, #177131, #195410, #174598, #36329, #79259, #157586 ),
 .UNSPECIFIED., .F., .F.,
 ( 4, 3, 3, 4 ),
 ( 0.000000000000000000, 0.0002000000000002785953, 0.001000000000045107602, 0.001967863649472123035 ),
 .UNSPECIFIED. ) ;
#168291 = FACE_OUTER_BOUND ( 'NONE', #182632, .T. ) ;
#168292 = DIRECTION ( 'NONE',  ( -1.000000000000000000, -0.000000000000000000, -0.000000000000000000 ) ) ;
#168293 = DIRECTION ( 'NONE',  ( 0.000000000000000000, 0.2617529984165031243, 0.9651348961777157509 ) ) ;
#168294 = EDGE_CURVE ( 'NONE', #210105, #209133, #192453, .T. ) ;
#168296 = VERTEX_POINT ( 'NONE', #48006 ) ;
#168295 = AXIS2_PLACEMENT_3D ( 'NONE', #185746, #86613, #7095 ) ;
#168297 = AXIS2_PLACEMENT_3D ( 'NONE', #84322, #243450, #62254 ) ;
#168298 = CIRCLE ( 'NONE', #114059, 0.1999999999999987899 ) ;
#168300 = ORIENTED_EDGE ( 'NONE', *, *, #168839, .T. ) ;
#168299 = EDGE_LOOP ( 'NONE', ( #20315, #86616, #248399, #54965 ) ) ;
#168301 = EDGE_LOOP ( 'NONE', ( #149467, #175893, #213640, #69364 ) ) ;
#168302 = DIRECTION ( 'NONE',  ( 1.000000000000000000, -0.000000000000000000, -0.000000000000000000 ) ) ;
#168303 = EDGE_CURVE ( 'NONE', #164247, #250604, #169288, .T. ) ;
#168304 = DIRECTION ( 'NONE',  ( 0.000000000000000000, 0.000000000000000000, -1.000000000000000000 ) ) ;
#168306 = CARTESIAN_POINT ( 'NONE',  ( 23.14999999999999858, 6.650000000011155876, -79.35000000000005116 ) ) ;
#168305 = CYLINDRICAL_SURFACE ( 'NONE', #178546, 0.1000000000000000472 ) ;
#168307 = LINE ( 'NONE', #89993, #28835 ) ;
#168308 = ORIENTED_EDGE ( 'NONE', *, *, #234533, .F. ) ;
#168309 = EDGE_CURVE ( 'NONE', #121066, #216063, #180007, .T. ) ;
#168310 = DIRECTION ( 'NONE',  ( 2.952720810173289112E-16, -1.000000000000000000, -0.000000000000000000 ) ) ;
#168311 = EDGE_CURVE ( 'NONE', #158502, #103462, #213282, .T. ) ;
#168312 = EDGE_LOOP ( 'NONE', ( #34734, #140906, #6186, #225436, #6415, #59507 ) ) ;
#168313 = CARTESIAN_POINT ( 'NONE',  ( -20.54999999999999716, 7.150000000011155876, -88.15000000000004832 ) ) ;
#168314 = DIRECTION ( 'NONE',  ( -1.000000000000000000, -0.000000000000000000, -0.000000000000000000 ) ) ;
#168315 = SPHERICAL_SURFACE ( 'NONE', #133243, 0.1000000000000000056 ) ;
#168316 = ORIENTED_EDGE ( 'NONE', *, *, #106491, .F. ) ;
#168317 = DIRECTION ( 'NONE',  ( 0.000000000000000000, 0.000000000000000000, -1.000000000000000000 ) ) ;
#168318 = ADVANCED_FACE ( 'NONE', ( #247501 ), #148409, .T. ) ;
#168319 = AXIS2_PLACEMENT_3D ( 'NONE', #120015, #222917, #83386 ) ;
#168320 = DIRECTION ( 'NONE',  ( 0.000000000000000000, 0.000000000000000000, 1.000000000000000000 ) ) ;
#168321 = ORIENTED_EDGE ( 'NONE', *, *, #99129, .T. ) ;
#168322 = ORIENTED_EDGE ( 'NONE', *, *, #106647, .F. ) ;
#168323 = CARTESIAN_POINT ( 'NONE',  ( -16.89081410710458542, 9.951318529858268036, -54.35440591983636693 ) ) ;
#168324 = DIRECTION ( 'NONE',  ( -1.000000000000000000, 0.000000000000000000, 0.000000000000000000 ) ) ;
#168325 = LINE ( 'NONE', #232119, #119598 ) ;
#168326 = EDGE_CURVE ( 'NONE', #16903, #87211, #85820, .T. ) ;
#168327 = DIRECTION ( 'NONE',  ( -1.000000000000000000, -0.000000000000000000, -0.000000000000000000 ) ) ;
#168328 = CARTESIAN_POINT ( 'NONE',  ( 20.94999999999999929, -8.999999999988842703, -124.1060308773475924 ) ) ;
#168329 = EDGE_CURVE ( 'NONE', #3474, #140520, #229873, .T. ) ;
#168330 = CARTESIAN_POINT ( 'NONE',  ( -21.14999999999999858, 11.65000000001115588, -67.10000000000005116 ) ) ;
#168331 = ORIENTED_EDGE ( 'NONE', *, *, #56372, .F. ) ;
#168332 = FACE_OUTER_BOUND ( 'NONE', #150853, .T. ) ;
#168333 = CARTESIAN_POINT ( 'NONE',  ( -20.94999999999999929, 14.05000000000000071, -5.513695070760990191 ) ) ;
#168335 = CYLINDRICAL_SURFACE ( 'NONE', #137176, 0.1999999999999987899 ) ;
#168334 = DIRECTION ( 'NONE',  ( 1.000000000000000000, 0.000000000000000000, -0.000000000000000000 ) ) ;
#168336 = CARTESIAN_POINT ( 'NONE',  ( -16.94107738177415712, 65.98576071487495653, -56.97310748452439810 ) ) ;
#168337 = DIRECTION ( 'NONE',  ( 1.000000000000000000, -7.304098846218134667E-16, -5.100424963727256530E-30 ) ) ;
#168338 = FACE_OUTER_BOUND ( 'NONE', #8573, .T. ) ;
#168339 = DIRECTION ( 'NONE',  ( -1.073024830501117725E-15, 6.982962677686266711E-15, -1.000000000000000000 ) ) ;
#168340 = VECTOR ( 'NONE', #103027, 1000.000000000000227 ) ;
#168342 = ORIENTED_EDGE ( 'NONE', *, *, #19807, .F. ) ;
#168341 = DIRECTION ( 'NONE',  ( 0.000000000000000000, 0.000000000000000000, -1.000000000000000000 ) ) ;
#168343 = AXIS2_PLACEMENT_3D ( 'NONE', #38827, #120950, #62233 ) ;
#168344 = AXIS2_PLACEMENT_3D ( 'NONE', #234658, #53457, #175994 ) ;
#168345 = AXIS2_PLACEMENT_3D ( 'NONE', #28453, #68837, #85774 ) ;
#168346 = EDGE_CURVE ( 'NONE', #36747, #179090, #88374, .T. ) ;
#168347 = ADVANCED_FACE ( 'NONE', ( #222783 ), #155071, .F. ) ;
#168348 = B_SPLINE_CURVE_WITH_KNOTS ( 'NONE', 3,
 ( #247616, #65121, #225462, #148524, #222906, #203361, #228059, #29883 ),
 .UNSPECIFIED., .F., .F.,
 ( 4, 2, 2, 4 ),
 ( 0.000000000000000000, 0.0001049670497869897433, 0.0002099340995739794867, 0.0004198681991479769711 ),
 .UNSPECIFIED. ) ;
#168349 = EDGE_CURVE ( 'NONE', #204714, #95921, #100824, .T. ) ;
#168351 = FACE_OUTER_BOUND ( 'NONE', #107490, .T. ) ;
#168350 = VECTOR ( 'NONE', #11935, 1000.000000000000000 ) ;
#168352 = DIRECTION ( 'NONE',  ( -0.8049926720990042694, 0.5932847527679310229, 4.142885285818786163E-15 ) ) ;
#168353 = ORIENTED_EDGE ( 'NONE', *, *, #42886, .T. ) ;
#168354 = VECTOR ( 'NONE', #157448, 999.9999999999998863 ) ;
#168355 = DIRECTION ( 'NONE',  ( 1.000000000000000000, -2.952720810173289112E-16, -2.061873921506763405E-30 ) ) ;
#168356 = AXIS2_PLACEMENT_3D ( 'NONE', #232929, #252447, #128680 ) ;
#168357 = DIRECTION ( 'NONE',  ( -0.8191520442889921316, 0.5735764363510457153, -0.000000000000000000 ) ) ;
#168358 = DIRECTION ( 'NONE',  ( 1.000000000000000000, 0.000000000000000000, 0.000000000000000000 ) ) ;
#168359 = AXIS2_PLACEMENT_3D ( 'NONE', #37342, #191295, #252502 ) ;
#168360 = AXIS2_PLACEMENT_3D ( 'NONE', #236337, #29510, #215488 ) ;
#168361 = ORIENTED_EDGE ( 'NONE', *, *, #40894, .F. ) ;
#168362 = DIRECTION ( 'NONE',  ( -4.391705002472927119E-16, -1.000000000000000000, -7.026728003956683390E-15 ) ) ;
#168363 = EDGE_LOOP ( 'NONE', ( #102508, #64618, #184430, #236980 ) ) ;
#168364 = DIRECTION ( 'NONE',  ( 0.000000000000000000, 9.769962616701369667E-15, 1.000000000000000000 ) ) ;
#168365 = DIRECTION ( 'NONE',  ( 0.000000000000000000, 0.4930308989875575865, 0.8700118002898125091 ) ) ;
#168366 = ORIENTED_EDGE ( 'NONE', *, *, #12349, .F. ) ;
#168367 = CARTESIAN_POINT ( 'NONE',  ( -21.05000000000000071, -0.09999999998884338825, -55.35000000000004405 ) ) ;
#168368 = TOROIDAL_SURFACE ( 'NONE', #105746, 0.2000000000000000111, 0.1000000000000000056 ) ;
#168369 = ADVANCED_FACE ( 'NONE', ( #31059 ), #135236, .F. ) ;
#168370 = APPLICATION_PROTOCOL_DEFINITION ( 'draft international standard', 'automotive_design', 1998, #232514 ) ;
#168372 = DIRECTION ( 'NONE',  ( -0.000000000000000000, 0.9876197685951279004, -0.1568667991644694115 ) ) ;
#168371 = AXIS2_PLACEMENT_3D ( 'NONE', #80152, #138841, #625 ) ;
#168374 = AXIS2_PLACEMENT_3D ( 'NONE', #246639, #227075, #47137 ) ;
#168373 = DIRECTION ( 'NONE',  ( 1.000000000000000000, 0.000000000000000000, 0.000000000000000000 ) ) ;
#168375 = FACE_OUTER_BOUND ( 'NONE', #185170, .T. ) ;
#168376 = ORIENTED_EDGE ( 'NONE', *, *, #182057, .F. ) ;
#168378 = EDGE_CURVE ( 'NONE', #140417, #63155, #92488, .T. ) ;
#168377 = DIRECTION ( 'NONE',  ( 0.000000000000000000, 0.000000000000000000, 1.000000000000000000 ) ) ;
#168379 = DIRECTION ( 'NONE',  ( -1.000000000000000000, 0.000000000000000000, 0.000000000000000000 ) ) ;
#168380 = TOROIDAL_SURFACE ( 'NONE', #1717, 0.4000000000000012990, 0.1000000000000000056 ) ;
#168381 = EDGE_CURVE ( 'NONE', #140287, #112792, #15329, .T. ) ;
#168382 = VECTOR ( 'NONE', #51693, 1000.000000000000000 ) ;
#168383 = EDGE_CURVE ( 'NONE', #231688, #162715, #74582, .T. ) ;
#168384 = LINE ( 'NONE', #133066, #28565 ) ;
#168385 = ORIENTED_EDGE ( 'NONE', *, *, #222848, .T. ) ;
#168386 = VERTEX_POINT ( 'NONE', #72749 ) ;
#168387 = AXIS2_PLACEMENT_3D ( 'NONE', #67, #163026, #159182 ) ;
#168388 = EDGE_CURVE ( 'NONE', #216036, #61669, #150757, .T. ) ;
#168389 = DIRECTION ( 'NONE',  ( -1.000000000000000000, -0.000000000000000000, -0.000000000000000000 ) ) ;
#168390 = AXIS2_PLACEMENT_3D ( 'NONE', #245390, #105839, #181573 ) ;
#168391 = AXIS2_PLACEMENT_3D ( 'NONE', #123457, #163873, #166465 ) ;
#168392 = CARTESIAN_POINT ( 'NONE',  ( -20.64999999999999858, 52.99650480578122824, -234.2878581050858884 ) ) ;
#168393 = FACE_OUTER_BOUND ( 'NONE', #133894, .T. ) ;
#168394 = CARTESIAN_POINT ( 'NONE',  ( -14.00000000000000178, 9.850000000011133849, -83.75000000000004263 ) ) ;
#168395 = FACE_OUTER_BOUND ( 'NONE', #58439, .T. ) ;
#168397 = DIRECTION ( 'NONE',  ( -1.000000000000000000, 0.000000000000000000, 0.000000000000000000 ) ) ;
#168396 = CARTESIAN_POINT ( 'NONE',  ( -21.14999999999994174, 76.00000000001119815, -36.02310748452479316 ) ) ;
#168398 = DIRECTION ( 'NONE',  ( 0.1538461538461468048, 0.9654630569144685426, 0.2102675597426226228 ) ) ;
#168399 = CARTESIAN_POINT ( 'NONE',  ( -17.73285935859749074, 65.14201819621466427, -113.2645456747330002 ) ) ;
#168400 = DIRECTION ( 'NONE',  ( 0.000000000000000000, 0.000000000000000000, 1.000000000000000000 ) ) ;
#168401 = ADVANCED_FACE ( 'NONE', ( #192672 ), #138272, .F. ) ;
#168403 = VERTEX_POINT ( 'NONE', #174435 ) ;
#168402 = CARTESIAN_POINT ( 'NONE',  ( -20.85000000000000142, 77.16412189325305349, -95.10825939895268277 ) ) ;
#168404 = CARTESIAN_POINT ( 'NONE',  ( 21.07971444708685738, 69.67020791838582738, -170.1109309208423213 ) ) ;
#168405 = EDGE_CURVE ( 'NONE', #32735, #183554, #220940, .T. ) ;
#168406 = CARTESIAN_POINT ( 'NONE',  ( -21.12757541349819590, -1.372498826969863917, -194.6737902636474757 ) ) ;
#168408 = CARTESIAN_POINT ( 'NONE',  ( 21.05000000000000071, 85.00000000001149658, -45.51707660717670478 ) ) ;
#168407 = DIRECTION ( 'NONE',  ( 0.000000000000000000, -0.2617529984165031243, -0.9651348961777158619 ) ) ;
#168409 = VERTEX_POINT ( 'NONE', #93556 ) ;
#168410 = DIRECTION ( 'NONE',  ( 0.000000000000000000, 0.000000000000000000, -1.000000000000000000 ) ) ;
#168412 = EDGE_CURVE ( 'NONE', #93031, #160519, #129893, .T. ) ;
#168411 = DIRECTION ( 'NONE',  ( 0.000000000000000000, 0.000000000000000000, -1.000000000000000000 ) ) ;
#168413 = DIRECTION ( 'NONE',  ( 0.000000000000000000, 0.2128009952263604232, -0.9770955615653316162 ) ) ;
#168414 = CARTESIAN_POINT ( 'NONE',  ( -21.07954640115405809, 69.67071230398704529, -103.0891151916641775 ) ) ;
#168415 = CARTESIAN_POINT ( 'NONE',  ( -21.45000000000000284, 68.29142135624881860, -48.37310748452437537 ) ) ;
#168416 = ORIENTED_EDGE ( 'NONE', *, *, #32335, .F. ) ;
#168417 = ORIENTED_EDGE ( 'NONE', *, *, #165643, .F. ) ;
#168418 = AXIS2_PLACEMENT_3D ( 'NONE', #9312, #129268, #250482 ) ;
#168419 = VECTOR ( 'NONE', #178745, 1000.000000000000114 ) ;
#168420 = DIRECTION ( 'NONE',  ( -0.000000000000000000, -0.9126074666063769270, -0.4088369013363283844 ) ) ;
#168421 = VERTEX_POINT ( 'NONE', #233098 ) ;
#168422 = CARTESIAN_POINT ( 'NONE',  ( 23.24999999999999289, 31.44980407958351876, -233.5445995079518582 ) ) ;
#168423 = AXIS2_PLACEMENT_3D ( 'NONE', #162638, #21839, #100053 ) ;
#168424 = EDGE_CURVE ( 'NONE', #200329, #87867, #25878, .T. ) ;
#168425 = ORIENTED_EDGE ( 'NONE', *, *, #221028, .T. ) ;
#168426 = CARTESIAN_POINT ( 'NONE',  ( 21.05000000000000426, 10.72371710471866812, -141.5944173916130921 ) ) ;
#168427 = CARTESIAN_POINT ( 'NONE',  ( -16.87036670365549895, 66.01058118071041747, -124.0026676018264169 ) ) ;
#168428 = AXIS2_PLACEMENT_3D ( 'NONE', #48, #114869, #37926 ) ;
#168429 = ADVANCED_FACE ( 'NONE', ( #54427 ), #133958, .F. ) ;
#168430 = VECTOR ( 'NONE', #242013, 1000.000000000000000 ) ;
#168431 = DIRECTION ( 'NONE',  ( 0.000000000000000000, -0.1480365673253065117, 0.9889818879709273425 ) ) ;
#168432 = ORIENTED_EDGE ( 'NONE', *, *, #206338, .T. ) ;
#168433 = EDGE_CURVE ( 'NONE', #21500, #96681, #50775, .T. ) ;
#168434 = VECTOR ( 'NONE', #99687, 1000.000000000000227 ) ;
#168435 = DIRECTION ( 'NONE',  ( -1.000000000000000000, 0.000000000000000000, -0.000000000000000000 ) ) ;
#168436 = EDGE_CURVE ( 'NONE', #62638, #225193, #171639, .T. ) ;
#168437 = CARTESIAN_POINT ( 'NONE',  ( 19.97071067811864609, 11.72071067811865674, -24.65000000000000213 ) ) ;
#168438 = DIRECTION ( 'NONE',  ( 0.000000000000000000, -1.000000000000000000, -6.982962677686266711E-15 ) ) ;
#168440 = AXIS2_PLACEMENT_3D ( 'NONE', #144276, #223824, #45204 ) ;
#168439 = DIRECTION ( 'NONE',  ( -0.000000000000000000, 1.000000000000000000, -0.000000000000000000 ) ) ;
#168441 = DIRECTION ( 'NONE',  ( -1.000000000000000000, -0.000000000000000000, -0.000000000000000000 ) ) ;
#168442 = VECTOR ( 'NONE', #89335, 1000.000000000000000 ) ;
#168443 = CARTESIAN_POINT ( 'NONE',  ( -21.05000000000000071, 14.05000000001115623, -72.51369507076104526 ) ) ;
#168444 = ORIENTED_EDGE ( 'NONE', *, *, #34428, .F. ) ;
#168446 = DIRECTION ( 'NONE',  ( 0.000000000000000000, 0.000000000000000000, -1.000000000000000000 ) ) ;
#168445 = CARTESIAN_POINT ( 'NONE',  ( 20.94999999999999929, 63.48958393997221350, -237.5313578019574265 ) ) ;
#168447 = ORIENTED_EDGE ( 'NONE', *, *, #172877, .T. ) ;
#168449 = ORIENTED_EDGE ( 'NONE', *, *, #114229, .F. ) ;
#168448 = CARTESIAN_POINT ( 'NONE',  ( -21.65000000000000213, 62.65526179112262639, -225.0299194783148948 ) ) ;
#168450 = CIRCLE ( 'NONE', #34562, 0.1000000000000028644 ) ;
#168451 = EDGE_LOOP ( 'NONE', ( #79578, #153120, #38291, #188099, #172964 ) ) ;
#168452 = DIRECTION ( 'NONE',  ( 1.000000000000000000, 0.000000000000000000, 0.000000000000000000 ) ) ;
#168453 = CARTESIAN_POINT ( 'NONE',  ( 14.45963434102923806, 66.54845833862673032, -151.5692319856938468 ) ) ;
#168454 = CARTESIAN_POINT ( 'NONE',  ( -20.54999999999999716, 74.05981308412474107, -190.6939882734710636 ) ) ;
#168455 = DIRECTION ( 'NONE',  ( 0.000000000000000000, 0.000000000000000000, -1.000000000000000000 ) ) ;
#168456 = VERTEX_POINT ( 'NONE', #50555 ) ;
#168457 = EDGE_CURVE ( 'NONE', #203424, #123298, #113345, .T. ) ;
#168458 = DIRECTION ( 'NONE',  ( 1.000000000000000000, -3.265361837132813093E-16, -2.280189983783949500E-30 ) ) ;
#168460 = CARTESIAN_POINT ( 'NONE',  ( 18.49999999999999289, 10.49142135624846439, -158.8500000000000227 ) ) ;
#168459 = VECTOR ( 'NONE', #136214, 1000.000000000000000 ) ;
#168461 = VERTEX_POINT ( 'NONE', #42566 ) ;
#168462 = DIRECTION ( 'NONE',  ( -0.000000000000000000, 1.000000000000000000, 0.000000000000000000 ) ) ;
#168463 = EDGE_CURVE ( 'NONE', #105422, #255259, #221827, .T. ) ;
#168464 = TOROIDAL_SURFACE ( 'NONE', #230782, 0.2000000000000000111, 0.1000000000000000056 ) ;
#168465 = CARTESIAN_POINT ( 'NONE',  ( 21.05000000000000071, 1.115623935689868526E-11, -98.60000000000005116 ) ) ;
#168466 = ORIENTED_EDGE ( 'NONE', *, *, #167212, .F. ) ;
#168467 = CARTESIAN_POINT ( 'NONE',  ( 18.39999999999999503, 23.69729366125098835, -229.5924034189314682 ) ) ;
#168468 = CIRCLE ( 'NONE', #197613, 0.1000000000000026007 ) ;
#168469 = AXIS2_PLACEMENT_3D ( 'NONE', #94064, #236154, #172381 ) ;
#168470 = ORIENTED_EDGE ( 'NONE', *, *, #167381, .F. ) ;
#168471 = CARTESIAN_POINT ( 'NONE',  ( 18.53317502108576775, 65.67736539654941907, -97.46251168765718376 ) ) ;
#168472 = ORIENTED_EDGE ( 'NONE', *, *, #133462, .F. ) ;
#168473 = DIRECTION ( 'NONE',  ( 1.000000000000000000, 0.000000000000000000, 0.000000000000000000 ) ) ;
#168474 = EDGE_CURVE ( 'NONE', #218583, #103201, #42794, .T. ) ;
#168475 = CARTESIAN_POINT ( 'NONE',  ( -22.47007471830798409, 7.543872110139036025, -199.3570250894167941 ) ) ;
#168476 = DIRECTION ( 'NONE',  ( 1.000000000000000000, 0.000000000000000000, 0.000000000000000000 ) ) ;
#168478 = EDGE_CURVE ( 'NONE', #68170, #144016, #242527, .T. ) ;
#168477 = LINE ( 'NONE', #207569, #34952 ) ;
#168479 = ORIENTED_EDGE ( 'NONE', *, *, #176462, .F. ) ;
#168480 = AXIS2_PLACEMENT_3D ( 'NONE', #234939, #195832, #58831 ) ;
#168481 = DIRECTION ( 'NONE',  ( 0.000000000000000000, 0.000000000000000000, -1.000000000000000000 ) ) ;
#168482 = ORIENTED_EDGE ( 'NONE', *, *, #14862, .T. ) ;
#168484 = DIRECTION ( 'NONE',  ( 0.000000000000000000, -0.8660254037844377084, -0.5000000000000016653 ) ) ;
#168483 = CARTESIAN_POINT ( 'NONE',  ( -21.07954640115405809, 69.67071230398747161, -170.0891151916640922 ) ) ;
#168485 = ORIENTED_EDGE ( 'NONE', *, *, #254286, .F. ) ;
#168486 = CARTESIAN_POINT ( 'NONE',  ( -14.00000000000000178, 9.849999999999978328, -16.75000000000000355 ) ) ;
#168487 = CARTESIAN_POINT ( 'NONE',  ( -20.64999999999999858, 48.91146289617405785, -253.9240286733484595 ) ) ;
#168488 = CARTESIAN_POINT ( 'NONE',  ( 20.95203847575071521, 59.07703819446410876, -225.8031978033470182 ) ) ;
#168489 = VECTOR ( 'NONE', #132093, 1000.000000000000000 ) ;
#168490 = EDGE_LOOP ( 'NONE', ( #115503, #192321, #256078 ) ) ;
#168492 = ORIENTED_EDGE ( 'NONE', *, *, #255519, .T. ) ;
#168491 = FACE_OUTER_BOUND ( 'NONE', #250979, .T. ) ;
#168493 = CARTESIAN_POINT ( 'NONE',  ( -18.59999999999999787, 7.654382455240002159, -241.6162809886059790 ) ) ;
#168495 = CARTESIAN_POINT ( 'NONE',  ( 21.05000000000000071, 70.60134440767089359, -223.4290147181903023 ) ) ;
#168494 = DIRECTION ( 'NONE',  ( -0.000000000000000000, 0.1350103645451876666, 0.9908441862701600211 ) ) ;
#168497 = EDGE_LOOP ( 'NONE', ( #10247, #224123, #228927, #10387 ) ) ;
#168496 = LINE ( 'NONE', #111039, #115331 ) ;
#168498 = VERTEX_POINT ( 'NONE', #136515 ) ;
#168499 = CARTESIAN_POINT ( 'NONE',  ( 23.24999999999999289, 5.950000000011163692, -56.69429769496518645 ) ) ;
#168500 = COLOUR_RGB ( '', 0.66274510, 0.83137255, 0.94901961) ;
#168501 = CARTESIAN_POINT ( 'NONE',  ( 22.47071067811865319, 1.115600667400684642E-11, -100.5000000000000284 ) ) ;
#168502 = VERTEX_POINT ( 'NONE', #239498 ) ;
#168503 = DIRECTION ( 'NONE',  ( 1.000000000000000000, -0.000000000000000000, -0.000000000000000000 ) ) ;
#168504 = ORIENTED_EDGE ( 'NONE', *, *, #207996, .T. ) ;
#168505 = LINE ( 'NONE', #185455, #186704 ) ;
#168506 = DIRECTION ( 'NONE',  ( 0.000000000000000000, -6.467318590049456648E-15, 1.000000000000000000 ) ) ;
#168507 = ORIENTED_EDGE ( 'NONE', *, *, #248886, .F. ) ;
#168508 = CARTESIAN_POINT ( 'NONE',  ( 23.14999999999999503, 11.75000000001116263, -188.8499999999999659 ) ) ;
#168509 = EDGE_CURVE ( 'NONE', #28335, #247013, #46880, .T. ) ;
#168510 = ORIENTED_EDGE ( 'NONE', *, *, #163419, .F. ) ;
#168511 = AXIS2_PLACEMENT_3D ( 'NONE', #31254, #187736, #7807 ) ;
#168512 = LINE ( 'NONE', #191912, #102068 ) ;
#168513 = VECTOR ( 'NONE', #153366, 1000.000000000000000 ) ;
#168514 = VECTOR ( 'NONE', #247495, 1000.000000000000000 ) ;
#168515 = AXIS2_PLACEMENT_3D ( 'NONE', #210431, #232576, #150459 ) ;
#168516 = EDGE_LOOP ( 'NONE', ( #54051, #14322, #87047, #162316 ) ) ;
#168517 = ORIENTED_EDGE ( 'NONE', *, *, #217126, .F. ) ;
#168518 = CARTESIAN_POINT ( 'NONE',  ( -21.05000000000000071, 61.06362902394928938, -234.0937223954992987 ) ) ;
#168519 = ORIENTED_EDGE ( 'NONE', *, *, #131049, .F. ) ;
#168520 =( GEOMETRIC_REPRESENTATION_CONTEXT ( 3 ) GLOBAL_UNCERTAINTY_ASSIGNED_CONTEXT ( ( #29565 ) ) GLOBAL_UNIT_ASSIGNED_CONTEXT ( ( #3045, #102129, #137422 ) ) REPRESENTATION_CONTEXT ( 'NONE', 'WORKASPACE' ) );
#168521 = EDGE_CURVE ( 'NONE', #60194, #123645, #77832, .T. ) ;
#168522 = CARTESIAN_POINT ( 'NONE',  ( 20.94999999999999574, 74.83729825007360148, -61.52310748452433131 ) ) ;
#168523 = VERTEX_POINT ( 'NONE', #102507 ) ;
#168525 = ORIENTED_EDGE ( 'NONE', *, *, #155855, .F. ) ;
#168524 = DIRECTION ( 'NONE',  ( 0.000000000000000000, -0.8068669527896844551, -0.5907332058517525963 ) ) ;
#168527 = ADVANCED_FACE ( 'NONE', ( #216061 ), #34454, .F. ) ;
#168526 = CARTESIAN_POINT ( 'NONE',  ( -20.94999999999999929, 1.835341550235569663, -45.05515129256298223 ) ) ;
#168528 = VERTEX_POINT ( 'NONE', #182091 ) ;
#168529 = DIRECTION ( 'NONE',  ( -1.000000000000000000, 0.000000000000000000, 0.000000000000000000 ) ) ;
#168530 = ORIENTED_EDGE ( 'NONE', *, *, #227717, .T. ) ;
#168533 = EDGE_LOOP ( 'NONE', ( #88011, #150898, #114924, #176160 ) ) ;
#168532 = VERTEX_POINT ( 'NONE', #41318 ) ;
#168531 = CARTESIAN_POINT ( 'NONE',  ( -20.64999999999999858, 53.03738849591485405, -234.3791188517465400 ) ) ;
#168535 = DIRECTION ( 'NONE',  ( 0.000000000000000000, -6.982962677686266711E-15, 1.000000000000000000 ) ) ;
#168534 = AXIS2_PLACEMENT_3D ( 'NONE', #89841, #130254, #11620 ) ;
#168536 = LINE ( 'NONE', #32873, #2482 ) ;
#168538 = EDGE_CURVE ( 'NONE', #30421, #214314, #192646, .T. ) ;
#168537 = ORIENTED_EDGE ( 'NONE', *, *, #34547, .F. ) ;
#168539 = TOROIDAL_SURFACE ( 'NONE', #235130, 0.9750000000000019762, 0.1000000000000000056 ) ;
#168540 = AXIS2_PLACEMENT_3D ( 'NONE', #227131, #207599, #9366 ) ;
#168541 = CIRCLE ( 'NONE', #164406, 0.09999999999999520384 ) ;
#168542 = EDGE_CURVE ( 'NONE', #230044, #46173, #238190, .T. ) ;
#168543 = CIRCLE ( 'NONE', #101827, 12.87500000000000178 ) ;
#168544 = EDGE_CURVE ( 'NONE', #13761, #197779, #116977, .T. ) ;
#168545 = ORIENTED_EDGE ( 'NONE', *, *, #41796, .T. ) ;
#168546 = CARTESIAN_POINT ( 'NONE',  ( 21.05000000000000071, 69.35000000001156195, -57.37310748452436826 ) ) ;
#168547 = DIRECTION ( 'NONE',  ( 1.000000000000000000, 0.000000000000000000, 0.000000000000000000 ) ) ;
#168549 = EDGE_LOOP ( 'NONE', ( #37704, #153535, #65038, #142219, #254260, #235539, #145673, #125730, #189602, #145625, #90274 ) ) ;
#168548 = CYLINDRICAL_SURFACE ( 'NONE', #90788, 0.09999999999999939493 ) ;
#168550 = CARTESIAN_POINT ( 'NONE',  ( -20.54999999999999716, 85.40000000001178648, -79.41707660717668205 ) ) ;
#168551 = VERTEX_POINT ( 'NONE', #81657 ) ;
#168552 = ADVANCED_FACE ( 'NONE', ( #20463 ), #97372, .F. ) ;
#168553 = DIRECTION ( 'NONE',  ( 1.000000000000000000, -0.000000000000000000, -0.000000000000000000 ) ) ;
#168554 = CARTESIAN_POINT ( 'NONE',  ( -23.15000000000000213, 1.925233644870972816, -146.7302435331261563 ) ) ;
#168555 = TOROIDAL_SURFACE ( 'NONE', #93470, 0.2000000000000000111, 0.1000000000000000056 ) ;
#168556 = ORIENTED_EDGE ( 'NONE', *, *, #139640, .F. ) ;
#168557 = AXIS2_PLACEMENT_3D ( 'NONE', #96216, #157528, #62237 ) ;
#168558 = DIRECTION ( 'NONE',  ( 0.000000000000000000, 0.000000000000000000, -1.000000000000000000 ) ) ;
#168559 = FACE_OUTER_BOUND ( 'NONE', #188573, .T. ) ;
#168560 = AXIS2_PLACEMENT_3D ( 'NONE', #38520, #18938, #140159 ) ;
#168561 = EDGE_CURVE ( 'NONE', #242970, #213303, #99947, .T. ) ;
#168562 = ORIENTED_EDGE ( 'NONE', *, *, #45395, .F. ) ;
#168564 = ORIENTED_EDGE ( 'NONE', *, *, #235689, .F. ) ;
#168563 = DIRECTION ( 'NONE',  ( -1.000000000000000000, -8.674042436075353235E-17, -1.619280515896125144E-16 ) ) ;
#168565 = AXIS2_PLACEMENT_3D ( 'NONE', #16651, #257756, #153636 ) ;
#168566 = DIRECTION ( 'NONE',  ( -0.000000000000000000, -6.982962677686266711E-15, 1.000000000000000000 ) ) ;
#168569 = VERTEX_POINT ( 'NONE', #38730 ) ;
#168568 = VERTEX_POINT ( 'NONE', #120859 ) ;
#168567 = VECTOR ( 'NONE', #36356, 1000.000000000000000 ) ;
#168570 = ORIENTED_EDGE ( 'NONE', *, *, #125824, .T. ) ;
#168571 = CYLINDRICAL_SURFACE ( 'NONE', #94925, 0.1000000000000055844 ) ;
#168572 = ORIENTED_EDGE ( 'NONE', *, *, #150937, .T. ) ;
#168573 = ORIENTED_EDGE ( 'NONE', *, *, #102039, .T. ) ;
#168574 = EDGE_LOOP ( 'NONE', ( #77706, #21444, #257184, #183909, #188692, #203507, #251112, #145516, #151928, #5214, #161243, #156010 ) ) ;
#168575 = DIRECTION ( 'NONE',  ( 0.000000000000000000, 1.000000000000000000, 0.000000000000000000 ) ) ;
#168576 = VECTOR ( 'NONE', #232957, 1000.000000000000227 ) ;
#168577 = VECTOR ( 'NONE', #236078, 1000.000000000000000 ) ;
#168578 = CARTESIAN_POINT ( 'NONE',  ( -23.25000000000000000, -1.851617760468904805, -45.10318971960366241 ) ) ;
#168579 = EDGE_CURVE ( 'NONE', #95316, #240059, #234319, .T. ) ;
#168580 = VERTEX_POINT ( 'NONE', #98649 ) ;
#168581 = ORIENTED_EDGE ( 'NONE', *, *, #176096, .T. ) ;
#168582 = LINE ( 'NONE', #32911, #242126 ) ;
#168583 = EDGE_LOOP ( 'NONE', ( #59676, #58573, #75103, #250806, #177171, #202423, #202637, #238352, #233705 ) ) ;
#168584 = ADVANCED_FACE ( 'NONE', ( #235626 ), #60836, .F. ) ;
#168585 = CARTESIAN_POINT ( 'NONE',  ( -18.40000000000000213, 11.48667500175767131, -24.25000000000000000 ) ) ;
#168586 = ORIENTED_EDGE ( 'NONE', *, *, #107818, .T. ) ;
#168587 = FACE_OUTER_BOUND ( 'NONE', #104090, .T. ) ;
#168589 = EDGE_LOOP ( 'NONE', ( #187475, #183036, #65110, #33788 ) ) ;
#168588 = CARTESIAN_POINT ( 'NONE',  ( -21.14999999999999858, 69.45934304831114048, -170.0231074845243882 ) ) ;
#168590 = CYLINDRICAL_SURFACE ( 'NONE', #113651, 0.1000000000000028644 ) ;
#168591 = CARTESIAN_POINT ( 'NONE',  ( -17.01825945287481545, 9.950000000011138823, -154.7500000000000284 ) ) ;
#168592 = DIRECTION ( 'NONE',  ( -0.9880948137434723000, -0.1538461538461483591, -1.074301950413233512E-15 ) ) ;
#168593 = CARTESIAN_POINT ( 'NONE',  ( -20.64999999999999858, 1.115600667400684642E-11, -100.5000000000000426 ) ) ;
#168594 = CIRCLE ( 'NONE', #51996, 0.09999999999999939493 ) ;
#168595 = LINE ( 'NONE', #69462, #199396 ) ;
#168596 = DIRECTION ( 'NONE',  ( 0.000000000000000000, 6.982962677686266711E-15, -1.000000000000000000 ) ) ;
#168597 = CARTESIAN_POINT ( 'NONE',  ( 18.60000000000000142, 38.30077178631847090, -261.1858881914067751 ) ) ;
#168598 = AXIS2_PLACEMENT_3D ( 'NONE', #165248, #85667, #88247 ) ;
#168599 = DIRECTION ( 'NONE',  ( 0.000000000000000000, 0.2617529984165045120, 0.9651348961777153068 ) ) ;
#168600 = EDGE_CURVE ( 'NONE', #254886, #237868, #142728, .T. ) ;
#168601 = VECTOR ( 'NONE', #91779, 1000.000000000000000 ) ;
#168602 = ORIENTED_EDGE ( 'NONE', *, *, #59660, .F. ) ;
#168603 = EDGE_CURVE ( 'NONE', #38009, #211815, #125991, .T. ) ;
#168604 = AXIS2_PLACEMENT_3D ( 'NONE', #193484, #233879, #72247 ) ;
#168605 = EDGE_LOOP ( 'NONE', ( #149118, #100461, #23817, #76173 ) ) ;
#168607 = ORIENTED_EDGE ( 'NONE', *, *, #247839, .F. ) ;
#168606 = DIRECTION ( 'NONE',  ( 0.000000000000000000, -0.8777080977375715243, 0.4791956752370512551 ) ) ;
#168608 = EDGE_LOOP ( 'NONE', ( #51327, #163582, #52311, #250191 ) ) ;
#168609 = CARTESIAN_POINT ( 'NONE',  ( -20.65000000000000568, 9.775875410973588586, -211.8174516384118817 ) ) ;
#168610 = EDGE_CURVE ( 'NONE', #46709, #148979, #105111, .T. ) ;
#168611 = DIRECTION ( 'NONE',  ( 0.000000000000000000, 0.2128009952263603677, -0.9770955615653313941 ) ) ;
#168613 = DIRECTION ( 'NONE',  ( 0.000000000000000000, -1.000000000000000000, 0.000000000000000000 ) ) ;
#168612 = DIRECTION ( 'NONE',  ( -1.000000000000000000, -2.952720810173289112E-16, 0.000000000000000000 ) ) ;
#168614 = EDGE_LOOP ( 'NONE', ( #78866, #59655, #227084, #224341, #7774, #40849, #162665, #246959, #147192, #151959, #228352, #38638 ) ) ;
#168616 = VERTEX_POINT ( 'NONE', #64699 ) ;
#168615 = AXIS2_PLACEMENT_3D ( 'NONE', #70788, #190739, #30365 ) ;
#168617 = EDGE_CURVE ( 'NONE', #205489, #212829, #205484, .T. ) ;
#168618 = EDGE_CURVE ( 'NONE', #160597, #14542, #80165, .T. ) ;
#168619 = CARTESIAN_POINT ( 'NONE',  ( 18.46082813848003212, -9.480749650896282077, -40.58437010271577350 ) ) ;
#168620 = VECTOR ( 'NONE', #110733, 1000.000000000000227 ) ;
#168621 = CARTESIAN_POINT ( 'NONE',  ( -20.94999999999999929, 1.115600667400684642E-11, -163.5000000000000284 ) ) ;
#168622 = EDGE_LOOP ( 'NONE', ( #1895, #140294, #235360, #251429 ) ) ;
#168623 = ORIENTED_EDGE ( 'NONE', *, *, #105570, .F. ) ;
#168624 = AXIS2_PLACEMENT_3D ( 'NONE', #60968, #218749, #222590 ) ;
#168625 = DIRECTION ( 'NONE',  ( 1.000000000000000000, -7.304098846218134667E-16, 0.000000000000000000 ) ) ;
#168626 = CARTESIAN_POINT ( 'NONE',  ( -16.81930730667006557, 9.936998068885200652, -180.2267677305381710 ) ) ;
#168627 = CARTESIAN_POINT ( 'NONE',  ( -20.94999999999999929, 67.23127455305835554, -235.8551265064784559 ) ) ;
#168628 = DIRECTION ( 'NONE',  ( 0.000000000000000000, -1.000000000000000000, 0.000000000000000000 ) ) ;
#168629 = ADVANCED_FACE ( 'NONE', ( #144219 ), #68563, .T. ) ;
#168630 = DIRECTION ( 'NONE',  ( 0.000000000000000000, -1.000000000000000000, -6.352154140967427193E-15 ) ) ;
#168632 = ORIENTED_EDGE ( 'NONE', *, *, #154892, .T. ) ;
#168631 = DIRECTION ( 'NONE',  ( 0.000000000000000000, -6.467318590049456648E-15, 1.000000000000000000 ) ) ;
#168633 = AXIS2_PLACEMENT_3D ( 'NONE', #115104, #254582, #195945 ) ;
#168634 = DIRECTION ( 'NONE',  ( 0.000000000000000000, -1.000000000000000000, -7.759275652592821052E-15 ) ) ;
#168635 = DIRECTION ( 'NONE',  ( -1.000000000000000000, -7.304098846218163263E-16, 4.217023435051627211E-16 ) ) ;
#168636 = DIRECTION ( 'NONE',  ( 0.000000000000000000, -0.05616704890742720696, 0.9984213852963240710 ) ) ;
#168637 = LINE ( 'NONE', #225947, #212319 ) ;
#168638 = VERTEX_POINT ( 'NONE', #127246 ) ;
#168639 = CARTESIAN_POINT ( 'NONE',  ( 12.42718393586866021, 66.62934494888835957, -85.49728422854349219 ) ) ;
#168640 = CARTESIAN_POINT ( 'NONE',  ( 21.14999999999999858, 1.115600667400684642E-11, -100.6000000000000227 ) ) ;
#168641 = CIRCLE ( 'NONE', #59652, 6.329289321881356400 ) ;
#168642 = CARTESIAN_POINT ( 'NONE',  ( -17.04761207306819060, 65.97354912661430149, -123.8731074845243683 ) ) ;
#168643 = CYLINDRICAL_SURFACE ( 'NONE', #120343, 0.1000000000000055844 ) ;
#168644 = CARTESIAN_POINT ( 'NONE',  ( -16.83558968593868954, 9.950000000011137047, -54.33769481238329746 ) ) ;
#168645 = CARTESIAN_POINT ( 'NONE',  ( -22.39999999999999858, 36.65892442174472876, -249.5511627012454596 ) ) ;
#168646 = CARTESIAN_POINT ( 'NONE',  ( -22.39999999999999858, 76.10085836911117951, -181.7726746080137445 ) ) ;
#168647 = LINE ( 'NONE', #108616, #229778 ) ;
#168648 = DIRECTION ( 'NONE',  ( -1.000000000000000000, -0.000000000000000000, -0.000000000000000000 ) ) ;
#168650 = ORIENTED_EDGE ( 'NONE', *, *, #30080, .F. ) ;
#168649 = VECTOR ( 'NONE', #1077, 1000.000000000000000 ) ;
#168651 = AXIS2_PLACEMENT_3D ( 'NONE', #73155, #75703, #152691 ) ;
#168652 = ORIENTED_EDGE ( 'NONE', *, *, #59452, .T. ) ;
#168653 = ORIENTED_EDGE ( 'NONE', *, *, #122032, .F. ) ;
#168654 = CARTESIAN_POINT ( 'NONE',  ( 18.69999999999999929, 0.000000000000000000, 0.000000000000000000 ) ) ;
#168655 = CARTESIAN_POINT ( 'NONE',  ( 18.39999999999999503, 5.650000000011139001, -113.1500000000000341 ) ) ;
#168656 = ADVANCED_FACE ( 'NONE', ( #65985 ), #184255, .F. ) ;
#168657 = EDGE_LOOP ( 'NONE', ( #140234, #222881, #161100, #80377 ) ) ;
#168658 = EDGE_CURVE ( 'NONE', #150597, #204820, #13585, .T. ) ;
#168659 = SHAPE_REPRESENTATION ( 'Injection Molded Chain Links', ( #2425 ), #114299 ) ;
#168660 = ORIENTED_EDGE ( 'NONE', *, *, #84753, .T. ) ;
#168661 = ADVANCED_FACE ( 'NONE', ( #107673 ), #146780, .T. ) ;
#168662 = ORIENTED_EDGE ( 'NONE', *, *, #36351, .F. ) ;
#168663 = DIRECTION ( 'NONE',  ( 0.000000000000000000, 0.000000000000000000, 1.000000000000000000 ) ) ;
#168664 = AXIS2_PLACEMENT_3D ( 'NONE', #21677, #77769, #215999 ) ;
#168665 = EDGE_LOOP ( 'NONE', ( #147312, #19391, #134957, #199605 ) ) ;
#168666 = DIRECTION ( 'NONE',  ( -1.000000000000000000, 7.136802563874201079E-16, 1.554319503706925800E-16 ) ) ;
#168667 = DIRECTION ( 'NONE',  ( 1.000000000000000000, 0.000000000000000000, 0.000000000000000000 ) ) ;
#168668 = CARTESIAN_POINT ( 'NONE',  ( 22.39999999999999503, 75.90000000001242597, -177.8138870828977360 ) ) ;
#168669 = CARTESIAN_POINT ( 'NONE',  ( -21.93642651522410247, 7.327166239336959208, -67.00000000000004263 ) ) ;
#168670 = DIRECTION ( 'NONE',  ( 2.715809747126117987E-16, 1.000000000000000000, 6.517943393102682774E-15 ) ) ;
#168672 = EDGE_LOOP ( 'NONE', ( #116890, #220174, #92680, #104371 ) ) ;
#168671 = DIRECTION ( 'NONE',  ( -0.000000000000000000, 1.000000000000000000, 1.734723475976807292E-15 ) ) ;
#168674 = CARTESIAN_POINT ( 'NONE',  ( 20.95512820512820440, 8.876151316299269567, -79.15000000000004832 ) ) ;
#168673 = PLANE ( 'NONE',  #216965 ) ;
#168675 = CARTESIAN_POINT ( 'NONE',  ( 18.49999999999999289, 65.79142135624906018, -78.25595019699899524 ) ) ;
#168676 = EDGE_LOOP ( 'NONE', ( #110840, #133256, #207590, #202764, #157297 ) ) ;
#168677 = CARTESIAN_POINT ( 'NONE',  ( 20.94999999999999574, 1.162701749949165642, -142.1000000000000227 ) ) ;
#168678 = DIRECTION ( 'NONE',  ( 0.7071067811865474617, 0.7071067811865474617, -0.000000000000000000 ) ) ;
#168679 = CARTESIAN_POINT ( 'NONE',  ( -20.94999999999999929, -11.74999999998884448, -36.60000000000000853 ) ) ;
#168680 = VERTEX_POINT ( 'NONE', #222463 ) ;
#168681 = CARTESIAN_POINT ( 'NONE',  ( -21.14999999999999858, 11.65000000001115588, -167.5999999999999659 ) ) ;
#168682 = B_SPLINE_CURVE_WITH_KNOTS ( 'NONE', 3,
 ( #255282, #20602, #16750, #177118, #240916, #100086, #235769, #179669, #976, #80515 ),
 .UNSPECIFIED., .F., .F.,
 ( 4, 2, 2, 2, 4 ),
 ( 5.262620404973387615E-16, 9.930191194504293527E-05, 0.0001986038238895596259, 0.0003972076477785142670, 0.0007944152955563421256 ),
 .UNSPECIFIED. ) ;
#168683 = EDGE_CURVE ( 'NONE', #14219, #73952, #38518, .T. ) ;
#168684 = CYLINDRICAL_SURFACE ( 'NONE', #86103, 0.09999999999999939493 ) ;
#168685 = ORIENTED_EDGE ( 'NONE', *, *, #85763, .T. ) ;
#168686 = CIRCLE ( 'NONE', #31298, 12.87499999999999822 ) ;
#168687 = DIRECTION ( 'NONE',  ( 0.000000000000000000, -1.000000000000000000, 0.000000000000000000 ) ) ;
#168688 = LINE ( 'NONE', #129513, #232747 ) ;
#168689 = CARTESIAN_POINT ( 'NONE',  ( 20.94999999999999929, 63.99342642423710714, -222.3880800784493772 ) ) ;
#168690 = EDGE_CURVE ( 'NONE', #214618, #100350, #7286, .T. ) ;
#168691 = FACE_OUTER_BOUND ( 'NONE', #138872, .T. ) ;
#168692 = ORIENTED_EDGE ( 'NONE', *, *, #67982, .F. ) ;
#168693 = ORIENTED_EDGE ( 'NONE', *, *, #130729, .T. ) ;
#168694 = ADVANCED_FACE ( 'NONE', ( #8585 ), #184641, .F. ) ;
#168695 = DIRECTION ( 'NONE',  ( 1.000000000000000000, 0.000000000000000000, 0.000000000000000000 ) ) ;
#168696 = DIRECTION ( 'NONE',  ( 0.000000000000000000, 0.8096735173027155286, -0.5868805631290315850 ) ) ;
#168697 = CARTESIAN_POINT ( 'NONE',  ( -21.05000000000000426, 65.60136641074581121, -241.9452829207083937 ) ) ;
#168698 = CARTESIAN_POINT ( 'NONE',  ( -22.39999999999999858, 11.75000000000000000, -0.1000000000000028644 ) ) ;
#168699 = ADVANCED_FACE ( 'NONE', ( #63405, #223758 ), #48984, .F. ) ;
#168701 = VECTOR ( 'NONE', #99816, 1000.000000000000000 ) ;
#168700 = DIRECTION ( 'NONE',  ( -1.000000000000000000, 0.000000000000000000, 0.000000000000000000 ) ) ;
#168702 = DIRECTION ( 'NONE',  ( 0.000000000000000000, 6.982962677686266711E-15, -1.000000000000000000 ) ) ;
#168703 = AXIS2_PLACEMENT_3D ( 'NONE', #132838, #57107, #54562 ) ;
#168704 = LINE ( 'NONE', #129529, #168489 ) ;
#168705 = LINE ( 'NONE', #90388, #196995 ) ;
#168707 = ORIENTED_EDGE ( 'NONE', *, *, #210005, .T. ) ;
#168706 = AXIS2_PLACEMENT_3D ( 'NONE', #59526, #58263, #217330 ) ;
#168708 = EDGE_CURVE ( 'NONE', #31369, #6262, #113532, .T. ) ;
#168709 = ORIENTED_EDGE ( 'NONE', *, *, #194738, .T. ) ;
#168711 = EDGE_CURVE ( 'NONE', #73216, #81857, #123397, .T. ) ;
#168710 = EDGE_CURVE ( 'NONE', #114106, #148744, #250885, .T. ) ;
#168712 = CARTESIAN_POINT ( 'NONE',  ( 20.94999999999999574, 70.10000000001235776, -159.8040077198679683 ) ) ;
#168713 = FACE_OUTER_BOUND ( 'NONE', #149428, .T. ) ;
#168714 = CARTESIAN_POINT ( 'NONE',  ( 20.84999999999998721, 11.75000000001115552, -167.5000000000000284 ) ) ;
#168716 = VERTEX_POINT ( 'NONE', #3428 ) ;
#168715 = DIRECTION ( 'NONE',  ( -0.000000000000000000, -1.000000000000000000, -0.000000000000000000 ) ) ;
#168717 = SPHERICAL_SURFACE ( 'NONE', #125728, 0.1000000000000000056 ) ;
#168718 = DIRECTION ( 'NONE',  ( 0.000000000000000000, 0.2128009952263403282, -0.9770955615653358350 ) ) ;
#168719 = DIRECTION ( 'NONE',  ( 0.000000000000000000, 0.000000000000000000, 1.000000000000000000 ) ) ;
#168720 = CARTESIAN_POINT ( 'NONE',  ( 20.94999999999999929, 76.00000000001142553, -36.02310748452432421 ) ) ;
#168721 = ORIENTED_EDGE ( 'NONE', *, *, #14990, .T. ) ;
#168722 = CARTESIAN_POINT ( 'NONE',  ( -23.15000000000000213, 34.89593390941166007, -248.6067769466879156 ) ) ;
#168723 = ORIENTED_EDGE ( 'NONE', *, *, #138827, .T. ) ;
#168724 = FACE_OUTER_BOUND ( 'NONE', #7873, .T. ) ;
#168725 = EDGE_LOOP ( 'NONE', ( #45237, #195098, #192908, #37749, #212247, #186780, #122350, #248558, #74347 ) ) ;
#168726 = DIRECTION ( 'NONE',  ( -1.000000000000000000, -0.000000000000000000, -0.000000000000000000 ) ) ;
#168727 = EDGE_CURVE ( 'NONE', #187756, #243905, #59314, .T. ) ;
#168728 = EDGE_CURVE ( 'NONE', #252057, #153545, #255062, .T. ) ;
#168729 = AXIS2_PLACEMENT_3D ( 'NONE', #202145, #139573, #238697 ) ;
#168730 = ORIENTED_EDGE ( 'NONE', *, *, #2562, .T. ) ;
#168731 = VECTOR ( 'NONE', #103064, 1000.000000000000000 ) ;
#168732 = CARTESIAN_POINT ( 'NONE',  ( -23.25000000000000000, 36.65892442174472876, -249.5511627012454596 ) ) ;
#168734 = CARTESIAN_POINT ( 'NONE',  ( 20.85000000000000142, 43.18640298906419162, -245.2812653309023574 ) ) ;
#168733 = CIRCLE ( 'NONE', #56224, 0.1000000000000013933 ) ;
#168735 = B_SPLINE_CURVE_WITH_KNOTS ( 'NONE', 3,
 ( #57668, #18568, #82350, #198478, #100627, #77235, #180219, #161946 ),
 .UNSPECIFIED., .F., .F.,
 ( 4, 2, 2, 4 ),
 ( 0.000000000000000000, 0.0001094981963948484779, 0.0002189963927896969558, 0.0004379927855793939117 ),
 .UNSPECIFIED. ) ;
#168736 = ADVANCED_FACE ( 'NONE', ( #132378 ), #175912, .F. ) ;
#168737 = DIRECTION ( 'NONE',  ( 0.000000000000000000, 0.000000000000000000, -1.000000000000000000 ) ) ;
#168738 = VERTEX_POINT ( 'NONE', #150662 ) ;
#168739 = AXIS2_PLACEMENT_3D ( 'NONE', #86268, #110998, #210114 ) ;
#168740 = VECTOR ( 'NONE', #132478, 999.9999999999998863 ) ;
#168742 = CARTESIAN_POINT ( 'NONE',  ( -16.87333278164150840, 9.882609784578846757, -13.13316780615338075 ) ) ;
#168741 = AXIS2_PLACEMENT_3D ( 'NONE', #166292, #147981, #127126 ) ;
#168743 = EDGE_CURVE ( 'NONE', #165923, #7536, #30339, .T. ) ;
#168744 = AXIS2_PLACEMENT_3D ( 'NONE', #219400, #177753, #14830 ) ;
#168745 = DIRECTION ( 'NONE',  ( 0.000000000000000000, 0.000000000000000000, 1.000000000000000000 ) ) ;
#168746 = EDGE_CURVE ( 'NONE', #14799, #136029, #26066, .T. ) ;
#168747 = CARTESIAN_POINT ( 'NONE',  ( 15.57250062127603307, 9.370689921602609829, -17.52646512666105139 ) ) ;
#168748 = DIRECTION ( 'NONE',  ( 1.000000000000000000, 0.000000000000000000, 0.000000000000000000 ) ) ;
#168749 = DIRECTION ( 'NONE',  ( 1.000000000000000000, 0.000000000000000000, 0.000000000000000000 ) ) ;
#168750 = ORIENTED_EDGE ( 'NONE', *, *, #62482, .T. ) ;
#168752 = ORIENTED_EDGE ( 'NONE', *, *, #203269, .F. ) ;
#168751 = DIRECTION ( 'NONE',  ( 0.000000000000000000, -6.982962677686266711E-15, 1.000000000000000000 ) ) ;
#168753 = CIRCLE ( 'NONE', #226959, 0.1000000000000013933 ) ;
#168754 = ORIENTED_EDGE ( 'NONE', *, *, #195527, .T. ) ;
#168755 = CARTESIAN_POINT ( 'NONE',  ( 18.39999999999999858, 47.00127771169579205, -255.4372249185379928 ) ) ;
#168756 = ORIENTED_EDGE ( 'NONE', *, *, #75206, .T. ) ;
#168757 = CARTESIAN_POINT ( 'NONE',  ( 23.40000000000005542, 77.83551161375991967, -47.52760213295649550 ) ) ;
#168758 = VECTOR ( 'NONE', #89453, 1000.000000000000000 ) ;
#168759 = CARTESIAN_POINT ( 'NONE',  ( 23.24999999999999645, 53.86595165227826243, -236.3638196928718855 ) ) ;
#168760 = DIRECTION ( 'NONE',  ( 0.000000000000000000, 1.734723475976997999E-14, 1.000000000000000000 ) ) ;
#168761 = ORIENTED_EDGE ( 'NONE', *, *, #71904, .F. ) ;
#168762 = ADVANCED_FACE ( 'NONE', ( #251020 ), #180182, .F. ) ;
#168764 = AXIS2_PLACEMENT_3D ( 'NONE', #148935, #27727, #210190 ) ;
#168763 = CYLINDRICAL_SURFACE ( 'NONE', #115690, 0.1000000000000028644 ) ;
#168765 = CARTESIAN_POINT ( 'NONE',  ( -16.87786941232801041, 66.04184528586654324, -48.64592168473038214 ) ) ;
#168766 = DIRECTION ( 'NONE',  ( -0.7071067811865389130, -5.024295867788141276E-15, 0.7071067811865561215 ) ) ;
#168767 = AXIS2_PLACEMENT_3D ( 'NONE', #118402, #195385, #16739 ) ;
#168768 = ORIENTED_EDGE ( 'NONE', *, *, #205689, .F. ) ;
#168770 = ORIENTED_EDGE ( 'NONE', *, *, #10714, .F. ) ;
#168769 = LINE ( 'NONE', #189572, #75764 ) ;
#168771 = CARTESIAN_POINT ( 'NONE',  ( -23.15000000000000213, 23.40438595358395091, -253.3416554127419431 ) ) ;
#168772 = CARTESIAN_POINT ( 'NONE',  ( 21.14999999999999858, 10.71339244341104013, -112.8500000000000369 ) ) ;
#168773 = ADVANCED_FACE ( 'NONE', ( #91962 ), #15017, .F. ) ;
#168774 = ORIENTED_EDGE ( 'NONE', *, *, #238430, .T. ) ;
#168775 = DIRECTION ( 'NONE',  ( 1.000000000000000000, 0.000000000000000000, 0.000000000000000000 ) ) ;
#168776 = CARTESIAN_POINT ( 'NONE',  ( -17.29838795455454559, 42.81805030517067223, -235.4272065966908656 ) ) ;
#168777 = DIRECTION ( 'NONE',  ( -0.7070776581709311559, -0.6233369439635936260, 0.3339045366652567126 ) ) ;
#168778 = ORIENTED_EDGE ( 'NONE', *, *, #46227, .F. ) ;
#168779 = LINE ( 'NONE', #167469, #104917 ) ;
#168780 = EDGE_CURVE ( 'NONE', #165019, #122696, #50254, .T. ) ;
#168781 = CARTESIAN_POINT ( 'NONE',  ( -20.54999999999999716, 76.00000000001213607, -136.5231074845243313 ) ) ;
#168782 = AXIS2_PLACEMENT_3D ( 'NONE', #108456, #105858, #107160 ) ;
#168783 = ORIENTED_EDGE ( 'NONE', *, *, #136292, .F. ) ;
#168784 = AXIS2_PLACEMENT_3D ( 'NONE', #51686, #213341, #93400 ) ;
#168785 = AXIS2_PLACEMENT_3D ( 'NONE', #131555, #89848, #251493 ) ;
#168786 = VERTEX_POINT ( 'NONE', #211930 ) ;
#168787 = CARTESIAN_POINT ( 'NONE',  ( 21.13614978966381841, 1.115648720638573240E-11, -94.00089529816622758 ) ) ;
#168788 = AXIS2_PLACEMENT_3D ( 'NONE', #208875, #30257, #74551 ) ;
#168789 = AXIS2_PLACEMENT_3D ( 'NONE', #30081, #243955, #109572 ) ;
#168790 = ORIENTED_EDGE ( 'NONE', *, *, #147144, .T. ) ;
#168791 = DIRECTION ( 'NONE',  ( -7.304098846218132695E-16, -0.9770955615653315052, -0.2128009952263603954 ) ) ;
#168792 = CARTESIAN_POINT ( 'NONE',  ( 21.05000000000000071, 85.50000000001251976, -179.9170766071767389 ) ) ;
#168794 = EDGE_LOOP ( 'NONE', ( #52049, #96416, #134348, #49949 ) ) ;
#168793 = CARTESIAN_POINT ( 'NONE',  ( 14.22821877134046353, 24.82620238936339874, -232.4854380501665787 ) ) ;
#168795 = FACE_OUTER_BOUND ( 'NONE', #117388, .T. ) ;
#168796 = CARTESIAN_POINT ( 'NONE',  ( -16.27683809663750480, 9.350000000011133849, -76.25000000000004263 ) ) ;
#168797 = DIRECTION ( 'NONE',  ( 1.000000000000000000, 0.000000000000000000, 0.000000000000000000 ) ) ;
#168798 = DIRECTION ( 'NONE',  ( 1.000000000000000000, 0.000000000000000000, 0.000000000000000000 ) ) ;
#168799 = CARTESIAN_POINT ( 'NONE',  ( -20.94999999999999929, 70.15000000001235492, -159.8906102602464330 ) ) ;
#168800 = VECTOR ( 'NONE', #251959, 1000.000000000000000 ) ;
#168801 = DIRECTION ( 'NONE',  ( 1.000000000000000000, 0.000000000000000000, 0.000000000000000000 ) ) ;
#168802 = LINE ( 'NONE', #248287, #111448 ) ;
#168804 = ORIENTED_EDGE ( 'NONE', *, *, #46038, .F. ) ;
#168803 = DIRECTION ( 'NONE',  ( 1.000000000000000000, 0.000000000000000000, 0.000000000000000000 ) ) ;
#168805 = DIRECTION ( 'NONE',  ( 0.000000000000000000, 0.000000000000000000, -1.000000000000000000 ) ) ;
#168806 = VECTOR ( 'NONE', #92445, 1000.000000000000000 ) ;
#168807 = CARTESIAN_POINT ( 'NONE',  ( -23.15000000000000213, 36.65892442174472876, -249.5511627012454596 ) ) ;
#168808 = AXIS2_PLACEMENT_3D ( 'NONE', #251739, #73138, #232198 ) ;
#168809 = CARTESIAN_POINT ( 'NONE',  ( 20.50589344625199217, 65.51681206853709227, -195.9501125058534114 ) ) ;
#168810 = FACE_OUTER_BOUND ( 'NONE', #1087, .T. ) ;
#168811 = ORIENTED_EDGE ( 'NONE', *, *, #235806, .T. ) ;
#168812 = CARTESIAN_POINT ( 'NONE',  ( 21.05000000000000071, 10.27540777873560707, -228.0704167471579069 ) ) ;
#168813 = EDGE_CURVE ( 'NONE', #26102, #216777, #196034, .T. ) ;
#168814 = CARTESIAN_POINT ( 'NONE',  ( -21.13614978966381130, 6.499104701844946597, -100.5000000000000142 ) ) ;
#168815 = CARTESIAN_POINT ( 'NONE',  ( -23.25000000000000000, 71.75000000001223555, -148.8731074845244109 ) ) ;
#168816 = ORIENTED_EDGE ( 'NONE', *, *, #189760, .F. ) ;
#168817 = CIRCLE ( 'NONE', #251977, 0.09999999999999939493 ) ;
#168818 = DIRECTION ( 'NONE',  ( -1.000000000000000000, 3.265361837132813093E-16, 2.280189983783949500E-30 ) ) ;
#168819 = CIRCLE ( 'NONE', #114609, 0.09999999999998898659 ) ;
#168820 = CARTESIAN_POINT ( 'NONE',  ( -21.00023020733438983, 61.06322362754159627, -234.1822973190417088 ) ) ;
#168821 = B_SPLINE_CURVE_WITH_KNOTS ( 'NONE', 3,
 ( #47543, #245773, #166266, #248335, #67128, #209203, #147955, #46266, #104930, #146642 ),
 .UNSPECIFIED., .F., .F.,
 ( 4, 3, 3, 4 ),
 ( -2.000561356212805974E-06, 0.000000000000000000, 1.787822682428821068E-05, 4.206475347090201300E-05 ),
 .UNSPECIFIED. ) ;
#168822 = ORIENTED_EDGE ( 'NONE', *, *, #172679, .F. ) ;
#168823 = CARTESIAN_POINT ( 'NONE',  ( -21.05000000000000071, 6.540656951712399803, -67.00000000000004263 ) ) ;
#168824 = ORIENTED_EDGE ( 'NONE', *, *, #218600, .F. ) ;
#168825 = EDGE_CURVE ( 'NONE', #132399, #163489, #191096, .T. ) ;
#168826 = CARTESIAN_POINT ( 'NONE',  ( -18.59999999999999787, -1.835859311432481045, -78.50443916879852679 ) ) ;
#168827 = ORIENTED_EDGE ( 'NONE', *, *, #212074, .T. ) ;
#168829 = EDGE_CURVE ( 'NONE', #140958, #41654, #210630, .T. ) ;
#168828 = DIRECTION ( 'NONE',  ( 0.000000000000000000, 0.000000000000000000, 1.000000000000000000 ) ) ;
#168830 = CARTESIAN_POINT ( 'NONE',  ( 21.05000000000000071, 63.48958393997221350, -237.5313578019574265 ) ) ;
#168831 = ORIENTED_EDGE ( 'NONE', *, *, #242474, .F. ) ;
#168832 = ORIENTED_EDGE ( 'NONE', *, *, #195440, .F. ) ;
#168833 = CARTESIAN_POINT ( 'NONE',  ( 18.59999994388910238, 85.36356618708315125, -129.3419902477232029 ) ) ;
#168835 = ORIENTED_EDGE ( 'NONE', *, *, #9684, .F. ) ;
#168834 =( NAMED_UNIT ( * ) SI_UNIT ( $, .STERADIAN. ) SOLID_ANGLE_UNIT ( ) );
#168836 = DIRECTION ( 'NONE',  ( 0.000000000000000000, 0.2128009952263485993, -0.9770955615653341697 ) ) ;
#168837 = CIRCLE ( 'NONE', #64734, 0.2000000000000027867 ) ;
#168838 = ORIENTED_EDGE ( 'NONE', *, *, #64309, .F. ) ;
#168839 = EDGE_CURVE ( 'NONE', #65124, #77581, #138451, .T. ) ;
#168840 = AXIS2_PLACEMENT_3D ( 'NONE', #252691, #135309, #212320 ) ;
#168841 = ADVANCED_FACE ( 'NONE', ( #39727 ), #63447, .T. ) ;
#168842 = ORIENTED_EDGE ( 'NONE', *, *, #171828, .F. ) ;
#168843 = CARTESIAN_POINT ( 'NONE',  ( 23.24999999999999645, 45.51971589178210564, -240.3486087337583399 ) ) ;
#168844 = FACE_OUTER_BOUND ( 'NONE', #187929, .T. ) ;
#168845 = CARTESIAN_POINT ( 'NONE',  ( 13.40000000000000036, -8.250000000000003553, 15.00000000000000355 ) ) ;
#168846 = EDGE_CURVE ( 'NONE', #30986, #187774, #238425, .T. ) ;
#168847 = DIRECTION ( 'NONE',  ( -0.000000000000000000, -6.982962677686266711E-15, 1.000000000000000000 ) ) ;
#168848 = CARTESIAN_POINT ( 'NONE',  ( 21.13461538461538325, 65.38541703798603066, -57.27310748452440947 ) ) ;
#168849 = CARTESIAN_POINT ( 'NONE',  ( -0.8999999999999437339, 67.75000000001118394, -10.02310748452479139 ) ) ;
#168850 = ORIENTED_EDGE ( 'NONE', *, *, #77891, .T. ) ;
#168851 = FACE_OUTER_BOUND ( 'NONE', #27650, .T. ) ;
#168852 = CARTESIAN_POINT ( 'NONE',  ( -20.64999999999999858, 70.22209180797715078, -215.6584443947398313 ) ) ;
#168853 = EDGE_CURVE ( 'NONE', #1294, #27375, #55412, .T. ) ;
#168854 = DIRECTION ( 'NONE',  ( 0.000000000000000000, 0.8814952561688428334, -0.4721928772777349015 ) ) ;
#168855 = ORIENTED_EDGE ( 'NONE', *, *, #203629, .F. ) ;
#168856 = PLANE ( 'NONE',  #22233 ) ;
#168857 = ORIENTED_EDGE ( 'NONE', *, *, #118529, .F. ) ;
#168858 = DIRECTION ( 'NONE',  ( -0.000000000000000000, 0.1298341882519953583, 0.9915357197604862671 ) ) ;
#168859 = ORIENTED_EDGE ( 'NONE', *, *, #141783, .T. ) ;
#168860 = AXIS2_PLACEMENT_3D ( 'NONE', #18220, #177330, #45484 ) ;
#168861 = EDGE_CURVE ( 'NONE', #177586, #206303, #59506, .T. ) ;
#168862 = DIRECTION ( 'NONE',  ( -5.603264701231743991E-32, 1.897661533703519897E-16, -1.000000000000000000 ) ) ;
#168863 = DIRECTION ( 'NONE',  ( 1.000000000000000000, 0.000000000000000000, 0.000000000000000000 ) ) ;
#168864 = VERTEX_POINT ( 'NONE', #99636 ) ;
#168865 = ORIENTED_EDGE ( 'NONE', *, *, #27840, .F. ) ;
#168867 = ORIENTED_EDGE ( 'NONE', *, *, #112993, .T. ) ;
#168866 = CARTESIAN_POINT ( 'NONE',  ( 18.59999999999999076, 11.65000000001115943, -158.8500000000000227 ) ) ;
#168868 = CARTESIAN_POINT ( 'NONE',  ( 21.05000000000000071, 6.350000000011161383, -43.34382208968312966 ) ) ;
#168869 = VERTEX_POINT ( 'NONE', #196200 ) ;
#168870 = DIRECTION ( 'NONE',  ( 1.000000000000000000, 0.000000000000000000, 0.000000000000000000 ) ) ;
#168871 = CARTESIAN_POINT ( 'NONE',  ( -18.50000000000000000, 65.70729864260985664, -64.06574559737244101 ) ) ;
#168872 = EDGE_CURVE ( 'NONE', #201908, #133, #219602, .T. ) ;
#168873 = VERTEX_POINT ( 'NONE', #198760 ) ;
#168874 = LINE ( 'NONE', #248367, #118629 ) ;
#168876 = FACE_OUTER_BOUND ( 'NONE', #65103, .T. ) ;
#168875 = AXIS2_PLACEMENT_3D ( 'NONE', #180060, #220476, #117512 ) ;
#168877 = AXIS2_PLACEMENT_3D ( 'NONE', #131220, #210763, #32154 ) ;
#168878 = ORIENTED_EDGE ( 'NONE', *, *, #73923, .F. ) ;
#168879 = AXIS2_PLACEMENT_3D ( 'NONE', #242388, #57643, #162890 ) ;
#168880 = CARTESIAN_POINT ( 'NONE',  ( -20.64999999999999858, 2.500000000011156409, -80.22462192276213955 ) ) ;
#168881 =( GEOMETRIC_REPRESENTATION_CONTEXT ( 3 ) GLOBAL_UNCERTAINTY_ASSIGNED_CONTEXT ( ( #24425 ) ) GLOBAL_UNIT_ASSIGNED_CONTEXT ( ( #216032, #173121, #253875 ) ) REPRESENTATION_CONTEXT ( 'NONE', 'WORKASPACE' ) );
#168882 = DIRECTION ( 'NONE',  ( 1.000000000000000000, 3.265361837132813093E-16, -0.000000000000000000 ) ) ;
#168883 = CYLINDRICAL_SURFACE ( 'NONE', #125925, 0.09999999999999939493 ) ;
#168885 = EDGE_LOOP ( 'NONE', ( #202202, #175915, #161707, #236851, #88588, #140665, #250723, #72265, #155044, #5434, #191067, #232451 ) ) ;
#168884 = DIRECTION ( 'NONE',  ( 1.000000000000000000, 0.000000000000000000, 0.000000000000000000 ) ) ;
#168886 = DIRECTION ( 'NONE',  ( -0.000000000000000000, 1.000000000000000000, -0.000000000000000000 ) ) ;
#168887 = CARTESIAN_POINT ( 'NONE',  ( 21.05000000000000071, 67.22371710471912820, -60.96447848938343839 ) ) ;
#168889 = CARTESIAN_POINT ( 'NONE',  ( -16.87331047859649757, 66.05000000001182059, -82.17310748452439384 ) ) ;
#168888 = CARTESIAN_POINT ( 'NONE',  ( -18.47140463609786210, -9.671474685209730637, -140.6727604582741264 ) ) ;
#168890 = CARTESIAN_POINT ( 'NONE',  ( -16.87036670365549895, 44.00112830765706917, -235.3159266546824995 ) ) ;
#168891 = CARTESIAN_POINT ( 'NONE',  ( 18.42555734704283665, -9.497158361925555070, -107.5398304977349682 ) ) ;
#168892 = CARTESIAN_POINT ( 'NONE',  ( 22.60000000000000142, 11.74956712348939192, 0.1008583690987087389 ) ) ;
#168893 = CARTESIAN_POINT ( 'NONE',  ( -21.05000000000000071, 75.96824164695659931, -176.2819546076071902 ) ) ;
#168894 = TOROIDAL_SURFACE ( 'NONE', #218714, 0.2000000000000000111, 0.1000000000000000056 ) ;
#168895 = VERTEX_POINT ( 'NONE', #235320 ) ;
#168896 = MECHANICAL_DESIGN_GEOMETRIC_PRESENTATION_REPRESENTATION (  '', ( #10648 ), #148010 ) ;
#168897 = ADVANCED_FACE ( 'NONE', ( #136191 ), #75294, .T. ) ;
#168898 = VECTOR ( 'NONE', #172009, 1000.000000000000000 ) ;
#168899 = VERTEX_POINT ( 'NONE', #200060 ) ;
#168900 = ORIENTED_EDGE ( 'NONE', *, *, #66088, .T. ) ;
#168901 = EDGE_CURVE ( 'NONE', #245959, #76969, #47053, .T. ) ;
#168902 = EDGE_CURVE ( 'NONE', #231733, #85086, #257394, .T. ) ;
#168903 = CARTESIAN_POINT ( 'NONE',  ( 18.59999999999999432, 74.27191306321832087, -216.6386724793566145 ) ) ;
#168904 = AXIS2_PLACEMENT_3D ( 'NONE', #222919, #79547, #2586 ) ;
#168905 = CIRCLE ( 'NONE', #143916, 0.3999999999999996891 ) ;
#168906 = CIRCLE ( 'NONE', #218930, 11.75000000000001066 ) ;
#168907 = FACE_OUTER_BOUND ( 'NONE', #322, .T. ) ;
#168908 = EDGE_LOOP ( 'NONE', ( #135796, #167664, #116593, #49546 ) ) ;
#168909 = EDGE_CURVE ( 'NONE', #105444, #41155, #205228, .T. ) ;
#168910 = DIRECTION ( 'NONE',  ( 0.000000000000000000, 0.2617529984165031243, 0.9651348961777157509 ) ) ;
#168911 = DIRECTION ( 'NONE',  ( 1.000000000000000000, 0.000000000000000000, 0.000000000000000000 ) ) ;
#168912 = ADVANCED_FACE ( 'NONE', ( #95794 ), #230234, .T. ) ;
#168913 = DIRECTION ( 'NONE',  ( 1.000000000000000000, 0.000000000000000000, 0.000000000000000000 ) ) ;
#168914 = ORIENTED_EDGE ( 'NONE', *, *, #98376, .F. ) ;
#168915 = EDGE_CURVE ( 'NONE', #36183, #239427, #74243, .T. ) ;
#168916 = ORIENTED_EDGE ( 'NONE', *, *, #210169, .T. ) ;
#168917 = CARTESIAN_POINT ( 'NONE',  ( -18.50000000000000000, 1.115600667400684642E-11, -33.50000000000000000 ) ) ;
#168918 = CARTESIAN_POINT ( 'NONE',  ( 20.94999999999999929, 85.00000000001222134, -145.9170766071767389 ) ) ;
#168919 = ORIENTED_EDGE ( 'NONE', *, *, #182521, .T. ) ;
#168920 = VECTOR ( 'NONE', #60396, 1000.000000000000000 ) ;
#168921 = EDGE_CURVE ( 'NONE', #31330, #232305, #17832, .T. ) ;
#168922 = DIRECTION ( 'NONE',  ( -0.000000000000000000, 1.000000000000000000, 0.000000000000000000 ) ) ;
#168923 = VERTEX_POINT ( 'NONE', #230726 ) ;
#168924 = DIRECTION ( 'NONE',  ( 1.000000000000000000, 0.000000000000000000, 0.000000000000000000 ) ) ;
#168925 = AXIS2_PLACEMENT_3D ( 'NONE', #84741, #143469, #120098 ) ;
#168927 = B_SPLINE_CURVE_WITH_KNOTS ( 'NONE', 3,
 ( #42731, #175850, #41476, #197945, #80543, #140533, #2301, #200523, #57135, #117144 ),
 .UNSPECIFIED., .F., .F.,
 ( 4, 3, 3, 4 ),
 ( 0.000000000000000000, 0.0002000000000002785953, 0.001000000000045107385, 0.001967863649472122601 ),
 .UNSPECIFIED. ) ;
#168926 = FACE_OUTER_BOUND ( 'NONE', #234000, .T. ) ;
#168928 = AXIS2_PLACEMENT_3D ( 'NONE', #72553, #251150, #152098 ) ;
#168930 = ORIENTED_EDGE ( 'NONE', *, *, #203291, .F. ) ;
#168929 = CARTESIAN_POINT ( 'NONE',  ( -1.739115166359751801E-14, 64.35000000001178933, -78.17310748452437963 ) ) ;
#168931 = FILL_AREA_STYLE ('',( #146720 ) ) ;
#168932 = FACE_OUTER_BOUND ( 'NONE', #251714, .T. ) ;
#168933 = DIRECTION ( 'NONE',  ( -0.7071067811865474617, -0.7071067811865474617, -0.000000000000000000 ) ) ;
#168934 = CYLINDRICAL_SURFACE ( 'NONE', #160935, 0.09999999999999609201 ) ;
#168936 = DIRECTION ( 'NONE',  ( -3.265361837132813093E-16, 1.000000000000000000, 0.000000000000000000 ) ) ;
#168935 = CARTESIAN_POINT ( 'NONE',  ( 33.30000000000001137, 3.332938107839120701, -347.0000000000001137 ) ) ;
#168937 = DIRECTION ( 'NONE',  ( 1.000000000000000000, 0.000000000000000000, 0.000000000000000000 ) ) ;
#168938 = LINE ( 'NONE', #148050, #247680 ) ;
#168939 = CARTESIAN_POINT ( 'NONE',  ( -21.59142135623730852, 7.850000000011158718, -88.15000000000004832 ) ) ;
#168940 = DIRECTION ( 'NONE',  ( 1.652117596168391700E-15, -1.000000000000000000, -6.982962677686266711E-15 ) ) ;
#168941 = VERTEX_POINT ( 'NONE', #153800 ) ;
#168942 = VERTEX_POINT ( 'NONE', #52054 ) ;
#168943 = EDGE_CURVE ( 'NONE', #39190, #253747, #151148, .T. ) ;
#168944 = PLANE ( 'NONE',  #155526 ) ;
#168945 = VERTEX_POINT ( 'NONE', #233304 ) ;
#168946 = CARTESIAN_POINT ( 'NONE',  ( -23.25000000000000000, 64.25000000001222134, -148.2731074845243882 ) ) ;
#168947 = ORIENTED_EDGE ( 'NONE', *, *, #13214, .F. ) ;
#168948 = PLANE ( 'NONE',  #77717 ) ;
#168949 = CYLINDRICAL_SURFACE ( 'NONE', #164960, 0.5000000000000004441 ) ;
#168950 = EDGE_CURVE ( 'NONE', #165929, #241281, #217743, .T. ) ;
#168951 = APPLICATION_CONTEXT ( 'automotive_design' ) ;
#168952 = ADVANCED_FACE ( 'NONE', ( #174647 ), #130314, .T. ) ;
#168953 = AXIS2_PLACEMENT_3D ( 'NONE', #182932, #145062, #165946 ) ;
#168954 = ORIENTED_EDGE ( 'NONE', *, *, #116270, .F. ) ;
#168955 = PLANE ( 'NONE',  #102848 ) ;
#168956 = AXIS2_PLACEMENT_3D ( 'NONE', #172980, #97200, #214619 ) ;
#168957 = EDGE_LOOP ( 'NONE', ( #253049, #61203, #119905, #74437 ) ) ;
#168958 = VERTEX_POINT ( 'NONE', #114616 ) ;
#168959 = ORIENTED_EDGE ( 'NONE', *, *, #127164, .F. ) ;
#168960 = AXIS2_PLACEMENT_3D ( 'NONE', #245135, #122639, #22253 ) ;
#168961 = DIRECTION ( 'NONE',  ( 0.000000000000000000, -1.000000000000000000, 6.308085367188393199E-16 ) ) ;
#168962 = FACE_OUTER_BOUND ( 'NONE', #134904, .T. ) ;
#168963 = DIRECTION ( 'NONE',  ( -0.000000000000000000, 0.9667078373770112698, 0.2558827019434132821 ) ) ;
#168964 = DIRECTION ( 'NONE',  ( 1.000000000000000000, 0.000000000000000000, 0.000000000000000000 ) ) ;
#168965 = CARTESIAN_POINT ( 'NONE',  ( -20.64999999999999858, 2.400000000011155432, -80.22462192276213955 ) ) ;
#168966 =( BOUNDED_SURFACE ( )  B_SPLINE_SURFACE ( 3, 2, ( 
 ( #172431, #155434, #211517 ),
 ( #53718, #151571, #13319 ),
 ( #32922, #233657, #113695 ),
 ( #194547, #34194, #135809 ),
 ( #73322, #17183, #234937 ),
 ( #154152, #134523, #116281 ),
 ( #133262, #77131, #212809 ),
 ( #195829, #112426, #191978 ) ),
 .UNSPECIFIED., .F., .F., .F. ) 
 B_SPLINE_SURFACE_WITH_KNOTS ( ( 4, 2, 2, 4 ),
 ( 3, 3 ),
 ( 0.0001704874539069695018, 0.0003809798300636460045, 0.0004862260181419842558, 0.0005914722062203225071 ),
 ( 0.000000000000000000, 1.000000000000000000 ),
 .UNSPECIFIED. ) 
 GEOMETRIC_REPRESENTATION_ITEM ( )  RATIONAL_B_SPLINE_SURFACE ( (
 ( 1.000000000000000000, 0.7071067811864699681, 1.000000000000000000),
 ( 1.000000000000000000, 0.7670648383577226559, 1.000000000000000000),
 ( 1.000000000000000000, 0.8204820770250529360, 1.000000000000000000),
 ( 1.000000000000000000, 0.8877218296113961182, 1.000000000000000000),
 ( 1.000000000000000000, 0.9080815932664115797, 1.000000000000000000),
 ( 1.000000000000000000, 0.9395541505862786691, 1.000000000000000000),
 ( 1.000000000000000000, 0.9506520335378314535, 1.000000000000000000),
 ( 1.000000000000000000, 0.9504532311154486601, 1.000000000000000000) ) ) 
 REPRESENTATION_ITEM ( '' )  SURFACE ( )  );
#168968 = DIRECTION ( 'NONE',  ( 0.000000000000000000, 2.891205793294679805E-16, -1.000000000000000000 ) ) ;
#168967 = CARTESIAN_POINT ( 'NONE',  ( -21.05000000000000071, 14.72981487416292623, -236.4853282537515895 ) ) ;
#168969 = CARTESIAN_POINT ( 'NONE',  ( -14.56556274378147720, 9.446557523083688679, -82.08994195434594587 ) ) ;
#168971 = VERTEX_POINT ( 'NONE', #112064 ) ;
#168970 = CARTESIAN_POINT ( 'NONE',  ( -21.05000000000000071, 68.11887992016828264, -227.8068560890360175 ) ) ;
#168973 = DIRECTION ( 'NONE',  ( 0.000000000000000000, 0.9553114395362733990, 0.2956011730205631016 ) ) ;
#168972 = LINE ( 'NONE', #69848, #125967 ) ;
#168974 = CARTESIAN_POINT ( 'NONE',  ( 23.24999999999999645, 73.90000000001244018, -170.0231074845244166 ) ) ;
#168975 = AXIS2_PLACEMENT_3D ( 'NONE', #172744, #214386, #35776 ) ;
#168976 = ORIENTED_EDGE ( 'NONE', *, *, #142265, .T. ) ;
#168977 = FACE_OUTER_BOUND ( 'NONE', #173206, .T. ) ;
#168978 = AXIS2_PLACEMENT_3D ( 'NONE', #48969, #9847, #165072 ) ;
#168979 = CARTESIAN_POINT ( 'NONE',  ( -18.59999999999999787, -4.375386779258390924, -188.8379487402709742 ) ) ;
#168980 = ORIENTED_EDGE ( 'NONE', *, *, #153866, .F. ) ;
#168981 = AXIS2_PLACEMENT_3D ( 'NONE', #130138, #71486, #149740 ) ;
#168982 = CARTESIAN_POINT ( 'NONE',  ( -16.83199030136658081, 60.99007385930059399, -220.9286596726492746 ) ) ;
#168983 = DIRECTION ( 'NONE',  ( 0.000000000000000000, 0.000000000000000000, 1.000000000000000000 ) ) ;
#168984 = VERTEX_POINT ( 'NONE', #169500 ) ;
#168985 = VERTEX_POINT ( 'NONE', #95047 ) ;
#168986 = DIRECTION ( 'NONE',  ( 1.000000000000000000, 0.000000000000000000, 0.000000000000000000 ) ) ;
#168987 = CARTESIAN_POINT ( 'NONE',  ( -18.37013991200266005, 64.50025238380034409, -160.8161304950415627 ) ) ;
#168988 = AXIS2_PLACEMENT_3D ( 'NONE', #126479, #207322, #168220 ) ;
#168989 = DIRECTION ( 'NONE',  ( 0.000000000000000000, 0.000000000000000000, -1.000000000000000000 ) ) ;
#168990 = ORIENTED_EDGE ( 'NONE', *, *, #42119, .F. ) ;
#168991 = CARTESIAN_POINT ( 'NONE',  ( -14.11361717019515893, 9.457426452500060421, -119.0000418684000607 ) ) ;
#168992 = EDGE_CURVE ( 'NONE', #71001, #179208, #205270, .T. ) ;
#168993 = FACE_OUTER_BOUND ( 'NONE', #176554, .T. ) ;
#168994 = CARTESIAN_POINT ( 'NONE',  ( 21.22070241538126467, 0.09891903054618129965, -127.5300537271303938 ) ) ;
#168995 = DIRECTION ( 'NONE',  ( 0.000000000000000000, 0.9126074666063622720, 0.4088369013363611360 ) ) ;
#168996 = EDGE_CURVE ( 'NONE', #147541, #184831, #27928, .T. ) ;
#168997 = TOROIDAL_SURFACE ( 'NONE', #186089, 0.2000000000000000111, 0.1000000000000000056 ) ;
#168998 = VECTOR ( 'NONE', #131675, 1000.000000000000000 ) ;
#168999 = VERTEX_POINT ( 'NONE', #190318 ) ;
#169000 = AXIS2_PLACEMENT_3D ( 'NONE', #193430, #137277, #73497 ) ;
#169001 = DIRECTION ( 'NONE',  ( -1.000000000000000000, 0.000000000000000000, -0.000000000000000000 ) ) ;
#169002 = EDGE_CURVE ( 'NONE', #147671, #17816, #138618, .T. ) ;
#169004 = ORIENTED_EDGE ( 'NONE', *, *, #244060, .T. ) ;
#169003 = CARTESIAN_POINT ( 'NONE',  ( -18.59999999999999787, 67.85909929089923764, -227.8797997985275856 ) ) ;
#169005 = ADVANCED_FACE ( 'NONE', ( #173358 ), #213711, .F. ) ;
#169006 = CYLINDRICAL_SURFACE ( 'NONE', #257605, 11.79999999999999716 ) ;
#169007 = CARTESIAN_POINT ( 'NONE',  ( -23.15000000000000213, 74.08971962617978591, -56.89173962932539297 ) ) ;
#169008 = DIRECTION ( 'NONE',  ( -0.1538461538461510236, 0.9880948137434718559, 0.000000000000000000 ) ) ;
#169009 = CARTESIAN_POINT ( 'NONE',  ( -20.64999999999999858, 68.85000000001228670, -157.6731074845243938 ) ) ;
#169010 = CARTESIAN_POINT ( 'NONE',  ( 21.05000000000000071, 85.40000000001221281, -146.4170766071767389 ) ) ;
#169011 = FACE_OUTER_BOUND ( 'NONE', #16696, .T. ) ;
#169012 = DIRECTION ( 'NONE',  ( 0.000000000000000000, -1.000000000000000000, -2.891205793294679805E-16 ) ) ;
#169013 = ORIENTED_EDGE ( 'NONE', *, *, #199764, .T. ) ;
#169014 = PLANE ( 'NONE',  #130146 ) ;
#169015 = DIRECTION ( 'NONE',  ( 1.000000000000000000, 0.000000000000000000, 0.000000000000000000 ) ) ;
#169016 =( LENGTH_UNIT ( ) NAMED_UNIT ( * ) SI_UNIT ( .MILLI., .METRE. ) );
#169017 = AXIS2_PLACEMENT_3D ( 'NONE', #152903, #168635, #171194 ) ;
#169018 = DIRECTION ( 'NONE',  ( -1.000000000000000000, -0.000000000000000000, 0.000000000000000000 ) ) ;
#169019 = FACE_OUTER_BOUND ( 'NONE', #157402, .T. ) ;
#169020 = EDGE_CURVE ( 'NONE', #210276, #38825, #105292, .T. ) ;
#169021 = EDGE_CURVE ( 'NONE', #217175, #64423, #122093, .T. ) ;
#169022 = VERTEX_POINT ( 'NONE', #92476 ) ;
#169023 = VERTEX_POINT ( 'NONE', #70392 ) ;
#169024 = DIRECTION ( 'NONE',  ( -1.000000000000000000, 0.000000000000000000, 0.000000000000000000 ) ) ;
#169026 = CARTESIAN_POINT ( 'NONE',  ( -20.94999999999999929, 64.35000000001208775, -129.5083017138703667 ) ) ;
#169025 = CIRCLE ( 'NONE', #48176, 0.09999999999999939493 ) ;
#169027 = DIRECTION ( 'NONE',  ( 1.073024830501117725E-15, -6.982962677686266711E-15, 1.000000000000000000 ) ) ;
#169028 = CARTESIAN_POINT ( 'NONE',  ( -20.85000000000000142, 65.66751761918648356, -63.92826094061123143 ) ) ;
#169029 = FACE_OUTER_BOUND ( 'NONE', #160144, .T. ) ;
#169030 = DIRECTION ( 'NONE',  ( -1.000000000000000000, 0.000000000000000000, -0.000000000000000000 ) ) ;
#169031 = EDGE_CURVE ( 'NONE', #124309, #238186, #35119, .T. ) ;
#169032 = CARTESIAN_POINT ( 'NONE',  ( -16.92132318717937522, 9.966070024005926342, -12.62240663035206900 ) ) ;
#169033 = EDGE_CURVE ( 'NONE', #241787, #222282, #208603, .T. ) ;
#169034 = CIRCLE ( 'NONE', #231728, 3.900000000000000799 ) ;
#169035 = VECTOR ( 'NONE', #207805, 1000.000000000000000 ) ;
#169036 = ORIENTED_EDGE ( 'NONE', *, *, #217114, .T. ) ;
#169037 = CARTESIAN_POINT ( 'NONE',  ( -18.43569575749026512, 85.51932773110408448, -62.55013110796496534 ) ) ;
#169038 = ORIENTED_EDGE ( 'NONE', *, *, #170165, .T. ) ;
#169039 = DIRECTION ( 'NONE',  ( 0.000000000000000000, -7.304098846218112382E-15, 1.000000000000000000 ) ) ;
#169040 = LINE ( 'NONE', #248535, #186864 ) ;
#169041 = EDGE_CURVE ( 'NONE', #129423, #46904, #71659, .T. ) ;
#169042 = CARTESIAN_POINT ( 'NONE',  ( -22.50000000000000000, 11.64976291803192154, 0.08880997638692984808 ) ) ;
#169043 = CARTESIAN_POINT ( 'NONE',  ( -18.50000000000000000, 7.476371755685454090, -241.7308184205399471 ) ) ;
#169044 = CARTESIAN_POINT ( 'NONE',  ( 18.36493879433277243, 85.50000080620219478, -62.60095882417268598 ) ) ;
#169045 = CYLINDRICAL_SURFACE ( 'NONE', #85132, 0.09999999999999939493 ) ;
#169046 = EDGE_CURVE ( 'NONE', #257484, #46494, #92856, .T. ) ;
#169047 = ORIENTED_EDGE ( 'NONE', *, *, #245359, .F. ) ;
#169048 = LINE ( 'NONE', #90737, #237147 ) ;
#169049 = DIRECTION ( 'NONE',  ( 0.000000000000000000, 0.2617529984165058998, 0.9651348961777149738 ) ) ;
#169050 = CARTESIAN_POINT ( 'NONE',  ( -16.87036670365548474, 9.989418819312801290, -54.47956011730205006 ) ) ;
#169051 = DIRECTION ( 'NONE',  ( 1.000000000000000000, 0.000000000000000000, 0.000000000000000000 ) ) ;
#169052 = VECTOR ( 'NONE', #193730, 1000.000000000000000 ) ;
#169053 = ADVANCED_FACE ( 'NONE', ( #61047 ), #119774, .F. ) ;
#169054 = AXIS2_PLACEMENT_3D ( 'NONE', #104898, #106201, #9683 ) ;
#169055 = CARTESIAN_POINT ( 'NONE',  ( 18.43709777086141344, 85.68240343348827537, -96.36626410711144786 ) ) ;
#169056 = CIRCLE ( 'NONE', #239757, 4.000000000000003553 ) ;
#169057 = ORIENTED_EDGE ( 'NONE', *, *, #257701, .T. ) ;
#169058 =( BOUNDED_CURVE ( )  B_SPLINE_CURVE ( 3, ( #90425, #249528, #107430, #30486 ),
 .UNSPECIFIED., .F., .F. ) 
 B_SPLINE_CURVE_WITH_KNOTS ( ( 4, 4 ),
 ( 4.712388980384689674, 6.283185307179586232 ),
 .UNSPECIFIED. ) 
 CURVE ( )  GEOMETRIC_REPRESENTATION_ITEM ( )  RATIONAL_B_SPLINE_CURVE ( ( 1.000000000000000000, 0.8047378541243649375, 0.8047378541243649375, 1.000000000000000000 ) ) 
 REPRESENTATION_ITEM ( '' )  );
#169060 = CARTESIAN_POINT ( 'NONE',  ( 23.14999999999999858, 7.980037321000002848, -237.6410835587014390 ) ) ;
#169059 = COLOUR_RGB ( '', 0.31764706, 0.68627451, 0.89019608) ;
#169061 = CARTESIAN_POINT ( 'NONE',  ( -20.64999999999999858, 1.115600667400684642E-11, -134.0000000000000284 ) ) ;
#169062 = ORIENTED_EDGE ( 'NONE', *, *, #85324, .T. ) ;
#169063 = EDGE_CURVE ( 'NONE', #155591, #5814, #117187, .T. ) ;
#169064 = VERTEX_POINT ( 'NONE', #175898 ) ;
#169065 = CARTESIAN_POINT ( 'NONE',  ( -18.59999999999999787, 11.65000000001115232, -146.2500000000000284 ) ) ;
#169066 = CARTESIAN_POINT ( 'NONE',  ( 21.06086055315972416, 11.17039406559869619, -211.0555683265898210 ) ) ;
#169067 = EDGE_CURVE ( 'NONE', #86736, #161343, #200567, .T. ) ;
#169068 = ORIENTED_EDGE ( 'NONE', *, *, #238614, .F. ) ;
#169069 = CARTESIAN_POINT ( 'NONE',  ( 21.04386569057615475, 64.25000000001148237, -42.88027013274464849 ) ) ;
#169070 = FACE_OUTER_BOUND ( 'NONE', #70663, .T. ) ;
#169071 = ORIENTED_EDGE ( 'NONE', *, *, #214551, .T. ) ;
#169072 = AXIS2_PLACEMENT_3D ( 'NONE', #193824, #170455, #72606 ) ;
#169073 = AXIS2_PLACEMENT_3D ( 'NONE', #95946, #153416, #114244 ) ;
#169074 = DIRECTION ( 'NONE',  ( 0.000000000000000000, -1.000000000000000000, -6.982962677686265922E-15 ) ) ;
#169075 = ORIENTED_EDGE ( 'NONE', *, *, #101136, .F. ) ;
#169076 = AXIS2_PLACEMENT_3D ( 'NONE', #47132, #69306, #203668 ) ;
#169077 = CARTESIAN_POINT ( 'NONE',  ( 21.03670563405601968, 10.62482368933940258, -79.32554688620919592 ) ) ;
#169078 = DIRECTION ( 'NONE',  ( 0.000000000000000000, -2.428612866367527723E-14, -1.000000000000000000 ) ) ;
#169080 = VERTEX_POINT ( 'NONE', #255348 ) ;
#169079 = DIRECTION ( 'NONE',  ( 0.000000000000000000, -0.2128009952263403282, 0.9770955615653358350 ) ) ;
#169081 = DIRECTION ( 'NONE',  ( 1.000000000000000000, 0.000000000000000000, 0.000000000000000000 ) ) ;
#169083 = TOROIDAL_SURFACE ( 'NONE', #256466, 0.2000000000000000111, 0.1000000000000000056 ) ;
#169082 = DIRECTION ( 'NONE',  ( -1.000000000000000000, 2.986185139342066933E-16, -6.665775143889695732E-16 ) ) ;
#169084 = DIRECTION ( 'NONE',  ( 1.000000000000000000, -7.304098846218133681E-16, 4.607487905232622991E-31 ) ) ;
#169085 = AXIS2_PLACEMENT_3D ( 'NONE', #224331, #225588, #46959 ) ;
#169086 = DIRECTION ( 'NONE',  ( 0.000000000000000000, 0.9126074666063753726, 0.4088369013363316040 ) ) ;
#169087 = CARTESIAN_POINT ( 'NONE',  ( 18.39999999999999503, 70.35000000001200249, -112.2731074845243313 ) ) ;
#169088 = CARTESIAN_POINT ( 'NONE',  ( 20.94999999999999929, 77.83534155023627932, -91.46795619196130644 ) ) ;
#169089 = CARTESIAN_POINT ( 'NONE',  ( -16.78055652883087134, 66.05322308388694807, -157.3623156469320179 ) ) ;
#169091 = ORIENTED_EDGE ( 'NONE', *, *, #16062, .T. ) ;
#169090 = DIRECTION ( 'NONE',  ( 0.000000000000000000, 0.000000000000000000, 1.000000000000000000 ) ) ;
#169092 = ORIENTED_EDGE ( 'NONE', *, *, #193254, .T. ) ;
#169094 = CARTESIAN_POINT ( 'NONE',  ( -15.75000000000001066, 9.350000000011142731, -83.86426760761615640 ) ) ;
#169093 = DIRECTION ( 'NONE',  ( 0.000000000000000000, 0.000000000000000000, -1.000000000000000000 ) ) ;
#169096 = VERTEX_POINT ( 'NONE', #140582 ) ;
#169095 = CARTESIAN_POINT ( 'NONE',  ( 20.95483826173899899, 8.876166204781142710, -109.0462755528995444 ) ) ;
#169097 = VERTEX_POINT ( 'NONE', #1053 ) ;
#169098 = CARTESIAN_POINT ( 'NONE',  ( 18.79999999999999716, -1.300000000000000044, -7.900000000000000355 ) ) ;
#169099 = DIRECTION ( 'NONE',  ( -0.000000000000000000, -6.982962677686266711E-15, 1.000000000000000000 ) ) ;
#169100 = AXIS2_PLACEMENT_3D ( 'NONE', #92172, #132598, #133867 ) ;
#169101 = AXIS2_PLACEMENT_3D ( 'NONE', #117663, #39448, #141090 ) ;
#169102 = DIRECTION ( 'NONE',  ( 0.000000000000000000, -1.000000000000000000, 0.000000000000000000 ) ) ;
#169103 = DIRECTION ( 'NONE',  ( -3.265361837132813093E-16, -1.000000000000000000, 7.445645354460596589E-46 ) ) ;
#169104 = VECTOR ( 'NONE', #241187, 1000.000000000000000 ) ;
#169105 = CARTESIAN_POINT ( 'NONE',  ( -20.94999999999999929, 74.26374286841446803, -91.45445515550682103 ) ) ;
#169106 = AXIS2_PLACEMENT_3D ( 'NONE', #148775, #165779, #49656 ) ;
#169107 = DIRECTION ( 'NONE',  ( 0.000000000000000000, -0.8814952561688431665, 0.4721928772777346794 ) ) ;
#169108 = DIRECTION ( 'NONE',  ( 0.000000000000000000, -0.2128009952264065807, 0.9770955615653215132 ) ) ;
#169109 = ORIENTED_EDGE ( 'NONE', *, *, #17896, .F. ) ;
#169110 = ORIENTED_EDGE ( 'NONE', *, *, #74182, .T. ) ;
#169111 = EDGE_CURVE ( 'NONE', #220350, #42401, #96313, .T. ) ;
#169112 = DIRECTION ( 'NONE',  ( 0.000000000000000000, 0.9770955615653313941, 0.2128009952263603677 ) ) ;
#169113 = ORIENTED_EDGE ( 'NONE', *, *, #116504, .T. ) ;
#169114 = CARTESIAN_POINT ( 'NONE',  ( -23.25000000000000000, 76.00000000001213607, -136.5231074845242745 ) ) ;
#169115 = ORIENTED_EDGE ( 'NONE', *, *, #220529, .T. ) ;
#169116 = DIRECTION ( 'NONE',  ( 0.000000000000000000, -6.853228547068871147E-15, 1.000000000000000000 ) ) ;
#169117 = CARTESIAN_POINT ( 'NONE',  ( -16.93658623642901873, 9.980381671668284937, -79.61190272912924115 ) ) ;
#169118 = EDGE_CURVE ( 'NONE', #241136, #198612, #76763, .T. ) ;
#169119 = CARTESIAN_POINT ( 'NONE',  ( -20.94999999999999929, 1.261786168576181755, -175.5864989635454378 ) ) ;
#169120 = ORIENTED_EDGE ( 'NONE', *, *, #231932, .T. ) ;
#169121 = DIRECTION ( 'NONE',  ( -1.000000000000000000, 0.000000000000000000, 0.000000000000000000 ) ) ;
#169122 = EDGE_LOOP ( 'NONE', ( #65573, #208288, #84162, #205860, #88324 ) ) ;
#169123 = EDGE_CURVE ( 'NONE', #51994, #59493, #30527, .T. ) ;
#169124 = DIRECTION ( 'NONE',  ( 1.000000000000000000, 0.000000000000000000, 0.000000000000000000 ) ) ;
#169125 = EDGE_CURVE ( 'NONE', #166628, #98827, #55894, .T. ) ;
#169126 = DIRECTION ( 'NONE',  ( 0.000000000000000000, 6.982962677686266711E-15, -1.000000000000000000 ) ) ;
#169127 = CARTESIAN_POINT ( 'NONE',  ( 23.14999999999999858, 76.00000000001213607, -136.5231074845242745 ) ) ;
#169128 = AXIS2_PLACEMENT_3D ( 'NONE', #88358, #149668, #184917 ) ;
#169129 = TOROIDAL_SURFACE ( 'NONE', #227357, 11.70000000000000462, 0.1000000000000000056 ) ;
#169130 = EDGE_LOOP ( 'NONE', ( #35395, #61040, #190416, #119929 ) ) ;
#169131 = DIRECTION ( 'NONE',  ( 1.000000000000000000, -0.000000000000000000, -0.000000000000000000 ) ) ;
#169132 = ORIENTED_EDGE ( 'NONE', *, *, #180289, .F. ) ;
#169135 = VERTEX_POINT ( 'NONE', #220142 ) ;
#169134 = CARTESIAN_POINT ( 'NONE',  ( 23.14999999999999858, 45.73145985849338047, -239.4600911154851133 ) ) ;
#169133 = CARTESIAN_POINT ( 'NONE',  ( -20.54999999999999716, 21.30332930069722863, -233.2143729774842882 ) ) ;
#169136 = CARTESIAN_POINT ( 'NONE',  ( -21.02374657821578197, 64.39999999919137963, -42.95131071432642500 ) ) ;
#169137 = VERTEX_POINT ( 'NONE', #97581 ) ;
#169138 = CARTESIAN_POINT ( 'NONE',  ( -20.65000000000000568, 7.250000000011138646, -143.2500000000000284 ) ) ;
#169139 = ORIENTED_EDGE ( 'NONE', *, *, #116769, .F. ) ;
#169140 = ADVANCED_FACE ( 'NONE', ( #135448 ), #121068, .F. ) ;
#169141 = SPHERICAL_SURFACE ( 'NONE', #57334, 0.1000000000000000056 ) ;
#169142 = DIRECTION ( 'NONE',  ( 1.000000000000000000, 0.000000000000000000, 0.000000000000000000 ) ) ;
#169143 = AXIS2_PLACEMENT_3D ( 'NONE', #186531, #101812, #82246 ) ;
#169144 = CARTESIAN_POINT ( 'NONE',  ( -17.78241384943523684, 53.43976629469171513, -230.1384318238924322 ) ) ;
#169145 = CARTESIAN_POINT ( 'NONE',  ( -21.05000000000000071, 74.16465844978715438, -57.96795619196135618 ) ) ;
#169146 = CIRCLE ( 'NONE', #10722, 0.2000000000000005107 ) ;
#169147 = ORIENTED_EDGE ( 'NONE', *, *, #21113, .T. ) ;
#169148 = CARTESIAN_POINT ( 'NONE',  ( 18.59999999999999432, 74.83729825007462466, -195.4231074845243654 ) ) ;
#169149 = CARTESIAN_POINT ( 'NONE',  ( -20.54999999999999716, 2.500000000011156409, -80.22462192276213955 ) ) ;
#169150 = ORIENTED_EDGE ( 'NONE', *, *, #211954, .T. ) ;
#169151 = CARTESIAN_POINT ( 'NONE',  ( -22.39999999999999858, 1.115600667400684642E-11, -25.70922040162659883 ) ) ;
#169152 = ORIENTED_EDGE ( 'NONE', *, *, #140332, .T. ) ;
#169153 = DIRECTION ( 'NONE',  ( 0.000000000000000000, 0.8814952561688430555, -0.4721928772777346239 ) ) ;
#169154 = VERTEX_POINT ( 'NONE', #80592 ) ;
#169155 = ADVANCED_FACE ( 'NONE', ( #160188 ), #113713, .T. ) ;
#169156 = LINE ( 'NONE', #247363, #201509 ) ;
#169157 = CARTESIAN_POINT ( 'NONE',  ( -22.45437739390954235, 76.00000000001246292, -181.6726782961230811 ) ) ;
#169158 = TOROIDAL_SURFACE ( 'NONE', #214913, 6.258578643762700899, 0.1000000000000000056 ) ;
#169160 = EDGE_LOOP ( 'NONE', ( #116397, #120779, #56876, #237171, #76598 ) ) ;
#169159 = DIRECTION ( 'NONE',  ( 1.000000000000000000, 2.952720810173289112E-16, -0.000000000000000000 ) ) ;
#169161 = CARTESIAN_POINT ( 'NONE',  ( 18.55857864376268296, 63.70395599151300559, -209.2544033210146210 ) ) ;
#169162 = CARTESIAN_POINT ( 'NONE',  ( -15.51798037960204013, 62.79576509294744824, -216.3871738676108976 ) ) ;
#169163 = CARTESIAN_POINT ( 'NONE',  ( -16.84793658983433318, 9.950000000011138823, -113.2336466778105404 ) ) ;
#169165 = EDGE_CURVE ( 'NONE', #144794, #58858, #145619, .T. ) ;
#169164 = EDGE_LOOP ( 'NONE', ( #205422, #246691, #257164, #9886 ) ) ;
#169166 = DIRECTION ( 'NONE',  ( 0.000000000000000000, -1.000000000000000000, 0.000000000000000000 ) ) ;
#169167 = DIRECTION ( 'NONE',  ( 0.000000000000000000, 0.000000000000000000, -1.000000000000000000 ) ) ;
#169168 = EDGE_LOOP ( 'NONE', ( #100742, #239337 ) ) ;
#169169 = CARTESIAN_POINT ( 'NONE',  ( -16.93255653858138388, 9.998451453988312920, -146.5816433679896988 ) ) ;
#169170 = AXIS2_PLACEMENT_3D ( 'NONE', #32656, #91309, #133009 ) ;
#169171 = AXIS2_PLACEMENT_3D ( 'NONE', #251303, #11438, #90954 ) ;
#169172 = AXIS2_PLACEMENT_3D ( 'NONE', #126711, #212677, #253064 ) ;
#169173 = AXIS2_PLACEMENT_3D ( 'NONE', #257093, #38115, #255813 ) ;
#169174 = ORIENTED_EDGE ( 'NONE', *, *, #211626, .T. ) ;
#169175 = CARTESIAN_POINT ( 'NONE',  ( 21.05000000000000071, 75.50266930301991408, -205.3568637872625686 ) ) ;
#169176 = DIRECTION ( 'NONE',  ( -0.000000000000000000, 0.1618390714546030229, 0.9868171638914231547 ) ) ;
#169179 = VERTEX_POINT ( 'NONE', #139285 ) ;
#169178 = ORIENTED_EDGE ( 'NONE', *, *, #168287, .T. ) ;
#169177 = CARTESIAN_POINT ( 'NONE',  ( -20.64999999999999858, 7.150000000011155876, -45.85000000000000142 ) ) ;
#169180 = FACE_OUTER_BOUND ( 'NONE', #257659, .T. ) ;
#169181 = LINE ( 'NONE', #212140, #102380 ) ;
#169182 = CARTESIAN_POINT ( 'NONE',  ( 18.54999999999999716, 44.13548170601889353, -235.2989316066074821 ) ) ;
#169183 = CIRCLE ( 'NONE', #31820, 2.000000000000001776 ) ;
#169185 = CARTESIAN_POINT ( 'NONE',  ( -14.56336952470180002, 66.55335465531629779, -51.11230102842421275 ) ) ;
#169184 = CARTESIAN_POINT ( 'NONE',  ( 21.05000000000000071, -8.730841121484171907, -110.0980747189843640 ) ) ;
#169186 = CARTESIAN_POINT ( 'NONE',  ( -23.49999999999994316, 79.78873604695631627, -7.297728304630792806 ) ) ;
#169187 = DIRECTION ( 'NONE',  ( 0.000000000000000000, -0.9126074666063771490, -0.4088369013363281623 ) ) ;
#169188 = DIRECTION ( 'NONE',  ( -1.000000000000000000, 0.000000000000000000, 0.000000000000000000 ) ) ;
#169189 = CARTESIAN_POINT ( 'NONE',  ( 23.25000000000000000, 69.09936979046463534, -247.6075824278584889 ) ) ;
#169190 = ORIENTED_EDGE ( 'NONE', *, *, #242400, .F. ) ;
#169191 = EDGE_LOOP ( 'NONE', ( #72264, #132288, #96835, #232573 ) ) ;
#169192 = EDGE_CURVE ( 'NONE', #101017, #152480, #102721, .T. ) ;
#169193 = DIRECTION ( 'NONE',  ( -4.408576920032448588E-17, -0.1350103645451807555, -0.9908441862701609093 ) ) ;
#169194 = AXIS2_PLACEMENT_3D ( 'NONE', #162308, #157181, #197555 ) ;
#169195 = EDGE_CURVE ( 'NONE', #100496, #125974, #66195, .T. ) ;
#169197 = EDGE_LOOP ( 'NONE', ( #61884, #52255, #13980, #186814, #238846, #210593, #230200 ) ) ;
#169196 = CARTESIAN_POINT ( 'NONE',  ( -23.15000000000000213, 87.48912529308798014, -106.1231074845242262 ) ) ;
#169198 = ORIENTED_EDGE ( 'NONE', *, *, #243010, .F. ) ;
#169199 = DIRECTION ( 'NONE',  ( -1.020425574104004196E-15, 0.000000000000000000, 1.000000000000000000 ) ) ;
#169200 = ORIENTED_EDGE ( 'NONE', *, *, #172983, .T. ) ;
#169201 = CARTESIAN_POINT ( 'NONE',  ( 21.11344571971300255, 43.49375376562721840, -234.8545817895094387 ) ) ;
#169202 = EDGE_CURVE ( 'NONE', #242362, #232547, #9657, .T. ) ;
#169203 = ADVANCED_FACE ( 'NONE', ( #87009 ), #127452, .T. ) ;
#169204 = VERTEX_POINT ( 'NONE', #44067 ) ;
#169205 = ADVANCED_FACE ( 'NONE', ( #246122 ), #25783, .T. ) ;
#169206 =( NAMED_UNIT ( * ) PLANE_ANGLE_UNIT ( ) SI_UNIT ( $, .RADIAN. ) );
#169207 = CARTESIAN_POINT ( 'NONE',  ( -20.12071067811865888, 9.320710678129810134, -112.8500000000000369 ) ) ;
#169208 = EDGE_CURVE ( 'NONE', #146292, #47640, #143140, .T. ) ;
#169211 = ORIENTED_EDGE ( 'NONE', *, *, #21386, .T. ) ;
#169210 = ORIENTED_EDGE ( 'NONE', *, *, #243296, .T. ) ;
#169209 = AXIS2_PLACEMENT_3D ( 'NONE', #138353, #135795, #253182 ) ;
#169212 = ORIENTED_EDGE ( 'NONE', *, *, #107179, .F. ) ;
#169215 = EDGE_CURVE ( 'NONE', #160332, #158841, #104005, .T. ) ;
#169214 = EDGE_CURVE ( 'NONE', #203569, #1805, #47898, .T. ) ;
#169213 = DIRECTION ( 'NONE',  ( 0.000000000000000000, -0.8660254037844412611, -0.4999999999999956701 ) ) ;
#169216 = EDGE_LOOP ( 'NONE', ( #143743, #170212, #254508, #237708 ) ) ;
#169217 = ORIENTED_EDGE ( 'NONE', *, *, #162500, .F. ) ;
#169218 = FACE_OUTER_BOUND ( 'NONE', #255110, .T. ) ;
#169219 = DIRECTION ( 'NONE',  ( 1.000000000000000000, 0.000000000000000000, 0.000000000000000000 ) ) ;
#169220 = CARTESIAN_POINT ( 'NONE',  ( -22.50000000000000000, 75.90000000001268177, -203.5231074845243597 ) ) ;
#169222 = EDGE_LOOP ( 'NONE', ( #123839, #133054, #184242, #107859 ) ) ;
#169221 = DIRECTION ( 'NONE',  ( 4.239556034732056743E-17, -0.1298341882520022694, -0.9915357197604852679 ) ) ;
#169223 = DIRECTION ( 'NONE',  ( -1.000000000000000000, -0.000000000000000000, -0.000000000000000000 ) ) ;
#169224 = CARTESIAN_POINT ( 'NONE',  ( 23.24999999999999645, 0.000000000000000000, 0.000000000000000000 ) ) ;
#169226 = ORIENTED_EDGE ( 'NONE', *, *, #70521, .F. ) ;
#169225 = FACE_OUTER_BOUND ( 'NONE', #225264, .T. ) ;
#169227 = DIRECTION ( 'NONE',  ( 1.000000000000000000, -0.000000000000000000, -0.000000000000000000 ) ) ;
#169228 = ORIENTED_EDGE ( 'NONE', *, *, #220109, .F. ) ;
#169229 = DIRECTION ( 'NONE',  ( -1.000000000000000000, 0.000000000000000000, -0.000000000000000000 ) ) ;
#169230 = ORIENTED_EDGE ( 'NONE', *, *, #172415, .F. ) ;
#169231 = CARTESIAN_POINT ( 'NONE',  ( 21.07928932188134397, 69.67148334361908724, -170.1220026301787982 ) ) ;
#169233 = EDGE_CURVE ( 'NONE', #169584, #58451, #38705, .T. ) ;
#169232 = DIRECTION ( 'NONE',  ( -0.000000000000000000, 0.9908441862701591329, 0.1350103645451946055 ) ) ;
#169234 = VECTOR ( 'NONE', #49678, 1000.000000000000114 ) ;
#169235 = ORIENTED_EDGE ( 'NONE', *, *, #167134, .F. ) ;
#169237 = CARTESIAN_POINT ( 'NONE',  ( -18.45140287520618116, -9.486077739518409047, -140.6405231266861335 ) ) ;
#169236 = DIRECTION ( 'NONE',  ( 1.000000000000000000, 0.000000000000000000, 0.000000000000000000 ) ) ;
#169238 = EDGE_CURVE ( 'NONE', #149927, #154055, #101187, .T. ) ;
#169239 = EDGE_CURVE ( 'NONE', #95759, #195345, #106579, .T. ) ;
#169240 = DIRECTION ( 'NONE',  ( 0.000000000000000000, -0.9651348961777157509, 0.2617529984165031243 ) ) ;
#169241 = CIRCLE ( 'NONE', #56731, 11.75000000000001066 ) ;
#169242 = CIRCLE ( 'NONE', #127511, 0.2000000000000057288 ) ;
#169243 = CARTESIAN_POINT ( 'NONE',  ( 18.39999999999999503, 64.25000000001188027, -90.37310748452439668 ) ) ;
#169244 = CARTESIAN_POINT ( 'NONE',  ( 23.14999999999999858, -3.899999999988843502, -134.0000000000000284 ) ) ;
#169245 = ORIENTED_EDGE ( 'NONE', *, *, #98480, .F. ) ;
#169246 = ORIENTED_EDGE ( 'NONE', *, *, #44656, .T. ) ;
#169247 = STYLED_ITEM ( 'NONE', ( #36835 ), #241103 ) ;
#169248 = EDGE_CURVE ( 'NONE', #33770, #211794, #184846, .T. ) ;
#169249 = DIRECTION ( 'NONE',  ( 1.000000000000000000, 0.000000000000000000, 0.000000000000000000 ) ) ;
#169250 = EDGE_LOOP ( 'NONE', ( #240965, #237919, #100129, #231061 ) ) ;
#169251 = CARTESIAN_POINT ( 'NONE',  ( -21.05000000000000071, 74.25000000001229239, -158.3535959266227451 ) ) ;
#169252 = ORIENTED_EDGE ( 'NONE', *, *, #108323, .F. ) ;
#169253 = CARTESIAN_POINT ( 'NONE',  ( -21.05000000000000071, 74.14897176987071248, -57.86919421510183525 ) ) ;
#169254 = CARTESIAN_POINT ( 'NONE',  ( -37.88850191057539973, -10.72142460728770352, 6.051435706882140053 ) ) ;
#169255 = EDGE_CURVE ( 'NONE', #89738, #226316, #6204, .T. ) ;
#169256 = FACE_OUTER_BOUND ( 'NONE', #22258, .T. ) ;
#169257 = EDGE_CURVE ( 'NONE', #174422, #73834, #201376, .T. ) ;
#169258 = EDGE_LOOP ( 'NONE', ( #887, #87918 ) ) ;
#169259 = CARTESIAN_POINT ( 'NONE',  ( -16.87372386987899020, 66.11939976637583527, -190.3738376126580363 ) ) ;
#169260 =( LENGTH_UNIT ( ) NAMED_UNIT ( * ) SI_UNIT ( .MILLI., .METRE. ) );
#169261 = AXIS2_PLACEMENT_3D ( 'NONE', #4156, #164536, #49708 ) ;
#169262 = ORIENTED_EDGE ( 'NONE', *, *, #183820, .T. ) ;
#169263 = ORIENTED_EDGE ( 'NONE', *, *, #168237, .F. ) ;
#169264 = CIRCLE ( 'NONE', #194380, 0.09999999999999767408 ) ;
#169265 = ORIENTED_EDGE ( 'NONE', *, *, #131112, .F. ) ;
#169266 = DIRECTION ( 'NONE',  ( -0.000000000000000000, 0.9126074666063770380, 0.4088369013363281068 ) ) ;
#169267 = CARTESIAN_POINT ( 'NONE',  ( 20.94999999999999929, 4.999999999999997335, -21.09473398108690390 ) ) ;
#169268 = DIRECTION ( 'NONE',  ( 1.734723475976817823E-14, 0.9126074666063771490, 0.4088369013363281623 ) ) ;
#169269 = DIRECTION ( 'NONE',  ( -1.000000000000000000, 0.000000000000000000, 0.000000000000000000 ) ) ;
#169270 = CARTESIAN_POINT ( 'NONE',  ( 20.94999999999999574, 5.900000000011102586, -177.7190997646563915 ) ) ;
#169271 = EDGE_CURVE ( 'NONE', #223519, #7738, #30716, .T. ) ;
#169273 = CARTESIAN_POINT ( 'NONE',  ( 21.12802099929860944, 8.780552590222212572, -12.24818998493161892 ) ) ;
#169272 = CARTESIAN_POINT ( 'NONE',  ( -20.85000000000000142, 7.783179459866048866, -245.3643104511423019 ) ) ;
#169275 = ORIENTED_EDGE ( 'NONE', *, *, #112718, .T. ) ;
#169274 = DIRECTION ( 'NONE',  ( -1.000000000000000000, -0.000000000000000000, -0.000000000000000000 ) ) ;
#169276 = CYLINDRICAL_SURFACE ( 'NONE', #86, 0.09999999999999530098 ) ;
#169277 = EDGE_LOOP ( 'NONE', ( #252281, #107371, #83215 ) ) ;
#169278 = AXIS2_PLACEMENT_3D ( 'NONE', #78916, #218435, #158512 ) ;
#169279 = CARTESIAN_POINT ( 'NONE',  ( -16.97683809663752186, 66.15000000001182912, -82.92547150272069700 ) ) ;
#169280 = CIRCLE ( 'NONE', #244223, 0.09999999999999520384 ) ;
#169281 = EDGE_LOOP ( 'NONE', ( #56432, #233069, #151539, #176647 ) ) ;
#169282 = ORIENTED_EDGE ( 'NONE', *, *, #177946, .F. ) ;
#169283 = CARTESIAN_POINT ( 'NONE',  ( -18.59999999999999787, 67.76783854423860021, -227.9206834886612114 ) ) ;
#169284 = DIRECTION ( 'NONE',  ( 1.000000000000000000, 0.000000000000000000, -0.000000000000000000 ) ) ;
#169285 = CARTESIAN_POINT ( 'NONE',  ( 18.49999999999999645, 1.728086936805617757, -120.8844350051678020 ) ) ;
#169286 = CARTESIAN_POINT ( 'NONE',  ( 20.04142135623730070, 64.35000000001245724, -181.7731074845244450 ) ) ;
#169287 = CIRCLE ( 'NONE', #189910, 4.049999999999987388 ) ;
#169288 = LINE ( 'NONE', #207100, #55056 ) ;
#169290 = VERTEX_POINT ( 'NONE', #186142 ) ;
#169289 = VECTOR ( 'NONE', #33286, 1000.000000000000114 ) ;
#169291 = VERTEX_POINT ( 'NONE', #225239 ) ;
#169292 = CIRCLE ( 'NONE', #252430, 0.1000000000000028644 ) ;
#169293 = CYLINDRICAL_SURFACE ( 'NONE', #49020, 0.09999999999999520384 ) ;
#169294 = ORIENTED_EDGE ( 'NONE', *, *, #163722, .F. ) ;
#169295 = CARTESIAN_POINT ( 'NONE',  ( -18.50000000000000000, 21.17283678855158513, -243.7231193059830332 ) ) ;
#169296 = CARTESIAN_POINT ( 'NONE',  ( 20.94999999999999929, 76.00000000001170974, -69.52310748452431710 ) ) ;
#169297 = VERTEX_POINT ( 'NONE', #4904 ) ;
#169298 = CYLINDRICAL_SURFACE ( 'NONE', #140451, 0.1000000000000002554 ) ;
#169299 = CARTESIAN_POINT ( 'NONE',  ( 22.01447462590973458, -1.448975298746754792, -193.8814978911055107 ) ) ;
#169300 = CIRCLE ( 'NONE', #244078, 0.1000000000000028644 ) ;
#169301 = CARTESIAN_POINT ( 'NONE',  ( 18.59999999999999787, -9.849999999999994316, 30.09999999999999787 ) ) ;
#169302 = CYLINDRICAL_SURFACE ( 'NONE', #117576, 2.000000000000001776 ) ;
#169303 = VERTEX_POINT ( 'NONE', #144415 ) ;
#169304 = CARTESIAN_POINT ( 'NONE',  ( -21.05000000000000071, -0.09999999998884338825, -122.3504291924552234 ) ) ;
#169305 = DIRECTION ( 'NONE',  ( 0.000000000000000000, 0.000000000000000000, 1.000000000000000000 ) ) ;
#169306 = DIRECTION ( 'NONE',  ( 1.000000000000000000, 0.000000000000000000, 0.000000000000000000 ) ) ;
#169307 = DIRECTION ( 'NONE',  ( 0.000000000000000000, -1.000000000000000000, 0.000000000000000000 ) ) ;
#169308 = EDGE_CURVE ( 'NONE', #191070, #115218, #88935, .T. ) ;
#169309 = FACE_OUTER_BOUND ( 'NONE', #149600, .T. ) ;
#169310 = AXIS2_PLACEMENT_3D ( 'NONE', #163718, #63312, #5900 ) ;
#169311 = DIRECTION ( 'NONE',  ( 0.000000000000000000, 0.000000000000000000, -1.000000000000000000 ) ) ;
#169312 = EDGE_CURVE ( 'NONE', #119288, #82975, #18034, .T. ) ;
#169313 = ORIENTED_EDGE ( 'NONE', *, *, #160420, .T. ) ;
#169314 = EDGE_CURVE ( 'NONE', #142934, #148718, #222200, .T. ) ;
#169315 = CARTESIAN_POINT ( 'NONE',  ( -16.91049119928363353, 66.05000000001231797, -157.4048278777152632 ) ) ;
#169316 = EDGE_CURVE ( 'NONE', #175937, #211183, #230416, .T. ) ;
#169317 = EDGE_LOOP ( 'NONE', ( #31891, #58021, #152961 ) ) ;
#169318 = CARTESIAN_POINT ( 'NONE',  ( -16.93415306273742260, 14.21635907292751000, -219.3040454656228349 ) ) ;
#169320 = VECTOR ( 'NONE', #188651, 1000.000000000000000 ) ;
#169319 = DIRECTION ( 'NONE',  ( 0.000000000000000000, 0.2617529984165152257, 0.9651348961777124202 ) ) ;
#169322 = EDGE_CURVE ( 'NONE', #77493, #71577, #34801, .T. ) ;
#169321 = CARTESIAN_POINT ( 'NONE',  ( 21.14999999999999858, 12.71802988599559470, -223.5105008658000258 ) ) ;
#169323 = CARTESIAN_POINT ( 'NONE',  ( 20.12518398540832010, 66.02491127934462156, -162.0264392320576974 ) ) ;
#169325 = ORIENTED_EDGE ( 'NONE', *, *, #244213, .T. ) ;
#169324 = AXIS2_PLACEMENT_3D ( 'NONE', #152143, #29635, #213357 ) ;
#169326 = DIRECTION ( 'NONE',  ( 0.5932847527679310229, -0.8049926720990042694, -6.366092712777067056E-16 ) ) ;
#169327 = CARTESIAN_POINT ( 'NONE',  ( -21.05000000000000071, 87.48912529308842068, -167.1231074845242688 ) ) ;
#169328 = AXIS2_PLACEMENT_3D ( 'NONE', #185568, #242963, #6928 ) ;
#169329 = CARTESIAN_POINT ( 'NONE',  ( 20.85000000000000142, 78.48087866980282001, -232.8271061603568910 ) ) ;
#169330 = PLANE ( 'NONE',  #238009 ) ;
#169331 = DIRECTION ( 'NONE',  ( -0.000000000000000000, 0.1350103645451876666, 0.9908441862701600211 ) ) ;
#169332 = CIRCLE ( 'NONE', #198510, 0.09999999999999736877 ) ;
#169333 = EDGE_CURVE ( 'NONE', #18724, #43445, #176459, .T. ) ;
#169334 = ORIENTED_EDGE ( 'NONE', *, *, #9843, .T. ) ;
#169335 = ORIENTED_EDGE ( 'NONE', *, *, #174492, .F. ) ;
#169336 = CYLINDRICAL_SURFACE ( 'NONE', #241531, 0.1000000000000124678 ) ;
#169337 = PLANE ( 'NONE',  #18489 ) ;
#169338 = FACE_OUTER_BOUND ( 'NONE', #242790, .T. ) ;
#169339 = CIRCLE ( 'NONE', #6797, 0.3999999999999975797 ) ;
#169340 = ORIENTED_EDGE ( 'NONE', *, *, #73552, .T. ) ;
#169341 = LINE ( 'NONE', #190159, #26374 ) ;
#169342 = ITEM_DEFINED_TRANSFORMATION ( 'NONE', 'NONE', #161022,  #2425 ) ;
#169343 = VECTOR ( 'NONE', #175413, 1000.000000000000000 ) ;
#169344 = CARTESIAN_POINT ( 'NONE',  ( -20.54999999999999716, 2.000000000011154189, -121.1753780772379230 ) ) ;
#169345 = AXIS2_PLACEMENT_3D ( 'NONE', #160665, #137215, #82344 ) ;
#169346 = VERTEX_POINT ( 'NONE', #148302 ) ;
#169347 = DIRECTION ( 'NONE',  ( 1.000000000000000000, 0.000000000000000000, 0.000000000000000000 ) ) ;
#169348 = EDGE_CURVE ( 'NONE', #111385, #56652, #130459, .T. ) ;
#169349 = ORIENTED_EDGE ( 'NONE', *, *, #85126, .T. ) ;
#169350 = EDGE_LOOP ( 'NONE', ( #44256, #75890, #20383, #9410 ) ) ;
#169351 = TOROIDAL_SURFACE ( 'NONE', #256743, 3.899999999999999467, 0.1000000000000000056 ) ;
#169352 = ORIENTED_EDGE ( 'NONE', *, *, #86375, .F. ) ;
#169353 = CARTESIAN_POINT ( 'NONE',  ( -23.15000000000000213, 71.65000000001228386, -157.6731074845243938 ) ) ;
#169354 = PLANE ( 'NONE',  #71568 ) ;
#169355 = CARTESIAN_POINT ( 'NONE',  ( 21.13461538461538325, 10.61458296203669427, -112.8500000000000369 ) ) ;
#169356 = EDGE_CURVE ( 'NONE', #79096, #99302, #68764, .T. ) ;
#169357 = DIRECTION ( 'NONE',  ( 0.000000000000000000, 0.000000000000000000, -1.000000000000000000 ) ) ;
#169358 = CARTESIAN_POINT ( 'NONE',  ( 20.94999999999999929, 76.00000000001213607, -136.5231074845243313 ) ) ;
#169359 = DIRECTION ( 'NONE',  ( 1.000000000000000000, 2.885090398161910739E-16, 6.283419270304611573E-17 ) ) ;
#169360 = CYLINDRICAL_SURFACE ( 'NONE', #234847, 0.09999999999999939493 ) ;
#169361 = EDGE_CURVE ( 'NONE', #34456, #18989, #132591, .T. ) ;
#169363 = FACE_OUTER_BOUND ( 'NONE', #110850, .T. ) ;
#169362 = LINE ( 'NONE', #248860, #53605 ) ;
#169364 = DIRECTION ( 'NONE',  ( 0.2834754621636439431, -0.2834754621636535465, -0.9161240771326838450 ) ) ;
#169365 = CARTESIAN_POINT ( 'NONE',  ( -16.88219499860498374, 9.950206425438743452, -113.1493096901073443 ) ) ;
#169366 = DIRECTION ( 'NONE',  ( 1.000000000000000000, 2.683427030341247466E-17, -8.429776912874270765E-16 ) ) ;
#169367 = CARTESIAN_POINT ( 'NONE',  ( 20.95576188350343116, 18.84758480880311282, -227.9749056404471332 ) ) ;
#169368 = AXIS2_PLACEMENT_3D ( 'NONE', #244283, #173809, #212883 ) ;
#169369 = EDGE_LOOP ( 'NONE', ( #26429, #174708, #45275, #239246 ) ) ;
#169370 = AXIS2_PLACEMENT_3D ( 'NONE', #231460, #108919, #132337 ) ;
#169371 = EDGE_LOOP ( 'NONE', ( #187839, #246150, #125502, #170068, #239796 ) ) ;
#169372 = AXIS2_PLACEMENT_3D ( 'NONE', #246991, #10966, #189611 ) ;
#169373 = CARTESIAN_POINT ( 'NONE',  ( -18.40000000000000213, -9.682403433476402199, -40.15684337741277687 ) ) ;
#169374 = TOROIDAL_SURFACE ( 'NONE', #131736, 11.70000000000000462, 0.1000000000000000056 ) ;
#169376 = DIRECTION ( 'NONE',  ( -0.000000000000000000, 0.08413937888704771384, -0.9964539953858891908 ) ) ;
#169375 = CARTESIAN_POINT ( 'NONE',  ( 20.02499999999999858, 52.06567329910104291, -231.9654557484363409 ) ) ;
#169377 = EDGE_CURVE ( 'NONE', #87492, #102074, #128743, .T. ) ;
#169378 = LINE ( 'NONE', #203330, #118630 ) ;
#169379 = DIRECTION ( 'NONE',  ( -0.000000000000000000, 1.000000000000000000, 6.982962677686266711E-15 ) ) ;
#169380 = DIRECTION ( 'NONE',  ( -1.000000000000000000, 7.304098846218134667E-16, 2.111765289898285610E-31 ) ) ;
#169381 = ADVANCED_FACE ( 'NONE', ( #170482 ), #9836, .T. ) ;
#169382 = ADVANCED_FACE ( 'NONE', ( #227827 ), #149605, .T. ) ;
#169383 = ORIENTED_EDGE ( 'NONE', *, *, #174786, .F. ) ;
#169384 = EDGE_LOOP ( 'NONE', ( #192506, #226348, #220106, #127239 ) ) ;
#169385 = CARTESIAN_POINT ( 'NONE',  ( -15.15564720441981628, 9.410708747047081602, -18.06920840584410826 ) ) ;
#169386 = EDGE_CURVE ( 'NONE', #44979, #96501, #8790, .T. ) ;
#169387 = ORIENTED_EDGE ( 'NONE', *, *, #55112, .T. ) ;
#169388 = DIRECTION ( 'NONE',  ( -0.000000000000000000, 0.3896596508880098009, 0.9209589331071360574 ) ) ;
#169389 = TOROIDAL_SURFACE ( 'NONE', #86104, 0.4000000000000009104, 0.1000000000000000056 ) ;
#169390 = CIRCLE ( 'NONE', #56871, 0.09999999999999954758 ) ;
#169391 = CARTESIAN_POINT ( 'NONE',  ( 21.08884785362045378, 6.357193367436396514, -133.9502169049331712 ) ) ;
#169392 = CIRCLE ( 'NONE', #252534, 0.8750000000000007772 ) ;
#169393 = ORIENTED_EDGE ( 'NONE', *, *, #203602, .F. ) ;
#169394 = DIRECTION ( 'NONE',  ( 0.000000000000000000, -6.982962677686266711E-15, 1.000000000000000000 ) ) ;
#169395 = EDGE_CURVE ( 'NONE', #74587, #113723, #5540, .T. ) ;
#169396 = ORIENTED_EDGE ( 'NONE', *, *, #39287, .F. ) ;
#169397 = CARTESIAN_POINT ( 'NONE',  ( 18.59999999999998366, 76.00000000001126921, -203.5231074845248997 ) ) ;
#169398 = DIRECTION ( 'NONE',  ( 0.000000000000000000, -1.000000000000000000, 0.000000000000000000 ) ) ;
#169399 = CARTESIAN_POINT ( 'NONE',  ( 22.59999999999999787, 11.64957080755595520, -133.9000000000000057 ) ) ;
#169400 = LINE ( 'NONE', #208505, #129182 ) ;
#169401 = CYLINDRICAL_SURFACE ( 'NONE', #105607, 0.09999999999998898659 ) ;
#169402 = CARTESIAN_POINT ( 'NONE',  ( -18.59999999999999787, 11.75000000001115552, -188.7499999999999716 ) ) ;
#169403 = CARTESIAN_POINT ( 'NONE',  ( -23.15000000000000213, 85.00000000001251976, -179.9170766071767389 ) ) ;
#169404 = CARTESIAN_POINT ( 'NONE',  ( -22.50485643085239573, 64.23176994213648072, -247.2158861856937051 ) ) ;
#169406 = ORIENTED_EDGE ( 'NONE', *, *, #203529, .T. ) ;
#169405 = DIRECTION ( 'NONE',  ( -1.000000000000000000, -0.000000000000000000, -0.000000000000000000 ) ) ;
#169408 = CARTESIAN_POINT ( 'NONE',  ( 20.94999999999999929, 74.16465844978787914, -158.4679561919613775 ) ) ;
#169407 = CARTESIAN_POINT ( 'NONE',  ( 20.85000000000000142, 69.29728574394107454, -247.8047749431123634 ) ) ;
#169409 = EDGE_LOOP ( 'NONE', ( #57625, #227750, #177268, #89205 ) ) ;
#169411 = VERTEX_POINT ( 'NONE', #208287 ) ;
#169410 = CARTESIAN_POINT ( 'NONE',  ( 20.94999999999999574, 74.14897176987143723, -158.3691942151018850 ) ) ;
#169412 = AXIS2_PLACEMENT_3D ( 'NONE', #8509, #160232, #248398 ) ;
#169413 = ORIENTED_EDGE ( 'NONE', *, *, #222561, .T. ) ;
#169414 = DIRECTION ( 'NONE',  ( -1.000000000000000000, -0.000000000000000000, -0.000000000000000000 ) ) ;
#169415 = DIRECTION ( 'NONE',  ( -0.000000000000000000, 0.1298341882519953583, 0.9915357197604862671 ) ) ;
#169416 = DIRECTION ( 'NONE',  ( 1.000000000000000000, 0.000000000000000000, 0.000000000000000000 ) ) ;
#169417 = CARTESIAN_POINT ( 'NONE',  ( -20.64999999999999858, 1.940186915899009490, -46.32911921105333164 ) ) ;
#169419 = LINE ( 'NONE', #248928, #160220 ) ;
#169418 = CIRCLE ( 'NONE', #215161, 0.09999999999999939493 ) ;
#169420 = CARTESIAN_POINT ( 'NONE',  ( -18.59999999999999787, 66.65000000001222702, -148.8731074845244393 ) ) ;
#169421 = CARTESIAN_POINT ( 'NONE',  ( -16.77779411440718249, 51.60854050822252503, -231.9553652180356949 ) ) ;
#169423 = AXIS2_PLACEMENT_3D ( 'NONE', #123151, #218368, #243083 ) ;
#169422 = DIRECTION ( 'NONE',  ( 0.000000000000000000, 0.2211802418851555596, -0.9752329468386637945 ) ) ;
#169424 = ORIENTED_EDGE ( 'NONE', *, *, #132365, .F. ) ;
#169425 = ORIENTED_EDGE ( 'NONE', *, *, #58546, .T. ) ;
#169426 = CARTESIAN_POINT ( 'NONE',  ( -21.05000000000000071, 1.835341550235567887, -45.15515129256298366 ) ) ;
#169427 = AXIS2_PLACEMENT_3D ( 'NONE', #5263, #207363, #246471 ) ;
#169428 = VECTOR ( 'NONE', #73933, 1000.000000000000000 ) ;
#169429 = VERTEX_POINT ( 'NONE', #72633 ) ;
#169430 = CARTESIAN_POINT ( 'NONE',  ( -20.90000000000000213, -11.65000000000000036, 11.89999999999999858 ) ) ;
#169431 = ORIENTED_EDGE ( 'NONE', *, *, #174582, .T. ) ;
#169432 = DIRECTION ( 'NONE',  ( 2.952720810173289112E-16, -1.000000000000000000, 0.000000000000000000 ) ) ;
#169433 = AXIS2_PLACEMENT_3D ( 'NONE', #118941, #1527, #36854 ) ;
#169434 = CARTESIAN_POINT ( 'NONE',  ( -20.00857864376270001, 66.85000000001205933, -124.1731074845243512 ) ) ;
#169435 = CARTESIAN_POINT ( 'NONE',  ( -22.49756042579671700, -2.402844128467869655, -189.6003603154819359 ) ) ;
#169436 = ADVANCED_FACE ( 'NONE', ( #29665 ), #189994, .F. ) ;
#169437 = CARTESIAN_POINT ( 'NONE',  ( -21.05000000000000071, -1.162701749926853712, -142.1000000000000227 ) ) ;
#169438 = CARTESIAN_POINT ( 'NONE',  ( 19.90000000000000568, 1.350000000000000089, 16.60000000000000142 ) ) ;
#169439 = ORIENTED_EDGE ( 'NONE', *, *, #132391, .T. ) ;
#169440 = DIRECTION ( 'NONE',  ( 0.000000000000000000, 0.000000000000000000, 1.000000000000000000 ) ) ;
#169441 = EDGE_CURVE ( 'NONE', #232170, #194376, #126367, .T. ) ;
#169442 = EDGE_CURVE ( 'NONE', #184107, #235379, #184619, .T. ) ;
#169443 = DIRECTION ( 'NONE',  ( 1.000000000000000000, -0.000000000000000000, -0.000000000000000000 ) ) ;
#169444 = DIRECTION ( 'NONE',  ( 1.000000000000000000, -4.625929269271478222E-14, 0.000000000000000000 ) ) ;
#169445 = CARTESIAN_POINT ( 'NONE',  ( -21.05000000000000071, 76.00000000001165290, -69.52310748452431710 ) ) ;
#169446 = CARTESIAN_POINT ( 'NONE',  ( -18.59999999999999787, 70.10000000001193143, -92.80400771986793984 ) ) ;
#169447 = EDGE_LOOP ( 'NONE', ( #16648, #191713, #180392 ) ) ;
#169449 = DIRECTION ( 'NONE',  ( 0.000000000000000000, 0.1480365673253036252, -0.9889818879709278976 ) ) ;
#169448 = CARTESIAN_POINT ( 'NONE',  ( 21.08035267497491105, 61.09867933414660257, -234.2775889333592829 ) ) ;
#169450 = AXIS2_PLACEMENT_3D ( 'NONE', #214194, #237609, #137214 ) ;
#169451 = ORIENTED_EDGE ( 'NONE', *, *, #257661, .F. ) ;
#169454 = ORIENTED_EDGE ( 'NONE', *, *, #209531, .F. ) ;
#169453 = CARTESIAN_POINT ( 'NONE',  ( -16.81931177881023487, 51.55410748565302725, -231.9897278734257497 ) ) ;
#169452 = CARTESIAN_POINT ( 'NONE',  ( 22.39999999999999503, 68.20922040163857503, -103.0231074845243739 ) ) ;
#169455 = DIRECTION ( 'NONE',  ( 0.000000000000000000, -0.1568667991644355497, 0.9876197685951332295 ) ) ;
#169456 = AXIS2_PLACEMENT_3D ( 'NONE', #150505, #65816, #149235 ) ;
#169457 = DIRECTION ( 'NONE',  ( -1.000000000000000000, -0.000000000000000000, -0.000000000000000000 ) ) ;
#169458 = CIRCLE ( 'NONE', #227845, 6.329289321881356400 ) ;
#169459 = DIRECTION ( 'NONE',  ( 0.000000000000000000, 0.2617529984165035684, 0.9651348961777156399 ) ) ;
#169460 = ORIENTED_EDGE ( 'NONE', *, *, #90860, .T. ) ;
#169461 = CYLINDRICAL_SURFACE ( 'NONE', #59503, 0.1000000000000000472 ) ;
#169462 = AXIS2_PLACEMENT_3D ( 'NONE', #175803, #158815, #77949 ) ;
#169463 = EDGE_CURVE ( 'NONE', #230071, #184335, #51734, .T. ) ;
#169464 = DIRECTION ( 'NONE',  ( 0.000000000000000000, 0.000000000000000000, -1.000000000000000000 ) ) ;
#169465 = CIRCLE ( 'NONE', #223377, 0.6000000000000033085 ) ;
#169467 = CARTESIAN_POINT ( 'NONE',  ( -18.69999999999999929, -10.64999999999999325, 31.59999999999999787 ) ) ;
#169466 = CYLINDRICAL_SURFACE ( 'NONE', #130448, 0.1000000000000000472 ) ;
#169468 = VECTOR ( 'NONE', #30347, 1000.000000000000000 ) ;
#169470 = VERTEX_POINT ( 'NONE', #71348 ) ;
#169469 = CARTESIAN_POINT ( 'NONE',  ( -18.59999999999999787, 47.07326788871598211, -255.0992659944397190 ) ) ;
#169471 = ORIENTED_EDGE ( 'NONE', *, *, #113175, .T. ) ;
#169472 = CARTESIAN_POINT ( 'NONE',  ( -17.73285935861322216, 10.85798180380187183, -110.7414381902193270 ) ) ;
#169473 = DIRECTION ( 'NONE',  ( 1.000000000000000000, 0.000000000000000000, 0.000000000000000000 ) ) ;
#169474 = AXIS2_PLACEMENT_3D ( 'NONE', #56561, #254749, #95710 ) ;
#169475 = CARTESIAN_POINT ( 'NONE',  ( 20.27550659511089037, 63.79409916874963216, -213.3197368432687426 ) ) ;
#169476 = ORIENTED_EDGE ( 'NONE', *, *, #34963, .F. ) ;
#169478 = AXIS2_PLACEMENT_3D ( 'NONE', #103464, #241715, #46073 ) ;
#169477 = CARTESIAN_POINT ( 'NONE',  ( 22.39999999999999503, 1.115600667400684642E-11, -155.8504291924551808 ) ) ;
#169479 = VECTOR ( 'NONE', #143979, 1000.000000000000000 ) ;
#169480 = EDGE_CURVE ( 'NONE', #169539, #53590, #30951, .T. ) ;
#169481 = CARTESIAN_POINT ( 'NONE',  ( 18.59999999999999076, 64.35000000001173248, -81.27310748452440237 ) ) ;
#169482 = DIRECTION ( 'NONE',  ( -1.000000000000000000, -0.000000000000000000, 0.000000000000000000 ) ) ;
#169483 = EDGE_CURVE ( 'NONE', #203753, #255048, #247149, .T. ) ;
#169484 = ORIENTED_EDGE ( 'NONE', *, *, #231689, .F. ) ;
#169485 = CARTESIAN_POINT ( 'NONE',  ( 20.97217846901852312, 60.89049786204130044, -225.3271215246448094 ) ) ;
#169486 = VECTOR ( 'NONE', #197387, 1000.000000000000000 ) ;
#169488 = EDGE_CURVE ( 'NONE', #239176, #25217, #251230, .T. ) ;
#169487 = VERTEX_POINT ( 'NONE', #191310 ) ;
#169489 = CYLINDRICAL_SURFACE ( 'NONE', #101432, 0.1000000000000033362 ) ;
#169490 = DIRECTION ( 'NONE',  ( -1.000000000000000000, 2.952720810173289112E-16, 2.061873921506763405E-30 ) ) ;
#169491 = ORIENTED_EDGE ( 'NONE', *, *, #91088, .F. ) ;
#169492 = ORIENTED_EDGE ( 'NONE', *, *, #243746, .T. ) ;
#169493 = CARTESIAN_POINT ( 'NONE',  ( -20.94999999999994600, 87.75000000001122658, -30.02310748452481448 ) ) ;
#169494 = ORIENTED_EDGE ( 'NONE', *, *, #41269, .T. ) ;
#169496 = ORIENTED_EDGE ( 'NONE', *, *, #118348, .F. ) ;
#169495 = CARTESIAN_POINT ( 'NONE',  ( 12.84435279558019971, 66.58929125296548079, -185.4538990786803083 ) ) ;
#169497 = VERTEX_POINT ( 'NONE', #75204 ) ;
#169498 = AXIS2_PLACEMENT_3D ( 'NONE', #200213, #25436, #179381 ) ;
#169499 = AXIS2_PLACEMENT_3D ( 'NONE', #7147, #25455, #243194 ) ;
#169503 = EDGE_CURVE ( 'NONE', #113723, #94186, #22345, .T. ) ;
#169502 = EDGE_LOOP ( 'NONE', ( #45302, #32398, #132314, #81835 ) ) ;
#169501 = ORIENTED_EDGE ( 'NONE', *, *, #161485, .T. ) ;
#169500 = CARTESIAN_POINT ( 'NONE',  ( 20.95512820512820440, 67.12384868372417657, -157.8731074845244109 ) ) ;
#169504 = CIRCLE ( 'NONE', #32110, 0.09999999999999609201 ) ;
#169505 = AXIS2_PLACEMENT_3D ( 'NONE', #133940, #31040, #169269 ) ;
#169506 = CARTESIAN_POINT ( 'NONE',  ( -18.50000000000000000, -9.421290279512154697, -107.3238821790262847 ) ) ;
#169507 = ORIENTED_EDGE ( 'NONE', *, *, #156048, .F. ) ;
#169508 = DIRECTION ( 'NONE',  ( 0.000000000000000000, -1.000000000000000000, -6.982962677686266711E-15 ) ) ;
#169509 = CARTESIAN_POINT ( 'NONE',  ( -20.94999999999999929, 76.00000000001142553, -36.02310748452432421 ) ) ;
#169510 = LINE ( 'NONE', #209890, #147374 ) ;
#169511 = CIRCLE ( 'NONE', #202778, 0.1000000000000028644 ) ;
#169512 = DIRECTION ( 'NONE',  ( 0.000000000000000000, -0.9126074666063770380, -0.4088369013363281068 ) ) ;
#169513 = ORIENTED_EDGE ( 'NONE', *, *, #226241, .T. ) ;
#169514 = ORIENTED_EDGE ( 'NONE', *, *, #151196, .T. ) ;
#169515 = EDGE_CURVE ( 'NONE', #178868, #168923, #113895, .T. ) ;
#169516 = DIRECTION ( 'NONE',  ( -0.000000000000000000, -0.000000000000000000, -1.000000000000000000 ) ) ;
#169518 = ORIENTED_EDGE ( 'NONE', *, *, #28964, .F. ) ;
#169517 = CARTESIAN_POINT ( 'NONE',  ( 18.49999999999999289, 63.68186668325585487, -209.1448000494835355 ) ) ;
#169519 = DIRECTION ( 'NONE',  ( 0.000000000000000000, 0.000000000000000000, -1.000000000000000000 ) ) ;
#169521 = ORIENTED_EDGE ( 'NONE', *, *, #29363, .T. ) ;
#169520 = DIRECTION ( 'NONE',  ( -1.000000000000000000, 0.000000000000000000, 0.000000000000000000 ) ) ;
#169522 = AXIS2_PLACEMENT_3D ( 'NONE', #73369, #74665, #249416 ) ;
#169523 = ORIENTED_EDGE ( 'NONE', *, *, #198285, .T. ) ;
#169524 = DIRECTION ( 'NONE',  ( 1.000000000000000000, 0.000000000000000000, 0.000000000000000000 ) ) ;
#169525 = EDGE_CURVE ( 'NONE', #22291, #88637, #163789, .T. ) ;
#169526 = EDGE_CURVE ( 'NONE', #40984, #84132, #55575, .T. ) ;
#169527 = VECTOR ( 'NONE', #189067, 1000.000000000000000 ) ;
#169528 = AXIS2_PLACEMENT_3D ( 'NONE', #10253, #92339, #91061 ) ;
#169529 = EDGE_LOOP ( 'NONE', ( #54352, #153631, #242286, #89108, #64982 ) ) ;
#169530 = DIRECTION ( 'NONE',  ( 0.000000000000000000, -0.4721928772777346239, -0.8814952561688430555 ) ) ;
#169531 = CIRCLE ( 'NONE', #69919, 11.79999999999999893 ) ;
#169532 = ADVANCED_FACE ( 'NONE', ( #138965 ), #122276, .F. ) ;
#169534 = VERTEX_POINT ( 'NONE', #16507 ) ;
#169533 = ORIENTED_EDGE ( 'NONE', *, *, #45027, .F. ) ;
#169535 = ORIENTED_EDGE ( 'NONE', *, *, #56272, .F. ) ;
#169537 = EDGE_CURVE ( 'NONE', #96642, #198075, #257601, .T. ) ;
#169536 = CARTESIAN_POINT ( 'NONE',  ( -16.94226253665225457, 9.950000000011137047, -54.05326540438422711 ) ) ;
#169538 = VERTEX_POINT ( 'NONE', #20363 ) ;
#169539 = VERTEX_POINT ( 'NONE', #56860 ) ;
#169540 = FACE_OUTER_BOUND ( 'NONE', #30704, .T. ) ;
#169542 = VERTEX_POINT ( 'NONE', #217232 ) ;
#169541 = CARTESIAN_POINT ( 'NONE',  ( -21.06715728752538297, 18.86061765788380740, -226.6874733728450053 ) ) ;
#169543 = DIRECTION ( 'NONE',  ( -1.000000000000000000, -0.000000000000000000, 0.000000000000000000 ) ) ;
#169544 = ADVANCED_FACE ( 'NONE', ( #154740 ), #78996, .T. ) ;
#169545 = CARTESIAN_POINT ( 'NONE',  ( 15.74999999999999645, 66.15000000001204228, -119.7731074845243739 ) ) ;
#169546 = DIRECTION ( 'NONE',  ( 0.000000000000000000, 1.000000000000000000, 0.000000000000000000 ) ) ;
#169547 = CARTESIAN_POINT ( 'NONE',  ( -18.35668295345803713, 11.47316190337362940, -191.7499999999999716 ) ) ;
#169548 = ORIENTED_EDGE ( 'NONE', *, *, #12477, .F. ) ;
#169549 = ORIENTED_EDGE ( 'NONE', *, *, #70304, .T. ) ;
#169550 = CARTESIAN_POINT ( 'NONE',  ( -23.15000000000000213, 67.23127455305841238, -235.8551265064783991 ) ) ;
#169552 = EDGE_CURVE ( 'NONE', #79511, #55514, #151335, .T. ) ;
#169551 = LINE ( 'NONE', #11737, #120306 ) ;
#169553 = ORIENTED_EDGE ( 'NONE', *, *, #150799, .T. ) ;
#169554 = VECTOR ( 'NONE', #167060, 1000.000000000000000 ) ;
#169555 = VECTOR ( 'NONE', #236272, 1000.000000000000114 ) ;
#169557 = EDGE_CURVE ( 'NONE', #123645, #210461, #255028, .T. ) ;
#169556 = VECTOR ( 'NONE', #120371, 1000.000000000000000 ) ;
#169558 = AXIS2_PLACEMENT_3D ( 'NONE', #110205, #128502, #50224 ) ;
#169559 = ADVANCED_FACE ( 'NONE', ( #60727, #140262, #256310, #179434, #236807 ), #235522, .T. ) ;
#169560 = DIRECTION ( 'NONE',  ( 1.000000000000000000, 0.000000000000000000, -0.000000000000000000 ) ) ;
#169561 = ORIENTED_EDGE ( 'NONE', *, *, #160313, .F. ) ;
#169562 = ORIENTED_EDGE ( 'NONE', *, *, #17567, .T. ) ;
#169563 = EDGE_CURVE ( 'NONE', #75472, #71835, #193850, .T. ) ;
#169564 = CARTESIAN_POINT ( 'NONE',  ( -21.05000000000000071, 64.36312671090855986, -196.7013482711997199 ) ) ;
#169565 = CARTESIAN_POINT ( 'NONE',  ( -18.59999999999999787, -1.261786168553869603, -175.5864989635454378 ) ) ;
#169566 = ORIENTED_EDGE ( 'NONE', *, *, #63995, .T. ) ;
#169567 = PLANE ( 'NONE',  #134665 ) ;
#169568 = ORIENTED_EDGE ( 'NONE', *, *, #180986, .F. ) ;
#169569 = CARTESIAN_POINT ( 'NONE',  ( 18.31572054635717706, -9.548475435767914021, -140.8505701647482056 ) ) ;
#169570 = CARTESIAN_POINT ( 'NONE',  ( -20.65000000000000568, 68.75000000001189449, -93.77310748452435973 ) ) ;
#169572 = DIRECTION ( 'NONE',  ( 0.000000000000000000, 0.000000000000000000, -1.000000000000000000 ) ) ;
#169571 = LINE ( 'NONE', #249080, #3174 ) ;
#169573 = CARTESIAN_POINT ( 'NONE',  ( -16.93388492042257454, 9.988541822527057690, -87.90054512318621960 ) ) ;
#169574 = ADVANCED_FACE ( 'NONE', ( #15221 ), #156024, .F. ) ;
#169575 = LINE ( 'NONE', #127843, #53485 ) ;
#169577 = EDGE_CURVE ( 'NONE', #122251, #181466, #155628, .T. ) ;
#169576 = CARTESIAN_POINT ( 'NONE',  ( -23.25000000000000000, 1.115651490242849210E-11, -163.3499999999999943 ) ) ;
#169578 = DIRECTION ( 'NONE',  ( 0.000000000000000000, 0.000000000000000000, 1.000000000000000000 ) ) ;
#169579 = AXIS2_PLACEMENT_3D ( 'NONE', #190797, #211619, #111227 ) ;
#169580 = EDGE_CURVE ( 'NONE', #237061, #10791, #204740, .T. ) ;
#169581 = VECTOR ( 'NONE', #5665, 1000.000000000000000 ) ;
#169582 = VECTOR ( 'NONE', #211635, 1000.000000000000000 ) ;
#169584 = VERTEX_POINT ( 'NONE', #184535 ) ;
#169583 = CARTESIAN_POINT ( 'NONE',  ( 20.85000000000000142, -1.835859311432481045, -78.50443916879852679 ) ) ;
#169586 = EDGE_LOOP ( 'NONE', ( #210191, #157393, #39902, #248706 ) ) ;
#169585 = ORIENTED_EDGE ( 'NONE', *, *, #12990, .T. ) ;
#169587 = AXIS2_PLACEMENT_3D ( 'NONE', #154652, #93355, #13831 ) ;
#169588 = EDGE_LOOP ( 'NONE', ( #76543, #107913, #257527, #54632 ) ) ;
#169589 = DIRECTION ( 'NONE',  ( -1.000000000000000000, 0.000000000000000000, -0.000000000000000000 ) ) ;
#169590 = FACE_OUTER_BOUND ( 'NONE', #195207, .T. ) ;
#169591 = EDGE_CURVE ( 'NONE', #24915, #175784, #68108, .T. ) ;
#169592 = DIRECTION ( 'NONE',  ( 0.000000000000000000, 1.224646799142185182E-16, 1.000000000000000000 ) ) ;
#169593 = EDGE_CURVE ( 'NONE', #237924, #123705, #213853, .T. ) ;
#169594 = CARTESIAN_POINT ( 'NONE',  ( -18.40000000000000213, 45.89348038176515843, -239.2231437130149061 ) ) ;
#169595 = ORIENTED_EDGE ( 'NONE', *, *, #110945, .F. ) ;
#169597 = B_SPLINE_CURVE_WITH_KNOTS ( 'NONE', 3,
 ( #220232, #81948, #98951, #1143, #178554, #239787 ),
 .UNSPECIFIED., .F., .F.,
 ( 4, 2, 4 ),
 ( 0.000000000000000000, 0.0001568709654583423218, 0.0003137419309166846436 ),
 .UNSPECIFIED. ) ;
#169596 = FACE_OUTER_BOUND ( 'NONE', #173287, .T. ) ;
#169598 = ORIENTED_EDGE ( 'NONE', *, *, #122687, .F. ) ;
#169599 = LINE ( 'NONE', #86122, #237575 ) ;
#169600 = CARTESIAN_POINT ( 'NONE',  ( -22.49756042579671700, 0.07804633702833754794, -88.85013503889771869 ) ) ;
#169601 = CARTESIAN_POINT ( 'NONE',  ( -21.13422380239047982, 1.404996820536673185, -230.6665987823094781 ) ) ;
#169602 = ORIENTED_EDGE ( 'NONE', *, *, #234304, .F. ) ;
#169603 = VECTOR ( 'NONE', #32946, 1000.000000000000000 ) ;
#169604 = DIRECTION ( 'NONE',  ( 1.000000000000000000, 0.000000000000000000, -0.000000000000000000 ) ) ;
#169605 = CARTESIAN_POINT ( 'NONE',  ( -18.59999999999999787, -1.851028230129704522, -45.15391326942249606 ) ) ;
#169606 = VERTEX_POINT ( 'NONE', #106271 ) ;
#169607 = ORIENTED_EDGE ( 'NONE', *, *, #129068, .T. ) ;
#169608 = CARTESIAN_POINT ( 'NONE',  ( 19.97071067811864609, 64.27928932189311695, -78.37310748452439668 ) ) ;
#169609 = DIRECTION ( 'NONE',  ( -1.000000000000000000, 0.000000000000000000, 0.000000000000000000 ) ) ;
#169610 = CARTESIAN_POINT ( 'NONE',  ( 21.05000000000000071, 87.65000000001194280, -103.0231074845242318 ) ) ;
#169611 = DIRECTION ( 'NONE',  ( 1.000000000000000000, 0.000000000000000000, 0.000000000000000000 ) ) ;
#169612 = DIRECTION ( 'NONE',  ( 0.000000000000000000, 0.2617529984165031243, 0.9651348961777157509 ) ) ;
#169613 = AXIS2_PLACEMENT_3D ( 'NONE', #213212, #132416, #230223 ) ;
#169614 = CARTESIAN_POINT ( 'NONE',  ( -21.11825140030074621, 6.445407565420032014, 0.007203620632664132876 ) ) ;
#169615 = ORIENTED_EDGE ( 'NONE', *, *, #203519, .F. ) ;
#169616 = DIRECTION ( 'NONE',  ( 1.000000000000000000, 0.000000000000000000, 0.000000000000000000 ) ) ;
#169617 = DIRECTION ( 'NONE',  ( 1.000000000000000000, 0.000000000000000000, 0.000000000000000000 ) ) ;
#169619 = CARTESIAN_POINT ( 'NONE',  ( -20.95613430942402644, 11.75000000001115552, -174.3571626482202817 ) ) ;
#169618 = DIRECTION ( 'NONE',  ( 0.000000000000000000, 1.000000000000000000, 0.000000000000000000 ) ) ;
#169620 = AXIS2_PLACEMENT_3D ( 'NONE', #56429, #117701, #201091 ) ;
#169621 = LINE ( 'NONE', #49622, #249982 ) ;
#169622 = EDGE_CURVE ( 'NONE', #89559, #5154, #145412, .T. ) ;
#169623 = DIRECTION ( 'NONE',  ( -1.000000000000000000, 1.652117596168391700E-15, 0.000000000000000000 ) ) ;
#169624 = DIRECTION ( 'NONE',  ( 0.000000000000000000, 0.000000000000000000, 1.000000000000000000 ) ) ;
#169625 = VECTOR ( 'NONE', #214599, 1000.000000000000000 ) ;
#169627 = VERTEX_POINT ( 'NONE', #45038 ) ;
#169626 = FACE_OUTER_BOUND ( 'NONE', #115825, .T. ) ;
#169628 = AXIS2_PLACEMENT_3D ( 'NONE', #233365, #108570, #54690 ) ;
#169629 = EDGE_CURVE ( 'NONE', #185332, #96541, #255494, .T. ) ;
#169630 = PRODUCT_DEFINITION_FORMATION_WITH_SPECIFIED_SOURCE ( 'ANY', '', #28562, .NOT_KNOWN. ) ;
#169631 = AXIS2_PLACEMENT_3D ( 'NONE', #18112, #216305, #238446 ) ;
#169632 = AXIS2_PLACEMENT_3D ( 'NONE', #116982, #101217, #97377 ) ;
#169633 = DIRECTION ( 'NONE',  ( -1.000000000000000000, 2.952720810173289112E-16, 2.061873921506763405E-30 ) ) ;
#169634 = DIRECTION ( 'NONE',  ( 1.000000000000000000, 0.000000000000000000, 0.000000000000000000 ) ) ;
#169635 = EDGE_CURVE ( 'NONE', #24156, #250150, #138979, .T. ) ;
#169636 = PLANE ( 'NONE',  #87966 ) ;
#169637 = CIRCLE ( 'NONE', #240331, 0.1000000000000124678 ) ;
#169638 = EDGE_LOOP ( 'NONE', ( #30975, #182536, #250203, #178735 ) ) ;
#169639 = DIRECTION ( 'NONE',  ( 0.000000000000000000, -0.5000000000000209832, -0.8660254037844264952 ) ) ;
#169640 = AXIS2_PLACEMENT_3D ( 'NONE', #75184, #94711, #252496 ) ;
#169641 = CARTESIAN_POINT ( 'NONE',  ( 27.30103769104855971, 12.20000000000000284, -347.0000000000001137 ) ) ;
#169642 = DIRECTION ( 'NONE',  ( 0.000000000000000000, 0.2128009952263603677, -0.9770955615653313941 ) ) ;
#169643 = AXIS2_PLACEMENT_3D ( 'NONE', #27467, #165669, #106941 ) ;
#169644 = ORIENTED_EDGE ( 'NONE', *, *, #163180, .F. ) ;
#169645 = DIRECTION ( 'NONE',  ( 1.000000000000000000, -3.265361837132813093E-16, -2.280189983783949500E-30 ) ) ;
#169648 = ORIENTED_EDGE ( 'NONE', *, *, #96205, .T. ) ;
#169647 = DIRECTION ( 'NONE',  ( 1.000000000000000000, 0.000000000000000000, 0.000000000000000000 ) ) ;
#169646 = AXIS2_PLACEMENT_3D ( 'NONE', #233848, #158205, #137298 ) ;
#169649 = DIRECTION ( 'NONE',  ( -1.000000000000000000, 0.000000000000000000, 0.000000000000000000 ) ) ;
#169650 = DIRECTION ( 'NONE',  ( 0.000000000000000000, -1.000000000000000000, 0.000000000000000000 ) ) ;
#169651 = ORIENTED_EDGE ( 'NONE', *, *, #119205, .F. ) ;
#169652 = DIRECTION ( 'NONE',  ( 0.000000000000000000, -1.000000000000000000, 0.000000000000000000 ) ) ;
#169653 = SHAPE_DEFINITION_REPRESENTATION ( #224130, #198303 ) ;
#169654 = CARTESIAN_POINT ( 'NONE',  ( -18.59999999999999787, 8.980461154494397746, -187.0187154576991304 ) ) ;
#169655 = CARTESIAN_POINT ( 'NONE',  ( -21.93642651522410247, 68.67283376068687062, -203.5231074845243882 ) ) ;
#169656 = CARTESIAN_POINT ( 'NONE',  ( -18.43599941264914222, 85.51932742860660142, -96.05013069500279244 ) ) ;
#169657 = ORIENTED_EDGE ( 'NONE', *, *, #173647, .F. ) ;
#169658 = DIRECTION ( 'NONE',  ( 0.000000000000000000, -0.8814952561688476074, 0.4721928772777262417 ) ) ;
#169659 = CARTESIAN_POINT ( 'NONE',  ( -21.05000000000000071, 76.00000000001263345, -195.6231074845243540 ) ) ;
#169660 = AXIS2_PLACEMENT_3D ( 'NONE', #131677, #225613, #207382 ) ;
#169661 = CIRCLE ( 'NONE', #82277, 0.1000000000000000472 ) ;
#169662 = VECTOR ( 'NONE', #132712, 1000.000000000000000 ) ;
#169663 = CARTESIAN_POINT ( 'NONE',  ( 20.94999999999999574, 8.926614585098251453, -175.9716830192230930 ) ) ;
#169664 = EDGE_LOOP ( 'NONE', ( #225163, #50677, #116147, #23152 ) ) ;
#169665 = EDGE_LOOP ( 'NONE', ( #57417, #177203, #216767, #128276 ) ) ;
#169666 = DIRECTION ( 'NONE',  ( 1.000000000000000000, 0.000000000000000000, 0.000000000000000000 ) ) ;
#169667 = EDGE_CURVE ( 'NONE', #211462, #75088, #222356, .T. ) ;
#169668 = DIRECTION ( 'NONE',  ( 0.000000000000000000, -6.982962677686266711E-15, 1.000000000000000000 ) ) ;
#169670 = AXIS2_PLACEMENT_3D ( 'NONE', #43178, #247788, #148707 ) ;
#169669 = LINE ( 'NONE', #70555, #85880 ) ;
#169671 = CARTESIAN_POINT ( 'NONE',  ( 21.04999999999999716, 8.871279686006799281, -146.1500000000000341 ) ) ;
#169672 = EDGE_CURVE ( 'NONE', #237026, #188354, #197280, .T. ) ;
#169673 = AXIS2_PLACEMENT_3D ( 'NONE', #2729, #120172, #185240 ) ;
#169675 = CARTESIAN_POINT ( 'NONE',  ( 22.42196299218230493, -2.476663215497191040, -189.6166965207286523 ) ) ;
#169674 = CARTESIAN_POINT ( 'NONE',  ( -20.94999999999999929, 64.25000000001161027, -62.50830171387040934 ) ) ;
#169676 = CARTESIAN_POINT ( 'NONE',  ( -21.07928932188134041, 75.90110485435802445, -176.3516241409176644 ) ) ;
#169677 = CARTESIAN_POINT ( 'NONE',  ( 20.85000000000000142, 11.65000000001115943, -60.21613433702191287 ) ) ;
#169678 = CARTESIAN_POINT ( 'NONE',  ( -20.54999999999999716, 87.75000000001205080, -124.1731074845242233 ) ) ;
#169679 = ORIENTED_EDGE ( 'NONE', *, *, #245669, .F. ) ;
#169681 = ORIENTED_EDGE ( 'NONE', *, *, #248639, .F. ) ;
#169680 = CARTESIAN_POINT ( 'NONE',  ( 12.33938619321247820, 62.72888572355475389, -216.6946536606585880 ) ) ;
#169682 = CARTESIAN_POINT ( 'NONE',  ( 23.15000000000000213, 87.65000000001246860, -173.1231074845242688 ) ) ;
#169684 = DIRECTION ( 'NONE',  ( -1.000000000000000000, 0.000000000000000000, 0.000000000000000000 ) ) ;
#169683 = DIRECTION ( 'NONE',  ( 0.000000000000000000, 0.4088369013363281623, -0.9126074666063771490 ) ) ;
#169685 = AXIS2_PLACEMENT_3D ( 'NONE', #29674, #84428, #126156 ) ;
#169686 = ADVANCED_FACE ( 'NONE', ( #162439 ), #62047, .T. ) ;
#169687 = ORIENTED_EDGE ( 'NONE', *, *, #237461, .F. ) ;
#169688 = DIRECTION ( 'NONE',  ( -1.000000000000000000, -2.952720810173289112E-16, 0.000000000000000000 ) ) ;
#169689 = CARTESIAN_POINT ( 'NONE',  ( -20.64999999999999858, 1.115600667400684642E-11, -121.1250000000000426 ) ) ;
#169690 = DIRECTION ( 'NONE',  ( 1.000000000000000000, -0.000000000000000000, -0.000000000000000000 ) ) ;
#169691 = CYLINDRICAL_SURFACE ( 'NONE', #239624, 0.1000000000000028644 ) ;
#169692 = EDGE_CURVE ( 'NONE', #41329, #229500, #181990, .T. ) ;
#169693 = ORIENTED_EDGE ( 'NONE', *, *, #48951, .F. ) ;
#169694 = ORIENTED_EDGE ( 'NONE', *, *, #65832, .F. ) ;
#169695 = AXIS2_PLACEMENT_3D ( 'NONE', #122970, #121696, #1711 ) ;
#169696 = CIRCLE ( 'NONE', #107279, 3.899999999999999467 ) ;
#169697 = AXIS2_PLACEMENT_3D ( 'NONE', #53127, #51823, #131379 ) ;
#169698 = CARTESIAN_POINT ( 'NONE',  ( 21.05000000000000426, 6.413826288824126642, -100.5857409370334636 ) ) ;
#169699 = EDGE_CURVE ( 'NONE', #197777, #90989, #84822, .T. ) ;
#169700 = ORIENTED_EDGE ( 'NONE', *, *, #37427, .T. ) ;
#169701 = CARTESIAN_POINT ( 'NONE',  ( 21.05000000000005400, 64.35000000001120668, -3.023107484524792277 ) ) ;
#169702 = AXIS2_PLACEMENT_3D ( 'NONE', #144446, #101446, #45371 ) ;
#169703 = FACE_OUTER_BOUND ( 'NONE', #20115, .T. ) ;
#169704 = CARTESIAN_POINT ( 'NONE',  ( -18.59999999999999787, 1.115600667400684642E-11, -167.5000000000000284 ) ) ;
#169705 = VERTEX_POINT ( 'NONE', #241949 ) ;
#169706 = ADVANCED_FACE ( 'NONE', ( #163709 ), #180709, .T. ) ;
#169707 = CARTESIAN_POINT ( 'NONE',  ( -20.00857864376270001, 9.250000000000001776, -21.15000000000000213 ) ) ;
#169708 = DIRECTION ( 'NONE',  ( 1.000000000000000000, 7.304098846218134667E-16, -0.000000000000000000 ) ) ;
#169709 = AXIS2_PLACEMENT_3D ( 'NONE', #38797, #115758, #118339 ) ;
#169710 = CARTESIAN_POINT ( 'NONE',  ( -23.25000000000000355, 70.35000000001181775, -82.17310748452435121 ) ) ;
#169711 = DIRECTION ( 'NONE',  ( 0.000000000000000000, 0.000000000000000000, -1.000000000000000000 ) ) ;
#169712 = DIRECTION ( 'NONE',  ( 2.952720810173289112E-16, 1.000000000000000000, -6.088138035986627436E-46 ) ) ;
#169713 = CARTESIAN_POINT ( 'NONE',  ( -16.87998658237729188, 66.05000000001223270, -149.3867470522638143 ) ) ;
#169714 = ORIENTED_EDGE ( 'NONE', *, *, #148438, .T. ) ;
#169716 = SPHERICAL_SURFACE ( 'NONE', #84936, 0.1000000000000000056 ) ;
#169715 = CARTESIAN_POINT ( 'NONE',  ( -16.98495255085919098, 10.00556436599476662, -12.63461720622050599 ) ) ;
#169717 = ORIENTED_EDGE ( 'NONE', *, *, #19987, .F. ) ;
#169719 = VERTEX_POINT ( 'NONE', #104968 ) ;
#169718 = DIRECTION ( 'NONE',  ( 0.000000000000000000, -0.2128009952263603954, 0.9770955615653315052 ) ) ;
#169720 = CIRCLE ( 'NONE', #136514, 0.1999999999999985401 ) ;
#169721 = ORIENTED_EDGE ( 'NONE', *, *, #128643, .T. ) ;
#169722 = CARTESIAN_POINT ( 'NONE',  ( -18.39418127959864790, 11.48390560170929220, -91.25000000000005684 ) ) ;
#169723 = DIRECTION ( 'NONE',  ( 1.000000000000000000, 0.000000000000000000, 0.000000000000000000 ) ) ;
#169724 = CARTESIAN_POINT ( 'NONE',  ( -23.49999999999994316, 86.36484105039212977, -51.23044614117323903 ) ) ;
#169725 = DIRECTION ( 'NONE',  ( 1.000000000000000000, 0.000000000000000000, 0.000000000000000000 ) ) ;
#169726 = ORIENTED_EDGE ( 'NONE', *, *, #97630, .F. ) ;
#169727 = DIRECTION ( 'NONE',  ( -1.000000000000000000, 0.000000000000000000, 0.000000000000000000 ) ) ;
#169728 = DIRECTION ( 'NONE',  ( 0.000000000000000000, -1.000000000000000000, 0.000000000000000000 ) ) ;
#169729 = EDGE_LOOP ( 'NONE', ( #166296, #120599, #208253, #8629 ) ) ;
#169730 = DIRECTION ( 'NONE',  ( 1.000000000000000000, 0.000000000000000000, 0.000000000000000000 ) ) ;
#169731 = DIRECTION ( 'NONE',  ( -0.000000000000000000, -1.000000000000000000, 6.308085367188393199E-16 ) ) ;
#169732 = EDGE_LOOP ( 'NONE', ( #122005, #253837, #152991, #101730 ) ) ;
#169733 = AXIS2_PLACEMENT_3D ( 'NONE', #90997, #233107, #89701 ) ;
#169734 = CARTESIAN_POINT ( 'NONE',  ( 23.14999999999999858, 64.35000000001218723, -143.5379132551783812 ) ) ;
#169735 = CIRCLE ( 'NONE', #157243, 4.300000000000039790 ) ;
#169736 = ADVANCED_FACE ( 'NONE', ( #245814 ), #244512, .F. ) ;
#169737 = ORIENTED_EDGE ( 'NONE', *, *, #181317, .F. ) ;
#169738 = DIRECTION ( 'NONE',  ( 0.000000000000000000, 0.000000000000000000, 1.000000000000000000 ) ) ;
#169739 = ORIENTED_EDGE ( 'NONE', *, *, #167151, .T. ) ;
#169740 = LINE ( 'NONE', #148870, #241942 ) ;
#169741 = CARTESIAN_POINT ( 'NONE',  ( 21.04999999999999716, 64.25000000001175238, -76.36470817442145176 ) ) ;
#169742 = CARTESIAN_POINT ( 'NONE',  ( -16.97683809663752186, 66.05000000001155058, -49.42547150272071121 ) ) ;
#169743 = EDGE_CURVE ( 'NONE', #105073, #192971, #95727, .T. ) ;
#169744 = CARTESIAN_POINT ( 'NONE',  ( -21.64999999999999858, 7.350000000011155166, -112.7500000000000284 ) ) ;
#169745 = ADVANCED_FACE ( 'NONE', ( #91866 ), #110144, .F. ) ;
#169746 = CIRCLE ( 'NONE', #82187, 0.09999999999998898659 ) ;
#169747 = EDGE_CURVE ( 'NONE', #88196, #59064, #172391, .T. ) ;
#169748 = VECTOR ( 'NONE', #142688, 1000.000000000000114 ) ;
#169749 = LINE ( 'NONE', #70643, #207136 ) ;
#169750 = CARTESIAN_POINT ( 'NONE',  ( 20.85000000000000142, 64.35000000001141984, -36.02310748452440237 ) ) ;
#169751 = ORIENTED_EDGE ( 'NONE', *, *, #57073, .F. ) ;
#169752 = LINE ( 'NONE', #112320, #160563 ) ;
#169753 = EDGE_LOOP ( 'NONE', ( #130183, #236485, #255768, #210369 ) ) ;
#169755 = LINE ( 'NONE', #31523, #58611 ) ;
#169754 = CARTESIAN_POINT ( 'NONE',  ( -20.94999999999999929, 14.86477715130881272, -235.7932433709592601 ) ) ;
#169756 = ORIENTED_EDGE ( 'NONE', *, *, #115364, .T. ) ;
#169757 = CIRCLE ( 'NONE', #107166, 0.09999999999999939493 ) ;
#169758 = FACE_OUTER_BOUND ( 'NONE', #226624, .T. ) ;
#169759 = DIRECTION ( 'NONE',  ( 1.186688945009010077E-16, -1.000000000000000000, -0.000000000000000000 ) ) ;
#169760 = CARTESIAN_POINT ( 'NONE',  ( -23.25000000000000000, 11.75000000001115552, -188.8499999999999659 ) ) ;
#169761 = CARTESIAN_POINT ( 'NONE',  ( 21.14999999999999858, 11.65000000001115943, -134.1000000000000227 ) ) ;
#169762 = EDGE_LOOP ( 'NONE', ( #238153, #29931, #107585 ) ) ;
#169764 = ORIENTED_EDGE ( 'NONE', *, *, #43740, .T. ) ;
#169763 = CARTESIAN_POINT ( 'NONE',  ( 20.94999999999999929, 84.66355140188112216, -112.5472086025915388 ) ) ;
#169765 = EDGE_CURVE ( 'NONE', #116008, #175005, #193205, .T. ) ;
#169767 = FACE_OUTER_BOUND ( 'NONE', #18067, .T. ) ;
#169766 =( BOUNDED_SURFACE ( )  B_SPLINE_SURFACE ( 3, 2, ( 
 ( #208443, #5051, #222833 ),
 ( #162903, #148458, #104164 ),
 ( #188853, #125043, #242399 ),
 ( #66348, #187596, #44224 ) ),
 .UNSPECIFIED., .F., .F., .F. ) 
 B_SPLINE_SURFACE_WITH_KNOTS ( ( 4, 4 ),
 ( 3, 3 ),
 ( -1.761828530288944705E-19, 0.0003124336600439507920 ),
 ( 0.000000000000000000, 1.000000000000000000 ),
 .UNSPECIFIED. ) 
 GEOMETRIC_REPRESENTATION_ITEM ( )  RATIONAL_B_SPLINE_SURFACE ( (
 ( 1.000000000000000000, 0.7071067811865475727, 1.000000000000000000),
 ( 1.000000000000000000, 0.7089187706049394633, 1.000000000000000000),
 ( 1.000000000000000000, 0.7039288185052764435, 1.000000000000000000),
 ( 1.000000000000000000, 0.7040654476015688612, 1.000000000000000000) ) ) 
 REPRESENTATION_ITEM ( '' )  SURFACE ( )  );
#169768 = EDGE_CURVE ( 'NONE', #120951, #17092, #105676, .T. ) ;
#169770 = CARTESIAN_POINT ( 'NONE',  ( -16.92570016628985385, 66.04121104227273520, -190.9024568144854470 ) ) ;
#169769 = CARTESIAN_POINT ( 'NONE',  ( -18.40000000000000213, 51.08739888604760182, -230.5155363996569520 ) ) ;
#169772 = ORIENTED_EDGE ( 'NONE', *, *, #202327, .T. ) ;
#169771 = DIRECTION ( 'NONE',  ( 1.000000000000000000, 0.000000000000000000, 0.000000000000000000 ) ) ;
#169773 = EDGE_LOOP ( 'NONE', ( #181010, #43012, #139622, #78448 ) ) ;
#169774 = TOROIDAL_SURFACE ( 'NONE', #227997, 7.800000000000000711, 0.1000000000000000056 ) ;
#169775 = VECTOR ( 'NONE', #104929, 1000.000000000000000 ) ;
#169776 = DIRECTION ( 'NONE',  ( 0.000000000000000000, -1.000000000000000000, 0.000000000000000000 ) ) ;
#169777 = ORIENTED_EDGE ( 'NONE', *, *, #247536, .T. ) ;
#169778 = DIRECTION ( 'NONE',  ( 1.073024830501117725E-15, -6.982962677686266711E-15, 1.000000000000000000 ) ) ;
#169779 = ORIENTED_EDGE ( 'NONE', *, *, #187515, .F. ) ;
#169780 = ADVANCED_FACE ( 'NONE', ( #108861 ), #252212, .F. ) ;
#169781 = EDGE_CURVE ( 'NONE', #234655, #103686, #234894, .T. ) ;
#169782 = DIRECTION ( 'NONE',  ( 0.000000000000000000, 0.000000000000000000, -1.000000000000000000 ) ) ;
#169783 = EDGE_CURVE ( 'NONE', #224224, #107664, #147997, .T. ) ;
#169784 = AXIS2_PLACEMENT_3D ( 'NONE', #191127, #254858, #150691 ) ;
#169785 = ORIENTED_EDGE ( 'NONE', *, *, #150371, .F. ) ;
#169786 = CARTESIAN_POINT ( 'NONE',  ( 23.24999999999999645, 76.00000000001195133, -103.0231074845243171 ) ) ;
#169787 = ORIENTED_EDGE ( 'NONE', *, *, #34341, .T. ) ;
#169788 = AXIS2_PLACEMENT_3D ( 'NONE', #63220, #4534, #64522 ) ;
#169789 = CIRCLE ( 'NONE', #144608, 0.1000000000000055844 ) ;
#169790 = FACE_OUTER_BOUND ( 'NONE', #204152, .T. ) ;
#169791 = CIRCLE ( 'NONE', #69815, 3.899999999999999467 ) ;
#169792 =( BOUNDED_CURVE ( )  B_SPLINE_CURVE ( 3, ( #180938, #119690, #239632, #182225 ),
 .UNSPECIFIED., .F., .F. ) 
 B_SPLINE_CURVE_WITH_KNOTS ( ( 4, 4 ),
 ( 2.589852378279007272, 2.850972632318391042 ),
 .UNSPECIFIED. ) 
 CURVE ( )  GEOMETRIC_REPRESENTATION_ITEM ( )  RATIONAL_B_SPLINE_CURVE ( ( 1.000000000000000000, 0.9943260843901262636, 0.9943260843901262636, 1.000000000000000000 ) ) 
 REPRESENTATION_ITEM ( '' )  );
#169793 = CARTESIAN_POINT ( 'NONE',  ( 18.59999999999999076, 36.65892442174935439, -249.5511627012433848 ) ) ;
#169794 = ORIENTED_EDGE ( 'NONE', *, *, #144780, .F. ) ;
#169795 = ORIENTED_EDGE ( 'NONE', *, *, #234793, .T. ) ;
#169797 = CARTESIAN_POINT ( 'NONE',  ( -18.50000000000000000, -9.480686695267820596, -73.94111516875786094 ) ) ;
#169796 = AXIS2_PLACEMENT_3D ( 'NONE', #77432, #35788, #14934 ) ;
#169798 = EDGE_CURVE ( 'NONE', #234821, #169810, #238988, .T. ) ;
#169799 = ORIENTED_EDGE ( 'NONE', *, *, #97789, .T. ) ;
#169800 = FACE_OUTER_BOUND ( 'NONE', #247486, .T. ) ;
#169801 = CIRCLE ( 'NONE', #57312, 0.1000000000000043493 ) ;
#169802 = ORIENTED_EDGE ( 'NONE', *, *, #78780, .F. ) ;
#169804 = ORIENTED_EDGE ( 'NONE', *, *, #152942, .F. ) ;
#169803 = CARTESIAN_POINT ( 'NONE',  ( -20.94999999999999929, 68.97833521811131163, -32.38954208262708079 ) ) ;
#169805 = ORIENTED_EDGE ( 'NONE', *, *, #5494, .T. ) ;
#169806 = FACE_OUTER_BOUND ( 'NONE', #81247, .T. ) ;
#169807 = ORIENTED_EDGE ( 'NONE', *, *, #167276, .F. ) ;
#169811 = ADVANCED_FACE ( 'NONE', ( #11048 ), #248377, .F. ) ;
#169810 = VERTEX_POINT ( 'NONE', #187141 ) ;
#169809 = ORIENTED_EDGE ( 'NONE', *, *, #220011, .F. ) ;
#169808 = DIRECTION ( 'NONE',  ( 1.000000000000000000, 0.000000000000000000, 0.000000000000000000 ) ) ;
#169812 = DIRECTION ( 'NONE',  ( 0.000000000000000000, -0.000000000000000000, 1.000000000000000000 ) ) ;
#169813 = DIRECTION ( 'NONE',  ( 0.000000000000000000, -1.000000000000000000, -6.982962677686266711E-15 ) ) ;
#169815 = VERTEX_POINT ( 'NONE', #68464 ) ;
#169814 = AXIS2_PLACEMENT_3D ( 'NONE', #253967, #217405, #101268 ) ;
#169816 = AXIS2_PLACEMENT_3D ( 'NONE', #257286, #213073, #236489 ) ;
#169817 = CIRCLE ( 'NONE', #111510, 0.1000000000000002554 ) ;
#169818 = CARTESIAN_POINT ( 'NONE',  ( -23.25000000000000000, 1.115600667400684642E-11, -67.00000000000004263 ) ) ;
#169819 = CIRCLE ( 'NONE', #107417, 0.09999999999998898659 ) ;
#169820 = VERTEX_POINT ( 'NONE', #12359 ) ;
#169821 = AXIS2_PLACEMENT_3D ( 'NONE', #195726, #37931, #151454 ) ;
#169822 = ADVANCED_FACE ( 'NONE', ( #231395 ), #255678, .F. ) ;
#169823 = CARTESIAN_POINT ( 'NONE',  ( -21.11825140030087411, 69.55459243459324625, -203.5303111051574945 ) ) ;
#169825 = ORIENTED_EDGE ( 'NONE', *, *, #103898, .T. ) ;
#169824 = DIRECTION ( 'NONE',  ( 0.000000000000000000, 0.8814952561688444987, -0.4721928772777320149 ) ) ;
#169826 = EDGE_LOOP ( 'NONE', ( #32533, #7352, #189261, #110995 ) ) ;
#169827 = AXIS2_PLACEMENT_3D ( 'NONE', #135409, #115865, #16784 ) ;
#169828 = DIRECTION ( 'NONE',  ( -1.000000000000000000, -0.000000000000000000, 0.000000000000000000 ) ) ;
#169829 = CARTESIAN_POINT ( 'NONE',  ( 18.58143601961975833, 65.56427058491767923, -111.7731074845243597 ) ) ;
#169831 = EDGE_LOOP ( 'NONE', ( #226476, #169150, #160456, #151510 ) ) ;
#169830 = EDGE_CURVE ( 'NONE', #176941, #154288, #1631, .T. ) ;
#169832 = DIRECTION ( 'NONE',  ( 1.000000000000000000, 0.000000000000000000, 0.000000000000000000 ) ) ;
#169833 = DIRECTION ( 'NONE',  ( -1.000000000000000000, -0.000000000000000000, 0.000000000000000000 ) ) ;
#169834 = EDGE_CURVE ( 'NONE', #16905, #90944, #209241, .T. ) ;
#169835 = ORIENTED_EDGE ( 'NONE', *, *, #135431, .T. ) ;
#169837 = VERTEX_POINT ( 'NONE', #52729 ) ;
#169836 = CARTESIAN_POINT ( 'NONE',  ( 19.99999999737951484, 54.38478828167306034, -228.7349980859749223 ) ) ;
#169838 = DIRECTION ( 'NONE',  ( 0.000000000000000000, -0.5000000000000014433, 0.8660254037844378194 ) ) ;
#169839 = CIRCLE ( 'NONE', #82276, 0.09999999999999939493 ) ;
#169840 = VECTOR ( 'NONE', #104044, 1000.000000000000000 ) ;
#169841 = CIRCLE ( 'NONE', #73962, 0.09999999999999939493 ) ;
#169842 = ADVANCED_FACE ( 'NONE', ( #132274 ), #47427, .F. ) ;
#169844 = ORIENTED_EDGE ( 'NONE', *, *, #194850, .T. ) ;
#169843 = VERTEX_POINT ( 'NONE', #31921 ) ;
#169845 = ORIENTED_EDGE ( 'NONE', *, *, #43348, .F. ) ;
#169847 = ADVANCED_FACE ( 'NONE', ( #73621 ), #176635, .F. ) ;
#169846 = CARTESIAN_POINT ( 'NONE',  ( -23.25000000000000000, 11.48087284840413425, -198.4995883060917663 ) ) ;
#169848 = ORIENTED_EDGE ( 'NONE', *, *, #173222, .F. ) ;
#169849 = ORIENTED_EDGE ( 'NONE', *, *, #120850, .F. ) ;
#169850 = CYLINDRICAL_SURFACE ( 'NONE', #21736, 0.1000000000000052097 ) ;
#169851 = ORIENTED_EDGE ( 'NONE', *, *, #13196, .F. ) ;
#169852 = DIRECTION ( 'NONE',  ( 1.000000000000000000, 0.000000000000000000, -0.000000000000000000 ) ) ;
#169853 = PLANE ( 'NONE',  #248292 ) ;
#169854 = ORIENTED_EDGE ( 'NONE', *, *, #72926, .T. ) ;
#169855 = AXIS2_PLACEMENT_3D ( 'NONE', #165384, #7586, #244907 ) ;
#169856 = AXIS2_PLACEMENT_3D ( 'NONE', #160262, #242326, #199376 ) ;
#169857 = ORIENTED_EDGE ( 'NONE', *, *, #239650, .F. ) ;
#169858 = CARTESIAN_POINT ( 'NONE',  ( -20.94999999999999929, 75.74389420791992222, -136.5580039261965908 ) ) ;
#169859 = CIRCLE ( 'NONE', #94790, 0.09999999999999939493 ) ;
#169860 = ORIENTED_EDGE ( 'NONE', *, *, #82999, .T. ) ;
#169861 = EDGE_CURVE ( 'NONE', #175048, #62010, #5722, .T. ) ;
#169862 = ADVANCED_FACE ( 'NONE', ( #247073 ), #159887, .T. ) ;
#169863 = AXIS2_PLACEMENT_3D ( 'NONE', #235236, #159564, #20060 ) ;
#169864 = CARTESIAN_POINT ( 'NONE',  ( -18.39999999999999858, 85.51932773110452501, -129.5501311079648872 ) ) ;
#169865 = ORIENTED_EDGE ( 'NONE', *, *, #107102, .F. ) ;
#169866 = EDGE_CURVE ( 'NONE', #70706, #114500, #243240, .T. ) ;
#169867 = CARTESIAN_POINT ( 'NONE',  ( -18.50000000000000000, 6.846123162363745074, -204.7377262668498190 ) ) ;
#169869 = ORIENTED_EDGE ( 'NONE', *, *, #62410, .T. ) ;
#169868 = DIRECTION ( 'NONE',  ( 0.1538461538461510236, 0.9880948137434718559, 0.000000000000000000 ) ) ;
#169870 = FACE_OUTER_BOUND ( 'NONE', #181130, .T. ) ;
#169871 = CARTESIAN_POINT ( 'NONE',  ( 23.14999999999999858, 4.775700934590584090, -179.3487681040459165 ) ) ;
#169872 = AXIS2_PLACEMENT_3D ( 'NONE', #213385, #252505, #92162 ) ;
#169873 = LINE ( 'NONE', #8194, #128731 ) ;
#169874 = DIRECTION ( 'NONE',  ( 1.000000000000000000, 0.000000000000000000, 0.000000000000000000 ) ) ;
#169875 = DIRECTION ( 'NONE',  ( 0.000000000000000000, 0.000000000000000000, -1.000000000000000000 ) ) ;
#169876 = DIRECTION ( 'NONE',  ( 0.000000000000000000, 0.000000000000000000, 1.000000000000000000 ) ) ;
#169878 = AXIS2_PLACEMENT_3D ( 'NONE', #250074, #187555, #50559 ) ;
#169877 = CARTESIAN_POINT ( 'NONE',  ( -21.05000000000000071, 6.413759733821432718, -33.58561306080397912 ) ) ;
#169879 = TOROIDAL_SURFACE ( 'NONE', #44934, 0.2000000000000000111, 0.1000000000000000056 ) ;
#169881 = EDGE_CURVE ( 'NONE', #65335, #100827, #134818, .T. ) ;
#169880 = DIRECTION ( 'NONE',  ( 0.000000000000000000, 0.000000000000000000, 1.000000000000000000 ) ) ;
#169883 = DIRECTION ( 'NONE',  ( -1.000000000000000000, -3.190570557967288949E-16, -6.948722487160392945E-17 ) ) ;
#169882 = AXIS2_PLACEMENT_3D ( 'NONE', #194754, #196026, #95617 ) ;
#169884 = EDGE_CURVE ( 'NONE', #123416, #39510, #39092, .T. ) ;
#169886 = VERTEX_POINT ( 'NONE', #96962 ) ;
#169885 = CIRCLE ( 'NONE', #178235, 11.64999999999998970 ) ;
#169887 = EDGE_CURVE ( 'NONE', #136730, #99760, #218206, .T. ) ;
#169888 = ORIENTED_EDGE ( 'NONE', *, *, #93068, .T. ) ;
#169890 = ORIENTED_EDGE ( 'NONE', *, *, #75467, .F. ) ;
#169889 = DIRECTION ( 'NONE',  ( 0.000000000000000000, 0.8814952561689112231, -0.4721928772776075589 ) ) ;
#169891 = ORIENTED_EDGE ( 'NONE', *, *, #89732, .F. ) ;
#169892 = DIRECTION ( 'NONE',  ( 1.000000000000000000, 0.000000000000000000, 0.000000000000000000 ) ) ;
#169893 = DIRECTION ( 'NONE',  ( 0.000000000000000000, -0.9908441862701596881, 0.1350103645451904977 ) ) ;
#169895 = CARTESIAN_POINT ( 'NONE',  ( 21.07928932188134397, 1.596973512272234830, -230.6572452218043736 ) ) ;
#169894 = DIRECTION ( 'NONE',  ( 0.000000000000000000, 0.000000000000000000, -1.000000000000000000 ) ) ;
#169896 = EDGE_CURVE ( 'NONE', #229112, #74863, #168298, .T. ) ;
#169897 = ORIENTED_EDGE ( 'NONE', *, *, #166456, .T. ) ;
#169898 = ORIENTED_EDGE ( 'NONE', *, *, #222517, .F. ) ;
#169899 = AXIS2_PLACEMENT_3D ( 'NONE', #11220, #90732, #51584 ) ;
#169900 =( NAMED_UNIT ( * ) SI_UNIT ( $, .STERADIAN. ) SOLID_ANGLE_UNIT ( ) );
#169901 = CARTESIAN_POINT ( 'NONE',  ( 18.46947024752518729, -9.509297157144928292, -40.48668944869792341 ) ) ;
#169902 = CYLINDRICAL_SURFACE ( 'NONE', #108122, 0.1000000000000028644 ) ;
#169903 = ORIENTED_EDGE ( 'NONE', *, *, #88156, .T. ) ;
#169904 = ORIENTED_EDGE ( 'NONE', *, *, #189330, .T. ) ;
#169905 = AXIS2_PLACEMENT_3D ( 'NONE', #49729, #144962, #204935 ) ;
#169906 = CARTESIAN_POINT ( 'NONE',  ( -16.87683809663753465, 9.864913778549569301, -180.7757156356384769 ) ) ;
#169907 = LINE ( 'NONE', #227251, #191433 ) ;
#169908 = CARTESIAN_POINT ( 'NONE',  ( -18.60000000000000142, -8.350000000000004974, 33.00000000000000000 ) ) ;
#169910 = ORIENTED_EDGE ( 'NONE', *, *, #25505, .F. ) ;
#169909 = DIRECTION ( 'NONE',  ( 1.000000000000000000, 0.000000000000000000, 0.000000000000000000 ) ) ;
#169911 = DIRECTION ( 'NONE',  ( 1.000000000000000000, 0.000000000000000000, 0.000000000000000000 ) ) ;
#169912 = DIRECTION ( 'NONE',  ( 0.000000000000000000, 0.9501938099239353175, -0.3116596277708039708 ) ) ;
#169913 = DIRECTION ( 'NONE',  ( 0.000000000000000000, 0.1350103645451835865, 0.9908441862701605762 ) ) ;
#169914 = LINE ( 'NONE', #224683, #204087 ) ;
#169915 = ORIENTED_EDGE ( 'NONE', *, *, #194505, .F. ) ;
#169916 = DIRECTION ( 'NONE',  ( 0.000000000000000000, -1.000000000000000000, -6.982962677686265922E-15 ) ) ;
#169917 = CYLINDRICAL_SURFACE ( 'NONE', #198515, 0.09999999999999939493 ) ;
#169919 = CARTESIAN_POINT ( 'NONE',  ( 20.94999999999999929, 0.000000000000000000, -33.50000000000000000 ) ) ;
#169918 = LINE ( 'NONE', #47329, #165861 ) ;
#169920 = CARTESIAN_POINT ( 'NONE',  ( -22.39999999999999858, 75.90000000001242597, -177.8138870828977360 ) ) ;
#169921 = CARTESIAN_POINT ( 'NONE',  ( -16.82542659449980249, 9.934499891438557384, -54.25536439997377869 ) ) ;
#169922 = LINE ( 'NONE', #51175, #95665 ) ;
#169923 = CARTESIAN_POINT ( 'NONE',  ( -18.40000000000000213, 64.25000000001261924, -190.8731074845244393 ) ) ;
#169924 = VECTOR ( 'NONE', #19196, 1000.000000000000000 ) ;
#169925 = AXIS2_PLACEMENT_3D ( 'NONE', #67274, #161258, #226322 ) ;
#169926 = DIRECTION ( 'NONE',  ( -0.000000000000000000, -0.1350103645451904977, 0.9908441862701596881 ) ) ;
#169927 = DIRECTION ( 'NONE',  ( 0.000000000000000000, 0.000000000000000000, -1.000000000000000000 ) ) ;
#169928 = AXIS2_PLACEMENT_3D ( 'NONE', #37473, #196521, #156150 ) ;
#169929 = VERTEX_POINT ( 'NONE', #137401 ) ;
#169930 = ORIENTED_EDGE ( 'NONE', *, *, #182553, .T. ) ;
#169931 = EDGE_LOOP ( 'NONE', ( #167700, #98606, #156984, #170748 ) ) ;
#169932 = EDGE_CURVE ( 'NONE', #27728, #122573, #147402, .T. ) ;
#169933 = DIRECTION ( 'NONE',  ( -0.000000000000000000, -0.2128009952263604232, 0.9770955615653316162 ) ) ;
#169934 = DIRECTION ( 'NONE',  ( -0.7071067811865475727, 0.7071067811865475727, 4.937700262164531476E-15 ) ) ;
#169935 = ORIENTED_EDGE ( 'NONE', *, *, #252306, .T. ) ;
#169936 = ORIENTED_EDGE ( 'NONE', *, *, #226605, .F. ) ;
#169938 = TOROIDAL_SURFACE ( 'NONE', #57443, 2.100000000000002309, 0.1000000000000000056 ) ;
#169937 =( LENGTH_UNIT ( ) NAMED_UNIT ( * ) SI_UNIT ( .MILLI., .METRE. ) );
#169939 = CIRCLE ( 'NONE', #124121, 0.09999999999999739653 ) ;
#169940 = EDGE_CURVE ( 'NONE', #128154, #31772, #43355, .T. ) ;
#169941 = EDGE_LOOP ( 'NONE', ( #111615, #227738, #175250, #196646 ) ) ;
#169942 = DIRECTION ( 'NONE',  ( 0.000000000000000000, 0.8814952561688469412, -0.4721928772777276850 ) ) ;
#169943 = ORIENTED_EDGE ( 'NONE', *, *, #162307, .T. ) ;
#169944 = CIRCLE ( 'NONE', #199119, 0.1000000000000124678 ) ;
#169945 = CARTESIAN_POINT ( 'NONE',  ( -22.57320508075687115, 64.35000000001195986, -103.0231074845243739 ) ) ;
#169946 = DIRECTION ( 'NONE',  ( 1.000000000000000000, 0.000000000000000000, -0.000000000000000000 ) ) ;
#169947 = DIRECTION ( 'NONE',  ( 0.000000000000000000, 0.000000000000000000, -1.000000000000000000 ) ) ;
#169948 = CARTESIAN_POINT ( 'NONE',  ( -21.51976009735018991, 6.910458441670358276, -67.00000000000004263 ) ) ;
#169949 = CYLINDRICAL_SURFACE ( 'NONE', #112000, 4.049999999999998046 ) ;
#169951 = ORIENTED_EDGE ( 'NONE', *, *, #78191, .F. ) ;
#169950 = CARTESIAN_POINT ( 'NONE',  ( -16.80070461187955999, 30.20900493031334477, -234.8084786630442977 ) ) ;
#169953 = FACE_OUTER_BOUND ( 'NONE', #57829, .T. ) ;
#169952 = CARTESIAN_POINT ( 'NONE',  ( 23.24999999999999289, 11.65000000000000746, -21.35000000000000142 ) ) ;
#169954 = CARTESIAN_POINT ( 'NONE',  ( 21.05000000000000071, -11.48912529306490349, -36.60000000000000142 ) ) ;
#169955 = ORIENTED_EDGE ( 'NONE', *, *, #157809, .F. ) ;
#169956 = DIRECTION ( 'NONE',  ( 0.000000000000000000, -0.2128009952258890225, 0.9770955615654342008 ) ) ;
#169957 = DIRECTION ( 'NONE',  ( 0.000000000000000000, 0.000000000000000000, 1.000000000000000000 ) ) ;
#169958 = FACE_OUTER_BOUND ( 'NONE', #232968, .T. ) ;
#169959 = EDGE_LOOP ( 'NONE', ( #216780, #138719, #95362, #146123 ) ) ;
#169960 = DIRECTION ( 'NONE',  ( 0.000000000000000000, 0.9770955615653316162, 0.2128009952263604232 ) ) ;
#169961 = AXIS2_PLACEMENT_3D ( 'NONE', #178560, #35208, #258010 ) ;
#169962 = CARTESIAN_POINT ( 'NONE',  ( -23.49999999999994316, 77.83551161375991967, -47.52760213295649550 ) ) ;
#169963 = VERTEX_POINT ( 'NONE', #34492 ) ;
#169964 = CIRCLE ( 'NONE', #178317, 0.09999999999999939493 ) ;
#169965 = AXIS2_PLACEMENT_3D ( 'NONE', #110620, #152349, #14110 ) ;
#169966 = DIRECTION ( 'NONE',  ( 0.000000000000000000, -0.4088369013363281068, 0.9126074666063770380 ) ) ;
#169967 = CARTESIAN_POINT ( 'NONE',  ( 22.60000000000000142, 64.25043287652226809, -69.62396585362311896 ) ) ;
#169968 = CARTESIAN_POINT ( 'NONE',  ( 21.05000000000000071, 1.148907358139439339E-11, -201.0000000000015064 ) ) ;
#169969 = ORIENTED_EDGE ( 'NONE', *, *, #64589, .T. ) ;
#169970 = AXIS2_PLACEMENT_3D ( 'NONE', #36899, #60264, #138495 ) ;
#169971 = ORIENTED_EDGE ( 'NONE', *, *, #47016, .T. ) ;
#169972 = ADVANCED_FACE ( 'NONE', ( #14920 ), #37063, .T. ) ;
#169973 = CARTESIAN_POINT ( 'NONE',  ( 20.94999999999999929, 71.18691588786205671, -57.58158972800053022 ) ) ;
#169974 = DIRECTION ( 'NONE',  ( 0.000000000000000000, 0.2617529984165031243, 0.9651348961777158619 ) ) ;
#169975 = CARTESIAN_POINT ( 'NONE',  ( 23.14999999999999503, 51.33926024308902214, -230.0993571250899095 ) ) ;
#169977 = CARTESIAN_POINT ( 'NONE',  ( -21.05000000000000071, -11.48912529306490349, -103.6000000000000369 ) ) ;
#169976 = DIRECTION ( 'NONE',  ( 1.000000000000000000, -2.952720810173289112E-16, -2.061873921506763405E-30 ) ) ;
#169978 = AXIS2_PLACEMENT_3D ( 'NONE', #138581, #218132, #79892 ) ;
#169980 = CARTESIAN_POINT ( 'NONE',  ( 21.05000000000000071, 82.48249193998721296, -215.5326005316167084 ) ) ;
#169979 = AXIS2_PLACEMENT_3D ( 'NONE', #202871, #24263, #25538 ) ;
#169981 = CARTESIAN_POINT ( 'NONE',  ( 20.94999999999999929, 76.00000000001213607, -136.5231074845243313 ) ) ;
#169982 = PLANE ( 'NONE',  #34715 ) ;
#169983 = AXIS2_PLACEMENT_3D ( 'NONE', #32123, #174219, #77612 ) ;
#169984 = ORIENTED_EDGE ( 'NONE', *, *, #150823, .T. ) ;
#169985 = DIRECTION ( 'NONE',  ( 0.000000000000000000, 6.982962677686266711E-15, -1.000000000000000000 ) ) ;
#169987 = ORIENTED_EDGE ( 'NONE', *, *, #188332, .T. ) ;
#169986 = DIRECTION ( 'NONE',  ( 0.000000000000000000, 0.000000000000000000, -1.000000000000000000 ) ) ;
#169988 = CARTESIAN_POINT ( 'NONE',  ( 18.49999999999999289, 65.79142135624982757, -178.8731074845244109 ) ) ;
#169989 = CIRCLE ( 'NONE', #228402, 0.09999999999998898659 ) ;
#169990 = DIRECTION ( 'NONE',  ( 0.000000000000000000, 0.000000000000000000, -1.000000000000000000 ) ) ;
#169991 = FACE_OUTER_BOUND ( 'NONE', #158934, .T. ) ;
#169992 = CARTESIAN_POINT ( 'NONE',  ( -16.80621392010908011, 66.05779742250423681, -123.8335155191076211 ) ) ;
#169993 = ADVANCED_FACE ( 'NONE', ( #213096 ), #175294, .F. ) ;
#169994 = DIRECTION ( 'NONE',  ( 0.000000000000000000, 0.2128009952263602844, -0.9770955615653315052 ) ) ;
#169996 = ORIENTED_EDGE ( 'NONE', *, *, #103779, .F. ) ;
#169995 = DIRECTION ( 'NONE',  ( -1.000000000000000000, 0.000000000000000000, 0.000000000000000000 ) ) ;
#169997 = FACE_BOUND ( 'NONE', #100769, .T. ) ;
#169998 = DIRECTION ( 'NONE',  ( 1.000000000000000000, 3.469446951953704435E-14, -2.003086131649669752E-14 ) ) ;
#169999 = CARTESIAN_POINT ( 'NONE',  ( -20.54999999999999716, 7.250000000011155521, -88.25000000000005684 ) ) ;
#170000 = FACE_OUTER_BOUND ( 'NONE', #92429, .T. ) ;
#170001 = EDGE_CURVE ( 'NONE', #82909, #218080, #116572, .T. ) ;
#170002 = ORIENTED_EDGE ( 'NONE', *, *, #182966, .F. ) ;
#170003 = FACE_OUTER_BOUND ( 'NONE', #99303, .T. ) ;
#170004 = EDGE_LOOP ( 'NONE', ( #55665, #96680, #192454, #178786 ) ) ;
#170005 = CARTESIAN_POINT ( 'NONE',  ( -20.94999999999999929, 74.16465844978819177, -191.9679561919613775 ) ) ;
#170007 = EDGE_CURVE ( 'NONE', #16708, #128766, #243070, .T. ) ;
#170006 = CIRCLE ( 'NONE', #228231, 0.1000000000000055844 ) ;
#170008 = ORIENTED_EDGE ( 'NONE', *, *, #14964, .T. ) ;
#170009 = CARTESIAN_POINT ( 'NONE',  ( 22.47071067811865319, 0.09909245471376171288, -126.2799252555019649 ) ) ;
#170010 = AXIS2_PLACEMENT_3D ( 'NONE', #51101, #210227, #31605 ) ;
#170011 = ORIENTED_EDGE ( 'NONE', *, *, #95384, .F. ) ;
#170012 = AXIS2_PLACEMENT_3D ( 'NONE', #20710, #100194, #179781 ) ;
#170013 = CYLINDRICAL_SURFACE ( 'NONE', #205828, 0.1000000000000025868 ) ;
#170015 = DIRECTION ( 'NONE',  ( -1.000000000000000000, 0.000000000000000000, 0.000000000000000000 ) ) ;
#170014 = CIRCLE ( 'NONE', #136618, 0.1000000000000028644 ) ;
#170016 = CIRCLE ( 'NONE', #65727, 0.09999999999999939493 ) ;
#170017 = ORIENTED_EDGE ( 'NONE', *, *, #14700, .F. ) ;
#170018 = CIRCLE ( 'NONE', #57518, 0.1999999999999987899 ) ;
#170019 = EDGE_CURVE ( 'NONE', #178023, #233092, #55772, .T. ) ;
#170020 = DIRECTION ( 'NONE',  ( 1.000000000000000000, 0.000000000000000000, 0.000000000000000000 ) ) ;
#170021 = LINE ( 'NONE', #243397, #82431 ) ;
#170022 = DIRECTION ( 'NONE',  ( 1.836970198721029441E-16, -0.4721928772777346239, -0.8814952561688430555 ) ) ;
#170023 = CARTESIAN_POINT ( 'NONE',  ( 13.54577453029515688, 9.450602096088521975, -18.44389596309666501 ) ) ;
#170024 = FACE_BOUND ( 'NONE', #55869, .T. ) ;
#170025 = ORIENTED_EDGE ( 'NONE', *, *, #200216, .T. ) ;
#170027 = AXIS2_PLACEMENT_3D ( 'NONE', #183550, #21913, #163989 ) ;
#170026 = CARTESIAN_POINT ( 'NONE',  ( -22.50000000000000000, 1.148907358139439339E-11, -201.0000000000015064 ) ) ;
#170028 = CIRCLE ( 'NONE', #57527, 4.000000000000003553 ) ;
#170029 = EDGE_LOOP ( 'NONE', ( #100898, #218631, #249216, #132772 ) ) ;
#170031 = ORIENTED_EDGE ( 'NONE', *, *, #132076, .T. ) ;
#170030 = CYLINDRICAL_SURFACE ( 'NONE', #210555, 0.09999999999999939493 ) ;
#170032 = EDGE_LOOP ( 'NONE', ( #43562, #44447, #145058, #74276 ) ) ;
#170033 = DIRECTION ( 'NONE',  ( 0.000000000000000000, -1.000000000000000000, 0.000000000000000000 ) ) ;
#170034 = ORIENTED_EDGE ( 'NONE', *, *, #241667, .T. ) ;
#170035 = DIRECTION ( 'NONE',  ( 1.000000000000000000, 0.000000000000000000, 0.000000000000000000 ) ) ;
#170036 = CARTESIAN_POINT ( 'NONE',  ( 22.47071067811864964, 0.09909245471376176839, -25.77992525550196135 ) ) ;
#170037 = DIRECTION ( 'NONE',  ( -1.000000000000000000, 0.000000000000000000, -0.000000000000000000 ) ) ;
#170038 = ORIENTED_EDGE ( 'NONE', *, *, #211769, .T. ) ;
#170039 = CARTESIAN_POINT ( 'NONE',  ( -16.89268316805466341, 66.04827818676987761, -123.8788599630699281 ) ) ;
#170040 = CARTESIAN_POINT ( 'NONE',  ( -20.64999999999999858, 68.75000000001199396, -115.3731074845243540 ) ) ;
#170041 = DIRECTION ( 'NONE',  ( -3.469446951953245002E-14, -0.2617529984164506107, -0.9651348961777299618 ) ) ;
#170042 = ORIENTED_EDGE ( 'NONE', *, *, #101414, .F. ) ;
#170043 = EDGE_CURVE ( 'NONE', #140929, #26421, #196114, .T. ) ;
#170044 = CIRCLE ( 'NONE', #224143, 0.09999999999998898659 ) ;
#170046 = EDGE_LOOP ( 'NONE', ( #256156, #224216, #108545, #250058 ) ) ;
#170045 = FACE_OUTER_BOUND ( 'NONE', #130636, .T. ) ;
#170047 = CARTESIAN_POINT ( 'NONE',  ( -20.64999999999999858, 9.593045456726526865, -211.4478935133083439 ) ) ;
#170048 = VECTOR ( 'NONE', #5629, 1000.000000000000000 ) ;
#170049 = DIRECTION ( 'NONE',  ( -4.391705002472928105E-16, 0.9770955615653315052, 0.2128009952263601179 ) ) ;
#170050 = CIRCLE ( 'NONE', #203319, 0.1000000000000043771 ) ;
#170051 = ORIENTED_EDGE ( 'NONE', *, *, #67402, .F. ) ;
#170052 = VECTOR ( 'NONE', #10758, 1000.000000000000000 ) ;
#170053 = CARTESIAN_POINT ( 'NONE',  ( -23.15000000000000213, 36.65892442174935439, -249.5511627012433848 ) ) ;
#170055 = EDGE_CURVE ( 'NONE', #170631, #208027, #256021, .T. ) ;
#170054 = CARTESIAN_POINT ( 'NONE',  ( -16.87036670365549540, 44.00112830765706207, -235.3159266546824995 ) ) ;
#170056 = DIRECTION ( 'NONE',  ( -1.000000000000000000, 0.000000000000000000, 0.000000000000000000 ) ) ;
#170057 = ORIENTED_EDGE ( 'NONE', *, *, #97754, .T. ) ;
#170058 = DIRECTION ( 'NONE',  ( -0.000000000000000000, -0.000000000000000000, -1.000000000000000000 ) ) ;
#170059 = AXIS2_PLACEMENT_3D ( 'NONE', #198690, #20071, #162158 ) ;
#170060 = ADVANCED_FACE ( 'NONE', ( #237804 ), #119147, .T. ) ;
#170061 = CARTESIAN_POINT ( 'NONE',  ( -23.15000000000000213, 11.65000000001115588, -100.5000000000000284 ) ) ;
#170062 = ORIENTED_EDGE ( 'NONE', *, *, #190076, .T. ) ;
#170063 = CIRCLE ( 'NONE', #220079, 11.89999999999999325 ) ;
#170064 = AXIS2_PLACEMENT_3D ( 'NONE', #249449, #209025, #51198 ) ;
#170065 = CIRCLE ( 'NONE', #86781, 0.1000000000000028644 ) ;
#170066 = EDGE_CURVE ( 'NONE', #60954, #119804, #59125, .T. ) ;
#170067 = AXIS2_PLACEMENT_3D ( 'NONE', #201860, #218839, #40249 ) ;
#170068 = ORIENTED_EDGE ( 'NONE', *, *, #74924, .F. ) ;
#170069 = CARTESIAN_POINT ( 'NONE',  ( 22.37643362114956247, 68.37421000605431232, -203.6221888582057886 ) ) ;
#170070 = EDGE_LOOP ( 'NONE', ( #163209, #132214, #232892, #45361, #229573 ) ) ;
#170071 = DIRECTION ( 'NONE',  ( 0.7071067811865475727, -0.7071067811865475727, 0.000000000000000000 ) ) ;
#170074 = EDGE_CURVE ( 'NONE', #69695, #231343, #47600, .T. ) ;
#170073 = ORIENTED_EDGE ( 'NONE', *, *, #197750, .F. ) ;
#170072 = CARTESIAN_POINT ( 'NONE',  ( 20.94999999999999574, 10.47338541492405994, -141.5786544642485580 ) ) ;
#170075 = LINE ( 'NONE', #146581, #257351 ) ;
#170076 = CARTESIAN_POINT ( 'NONE',  ( 18.39999999999999147, 19.44861527341281615, -230.3234391047226666 ) ) ;
#170077 = CARTESIAN_POINT ( 'NONE',  ( -18.39999999999999858, -9.499999999988849808, -40.53206939669966857 ) ) ;
#170078 = CARTESIAN_POINT ( 'NONE',  ( -16.97683809663753962, 9.949999999999983302, -20.22847083211057750 ) ) ;
#170079 = CARTESIAN_POINT ( 'NONE',  ( 21.05000000000000071, 5.000000000011153745, -45.90526601891310321 ) ) ;
#170080 = VECTOR ( 'NONE', #19588, 1000.000000000000000 ) ;
#170081 = ADVANCED_FACE ( 'NONE', ( #21349 ), #230814, .T. ) ;
#170082 = CARTESIAN_POINT ( 'NONE',  ( 20.94999999999999929, 76.00000000001216449, -140.6231074845243256 ) ) ;
#170083 = ADVANCED_FACE ( 'NONE', ( #220800 ), #26472, .T. ) ;
#170084 = DIRECTION ( 'NONE',  ( 1.000000000000000000, 0.000000000000000000, 0.000000000000000000 ) ) ;
#170086 = ORIENTED_EDGE ( 'NONE', *, *, #219934, .F. ) ;
#170085 = DIRECTION ( 'NONE',  ( 1.000000000000000000, 0.000000000000000000, 0.000000000000000000 ) ) ;
#170088 = ADVANCED_FACE ( 'NONE', ( #244200 ), #210137, .T. ) ;
#170087 = CARTESIAN_POINT ( 'NONE',  ( 18.49999999999998934, 11.65000000001115943, -192.2499999999999716 ) ) ;
#170089 = DIRECTION ( 'NONE',  ( -1.000000000000000000, 0.000000000000000000, 0.000000000000000000 ) ) ;
#170091 = ADVANCED_FACE ( 'NONE', ( #44747 ), #61732, .T. ) ;
#170090 = CARTESIAN_POINT ( 'NONE',  ( 19.75857864376268935, 64.35000000001147669, -44.67310748452440095 ) ) ;
#170092 = CARTESIAN_POINT ( 'NONE',  ( 23.14999999999998437, 67.23127455305841238, -235.8551265064783991 ) ) ;
#170093 = ADVANCED_FACE ( 'NONE', ( #219505 ), #202526, .T. ) ;
#170094 = ORIENTED_EDGE ( 'NONE', *, *, #88365, .F. ) ;
#170095 = FACE_OUTER_BOUND ( 'NONE', #116640, .T. ) ;
#170096 = CARTESIAN_POINT ( 'NONE',  ( 23.14999999999999503, 56.06656052939784729, -228.0911609752645290 ) ) ;
#170097 = AXIS2_PLACEMENT_3D ( 'NONE', #143647, #139785, #219330 ) ;
#170098 = VECTOR ( 'NONE', #79778, 999.9999999999998863 ) ;
#170099 = AXIS2_PLACEMENT_3D ( 'NONE', #241651, #158302, #83817 ) ;
#170100 = ORIENTED_EDGE ( 'NONE', *, *, #201253, .F. ) ;
#170101 = AXIS2_PLACEMENT_3D ( 'NONE', #32036, #12465, #232797 ) ;
#170102 = DIRECTION ( 'NONE',  ( 0.000000000000000000, -0.4999999999999689138, -0.8660254037844565822 ) ) ;
#170103 = CARTESIAN_POINT ( 'NONE',  ( -18.50000000000000000, 47.89822068137787170, -246.3100470504847692 ) ) ;
#170104 = EDGE_LOOP ( 'NONE', ( #28906, #256168, #46284, #5144 ) ) ;
#170105 = CARTESIAN_POINT ( 'NONE',  ( -16.87368910959167678, 66.03872618332120226, -190.9106143878838395 ) ) ;
#170106 = EDGE_CURVE ( 'NONE', #69997, #91291, #160851, .T. ) ;
#170107 = ORIENTED_EDGE ( 'NONE', *, *, #139148, .T. ) ;
#170108 = ADVANCED_FACE ( 'NONE', ( #103398 ), #208567, .T. ) ;
#170109 = DIRECTION ( 'NONE',  ( 0.000000000000000000, 1.000000000000000000, 0.000000000000000000 ) ) ;
#170111 = VERTEX_POINT ( 'NONE', #60431 ) ;
#170110 = CARTESIAN_POINT ( 'NONE',  ( -16.87683809663752399, 54.76195096157879760, -90.37310748452445353 ) ) ;
#170112 = CARTESIAN_POINT ( 'NONE',  ( -18.40000000000000213, 70.35000000001159037, -56.87310748452436115 ) ) ;
#170113 = ORIENTED_EDGE ( 'NONE', *, *, #139817, .T. ) ;
#170114 = LINE ( 'NONE', #31868, #22141 ) ;
#170115 = AXIS2_PLACEMENT_3D ( 'NONE', #181794, #3129, #80079 ) ;
#170116 = VERTEX_POINT ( 'NONE', #159558 ) ;
#170118 = EDGE_CURVE ( 'NONE', #7520, #17436, #10227, .T. ) ;
#170117 = ORIENTED_EDGE ( 'NONE', *, *, #247839, .T. ) ;
#170120 = LINE ( 'NONE', #245761, #94427 ) ;
#170119 = VECTOR ( 'NONE', #80817, 1000.000000000000114 ) ;
#170122 = ORIENTED_EDGE ( 'NONE', *, *, #162162, .F. ) ;
#170121 = CARTESIAN_POINT ( 'NONE',  ( 13.12220780326572367, 9.430633469083957721, -48.73176579482409210 ) ) ;
#170123 = DIRECTION ( 'NONE',  ( 0.000000000000000000, 0.2128009952263601456, -0.9770955615653316162 ) ) ;
#170124 = ORIENTED_EDGE ( 'NONE', *, *, #159102, .T. ) ;
#170125 = CIRCLE ( 'NONE', #57632, 0.09999999999999939493 ) ;
#170126 = ORIENTED_EDGE ( 'NONE', *, *, #65672, .F. ) ;
#170127 = DIRECTION ( 'NONE',  ( 1.000000000000000000, -3.265361837132813093E-16, -2.280189983783949500E-30 ) ) ;
#170128 = DIRECTION ( 'NONE',  ( 0.000000000000000000, 0.8660254037844411501, 0.4999999999999956701 ) ) ;
#170129 = ORIENTED_EDGE ( 'NONE', *, *, #235454, .T. ) ;
#170130 = DIRECTION ( 'NONE',  ( 0.000000000000000000, 1.265107689135680095E-16, -1.000000000000000000 ) ) ;
#170131 = CARTESIAN_POINT ( 'NONE',  ( 18.49999999999999645, 16.60731133254646963, -240.9277311905271688 ) ) ;
#170132 = CARTESIAN_POINT ( 'NONE',  ( 0.9000000000000546452, 67.65000000001118963, -5.981686128287480919 ) ) ;
#170134 = ORIENTED_EDGE ( 'NONE', *, *, #102026, .F. ) ;
#170133 = EDGE_CURVE ( 'NONE', #50042, #4950, #135081, .T. ) ;
#170135 = DIRECTION ( 'NONE',  ( 1.000000000000000000, 0.000000000000000000, 0.000000000000000000 ) ) ;
#170136 = DIRECTION ( 'NONE',  ( -1.000000000000000000, -0.000000000000000000, 0.000000000000000000 ) ) ;
#170137 = DIRECTION ( 'NONE',  ( -1.000000000000000000, 0.000000000000000000, 0.000000000000000000 ) ) ;
#170138 = EDGE_CURVE ( 'NONE', #161165, #11869, #139173, .T. ) ;
#170139 = VECTOR ( 'NONE', #179521, 1000.000000000000000 ) ;
#170140 = ORIENTED_EDGE ( 'NONE', *, *, #198574, .T. ) ;
#170141 = DIRECTION ( 'NONE',  ( 1.000000000000000000, 0.000000000000000000, 0.000000000000000000 ) ) ;
#170142 = EDGE_LOOP ( 'NONE', ( #143752, #138681, #65064, #78797 ) ) ;
#170143 = CARTESIAN_POINT ( 'NONE',  ( -18.42609945526383086, -7.792936248106745900, -209.8606554160495250 ) ) ;
#170144 = CIRCLE ( 'NONE', #236717, 0.09999999999999939493 ) ;
#170145 = ORIENTED_EDGE ( 'NONE', *, *, #222706, .T. ) ;
#170146 = AXIS2_PLACEMENT_3D ( 'NONE', #13780, #30802, #172901 ) ;
#170147 = DIRECTION ( 'NONE',  ( 1.000000000000000000, 0.000000000000000000, 0.000000000000000000 ) ) ;
#170148 = DIRECTION ( 'NONE',  ( 2.465190328815662439E-32, -0.9126074666063770380, -0.4088369013363282178 ) ) ;
#170149 = ORIENTED_EDGE ( 'NONE', *, *, #130311, .T. ) ;
#170150 = ORIENTED_EDGE ( 'NONE', *, *, #1338, .T. ) ;
#170152 = EDGE_CURVE ( 'NONE', #220305, #53442, #251639, .T. ) ;
#170151 = CARTESIAN_POINT ( 'NONE',  ( 23.14999999999999503, 64.35000000001204512, -124.3731074845243825 ) ) ;
#170153 = CARTESIAN_POINT ( 'NONE',  ( -20.64999999999999858, 7.150000000011155876, -45.85000000000000142 ) ) ;
#170154 = ORIENTED_EDGE ( 'NONE', *, *, #176955, .T. ) ;
#170155 = CIRCLE ( 'NONE', #249409, 0.09999999999999939493 ) ;
#170156 = CARTESIAN_POINT ( 'NONE',  ( -20.54999999999999716, 74.00000000001186606, -89.79848556176222019 ) ) ;
#170157 = EDGE_CURVE ( 'NONE', #144289, #3432, #122656, .T. ) ;
#170158 = VERTEX_POINT ( 'NONE', #250627 ) ;
#170159 = CARTESIAN_POINT ( 'NONE',  ( -18.50000000000000000, 38.28679861725831302, -261.0868692510649680 ) ) ;
#170160 = EDGE_CURVE ( 'NONE', #222295, #111061, #235082, .T. ) ;
#170161 = VECTOR ( 'NONE', #72595, 999.9999999999998863 ) ;
#170162 = AXIS2_PLACEMENT_3D ( 'NONE', #26522, #106012, #212857 ) ;
#170164 = ORIENTED_EDGE ( 'NONE', *, *, #68709, .T. ) ;
#170163 = AXIS2_PLACEMENT_3D ( 'NONE', #13529, #115191, #194753 ) ;
#170165 = EDGE_CURVE ( 'NONE', #23345, #93776, #30346, .T. ) ;
#170169 = EDGE_CURVE ( 'NONE', #249282, #210105, #146380, .T. ) ;
#170168 = ADVANCED_FACE ( 'NONE', ( #225906 ), #43535, .T. ) ;
#170167 = CARTESIAN_POINT ( 'NONE',  ( 18.49999999999999289, 11.65000000000000391, 11.75000000000000000 ) ) ;
#170166 = AXIS2_PLACEMENT_3D ( 'NONE', #32409, #12836, #110626 ) ;
#170170 = CARTESIAN_POINT ( 'NONE',  ( -16.78569801330232991, 22.98318547630623954, -230.9401490402474622 ) ) ;
#170171 = SHAPE_REPRESENTATION ( 'Snap Open Cable Crossbars 11', ( #2425 ), #185768 ) ;
#170172 = CARTESIAN_POINT ( 'NONE',  ( -21.09610168723073187, 6.378955715235938406, -66.96641049310854044 ) ) ;
#170174 = VERTEX_POINT ( 'NONE', #246777 ) ;
#170173 = DIRECTION ( 'NONE',  ( 1.000000000000000000, 0.000000000000000000, 0.000000000000000000 ) ) ;
#170176 = TOROIDAL_SURFACE ( 'NONE', #199168, 0.2000000000000000111, 0.1000000000000000056 ) ;
#170175 = DIRECTION ( 'NONE',  ( 1.000000000000000000, -0.000000000000000000, -0.000000000000000000 ) ) ;
#170177 = CARTESIAN_POINT ( 'NONE',  ( -20.94999999999994600, 66.15000000001120384, -4.623107484524796362 ) ) ;
#170178 = PLANE ( 'NONE',  #60966 ) ;
#170180 = FACE_OUTER_BOUND ( 'NONE', #68919, .T. ) ;
#170179 = SPHERICAL_SURFACE ( 'NONE', #223350, 0.1000000000000000056 ) ;
#170181 = CARTESIAN_POINT ( 'NONE',  ( -21.05000000000000071, 69.70000000001193996, -102.9231074845243512 ) ) ;
#170182 = CARTESIAN_POINT ( 'NONE',  ( 21.05000000000000071, 87.65000000001236913, -170.0231074845242745 ) ) ;
#170183 = AXIS2_PLACEMENT_3D ( 'NONE', #53570, #232226, #113541 ) ;
#170184 = CARTESIAN_POINT ( 'NONE',  ( -21.14999999999999858, 56.01362831242966678, -232.7091905853083347 ) ) ;
#170185 = CARTESIAN_POINT ( 'NONE',  ( -21.14999999999999503, 76.00000000001243450, -176.5637644362255969 ) ) ;
#170186 = EDGE_CURVE ( 'NONE', #155345, #137276, #29066, .T. ) ;
#170187 = EDGE_CURVE ( 'NONE', #198491, #39296, #210248, .T. ) ;
#170188 = ORIENTED_EDGE ( 'NONE', *, *, #9258, .F. ) ;
#170189 = CIRCLE ( 'NONE', #45053, 0.09999999999999939493 ) ;
#170190 = CIRCLE ( 'NONE', #215902, 0.1000000000000002692 ) ;
#170191 = VECTOR ( 'NONE', #233380, 1000.000000000000000 ) ;
#170192 = AXIS2_PLACEMENT_3D ( 'NONE', #57546, #178834, #160547 ) ;
#170193 = ORIENTED_EDGE ( 'NONE', *, *, #56379, .F. ) ;
#170194 = ADVANCED_FACE ( 'NONE', ( #48581 ), #207679, .F. ) ;
#170195 = VERTEX_POINT ( 'NONE', #9459 ) ;
#170196 = AXIS2_PLACEMENT_3D ( 'NONE', #99375, #44568, #178981 ) ;
#170197 = EDGE_CURVE ( 'NONE', #11705, #71313, #12056, .T. ) ;
#170198 = FACE_OUTER_BOUND ( 'NONE', #47952, .T. ) ;
#170199 = EDGE_CURVE ( 'NONE', #149075, #20245, #14338, .T. ) ;
#170200 = ORIENTED_EDGE ( 'NONE', *, *, #105721, .F. ) ;
#170201 =( NAMED_UNIT ( * ) PLANE_ANGLE_UNIT ( ) SI_UNIT ( $, .RADIAN. ) );
#170202 = LINE ( 'NONE', #51451, #153305 ) ;
#170203 = CARTESIAN_POINT ( 'NONE',  ( -16.88593481969334320, 63.08568185945787121, -213.1256680011580897 ) ) ;
#170204 = PRODUCT ( 'Injection Molded Chain Links 6', 'Injection Molded Chain Links 6', '', ( #93915 ) ) ;
#170205 = DIRECTION ( 'NONE',  ( 1.000000000000000000, 0.000000000000000000, 0.000000000000000000 ) ) ;
#170206 = EDGE_LOOP ( 'NONE', ( #82449, #142765, #27313, #240647 ) ) ;
#170207 = AXIS2_PLACEMENT_3D ( 'NONE', #81528, #41181, #221061 ) ;
#170208 = AXIS2_PLACEMENT_3D ( 'NONE', #71817, #131768, #31426 ) ;
#170209 = VERTEX_POINT ( 'NONE', #30327 ) ;
#170210 = CARTESIAN_POINT ( 'NONE',  ( 23.15000000000000213, 24.12844930803501242, -253.0488546976795021 ) ) ;
#170211 = DIRECTION ( 'NONE',  ( -1.000000000000000000, -2.885090398161910739E-16, -6.283419270304611573E-17 ) ) ;
#170212 = ORIENTED_EDGE ( 'NONE', *, *, #131915, .T. ) ;
#170213 = EDGE_CURVE ( 'NONE', #255434, #188196, #22703, .T. ) ;
#170214 = DIRECTION ( 'NONE',  ( -0.000000000000000000, -0.000000000000000000, -1.000000000000000000 ) ) ;
#170216 = ORIENTED_EDGE ( 'NONE', *, *, #226601, .T. ) ;
#170215 = CARTESIAN_POINT ( 'NONE',  ( 20.94999999999999574, 74.16465844978765176, -124.9679561919613207 ) ) ;
#170217 = FACE_BOUND ( 'NONE', #106382, .T. ) ;
#170218 = DIRECTION ( 'NONE',  ( 1.000000000000000000, 0.000000000000000000, -0.000000000000000000 ) ) ;
#170220 = ORIENTED_EDGE ( 'NONE', *, *, #185421, .T. ) ;
#170219 = CARTESIAN_POINT ( 'NONE',  ( -18.50000000000000711, 64.25000000001161027, -62.50830171387040934 ) ) ;
#170221 = AXIS2_PLACEMENT_3D ( 'NONE', #245588, #86472, #202602 ) ;
#170222 = DIRECTION ( 'NONE',  ( 0.000000000000000000, -0.4721928772777320149, -0.8814952561688444987 ) ) ;
#170223 = DIRECTION ( 'NONE',  ( -1.000000000000000000, -0.000000000000000000, -0.000000000000000000 ) ) ;
#170224 = CARTESIAN_POINT ( 'NONE',  ( -18.50000000000000000, 10.63601275468165142, -265.6051570720007931 ) ) ;
#170225 = TOROIDAL_SURFACE ( 'NONE', #203498, 4.900000000000000355, 0.1000000000000000056 ) ;
#170226 = FACE_OUTER_BOUND ( 'NONE', #70093, .T. ) ;
#170227 = EDGE_CURVE ( 'NONE', #89902, #81187, #190700, .T. ) ;
#170229 = DIRECTION ( 'NONE',  ( -1.000000000000000000, -0.000000000000000000, -0.000000000000000000 ) ) ;
#170228 = CARTESIAN_POINT ( 'NONE',  ( -20.64999999999999858, 7.250000000011155521, -112.8500000000000369 ) ) ;
#170230 = DIRECTION ( 'NONE',  ( 0.000000000000000000, -0.9908441862701791170, 0.1350103645450472789 ) ) ;
#170231 = AXIS2_PLACEMENT_3D ( 'NONE', #255535, #174822, #74427 ) ;
#170232 = LINE ( 'NONE', #150617, #97616 ) ;
#170233 = FACE_OUTER_BOUND ( 'NONE', #5841, .T. ) ;
#170234 = CARTESIAN_POINT ( 'NONE',  ( 20.85000000000000142, 77.83585931145546510, -91.51866831572576189 ) ) ;
#170236 = ORIENTED_EDGE ( 'NONE', *, *, #26071, .T. ) ;
#170235 = TOROIDAL_SURFACE ( 'NONE', #111944, 4.099999999999999645, 0.1000000000000000056 ) ;
#170237 = LINE ( 'NONE', #171498, #230515 ) ;
#170238 = EDGE_LOOP ( 'NONE', ( #45087, #85226, #1679, #162682 ) ) ;
#170239 = DIRECTION ( 'NONE',  ( -1.000000000000000000, -0.000000000000000000, 0.000000000000000000 ) ) ;
#170240 = ORIENTED_EDGE ( 'NONE', *, *, #117861, .T. ) ;
#170241 = EDGE_CURVE ( 'NONE', #44391, #84620, #176816, .T. ) ;
#170242 = CARTESIAN_POINT ( 'NONE',  ( -23.25000000000000000, 6.933893972137497030, -70.78564583437358237 ) ) ;
#170243 = DIRECTION ( 'NONE',  ( -0.000000000000000000, 1.000000000000000000, 6.982962677686266711E-15 ) ) ;
#170244 = AXIS2_PLACEMENT_3D ( 'NONE', #137493, #20150, #113473 ) ;
#170245 = CIRCLE ( 'NONE', #174533, 0.09999999999998898659 ) ;
#170246 = VERTEX_POINT ( 'NONE', #91569 ) ;
#170247 = AXIS2_PLACEMENT_3D ( 'NONE', #153130, #255980, #13587 ) ;
#170248 = DIRECTION ( 'NONE',  ( -1.000000000000000000, 0.000000000000000000, -0.000000000000000000 ) ) ;
#170249 = ADVANCED_FACE ( 'NONE', ( #171154 ), #255867, .T. ) ;
#170250 = VERTEX_POINT ( 'NONE', #112429 ) ;
#170251 = VERTEX_POINT ( 'NONE', #206385 ) ;
#170252 = DIRECTION ( 'NONE',  ( 0.000000000000000000, 0.000000000000000000, -1.000000000000000000 ) ) ;
#170253 = CARTESIAN_POINT ( 'NONE',  ( -20.54999999999999716, 2.400000000011155432, -113.7246219227621395 ) ) ;
#170254 = CARTESIAN_POINT ( 'NONE',  ( 21.05000000000000071, 68.35681244624937847, -231.7050464529141891 ) ) ;
#170255 = CARTESIAN_POINT ( 'NONE',  ( 13.54577453029515866, 27.84954713259350711, -234.1111166998236683 ) ) ;
#170256 = DIRECTION ( 'NONE',  ( 0.000000000000000000, 0.000000000000000000, -1.000000000000000000 ) ) ;
#170258 = DIRECTION ( 'NONE',  ( 0.000000000000000000, 1.000000000000000000, 0.000000000000000000 ) ) ;
#170257 = DIRECTION ( 'NONE',  ( 1.000000000000000000, 0.000000000000000000, 0.000000000000000000 ) ) ;
#170259 = CARTESIAN_POINT ( 'NONE',  ( 18.49999999999999289, 10.20857864377384416, -58.15000000000000568 ) ) ;
#170261 = EDGE_LOOP ( 'NONE', ( #247325, #179980, #2875, #93362, #116939, #133934, #171215, #117137, #169607, #111446, #99480 ) ) ;
#170260 = DIRECTION ( 'NONE',  ( 0.000000000000000000, 1.000000000000000000, 0.000000000000000000 ) ) ;
#170263 = CARTESIAN_POINT ( 'NONE',  ( -23.15000000000000213, 87.65000000001222702, -148.2731074845242176 ) ) ;
#170262 = DIRECTION ( 'NONE',  ( -0.000000000000000000, -6.982962677686266711E-15, 1.000000000000000000 ) ) ;
#170264 = CARTESIAN_POINT ( 'NONE',  ( -23.15000000000000213, 64.35000000001166143, -69.52310748452440237 ) ) ;
#170265 = ORIENTED_EDGE ( 'NONE', *, *, #135274, .T. ) ;
#170266 = CARTESIAN_POINT ( 'NONE',  ( -18.43599941264894326, -9.519327428583080675, -174.4729767895220220 ) ) ;
#170267 = CIRCLE ( 'NONE', #116066, 0.1000000000000018513 ) ;
#170268 = DIRECTION ( 'NONE',  ( 0.000000000000000000, 0.000000000000000000, 1.000000000000000000 ) ) ;
#170269 = ORIENTED_EDGE ( 'NONE', *, *, #41112, .T. ) ;
#170270 = DIRECTION ( 'NONE',  ( 1.000000000000000000, -0.000000000000000000, -0.000000000000000000 ) ) ;
#170271 = CARTESIAN_POINT ( 'NONE',  ( 23.15000000000000213, -11.64999999998883595, -197.8999999999999773 ) ) ;
#170272 = CARTESIAN_POINT ( 'NONE',  ( 15.52844286134407525, 66.62433047358608462, -87.15531747513846028 ) ) ;
#170273 = VERTEX_POINT ( 'NONE', #27777 ) ;
#170274 = ORIENTED_EDGE ( 'NONE', *, *, #161076, .F. ) ;
#170275 = CARTESIAN_POINT ( 'NONE',  ( 21.05000000000000071, 77.83534155023701828, -191.9679561919613491 ) ) ;
#170276 = DIRECTION ( 'NONE',  ( 0.000000000000000000, -0.2128009952263403282, 0.9770955615653358350 ) ) ;
#170277 = DIRECTION ( 'NONE',  ( 1.000000000000000000, 0.000000000000000000, 0.000000000000000000 ) ) ;
#170278 = ORIENTED_EDGE ( 'NONE', *, *, #128949, .F. ) ;
#170279 = CARTESIAN_POINT ( 'NONE',  ( -23.25000000000000000, -1.835859311443637010, -45.00443916879852679 ) ) ;
#170281 = EDGE_CURVE ( 'NONE', #153822, #200447, #6888, .T. ) ;
#170280 = CYLINDRICAL_SURFACE ( 'NONE', #133405, 0.9000000000000014655 ) ;
#170282 = LINE ( 'NONE', #69875, #28888 ) ;
#170283 = VECTOR ( 'NONE', #140782, 1000.000000000000000 ) ;
#170284 = DIRECTION ( 'NONE',  ( -3.265361837132813093E-16, 1.000000000000000000, 0.000000000000000000 ) ) ;
#170285 = AXIS2_PLACEMENT_3D ( 'NONE', #246778, #68153, #148997 ) ;
#170286 = AXIS2_PLACEMENT_3D ( 'NONE', #141369, #121830, #220895 ) ;
#170287 = EDGE_LOOP ( 'NONE', ( #176401, #95507, #157923, #215265 ) ) ;
#170288 = CARTESIAN_POINT ( 'NONE',  ( -23.15000000000000213, 1.910280373842936141, -146.6313678551989597 ) ) ;
#170290 = ORIENTED_EDGE ( 'NONE', *, *, #50169, .T. ) ;
#170289 = CARTESIAN_POINT ( 'NONE',  ( -16.94107738177414291, 65.98576071487519812, -82.07310748452438531 ) ) ;
#170291 = AXIS2_PLACEMENT_3D ( 'NONE', #18826, #99620, #254818 ) ;
#170292 = CARTESIAN_POINT ( 'NONE',  ( 23.14999999999999858, 76.00000000001126921, -203.5231074845248997 ) ) ;
#170293 = DIRECTION ( 'NONE',  ( -3.265361837132813093E-16, 1.000000000000000000, 0.000000000000000000 ) ) ;
#170294 = CARTESIAN_POINT ( 'NONE',  ( -21.14999999999999858, 41.46275801244657799, -260.2743004338703940 ) ) ;
#170295 = ADVANCED_FACE ( 'NONE', ( #66870 ), #107271, .T. ) ;
#170296 = DIRECTION ( 'NONE',  ( 0.000000000000000000, 0.000000000000000000, 1.000000000000000000 ) ) ;
#170297 = ORIENTED_EDGE ( 'NONE', *, *, #108665, .F. ) ;
#170298 = CARTESIAN_POINT ( 'NONE',  ( 21.08804582317332077, 8.878166167091915639, -12.34999982940562191 ) ) ;
#170299 = LINE ( 'NONE', #231522, #180170 ) ;
#170300 = DIRECTION ( 'NONE',  ( 0.000000000000000000, -1.000000000000000000, 0.000000000000000000 ) ) ;
#170301 = EDGE_CURVE ( 'NONE', #47971, #58501, #193400, .T. ) ;
#170302 = ORIENTED_EDGE ( 'NONE', *, *, #201246, .T. ) ;
#170303 = CARTESIAN_POINT ( 'NONE',  ( -23.15000000000000213, -11.38316329222462464, -203.4791315943886048 ) ) ;
#170304 = DIRECTION ( 'NONE',  ( -1.000000000000000000, -0.000000000000000000, -0.000000000000000000 ) ) ;
#170305 = CIRCLE ( 'NONE', #99309, 2.000000000000002665 ) ;
#170306 = TOROIDAL_SURFACE ( 'NONE', #24527, 11.90000000000000213, 0.1000000000000000056 ) ;
#170307 = CARTESIAN_POINT ( 'NONE',  ( -16.88460203013676519, 51.63142026009736441, -231.9356287555948199 ) ) ;
#170308 = CIRCLE ( 'NONE', #95244, 2.000000000000001776 ) ;
#170309 = CARTESIAN_POINT ( 'NONE',  ( 21.14999999999999858, 6.540656951712402467, -167.4999999999999716 ) ) ;
#170310 = ADVANCED_FACE ( 'NONE', ( #94128, #13323 ), #113698, .T. ) ;
#170311 = DIRECTION ( 'NONE',  ( 0.000000000000000000, 0.9274965247785529332, -0.3738317757009255171 ) ) ;
#170312 = AXIS2_PLACEMENT_3D ( 'NONE', #71078, #206716, #68497 ) ;
#170313 = EDGE_LOOP ( 'NONE', ( #124341, #86421, #185228, #190417 ) ) ;
#170314 = EDGE_LOOP ( 'NONE', ( #240048, #65344, #233505, #182345 ) ) ;
#170315 = DIRECTION ( 'NONE',  ( 1.000000000000000000, 0.000000000000000000, 0.000000000000000000 ) ) ;
#170316 = EDGE_CURVE ( 'NONE', #176651, #141149, #164160, .T. ) ;
#170317 = DIRECTION ( 'NONE',  ( -2.940209281316622988E-16, -0.4088369013363260529, 0.9126074666063779262 ) ) ;
#170318 = CARTESIAN_POINT ( 'NONE',  ( -21.64999999999999858, 21.39776787615277343, -233.0380739262505472 ) ) ;
#170319 = EDGE_CURVE ( 'NONE', #126259, #109005, #197452, .T. ) ;
#170320 = CARTESIAN_POINT ( 'NONE',  ( 23.15000000000000213, 87.65000000001246860, -173.1231074845242688 ) ) ;
#170321 = CARTESIAN_POINT ( 'NONE',  ( -21.22070241538126112, 6.469946272880768845, -133.9010809694649993 ) ) ;
#170322 = EDGE_CURVE ( 'NONE', #190824, #16272, #64376, .T. ) ;
#170323 = CARTESIAN_POINT ( 'NONE',  ( 22.42357213249528769, 7.672932386359915924, 0.09908696400155941886 ) ) ;
#170324 = DIRECTION ( 'NONE',  ( 1.000000000000000000, -0.000000000000000000, -0.000000000000000000 ) ) ;
#170325 = ADVANCED_FACE ( 'NONE', ( #74615 ), #5176, .T. ) ;
#170326 = LINE ( 'NONE', #252359, #245448 ) ;
#170328 = CARTESIAN_POINT ( 'NONE',  ( 21.05000000000000071, 5.399999999999998579, -12.40526601891309788 ) ) ;
#170327 = VECTOR ( 'NONE', #212653, 1000.000000000000114 ) ;
#170329 = ORIENTED_EDGE ( 'NONE', *, *, #200622, .T. ) ;
#170330 = LINE ( 'NONE', #205536, #215033 ) ;
#170331 = VERTEX_POINT ( 'NONE', #117548 ) ;
#170332 = CARTESIAN_POINT ( 'NONE',  ( -20.94999999999999929, 1.115600667400684642E-11, -200.9999999999999432 ) ) ;
#170334 = EDGE_CURVE ( 'NONE', #158504, #94457, #160072, .T. ) ;
#170333 = DIRECTION ( 'NONE',  ( 1.000000000000000000, 0.000000000000000000, -0.000000000000000000 ) ) ;
#170335 = AXIS2_PLACEMENT_3D ( 'NONE', #102133, #223381, #85135 ) ;
#170336 = CARTESIAN_POINT ( 'NONE',  ( 21.05543885634738643, 8.775771046858691804, -79.18438447071473263 ) ) ;
#170337 = CARTESIAN_POINT ( 'NONE',  ( -22.60000000000080789, -3.206176855256876124, -228.1422739711507859 ) ) ;
#170338 = CARTESIAN_POINT ( 'NONE',  ( 13.40000000000005898, 64.25000000001119815, -18.32310748452479388 ) ) ;
#170339 = CARTESIAN_POINT ( 'NONE',  ( 18.37172112093826115, 85.57096165225489415, -62.70637303104068394 ) ) ;
#170340 = CYLINDRICAL_SURFACE ( 'NONE', #35146, 0.1000000000000064587 ) ;
#170341 = ORIENTED_EDGE ( 'NONE', *, *, #60497, .T. ) ;
#170342 = EDGE_CURVE ( 'NONE', #186401, #104851, #114258, .T. ) ;
#170343 = DIRECTION ( 'NONE',  ( 0.000000000000000000, -0.9209589331071864615, 0.3896596508878908960 ) ) ;
#170344 = CARTESIAN_POINT ( 'NONE',  ( 18.59999999999999432, -1.162701749926853712, -142.1000000000000227 ) ) ;
#170345 = DIRECTION ( 'NONE',  ( 1.000000000000000000, 0.000000000000000000, 0.000000000000000000 ) ) ;
#170346 = CYLINDRICAL_SURFACE ( 'NONE', #251979, 0.09999999999999939493 ) ;
#170347 = AXIS2_PLACEMENT_3D ( 'NONE', #33185, #35738, #133523 ) ;
#170348 = CIRCLE ( 'NONE', #207738, 0.1000000000000015737 ) ;
#170349 = AXIS2_PLACEMENT_3D ( 'NONE', #43875, #84220, #166419 ) ;
#170350 = LINE ( 'NONE', #249838, #78923 ) ;
#170351 = AXIS2_PLACEMENT_3D ( 'NONE', #103554, #26634, #164847 ) ;
#170352 = ORIENTED_EDGE ( 'NONE', *, *, #81627, .T. ) ;
#170353 = DIRECTION ( 'NONE',  ( -1.000000000000000000, -0.000000000000000000, -0.000000000000000000 ) ) ;
#170355 = EDGE_CURVE ( 'NONE', #62202, #152968, #233660, .T. ) ;
#170354 = DIRECTION ( 'NONE',  ( 1.000000000000000000, -0.000000000000000000, -0.000000000000000000 ) ) ;
#170356 = EDGE_LOOP ( 'NONE', ( #14574, #214695, #158759, #21660 ) ) ;
#170357 = ORIENTED_EDGE ( 'NONE', *, *, #245037, .T. ) ;
#170358 = CARTESIAN_POINT ( 'NONE',  ( 21.05000000000000071, 11.65000000001115943, -167.5999999999999659 ) ) ;
#170359 = CARTESIAN_POINT ( 'NONE',  ( 18.59999999999999432, -9.480686695267811714, -73.94111516875786094 ) ) ;
#170360 = AXIS2_PLACEMENT_3D ( 'NONE', #82037, #258095, #79490 ) ;
#170361 = ORIENTED_EDGE ( 'NONE', *, *, #154586, .T. ) ;
#170362 = CARTESIAN_POINT ( 'NONE',  ( 20.12500000000000000, 40.07562767317620711, -237.3368484665046765 ) ) ;
#170363 = CARTESIAN_POINT ( 'NONE',  ( -22.50000000000000000, 76.00000000001199396, -109.2731074845243171 ) ) ;
#170364 = CIRCLE ( 'NONE', #203642, 0.09999999999999939493 ) ;
#170365 = ORIENTED_EDGE ( 'NONE', *, *, #104652, .T. ) ;
#170366 = EDGE_CURVE ( 'NONE', #101254, #88561, #214231, .T. ) ;
#170367 = CIRCLE ( 'NONE', #74690, 7.720710678118678061 ) ;
#170368 = AXIS2_PLACEMENT_3D ( 'NONE', #63688, #102795, #4976 ) ;
#170369 = AXIS2_PLACEMENT_3D ( 'NONE', #241353, #22317, #185218 ) ;
#170370 = DIRECTION ( 'NONE',  ( 0.000000000000000000, 0.5868805631290353597, 0.8096735173027127530 ) ) ;
#170371 = ORIENTED_EDGE ( 'NONE', *, *, #177704, .T. ) ;
#170372 = CARTESIAN_POINT ( 'NONE',  ( -21.05000000000000071, 69.38854649060172619, -247.7638912529787660 ) ) ;
#170373 = AXIS2_PLACEMENT_3D ( 'NONE', #111137, #250633, #88984 ) ;
#170374 = DIRECTION ( 'NONE',  ( 0.000000000000000000, 1.000000000000000000, 6.982962677686266711E-15 ) ) ;
#170377 = EDGE_CURVE ( 'NONE', #202760, #214529, #247542, .T. ) ;
#170376 = EDGE_LOOP ( 'NONE', ( #177223, #111040, #188070, #73999 ) ) ;
#170375 = FACE_OUTER_BOUND ( 'NONE', #97024, .T. ) ;
#170378 = FACE_OUTER_BOUND ( 'NONE', #79700, .T. ) ;
#170380 = UNCERTAINTY_MEASURE_WITH_UNIT (LENGTH_MEASURE( 1.000000000000000082E-05 ), #57419, 'distance_accuracy_value', 'NONE');
#170379 = LINE ( 'NONE', #133758, #198859 ) ;
#170381 = CARTESIAN_POINT ( 'NONE',  ( -22.59999999999999787, 11.45898712536580177, -198.4011321578509524 ) ) ;
#170382 = DIRECTION ( 'NONE',  ( 0.000000000000000000, 0.000000000000000000, 1.000000000000000000 ) ) ;
#170383 = DIRECTION ( 'NONE',  ( -1.000000000000000000, 0.000000000000000000, -0.000000000000000000 ) ) ;
#170384 = ADVANCED_FACE ( 'NONE', ( #39324 ), #53721, .T. ) ;
#170385 = DIRECTION ( 'NONE',  ( -1.000000000000000000, -0.000000000000000000, -0.000000000000000000 ) ) ;
#170386 = CARTESIAN_POINT ( 'NONE',  ( 23.14999999999999503, 6.650000000011155876, -54.85000000000000142 ) ) ;
#170387 = EDGE_CURVE ( 'NONE', #163445, #206620, #34197, .T. ) ;
#170389 = ORIENTED_EDGE ( 'NONE', *, *, #174078, .F. ) ;
#170388 = CARTESIAN_POINT ( 'NONE',  ( 22.57320508075688537, 64.35000000001214460, -136.5231074845243597 ) ) ;
#170390 = EDGE_LOOP ( 'NONE', ( #198965, #184658, #91494 ) ) ;
#170392 = CARTESIAN_POINT ( 'NONE',  ( -20.64999999999999858, 4.350000000011156054, -79.35000000000005116 ) ) ;
#170391 = CARTESIAN_POINT ( 'NONE',  ( 23.15000000000000213, 87.75000000001179501, -81.67310748452422331 ) ) ;
#170394 = EDGE_LOOP ( 'NONE', ( #63944, #9309, #86333, #252659 ) ) ;
#170393 = DIRECTION ( 'NONE',  ( 0.7071067811865474617, -0.7071067811865474617, -4.937700262164531476E-15 ) ) ;
#170395 = ORIENTED_EDGE ( 'NONE', *, *, #243595, .T. ) ;
#170396 = CARTESIAN_POINT ( 'NONE',  ( -21.07016717457007005, 1.556953976783240323, -230.7479980709940719 ) ) ;
#170397 = EDGE_CURVE ( 'NONE', #16494, #213315, #72788, .T. ) ;
#170398 = VECTOR ( 'NONE', #200107, 1000.000000000000000 ) ;
#170399 = PLANE ( 'NONE',  #47113 ) ;
#170401 = ADVANCED_FACE ( 'NONE', ( #17186 ), #255731, .F. ) ;
#170400 = CARTESIAN_POINT ( 'NONE',  ( -21.65000000000000213, 10.04999999999998295, -20.85000000000000142 ) ) ;
#170402 = CARTESIAN_POINT ( 'NONE',  ( 15.48841904831874849, 62.27936944010919973, -221.4051505845420991 ) ) ;
#170403 = CYLINDRICAL_SURFACE ( 'NONE', #4926, 0.1000000000000028644 ) ;
#170404 = LINE ( 'NONE', #107803, #256999 ) ;
#170405 = VECTOR ( 'NONE', #7638, 1000.000000000000000 ) ;
#170406 = CIRCLE ( 'NONE', #203683, 0.2000000000000057288 ) ;
#170407 = CARTESIAN_POINT ( 'NONE',  ( 21.05000000000000071, 48.50000630096247534, -244.2465039064066161 ) ) ;
#170408 = ORIENTED_EDGE ( 'NONE', *, *, #4800, .F. ) ;
#170409 = EDGE_LOOP ( 'NONE', ( #171397, #42087, #159895 ) ) ;
#170410 = LINE ( 'NONE', #208214, #64770 ) ;
#170411 = VECTOR ( 'NONE', #186336, 1000.000000000000227 ) ;
#170412 = ORIENTED_EDGE ( 'NONE', *, *, #183154, .T. ) ;
#170413 = CARTESIAN_POINT ( 'NONE',  ( 20.95512820512820440, 65.37615131630045084, -162.3581939154368285 ) ) ;
#170414 = ORIENTED_EDGE ( 'NONE', *, *, #147266, .T. ) ;
#170415 = DIRECTION ( 'NONE',  ( -0.000000000000000000, -0.9887567792719339499, -0.1495327102803676589 ) ) ;
#170416 = AXIS2_PLACEMENT_3D ( 'NONE', #64648, #25540, #163764 ) ;
#170417 = ADVANCED_FACE ( 'NONE', ( #159266 ), #60273, .T. ) ;
#170418 = CARTESIAN_POINT ( 'NONE',  ( 20.94999999999999929, 10.72371710470752504, -12.15000000000000036 ) ) ;
#170419 = CARTESIAN_POINT ( 'NONE',  ( -22.39999999999999858, 75.90000000001219860, -144.3138870828977076 ) ) ;
#170420 = ADVANCED_FACE ( 'NONE', ( #238790 ), #143661, .F. ) ;
#170421 = ORIENTED_EDGE ( 'NONE', *, *, #177492, .T. ) ;
#170422 = EDGE_CURVE ( 'NONE', #87397, #72158, #251810, .T. ) ;
#170423 = CYLINDRICAL_SURFACE ( 'NONE', #112939, 0.1000000000000028644 ) ;
#170424 = ORIENTED_EDGE ( 'NONE', *, *, #181837, .F. ) ;
#170425 = AXIS2_PLACEMENT_3D ( 'NONE', #27876, #164788, #89090 ) ;
#170426 = DIRECTION ( 'NONE',  ( 1.000000000000000000, 0.000000000000000000, 0.000000000000000000 ) ) ;
#170427 = AXIS2_PLACEMENT_3D ( 'NONE', #185789, #28032, #7136 ) ;
#170428 = ORIENTED_EDGE ( 'NONE', *, *, #243861, .T. ) ;
#170429 = EDGE_CURVE ( 'NONE', #96910, #238407, #47776, .T. ) ;
#170430 = DIRECTION ( 'NONE',  ( 0.000000000000000000, 0.4999999999999088507, -0.8660254037844913322 ) ) ;
#170431 = ORIENTED_EDGE ( 'NONE', *, *, #247710, .F. ) ;
#170434 = ORIENTED_EDGE ( 'NONE', *, *, #50853, .F. ) ;
#170433 = CARTESIAN_POINT ( 'NONE',  ( 18.50000324121758055, 46.33100819526736558, -243.0553980158186391 ) ) ;
#170432 = CARTESIAN_POINT ( 'NONE',  ( 21.10000000000000142, -11.75000000000000000, 12.09999999999999609 ) ) ;
#170435 = DIRECTION ( 'NONE',  ( 1.000000000000000000, 0.000000000000000000, 0.000000000000000000 ) ) ;
#170436 = VECTOR ( 'NONE', #111033, 1000.000000000000000 ) ;
#170437 = ORIENTED_EDGE ( 'NONE', *, *, #37365, .F. ) ;
#170438 = CARTESIAN_POINT ( 'NONE',  ( 20.85000000000000142, 76.00000000001213607, -136.5231074845243313 ) ) ;
#170439 = ORIENTED_EDGE ( 'NONE', *, *, #60511, .F. ) ;
#170440 = FACE_OUTER_BOUND ( 'NONE', #128616, .T. ) ;
#170441 = EDGE_LOOP ( 'NONE', ( #118945, #50380, #125947, #94282 ) ) ;
#170442 = LINE ( 'NONE', #230355, #168382 ) ;
#170443 = LINE ( 'NONE', #187399, #167855 ) ;
#170444 = DIRECTION ( 'NONE',  ( 0.000000000000000000, 1.000000000000000000, -0.000000000000000000 ) ) ;
#170445 = CARTESIAN_POINT ( 'NONE',  ( -18.39999999999999858, 85.68240343348880117, -163.3662641071115047 ) ) ;
#170446 = EDGE_CURVE ( 'NONE', #163287, #234881, #65278, .T. ) ;
#170447 = ORIENTED_EDGE ( 'NONE', *, *, #252726, .F. ) ;
#170448 = DIRECTION ( 'NONE',  ( 0.000000000000000000, -1.000000000000000000, -6.982962677686265922E-15 ) ) ;
#170449 = DIRECTION ( 'NONE',  ( -1.000000000000000000, -9.012599976027990443E-15, -6.882867235861669241E-14 ) ) ;
#170450 = CIRCLE ( 'NONE', #116433, 0.1000000000000013933 ) ;
#170451 = CARTESIAN_POINT ( 'NONE',  ( -12.84409460144757098, 66.58931770574434950, -154.5919640425762225 ) ) ;
#170452 = VERTEX_POINT ( 'NONE', #224350 ) ;
#170453 = CARTESIAN_POINT ( 'NONE',  ( -18.59999999999999787, 1.736257131608553550, -179.0686523290174819 ) ) ;
#170454 = ORIENTED_EDGE ( 'NONE', *, *, #234905, .T. ) ;
#170455 = DIRECTION ( 'NONE',  ( -2.602085213965226419E-14, -0.000000000000000000, -1.000000000000000000 ) ) ;
#170456 = ORIENTED_EDGE ( 'NONE', *, *, #104010, .F. ) ;
#170457 = CARTESIAN_POINT ( 'NONE',  ( 18.59999999999999787, 47.95459712139159336, -246.5019368548292675 ) ) ;
#170458 = CARTESIAN_POINT ( 'NONE',  ( -22.60000000000094289, 75.89914163091394528, -181.7726746080137730 ) ) ;
#170460 = ORIENTED_EDGE ( 'NONE', *, *, #223238, .F. ) ;
#170459 = FACE_OUTER_BOUND ( 'NONE', #680, .T. ) ;
#170461 = CARTESIAN_POINT ( 'NONE',  ( -21.65000000000000213, 9.949999999999985079, -12.65000000000000213 ) ) ;
#170462 = ORIENTED_EDGE ( 'NONE', *, *, #119533, .T. ) ;
#170463 = CARTESIAN_POINT ( 'NONE',  ( 19.97071067811864609, 11.72071067812981404, -58.15000000000000568 ) ) ;
#170464 = EDGE_CURVE ( 'NONE', #44597, #206865, #230990, .T. ) ;
#170465 = CARTESIAN_POINT ( 'NONE',  ( 20.12500000000000000, 9.750000000011153745, -54.65000000000000568 ) ) ;
#170466 = VERTEX_POINT ( 'NONE', #104379 ) ;
#170467 = AXIS2_PLACEMENT_3D ( 'NONE', #42645, #217415, #19235 ) ;
#170469 = AXIS2_PLACEMENT_3D ( 'NONE', #6889, #186832, #27778 ) ;
#170468 = FACE_OUTER_BOUND ( 'NONE', #18613, .T. ) ;
#170471 = EDGE_CURVE ( 'NONE', #17853, #163251, #139365, .T. ) ;
#170470 = CARTESIAN_POINT ( 'NONE',  ( 18.59999999999999432, 1.728086936794463346, 13.11556499483223348 ) ) ;
#170472 = ORIENTED_EDGE ( 'NONE', *, *, #9210, .F. ) ;
#170473 = AXIS2_PLACEMENT_3D ( 'NONE', #109001, #188550, #69918 ) ;
#170475 = DIRECTION ( 'NONE',  ( -1.000000000000000000, -0.000000000000000000, -0.000000000000000000 ) ) ;
#170474 = AXIS2_PLACEMENT_3D ( 'NONE', #73658, #180132, #1470 ) ;
#170476 = EDGE_LOOP ( 'NONE', ( #113087, #120715, #250366, #254045 ) ) ;
#170477 = ADVANCED_FACE ( 'NONE', ( #79687 ), #89477, .F. ) ;
#170478 = CARTESIAN_POINT ( 'NONE',  ( 12.30626653967340900, 9.356790025057035720, -117.7048265086139338 ) ) ;
#170479 = VECTOR ( 'NONE', #195902, 1000.000000000000000 ) ;
#170481 = EDGE_CURVE ( 'NONE', #219794, #119221, #120717, .T. ) ;
#170480 = CARTESIAN_POINT ( 'NONE',  ( -18.47690164073606667, -9.464844538001081276, -73.70138093983609906 ) ) ;
#170484 = ORIENTED_EDGE ( 'NONE', *, *, #241913, .T. ) ;
#170483 = VERTEX_POINT ( 'NONE', #63998 ) ;
#170482 = FACE_OUTER_BOUND ( 'NONE', #141723, .T. ) ;
#170486 = DIRECTION ( 'NONE',  ( 1.000000000000000000, 0.000000000000000000, 0.000000000000000000 ) ) ;
#170485 = CIRCLE ( 'NONE', #124651, 0.1000000000000013933 ) ;
#170487 = AXIS2_PLACEMENT_3D ( 'NONE', #47035, #206136, #50881 ) ;
#170488 = CARTESIAN_POINT ( 'NONE',  ( 21.14999999999999503, 75.39949836213487799, -250.2448839681187849 ) ) ;
#170489 = CARTESIAN_POINT ( 'NONE',  ( -16.94445028196807002, 9.992063609697737547, -20.89266982158155628 ) ) ;
#170490 = TOROIDAL_SURFACE ( 'NONE', #233194, 12.77499999999999858, 0.1000000000000000056 ) ;
#170492 = LINE ( 'NONE', #150868, #146094 ) ;
#170491 = DIRECTION ( 'NONE',  ( 1.000000000000000000, -0.000000000000000000, 0.000000000000000000 ) ) ;
#170493 = CARTESIAN_POINT ( 'NONE',  ( 21.05000000000000071, 69.74218538953552127, -69.62089777583315708 ) ) ;
#170494 = DIRECTION ( 'NONE',  ( 0.000000000000000000, 0.000000000000000000, -1.000000000000000000 ) ) ;
#170495 = LINE ( 'NONE', #208298, #222542 ) ;
#170496 = LINE ( 'NONE', #13946, #242407 ) ;
#170497 = ADVANCED_FACE ( 'NONE', ( #139654 ), #180108, .F. ) ;
#170498 = EDGE_CURVE ( 'NONE', #159544, #68788, #22331, .T. ) ;
#170499 = ORIENTED_EDGE ( 'NONE', *, *, #151999, .T. ) ;
#170500 = EDGE_LOOP ( 'NONE', ( #64263, #42447, #149825, #9247 ) ) ;
#170501 = CARTESIAN_POINT ( 'NONE',  ( -22.59999999999999787, 11.74956712350054744, -33.39914163090129762 ) ) ;
#170503 = ORIENTED_EDGE ( 'NONE', *, *, #26461, .T. ) ;
#170502 = CARTESIAN_POINT ( 'NONE',  ( -23.15000000000000213, 85.00000000001251976, -179.9170766071767389 ) ) ;
#170504 = ORIENTED_EDGE ( 'NONE', *, *, #209158, .T. ) ;
#170505 = DIRECTION ( 'NONE',  ( 0.000000000000000000, -6.982962677686266711E-15, 1.000000000000000000 ) ) ;
#170506 =( BOUNDED_SURFACE ( )  B_SPLINE_SURFACE ( 3, 2, ( 
 ( #147419, #152592, #9190 ),
 ( #209974, #88703, #109561 ),
 ( #92567, #69195, #127864 ),
 ( #251655, #249106, #106992 ),
 ( #169601, #148717, #70490 ),
 ( #228252, #186558, #7924 ) ),
 .UNSPECIFIED., .F., .F., .F. ) 
 B_SPLINE_SURFACE_WITH_KNOTS ( ( 4, 2, 4 ),
 ( 3, 3 ),
 ( 0.0001792624049599619591, 0.0003686986002124806685, 0.0005581347954649993779 ),
 ( 0.000000000000000000, 1.000000000000000000 ),
 .UNSPECIFIED. ) 
 GEOMETRIC_REPRESENTATION_ITEM ( )  RATIONAL_B_SPLINE_SURFACE ( (
 ( 1.000000000000000000, 0.9238795325112744150, 1.000000000000000000),
 ( 1.000000000000000000, 0.9229318695233699188, 1.000000000000000000),
 ( 1.000000000000000000, 0.8926288119236824858, 1.000000000000000000),
 ( 1.000000000000000000, 0.8123777807264993545, 1.000000000000000000),
 ( 1.000000000000000000, 0.7629087100935405541, 1.000000000000000000),
 ( 1.000000000000000000, 0.7071067811866220687, 1.000000000000000000) ) ) 
 REPRESENTATION_ITEM ( '' )  SURFACE ( )  );
#170507 = ORIENTED_EDGE ( 'NONE', *, *, #187504, .F. ) ;
#170508 = CARTESIAN_POINT ( 'NONE',  ( 21.04999999999999716, 43.40169206266419621, -234.8839448309778106 ) ) ;
#170509 = EDGE_CURVE ( 'NONE', #17499, #54475, #26944, .T. ) ;
#170510 = ORIENTED_EDGE ( 'NONE', *, *, #158866, .T. ) ;
#170511 = CARTESIAN_POINT ( 'NONE',  ( 18.52928932188133970, 10.27928932189250411, -125.1500000000000341 ) ) ;
#170512 = DIRECTION ( 'NONE',  ( 0.000000000000000000, -7.086529944415894657E-15, 1.000000000000000000 ) ) ;
#170513 = ADVANCED_FACE ( 'NONE', ( #103101 ), #19754, .T. ) ;
#170514 = B_SPLINE_CURVE_WITH_KNOTS ( 'NONE', 3,
 ( #191775, #7978, #247860, #48370 ),
 .UNSPECIFIED., .F., .F.,
 ( 4, 4 ),
 ( 0.000000000000000000, 0.0002118541922231814993 ),
 .UNSPECIFIED. ) ;
#170515 = CIRCLE ( 'NONE', #199716, 0.09999999999999939493 ) ;
#170517 = ORIENTED_EDGE ( 'NONE', *, *, #23443, .F. ) ;
#170516 = VERTEX_POINT ( 'NONE', #242623 ) ;
#170518 = VERTEX_POINT ( 'NONE', #46979 ) ;
#170519 = ORIENTED_EDGE ( 'NONE', *, *, #74619, .T. ) ;
#170520 = ORIENTED_EDGE ( 'NONE', *, *, #162515, .F. ) ;
#170521 = DIRECTION ( 'NONE',  ( 0.000000000000000000, -0.2617529984165035684, -0.9651348961777156399 ) ) ;
#170522 = CYLINDRICAL_SURFACE ( 'NONE', #199008, 0.09999999999999724387 ) ;
#170523 = CARTESIAN_POINT ( 'NONE',  ( -23.25000000000000000, 11.75000000001115552, -55.25000000000004974 ) ) ;
#170525 = ORIENTED_EDGE ( 'NONE', *, *, #67990, .T. ) ;
#170524 = DIRECTION ( 'NONE',  ( 1.000000000000000000, 0.000000000000000000, -0.000000000000000000 ) ) ;
#170526 = AXIS2_PLACEMENT_3D ( 'NONE', #167307, #208972, #30356 ) ;
#170527 = DIRECTION ( 'NONE',  ( 0.000000000000000000, -1.000000000000000000, 0.000000000000000000 ) ) ;
#170528 = EDGE_CURVE ( 'NONE', #257284, #101749, #247769, .T. ) ;
#170529 = DIRECTION ( 'NONE',  ( 2.715809747126116508E-16, -1.000000000000000000, 0.000000000000000000 ) ) ;
#170531 = ORIENTED_EDGE ( 'NONE', *, *, #83740, .F. ) ;
#170530 = CARTESIAN_POINT ( 'NONE',  ( -20.94999999999999929, 55.49311008795314137, -234.6486875357297492 ) ) ;
#170532 = ORIENTED_EDGE ( 'NONE', *, *, #200971, .F. ) ;
#170533 = CARTESIAN_POINT ( 'NONE',  ( 18.59999999999999787, 1.115600667400684642E-11, -67.00000000000004263 ) ) ;
#170534 = VERTEX_POINT ( 'NONE', #26170 ) ;
#170535 = CYLINDRICAL_SURFACE ( 'NONE', #114314, 0.5000000000000014433 ) ;
#170536 = DIRECTION ( 'NONE',  ( -2.978066053179067751E-16, 1.000000000000000000, 2.382452842543254201E-15 ) ) ;
#170538 = EDGE_CURVE ( 'NONE', #189217, #247064, #64329, .T. ) ;
#170537 = ORIENTED_EDGE ( 'NONE', *, *, #241311, .T. ) ;
#170541 = CARTESIAN_POINT ( 'NONE',  ( -21.05000000000000071, 87.48912529308852015, -172.9231074845242802 ) ) ;
#170540 = DIRECTION ( 'NONE',  ( 0.000000000000000000, 0.000000000000000000, -1.000000000000000000 ) ) ;
#170539 = AXIS2_PLACEMENT_3D ( 'NONE', #220883, #61832, #202618 ) ;
#170542 = CIRCLE ( 'NONE', #8003, 12.77499999999999503 ) ;
#170543 = DIRECTION ( 'NONE',  ( 0.000000000000000000, -7.116814260417668513E-15, 1.000000000000000000 ) ) ;
#170544 = DIRECTION ( 'NONE',  ( 1.000000000000000000, 0.000000000000000000, 0.000000000000000000 ) ) ;
#170545 = CARTESIAN_POINT ( 'NONE',  ( -21.05000000000000071, 6.300000000011169554, -134.1000000000000227 ) ) ;
#170546 = AXIS2_PLACEMENT_3D ( 'NONE', #131819, #70600, #229645 ) ;
#170547 = ORIENTED_EDGE ( 'NONE', *, *, #136160, .T. ) ;
#170548 = ORIENTED_EDGE ( 'NONE', *, *, #102941, .T. ) ;
#170549 = CARTESIAN_POINT ( 'NONE',  ( 20.95429402530546170, 8.876194151102188457, -8.523086697937838352 ) ) ;
#170550 = CARTESIAN_POINT ( 'NONE',  ( -23.15000000000000213, 1.580567032079710055, -244.0902705724231794 ) ) ;
#170551 = ORIENTED_EDGE ( 'NONE', *, *, #117769, .T. ) ;
#170552 = CARTESIAN_POINT ( 'NONE',  ( -21.05000000000000071, 0.000000000000000000, -21.69999999999999929 ) ) ;
#170553 = ORIENTED_EDGE ( 'NONE', *, *, #87392, .T. ) ;
#170554 = ADVANCED_FACE ( 'NONE', ( #186525 ), #197821, .T. ) ;
#170555 = CARTESIAN_POINT ( 'NONE',  ( 18.54999999999999716, 66.05000000001186322, -90.37310748452443931 ) ) ;
#170556 = DIRECTION ( 'NONE',  ( 0.000000000000000000, 0.000000000000000000, 1.000000000000000000 ) ) ;
#170557 = AXIS2_PLACEMENT_3D ( 'NONE', #254220, #157762, #153912 ) ;
#170558 = AXIS2_PLACEMENT_3D ( 'NONE', #75379, #154918, #135305 ) ;
#170559 = DIRECTION ( 'NONE',  ( 0.000000000000000000, -1.000000000000000000, 1.713307136767217392E-15 ) ) ;
#170560 = VERTEX_POINT ( 'NONE', #6584 ) ;
#170561 = CARTESIAN_POINT ( 'NONE',  ( -21.14999999999994174, 87.60324567546805952, -34.17184040628037422 ) ) ;
#170563 = EDGE_LOOP ( 'NONE', ( #42917, #176241, #146009 ) ) ;
#170562 = VECTOR ( 'NONE', #124980, 1000.000000000000000 ) ;
#170564 = ORIENTED_EDGE ( 'NONE', *, *, #208392, .T. ) ;
#170565 = AXIS2_PLACEMENT_3D ( 'NONE', #209411, #132449, #170343 ) ;
#170566 = COLOUR_RGB ( '', 0.66274510, 0.83137255, 0.94901961) ;
#170567 = ORIENTED_EDGE ( 'NONE', *, *, #201177, .T. ) ;
#170568 = TOROIDAL_SURFACE ( 'NONE', #45623, 4.149999999999999467, 0.1000000000000000056 ) ;
#170569 = CARTESIAN_POINT ( 'NONE',  ( -18.59999999999999787, 68.75000000001199396, -115.1731074845243512 ) ) ;
#170570 = CARTESIAN_POINT ( 'NONE',  ( -18.59999999999999787, 1.115600667400684642E-11, -167.4999999999999716 ) ) ;
#170571 = CARTESIAN_POINT ( 'NONE',  ( -21.08376601933334271, 0.06377601094103312052, -127.6580527287243001 ) ) ;
#170572 = CARTESIAN_POINT ( 'NONE',  ( 20.94999999999999929, 19.05165861791954285, -232.6888762659126826 ) ) ;
#170573 = DIRECTION ( 'NONE',  ( -3.265361837132813093E-16, 1.000000000000000000, 0.000000000000000000 ) ) ;
#170574 = VECTOR ( 'NONE', #38048, 1000.000000000000000 ) ;
#170575 = CARTESIAN_POINT ( 'NONE',  ( 22.48508240969612260, -3.118744460784280914, -228.1908567849118867 ) ) ;
#170577 = EDGE_LOOP ( 'NONE', ( #98913, #59821, #46598, #49574 ) ) ;
#170576 = FACE_OUTER_BOUND ( 'NONE', #445, .T. ) ;
#170578 = CARTESIAN_POINT ( 'NONE',  ( -21.14999999999994174, 73.58898499266442172, -51.80813886865390572 ) ) ;
#170579 = EDGE_LOOP ( 'NONE', ( #85400, #242549, #204939, #144239 ) ) ;
#170580 = LINE ( 'NONE', #132688, #198787 ) ;
#170581 = VERTEX_POINT ( 'NONE', #206082 ) ;
#170582 = EDGE_LOOP ( 'NONE', ( #17669, #240689, #238357, #35147 ) ) ;
#170583 = DIRECTION ( 'NONE',  ( 0.000000000000000000, 0.000000000000000000, -1.000000000000000000 ) ) ;
#170584 = CARTESIAN_POINT ( 'NONE',  ( -16.93906926870270624, 10.01214687095770906, -46.05345230722682004 ) ) ;
#170585 = DIRECTION ( 'NONE',  ( 0.000000000000000000, -0.8660254037844377084, -0.5000000000000016653 ) ) ;
#170586 = DIRECTION ( 'NONE',  ( 0.000000000000000000, 0.9908441862701600211, -0.1350103645451876666 ) ) ;
#170587 = AXIS2_PLACEMENT_3D ( 'NONE', #10459, #105670, #146100 ) ;
#170588 = CARTESIAN_POINT ( 'NONE',  ( 20.89192007715127986, 18.40923646582965034, -236.9894833875398206 ) ) ;
#170589 = VERTEX_POINT ( 'NONE', #33581 ) ;
#170590 = ORIENTED_EDGE ( 'NONE', *, *, #136519, .T. ) ;
#170591 = FACE_OUTER_BOUND ( 'NONE', #128111, .T. ) ;
#170592 = ORIENTED_EDGE ( 'NONE', *, *, #253676, .F. ) ;
#170593 = CARTESIAN_POINT ( 'NONE',  ( 22.50000000000000000, 75.90000000001273861, -211.3138870828977360 ) ) ;
#170594 = EDGE_LOOP ( 'NONE', ( #187666, #225948, #175653, #1878 ) ) ;
#170595 = DIRECTION ( 'NONE',  ( 1.000000000000000000, -0.000000000000000000, -0.000000000000000000 ) ) ;
#170596 = CARTESIAN_POINT ( 'NONE',  ( -20.87155475150660777, 11.75000000001115197, -60.09558652915745114 ) ) ;
#170597 = CYLINDRICAL_SURFACE ( 'NONE', #115430, 11.75000000000001066 ) ;
#170598 = DIRECTION ( 'NONE',  ( 0.000000000000000000, -0.9942466578594181259, 0.1071148137998542138 ) ) ;
#170599 = ORIENTED_EDGE ( 'NONE', *, *, #181547, .F. ) ;
#170600 = DIRECTION ( 'NONE',  ( 0.000000000000000000, 0.000000000000000000, -1.000000000000000000 ) ) ;
#170601 = CARTESIAN_POINT ( 'NONE',  ( 20.94999999999999929, 71.00000000001223555, -148.9283735034374843 ) ) ;
#170602 = CARTESIAN_POINT ( 'NONE',  ( -23.25000000000000000, 2.000000000011154189, -46.72462192276210402 ) ) ;
#170603 = AXIS2_PLACEMENT_3D ( 'NONE', #160123, #239640, #35061 ) ;
#170604 = DIRECTION ( 'NONE',  ( 0.000000000000000000, 3.469446951953515108E-14, 1.000000000000000000 ) ) ;
#170606 = EDGE_CURVE ( 'NONE', #115375, #216022, #87399, .T. ) ;
#170605 = CARTESIAN_POINT ( 'NONE',  ( 20.04142135623730070, 11.65000000001115943, -121.8500000000000369 ) ) ;
#170607 = VECTOR ( 'NONE', #191171, 1000.000000000000000 ) ;
#170608 = DIRECTION ( 'NONE',  ( 0.000000000000000000, 0.000000000000000000, 1.000000000000000000 ) ) ;
#170609 = AXIS2_PLACEMENT_3D ( 'NONE', #126593, #27535, #107011 ) ;
#170610 = ORIENTED_EDGE ( 'NONE', *, *, #55270, .T. ) ;
#170611 =( BOUNDED_CURVE ( )  B_SPLINE_CURVE ( 3, ( #82353, #257123, #98062, #240193 ),
 .UNSPECIFIED., .F., .T. ) 
 B_SPLINE_CURVE_WITH_KNOTS ( ( 4, 4 ),
 ( 3.752122642744585068, 4.712388980384675463 ),
 .UNSPECIFIED. ) 
 CURVE ( )  GEOMETRIC_REPRESENTATION_ITEM ( )  RATIONAL_B_SPLINE_CURVE ( ( 1.000000000000000000, 0.9246222802177217481, 0.9246222802177217481, 1.000000000000000000 ) ) 
 REPRESENTATION_ITEM ( '' )  );
#170612 = CARTESIAN_POINT ( 'NONE',  ( 21.12400247839510214, 10.72148804403030198, -12.25000000000000178 ) ) ;
#170613 = ADVANCED_FACE ( 'NONE', ( #9163 ), #113072, .T. ) ;
#170614 = ORIENTED_EDGE ( 'NONE', *, *, #51005, .F. ) ;
#170615 = CARTESIAN_POINT ( 'NONE',  ( 14.45204356427542614, 66.54933111084474717, -154.9675609943171253 ) ) ;
#170616 = CARTESIAN_POINT ( 'NONE',  ( -16.94132844910802760, 14.21029813284434695, -219.2911855031067034 ) ) ;
#170617 = DIRECTION ( 'NONE',  ( -1.000000000000000000, -0.000000000000000000, -0.000000000000000000 ) ) ;
#170618 = CARTESIAN_POINT ( 'NONE',  ( -21.05000000000000071, 77.26178616857662007, -61.43660852097883662 ) ) ;
#170619 = CARTESIAN_POINT ( 'NONE',  ( 23.24999999999999645, 7.128833340093095217, -233.7327013124392749 ) ) ;
#170620 = CARTESIAN_POINT ( 'NONE',  ( 20.97217846901852312, 67.12455827530264685, -161.5218798005872145 ) ) ;
#170622 = EDGE_CURVE ( 'NONE', #224045, #180552, #228219, .T. ) ;
#170621 = AXIS2_PLACEMENT_3D ( 'NONE', #25627, #179582, #201688 ) ;
#170623 = EDGE_LOOP ( 'NONE', ( #55831, #226187, #111000, #118439 ) ) ;
#170624 = CARTESIAN_POINT ( 'NONE',  ( -18.40000000000000213, 64.51332499825441857, -127.2731074845243882 ) ) ;
#170625 = AXIS2_PLACEMENT_3D ( 'NONE', #140932, #58789, #142201 ) ;
#170626 = DIRECTION ( 'NONE',  ( -1.000000000000000000, 2.952720810173289112E-16, 2.061873921506763405E-30 ) ) ;
#170627 = FACE_OUTER_BOUND ( 'NONE', #158247, .T. ) ;
#170628 = PLANE ( 'NONE',  #71634 ) ;
#170629 = DIRECTION ( 'NONE',  ( 0.000000000000000000, -1.000000000000000000, -6.982962677686265922E-15 ) ) ;
#170630 = VERTEX_POINT ( 'NONE', #147388 ) ;
#170631 = VERTEX_POINT ( 'NONE', #252564 ) ;
#170632 = DIRECTION ( 'NONE',  ( 0.000000000000000000, -0.2617529984165035128, -0.9651348961777155289 ) ) ;
#170633 = FACE_OUTER_BOUND ( 'NONE', #204328, .T. ) ;
#170635 = EDGE_CURVE ( 'NONE', #38009, #168616, #165693, .T. ) ;
#170634 = CARTESIAN_POINT ( 'NONE',  ( 23.24999999999999645, 73.90000000001190017, -103.0231074845243171 ) ) ;
#170636 = CARTESIAN_POINT ( 'NONE',  ( -21.53752568617684915, 69.21319212550857003, -170.1220819458087306 ) ) ;
#170637 = EDGE_CURVE ( 'NONE', #129641, #23721, #14517, .T. ) ;
#170638 = ORIENTED_EDGE ( 'NONE', *, *, #215394, .F. ) ;
#170639 = DIRECTION ( 'NONE',  ( 1.186688945009009831E-16, -0.9770955615653313941, -0.2128009952263603677 ) ) ;
#170640 = EDGE_CURVE ( 'NONE', #48880, #242139, #81111, .T. ) ;
#170641 = LINE ( 'NONE', #211001, #129891 ) ;
#170642 = ORIENTED_EDGE ( 'NONE', *, *, #88206, .T. ) ;
#170643 = CARTESIAN_POINT ( 'NONE',  ( -18.59999999999999787, -1.162701749926853712, -142.1000000000000227 ) ) ;
#170644 = CIRCLE ( 'NONE', #8101, 0.1000000000000028644 ) ;
#170645 = EDGE_CURVE ( 'NONE', #164855, #60863, #160267, .T. ) ;
#170646 = EDGE_LOOP ( 'NONE', ( #2259, #214376, #79350, #118223 ) ) ;
#170647 = ORIENTED_EDGE ( 'NONE', *, *, #58134, .F. ) ;
#170648 = VERTEX_POINT ( 'NONE', #15272 ) ;
#170649 = CARTESIAN_POINT ( 'NONE',  ( 5.999999999999997335, -11.34999999999999964, 13.90000000000000213 ) ) ;
#170650 = DIRECTION ( 'NONE',  ( 1.000000000000000000, -5.204170427930452838E-14, 0.000000000000000000 ) ) ;
#170651 = CARTESIAN_POINT ( 'NONE',  ( 21.14999999999999858, 64.25000000001269029, -203.4231074845244507 ) ) ;
#170652 = FACE_OUTER_BOUND ( 'NONE', #70108, .T. ) ;
#170653 = DIRECTION ( 'NONE',  ( -1.000000000000000000, 3.265361837132813093E-16, 2.280189983783949500E-30 ) ) ;
#170654 = CARTESIAN_POINT ( 'NONE',  ( 18.59999999999999076, 11.01970663298110154, -220.3481540650095098 ) ) ;
#170655 = EDGE_CURVE ( 'NONE', #96043, #233701, #193904, .T. ) ;
#170657 = CARTESIAN_POINT ( 'NONE',  ( -20.65000000000000568, 17.95055421627409231, -233.1200372299043693 ) ) ;
#170656 = CARTESIAN_POINT ( 'NONE',  ( 21.00000000000000000, 66.25000000001179501, -81.87310748452438247 ) ) ;
#170658 = AXIS2_PLACEMENT_3D ( 'NONE', #75068, #234099, #169039 ) ;
#170659 = CARTESIAN_POINT ( 'NONE',  ( 20.85000000000000142, 1.115600667400684642E-11, -167.5000000000000284 ) ) ;
#170660 = AXIS2_PLACEMENT_3D ( 'NONE', #248423, #222751, #44140 ) ;
#170661 = CARTESIAN_POINT ( 'NONE',  ( 20.95512828230143398, 22.07647316018445949, -231.6703166944364511 ) ) ;
#170662 = CARTESIAN_POINT ( 'NONE',  ( 18.59999999999999787, -1.835341550213255957, -45.05515129256298223 ) ) ;
#170663 = VECTOR ( 'NONE', #10913, 1000.000000000000000 ) ;
#170665 = CARTESIAN_POINT ( 'NONE',  ( 20.95566103547454517, 18.87012517599244177, -227.9764669589508514 ) ) ;
#170664 = CIRCLE ( 'NONE', #179028, 0.2000000000000057288 ) ;
#170666 = EDGE_LOOP ( 'NONE', ( #208942, #111687, #223997, #223641 ) ) ;
#170667 = CARTESIAN_POINT ( 'NONE',  ( -18.44204374631835819, -9.491036389598342282, -40.12620127022106686 ) ) ;
#170668 = DIRECTION ( 'NONE',  ( 1.000000000000000000, 0.000000000000000000, 0.000000000000000000 ) ) ;
#170669 = DIRECTION ( 'NONE',  ( 1.000000000000000000, 2.952720810173289112E-16, -0.000000000000000000 ) ) ;
#170670 = CIRCLE ( 'NONE', #228877, 0.09999999999999992228 ) ;
#170671 = DIRECTION ( 'NONE',  ( 0.000000000000000000, 7.056502275159890043E-15, -1.000000000000000000 ) ) ;
#170672 = DIRECTION ( 'NONE',  ( 0.000000000000000000, -1.000000000000000000, -0.000000000000000000 ) ) ;
#170673 = CARTESIAN_POINT ( 'NONE',  ( 18.59999999999999787, 1.851028230140860487, -11.65391326942249250 ) ) ;
#170674 = ORIENTED_EDGE ( 'NONE', *, *, #108785, .T. ) ;
#170675 = ORIENTED_EDGE ( 'NONE', *, *, #44023, .T. ) ;
#170676 = AXIS2_PLACEMENT_3D ( 'NONE', #68901, #108013, #148431 ) ;
#170678 = AXIS2_PLACEMENT_3D ( 'NONE', #201447, #85331, #181899 ) ;
#170677 = CARTESIAN_POINT ( 'NONE',  ( 20.94999999999999929, 68.16863917788211324, -213.8681745540812926 ) ) ;
#170679 = EDGE_LOOP ( 'NONE', ( #78989, #229168, #39614, #249652 ) ) ;
#170680 = DIRECTION ( 'NONE',  ( -0.000000000000000000, -6.982962677686266711E-15, 1.000000000000000000 ) ) ;
#170681 = VECTOR ( 'NONE', #226963, 1000.000000000000000 ) ;
#170682 = EDGE_CURVE ( 'NONE', #196712, #178378, #79527, .T. ) ;
#170683 = EDGE_CURVE ( 'NONE', #127414, #150586, #118203, .T. ) ;
#170684 = ORIENTED_EDGE ( 'NONE', *, *, #49941, .T. ) ;
#170685 = FACE_OUTER_BOUND ( 'NONE', #249439, .T. ) ;
#170686 = ORIENTED_EDGE ( 'NONE', *, *, #11241, .T. ) ;
#170687 = EDGE_CURVE ( 'NONE', #247975, #187820, #219476, .T. ) ;
#170689 = EDGE_CURVE ( 'NONE', #295, #56834, #114448, .T. ) ;
#170688 = CARTESIAN_POINT ( 'NONE',  ( -17.22361732159832215, 10.34515565860243314, -11.37078452586713517 ) ) ;
#170690 = CARTESIAN_POINT ( 'NONE',  ( -23.25000000000000000, -1.249999999988843369, -74.80048075441509070 ) ) ;
#170691 = DIRECTION ( 'NONE',  ( 1.000000000000000000, 0.000000000000000000, 0.000000000000000000 ) ) ;
#170692 = DIRECTION ( 'NONE',  ( 1.000000000000000000, 1.186688945009010077E-16, 0.000000000000000000 ) ) ;
#170693 = DIRECTION ( 'NONE',  ( -1.000000000000000000, 2.952720810173289112E-16, 2.061873921506763405E-30 ) ) ;
#170694 = CARTESIAN_POINT ( 'NONE',  ( 21.05000000000000071, 67.22371710471918504, -69.52310748452437394 ) ) ;
#170695 = ADVANCED_FACE ( 'NONE', ( #115636 ), #136454, .T. ) ;
#170696 = CARTESIAN_POINT ( 'NONE',  ( -23.25000000000000000, 76.00000000001188027, -99.12310748452429721 ) ) ;
#170697 = FACE_OUTER_BOUND ( 'NONE', #130393, .T. ) ;
#170699 = ORIENTED_EDGE ( 'NONE', *, *, #37856, .T. ) ;
#170698 = CARTESIAN_POINT ( 'NONE',  ( 18.33683296300427656, -0.6949276719145931480, -242.5042195544717742 ) ) ;
#170701 = DIRECTION ( 'NONE',  ( 1.000000000000000000, 0.000000000000000000, 0.000000000000000000 ) ) ;
#170700 = CARTESIAN_POINT ( 'NONE',  ( -21.05000000000000071, 1.115649653272650466E-11, -138.0000000000000284 ) ) ;
#170702 = ORIENTED_EDGE ( 'NONE', *, *, #38220, .F. ) ;
#170703 = ORIENTED_EDGE ( 'NONE', *, *, #120711, .F. ) ;
#170704 = AXIS2_PLACEMENT_3D ( 'NONE', #157208, #195042, #140161 ) ;
#170705 = ADVANCED_FACE ( 'NONE', ( #195202 ), #58204, .F. ) ;
#170706 = EDGE_LOOP ( 'NONE', ( #76986, #253907, #102164, #27959 ) ) ;
#170707 = DIRECTION ( 'NONE',  ( 0.000000000000000000, 2.168404344971247498E-15, 1.000000000000000000 ) ) ;
#170709 = EDGE_CURVE ( 'NONE', #26421, #255695, #158642, .T. ) ;
#170708 = ADVANCED_FACE ( 'NONE', ( #60778 ), #181102, .T. ) ;
#170710 = CARTESIAN_POINT ( 'NONE',  ( -23.15000000000000213, 1.115600667400684642E-11, -104.6500000000000341 ) ) ;
#170711 = CARTESIAN_POINT ( 'NONE',  ( 20.94999999999999929, 76.00000000001210765, -132.4231074845243370 ) ) ;
#170712 = CYLINDRICAL_SURFACE ( 'NONE', #64216, 0.09999999999999939493 ) ;
#170713 = AXIS2_PLACEMENT_3D ( 'NONE', #250657, #211553, #92869 ) ;
#170714 = DIRECTION ( 'NONE',  ( 0.000000000000000000, -0.9651348961777379554, 0.2617529984164210233 ) ) ;
#170715 = CYLINDRICAL_SURFACE ( 'NONE', #203672, 0.5000000000000004441 ) ;
#170716 = DIRECTION ( 'NONE',  ( -1.000000000000000000, 0.000000000000000000, -0.000000000000000000 ) ) ;
#170717 = ADVANCED_FACE ( 'NONE', ( #76494 ), #256360, .T. ) ;
#170718 = DIRECTION ( 'NONE',  ( -0.000000000000000000, 0.2617529984165031243, 0.9651348961777157509 ) ) ;
#170719 = ORIENTED_EDGE ( 'NONE', *, *, #46570, .F. ) ;
#170720 = VERTEX_POINT ( 'NONE', #79044 ) ;
#170721 = CARTESIAN_POINT ( 'NONE',  ( 17.74533788810829904, 65.18150020854172055, -180.3367301594719834 ) ) ;
#170722 = ADVANCED_FACE ( 'NONE', ( #37401 ), #197633, .T. ) ;
#170723 = EDGE_CURVE ( 'NONE', #75742, #56430, #189463, .T. ) ;
#170724 = VECTOR ( 'NONE', #27602, 1000.000000000000114 ) ;
#170725 = ORIENTED_EDGE ( 'NONE', *, *, #234699, .F. ) ;
#170726 = DIRECTION ( 'NONE',  ( 0.000000000000000000, 0.9934243067848629316, -0.1144908148674594617 ) ) ;
#170728 = VERTEX_POINT ( 'NONE', #96055 ) ;
#170727 = CIRCLE ( 'NONE', #133254, 7.791421356237310469 ) ;
#170729 = DIRECTION ( 'NONE',  ( 1.000000000000000000, 0.000000000000000000, 0.000000000000000000 ) ) ;
#170730 = EDGE_CURVE ( 'NONE', #235569, #213025, #131179, .T. ) ;
#170731 = CIRCLE ( 'NONE', #183163, 7.800000000000000711 ) ;
#170732 = DIRECTION ( 'NONE',  ( 1.000000000000000000, 0.000000000000000000, 0.000000000000000000 ) ) ;
#170733 = CARTESIAN_POINT ( 'NONE',  ( -23.25000000000000000, 36.65892442174472876, -249.5511627012454596 ) ) ;
#170734 = CARTESIAN_POINT ( 'NONE',  ( -22.39999999999999858, 0.1000000000111554016, -159.7092204016265384 ) ) ;
#170735 = DIRECTION ( 'NONE',  ( 0.000000000000000000, 0.000000000000000000, -1.000000000000000000 ) ) ;
#170736 = VERTEX_POINT ( 'NONE', #175625 ) ;
#170737 = EDGE_CURVE ( 'NONE', #249301, #227798, #177019, .T. ) ;
#170738 = AXIS2_PLACEMENT_3D ( 'NONE', #128865, #147119, #87141 ) ;
#170739 = AXIS2_PLACEMENT_3D ( 'NONE', #107117, #167133, #87540 ) ;
#170740 = CARTESIAN_POINT ( 'NONE',  ( -18.59999999999999787, 9.250000000011157297, -54.75000000000000000 ) ) ;
#170741 = DIRECTION ( 'NONE',  ( 0.000000000000000000, -0.2128009952263605897, 0.9770955615653315052 ) ) ;
#170742 = CARTESIAN_POINT ( 'NONE',  ( -22.39999999999999858, 75.90000000001242597, -177.8138870828977360 ) ) ;
#170743 = DIRECTION ( 'NONE',  ( 0.000000000000000000, 0.9126074666063769270, 0.4088369013363280513 ) ) ;
#170744 = SPHERICAL_SURFACE ( 'NONE', #247473, 0.1000000000000000056 ) ;
#170745 = ORIENTED_EDGE ( 'NONE', *, *, #145340, .F. ) ;
#170747 = DIRECTION ( 'NONE',  ( 0.000000000000000000, 4.440892098500631684E-15, -1.000000000000000000 ) ) ;
#170746 = CARTESIAN_POINT ( 'NONE',  ( -16.95709691156655907, 60.94199036320039653, -221.0320208310369026 ) ) ;
#170748 = ORIENTED_EDGE ( 'NONE', *, *, #172912, .T. ) ;
#170751 = EDGE_LOOP ( 'NONE', ( #255003, #31429, #236568, #222529 ) ) ;
#170750 = CARTESIAN_POINT ( 'NONE',  ( 20.95224633520496127, 67.09947783345508299, -161.5298310366031558 ) ) ;
#170749 = DIRECTION ( 'NONE',  ( 0.000000000000000000, -0.8814952561688476074, 0.4721928772777262417 ) ) ;
#170752 = DIRECTION ( 'NONE',  ( 7.304098846218134667E-16, -1.000000000000000000, 0.000000000000000000 ) ) ;
#170753 = AXIS2_PLACEMENT_3D ( 'NONE', #8363, #128311, #147876 ) ;
#170754 = TOROIDAL_SURFACE ( 'NONE', #253880, 4.099999999999999645, 0.1000000000000000056 ) ;
#170755 = AXIS2_PLACEMENT_3D ( 'NONE', #123516, #203039, #27011 ) ;
#170756 = DIRECTION ( 'NONE',  ( 0.000000000000000000, 0.000000000000000000, -1.000000000000000000 ) ) ;
#170757 = ORIENTED_EDGE ( 'NONE', *, *, #225088, .F. ) ;
#170758 = CYLINDRICAL_SURFACE ( 'NONE', #130455, 0.1000000000000024342 ) ;
#170759 = CIRCLE ( 'NONE', #87297, 0.09999999999998898659 ) ;
#170760 = CARTESIAN_POINT ( 'NONE',  ( -21.65000000000000213, 9.950000000011140600, -188.2499999999999716 ) ) ;
#170762 = FACE_OUTER_BOUND ( 'NONE', #217299, .T. ) ;
#170761 = DIRECTION ( 'NONE',  ( 0.000000000000000000, 0.000000000000000000, -1.000000000000000000 ) ) ;
#170764 = ORIENTED_EDGE ( 'NONE', *, *, #71559, .T. ) ;
#170763 = CARTESIAN_POINT ( 'NONE',  ( 18.49999999999999645, 0.6770221356676882074, -212.8807256103264649 ) ) ;
#170765 = ORIENTED_EDGE ( 'NONE', *, *, #203291, .T. ) ;
#170766 = CARTESIAN_POINT ( 'NONE',  ( -18.37013991200266005, 11.49974761622312691, -109.7069769894829250 ) ) ;
#170767 = DIRECTION ( 'NONE',  ( 1.000000000000000000, 0.000000000000000000, 0.000000000000000000 ) ) ;
#170768 = DIRECTION ( 'NONE',  ( 1.836970198721029934E-16, -0.9770955615653316162, -0.2128009952263604232 ) ) ;
#170769 = VERTEX_POINT ( 'NONE', #81601 ) ;
#170770 = DIRECTION ( 'NONE',  ( 0.000000000000000000, 0.9908441862701791170, -0.1350103645450472789 ) ) ;
#170771 = DIRECTION ( 'NONE',  ( 0.000000000000000000, 0.000000000000000000, -1.000000000000000000 ) ) ;
#170772 = CARTESIAN_POINT ( 'NONE',  ( 18.79999999999999716, -1.212568896937008089, -8.000000000000000000 ) ) ;
#170773 = ORIENTED_EDGE ( 'NONE', *, *, #117834, .T. ) ;
#170774 = CARTESIAN_POINT ( 'NONE',  ( -20.54999999999999716, 67.23127455305835554, -235.8551265064784559 ) ) ;
#170775 = VECTOR ( 'NONE', #95631, 1000.000000000000000 ) ;
#170776 = DIRECTION ( 'NONE',  ( -1.000000000000000000, 0.000000000000000000, 0.000000000000000000 ) ) ;
#170777 = EDGE_CURVE ( 'NONE', #130320, #84861, #64547, .T. ) ;
#170778 = AXIS2_PLACEMENT_3D ( 'NONE', #83462, #80909, #44381 ) ;
#170779 = ORIENTED_EDGE ( 'NONE', *, *, #31941, .F. ) ;
#170780 = DIRECTION ( 'NONE',  ( 0.000000000000000000, 0.2617529984165152257, 0.9651348961777124202 ) ) ;
#170782 = EDGE_CURVE ( 'NONE', #88024, #38614, #97841, .T. ) ;
#170781 = CARTESIAN_POINT ( 'NONE',  ( 20.85000000000000142, 68.97833521811233481, -166.1895420826271277 ) ) ;
#170783 = AXIS2_PLACEMENT_3D ( 'NONE', #207431, #224394, #147439 ) ;
#170784 = ORIENTED_EDGE ( 'NONE', *, *, #95841, .F. ) ;
#170785 = ORIENTED_EDGE ( 'NONE', *, *, #88689, .F. ) ;
#170786 = EDGE_CURVE ( 'NONE', #194778, #225349, #176921, .T. ) ;
#170787 = DIRECTION ( 'NONE',  ( 0.000000000000000000, 0.2617529984165031243, 0.9651348961777157509 ) ) ;
#170788 = ORIENTED_EDGE ( 'NONE', *, *, #12503, .F. ) ;
#170791 = EDGE_CURVE ( 'NONE', #206496, #61365, #85176, .T. ) ;
#170790 = ORIENTED_EDGE ( 'NONE', *, *, #84867, .F. ) ;
#170789 = CARTESIAN_POINT ( 'NONE',  ( -21.05000000000000071, 1.162701749949165642, -108.6000000000000227 ) ) ;
#170792 = ORIENTED_EDGE ( 'NONE', *, *, #45079, .F. ) ;
#170793 = AXIS2_PLACEMENT_3D ( 'NONE', #46452, #191142, #249810 ) ;
#170796 = VERTEX_POINT ( 'NONE', #226255 ) ;
#170795 = VERTEX_POINT ( 'NONE', #205421 ) ;
#170794 = CARTESIAN_POINT ( 'NONE',  ( -15.75000000000000355, 9.849999999999978328, -16.75000000000000355 ) ) ;
#170797 = CIRCLE ( 'NONE', #91637, 0.09999999999998898659 ) ;
#170798 = CARTESIAN_POINT ( 'NONE',  ( -23.15000000000000213, -8.999999999988844479, -90.60603087734760663 ) ) ;
#170799 = ORIENTED_EDGE ( 'NONE', *, *, #193644, .F. ) ;
#170800 = CARTESIAN_POINT ( 'NONE',  ( 20.95512820512820440, 22.03025613173517883, -231.6455594930189648 ) ) ;
#170801 = CARTESIAN_POINT ( 'NONE',  ( -20.85000000000000142, -11.74999999998884448, -97.60000000000005116 ) ) ;
#170802 = VECTOR ( 'NONE', #215389, 1000.000000000000000 ) ;
#170803 = CARTESIAN_POINT ( 'NONE',  ( 18.59999999999999787, 67.23127455305841238, -235.8551265064783991 ) ) ;
#170804 = EDGE_CURVE ( 'NONE', #134285, #46294, #135454, .T. ) ;
#170805 = DIRECTION ( 'NONE',  ( 1.000000000000000000, 0.000000000000000000, -0.000000000000000000 ) ) ;
#170806 = FACE_OUTER_BOUND ( 'NONE', #71862, .T. ) ;
#170808 = EDGE_CURVE ( 'NONE', #4559, #231216, #85544, .T. ) ;
#170807 = ORIENTED_EDGE ( 'NONE', *, *, #119706, .F. ) ;
#170809 = ORIENTED_EDGE ( 'NONE', *, *, #47159, .T. ) ;
#170810 = ORIENTED_EDGE ( 'NONE', *, *, #98760, .T. ) ;
#170811 = CARTESIAN_POINT ( 'NONE',  ( 21.13461538461538325, 8.885417037985616773, -146.3500000000000227 ) ) ;
#170813 = EDGE_LOOP ( 'NONE', ( #218428, #67719, #213417, #119133 ) ) ;
#170812 = CARTESIAN_POINT ( 'NONE',  ( -16.93415306273742260, 66.00437774000003799, -182.6130505421640180 ) ) ;
#170814 = CARTESIAN_POINT ( 'NONE',  ( -21.14999999999999858, 76.10000000001245724, -181.6726782920691505 ) ) ;
#170816 = VERTEX_POINT ( 'NONE', #222399 ) ;
#170815 = CARTESIAN_POINT ( 'NONE',  ( 18.44364597020195262, 78.23832191996586971, -231.5273892603947559 ) ) ;
#170817 = ORIENTED_EDGE ( 'NONE', *, *, #82261, .F. ) ;
#170818 = DIRECTION ( 'NONE',  ( 0.7071067811865475727, 0.6824534298470373850, -0.1850873201762210096 ) ) ;
#170819 = EDGE_CURVE ( 'NONE', #181057, #90904, #31883, .T. ) ;
#170820 = ORIENTED_EDGE ( 'NONE', *, *, #143512, .F. ) ;
#170821 = AXIS2_PLACEMENT_3D ( 'NONE', #242818, #121624, #241542 ) ;
#170822 = TOROIDAL_SURFACE ( 'NONE', #129079, 0.2000000000000000111, 0.1000000000000000056 ) ;
#170823 = CARTESIAN_POINT ( 'NONE',  ( -16.83233564386404169, 9.930221796595755990, -180.2754793365243415 ) ) ;
#170824 = DIRECTION ( 'NONE',  ( -1.000000000000000000, 0.000000000000000000, 0.000000000000000000 ) ) ;
#170825 = ADVANCED_FACE ( 'NONE', ( #42503 ), #206721, .F. ) ;
#170827 = VERTEX_POINT ( 'NONE', #122057 ) ;
#170826 = ORIENTED_EDGE ( 'NONE', *, *, #176870, .T. ) ;
#170828 = VERTEX_POINT ( 'NONE', #22984 ) ;
#170829 = LINE ( 'NONE', #54666, #161207 ) ;
#170830 = ORIENTED_EDGE ( 'NONE', *, *, #98558, .F. ) ;
#170831 = ORIENTED_EDGE ( 'NONE', *, *, #14656, .T. ) ;
#170832 = FACE_OUTER_BOUND ( 'NONE', #110855, .T. ) ;
#170834 = ORIENTED_EDGE ( 'NONE', *, *, #237275, .T. ) ;
#170833 = CARTESIAN_POINT ( 'NONE',  ( 21.05000000000000071, 48.98768910550767686, -253.5949463715719787 ) ) ;
#170835 = LINE ( 'NONE', #71700, #119166 ) ;
#170837 = CARTESIAN_POINT ( 'NONE',  ( 21.05000000000000071, -1.849084418615859926, -78.65601052144717187 ) ) ;
#170836 = FACE_OUTER_BOUND ( 'NONE', #37474, .T. ) ;
#170838 = ADVANCED_FACE ( 'NONE', ( #144159 ), #7222, .F. ) ;
#170839 = LINE ( 'NONE', #93802, #57456 ) ;
#170840 = CARTESIAN_POINT ( 'NONE',  ( -18.39418127959864790, 11.48390560170929220, -191.7499999999999716 ) ) ;
#170841 = ORIENTED_EDGE ( 'NONE', *, *, #191309, .T. ) ;
#170842 = ADVANCED_FACE ( 'NONE', ( #182031 ), #223698, .F. ) ;
#170843 = EDGE_LOOP ( 'NONE', ( #185516, #92319, #240214, #236001 ) ) ;
#170844 = CARTESIAN_POINT ( 'NONE',  ( 18.40916198585733454, 85.50000000001185185, -96.42291785270107596 ) ) ;
#170846 = AXIS2_PLACEMENT_3D ( 'NONE', #149161, #128305, #29237 ) ;
#170845 = DIRECTION ( 'NONE',  ( -1.000000000000000000, -0.000000000000000000, 0.000000000000000000 ) ) ;
#170847 = CYLINDRICAL_SURFACE ( 'NONE', #45427, 0.09999999999999939493 ) ;
#170848 = VECTOR ( 'NONE', #95741, 1000.000000000000000 ) ;
#170849 = CIRCLE ( 'NONE', #29182, 11.80000000000000426 ) ;
#170850 = VECTOR ( 'NONE', #200355, 1000.000000000000000 ) ;
#170852 = ADVANCED_FACE ( 'NONE', ( #86751 ), #244555, .F. ) ;
#170851 = ORIENTED_EDGE ( 'NONE', *, *, #75148, .F. ) ;
#170853 = CARTESIAN_POINT ( 'NONE',  ( 21.14999999999999858, 44.24607648097409651, -236.5241869975821487 ) ) ;
#170854 = VECTOR ( 'NONE', #248840, 1000.000000000000000 ) ;
#170855 = CARTESIAN_POINT ( 'NONE',  ( 18.59999999999999432, 47.92640890138473253, -246.4059919526569900 ) ) ;
#170856 = VERTEX_POINT ( 'NONE', #162479 ) ;
#170857 = ORIENTED_EDGE ( 'NONE', *, *, #249609, .T. ) ;
#170858 = DIRECTION ( 'NONE',  ( -3.440080580676165868E-14, 0.3848449534832963370, 0.9229812358755945523 ) ) ;
#170859 = CARTESIAN_POINT ( 'NONE',  ( -23.49999999999994316, 64.25000000001119815, -3.123107484524795474 ) ) ;
#170860 = EDGE_LOOP ( 'NONE', ( #255953, #230381 ) ) ;
#170861 = CARTESIAN_POINT ( 'NONE',  ( -18.46856557590792391, -9.474215907775342060, -174.6019862408821837 ) ) ;
#170863 = ORIENTED_EDGE ( 'NONE', *, *, #257141, .T. ) ;
#170862 =( REPRESENTATION_RELATIONSHIP ('NONE','NONE', #36900, #215063 ) REPRESENTATION_RELATIONSHIP_WITH_TRANSFORMATION ( #8945 )SHAPE_REPRESENTATION_RELATIONSHIP( ) );
#170864 = EDGE_CURVE ( 'NONE', #58850, #152824, #6277, .T. ) ;
#170865 = CARTESIAN_POINT ( 'NONE',  ( -21.05000000000000426, 6.270085863700293416, -100.4651319969869263 ) ) ;
#170866 = DIRECTION ( 'NONE',  ( 1.000000000000000000, 0.000000000000000000, 0.000000000000000000 ) ) ;
#170868 = CARTESIAN_POINT ( 'NONE',  ( 12.25000000000000000, 9.850000000011137402, -150.7500000000000284 ) ) ;
#170867 = CARTESIAN_POINT ( 'NONE',  ( -18.50000000000000000, 0.000000000000000000, 0.000000000000000000 ) ) ;
#170869 = LINE ( 'NONE', #147394, #48485 ) ;
#170870 = AXIS2_PLACEMENT_3D ( 'NONE', #91973, #52838, #171551 ) ;
#170871 = CARTESIAN_POINT ( 'NONE',  ( -22.50000000000000000, 12.67709964810648238, -223.3751320524553705 ) ) ;
#170872 = VECTOR ( 'NONE', #4644, 1000.000000000000000 ) ;
#170874 = ADVANCED_FACE ( 'NONE', ( #84146 ), #251991, .T. ) ;
#170873 = DIRECTION ( 'NONE',  ( 0.000000000000000000, -0.9126074666063768159, -0.4088369013363282178 ) ) ;
#170876 = EDGE_LOOP ( 'NONE', ( #184844, #11791, #251120, #241807 ) ) ;
#170875 = CARTESIAN_POINT ( 'NONE',  ( -23.25000000000000000, 76.00000000001244871, -167.9231074845243938 ) ) ;
#170878 = ORIENTED_EDGE ( 'NONE', *, *, #145478, .F. ) ;
#170877 = ORIENTED_EDGE ( 'NONE', *, *, #254228, .T. ) ;
#170879 = VERTEX_POINT ( 'NONE', #241994 ) ;
#170880 = CARTESIAN_POINT ( 'NONE',  ( -16.77902162784672768, 60.94595240997173136, -221.0310918376485745 ) ) ;
#170881 = CARTESIAN_POINT ( 'NONE',  ( -21.05000000000000071, 14.05000000000000071, -5.513695070760990191 ) ) ;
#170883 = CARTESIAN_POINT ( 'NONE',  ( -22.59999985501179154, 11.74986979301414358, -33.43440133020047256 ) ) ;
#170882 = DIRECTION ( 'NONE',  ( 0.000000000000000000, 0.8814952561688476074, -0.4721928772777262417 ) ) ;
#170884 = CARTESIAN_POINT ( 'NONE',  ( -23.15000000000000213, 87.65000000001174385, -81.27310748452423184 ) ) ;
#170885 = ORIENTED_EDGE ( 'NONE', *, *, #237420, .F. ) ;
#170886 = DIRECTION ( 'NONE',  ( -0.000000000000000000, 1.000000000000000000, 8.717686153663073805E-15 ) ) ;
#170887 = ORIENTED_EDGE ( 'NONE', *, *, #54012, .F. ) ;
#170888 = VERTEX_POINT ( 'NONE', #102449 ) ;
#170889 = CARTESIAN_POINT ( 'NONE',  ( 20.04142135623730070, 64.35000000001173248, -81.27310748452440237 ) ) ;
#170890 = DIRECTION ( 'NONE',  ( 0.000000000000000000, 0.000000000000000000, -1.000000000000000000 ) ) ;
#170891 = DIRECTION ( 'NONE',  ( -1.000000000000000000, 0.000000000000000000, 0.000000000000000000 ) ) ;
#170892 = ORIENTED_EDGE ( 'NONE', *, *, #22619, .F. ) ;
#170893 = AXIS2_PLACEMENT_3D ( 'NONE', #12555, #231590, #112918 ) ;
#170894 = DIRECTION ( 'NONE',  ( -0.000000000000000000, -0.000000000000000000, 1.000000000000000000 ) ) ;
#170895 = CARTESIAN_POINT ( 'NONE',  ( 22.50046968638161360, 0.04516984715162254693, -155.7499548455311924 ) ) ;
#170896 = VERTEX_POINT ( 'NONE', #145451 ) ;
#170897 = ORIENTED_EDGE ( 'NONE', *, *, #147777, .F. ) ;
#170898 = CARTESIAN_POINT ( 'NONE',  ( -16.89268316805465986, 9.951721813253337601, -54.35575247854554704 ) ) ;
#170899 = DIRECTION ( 'NONE',  ( -1.000000000000000000, -7.304098846218133681E-16, 4.217023435051677994E-16 ) ) ;
#170900 = AXIS2_PLACEMENT_3D ( 'NONE', #250372, #47011, #190421 ) ;
#170901 = DIRECTION ( 'NONE',  ( 0.000000000000000000, -0.9126074666063545004, -0.4088369013363783999 ) ) ;
#170902 = DIRECTION ( 'NONE',  ( 1.000000000000000000, 0.000000000000000000, 0.000000000000000000 ) ) ;
#170903 = DIRECTION ( 'NONE',  ( 0.000000000000000000, 0.000000000000000000, -1.000000000000000000 ) ) ;
#170904 = DIRECTION ( 'NONE',  ( 0.000000000000000000, 6.982962677686266711E-15, -1.000000000000000000 ) ) ;
#170905 = ORIENTED_EDGE ( 'NONE', *, *, #19987, .T. ) ;
#170906 = CARTESIAN_POINT ( 'NONE',  ( 18.79999999999999716, -10.84999999999999076, 32.89999999999999858 ) ) ;
#170907 = FACE_OUTER_BOUND ( 'NONE', #201187, .T. ) ;
#170909 = CARTESIAN_POINT ( 'NONE',  ( -20.85000000000000142, 7.021664781911246322, -204.8335654018972605 ) ) ;
#170908 = CARTESIAN_POINT ( 'NONE',  ( -21.55000000000000071, 7.150000000011155876, -188.7499999999999716 ) ) ;
#170910 = DIRECTION ( 'NONE',  ( 0.000000000000000000, -1.214306433183730130E-13, 1.000000000000000000 ) ) ;
#170911 = CARTESIAN_POINT ( 'NONE',  ( -18.41353343127311959, -9.500000000000005329, -7.032069396699669461 ) ) ;
#170912 = DIRECTION ( 'NONE',  ( 0.000000000000000000, 0.000000000000000000, 1.000000000000000000 ) ) ;
#170913 = DIRECTION ( 'NONE',  ( 0.000000000000000000, 1.000000000000000000, 6.982962677686266711E-15 ) ) ;
#170914 = AXIS2_PLACEMENT_3D ( 'NONE', #44264, #23439, #204597 ) ;
#170916 = ORIENTED_EDGE ( 'NONE', *, *, #108979, .F. ) ;
#170915 = LINE ( 'NONE', #112195, #3075 ) ;
#170917 = TOROIDAL_SURFACE ( 'NONE', #58389, 1.900000000000002576, 0.1000000000000000056 ) ;
#170918 = AXIS2_PLACEMENT_3D ( 'NONE', #229889, #31718, #10843 ) ;
#170919 = DIRECTION ( 'NONE',  ( 2.952720810173289112E-16, 1.000000000000000000, 6.938893903907222067E-15 ) ) ;
#170920 = EDGE_CURVE ( 'NONE', #72979, #206286, #214566, .T. ) ;
#170921 = VECTOR ( 'NONE', #126273, 1000.000000000000000 ) ;
#170922 = VECTOR ( 'NONE', #41728, 1000.000000000000000 ) ;
#170923 = CARTESIAN_POINT ( 'NONE',  ( 23.14999999999999147, 76.00000000001237765, -170.0231074845243597 ) ) ;
#170924 = EDGE_CURVE ( 'NONE', #178121, #177294, #168837, .T. ) ;
#170925 = ADVANCED_FACE ( 'NONE', ( #163754 ), #5928, .T. ) ;
#170926 = DIRECTION ( 'NONE',  ( -0.000000000000000000, -0.4721928772777346239, -0.8814952561688430555 ) ) ;
#170927 = CARTESIAN_POINT ( 'NONE',  ( 12.84435279558019261, 9.410708747058235346, -85.06920840584413668 ) ) ;
#170928 = CARTESIAN_POINT ( 'NONE',  ( -23.15000000000000213, 1.115625160336667635E-11, -69.00000000000000000 ) ) ;
#170929 = AXIS2_PLACEMENT_3D ( 'NONE', #198128, #221519, #201987 ) ;
#170930 = DIRECTION ( 'NONE',  ( 0.000000000000000000, 6.982962677686266711E-15, -1.000000000000000000 ) ) ;
#170931 = AXIS2_PLACEMENT_3D ( 'NONE', #91007, #186271, #29793 ) ;
#170932 = CARTESIAN_POINT ( 'NONE',  ( -21.05000000000000426, -0.02103547652895997738, -94.19554417805240121 ) ) ;
#170933 = LINE ( 'NONE', #135582, #182167 ) ;
#170934 = CIRCLE ( 'NONE', #187457, 0.09999999999999982514 ) ;
#170935 = VECTOR ( 'NONE', #118903, 1000.000000000000114 ) ;
#170936 = ORIENTED_EDGE ( 'NONE', *, *, #200952, .F. ) ;
#170937 = CARTESIAN_POINT ( 'NONE',  ( 20.94999999999999929, 76.00000000001213607, -136.5231074845243313 ) ) ;
#170938 = VERTEX_POINT ( 'NONE', #62082 ) ;
#170939 = CARTESIAN_POINT ( 'NONE',  ( -17.11825945287482753, 44.09459801588531036, -235.2076708599468020 ) ) ;
#170940 = EDGE_CURVE ( 'NONE', #80974, #225893, #139550, .T. ) ;
#170941 = DIRECTION ( 'NONE',  ( 1.000000000000000000, 0.000000000000000000, 0.000000000000000000 ) ) ;
#170942 = ORIENTED_EDGE ( 'NONE', *, *, #188638, .F. ) ;
#170943 = CARTESIAN_POINT ( 'NONE',  ( -18.40000000000000213, 11.47316190337362762, -113.0500000000000398 ) ) ;
#170944 = PRODUCT_CONTEXT ( 'NONE', #235521, 'mechanical' ) ;
#170945 = CARTESIAN_POINT ( 'NONE',  ( -20.94999999999999929, 65.70729864260985664, -64.06574559737245522 ) ) ;
#170946 = VECTOR ( 'NONE', #110783, 1000.000000000000000 ) ;
#170947 = DIRECTION ( 'NONE',  ( -2.605671645643297230E-15, 0.9910465087640865089, 0.1335171055202867274 ) ) ;
#170948 = CARTESIAN_POINT ( 'NONE',  ( 22.49436431346199683, 64.35004905235818740, -69.59001101424667013 ) ) ;
#170949 = EDGE_LOOP ( 'NONE', ( #42232, #138932, #57474, #34783 ) ) ;
#170950 = CARTESIAN_POINT ( 'NONE',  ( 21.00000000000000000, 66.25000000001179501, -81.77310748452437394 ) ) ;
#170951 = CARTESIAN_POINT ( 'NONE',  ( 18.57071067811864040, 10.17928932189250091, -188.8499999999999659 ) ) ;
#170952 = CARTESIAN_POINT ( 'NONE',  ( 20.95346350065193519, 8.887177249185651107, -176.0117319470353721 ) ) ;
#170953 = ADVANCED_FACE ( 'NONE', ( #191037 ), #51467, .T. ) ;
#170954 = ORIENTED_EDGE ( 'NONE', *, *, #10721, .F. ) ;
#170955 = EDGE_CURVE ( 'NONE', #23820, #123298, #150609, .T. ) ;
#170956 = ORIENTED_EDGE ( 'NONE', *, *, #9094, .F. ) ;
#170957 = CARTESIAN_POINT ( 'NONE',  ( 18.59999999999999432, 1.162701749949165642, -75.00000000000004263 ) ) ;
#170958 = AXIS2_PLACEMENT_3D ( 'NONE', #179069, #202452, #117773 ) ;
#170959 = CARTESIAN_POINT ( 'NONE',  ( -22.01447462590973103, 68.73619979878202457, -103.1221444845838846 ) ) ;
#170960 = CARTESIAN_POINT ( 'NONE',  ( 23.15000000000000213, 85.50000000001251976, -179.9170766071767389 ) ) ;
#170961 = CYLINDRICAL_SURFACE ( 'NONE', #107572, 0.09999999999998898659 ) ;
#170962 = AXIS2_PLACEMENT_3D ( 'NONE', #141865, #40237, #101409 ) ;
#170963 = EDGE_CURVE ( 'NONE', #4469, #78065, #181289, .T. ) ;
#170965 = CARTESIAN_POINT ( 'NONE',  ( -20.64999999999999858, 85.50000000001197975, -112.9170766071766820 ) ) ;
#170964 = DIRECTION ( 'NONE',  ( 0.000000000000000000, -0.008583690987135041833, 0.9999631594459055250 ) ) ;
#170966 = CARTESIAN_POINT ( 'NONE',  ( 23.15000000000000213, -11.48912529306489994, -197.8999999999999773 ) ) ;
#170967 = DIRECTION ( 'NONE',  ( 0.000000000000000000, 0.000000000000000000, 1.000000000000000000 ) ) ;
#170968 = ORIENTED_EDGE ( 'NONE', *, *, #177174, .F. ) ;
#170969 = CIRCLE ( 'NONE', #58455, 0.09999999999998898659 ) ;
#170971 = ORIENTED_EDGE ( 'NONE', *, *, #55953, .T. ) ;
#170970 = CARTESIAN_POINT ( 'NONE',  ( -16.87435696428308063, 12.41403408133939301, -211.2428803809670512 ) ) ;
#170972 = CARTESIAN_POINT ( 'NONE',  ( 21.11927991906888025, 69.55150688152096450, -170.0321911639983057 ) ) ;
#170973 = CARTESIAN_POINT ( 'NONE',  ( -23.25000000000000000, 73.40000000001259650, -190.2984855617622770 ) ) ;
#170975 = DIRECTION ( 'NONE',  ( 0.000000000000000000, 0.000000000000000000, -1.000000000000000000 ) ) ;
#170974 = CARTESIAN_POINT ( 'NONE',  ( 18.49999999999999645, 77.86671491006937629, -124.7704322382422788 ) ) ;
#170976 = VERTEX_POINT ( 'NONE', #211876 ) ;
#170977 = CARTESIAN_POINT ( 'NONE',  ( 20.94999999999999574, 87.75000000001264766, -200.4231074845242802 ) ) ;
#170978 = CARTESIAN_POINT ( 'NONE',  ( 20.00000000000000355, 64.25000000001196554, -111.8731074845243825 ) ) ;
#170979 = CARTESIAN_POINT ( 'NONE',  ( -21.05000000000000071, 69.52192177891696190, -102.9231075492185568 ) ) ;
#170980 = DIRECTION ( 'NONE',  ( -5.603264701231743991E-32, -7.172728831056617961E-15, 1.000000000000000000 ) ) ;
#170981 = ORIENTED_EDGE ( 'NONE', *, *, #85531, .T. ) ;
#170982 = ORIENTED_EDGE ( 'NONE', *, *, #109231, .F. ) ;
#170983 = ADVANCED_FACE ( 'NONE', ( #228858 ), #227563, .T. ) ;
#170984 = AXIS2_PLACEMENT_3D ( 'NONE', #66216, #205709, #127468 ) ;
#170985 = CARTESIAN_POINT ( 'NONE',  ( -16.80117486205003630, 9.949657268323468529, -54.34885487292548589 ) ) ;
#170986 = ORIENTED_EDGE ( 'NONE', *, *, #206612, .F. ) ;
#170987 = LINE ( 'NONE', #229631, #209614 ) ;
#170988 = AXIS2_PLACEMENT_3D ( 'NONE', #190, #103133, #182711 ) ;
#170989 = AXIS2_PLACEMENT_3D ( 'NONE', #165754, #65341, #144868 ) ;
#170990 = DIRECTION ( 'NONE',  ( 0.000000000000000000, 0.1568667991644863147, 0.9876197685951252359 ) ) ;
#170991 = CARTESIAN_POINT ( 'NONE',  ( -21.12757541349819590, 65.53186650915749567, -242.1014610283184254 ) ) ;
#170992 = VECTOR ( 'NONE', #248069, 1000.000000000000000 ) ;
#170993 = EDGE_CURVE ( 'NONE', #209272, #242248, #213136, .T. ) ;
#170994 = FACE_OUTER_BOUND ( 'NONE', #148570, .T. ) ;
#170995 = ORIENTED_EDGE ( 'NONE', *, *, #171593, .T. ) ;
#170996 = DIRECTION ( 'NONE',  ( 0.000000000000000000, -0.2617529984165035684, -0.9651348961777156399 ) ) ;
#170997 = EDGE_CURVE ( 'NONE', #142984, #2330, #222945, .T. ) ;
#170999 = ADVANCED_FACE ( 'NONE', ( #110179, #31963 ), #68502, .F. ) ;
#170998 = PLANE ( 'NONE',  #3875 ) ;
#171000 = CARTESIAN_POINT ( 'NONE',  ( -17.11825945287482753, 23.02528674727019364, -230.8469138855057281 ) ) ;
#171001 = CARTESIAN_POINT ( 'NONE',  ( 21.72449340488909897, 51.48232928251994167, -231.6416980232910987 ) ) ;
#171002 = CARTESIAN_POINT ( 'NONE',  ( -21.45000000000000284, 10.16011026985487398, -211.4267369781599939 ) ) ;
#171004 = AXIS2_PLACEMENT_3D ( 'NONE', #120785, #123333, #202853 ) ;
#171003 = DIRECTION ( 'NONE',  ( -3.265361837132813093E-16, -1.000000000000000000, -7.086529944415894657E-15 ) ) ;
#171005 = AXIS2_PLACEMENT_3D ( 'NONE', #13234, #51020, #247962 ) ;
#171006 = CARTESIAN_POINT ( 'NONE',  ( -16.84793658983438291, 66.05000000001224691, -149.2567541623344312 ) ) ;
#171007 = VERTEX_POINT ( 'NONE', #9802 ) ;
#171009 = CARTESIAN_POINT ( 'NONE',  ( -16.89020380669786547, 9.950000000011137047, -180.2574111481105206 ) ) ;
#171008 = DIRECTION ( 'NONE',  ( 1.000000000000000000, 1.541880601228652843E-16, 2.878400969107353907E-16 ) ) ;
#171010 = ORIENTED_EDGE ( 'NONE', *, *, #51067, .F. ) ;
#171012 = EDGE_LOOP ( 'NONE', ( #98308, #46345, #238573 ) ) ;
#171011 = CARTESIAN_POINT ( 'NONE',  ( -21.65000000000000213, 21.70314669089253812, -233.3151006027785286 ) ) ;
#171013 = EDGE_CURVE ( 'NONE', #63208, #216812, #152060, .T. ) ;
#171014 = ORIENTED_EDGE ( 'NONE', *, *, #41956, .T. ) ;
#171015 = DIRECTION ( 'NONE',  ( 1.000000000000000000, 0.000000000000000000, 0.000000000000000000 ) ) ;
#171016 = EDGE_CURVE ( 'NONE', #191153, #251642, #127094, .T. ) ;
#171017 = CARTESIAN_POINT ( 'NONE',  ( 20.73486653747088582, 7.250000000011182166, -109.7500000000000426 ) ) ;
#171018 = CARTESIAN_POINT ( 'NONE',  ( 18.49999999999999289, 65.79142135392861235, -78.32060061889450253 ) ) ;
#171019 = DIRECTION ( 'NONE',  ( 0.000000000000000000, 0.000000000000000000, -1.000000000000000000 ) ) ;
#171020 = ORIENTED_EDGE ( 'NONE', *, *, #19115, .T. ) ;
#171021 = CARTESIAN_POINT ( 'NONE',  ( 21.97500000000000497, 9.750000000011153745, -54.65000000000000568 ) ) ;
#171023 = EDGE_CURVE ( 'NONE', #82199, #161543, #172777, .T. ) ;
#171022 = CARTESIAN_POINT ( 'NONE',  ( 23.14999999999999858, 1.115600667400684642E-11, -167.5000000000000284 ) ) ;
#171024 = ORIENTED_EDGE ( 'NONE', *, *, #245706, .T. ) ;
#171025 = DIRECTION ( 'NONE',  ( 0.000000000000000000, 0.000000000000000000, -1.000000000000000000 ) ) ;
#171026 = VECTOR ( 'NONE', #116140, 1000.000000000000000 ) ;
#171027 = EDGE_CURVE ( 'NONE', #43473, #175390, #71083, .T. ) ;
#171028 = CIRCLE ( 'NONE', #141736, 0.1000000000000024342 ) ;
#171030 = CIRCLE ( 'NONE', #204272, 0.1000000000000028644 ) ;
#171029 = CARTESIAN_POINT ( 'NONE',  ( 21.15000000000004476, 74.83745509109094485, -44.02310748452479316 ) ) ;
#171031 = ORIENTED_EDGE ( 'NONE', *, *, #243562, .T. ) ;
#171032 = EDGE_CURVE ( 'NONE', #73797, #63552, #10590, .T. ) ;
#171033 = EDGE_CURVE ( 'NONE', #236989, #239741, #243804, .T. ) ;
#171034 = ORIENTED_EDGE ( 'NONE', *, *, #91931, .T. ) ;
#171035 = AXIS2_PLACEMENT_3D ( 'NONE', #240489, #197499, #97082 ) ;
#171036 = CARTESIAN_POINT ( 'NONE',  ( 18.58222699835054570, 65.66799936921529479, -97.42993998886008455 ) ) ;
#171037 = VERTEX_POINT ( 'NONE', #133595 ) ;
#171038 = CARTESIAN_POINT ( 'NONE',  ( 21.05000000000000071, 75.90220970870363715, -176.2809220950004772 ) ) ;
#171039 = EDGE_CURVE ( 'NONE', #248809, #224580, #114025, .T. ) ;
#171040 = DIRECTION ( 'NONE',  ( 0.000000000000000000, 0.2128009952263605620, -0.9770955615653315052 ) ) ;
#171041 = FACE_OUTER_BOUND ( 'NONE', #43604, .T. ) ;
#171042 = CYLINDRICAL_SURFACE ( 'NONE', #66115, 0.8750000000000007772 ) ;
#171043 = ADVANCED_FACE ( 'NONE', ( #193585 ), #202117, .F. ) ;
#171044 = CIRCLE ( 'NONE', #29374, 4.000000000000003553 ) ;
#171045 = EDGE_CURVE ( 'NONE', #151129, #2421, #108898, .T. ) ;
#171046 = EDGE_CURVE ( 'NONE', #230526, #135659, #131371, .T. ) ;
#171047 = CARTESIAN_POINT ( 'NONE',  ( 23.04999999999999716, 67.17743825834580207, -145.7731074845244450 ) ) ;
#171048 = DIRECTION ( 'NONE',  ( -4.701977403289178758E-30, 0.9126074666063700436, 0.4088369013363439830 ) ) ;
#171049 = EDGE_LOOP ( 'NONE', ( #92368, #186829, #179865, #59103, #73718, #91424, #67443, #188741 ) ) ;
#171050 = CARTESIAN_POINT ( 'NONE',  ( -21.04999999999999716, 8.794517532467699183, -245.5155488533044945 ) ) ;
#171051 = VERTEX_POINT ( 'NONE', #37098 ) ;
#171053 = DIRECTION ( 'NONE',  ( 0.000000000000000000, -1.000000000000000000, 0.000000000000000000 ) ) ;
#171052 = CARTESIAN_POINT ( 'NONE',  ( 21.05000000000000071, -11.74999999998883560, -198.0999999999999659 ) ) ;
#171054 = ORIENTED_EDGE ( 'NONE', *, *, #246787, .T. ) ;
#171055 = DIRECTION ( 'NONE',  ( 0.000000000000000000, 0.000000000000000000, -1.000000000000000000 ) ) ;
#171056 = DIRECTION ( 'NONE',  ( 1.000000000000000000, 0.000000000000000000, 0.000000000000000000 ) ) ;
#171057 = CARTESIAN_POINT ( 'NONE',  ( 21.00000000000000000, 66.25000000001151079, -48.37310748452438958 ) ) ;
#171058 = VERTEX_POINT ( 'NONE', #138694 ) ;
#171060 = EDGE_LOOP ( 'NONE', ( #112849, #70892, #23883, #177316, #124231 ) ) ;
#171059 = DIRECTION ( 'NONE',  ( 7.304098846218134667E-16, -1.000000000000000000, -6.982962677686267499E-15 ) ) ;
#171061 = EDGE_CURVE ( 'NONE', #198610, #80091, #239126, .T. ) ;
#171062 = TOROIDAL_SURFACE ( 'NONE', #100239, 0.4000000000000015210, 0.1000000000000000056 ) ;
#171064 = FACE_OUTER_BOUND ( 'NONE', #24658, .T. ) ;
#171063 = CARTESIAN_POINT ( 'NONE',  ( -20.64999999999999858, 1.115600667400684642E-11, -198.9999999999999432 ) ) ;
#171066 = ORIENTED_EDGE ( 'NONE', *, *, #48973, .F. ) ;
#171065 = CARTESIAN_POINT ( 'NONE',  ( 23.14999999999999503, 51.38014393322265505, -230.1906178717505327 ) ) ;
#171067 = AXIS2_PLACEMENT_3D ( 'NONE', #55387, #134931, #231513 ) ;
#171068 = ORIENTED_EDGE ( 'NONE', *, *, #241553, .F. ) ;
#171069 = CIRCLE ( 'NONE', #179231, 0.1000000000000028644 ) ;
#171070 = CARTESIAN_POINT ( 'NONE',  ( 23.14999999999998437, 1.115600667400684642E-11, -134.0000000000000000 ) ) ;
#171071 = ORIENTED_EDGE ( 'NONE', *, *, #252166, .T. ) ;
#171072 = DIRECTION ( 'NONE',  ( -1.000000000000000000, 0.000000000000000000, 0.000000000000000000 ) ) ;
#171073 = ORIENTED_EDGE ( 'NONE', *, *, #167696, .T. ) ;
#171074 = AXIS2_PLACEMENT_3D ( 'NONE', #231801, #234341, #141338 ) ;
#171075 = DIRECTION ( 'NONE',  ( 1.000000000000000000, -0.000000000000000000, -0.000000000000000000 ) ) ;
#171076 = ORIENTED_EDGE ( 'NONE', *, *, #252747, .F. ) ;
#171077 = CARTESIAN_POINT ( 'NONE',  ( 21.14999999999999858, 76.00000000001229239, -157.8731074845243540 ) ) ;
#171078 = ADVANCED_FACE ( 'NONE', ( #77451 ), #99578, .T. ) ;
#171079 = ORIENTED_EDGE ( 'NONE', *, *, #81238, .T. ) ;
#171080 = VECTOR ( 'NONE', #57056, 1000.000000000000000 ) ;
#171082 = EDGE_CURVE ( 'NONE', #128967, #185020, #197998, .T. ) ;
#171081 = CARTESIAN_POINT ( 'NONE',  ( -0.8999999999999993561, -9.650000000000003908, 28.60000000000000142 ) ) ;
#171083 = AXIS2_PLACEMENT_3D ( 'NONE', #56764, #257506, #35970 ) ;
#171085 = ORIENTED_EDGE ( 'NONE', *, *, #30834, .T. ) ;
#171084 = AXIS2_PLACEMENT_3D ( 'NONE', #220692, #119031, #101989 ) ;
#171086 = ORIENTED_EDGE ( 'NONE', *, *, #81038, .T. ) ;
#171087 = CARTESIAN_POINT ( 'NONE',  ( -18.40000000000000213, -9.499999999988849808, -73.92214984933045230 ) ) ;
#171088 = AXIS2_PLACEMENT_3D ( 'NONE', #132066, #101894, #19841 ) ;
#171089 = EDGE_LOOP ( 'NONE', ( #22757, #41492, #160632, #232559 ) ) ;
#171090 = FACE_OUTER_BOUND ( 'NONE', #233893, .T. ) ;
#171091 = ORIENTED_EDGE ( 'NONE', *, *, #18388, .F. ) ;
#171094 = EDGE_CURVE ( 'NONE', #14889, #127805, #235409, .T. ) ;
#171093 = VERTEX_POINT ( 'NONE', #55310 ) ;
#171092 = DIRECTION ( 'NONE',  ( 0.000000000000000000, -6.982962677686266711E-15, 1.000000000000000000 ) ) ;
#171095 = AXIS2_PLACEMENT_3D ( 'NONE', #124075, #224433, #165777 ) ;
#171096 = AXIS2_PLACEMENT_3D ( 'NONE', #62244, #42674, #21838 ) ;
#171097 = ORIENTED_EDGE ( 'NONE', *, *, #26286, .T. ) ;
#171098 = CARTESIAN_POINT ( 'NONE',  ( -20.64999999999999858, 2.400000000011155432, -53.77537807723790309 ) ) ;
#171099 = VERTEX_POINT ( 'NONE', #216972 ) ;
#171102 = VERTEX_POINT ( 'NONE', #119185 ) ;
#171101 = ORIENTED_EDGE ( 'NONE', *, *, #136357, .T. ) ;
#171100 = DIRECTION ( 'NONE',  ( 2.952720810173289112E-16, 1.000000000000000000, -6.088138035986627436E-46 ) ) ;
#171103 = EDGE_CURVE ( 'NONE', #65265, #241989, #156352, .T. ) ;
#171104 = CARTESIAN_POINT ( 'NONE',  ( 18.39999999999997371, 62.50563584222673796, -209.4474707446456421 ) ) ;
#171105 = ORIENTED_EDGE ( 'NONE', *, *, #125056, .F. ) ;
#171106 = AXIS2_PLACEMENT_3D ( 'NONE', #125025, #207129, #8921 ) ;
#171107 = AXIS2_PLACEMENT_3D ( 'NONE', #28972, #68044, #91469 ) ;
#171108 = AXIS2_PLACEMENT_3D ( 'NONE', #256425, #116989, #196515 ) ;
#171109 = CIRCLE ( 'NONE', #141827, 0.09999999999999939493 ) ;
#171110 = CARTESIAN_POINT ( 'NONE',  ( -23.15000000000000213, 20.01397631055648674, -237.6853859230195098 ) ) ;
#171111 = ORIENTED_EDGE ( 'NONE', *, *, #78632, .T. ) ;
#171112 = LINE ( 'NONE', #73280, #224537 ) ;
#171114 = ORIENTED_EDGE ( 'NONE', *, *, #121309, .T. ) ;
#171113 = LINE ( 'NONE', #17149, #215863 ) ;
#171115 = FACE_OUTER_BOUND ( 'NONE', #219113, .T. ) ;
#171116 = ORIENTED_EDGE ( 'NONE', *, *, #128, .T. ) ;
#171117 = CARTESIAN_POINT ( 'NONE',  ( 21.04999999999963478, 65.45624872451622878, -95.46671967585933771 ) ) ;
#171118 = LINE ( 'NONE', #51080, #235685 ) ;
#171119 = ORIENTED_EDGE ( 'NONE', *, *, #78223, .T. ) ;
#171120 = CARTESIAN_POINT ( 'NONE',  ( 18.45068634130097607, 85.48650607335434870, -62.45432905335616169 ) ) ;
#171121 = CIRCLE ( 'NONE', #87839, 0.09999999999998898659 ) ;
#171122 = CARTESIAN_POINT ( 'NONE',  ( 18.53317502108576420, 18.39833411442328170, -236.9692678682430085 ) ) ;
#171123 = EDGE_LOOP ( 'NONE', ( #25744, #234849, #110584, #172829 ) ) ;
#171125 = VERTEX_POINT ( 'NONE', #198709 ) ;
#171124 = FACE_OUTER_BOUND ( 'NONE', #249435, .T. ) ;
#171126 = CARTESIAN_POINT ( 'NONE',  ( 23.15000000000000213, -4.259020970815407203, -226.0869574510824123 ) ) ;
#171128 = ORIENTED_EDGE ( 'NONE', *, *, #68638, .F. ) ;
#171127 = ORIENTED_EDGE ( 'NONE', *, *, #47631, .F. ) ;
#171129 = ORIENTED_EDGE ( 'NONE', *, *, #182149, .F. ) ;
#171130 = DIRECTION ( 'NONE',  ( 0.000000000000000000, 0.1455152366551500653, 0.9893560106964507384 ) ) ;
#171131 = ORIENTED_EDGE ( 'NONE', *, *, #74505, .T. ) ;
#171132 = ORIENTED_EDGE ( 'NONE', *, *, #32872, .F. ) ;
#171133 = SPHERICAL_SURFACE ( 'NONE', #196676, 0.1000000000000000056 ) ;
#171134 = EDGE_LOOP ( 'NONE', ( #152783, #240094, #95555, #133817 ) ) ;
#171135 = CARTESIAN_POINT ( 'NONE',  ( -20.94999999999999929, 87.65000000001212754, -133.4231074845242233 ) ) ;
#171136 = DIRECTION ( 'NONE',  ( 0.000000000000000000, 0.8490545835447238510, 0.5283051335749973099 ) ) ;
#171137 = ADVANCED_FACE ( 'NONE', ( #137434 ), #253534, .T. ) ;
#171138 = CIRCLE ( 'NONE', #229366, 0.09999999999999949207 ) ;
#171139 = ORIENTED_EDGE ( 'NONE', *, *, #21973, .T. ) ;
#171140 = EDGE_CURVE ( 'NONE', #250359, #137736, #85362, .T. ) ;
#171141 = ORIENTED_EDGE ( 'NONE', *, *, #144780, .T. ) ;
#171142 = CARTESIAN_POINT ( 'NONE',  ( 23.24999999999999289, -4.149999999988843058, -67.00000000000004263 ) ) ;
#171143 = ORIENTED_EDGE ( 'NONE', *, *, #256017, .F. ) ;
#171144 = VECTOR ( 'NONE', #237768, 1000.000000000000000 ) ;
#171145 = EDGE_CURVE ( 'NONE', #204523, #148718, #248079, .T. ) ;
#171146 = AXIS2_PLACEMENT_3D ( 'NONE', #62122, #40018, #122096 ) ;
#171147 = DIRECTION ( 'NONE',  ( -0.7071067811865475727, 0.7071067811865475727, 4.937700262164531476E-15 ) ) ;
#171148 = ORIENTED_EDGE ( 'NONE', *, *, #227422, .T. ) ;
#171149 = SPHERICAL_SURFACE ( 'NONE', #229202, 0.1000000000000000056 ) ;
#171152 = ADVANCED_FACE ( 'NONE', ( #196144 ), #228359, .T. ) ;
#171151 = ORIENTED_EDGE ( 'NONE', *, *, #251186, .F. ) ;
#171150 = CARTESIAN_POINT ( 'NONE',  ( 18.49999999999998934, 54.48300931968434213, -228.8005724072070564 ) ) ;
#171153 = DIRECTION ( 'NONE',  ( 0.000000000000000000, -6.417474130781252121E-15, 1.000000000000000000 ) ) ;
#171154 = FACE_OUTER_BOUND ( 'NONE', #95155, .T. ) ;
#171155 = ADVANCED_FACE ( 'NONE', ( #61769 ), #104706, .T. ) ;
#171156 = DIRECTION ( 'NONE',  ( -1.000000000000000000, -0.000000000000000000, 0.000000000000000000 ) ) ;
#171157 = DIRECTION ( 'NONE',  ( 0.000000000000000000, 0.000000000000000000, -1.000000000000000000 ) ) ;
#171158 = DIRECTION ( 'NONE',  ( 0.000000000000000000, -0.000000000000000000, 1.000000000000000000 ) ) ;
#171159 = FACE_OUTER_BOUND ( 'NONE', #149895, .T. ) ;
#171160 = AXIS2_PLACEMENT_3D ( 'NONE', #151570, #191977, #177564 ) ;
#171161 = B_SPLINE_CURVE_WITH_KNOTS ( 'NONE', 3,
 ( #9148, #169547, #246467, #67827, #109511, #170840, #91256 ),
 .UNSPECIFIED., .F., .F.,
 ( 4, 3, 4 ),
 ( 0.000000000000000000, 3.882884552234471334E-05, 5.798605692158473166E-05 ),
 .UNSPECIFIED. ) ;
#171162 = CYLINDRICAL_SURFACE ( 'NONE', #99394, 11.75000000000001066 ) ;
#171163 = CARTESIAN_POINT ( 'NONE',  ( 21.93642651522410247, 33.66330848088261263, -242.8643360821705528 ) ) ;
#171164 = FACE_OUTER_BOUND ( 'NONE', #219165, .T. ) ;
#171165 = EDGE_CURVE ( 'NONE', #35302, #56619, #206394, .T. ) ;
#171166 = DIRECTION ( 'NONE',  ( 7.589415207398576792E-15, -1.000000000000000000, -0.000000000000000000 ) ) ;
#171167 = AXIS2_PLACEMENT_3D ( 'NONE', #79412, #238504, #220245 ) ;
#171168 = ORIENTED_EDGE ( 'NONE', *, *, #195879, .T. ) ;
#171169 = CIRCLE ( 'NONE', #125333, 0.1000000000000017958 ) ;
#171170 = VECTOR ( 'NONE', #168142, 1000.000000000000000 ) ;
#171172 = VERTEX_POINT ( 'NONE', #22671 ) ;
#171171 = ORIENTED_EDGE ( 'NONE', *, *, #30944, .F. ) ;
#171173 = ORIENTED_EDGE ( 'NONE', *, *, #191107, .T. ) ;
#171175 = EDGE_CURVE ( 'NONE', #105944, #48863, #218840, .T. ) ;
#171174 = DIRECTION ( 'NONE',  ( 0.000000000000000000, -1.000000000000000000, 0.000000000000000000 ) ) ;
#171176 = CARTESIAN_POINT ( 'NONE',  ( -20.64999999999999858, 71.65000000001222702, -148.8731074845244109 ) ) ;
#171178 = CARTESIAN_POINT ( 'NONE',  ( 18.59999999999999076, 79.19526988099229925, -196.1889237952725296 ) ) ;
#171177 = DIRECTION ( 'NONE',  ( -1.000000000000000000, -0.000000000000000000, -0.000000000000000000 ) ) ;
#171179 = ORIENTED_EDGE ( 'NONE', *, *, #187799, .F. ) ;
#171180 = VERTEX_POINT ( 'NONE', #124320 ) ;
#171181 =( NAMED_UNIT ( * ) PLANE_ANGLE_UNIT ( ) SI_UNIT ( $, .RADIAN. ) );
#171182 = CARTESIAN_POINT ( 'NONE',  ( -20.54999999999999716, 85.50000000001188027, -93.12913836187179584 ) ) ;
#171184 = AXIS2_PLACEMENT_3D ( 'NONE', #85671, #201801, #23199 ) ;
#171183 = DIRECTION ( 'NONE',  ( 1.000000000000000000, 0.000000000000000000, 0.000000000000000000 ) ) ;
#171185 = LINE ( 'NONE', #69486, #158052 ) ;
#171186 = VERTEX_POINT ( 'NONE', #160891 ) ;
#171187 = EDGE_LOOP ( 'NONE', ( #48857, #167066, #252732, #105616 ) ) ;
#171188 = CYLINDRICAL_SURFACE ( 'NONE', #108843, 0.09999999999999939493 ) ;
#171189 = CARTESIAN_POINT ( 'NONE',  ( 23.24999999999999289, 11.65000000001116298, -122.2500000000000284 ) ) ;
#171190 = CARTESIAN_POINT ( 'NONE',  ( -18.39999999999999858, 78.24390740893980478, -231.6169762517609172 ) ) ;
#171192 = ORIENTED_EDGE ( 'NONE', *, *, #132353, .T. ) ;
#171191 = CYLINDRICAL_SURFACE ( 'NONE', #147913, 0.9000000000000014655 ) ;
#171193 = FACE_OUTER_BOUND ( 'NONE', #93866, .T. ) ;
#171194 = DIRECTION ( 'NONE',  ( 0.000000000000000000, 1.000000000000000000, 0.000000000000000000 ) ) ;
#171195 = DIRECTION ( 'NONE',  ( -1.000000000000000000, 0.000000000000000000, 0.000000000000000000 ) ) ;
#171196 = CARTESIAN_POINT ( 'NONE',  ( 18.46082813847993975, 85.48074965091940669, -95.93873738180860755 ) ) ;
#171197 = VERTEX_POINT ( 'NONE', #143861 ) ;
#171198 = CARTESIAN_POINT ( 'NONE',  ( 15.31784899511110076, 66.60336962369413527, -85.11605009170608582 ) ) ;
#171199 = DIRECTION ( 'NONE',  ( 0.000000000000000000, 0.1495327102803078179, 0.9887567792719429427 ) ) ;
#171200 = AXIS2_PLACEMENT_3D ( 'NONE', #12554, #210733, #232890 ) ;
#171203 = FACE_OUTER_BOUND ( 'NONE', #111734, .T. ) ;
#171202 = VECTOR ( 'NONE', #87135, 1000.000000000000227 ) ;
#171201 = DIRECTION ( 'NONE',  ( -1.000000000000000000, -0.000000000000000000, -0.000000000000000000 ) ) ;
#171205 = DIRECTION ( 'NONE',  ( 1.000000000000000000, 0.000000000000000000, 0.000000000000000000 ) ) ;
#171204 = VECTOR ( 'NONE', #106118, 1000.000000000000114 ) ;
#171206 = DIRECTION ( 'NONE',  ( 1.000000000000000000, -0.000000000000000000, -0.000000000000000000 ) ) ;
#171207 = CIRCLE ( 'NONE', #112896, 0.1000000000000026007 ) ;
#171208 = CARTESIAN_POINT ( 'NONE',  ( -23.15000000000000213, 76.00000000001213607, -136.5231074845242745 ) ) ;
#171209 = CARTESIAN_POINT ( 'NONE',  ( -20.54999999999999716, 2.500000000011154633, -154.2753780772379173 ) ) ;
#171210 = CARTESIAN_POINT ( 'NONE',  ( -18.40000000000000213, 64.51332499825466016, -160.7731074845244450 ) ) ;
#171211 = LINE ( 'NONE', #194608, #76726 ) ;
#171212 = ORIENTED_EDGE ( 'NONE', *, *, #188343, .T. ) ;
#171213 = EDGE_CURVE ( 'NONE', #188383, #60897, #93958, .T. ) ;
#171214 = AXIS2_PLACEMENT_3D ( 'NONE', #231222, #70876, #90395 ) ;
#171215 = ORIENTED_EDGE ( 'NONE', *, *, #148288, .T. ) ;
#171216 = ORIENTED_EDGE ( 'NONE', *, *, #23237, .T. ) ;
#171217 = CARTESIAN_POINT ( 'NONE',  ( -21.98333005346336577, 1.115600667400684642E-11, -160.1259246709432773 ) ) ;
#171218 = CARTESIAN_POINT ( 'NONE',  ( -23.25000000000000000, -10.72348020702290583, -206.5081278352411402 ) ) ;
#171219 = ORIENTED_EDGE ( 'NONE', *, *, #139760, .F. ) ;
#171220 = EDGE_CURVE ( 'NONE', #200879, #154355, #123187, .T. ) ;
#171221 = CIRCLE ( 'NONE', #225311, 11.89999999999999325 ) ;
#171222 = ORIENTED_EDGE ( 'NONE', *, *, #26142, .F. ) ;
#171223 = EDGE_CURVE ( 'NONE', #33906, #146901, #98198, .T. ) ;
#171224 = FILL_AREA_STYLE_COLOUR ( '', #81677 ) ;
#171225 = EDGE_CURVE ( 'NONE', #88951, #103901, #220834, .T. ) ;
#171226 = EDGE_LOOP ( 'NONE', ( #113648, #153579, #215343, #210418 ) ) ;
#171227 = DIRECTION ( 'NONE',  ( 0.000000000000000000, 0.000000000000000000, -1.000000000000000000 ) ) ;
#171228 = ORIENTED_EDGE ( 'NONE', *, *, #123355, .T. ) ;
#171229 = CARTESIAN_POINT ( 'NONE',  ( 22.39999999999999503, 55.98745301258800566, -232.8057040749260977 ) ) ;
#171230 = CYLINDRICAL_SURFACE ( 'NONE', #53492, 0.09999999999998898659 ) ;
#171231 = CARTESIAN_POINT ( 'NONE',  ( -18.59999999999999787, -1.637172712959223952, -145.5821533654720383 ) ) ;
#171232 =( BOUNDED_CURVE ( )  B_SPLINE_CURVE ( 3, ( #198335, #120126, #234910, #219172 ),
 .UNSPECIFIED., .F., .F. ) 
 B_SPLINE_CURVE_WITH_KNOTS ( ( 4, 4 ),
 ( 2.589852378279005940, 2.850972632318389710 ),
 .UNSPECIFIED. ) 
 CURVE ( )  GEOMETRIC_REPRESENTATION_ITEM ( )  RATIONAL_B_SPLINE_CURVE ( ( 1.000000000000000000, 0.9943260843901262636, 0.9943260843901262636, 1.000000000000000000 ) ) 
 REPRESENTATION_ITEM ( '' )  );
#171233 = DIRECTION ( 'NONE',  ( -1.000000000000000000, -0.000000000000000000, 0.000000000000000000 ) ) ;
#171234 = LINE ( 'NONE', #90349, #120221 ) ;
#171236 = VERTEX_POINT ( 'NONE', #43500 ) ;
#171235 = CARTESIAN_POINT ( 'NONE',  ( -16.83233564386400616, 30.08637999345557290, -234.7652289483340269 ) ) ;
#171238 = CARTESIAN_POINT ( 'NONE',  ( 19.99999999738042789, 11.75000000001116263, -192.1871719496316473 ) ) ;
#171237 = LINE ( 'NONE', #116363, #246222 ) ;
#171239 = EDGE_CURVE ( 'NONE', #244782, #104618, #223129, .T. ) ;
#171241 = CARTESIAN_POINT ( 'NONE',  ( -16.87242674293849731, 9.949999999999983302, -20.85109024637234754 ) ) ;
#171240 = AXIS2_PLACEMENT_3D ( 'NONE', #105458, #224150, #242429 ) ;
#171242 = CARTESIAN_POINT ( 'NONE',  ( 18.59999999999999787, -11.65000000000000036, 30.00000000000000000 ) ) ;
#171243 = CARTESIAN_POINT ( 'NONE',  ( 23.24999999999999645, 76.00000000001244871, -170.0231074845243597 ) ) ;
#171245 = EDGE_CURVE ( 'NONE', #15348, #932, #162178, .T. ) ;
#171244 = DIRECTION ( 'NONE',  ( 0.000000000000000000, -6.352154140967427193E-15, 1.000000000000000000 ) ) ;
#171246 = ORIENTED_EDGE ( 'NONE', *, *, #82634, .F. ) ;
#171247 = AXIS2_PLACEMENT_3D ( 'NONE', #7006, #63114, #68277 ) ;
#171248 = CARTESIAN_POINT ( 'NONE',  ( -23.25000000000000000, 36.65892442174472876, -249.5511627012454596 ) ) ;
#171249 = PRODUCT_DEFINITION ( 'UNKNOWN', '', #157115, #32847 ) ;
#171250 = AXIS2_PLACEMENT_3D ( 'NONE', #38887, #97522, #239642 ) ;
#171251 = FACE_OUTER_BOUND ( 'NONE', #97297, .T. ) ;
#171252 = ORIENTED_EDGE ( 'NONE', *, *, #243405, .F. ) ;
#171253 = CARTESIAN_POINT ( 'NONE',  ( -18.59999999999999787, 66.85000000001221565, -148.2731074845243597 ) ) ;
#171254 = CIRCLE ( 'NONE', #21378, 0.1999999999999976519 ) ;
#171255 = EDGE_CURVE ( 'NONE', #231797, #240937, #47320, .T. ) ;
#171257 = FACE_OUTER_BOUND ( 'NONE', #15610, .T. ) ;
#171256 = TOROIDAL_SURFACE ( 'NONE', #179410, 0.2000000000000000111, 0.1000000000000000056 ) ;
#171258 = DIRECTION ( 'NONE',  ( -1.000000000000000000, -2.952720810173289112E-16, 0.000000000000000000 ) ) ;
#171259 = ADVANCED_FACE ( 'NONE', ( #244243 ), #46050, .F. ) ;
#171260 = ORIENTED_EDGE ( 'NONE', *, *, #43038, .F. ) ;
#171261 = EDGE_CURVE ( 'NONE', #244808, #79539, #64346, .T. ) ;
#171262 = ORIENTED_EDGE ( 'NONE', *, *, #69892, .F. ) ;
#171263 = DIRECTION ( 'NONE',  ( 1.000000000000000000, -0.000000000000000000, -0.000000000000000000 ) ) ;
#171264 = CARTESIAN_POINT ( 'NONE',  ( 20.95392731769792150, 10.49313854003750635, -207.4367068100602012 ) ) ;
#171265 = CARTESIAN_POINT ( 'NONE',  ( 20.88420186297724257, 65.66974365629718591, -164.4360145562605453 ) ) ;
#171266 = FACE_OUTER_BOUND ( 'NONE', #112174, .T. ) ;
#171268 = DIRECTION ( 'NONE',  ( 1.000000000000000000, 0.000000000000000000, 0.000000000000000000 ) ) ;
#171267 = CARTESIAN_POINT ( 'NONE',  ( -23.15000000000000213, 11.75000000001115552, -188.8499999999999659 ) ) ;
#171269 = AXIS2_PLACEMENT_3D ( 'NONE', #64489, #81443, #223534 ) ;
#171270 = DIRECTION ( 'NONE',  ( -1.000000000000000000, 0.000000000000000000, 0.000000000000000000 ) ) ;
#171271 = LINE ( 'NONE', #128247, #169035 ) ;
#171273 = CARTESIAN_POINT ( 'NONE',  ( 19.75857864376268935, 64.35000000001251408, -178.7731074845244450 ) ) ;
#171272 = AXIS2_PLACEMENT_3D ( 'NONE', #192463, #145315, #81464 ) ;
#171274 = ORIENTED_EDGE ( 'NONE', *, *, #80279, .F. ) ;
#171275 = DIRECTION ( 'NONE',  ( 0.000000000000000000, -1.000000000000000000, 0.000000000000000000 ) ) ;
#171277 = ORIENTED_EDGE ( 'NONE', *, *, #112733, .F. ) ;
#171276 = CARTESIAN_POINT ( 'NONE',  ( 18.39999999999999858, -9.600000000000003197, -40.10018939122204529 ) ) ;
#171278 = CARTESIAN_POINT ( 'NONE',  ( 22.47007471830798409, 68.27928934808592487, -170.0231074845244166 ) ) ;
#171279 = CARTESIAN_POINT ( 'NONE',  ( -20.94999999999999929, -11.48912529306489994, -197.8999999999999773 ) ) ;
#171281 = CARTESIAN_POINT ( 'NONE',  ( 20.85000000000000142, 6.846123162363745074, -70.73772626684986164 ) ) ;
#171280 = LINE ( 'NONE', #13447, #166918 ) ;
#171282 = AXIS2_PLACEMENT_3D ( 'NONE', #42934, #177343, #198146 ) ;
#171283 = DIRECTION ( 'NONE',  ( 0.000000000000000000, -1.000000000000000000, -6.982962677686265922E-15 ) ) ;
#171284 = DIRECTION ( 'NONE',  ( -0.000000000000000000, -0.000000000000000000, -1.000000000000000000 ) ) ;
#171286 = ORIENTED_EDGE ( 'NONE', *, *, #73263, .F. ) ;
#171285 = CARTESIAN_POINT ( 'NONE',  ( -23.15000000000000213, -8.999999999988844479, -191.7060308773475299 ) ) ;
#171287 = DIRECTION ( 'NONE',  ( -3.265361837132813093E-16, -1.000000000000000000, -7.086529944415894657E-15 ) ) ;
#171288 = CARTESIAN_POINT ( 'NONE',  ( -20.54999999999999716, 2.761092913073515120, -213.6778149113116854 ) ) ;
#171289 = CIRCLE ( 'NONE', #4610, 0.09999999999999992228 ) ;
#171290 = CARTESIAN_POINT ( 'NONE',  ( -18.50000000000000000, 77.16270174994990327, -94.92310748452430857 ) ) ;
#171291 = DIRECTION ( 'NONE',  ( 0.000000000000000000, -0.9915357197604982575, 0.1298341882519033486 ) ) ;
#171292 = ORIENTED_EDGE ( 'NONE', *, *, #58095, .F. ) ;
#171293 = DIRECTION ( 'NONE',  ( 0.000000000000000000, 0.000000000000000000, -1.000000000000000000 ) ) ;
#171294 = ORIENTED_EDGE ( 'NONE', *, *, #156101, .T. ) ;
#171295 = EDGE_CURVE ( 'NONE', #180641, #104754, #23256, .T. ) ;
#171296 = CARTESIAN_POINT ( 'NONE',  ( 22.49999999999996803, 75.89914163091405896, -215.2726746080137445 ) ) ;
#171297 = ORIENTED_EDGE ( 'NONE', *, *, #57593, .F. ) ;
#171299 = DIRECTION ( 'NONE',  ( 1.000000000000000000, 0.000000000000000000, 0.000000000000000000 ) ) ;
#171298 = CIRCLE ( 'NONE', #58782, 0.09999999999998898659 ) ;
#171300 =( GEOMETRIC_REPRESENTATION_CONTEXT ( 3 ) GLOBAL_UNCERTAINTY_ASSIGNED_CONTEXT ( ( #98825 ) ) GLOBAL_UNIT_ASSIGNED_CONTEXT ( ( #203409, #222950, #185123 ) ) REPRESENTATION_CONTEXT ( 'NONE', 'WORKASPACE' ) );
#171301 = AXIS2_PLACEMENT_3D ( 'NONE', #217349, #103814, #79122 ) ;
#171302 = ORIENTED_EDGE ( 'NONE', *, *, #3784, .F. ) ;
#171303 = VECTOR ( 'NONE', #185795, 1000.000000000000000 ) ;
#171304 = CARTESIAN_POINT ( 'NONE',  ( -18.40000000000000213, 5.650000000011139001, -146.6500000000000341 ) ) ;
#171305 = DIRECTION ( 'NONE',  ( 1.000000000000000000, 0.000000000000000000, 0.000000000000000000 ) ) ;
#171306 = EDGE_CURVE ( 'NONE', #188373, #207310, #256389, .T. ) ;
#171307 = FACE_OUTER_BOUND ( 'NONE', #34837, .T. ) ;
#171308 = ORIENTED_EDGE ( 'NONE', *, *, #75951, .T. ) ;
#171309 =( BOUNDED_CURVE ( )  B_SPLINE_CURVE ( 3, ( #37382, #99866, #179461, #765 ),
 .UNSPECIFIED., .F., .F. ) 
 B_SPLINE_CURVE_WITH_KNOTS ( ( 4, 4 ),
 ( 0.3000847527772370071, 0.5497968875596818128 ),
 .UNSPECIFIED. ) 
 CURVE ( )  GEOMETRIC_REPRESENTATION_ITEM ( )  RATIONAL_B_SPLINE_CURVE ( ( 1.000000000000000000, 0.9948104011409419911, 0.9948104011409419911, 1.000000000000000000 ) ) 
 REPRESENTATION_ITEM ( '' )  );
#171310 = EDGE_CURVE ( 'NONE', #208877, #141175, #202566, .T. ) ;
#171311 = CARTESIAN_POINT ( 'NONE',  ( -16.80070461187906972, 9.950000000000081002, -12.64696382916064366 ) ) ;
#171312 = CARTESIAN_POINT ( 'NONE',  ( 23.15000000000000213, -9.499999999988848032, -43.39396912265245021 ) ) ;
#171313 = DIRECTION ( 'NONE',  ( 0.000000000000000000, -6.982962677686266711E-15, 1.000000000000000000 ) ) ;
#171314 = ADVANCED_FACE ( 'NONE', ( #4347 ), #242964, .F. ) ;
#171315 = DIRECTION ( 'NONE',  ( 0.000000000000000000, 0.9126074666063660468, 0.4088369013363524762 ) ) ;
#171316 = FACE_OUTER_BOUND ( 'NONE', #132140, .T. ) ;
#171317 = ORIENTED_EDGE ( 'NONE', *, *, #54909, .T. ) ;
#171318 = CARTESIAN_POINT ( 'NONE',  ( -20.64999999999999858, 1.115600667400684642E-11, -33.50000000000000000 ) ) ;
#171319 = ORIENTED_EDGE ( 'NONE', *, *, #137839, .F. ) ;
#171321 = ORIENTED_EDGE ( 'NONE', *, *, #200063, .T. ) ;
#171320 = CARTESIAN_POINT ( 'NONE',  ( 20.94999999999999574, 5.900000000011102586, -43.71909976465641989 ) ) ;
#171322 = EDGE_CURVE ( 'NONE', #134956, #136601, #210667, .T. ) ;
#171323 = VERTEX_POINT ( 'NONE', #112471 ) ;
#171324 = CARTESIAN_POINT ( 'NONE',  ( 18.41356215285961895, 85.50000000001266187, -196.4910380878247054 ) ) ;
#171325 = EDGE_CURVE ( 'NONE', #49350, #30904, #102292, .T. ) ;
#171326 = ORIENTED_EDGE ( 'NONE', *, *, #234304, .T. ) ;
#171327 = CARTESIAN_POINT ( 'NONE',  ( -20.00857864376270001, 66.65000000001198543, -115.3731074845243683 ) ) ;
#171328 = CARTESIAN_POINT ( 'NONE',  ( 21.07016717457011623, 1.115542603292150199E-11, -27.17905916189909377 ) ) ;
#171329 = DIRECTION ( 'NONE',  ( -1.000000000000000000, -0.000000000000000000, -0.000000000000000000 ) ) ;
#171330 = VERTEX_POINT ( 'NONE', #111178 ) ;
#171331 = CARTESIAN_POINT ( 'NONE',  ( -23.49999999999994316, 74.26359666348515987, -47.54092689884382850 ) ) ;
#171332 = CARTESIAN_POINT ( 'NONE',  ( -18.50000000000000000, 66.85000000001228670, -157.6731074845244223 ) ) ;
#171333 = ORIENTED_EDGE ( 'NONE', *, *, #248831, .T. ) ;
#171335 = ORIENTED_EDGE ( 'NONE', *, *, #138898, .T. ) ;
#171334 = DIRECTION ( 'NONE',  ( 0.000000000000000000, -0.8660254037844384856, 0.5000000000000003331 ) ) ;
#171336 = DIRECTION ( 'NONE',  ( 0.000000000000000000, 0.000000000000000000, 1.000000000000000000 ) ) ;
#171337 = CARTESIAN_POINT ( 'NONE',  ( 21.14999999999999858, 9.083217576421224848, -211.4565844547649931 ) ) ;
#171338 = EDGE_CURVE ( 'NONE', #250601, #195729, #243979, .T. ) ;
#171339 = ADVANCED_FACE ( 'NONE', ( #147737 ), #249411, .F. ) ;
#171340 = ORIENTED_EDGE ( 'NONE', *, *, #210155, .T. ) ;
#171341 =( BOUNDED_CURVE ( )  B_SPLINE_CURVE ( 3, ( #84396, #184827, #62329, #223949 ),
 .UNSPECIFIED., .F., .F. ) 
 B_SPLINE_CURVE_WITH_KNOTS ( ( 4, 4 ),
 ( 4.712388980384691450, 6.231880751915386263 ),
 .UNSPECIFIED. ) 
 CURVE ( )  GEOMETRIC_REPRESENTATION_ITEM ( )  RATIONAL_B_SPLINE_CURVE ( ( 1.000000000000000000, 0.8166740347213231610, 0.8166740347213231610, 1.000000000000000000 ) ) 
 REPRESENTATION_ITEM ( '' )  );
#171342 = DIRECTION ( 'NONE',  ( -1.000000000000000000, 0.000000000000000000, 0.000000000000000000 ) ) ;
#171343 = AXIS2_PLACEMENT_3D ( 'NONE', #57932, #220866, #119223 ) ;
#171344 = CARTESIAN_POINT ( 'NONE',  ( -20.54999999999999716, 68.76258920191057200, -222.5680764032308048 ) ) ;
#171345 = ORIENTED_EDGE ( 'NONE', *, *, #116598, .T. ) ;
#171346 = CARTESIAN_POINT ( 'NONE',  ( -20.94999999999999929, 1.835341550224413698, -11.55515129256298046 ) ) ;
#171347 = ADVANCED_FACE ( 'NONE', ( #228565 ), #207723, .T. ) ;
#171348 = DIRECTION ( 'NONE',  ( 0.000000000000000000, 0.000000000000000000, -1.000000000000000000 ) ) ;
#171349 = FACE_OUTER_BOUND ( 'NONE', #203241, .T. ) ;
#171350 = EDGE_CURVE ( 'NONE', #38707, #208826, #52460, .T. ) ;
#171351 = ADVANCED_FACE ( 'NONE', ( #231146 ), #250670, .F. ) ;
#171353 = ORIENTED_EDGE ( 'NONE', *, *, #31730, .T. ) ;
#171352 = VECTOR ( 'NONE', #136926, 1000.000000000000000 ) ;
#171354 = DIRECTION ( 'NONE',  ( -1.000000000000000000, -0.000000000000000000, -0.000000000000000000 ) ) ;
#171355 = ORIENTED_EDGE ( 'NONE', *, *, #245388, .T. ) ;
#171356 = DIRECTION ( 'NONE',  ( 1.000000000000000000, -7.136802563874195162E-16, -1.554319503706929005E-16 ) ) ;
#171357 = CYLINDRICAL_SURFACE ( 'NONE', #204070, 0.09999999999999939493 ) ;
#171359 = ORIENTED_EDGE ( 'NONE', *, *, #144500, .F. ) ;
#171358 = CARTESIAN_POINT ( 'NONE',  ( -20.90000000000000213, 11.50977166988710820, 1.786320531569725478 ) ) ;
#171361 = EDGE_CURVE ( 'NONE', #14308, #181057, #70791, .T. ) ;
#171360 = DIRECTION ( 'NONE',  ( 0.000000000000000000, -6.938893903907222067E-15, 1.000000000000000000 ) ) ;
#171362 = CARTESIAN_POINT ( 'NONE',  ( 21.14999999999999858, 65.28660755661168480, -57.27310748452439526 ) ) ;
#171363 = DIRECTION ( 'NONE',  ( 1.000000000000000000, -3.151514657663852580E-16, 8.547182517843351137E-17 ) ) ;
#171364 = CARTESIAN_POINT ( 'NONE',  ( -16.88560720703333473, 22.97666984193590167, -230.9336739665168921 ) ) ;
#171365 = DIRECTION ( 'NONE',  ( 0.000000000000000000, 0.2617529984165152257, 0.9651348961777124202 ) ) ;
#171366 = EDGE_CURVE ( 'NONE', #233386, #255134, #131562, .T. ) ;
#171367 = CARTESIAN_POINT ( 'NONE',  ( -17.01764560440328466, 9.950000000011138823, -79.74999999921324445 ) ) ;
#171368 = LINE ( 'NONE', #189609, #53188 ) ;
#171370 = ORIENTED_EDGE ( 'NONE', *, *, #168544, .F. ) ;
#171369 = CARTESIAN_POINT ( 'NONE',  ( 23.15000000000000213, 85.00000000001222134, -146.4170766071767389 ) ) ;
#171371 = AXIS2_PLACEMENT_3D ( 'NONE', #22557, #96902, #159501 ) ;
#171372 = CARTESIAN_POINT ( 'NONE',  ( -23.25000000000000000, 76.00000000001170974, -69.52310748452431710 ) ) ;
#171373 = DIRECTION ( 'NONE',  ( 0.000000000000000000, 0.01562500000001262185, 0.9998779222360095753 ) ) ;
#171374 = DIRECTION ( 'NONE',  ( -1.000000000000000000, 0.000000000000000000, 0.000000000000000000 ) ) ;
#171375 = DIRECTION ( 'NONE',  ( 1.000000000000000000, 0.000000000000000000, 0.000000000000000000 ) ) ;
#171376 = VERTEX_POINT ( 'NONE', #149035 ) ;
#171377 = VECTOR ( 'NONE', #7140, 1000.000000000000000 ) ;
#171378 = CIRCLE ( 'NONE', #87916, 0.09999999999998997191 ) ;
#171379 = FACE_OUTER_BOUND ( 'NONE', #205566, .T. ) ;
#171380 = FACE_OUTER_BOUND ( 'NONE', #124557, .T. ) ;
#171381 = VECTOR ( 'NONE', #157451, 1000.000000000000000 ) ;
#171382 = ORIENTED_EDGE ( 'NONE', *, *, #77192, .T. ) ;
#171384 = EDGE_CURVE ( 'NONE', #135417, #51212, #227258, .T. ) ;
#171383 = DIRECTION ( 'NONE',  ( 0.000000000000000000, -0.8660254037844387076, 0.4999999999999998335 ) ) ;
#171385 = ORIENTED_EDGE ( 'NONE', *, *, #17947, .F. ) ;
#171386 = DIRECTION ( 'NONE',  ( 1.000000000000000000, 0.000000000000000000, 0.000000000000000000 ) ) ;
#171387 = ORIENTED_EDGE ( 'NONE', *, *, #68303, .T. ) ;
#171388 = CARTESIAN_POINT ( 'NONE',  ( 18.50000000000000000, -9.499999999988842703, -155.7499999999999716 ) ) ;
#171390 = EDGE_LOOP ( 'NONE', ( #131091, #87061, #133809, #248485 ) ) ;
#171389 = CARTESIAN_POINT ( 'NONE',  ( 22.00411653889219465, 75.90096189422516204, -143.7765503521648043 ) ) ;
#171391 = CIRCLE ( 'NONE', #58896, 0.09999999999999609201 ) ;
#171392 = DIRECTION ( 'NONE',  ( 0.000000000000000000, 0.000000000000000000, 1.000000000000000000 ) ) ;
#171393 = ORIENTED_EDGE ( 'NONE', *, *, #228726, .F. ) ;
#171394 = CARTESIAN_POINT ( 'NONE',  ( -23.15000000000000213, 2.500000000011154633, -187.7753780772378889 ) ) ;
#171395 = ORIENTED_EDGE ( 'NONE', *, *, #64383, .F. ) ;
#171397 = ORIENTED_EDGE ( 'NONE', *, *, #122583, .T. ) ;
#171396 = ORIENTED_EDGE ( 'NONE', *, *, #61683, .T. ) ;
#171398 = CARTESIAN_POINT ( 'NONE',  ( -20.54999999999999716, 22.34215363070824623, -231.2750834139128528 ) ) ;
#171400 = VERTEX_POINT ( 'NONE', #232429 ) ;
#171399 = LINE ( 'NONE', #210491, #22344 ) ;
#171401 = EDGE_CURVE ( 'NONE', #196796, #145911, #235596, .T. ) ;
#171402 = DIRECTION ( 'NONE',  ( 1.000000000000000000, 0.000000000000000000, 0.000000000000000000 ) ) ;
#171403 = ORIENTED_EDGE ( 'NONE', *, *, #88663, .F. ) ;
#171404 = ORIENTED_EDGE ( 'NONE', *, *, #153100, .F. ) ;
#171405 = DIRECTION ( 'NONE',  ( 0.000000000000000000, 0.000000000000000000, 1.000000000000000000 ) ) ;
#171407 = LINE ( 'NONE', #215615, #109739 ) ;
#171406 = AXIS2_PLACEMENT_3D ( 'NONE', #72821, #171934, #48085 ) ;
#171408 = CARTESIAN_POINT ( 'NONE',  ( 20.46382478191414833, 10.59862044129738123, -7.677814469345459969 ) ) ;
#171409 = ORIENTED_EDGE ( 'NONE', *, *, #229851, .T. ) ;
#171410 = CARTESIAN_POINT ( 'NONE',  ( -20.64999999999999858, 1.115600667400684642E-11, -146.9749999999999943 ) ) ;
#171411 = CARTESIAN_POINT ( 'NONE',  ( 23.40000000000005542, 87.51781941433023349, -37.75951082105083145 ) ) ;
#171412 = CARTESIAN_POINT ( 'NONE',  ( -23.25000000000000000, 79.38304387823772856, -235.9388060597213723 ) ) ;
#171413 = AXIS2_PLACEMENT_3D ( 'NONE', #189130, #87446, #10506 ) ;
#171414 = VERTEX_POINT ( 'NONE', #251963 ) ;
#171415 = FACE_OUTER_BOUND ( 'NONE', #232263, .T. ) ;
#171416 = DIRECTION ( 'NONE',  ( -1.000000000000000000, -0.000000000000000000, 0.000000000000000000 ) ) ;
#171417 = DIRECTION ( 'NONE',  ( -0.000000000000000000, -0.2128009952263603677, 0.9770955615653313941 ) ) ;
#171418 = CARTESIAN_POINT ( 'NONE',  ( 21.05000000000000071, 11.65000000001116298, -67.00000000000004263 ) ) ;
#171419 = CIRCLE ( 'NONE', #4753, 0.09999999999999080458 ) ;
#171420 = VERTEX_POINT ( 'NONE', #29114 ) ;
#171421 = CARTESIAN_POINT ( 'NONE',  ( 22.40000000000010516, 1.020245298088821341E-11, -55.24956710754111811 ) ) ;
#171422 = ORIENTED_EDGE ( 'NONE', *, *, #230496, .F. ) ;
#171423 = CARTESIAN_POINT ( 'NONE',  ( -18.60000000000000142, -7.567701079425733113, -210.0537230116848377 ) ) ;
#171424 = VERTEX_POINT ( 'NONE', #73363 ) ;
#171425 = CARTESIAN_POINT ( 'NONE',  ( 23.24999999999999289, 6.649999999999999467, -21.15000000000000213 ) ) ;
#171426 = LINE ( 'NONE', #21007, #43928 ) ;
#171427 = ORIENTED_EDGE ( 'NONE', *, *, #36968, .T. ) ;
#171428 = AXIS2_PLACEMENT_3D ( 'NONE', #50598, #231846, #28540 ) ;
#171429 = VERTEX_POINT ( 'NONE', #126887 ) ;
#171430 = CARTESIAN_POINT ( 'NONE',  ( -18.59999999999999787, -1.835859311432481045, -179.0044391687985410 ) ) ;
#171431 = DIRECTION ( 'NONE',  ( 0.000000000000000000, -6.530723674265620862E-15, 1.000000000000000000 ) ) ;
#171432 = ORIENTED_EDGE ( 'NONE', *, *, #17272, .T. ) ;
#171433 = EDGE_LOOP ( 'NONE', ( #129696, #35925, #83137 ) ) ;
#171434 = DIRECTION ( 'NONE',  ( -1.284434275755705296E-16, 0.7071067811865471286, 0.7071067811865479058 ) ) ;
#171435 = AXIS2_PLACEMENT_3D ( 'NONE', #257332, #174052, #95734 ) ;
#171436 = PLANE ( 'NONE',  #64751 ) ;
#171437 = ORIENTED_EDGE ( 'NONE', *, *, #68258, .T. ) ;
#171438 = EDGE_CURVE ( 'NONE', #61324, #149131, #2359, .T. ) ;
#171439 = VECTOR ( 'NONE', #238320, 1000.000000000000000 ) ;
#171440 = AXIS2_PLACEMENT_3D ( 'NONE', #109411, #188966, #32501 ) ;
#171441 = ORIENTED_EDGE ( 'NONE', *, *, #157634, .T. ) ;
#171442 = DIRECTION ( 'NONE',  ( 0.000000000000000000, -0.1350103645451945777, 0.9908441862701590219 ) ) ;
#171443 = CIRCLE ( 'NONE', #92290, 0.09999999999999646672 ) ;
#171444 = EDGE_CURVE ( 'NONE', #55352, #51091, #248107, .T. ) ;
#171445 = CARTESIAN_POINT ( 'NONE',  ( -21.55000000000000071, 68.65000000001261071, -191.2731074845244166 ) ) ;
#171446 = AXIS2_PLACEMENT_3D ( 'NONE', #148891, #129316, #228434 ) ;
#171447 = EDGE_CURVE ( 'NONE', #63327, #214842, #127282, .T. ) ;
#171448 = DIRECTION ( 'NONE',  ( 0.000000000000000000, 0.000000000000000000, 1.000000000000000000 ) ) ;
#171450 = ORIENTED_EDGE ( 'NONE', *, *, #108014, .F. ) ;
#171449 = DIRECTION ( 'NONE',  ( 0.000000000000000000, -0.07893460099012301889, 0.9968797965484754720 ) ) ;
#171451 = DIRECTION ( 'NONE',  ( 0.000000000000000000, 0.000000000000000000, 1.000000000000000000 ) ) ;
#171452 = LINE ( 'NONE', #231399, #173472 ) ;
#171454 = CARTESIAN_POINT ( 'NONE',  ( -18.41431012584568094, 58.55944756805622120, -223.9431743560560335 ) ) ;
#171453 = CARTESIAN_POINT ( 'NONE',  ( -16.94445028196807002, 9.992063609708893068, -154.8926698215815634 ) ) ;
#171455 = CYLINDRICAL_SURFACE ( 'NONE', #232202, 0.09999999999998898659 ) ;
#171456 = DIRECTION ( 'NONE',  ( -0.000000000000000000, 0.2605042016806385363, 0.9654727137038795481 ) ) ;
#171457 = ADVANCED_FACE ( 'NONE', ( #246819 ), #49907, .F. ) ;
#171458 = CARTESIAN_POINT ( 'NONE',  ( 20.02499999999999858, 66.25000000001253397, -182.2731074845244450 ) ) ;
#171459 = AXIS2_PLACEMENT_3D ( 'NONE', #5703, #123121, #183100 ) ;
#171460 = FACE_OUTER_BOUND ( 'NONE', #134021, .T. ) ;
#171461 = CIRCLE ( 'NONE', #58966, 0.09999999999999632794 ) ;
#171463 = ORIENTED_EDGE ( 'NONE', *, *, #124960, .F. ) ;
#171462 = CIRCLE ( 'NONE', #150582, 0.09999999999999939493 ) ;
#171464 = AXIS2_PLACEMENT_3D ( 'NONE', #164429, #243948, #35217 ) ;
#171465 = ORIENTED_EDGE ( 'NONE', *, *, #64638, .T. ) ;
#171466 = EDGE_CURVE ( 'NONE', #245034, #92834, #69501, .T. ) ;
#171467 = FACE_OUTER_BOUND ( 'NONE', #5559, .T. ) ;
#171468 = CARTESIAN_POINT ( 'NONE',  ( -18.39999999999999858, 8.780520186313291120, -245.4165333277510115 ) ) ;
#171469 = ORIENTED_EDGE ( 'NONE', *, *, #222009, .F. ) ;
#171470 =( NAMED_UNIT ( * ) SI_UNIT ( $, .STERADIAN. ) SOLID_ANGLE_UNIT ( ) );
#171471 = FACE_OUTER_BOUND ( 'NONE', #154320, .T. ) ;
#171472 = DIRECTION ( 'NONE',  ( -1.000000000000000000, 7.304098846218163263E-16, -4.217023435051627211E-16 ) ) ;
#171473 = CARTESIAN_POINT ( 'NONE',  ( 23.24999999999999289, 69.35000000001180354, -81.87310748452435405 ) ) ;
#171475 = VERTEX_POINT ( 'NONE', #18499 ) ;
#171474 = AXIS2_PLACEMENT_3D ( 'NONE', #226951, #45742, #47005 ) ;
#171476 = EDGE_LOOP ( 'NONE', ( #174918, #172373, #204933, #131836 ) ) ;
#171477 = DIRECTION ( 'NONE',  ( 1.000000000000000000, -0.000000000000000000, -0.000000000000000000 ) ) ;
#171478 = CARTESIAN_POINT ( 'NONE',  ( 18.59999999999999787, 79.37986612816742138, -196.2658927859692142 ) ) ;
#171479 = VERTEX_POINT ( 'NONE', #233703 ) ;
#171480 = CARTESIAN_POINT ( 'NONE',  ( 22.47071067811865319, 0.09909245471376171288, -92.77992525550199332 ) ) ;
#171481 = VERTEX_POINT ( 'NONE', #77174 ) ;
#171482 = LINE ( 'NONE', #238815, #220325 ) ;
#171483 = VECTOR ( 'NONE', #56841, 1000.000000000000000 ) ;
#171486 = EDGE_CURVE ( 'NONE', #41259, #53690, #214131, .T. ) ;
#171485 = ORIENTED_EDGE ( 'NONE', *, *, #65152, .T. ) ;
#171484 = DIRECTION ( 'NONE',  ( -2.978066053179069723E-16, -1.000000000000000000, -7.147358527629766941E-15 ) ) ;
#171487 = CARTESIAN_POINT ( 'NONE',  ( -20.85000000000000142, 76.00000000001170974, -69.52310748452431710 ) ) ;
#171488 = DIRECTION ( 'NONE',  ( 2.952720810173289112E-16, 0.9651348961777191926, -0.2617529984164898571 ) ) ;
#171489 = CARTESIAN_POINT ( 'NONE',  ( 20.46382478191414833, 65.40137955871450970, -95.34529301517892463 ) ) ;
#171491 = CARTESIAN_POINT ( 'NONE',  ( 20.72390388899123792, 10.58996311843359273, -108.0113482957451509 ) ) ;
#171490 = DIRECTION ( 'NONE',  ( -0.000000000000000000, 0.000000000000000000, 1.000000000000000000 ) ) ;
#171492 = DIRECTION ( 'NONE',  ( 1.000000000000000000, -0.000000000000000000, -0.000000000000000000 ) ) ;
#171493 = CARTESIAN_POINT ( 'NONE',  ( -20.85000000000000142, -1.164121893230052995, -141.9148480855716343 ) ) ;
#171494 = CARTESIAN_POINT ( 'NONE',  ( -21.05000000000000071, 77.16270174994990327, -95.02310748452430289 ) ) ;
#171495 = DIRECTION ( 'NONE',  ( 0.000000000000000000, 0.000000000000000000, -1.000000000000000000 ) ) ;
#171496 = ORIENTED_EDGE ( 'NONE', *, *, #150886, .F. ) ;
#171497 = EDGE_CURVE ( 'NONE', #164364, #56834, #34237, .T. ) ;
#171499 = CIRCLE ( 'NONE', #50816, 0.1000000000000028644 ) ;
#171498 = CARTESIAN_POINT ( 'NONE',  ( 20.94999999999999574, 68.59681812508419796, -224.1344059333694361 ) ) ;
#171500 = ORIENTED_EDGE ( 'NONE', *, *, #126075, .T. ) ;
#171501 = CARTESIAN_POINT ( 'NONE',  ( 21.05000000000000071, 55.59258605799641373, -234.6589115948038966 ) ) ;
#171502 = ORIENTED_EDGE ( 'NONE', *, *, #229538, .F. ) ;
#171503 = DIRECTION ( 'NONE',  ( 0.000000000000000000, 0.000000000000000000, 1.000000000000000000 ) ) ;
#171504 = DIRECTION ( 'NONE',  ( -1.000000000000000000, -0.000000000000000000, -0.000000000000000000 ) ) ;
#171505 = ADVANCED_FACE ( 'NONE', ( #236254 ), #193932, .T. ) ;
#171506 = ORIENTED_EDGE ( 'NONE', *, *, #206753, .T. ) ;
#171507 = CARTESIAN_POINT ( 'NONE',  ( -21.05000000000000426, 30.86995437684646504, -252.0366859498333554 ) ) ;
#171508 =( NAMED_UNIT ( * ) SI_UNIT ( $, .STERADIAN. ) SOLID_ANGLE_UNIT ( ) );
#171509 = EDGE_CURVE ( 'NONE', #177211, #142689, #257051, .T. ) ;
#171510 = AXIS2_PLACEMENT_3D ( 'NONE', #119917, #144565, #221523 ) ;
#171512 = VERTEX_POINT ( 'NONE', #193290 ) ;
#171511 = TOROIDAL_SURFACE ( 'NONE', #88055, 11.89999999999999858, 0.1000000000000000056 ) ;
#171513 = ORIENTED_EDGE ( 'NONE', *, *, #240391, .F. ) ;
#171514 = AXIS2_PLACEMENT_3D ( 'NONE', #150443, #229957, #153032 ) ;
#171515 = DIRECTION ( 'NONE',  ( 0.000000000000000000, -1.000000000000000000, -6.982962677686265922E-15 ) ) ;
#171516 = DIRECTION ( 'NONE',  ( 1.000000000000000000, -0.000000000000000000, -0.000000000000000000 ) ) ;
#171517 = CARTESIAN_POINT ( 'NONE',  ( -18.50000000000000000, 11.75000000001115197, -88.35000000000003695 ) ) ;
#171518 = FACE_OUTER_BOUND ( 'NONE', #120300, .T. ) ;
#171519 = CARTESIAN_POINT ( 'NONE',  ( -23.15000000000000213, 64.35000000001205933, -124.3731074845243825 ) ) ;
#171520 = EDGE_CURVE ( 'NONE', #236424, #107194, #27372, .T. ) ;
#171522 = DIRECTION ( 'NONE',  ( 1.000000000000000000, -7.304098846218133681E-16, 4.217023435051677994E-16 ) ) ;
#171521 = CARTESIAN_POINT ( 'NONE',  ( 18.59999999999999787, 77.26327546522863088, -28.12124281777790813 ) ) ;
#171523 = CARTESIAN_POINT ( 'NONE',  ( -13.88555196119803448, 9.457431528860068326, -81.99991693789972658 ) ) ;
#171525 = VERTEX_POINT ( 'NONE', #15959 ) ;
#171524 = DIRECTION ( 'NONE',  ( -1.000000000000000000, 0.000000000000000000, 0.000000000000000000 ) ) ;
#171526 = CARTESIAN_POINT ( 'NONE',  ( 20.74897398619109268, 10.59569302167756888, -74.67931145625556155 ) ) ;
#171527 = CARTESIAN_POINT ( 'NONE',  ( -21.04999999999994387, 65.15000000001120384, -3.123107484524795474 ) ) ;
#171528 = ORIENTED_EDGE ( 'NONE', *, *, #90610, .F. ) ;
#171529 = DIRECTION ( 'NONE',  ( -1.000000000000000000, 0.000000000000000000, 0.000000000000000000 ) ) ;
#171530 = CARTESIAN_POINT ( 'NONE',  ( 21.05281448260627641, 8.776010158548784190, -146.1735579118114288 ) ) ;
#171532 = ADVANCED_FACE ( 'NONE', ( #197118 ), #176309, .T. ) ;
#171531 = LINE ( 'NONE', #29463, #128991 ) ;
#171534 = EDGE_CURVE ( 'NONE', #40979, #101028, #38078, .T. ) ;
#171533 = ORIENTED_EDGE ( 'NONE', *, *, #77243, .F. ) ;
#171535 = VECTOR ( 'NONE', #226702, 1000.000000000000000 ) ;
#171536 = CARTESIAN_POINT ( 'NONE',  ( -16.81930730667007623, 60.97200056715625749, -220.9710398144006547 ) ) ;
#171537 = DIRECTION ( 'NONE',  ( 0.000000000000000000, 0.000000000000000000, -1.000000000000000000 ) ) ;
#171538 = DIRECTION ( 'NONE',  ( 0.000000000000000000, 0.4999999999999088507, -0.8660254037844913322 ) ) ;
#171539 = ORIENTED_EDGE ( 'NONE', *, *, #61842, .F. ) ;
#171540 = ORIENTED_EDGE ( 'NONE', *, *, #62639, .F. ) ;
#171541 = EDGE_CURVE ( 'NONE', #217495, #167927, #81452, .T. ) ;
#171542 = DIRECTION ( 'NONE',  ( 0.000000000000000000, 0.000000000000000000, -1.000000000000000000 ) ) ;
#171543 = CARTESIAN_POINT ( 'NONE',  ( -18.41431012584568450, 64.51252797080414325, -160.7963434976261112 ) ) ;
#171544 = CARTESIAN_POINT ( 'NONE',  ( 20.94999999999999929, 5.000000000011153745, -179.9052660189130677 ) ) ;
#171546 = ADVANCED_FACE ( 'NONE', ( #194593 ), #115027, .T. ) ;
#171545 = LINE ( 'NONE', #172848, #59263 ) ;
#171547 = EDGE_LOOP ( 'NONE', ( #75004, #239073, #216499, #105479 ) ) ;
#171548 = ADVANCED_FACE ( 'NONE', ( #237546 ), #194126, .F. ) ;
#171549 = CARTESIAN_POINT ( 'NONE',  ( 15.06592377766032165, 46.82384836101673642, -234.6777522051880283 ) ) ;
#171550 = AXIS2_PLACEMENT_3D ( 'NONE', #152734, #210124, #52292 ) ;
#171551 = DIRECTION ( 'NONE',  ( 0.000000000000000000, 0.000000000000000000, -1.000000000000000000 ) ) ;
#171552 = CIRCLE ( 'NONE', #204829, 0.09999999999999939493 ) ;
#171553 = CARTESIAN_POINT ( 'NONE',  ( 20.94999999999999929, 5.000000000011153745, -54.59473398108690390 ) ) ;
#171554 = DIRECTION ( 'NONE',  ( 0.000000000000000000, -0.3738317757008748909, -0.9274965247785733613 ) ) ;
#171555 = ORIENTED_EDGE ( 'NONE', *, *, #54292, .F. ) ;
#171556 = CYLINDRICAL_SURFACE ( 'NONE', #109320, 0.09999999999999939493 ) ;
#171558 = ORIENTED_EDGE ( 'NONE', *, *, #3752, .F. ) ;
#171557 = FACE_OUTER_BOUND ( 'NONE', #173250, .T. ) ;
#171559 = CARTESIAN_POINT ( 'NONE',  ( 18.59999999999999787, -9.399999999988843058, -174.3820418481727188 ) ) ;
#171561 = ADVANCED_FACE ( 'NONE', ( #203 ), #215404, .T. ) ;
#171560 = CARTESIAN_POINT ( 'NONE',  ( 22.48970261584622321, 31.84544391280713072, -238.9419228052725543 ) ) ;
#171562 = CYLINDRICAL_SURFACE ( 'NONE', #33663, 11.80000000000000249 ) ;
#171563 = CARTESIAN_POINT ( 'NONE',  ( 21.05000000000000071, -9.499999999988844479, -191.1060308773475072 ) ) ;
#171564 = EDGE_CURVE ( 'NONE', #201210, #96287, #198413, .T. ) ;
#171565 = CARTESIAN_POINT ( 'NONE',  ( -20.54999999999999716, 5.159242054424403534, -213.4109969955686665 ) ) ;
#171566 = VERTEX_POINT ( 'NONE', #135852 ) ;
#171567 = LINE ( 'NONE', #128559, #200553 ) ;
#171568 = DIRECTION ( 'NONE',  ( -1.000000000000000000, 0.000000000000000000, -0.000000000000000000 ) ) ;
#171569 = DIRECTION ( 'NONE',  ( 0.000000000000000000, 0.8814952561688430555, -0.4721928772777346239 ) ) ;
#171570 = AXIS2_PLACEMENT_3D ( 'NONE', #177033, #122172, #99995 ) ;
#171571 = VERTEX_POINT ( 'NONE', #19796 ) ;
#171572 = CARTESIAN_POINT ( 'NONE',  ( -20.64999999999999858, 7.150000000011155876, -146.2500000000000284 ) ) ;
#171573 = CARTESIAN_POINT ( 'NONE',  ( -18.59999999999999787, 11.65000000001115232, -54.85000000000000142 ) ) ;
#171574 = LINE ( 'NONE', #104168, #238027 ) ;
#171575 = CARTESIAN_POINT ( 'NONE',  ( 11.60000000000000142, -12.24999999999999822, 15.00000000000000355 ) ) ;
#171576 = EDGE_CURVE ( 'NONE', #173596, #229669, #177580, .T. ) ;
#171577 = CARTESIAN_POINT ( 'NONE',  ( 21.05000000000000071, 6.540656951712403355, -167.5999999999999659 ) ) ;
#171578 = CARTESIAN_POINT ( 'NONE',  ( 14.22916352759893854, 9.457410930301318075, -185.9999159087462886 ) ) ;
#171579 = ORIENTED_EDGE ( 'NONE', *, *, #148210, .F. ) ;
#171580 = VERTEX_POINT ( 'NONE', #234982 ) ;
#171581 = DIRECTION ( 'NONE',  ( -1.000000000000000000, 0.000000000000000000, 0.000000000000000000 ) ) ;
#171582 = CARTESIAN_POINT ( 'NONE',  ( 22.60000000000000142, 0.1008583691098682150, -88.75043287651064361 ) ) ;
#171583 = VECTOR ( 'NONE', #155080, 1000.000000000000000 ) ;
#171584 = FACE_OUTER_BOUND ( 'NONE', #253631, .T. ) ;
#171585 = FACE_OUTER_BOUND ( 'NONE', #34365, .T. ) ;
#171586 = DIRECTION ( 'NONE',  ( 0.000000000000000000, -3.552713678800542739E-15, 1.000000000000000000 ) ) ;
#171587 = VECTOR ( 'NONE', #227950, 1000.000000000000114 ) ;
#171588 = EDGE_CURVE ( 'NONE', #250894, #13299, #133311, .T. ) ;
#171589 = DIRECTION ( 'NONE',  ( 0.000000000000000000, 0.000000000000000000, -1.000000000000000000 ) ) ;
#171590 = VECTOR ( 'NONE', #225512, 1000.000000000000000 ) ;
#171591 = CARTESIAN_POINT ( 'NONE',  ( -16.93226657140833069, 9.999543822735571297, -113.0787131109736521 ) ) ;
#171592 = TOROIDAL_SURFACE ( 'NONE', #92440, 0.9750000000000019762, 0.1000000000000000056 ) ;
#171593 = EDGE_CURVE ( 'NONE', #67110, #189061, #81631, .T. ) ;
#171594 = AXIS2_PLACEMENT_3D ( 'NONE', #3003, #58152, #145085 ) ;
#171595 = FACE_OUTER_BOUND ( 'NONE', #91694, .T. ) ;
#171596 = ORIENTED_EDGE ( 'NONE', *, *, #95569, .T. ) ;
#171597 = DIRECTION ( 'NONE',  ( 7.304098846218136639E-16, -0.4721928772777346239, -0.8814952561688430555 ) ) ;
#171598 = ADVANCED_FACE ( 'NONE', ( #120202 ), #62759, .F. ) ;
#171599 = AXIS2_PLACEMENT_3D ( 'NONE', #87161, #247541, #49332 ) ;
#171600 = EDGE_CURVE ( 'NONE', #258086, #124815, #40671, .T. ) ;
#171601 = ORIENTED_EDGE ( 'NONE', *, *, #226737, .T. ) ;
#171602 = DIRECTION ( 'NONE',  ( 1.000000000000000000, 0.000000000000000000, 0.000000000000000000 ) ) ;
#171603 = CARTESIAN_POINT ( 'NONE',  ( 20.95595624212412389, 10.62389120309414992, -7.629632914126892373 ) ) ;
#171604 = CARTESIAN_POINT ( 'NONE',  ( 21.05000000000000071, 8.776282895303632259, -79.15000000000004832 ) ) ;
#171605 = SPHERICAL_SURFACE ( 'NONE', #194816, 0.1000000000000000056 ) ;
#171607 = EDGE_CURVE ( 'NONE', #11996, #92498, #44274, .T. ) ;
#171606 = CARTESIAN_POINT ( 'NONE',  ( 21.07964655665547582, 22.04583520435846822, -231.7687797005887091 ) ) ;
#171609 = CYLINDRICAL_SURFACE ( 'NONE', #153799, 0.09999999999999939493 ) ;
#171608 = AXIS2_PLACEMENT_3D ( 'NONE', #210278, #31661, #111168 ) ;
#171610 = DIRECTION ( 'NONE',  ( 0.000000000000000000, -0.9915357197604804940, 0.1298341882520397950 ) ) ;
#171611 = VERTEX_POINT ( 'NONE', #199724 ) ;
#171612 = LINE ( 'NONE', #166473, #228959 ) ;
#171613 = DIRECTION ( 'NONE',  ( 0.000000000000000000, 0.000000000000000000, -1.000000000000000000 ) ) ;
#171614 = CARTESIAN_POINT ( 'NONE',  ( -23.15000000000000213, 1.115600667400684642E-11, -67.00000000000000000 ) ) ;
#171615 = LINE ( 'NONE', #192432, #256015 ) ;
#171616 = TOROIDAL_SURFACE ( 'NONE', #84038, 0.6000000000000004219, 0.1000000000000000056 ) ;
#171617 = AXIS2_PLACEMENT_3D ( 'NONE', #131241, #49133, #73876 ) ;
#171618 = CARTESIAN_POINT ( 'NONE',  ( 18.58719872626880587, 85.56664439761047447, -96.20062928812723158 ) ) ;
#171619 = EDGE_CURVE ( 'NONE', #190986, #236967, #173311, .T. ) ;
#171620 = ADVANCED_FACE ( 'NONE', ( #183986 ), #52626, .T. ) ;
#171621 = EDGE_LOOP ( 'NONE', ( #82830, #69320, #1036, #105371 ) ) ;
#171622 = AXIS2_PLACEMENT_3D ( 'NONE', #94863, #11505, #130139 ) ;
#171623 = ORIENTED_EDGE ( 'NONE', *, *, #82726, .F. ) ;
#171624 = EDGE_CURVE ( 'NONE', #121003, #210954, #84847, .T. ) ;
#171625 = AXIS2_PLACEMENT_3D ( 'NONE', #10013, #7435, #166549 ) ;
#171626 = ORIENTED_EDGE ( 'NONE', *, *, #42233, .F. ) ;
#171627 = CARTESIAN_POINT ( 'NONE',  ( -20.90000000000000213, 11.50977166988710820, -1.786320531569725478 ) ) ;
#171628 = CARTESIAN_POINT ( 'NONE',  ( 18.44444291854881612, -9.490101180932075664, -174.1289039648910375 ) ) ;
#171629 = ORIENTED_EDGE ( 'NONE', *, *, #162409, .F. ) ;
#171630 = CARTESIAN_POINT ( 'NONE',  ( 18.44208962362688098, -9.552340496897864242, -174.3421730554626379 ) ) ;
#171631 = DIRECTION ( 'NONE',  ( 1.000000000000000000, 0.000000000000000000, 0.000000000000000000 ) ) ;
#171632 = TOROIDAL_SURFACE ( 'NONE', #109043, 3.899999999999999467, 0.1000000000000000056 ) ;
#171633 = VERTEX_POINT ( 'NONE', #121479 ) ;
#171634 = EDGE_CURVE ( 'NONE', #56953, #164631, #202483, .T. ) ;
#171635 = EDGE_CURVE ( 'NONE', #150487, #250267, #24940, .T. ) ;
#171636 = VECTOR ( 'NONE', #188862, 1000.000000000000000 ) ;
#171637 =( BOUNDED_SURFACE ( )  B_SPLINE_SURFACE ( 3, 2, ( 
 ( #240977, #165281, #27092 ),
 ( #81854, #204393, #3629 ),
 ( #162733, #106569, #143131 ),
 ( #23234, #146983, #242242 ) ),
 .UNSPECIFIED., .F., .F., .T. ) 
 B_SPLINE_SURFACE_WITH_KNOTS ( ( 4, 4 ),
 ( 3, 3 ),
 ( 6.938893903907228378E-18, 0.001979672783031562362 ),
 ( 0.000000000000000000, 1.000000000000000000 ),
 .UNSPECIFIED. ) 
 GEOMETRIC_REPRESENTATION_ITEM ( )  RATIONAL_B_SPLINE_SURFACE ( (
 ( 1.000000000000000000, 0.7103081912008362142, 1.000000000000000000),
 ( 1.000000000000000000, 0.7104998333558624202, 1.000000000000000000),
 ( 1.000000000000000000, 0.7107238315756159164, 1.000000000000000000),
 ( 1.000000000000000000, 0.7110073749539299603, 1.000000000000000000) ) ) 
 REPRESENTATION_ITEM ( '' )  SURFACE ( )  );
#171638 = CIRCLE ( 'NONE', #117455, 0.09999999999998898659 ) ;
#171639 = CIRCLE ( 'NONE', #59140, 0.09999999999998898659 ) ;
#171640 = CARTESIAN_POINT ( 'NONE',  ( 18.52351027002947603, -9.642162904684033364, -174.2150469505097874 ) ) ;
#171641 = ADVANCED_FACE ( 'NONE', ( #202273 ), #114993, .F. ) ;
#171642 = ORIENTED_EDGE ( 'NONE', *, *, #232564, .T. ) ;
#171643 = FACE_OUTER_BOUND ( 'NONE', #80227, .T. ) ;
#171644 = DIRECTION ( 'NONE',  ( -0.7071067811865389130, 0.6453109281988527179, 0.2890913453342166539 ) ) ;
#171646 = VERTEX_POINT ( 'NONE', #164439 ) ;
#171645 = DIRECTION ( 'NONE',  ( 0.000000000000000000, 0.000000000000000000, 1.000000000000000000 ) ) ;
#171647 = ADVANCED_FACE ( 'NONE', ( #185277 ), #240120, .F. ) ;
#171648 = DIRECTION ( 'NONE',  ( 1.000000000000000000, -0.000000000000000000, 0.000000000000000000 ) ) ;
#171649 = CARTESIAN_POINT ( 'NONE',  ( 21.05000000000000071, 6.257814610487280937, -133.9022097086912311 ) ) ;
#171650 = CARTESIAN_POINT ( 'NONE',  ( -16.97683809663752186, 50.93224991157930504, -232.2540631895259082 ) ) ;
#171651 = DIRECTION ( 'NONE',  ( 1.000000000000000000, 0.000000000000000000, 0.000000000000000000 ) ) ;
#171652 = EDGE_CURVE ( 'NONE', #133332, #30250, #239909, .T. ) ;
#171653 = CARTESIAN_POINT ( 'NONE',  ( 20.94999999999999574, 16.53615870702968138, -240.8540256063542984 ) ) ;
#171654 = DIRECTION ( 'NONE',  ( 1.000000000000000000, -1.335000415235278971E-16, 2.979993593738921214E-16 ) ) ;
#171655 = DIRECTION ( 'NONE',  ( 1.000000000000000000, 0.000000000000000000, 0.000000000000000000 ) ) ;
#171657 = VERTEX_POINT ( 'NONE', #243956 ) ;
#171656 = CARTESIAN_POINT ( 'NONE',  ( 21.05000000000000071, 70.15000000001211333, -126.3906102602463619 ) ) ;
#171658 = EDGE_LOOP ( 'NONE', ( #154176, #141509, #69992, #133163 ) ) ;
#171660 = CARTESIAN_POINT ( 'NONE',  ( -12.42749937872396337, 9.370689921613768902, -84.52646512666109402 ) ) ;
#171659 = DIRECTION ( 'NONE',  ( 0.000000000000000000, 0.000000000000000000, 1.000000000000000000 ) ) ;
#171662 = ORIENTED_EDGE ( 'NONE', *, *, #206842, .T. ) ;
#171661 = CARTESIAN_POINT ( 'NONE',  ( 20.94999999999999574, 46.59314322379660922, -243.1831726892433210 ) ) ;
#171663 = VERTEX_POINT ( 'NONE', #103146 ) ;
#171664 = CARTESIAN_POINT ( 'NONE',  ( 23.14999999999999503, 11.65000000001116298, -79.15000000000004832 ) ) ;
#171665 = VECTOR ( 'NONE', #2445, 1000.000000000000000 ) ;
#171666 = CARTESIAN_POINT ( 'NONE',  ( 18.59999999999999076, 6.650000000011155876, -121.8500000000000369 ) ) ;
#171667 = DIRECTION ( 'NONE',  ( 0.000000000000000000, 0.000000000000000000, 1.000000000000000000 ) ) ;
#171668 = CARTESIAN_POINT ( 'NONE',  ( -18.59999999999999787, 11.65000000001115232, -112.6500000000000341 ) ) ;
#171669 = ADVANCED_FACE ( 'NONE', ( #2763 ), #238829, .T. ) ;
#171670 = CARTESIAN_POINT ( 'NONE',  ( -23.25000000000000000, 11.38316329224760359, -198.5208684056144079 ) ) ;
#171671 = DIRECTION ( 'NONE',  ( 0.7071067811865214825, -0.7071067811865735520, 0.000000000000000000 ) ) ;
#171672 = CYLINDRICAL_SURFACE ( 'NONE', #160540, 0.09999999999999939493 ) ;
#171673 = EDGE_CURVE ( 'NONE', #5531, #220045, #40014, .T. ) ;
#171674 = ORIENTED_EDGE ( 'NONE', *, *, #200150, .T. ) ;
#171675 = ORIENTED_EDGE ( 'NONE', *, *, #45085, .F. ) ;
#171676 = FACE_OUTER_BOUND ( 'NONE', #42398, .T. ) ;
#171677 = EDGE_LOOP ( 'NONE', ( #4145, #42593, #234421, #71404 ) ) ;
#171678 = PLANE ( 'NONE',  #171924 ) ;
#171679 = ORIENTED_EDGE ( 'NONE', *, *, #144056, .T. ) ;
#171680 = CARTESIAN_POINT ( 'NONE',  ( 20.10000000000000853, 3.362550747017865493, 28.82623795144604983 ) ) ;
#171681 = AXIS2_PLACEMENT_3D ( 'NONE', #159695, #239219, #140099 ) ;
#171682 = LINE ( 'NONE', #212073, #163742 ) ;
#171683 = EDGE_CURVE ( 'NONE', #129928, #37535, #106589, .T. ) ;
#171684 = CYLINDRICAL_SURFACE ( 'NONE', #27615, 0.09999999999999939493 ) ;
#171685 = ORIENTED_EDGE ( 'NONE', *, *, #123843, .F. ) ;
#171687 = CARTESIAN_POINT ( 'NONE',  ( 21.13736287352038445, 22.07931554675867858, -232.6128641271329229 ) ) ;
#171686 = SHAPE_REPRESENTATION ( 'Injection Molded Chain Links 13', ( #2425 ), #164577 ) ;
#171688 = ORIENTED_EDGE ( 'NONE', *, *, #207305, .F. ) ;
#171689 = CARTESIAN_POINT ( 'NONE',  ( -20.64999999999999858, 73.60000000001254250, -183.2477294072864709 ) ) ;
#171690 = CARTESIAN_POINT ( 'NONE',  ( 21.04999999999999716, 8.871279686006802834, -109.0586289951409498 ) ) ;
#171691 = VERTEX_POINT ( 'NONE', #64041 ) ;
#171693 = DIRECTION ( 'NONE',  ( 2.952720810173289112E-16, -1.000000000000000000, -0.000000000000000000 ) ) ;
#171692 = VECTOR ( 'NONE', #7646, 1000.000000000000000 ) ;
#171694 = VERTEX_POINT ( 'NONE', #143576 ) ;
#171697 = VERTEX_POINT ( 'NONE', #65318 ) ;
#171696 = CARTESIAN_POINT ( 'NONE',  ( 20.85000000000000142, -1.835859311432481045, -78.50443916879852679 ) ) ;
#171695 = CARTESIAN_POINT ( 'NONE',  ( 22.49999999999999289, 55.96443555106008461, -232.8914797391818752 ) ) ;
#171698 = EDGE_CURVE ( 'NONE', #247553, #28931, #244156, .T. ) ;
#171699 = CARTESIAN_POINT ( 'NONE',  ( 23.25000000000000000, -11.64999999998884483, -67.00000000000004263 ) ) ;
#171700 = ORIENTED_EDGE ( 'NONE', *, *, #56023, .T. ) ;
#171701 = VECTOR ( 'NONE', #102959, 1000.000000000000000 ) ;
#171702 = VERTEX_POINT ( 'NONE', #50868 ) ;
#171703 = CIRCLE ( 'NONE', #59195, 0.1000000000000028644 ) ;
#171704 = DIRECTION ( 'NONE',  ( -1.000000000000000000, -1.394253735153569469E-16, -2.602809386958778209E-16 ) ) ;
#171705 = ORIENTED_EDGE ( 'NONE', *, *, #226538, .F. ) ;
#171706 = CARTESIAN_POINT ( 'NONE',  ( 18.59999999999999076, 11.75000000001115907, -88.75000000000004263 ) ) ;
#171707 = CARTESIAN_POINT ( 'NONE',  ( -20.54999999999999716, 2.399999999999999467, -20.27537807723789953 ) ) ;
#171708 = CARTESIAN_POINT ( 'NONE',  ( -21.05000000000000071, -1.162701749926853712, -108.6000000000000227 ) ) ;
#171709 = CARTESIAN_POINT ( 'NONE',  ( 18.54148534481893762, 67.49261718274587452, -195.4446851895584416 ) ) ;
#171710 = CARTESIAN_POINT ( 'NONE',  ( -16.77683809663752257, 9.950000000011138823, -87.85000000000005116 ) ) ;
#171711 = CIRCLE ( 'NONE', #17543, 0.1000000000000028644 ) ;
#171712 = ORIENTED_EDGE ( 'NONE', *, *, #157105, .T. ) ;
#171713 = CIRCLE ( 'NONE', #246690, 0.1000000000000025591 ) ;
#171714 = CARTESIAN_POINT ( 'NONE',  ( -16.93262454970420094, 44.04387347954221354, -235.2829689446594159 ) ) ;
#171715 = CARTESIAN_POINT ( 'NONE',  ( -21.04386569057497525, 64.25000000001236344, -109.8802701327446130 ) ) ;
#171716 = CARTESIAN_POINT ( 'NONE',  ( 21.08376601933332495, 6.341947271286813681, -33.43622398907000104 ) ) ;
#171717 = VERTEX_POINT ( 'NONE', #107004 ) ;
#171718 = CYLINDRICAL_SURFACE ( 'NONE', #22048, 0.09999999999999939493 ) ;
#171719 = VERTEX_POINT ( 'NONE', #146138 ) ;
#171720 = CARTESIAN_POINT ( 'NONE',  ( 23.14999999999999858, 5.900000000011162093, -123.7809002353436654 ) ) ;
#171721 = ORIENTED_EDGE ( 'NONE', *, *, #46960, .T. ) ;
#171722 = CARTESIAN_POINT ( 'NONE',  ( 20.94999999999999929, -11.48912529306489994, -197.8999999999999773 ) ) ;
#171723 = DIRECTION ( 'NONE',  ( -1.000000000000000000, 0.000000000000000000, 0.000000000000000000 ) ) ;
#171725 = EDGE_LOOP ( 'NONE', ( #195651, #195229, #49401, #145736, #131322, #26441, #205846, #218402, #131932, #23708 ) ) ;
#171724 = DIRECTION ( 'NONE',  ( 0.000000000000000000, 1.734723475976997999E-14, -1.000000000000000000 ) ) ;
#171726 = DIRECTION ( 'NONE',  ( -0.000000000000000000, -0.8127272543710951647, 0.5826443254700256480 ) ) ;
#171727 = VERTEX_POINT ( 'NONE', #208710 ) ;
#171728 = DIRECTION ( 'NONE',  ( 1.000000000000000000, 0.000000000000000000, 0.000000000000000000 ) ) ;
#171729 = TOROIDAL_SURFACE ( 'NONE', #121651, 3.899999999999999467, 0.1000000000000000056 ) ;
#171731 = EDGE_CURVE ( 'NONE', #22950, #70645, #219035, .T. ) ;
#171730 = AXIS2_PLACEMENT_3D ( 'NONE', #200098, #120581, #21478 ) ;
#171732 = LINE ( 'NONE', #152164, #247734 ) ;
#171733 = ORIENTED_EDGE ( 'NONE', *, *, #243030, .T. ) ;
#171734 = CIRCLE ( 'NONE', #204995, 11.70000000000000284 ) ;
#171735 = DIRECTION ( 'NONE',  ( 0.000000000000000000, -0.9908441862701605762, -0.1350103645451835310 ) ) ;
#171736 = DIRECTION ( 'NONE',  ( -1.000000000000000000, 0.000000000000000000, -0.000000000000000000 ) ) ;
#171737 = ORIENTED_EDGE ( 'NONE', *, *, #9090, .T. ) ;
#171738 = CARTESIAN_POINT ( 'NONE',  ( 18.59999999999999787, 72.05339752741123505, -225.0867394276846483 ) ) ;
#171739 = ORIENTED_EDGE ( 'NONE', *, *, #24740, .F. ) ;
#171740 = DIRECTION ( 'NONE',  ( -1.000000000000000000, 7.304098846218134667E-16, 5.100424963727256530E-30 ) ) ;
#171741 = CARTESIAN_POINT ( 'NONE',  ( -18.40000000000000213, 62.23844973457045882, -209.3750075427748527 ) ) ;
#171742 = EDGE_CURVE ( 'NONE', #193752, #251409, #108312, .T. ) ;
#171743 = CIRCLE ( 'NONE', #205008, 7.800000000000001599 ) ;
#171744 = EDGE_CURVE ( 'NONE', #252820, #42259, #156727, .T. ) ;
#171747 = ORIENTED_EDGE ( 'NONE', *, *, #238534, .T. ) ;
#171746 = EDGE_LOOP ( 'NONE', ( #75619, #147562, #212126 ) ) ;
#171745 = DIRECTION ( 'NONE',  ( -1.000000000000000000, 0.000000000000000000, 0.000000000000000000 ) ) ;
#171748 = DIRECTION ( 'NONE',  ( -1.000000000000000000, 0.000000000000000000, 0.000000000000000000 ) ) ;
#171749 = DIRECTION ( 'NONE',  ( 1.000000000000000000, 0.000000000000000000, -0.000000000000000000 ) ) ;
#171750 = CARTESIAN_POINT ( 'NONE',  ( -20.54999999999999716, 7.128833340094563376, -233.7327013124401276 ) ) ;
#171752 = CARTESIAN_POINT ( 'NONE',  ( -24.30000000000000071, 3.175288713399619045, -347.0000000000001137 ) ) ;
#171751 = DIRECTION ( 'NONE',  ( 1.000000000000000000, 0.000000000000000000, 0.000000000000000000 ) ) ;
#171753 = DIRECTION ( 'NONE',  ( -2.561896900575096011E-15, -0.5907332058517279494, 0.8068669527897025517 ) ) ;
#171754 = CYLINDRICAL_SURFACE ( 'NONE', #198294, 0.1000000000000072220 ) ;
#171755 = EDGE_CURVE ( 'NONE', #32241, #149370, #148312, .T. ) ;
#171756 = DIRECTION ( 'NONE',  ( 1.000000000000000000, 0.000000000000000000, 0.000000000000000000 ) ) ;
#171757 = VECTOR ( 'NONE', #213774, 1000.000000000000000 ) ;
#171758 = CARTESIAN_POINT ( 'NONE',  ( 20.94999999999999929, 77.16412189325258453, -28.10825939895270764 ) ) ;
#171759 = VERTEX_POINT ( 'NONE', #126586 ) ;
#171760 = ORIENTED_EDGE ( 'NONE', *, *, #515, .F. ) ;
#171761 = ADVANCED_FACE ( 'NONE', ( #49613 ), #207423, .T. ) ;
#171762 = CARTESIAN_POINT ( 'NONE',  ( -14.00000000000000178, 9.850000000011133849, -117.2500000000000284 ) ) ;
#171764 = ORIENTED_EDGE ( 'NONE', *, *, #229981, .T. ) ;
#171763 = EDGE_CURVE ( 'NONE', #217031, #80663, #246522, .T. ) ;
#171765 = ORIENTED_EDGE ( 'NONE', *, *, #36169, .T. ) ;
#171767 = DIRECTION ( 'NONE',  ( 1.000000000000000000, 0.000000000000000000, 0.000000000000000000 ) ) ;
#171766 = TOROIDAL_SURFACE ( 'NONE', #205022, 3.899999999999999467, 0.1000000000000000056 ) ;
#171768 = ORIENTED_EDGE ( 'NONE', *, *, #142886, .T. ) ;
#171769 = EDGE_CURVE ( 'NONE', #239767, #172933, #87443, .T. ) ;
#171770 = AXIS2_PLACEMENT_3D ( 'NONE', #108957, #146792, #223768 ) ;
#171771 = ORIENTED_EDGE ( 'NONE', *, *, #105931, .F. ) ;
#171773 = EDGE_CURVE ( 'NONE', #43551, #234552, #48352, .T. ) ;
#171772 = AXIS2_PLACEMENT_3D ( 'NONE', #242534, #105557, #23532 ) ;
#171774 = AXIS2_PLACEMENT_3D ( 'NONE', #71968, #131931, #53677 ) ;
#171775 = DIRECTION ( 'NONE',  ( -1.000000000000000000, 0.000000000000000000, -0.000000000000000000 ) ) ;
#171776 = AXIS2_PLACEMENT_3D ( 'NONE', #147361, #89943, #209919 ) ;
#171778 = VERTEX_POINT ( 'NONE', #167031 ) ;
#171777 = ORIENTED_EDGE ( 'NONE', *, *, #189173, .T. ) ;
#171779 = ORIENTED_EDGE ( 'NONE', *, *, #29248, .F. ) ;
#171780 = AXIS2_PLACEMENT_3D ( 'NONE', #142971, #244657, #46450 ) ;
#171781 = EDGE_LOOP ( 'NONE', ( #94367, #243125, #213747, #66265 ) ) ;
#171783 = ORIENTED_EDGE ( 'NONE', *, *, #68217, .F. ) ;
#171782 = VECTOR ( 'NONE', #225486, 1000.000000000000000 ) ;
#171784 = CYLINDRICAL_SURFACE ( 'NONE', #142850, 0.09999999999999939493 ) ;
#171785 = DIRECTION ( 'NONE',  ( -1.000000000000000000, 0.000000000000000000, 0.000000000000000000 ) ) ;
#171786 = CARTESIAN_POINT ( 'NONE',  ( -15.57281606413133090, 9.370655051134637148, -185.0258232559808675 ) ) ;
#171787 = ORIENTED_EDGE ( 'NONE', *, *, #231444, .T. ) ;
#171788 = CARTESIAN_POINT ( 'NONE',  ( 20.94999999999999929, 1.115600667400684642E-11, -100.5000000000000426 ) ) ;
#171789 = DIRECTION ( 'NONE',  ( -1.000000000000000000, -0.000000000000000000, -0.000000000000000000 ) ) ;
#171791 = EDGE_LOOP ( 'NONE', ( #111794, #192548, #14721, #241233 ) ) ;
#171790 = FACE_OUTER_BOUND ( 'NONE', #232096, .T. ) ;
#171792 = DIRECTION ( 'NONE',  ( 2.952720810173288619E-16, -0.4721928772777346239, -0.8814952561688430555 ) ) ;
#171793 = ORIENTED_EDGE ( 'NONE', *, *, #236832, .F. ) ;
#171794 = SPHERICAL_SURFACE ( 'NONE', #62149, 0.1000000000000000056 ) ;
#171795 = AXIS2_PLACEMENT_3D ( 'NONE', #204177, #184624, #69838 ) ;
#171797 = ADVANCED_FACE ( 'NONE', ( #127875 ), #209985, .T. ) ;
#171796 = ORIENTED_EDGE ( 'NONE', *, *, #112447, .F. ) ;
#171798 = AXIS2_PLACEMENT_3D ( 'NONE', #92609, #169647, #249153 ) ;
#171799 = DIRECTION ( 'NONE',  ( 0.000000000000000000, -0.9553114395362878319, -0.2956011730205167498 ) ) ;
#171801 = ORIENTED_EDGE ( 'NONE', *, *, #150339, .F. ) ;
#171800 = AXIS2_PLACEMENT_3D ( 'NONE', #7101, #61960, #86620 ) ;
#171802 = CIRCLE ( 'NONE', #92646, 0.09999999999999939493 ) ;
#171804 = DIRECTION ( 'NONE',  ( 0.000000000000000000, 0.000000000000000000, 1.000000000000000000 ) ) ;
#171803 = FACE_OUTER_BOUND ( 'NONE', #243133, .T. ) ;
#171805 = CIRCLE ( 'NONE', #17629, 0.1000000000000000472 ) ;
#171806 = DIRECTION ( 'NONE',  ( 0.000000000000000000, -7.304098846218139203E-15, 1.000000000000000000 ) ) ;
#171807 = DIRECTION ( 'NONE',  ( 0.000000000000000000, -1.000000000000000000, -6.982962677686265922E-15 ) ) ;
#171808 = DIRECTION ( 'NONE',  ( -0.000000000000000000, 1.000000000000000000, 6.982962677686266711E-15 ) ) ;
#171810 = EDGE_LOOP ( 'NONE', ( #51089, #77628, #51028, #81530 ) ) ;
#171809 = CIRCLE ( 'NONE', #50943, 1.749999999999999778 ) ;
#171811 = ORIENTED_EDGE ( 'NONE', *, *, #11440, .F. ) ;
#171812 = CIRCLE ( 'NONE', #142530, 0.5000000000000004441 ) ;
#171813 = EDGE_CURVE ( 'NONE', #82125, #203694, #127461, .T. ) ;
#171814 = CARTESIAN_POINT ( 'NONE',  ( 23.14999999999998437, 35.00313497133259943, -245.8551024614896505 ) ) ;
#171815 = DIRECTION ( 'NONE',  ( 0.000000000000000000, 0.2617529984165031243, 0.9651348961777157509 ) ) ;
#171816 = ORIENTED_EDGE ( 'NONE', *, *, #203886, .T. ) ;
#171817 = DIRECTION ( 'NONE',  ( 1.000000000000000000, -0.000000000000000000, -0.000000000000000000 ) ) ;
#171818 = ORIENTED_EDGE ( 'NONE', *, *, #167966, .T. ) ;
#171819 = CARTESIAN_POINT ( 'NONE',  ( -22.50000000000094147, 0.1008583691097610646, -55.25043287651063650 ) ) ;
#171820 = AXIS2_PLACEMENT_3D ( 'NONE', #28104, #189721, #12389 ) ;
#171821 = CARTESIAN_POINT ( 'NONE',  ( 20.95512820512820440, 60.15812638745688901, -221.3479132702343009 ) ) ;
#171822 = DIRECTION ( 'NONE',  ( 0.000000000000000000, 1.000000000000000000, -6.308085367188393199E-16 ) ) ;
#171823 = ORIENTED_EDGE ( 'NONE', *, *, #101472, .T. ) ;
#171824 = DIRECTION ( 'NONE',  ( 1.000000000000000000, 0.000000000000000000, -0.000000000000000000 ) ) ;
#171825 = FILL_AREA_STYLE_COLOUR ( '', #68909 ) ;
#171826 = CIRCLE ( 'NONE', #205084, 0.8750000000000007772 ) ;
#171827 = AXIS2_PLACEMENT_3D ( 'NONE', #91746, #171334, #145931 ) ;
#171828 = EDGE_CURVE ( 'NONE', #93087, #132474, #52167, .T. ) ;
#171829 = ORIENTED_EDGE ( 'NONE', *, *, #117947, .T. ) ;
#171831 = EDGE_LOOP ( 'NONE', ( #104240, #36524, #39000, #42524 ) ) ;
#171830 = AXIS2_PLACEMENT_3D ( 'NONE', #187240, #145512, #226315 ) ;
#171832 = ORIENTED_EDGE ( 'NONE', *, *, #43026, .F. ) ;
#171833 = CARTESIAN_POINT ( 'NONE',  ( -20.94999999999999929, -11.64999999998884483, -164.5000000000000000 ) ) ;
#171834 = CARTESIAN_POINT ( 'NONE',  ( -20.85000000000000142, -1.164121893241208960, -41.21484808557161017 ) ) ;
#171835 = CARTESIAN_POINT ( 'NONE',  ( 23.24999999999999289, 69.45000000001199680, -115.1731074845243512 ) ) ;
#171836 = CARTESIAN_POINT ( 'NONE',  ( -18.59999999999999787, 44.43513953521873106, -247.3415577889845736 ) ) ;
#171837 = CARTESIAN_POINT ( 'NONE',  ( 21.14999999999999858, 76.00000000001219291, -143.0637644362255401 ) ) ;
#171838 = EDGE_CURVE ( 'NONE', #191945, #136081, #11802, .T. ) ;
#171840 = LINE ( 'NONE', #72731, #99157 ) ;
#171839 = LINE ( 'NONE', #11457, #228779 ) ;
#171842 = ORIENTED_EDGE ( 'NONE', *, *, #154169, .F. ) ;
#171841 = CARTESIAN_POINT ( 'NONE',  ( 18.59999999999998721, 19.85039924724470950, -102.7803030578013903 ) ) ;
#171843 = CARTESIAN_POINT ( 'NONE',  ( 17.74533788810830259, 10.81849979148194763, -43.81362267494758811 ) ) ;
#171844 = EDGE_LOOP ( 'NONE', ( #120291, #183519, #129396, #221384 ) ) ;
#171845 = SPHERICAL_SURFACE ( 'NONE', #98799, 0.1000000000000000056 ) ;
#171846 = ORIENTED_EDGE ( 'NONE', *, *, #207253, .F. ) ;
#171847 = ORIENTED_EDGE ( 'NONE', *, *, #245953, .F. ) ;
#171848 = FACE_OUTER_BOUND ( 'NONE', #32917, .T. ) ;
#171849 = CARTESIAN_POINT ( 'NONE',  ( -16.93255653858138388, 9.998451453988312920, -46.08164336798968463 ) ) ;
#171851 = ADVANCED_FACE ( 'NONE', ( #226968 ), #187864, .F. ) ;
#171850 = CARTESIAN_POINT ( 'NONE',  ( -21.05000000000000071, 76.10000000001274145, -210.0637644362255969 ) ) ;
#171852 = EDGE_CURVE ( 'NONE', #109261, #144129, #31376, .T. ) ;
#171853 = DIRECTION ( 'NONE',  ( 0.000000000000000000, -0.4721928772777346239, -0.8814952561688430555 ) ) ;
#171854 = DIRECTION ( 'NONE',  ( 0.000000000000000000, 0.2617529984165152257, 0.9651348961777124202 ) ) ;
#171855 = ORIENTED_EDGE ( 'NONE', *, *, #11081, .T. ) ;
#171856 = ORIENTED_EDGE ( 'NONE', *, *, #152153, .T. ) ;
#171857 = EDGE_CURVE ( 'NONE', #77148, #219131, #148729, .T. ) ;
#171858 = AXIS2_PLACEMENT_3D ( 'NONE', #13143, #69269, #92660 ) ;
#171859 = CARTESIAN_POINT ( 'NONE',  ( -18.59999999999999787, 77.26327546522911405, -95.12124281777788326 ) ) ;
#171860 = ORIENTED_EDGE ( 'NONE', *, *, #147284, .T. ) ;
#171861 = FACE_OUTER_BOUND ( 'NONE', #101443, .T. ) ;
#171862 = CARTESIAN_POINT ( 'NONE',  ( 22.39999999999999858, 76.00000000001267608, -203.5231074845243597 ) ) ;
#171863 = ORIENTED_EDGE ( 'NONE', *, *, #53047, .F. ) ;
#171864 = DIRECTION ( 'NONE',  ( 0.000000000000000000, 0.8660254037844420383, -0.4999999999999943379 ) ) ;
#171865 = CARTESIAN_POINT ( 'NONE',  ( 20.84999999999999432, 7.675662554762638479, -241.7139905447625381 ) ) ;
#171866 = CARTESIAN_POINT ( 'NONE',  ( -22.48970261584618058, 64.35000000001166143, -69.57847697274181087 ) ) ;
#171867 = LINE ( 'NONE', #130122, #9240 ) ;
#171868 = EDGE_LOOP ( 'NONE', ( #18131, #80379, #30121, #189823 ) ) ;
#171869 = DIRECTION ( 'NONE',  ( 0.000000000000000000, 0.2818822000686317941, -0.9594490217226071538 ) ) ;
#171870 = LINE ( 'NONE', #200057, #41705 ) ;
#171871 = DIRECTION ( 'NONE',  ( 0.000000000000000000, -6.467318590049456648E-15, 1.000000000000000000 ) ) ;
#171872 = CARTESIAN_POINT ( 'NONE',  ( 23.14999999999999503, 64.35000000001254250, -182.1731074845244507 ) ) ;
#171873 = DIRECTION ( 'NONE',  ( 0.000000000000000000, 0.000000000000000000, -1.000000000000000000 ) ) ;
#171874 = LINE ( 'NONE', #250093, #119829 ) ;
#171876 = EDGE_LOOP ( 'NONE', ( #231558, #80512, #201802, #144101, #190798, #230891, #88849 ) ) ;
#171875 = CIRCLE ( 'NONE', #134217, 11.75000000000001066 ) ;
#171877 = CARTESIAN_POINT ( 'NONE',  ( 21.04116576186320486, 10.62466307875135563, -12.32858176862772126 ) ) ;
#171878 = EDGE_LOOP ( 'NONE', ( #231089, #239643, #52123, #232414 ) ) ;
#171879 = ADVANCED_FACE ( 'NONE', ( #165733 ), #71768, .T. ) ;
#171880 = DIRECTION ( 'NONE',  ( 0.000000000000000000, 0.9126074666062508056, 0.4088369013366094928 ) ) ;
#171881 = EDGE_CURVE ( 'NONE', #197319, #78569, #198384, .T. ) ;
#171882 = DIRECTION ( 'NONE',  ( -1.000000000000000000, -1.186688945009010077E-16, -0.000000000000000000 ) ) ;
#171883 = CARTESIAN_POINT ( 'NONE',  ( 23.40000000000005542, 77.73640333653723644, -47.54092689884382850 ) ) ;
#171884 = LINE ( 'NONE', #248827, #184060 ) ;
#171885 = DIRECTION ( 'NONE',  ( 0.000000000000000000, -1.000000000000000000, 0.000000000000000000 ) ) ;
#171886 = ORIENTED_EDGE ( 'NONE', *, *, #198514, .F. ) ;
#171887 = CARTESIAN_POINT ( 'NONE',  ( -16.94309007106720344, 66.00777380744206368, -123.9173162019688732 ) ) ;
#171888 = CARTESIAN_POINT ( 'NONE',  ( -16.89268316805465986, 66.04827818676963602, -82.16735500597883401 ) ) ;
#171889 = CARTESIAN_POINT ( 'NONE',  ( 21.93340585971088785, 10.58724339642392032, -227.2765004563024434 ) ) ;
#171890 = LINE ( 'NONE', #251381, #108835 ) ;
#171891 = EDGE_CURVE ( 'NONE', #109039, #215142, #152602, .T. ) ;
#171892 = AXIS2_PLACEMENT_3D ( 'NONE', #215778, #37182, #116694 ) ;
#171893 = CARTESIAN_POINT ( 'NONE',  ( 23.14999999999999503, 11.65000000001116298, -121.8500000000000369 ) ) ;
#171894 = VERTEX_POINT ( 'NONE', #198108 ) ;
#171895 = ORIENTED_EDGE ( 'NONE', *, *, #160624, .F. ) ;
#171896 = CARTESIAN_POINT ( 'NONE',  ( -21.14999999999994174, 82.64476912853859858, -26.37791261425322986 ) ) ;
#171898 = FACE_OUTER_BOUND ( 'NONE', #187304, .T. ) ;
#171897 = AXIS2_PLACEMENT_3D ( 'NONE', #72729, #130091, #208379 ) ;
#171899 = CARTESIAN_POINT ( 'NONE',  ( -18.60000000000000853, -9.364240527579751117, -107.6802485818408002 ) ) ;
#171900 = PLANE ( 'NONE',  #1435 ) ;
#171901 = DIRECTION ( 'NONE',  ( 0.000000000000000000, 0.000000000000000000, 1.000000000000000000 ) ) ;
#171902 = ORIENTED_EDGE ( 'NONE', *, *, #171466, .T. ) ;
#171903 = CARTESIAN_POINT ( 'NONE',  ( 23.14999999999998437, 3.957237024351080823, -200.1381559693347754 ) ) ;
#171904 = ITEM_DEFINED_TRANSFORMATION ( 'NONE', 'NONE', #206804,  #2425 ) ;
#171905 = DIRECTION ( 'NONE',  ( -1.000000000000000000, -0.000000000000000000, -0.000000000000000000 ) ) ;
#171906 = CIRCLE ( 'NONE', #63512, 11.75000000000000000 ) ;
#171907 = ORIENTED_EDGE ( 'NONE', *, *, #182099, .F. ) ;
#171908 = AXIS2_PLACEMENT_3D ( 'NONE', #61021, #97559, #174623 ) ;
#171909 = CARTESIAN_POINT ( 'NONE',  ( -20.54999999999999716, 84.66355140188105111, -93.49900636645693908 ) ) ;
#171910 = EDGE_CURVE ( 'NONE', #160136, #233017, #135554, .T. ) ;
#171911 = ORIENTED_EDGE ( 'NONE', *, *, #165608, .F. ) ;
#171913 = ORIENTED_EDGE ( 'NONE', *, *, #109488, .F. ) ;
#171912 = CARTESIAN_POINT ( 'NONE',  ( -20.64999999999999858, 1.115625160336667635E-11, -136.0000000000000284 ) ) ;
#171914 = AXIS2_PLACEMENT_3D ( 'NONE', #88547, #166861, #203391 ) ;
#171915 = EDGE_CURVE ( 'NONE', #193539, #254970, #60806, .T. ) ;
#171916 = ORIENTED_EDGE ( 'NONE', *, *, #41030, .T. ) ;
#171917 = DIRECTION ( 'NONE',  ( 1.000000000000000000, 0.000000000000000000, 0.000000000000000000 ) ) ;
#171918 = DIRECTION ( 'NONE',  ( -2.602085213965226419E-14, 0.2128009952263604232, -0.9770955615653316162 ) ) ;
#171919 = CARTESIAN_POINT ( 'NONE',  ( 21.14999999999999858, 11.65000000001115943, -167.5999999999999659 ) ) ;
#171920 = DIRECTION ( 'NONE',  ( 0.000000000000000000, -0.9976611540403004241, -0.06835365183350541884 ) ) ;
#171922 = AXIS2_PLACEMENT_3D ( 'NONE', #184659, #6015, #26911 ) ;
#171921 = DIRECTION ( 'NONE',  ( 0.000000000000000000, 0.000000000000000000, 1.000000000000000000 ) ) ;
#171923 = EDGE_CURVE ( 'NONE', #148712, #115637, #152810, .T. ) ;
#171925 = DIRECTION ( 'NONE',  ( 0.000000000000000000, 0.8660254037844378194, 0.5000000000000016653 ) ) ;
#171924 = AXIS2_PLACEMENT_3D ( 'NONE', #167823, #206921, #69998 ) ;
#171926 = AXIS2_PLACEMENT_3D ( 'NONE', #154299, #233796, #2856 ) ;
#171927 = CARTESIAN_POINT ( 'NONE',  ( -16.77683809663752257, 23.65833333334447985, -150.7500000000000284 ) ) ;
#171930 = CARTESIAN_POINT ( 'NONE',  ( -16.87036670365549895, 65.91505003675629837, -56.97310748452439810 ) ) ;
#171929 = AXIS2_PLACEMENT_3D ( 'NONE', #131340, #50497, #230448 ) ;
#171928 = DIRECTION ( 'NONE',  ( 0.000000000000000000, 0.1350103645451807555, 0.9908441862701609093 ) ) ;
#171931 = CARTESIAN_POINT ( 'NONE',  ( 21.05000000000000426, -1.358660982773625348, -194.8406220977909982 ) ) ;
#171932 = EDGE_CURVE ( 'NONE', #145382, #197944, #15657, .T. ) ;
#171933 = LINE ( 'NONE', #194044, #85364 ) ;
#171934 = DIRECTION ( 'NONE',  ( -1.000000000000000000, -0.000000000000000000, -0.000000000000000000 ) ) ;
#171935 = CARTESIAN_POINT ( 'NONE',  ( 20.95496329884391784, 18.79541830518007473, -227.9940942717060466 ) ) ;
#171936 = VERTEX_POINT ( 'NONE', #136847 ) ;
#171937 = CARTESIAN_POINT ( 'NONE',  ( -20.96428641294214046, 11.75000000001149481, -93.67489317794102988 ) ) ;
#171938 = CARTESIAN_POINT ( 'NONE',  ( 18.50000000000000000, -10.35479209691423996, -194.7565409830737337 ) ) ;
#171939 = DIRECTION ( 'NONE',  ( -0.000000000000000000, -6.982962677686266711E-15, 1.000000000000000000 ) ) ;
#171940 = EDGE_CURVE ( 'NONE', #7325, #12615, #40393, .T. ) ;
#171942 = ADVANCED_FACE ( 'NONE', ( #237243 ), #31989, .F. ) ;
#171941 = EDGE_CURVE ( 'NONE', #250193, #21068, #157756, .T. ) ;
#171943 = DIRECTION ( 'NONE',  ( -1.000000000000000000, -0.000000000000000000, -0.000000000000000000 ) ) ;
#171944 = FACE_OUTER_BOUND ( 'NONE', #228802, .T. ) ;
#171945 = CARTESIAN_POINT ( 'NONE',  ( 21.14999999999999858, 1.115600667400684642E-11, -55.35042919245524473 ) ) ;
#171946 = VERTEX_POINT ( 'NONE', #76869 ) ;
#171947 = VERTEX_POINT ( 'NONE', #36500 ) ;
#171948 = DIRECTION ( 'NONE',  ( 1.000000000000000000, 0.000000000000000000, 0.000000000000000000 ) ) ;
#171949 = ORIENTED_EDGE ( 'NONE', *, *, #156392, .F. ) ;
#171950 = DIRECTION ( 'NONE',  ( -1.000000000000000000, -0.000000000000000000, -0.000000000000000000 ) ) ;
#171951 = LINE ( 'NONE', #53248, #180576 ) ;
#171952 = AXIS2_PLACEMENT_3D ( 'NONE', #137291, #100705, #198554 ) ;
#171953 = ADVANCED_FACE ( 'NONE', ( #116024 ), #169389, .F. ) ;
#171954 = EDGE_CURVE ( 'NONE', #217616, #86618, #156458, .T. ) ;
#171955 = ORIENTED_EDGE ( 'NONE', *, *, #249252, .T. ) ;
#171956 = CYLINDRICAL_SURFACE ( 'NONE', #1882, 0.09999999999999939493 ) ;
#171957 = ADVANCED_FACE ( 'NONE', ( #93871 ), #106790, .T. ) ;
#171958 = CIRCLE ( 'NONE', #205218, 12.97499999999999964 ) ;
#171959 = ORIENTED_EDGE ( 'NONE', *, *, #80175, .T. ) ;
#171960 = FACE_OUTER_BOUND ( 'NONE', #153794, .T. ) ;
#171961 = LINE ( 'NONE', #126374, #199380 ) ;
#171963 = VECTOR ( 'NONE', #38421, 1000.000000000000000 ) ;
#171962 = CARTESIAN_POINT ( 'NONE',  ( 22.39999999999999858, 29.50811709945092076, -252.6450601445781103 ) ) ;
#171964 = FACE_OUTER_BOUND ( 'NONE', #197747, .T. ) ;
#171965 = LINE ( 'NONE', #113227, #22466 ) ;
#171966 = EDGE_CURVE ( 'NONE', #152492, #39190, #173500, .T. ) ;
#171967 = CARTESIAN_POINT ( 'NONE',  ( -21.53699400384661899, 1.514529946271319711E-11, -60.21228820675978000 ) ) ;
#171968 = TOROIDAL_SURFACE ( 'NONE', #238370, 0.2000000000000000111, 0.1000000000000000056 ) ;
#171969 = CYLINDRICAL_SURFACE ( 'NONE', #250884, 0.1000000000000048767 ) ;
#171971 = CARTESIAN_POINT ( 'NONE',  ( -18.59999999999999787, 0.4879293624014888198, -209.1697915983179428 ) ) ;
#171970 = TOROIDAL_SURFACE ( 'NONE', #59447, 11.90000000000000391, 0.1000000000000000056 ) ;
#171974 = ORIENTED_EDGE ( 'NONE', *, *, #44023, .F. ) ;
#171973 = EDGE_CURVE ( 'NONE', #236786, #295, #216383, .T. ) ;
#171972 = CARTESIAN_POINT ( 'NONE',  ( -18.59999999999999787, 9.150000000011157653, -55.25000000000004974 ) ) ;
#171976 = DIRECTION ( 'NONE',  ( 1.000000000000000000, 0.000000000000000000, 0.000000000000000000 ) ) ;
#171975 = CARTESIAN_POINT ( 'NONE',  ( 18.59999999999999076, 2.923777413779048207, -208.5507632484912222 ) ) ;
#171977 = ORIENTED_EDGE ( 'NONE', *, *, #111082, .F. ) ;
#171979 = ORIENTED_EDGE ( 'NONE', *, *, #233220, .F. ) ;
#171978 = SURFACE_SIDE_STYLE ('',( #110676 ) ) ;
#171980 = EDGE_LOOP ( 'NONE', ( #107869, #18740, #71786, #96250 ) ) ;
#171981 = CARTESIAN_POINT ( 'NONE',  ( 20.27550659511088682, 66.78395627750303731, -93.77310748452437394 ) ) ;
#171982 = DIRECTION ( 'NONE',  ( -1.000000000000000000, 0.000000000000000000, 0.000000000000000000 ) ) ;
#171983 = VECTOR ( 'NONE', #144347, 1000.000000000000000 ) ;
#171984 = CARTESIAN_POINT ( 'NONE',  ( -17.11825945287482753, 23.11343627288707481, -230.8941331732335129 ) ) ;
#171985 = CARTESIAN_POINT ( 'NONE',  ( 18.41789779300683705, -9.500000000000000000, -7.032069666360214022 ) ) ;
#171986 = CARTESIAN_POINT ( 'NONE',  ( 18.54999999999999716, 8.750000000000024869, -9.250000000000001776 ) ) ;
#171987 = ADVANCED_FACE ( 'NONE', ( #74352 ), #92577, .T. ) ;
#171988 = DIRECTION ( 'NONE',  ( 0.000000000000000000, 0.3994087351226822125, 0.9167729611565227366 ) ) ;
#171989 = CIRCLE ( 'NONE', #59467, 0.09999999999999939493 ) ;
#171990 = CARTESIAN_POINT ( 'NONE',  ( -17.73285935859659190, 12.78867406748397073, -208.6962744657041924 ) ) ;
#171991 = VECTOR ( 'NONE', #215144, 1000.000000000000000 ) ;
#171992 = CARTESIAN_POINT ( 'NONE',  ( -20.94999999999999929, 74.16465844978819177, -191.9679561919613775 ) ) ;
#171993 = EDGE_CURVE ( 'NONE', #76541, #138896, #185901, .T. ) ;
#171994 = CIRCLE ( 'NONE', #59477, 14.30833333333334956 ) ;
#171995 = VERTEX_POINT ( 'NONE', #95160 ) ;
#171996 = ORIENTED_EDGE ( 'NONE', *, *, #64293, .F. ) ;
#171997 = LINE ( 'NONE', #126400, #118775 ) ;
#171998 = ORIENTED_EDGE ( 'NONE', *, *, #186038, .T. ) ;
#171999 = LINE ( 'NONE', #228090, #38424 ) ;
#172000 = ORIENTED_EDGE ( 'NONE', *, *, #48346, .F. ) ;
#172002 = CIRCLE ( 'NONE', #51118, 0.1000000000000028644 ) ;
#172001 = LINE ( 'NONE', #94977, #30247 ) ;
#172003 = VECTOR ( 'NONE', #246906, 1000.000000000000000 ) ;
#172004 = AXIS2_PLACEMENT_3D ( 'NONE', #69360, #68057, #207588 ) ;
#172005 = CIRCLE ( 'NONE', #213652, 0.9750000000000036415 ) ;
#172006 = CYLINDRICAL_SURFACE ( 'NONE', #109379, 0.1000000000000028644 ) ;
#172007 = CYLINDRICAL_SURFACE ( 'NONE', #22765, 0.1000000000000101918 ) ;
#172008 = ADVANCED_FACE ( 'NONE', ( #73073 ), #114728, .F. ) ;
#172009 = DIRECTION ( 'NONE',  ( -1.000000000000000000, -0.000000000000000000, -0.000000000000000000 ) ) ;
#172010 = ORIENTED_EDGE ( 'NONE', *, *, #75132, .T. ) ;
#172011 = CARTESIAN_POINT ( 'NONE',  ( -18.46154800491014569, -9.480206274230836172, -207.6574508383814361 ) ) ;
#172012 = FACE_OUTER_BOUND ( 'NONE', #28328, .T. ) ;
#172013 = FACE_OUTER_BOUND ( 'NONE', #3789, .T. ) ;
#172014 = CARTESIAN_POINT ( 'NONE',  ( 18.49999999999999645, 5.699452464332751767, -20.95772604343016710 ) ) ;
#172015 = EDGE_LOOP ( 'NONE', ( #188704, #242500, #77863, #249617 ) ) ;
#172017 = CARTESIAN_POINT ( 'NONE',  ( -18.49372193242234275, 85.44248452336948674, -29.25832622448972842 ) ) ;
#172016 = CARTESIAN_POINT ( 'NONE',  ( 12.25000000000000000, 66.15000000001185754, -86.27310748452437394 ) ) ;
#172018 = AXIS2_PLACEMENT_3D ( 'NONE', #67752, #145994, #85994 ) ;
#172019 = ORIENTED_EDGE ( 'NONE', *, *, #169515, .T. ) ;
#172022 = VERTEX_POINT ( 'NONE', #242363 ) ;
#172021 = CARTESIAN_POINT ( 'NONE',  ( -18.40000000000000213, 64.51332499825430489, -112.2731074845243739 ) ) ;
#172020 = DIRECTION ( 'NONE',  ( 1.000000000000000000, 0.000000000000000000, 0.000000000000000000 ) ) ;
#172023 = DIRECTION ( 'NONE',  ( 0.000000000000000000, -0.8068669527897506244, -0.5907332058516622242 ) ) ;
#172024 = VECTOR ( 'NONE', #216269, 1000.000000000000000 ) ;
#172025 = CARTESIAN_POINT ( 'NONE',  ( -22.50000000000000000, 1.115600667400684642E-11, -100.4000000000000341 ) ) ;
#172026 = ORIENTED_EDGE ( 'NONE', *, *, #164431, .T. ) ;
#172027 = CARTESIAN_POINT ( 'NONE',  ( 23.14999999999999858, 70.88170441948386724, -234.2197789011331679 ) ) ;
#172029 = CARTESIAN_POINT ( 'NONE',  ( -20.94999999999999929, 70.15000000001163016, -59.39061026024639744 ) ) ;
#172028 =( BOUNDED_SURFACE ( )  B_SPLINE_SURFACE ( 3, 2, ( 
 ( #144224, #47695, #145517 ),
 ( #106378, #127251, #42573 ),
 ( #242053, #124690, #85515 ),
 ( #105074, #24320, #162547 ) ),
 .UNSPECIFIED., .F., .F., .F. ) 
 B_SPLINE_SURFACE_WITH_KNOTS ( ( 4, 4 ),
 ( 3, 3 ),
 ( 0.04058434257139475337, 0.04256401539001600232 ),
 ( 0.000000000000000000, 1.000000000000000000 ),
 .UNSPECIFIED. ) 
 GEOMETRIC_REPRESENTATION_ITEM ( )  RATIONAL_B_SPLINE_SURFACE ( (
 ( 1.000000000000000000, 0.7103081912008297749, 1.000000000000000000),
 ( 1.000000000000000000, 0.7104998333555460066, 1.000000000000000000),
 ( 1.000000000000000000, 0.7107238315755025626, 1.000000000000000000),
 ( 1.000000000000000000, 0.7110073749539292942, 1.000000000000000000) ) ) 
 REPRESENTATION_ITEM ( '' )  SURFACE ( )  );
#172030 = DIRECTION ( 'NONE',  ( 0.000000000000000000, 0.000000000000000000, -1.000000000000000000 ) ) ;
#172032 = ORIENTED_EDGE ( 'NONE', *, *, #257492, .F. ) ;
#172031 = CARTESIAN_POINT ( 'NONE',  ( -21.05000000000000071, -1.261786168565025568, -8.086498963545480478 ) ) ;
#172033 = ORIENTED_EDGE ( 'NONE', *, *, #15350, .F. ) ;
#172034 = DIRECTION ( 'NONE',  ( 0.000000000000000000, -6.938893903907222067E-15, 1.000000000000000000 ) ) ;
#172036 = CARTESIAN_POINT ( 'NONE',  ( 18.46082813848004989, -9.480749650896276748, -74.08437010271569534 ) ) ;
#172035 = VECTOR ( 'NONE', #238824, 1000.000000000000000 ) ;
#172037 = FACE_OUTER_BOUND ( 'NONE', #185709, .T. ) ;
#172038 = CARTESIAN_POINT ( 'NONE',  ( -23.15000000000000213, -11.64999999998884483, -167.4999999999999432 ) ) ;
#172039 = ORIENTED_EDGE ( 'NONE', *, *, #44478, .F. ) ;
#172040 = CARTESIAN_POINT ( 'NONE',  ( 18.50000000000000000, -9.499999999988842703, -40.53206939669966857 ) ) ;
#172041 = AXIS2_PLACEMENT_3D ( 'NONE', #151742, #112594, #187009 ) ;
#172042 = CARTESIAN_POINT ( 'NONE',  ( -20.64999999999999858, 76.00000000001212186, -134.5231074845243313 ) ) ;
#172043 = FACE_OUTER_BOUND ( 'NONE', #30301, .T. ) ;
#172044 = ORIENTED_EDGE ( 'NONE', *, *, #248985, .F. ) ;
#172045 = FACE_OUTER_BOUND ( 'NONE', #4088, .T. ) ;
#172046 = DIRECTION ( 'NONE',  ( -1.000000000000000000, -0.000000000000000000, -0.000000000000000000 ) ) ;
#172047 = ADVANCED_FACE ( 'NONE', ( #218947 ), #121181, .T. ) ;
#172048 = VERTEX_POINT ( 'NONE', #203243 ) ;
#172049 = CARTESIAN_POINT ( 'NONE',  ( 23.14999999999999858, 1.115600667400684642E-11, -167.4999999999999716 ) ) ;
#172050 = LINE ( 'NONE', #129042, #139672 ) ;
#172052 = ORIENTED_EDGE ( 'NONE', *, *, #256188, .F. ) ;
#172051 = AXIS2_PLACEMENT_3D ( 'NONE', #236353, #35622, #56411 ) ;
#172053 = EDGE_LOOP ( 'NONE', ( #188046, #146820, #2230, #65563 ) ) ;
#172054 = DIRECTION ( 'NONE',  ( 0.000000000000000000, -0.8660254037844387076, 0.4999999999999998335 ) ) ;
#172055 = EDGE_LOOP ( 'NONE', ( #147277, #80546, #189854, #30256 ) ) ;
#172057 = ORIENTED_EDGE ( 'NONE', *, *, #139444, .T. ) ;
#172056 = DIRECTION ( 'NONE',  ( 0.000000000000000000, 0.5000000000000128786, 0.8660254037844311581 ) ) ;
#172058 = ORIENTED_EDGE ( 'NONE', *, *, #152170, .F. ) ;
#172059 = EDGE_CURVE ( 'NONE', #172794, #202854, #241112, .T. ) ;
#172060 = ADVANCED_FACE ( 'NONE', ( #159017 ), #141979, .F. ) ;
#172063 = ORIENTED_EDGE ( 'NONE', *, *, #153945, .T. ) ;
#172062 = ORIENTED_EDGE ( 'NONE', *, *, #208725, .T. ) ;
#172061 = CARTESIAN_POINT ( 'NONE',  ( 23.14999999999999503, 61.95000000001175522, -75.03680255528533394 ) ) ;
#172064 = CYLINDRICAL_SURFACE ( 'NONE', #10734, 7.899999999999990585 ) ;
#172065 = AXIS2_PLACEMENT_3D ( 'NONE', #146515, #143956, #147834 ) ;
#172066 = ORIENTED_EDGE ( 'NONE', *, *, #155300, .T. ) ;
#172067 = DIRECTION ( 'NONE',  ( 0.000000000000000000, 0.000000000000000000, -1.000000000000000000 ) ) ;
#172068 = CARTESIAN_POINT ( 'NONE',  ( 20.95512820512820440, 8.876151316299271343, -109.0586289951409924 ) ) ;
#172069 = CARTESIAN_POINT ( 'NONE',  ( -18.50000000000000000, -1.162701749926853712, -108.6000000000000227 ) ) ;
#172070 = CIRCLE ( 'NONE', #67794, 0.09999999999999939493 ) ;
#172071 = DIRECTION ( 'NONE',  ( -1.000000000000000000, 0.000000000000000000, 0.000000000000000000 ) ) ;
#172072 = FACE_OUTER_BOUND ( 'NONE', #89179, .T. ) ;
#172073 = ORIENTED_EDGE ( 'NONE', *, *, #107725, .F. ) ;
#172074 = ORIENTED_EDGE ( 'NONE', *, *, #76590, .F. ) ;
#172075 = ORIENTED_EDGE ( 'NONE', *, *, #127272, .F. ) ;
#172076 = AXIS2_PLACEMENT_3D ( 'NONE', #222442, #103782, #60817 ) ;
#172077 = EDGE_CURVE ( 'NONE', #191947, #229077, #15232, .T. ) ;
#172078 = CARTESIAN_POINT ( 'NONE',  ( -20.94999999999999929, 1.115600667400684642E-11, -196.9999999999999432 ) ) ;
#172081 = VERTEX_POINT ( 'NONE', #221504 ) ;
#172080 = EDGE_CURVE ( 'NONE', #203380, #182530, #157155, .T. ) ;
#172079 = CARTESIAN_POINT ( 'NONE',  ( -16.94132844910799918, 66.00756324483221249, -182.6269057285421411 ) ) ;
#172082 = DIRECTION ( 'NONE',  ( 0.000000000000000000, 1.000000000000000000, 6.853228547068871147E-15 ) ) ;
#172084 = ORIENTED_EDGE ( 'NONE', *, *, #142953, .T. ) ;
#172083 = CARTESIAN_POINT ( 'NONE',  ( -18.50000000000000000, 77.36242903720497566, -61.63422623660309796 ) ) ;
#172085 = ORIENTED_EDGE ( 'NONE', *, *, #153694, .F. ) ;
#172086 = DIRECTION ( 'NONE',  ( 0.000000000000000000, -6.982962677686266711E-15, 1.000000000000000000 ) ) ;
#172087 = EDGE_CURVE ( 'NONE', #242008, #112934, #48535, .T. ) ;
#172088 = AXIS2_PLACEMENT_3D ( 'NONE', #92527, #73017, #152551 ) ;
#172089 = AXIS2_PLACEMENT_3D ( 'NONE', #204072, #63279, #103669 ) ;
#172090 = ORIENTED_EDGE ( 'NONE', *, *, #27430, .T. ) ;
#172091 = AXIS2_PLACEMENT_3D ( 'NONE', #39797, #75067, #196261 ) ;
#172092 = EDGE_CURVE ( 'NONE', #246033, #173624, #211045, .T. ) ;
#172093 = CARTESIAN_POINT ( 'NONE',  ( -21.55000000000000426, 65.32753222054176945, -213.4247798787853867 ) ) ;
#172094 = DIRECTION ( 'NONE',  ( 1.000000000000000000, 0.000000000000000000, 0.000000000000000000 ) ) ;
#172096 = ORIENTED_EDGE ( 'NONE', *, *, #146283, .T. ) ;
#172095 = VERTEX_POINT ( 'NONE', #200688 ) ;
#172097 = VERTEX_POINT ( 'NONE', #123718 ) ;
#172098 = DIRECTION ( 'NONE',  ( 0.000000000000000000, -1.000000000000000000, 0.000000000000000000 ) ) ;
#172100 = ORIENTED_EDGE ( 'NONE', *, *, #224797, .F. ) ;
#172099 = EDGE_CURVE ( 'NONE', #243260, #86736, #94317, .T. ) ;
#172101 = ORIENTED_EDGE ( 'NONE', *, *, #141432, .T. ) ;
#172103 = CYLINDRICAL_SURFACE ( 'NONE', #26011, 0.09999999999999892308 ) ;
#172102 = VECTOR ( 'NONE', #68841, 1000.000000000000000 ) ;
#172105 = VERTEX_POINT ( 'NONE', #161576 ) ;
#172104 = CARTESIAN_POINT ( 'NONE',  ( -20.64999999999999858, 1.925233644859811521, -20.76975646687386501 ) ) ;
#172106 = CARTESIAN_POINT ( 'NONE',  ( -18.69999999999999929, -1.410778198689824459, -7.973296578895943121 ) ) ;
#172108 = DIRECTION ( 'NONE',  ( 1.000000000000000000, 0.000000000000000000, 0.000000000000000000 ) ) ;
#172107 = DIRECTION ( 'NONE',  ( 0.000000000000000000, 0.9698110461157734008, 0.2438576117980102709 ) ) ;
#172109 = DIRECTION ( 'NONE',  ( 0.000000000000000000, -0.9550021345545507412, 0.2965989261549202838 ) ) ;
#172110 = DIRECTION ( 'NONE',  ( -0.7071067811865457964, -0.2890913453342138228, 0.6453109281988466117 ) ) ;
#172111 = VERTEX_POINT ( 'NONE', #5015 ) ;
#172112 = AXIS2_PLACEMENT_3D ( 'NONE', #87801, #206491, #108677 ) ;
#172113 = VECTOR ( 'NONE', #245433, 1000.000000000000000 ) ;
#172114 = AXIS2_PLACEMENT_3D ( 'NONE', #224169, #144625, #238608 ) ;
#172116 = EDGE_CURVE ( 'NONE', #38660, #209135, #81813, .T. ) ;
#172115 = ORIENTED_EDGE ( 'NONE', *, *, #183615, .F. ) ;
#172118 = AXIS2_PLACEMENT_3D ( 'NONE', #177962, #116683, #196219 ) ;
#172117 = CARTESIAN_POINT ( 'NONE',  ( 18.58725287972292506, 85.56662691070332016, -96.20060267875838633 ) ) ;
#172119 = FACE_OUTER_BOUND ( 'NONE', #254346, .T. ) ;
#172120 = DIRECTION ( 'NONE',  ( 2.952720810173289112E-16, 1.000000000000000000, 1.261617073437673512E-14 ) ) ;
#172121 = ORIENTED_EDGE ( 'NONE', *, *, #218099, .T. ) ;
#172122 = DIRECTION ( 'NONE',  ( 0.000000000000000000, 1.000000000000000000, 0.000000000000000000 ) ) ;
#172123 = CARTESIAN_POINT ( 'NONE',  ( 21.05000000000000071, 76.00000000001165290, -69.52310748452431710 ) ) ;
#172124 = DIRECTION ( 'NONE',  ( 1.000000000000000000, -0.000000000000000000, -0.000000000000000000 ) ) ;
#172125 = ORIENTED_EDGE ( 'NONE', *, *, #141473, .T. ) ;
#172126 = ORIENTED_EDGE ( 'NONE', *, *, #91758, .T. ) ;
#172127 =( BOUNDED_CURVE ( )  B_SPLINE_CURVE ( 3, ( #59392, #239357, #218480, #123260 ),
 .UNSPECIFIED., .F., .T. ) 
 B_SPLINE_CURVE_WITH_KNOTS ( ( 4, 4 ),
 ( 5.731445031868799056, 5.983100554402348337 ),
 .UNSPECIFIED. ) 
 CURVE ( )  GEOMETRIC_REPRESENTATION_ITEM ( )  RATIONAL_B_SPLINE_CURVE ( ( 1.000000000000000000, 0.9947294176030464508, 0.9947294176030464508, 1.000000000000000000 ) ) 
 REPRESENTATION_ITEM ( '' )  );
#172128 = DIRECTION ( 'NONE',  ( 1.000000000000000000, -0.000000000000000000, 0.000000000000000000 ) ) ;
#172129 = DIRECTION ( 'NONE',  ( 0.000000000000000000, 0.000000000000000000, 1.000000000000000000 ) ) ;
#172130 = ORIENTED_EDGE ( 'NONE', *, *, #69153, .F. ) ;
#172131 = CARTESIAN_POINT ( 'NONE',  ( -20.85000000000000142, 77.73670573947940454, -91.50568489690056140 ) ) ;
#172132 = ORIENTED_EDGE ( 'NONE', *, *, #221548, .T. ) ;
#172133 = CARTESIAN_POINT ( 'NONE',  ( 18.43466021071414929, -9.494190690445382330, -140.6170615601278939 ) ) ;
#172134 = CARTESIAN_POINT ( 'NONE',  ( -17.78043020864320667, 10.85359211201683927, -144.3369508342798042 ) ) ;
#172136 = CARTESIAN_POINT ( 'NONE',  ( 23.24999999999999289, 52.81534179157632991, -244.1198638051726277 ) ) ;
#172135 = DIRECTION ( 'NONE',  ( 0.000000000000000000, -0.8660254037844377084, -0.5000000000000016653 ) ) ;
#172137 = CARTESIAN_POINT ( 'NONE',  ( -20.64999999999999858, 68.75000000001185185, -90.67310748452436542 ) ) ;
#172138 = DIRECTION ( 'NONE',  ( 1.000000000000000000, 0.000000000000000000, 0.000000000000000000 ) ) ;
#172139 = CARTESIAN_POINT ( 'NONE',  ( -20.64999999999999858, 76.00000000001170974, -69.52310748452431710 ) ) ;
#172140 = CIRCLE ( 'NONE', #59622, 4.049999999999995381 ) ;
#172141 = AXIS2_PLACEMENT_3D ( 'NONE', #59155, #3054, #239122 ) ;
#172143 = ORIENTED_EDGE ( 'NONE', *, *, #181352, .T. ) ;
#172142 = LINE ( 'NONE', #215072, #223287 ) ;
#172144 = EDGE_CURVE ( 'NONE', #118994, #153767, #7026, .T. ) ;
#172146 = ORIENTED_EDGE ( 'NONE', *, *, #135001, .T. ) ;
#172145 = ORIENTED_EDGE ( 'NONE', *, *, #253073, .T. ) ;
#172147 = ORIENTED_EDGE ( 'NONE', *, *, #42418, .F. ) ;
#172148 = EDGE_CURVE ( 'NONE', #239427, #11679, #252527, .T. ) ;
#172149 = AXIS2_PLACEMENT_3D ( 'NONE', #86678, #188376, #123272 ) ;
#172150 = DIRECTION ( 'NONE',  ( -1.000000000000000000, -0.000000000000000000, 0.000000000000000000 ) ) ;
#172151 = CARTESIAN_POINT ( 'NONE',  ( -18.40000000000000213, 11.48667500176882861, -191.7499999999999716 ) ) ;
#172152 = EDGE_CURVE ( 'NONE', #90910, #26647, #160299, .T. ) ;
#172153 = ADVANCED_FACE ( 'NONE', ( #224077 ), #125005, .T. ) ;
#172155 = DIRECTION ( 'NONE',  ( 1.000000000000000000, -0.000000000000000000, -0.000000000000000000 ) ) ;
#172154 = CARTESIAN_POINT ( 'NONE',  ( -18.40000000000000213, 45.89348038176515843, -239.2231437130149061 ) ) ;
#172156 = CARTESIAN_POINT ( 'NONE',  ( -21.05000000000000071, 28.67750504931771616, -258.3094128005139396 ) ) ;
#172157 = ORIENTED_EDGE ( 'NONE', *, *, #114741, .F. ) ;
#172158 = VECTOR ( 'NONE', #20513, 999.9999999999998863 ) ;
#172159 = FACE_OUTER_BOUND ( 'NONE', #134383, .T. ) ;
#172160 = ORIENTED_EDGE ( 'NONE', *, *, #70962, .T. ) ;
#172161 = ORIENTED_EDGE ( 'NONE', *, *, #148768, .F. ) ;
#172162 = LINE ( 'NONE', #213809, #91823 ) ;
#172163 = VECTOR ( 'NONE', #129667, 1000.000000000000000 ) ;
#172164 = LINE ( 'NONE', #54732, #126602 ) ;
#172165 = EDGE_CURVE ( 'NONE', #256630, #164668, #138160, .T. ) ;
#172166 = CIRCLE ( 'NONE', #80484, 11.80000000000000426 ) ;
#172167 = TOROIDAL_SURFACE ( 'NONE', #59449, 0.2000000000000000111, 0.1000000000000000056 ) ;
#172168 = CYLINDRICAL_SURFACE ( 'NONE', #104180, 4.000000000000003553 ) ;
#172169 = EDGE_CURVE ( 'NONE', #215894, #27850, #42895, .T. ) ;
#172170 = EDGE_CURVE ( 'NONE', #42512, #186782, #19517, .T. ) ;
#172171 = CARTESIAN_POINT ( 'NONE',  ( -20.85000000000000142, 11.75000000001115197, -60.15839931010294350 ) ) ;
#172172 = AXIS2_PLACEMENT_3D ( 'NONE', #130296, #89882, #70367 ) ;
#172173 = DIRECTION ( 'NONE',  ( -0.000000000000000000, -0.9126074666063771490, -0.4088369013363281623 ) ) ;
#172174 = EDGE_LOOP ( 'NONE', ( #181611, #137225, #152945, #7634, #158444, #248984, #242398 ) ) ;
#172175 = ORIENTED_EDGE ( 'NONE', *, *, #14106, .F. ) ;
#172176 = FACE_OUTER_BOUND ( 'NONE', #215327, .T. ) ;
#172177 = CARTESIAN_POINT ( 'NONE',  ( 22.60000000000000142, 0.1008583691098682150, -88.75043287651064361 ) ) ;
#172178 = EDGE_CURVE ( 'NONE', #186373, #36582, #194317, .T. ) ;
#172179 = CYLINDRICAL_SURFACE ( 'NONE', #207067, 0.09999999999998898659 ) ;
#172180 = DIRECTION ( 'NONE',  ( 0.000000000000000000, -1.000000000000000000, 0.000000000000000000 ) ) ;
#172181 = DIRECTION ( 'NONE',  ( 0.000000000000000000, 1.000000000000000000, 0.000000000000000000 ) ) ;
#172183 = CIRCLE ( 'NONE', #163753, 0.1000000000000054040 ) ;
#172182 = DIRECTION ( 'NONE',  ( -1.000000000000000000, 0.000000000000000000, 0.000000000000000000 ) ) ;
#172184 = DIRECTION ( 'NONE',  ( 1.000000000000000000, 0.000000000000000000, 0.000000000000000000 ) ) ;
#172185 = FACE_OUTER_BOUND ( 'NONE', #85498, .T. ) ;
#172186 = VECTOR ( 'NONE', #52956, 1000.000000000000000 ) ;
#172187 = ADVANCED_FACE ( 'NONE', ( #190109 ), #89699, .F. ) ;
#172189 = CARTESIAN_POINT ( 'NONE',  ( -20.85000000000000142, 0.000000000000000000, -33.50000000000000000 ) ) ;
#172188 = CARTESIAN_POINT ( 'NONE',  ( -22.45372860728439690, 0.01492061954848863947, 11.64979713470387424 ) ) ;
#172190 = DIRECTION ( 'NONE',  ( -1.000000000000000000, -0.000000000000000000, -0.000000000000000000 ) ) ;
#172191 = FACE_BOUND ( 'NONE', #62740, .T. ) ;
#172192 = AXIS2_PLACEMENT_3D ( 'NONE', #216599, #37993, #21000 ) ;
#172193 = DIRECTION ( 'NONE',  ( 0.000000000000000000, 0.000000000000000000, 1.000000000000000000 ) ) ;
#172194 = CYLINDRICAL_SURFACE ( 'NONE', #256583, 0.1000000000000028644 ) ;
#172195 = EDGE_CURVE ( 'NONE', #233797, #177788, #165240, .T. ) ;
#172197 = ORIENTED_EDGE ( 'NONE', *, *, #64632, .T. ) ;
#172196 = CARTESIAN_POINT ( 'NONE',  ( 19.97071067811864609, 54.36283943849028333, -228.7769250045207912 ) ) ;
#172198 = VECTOR ( 'NONE', #81863, 1000.000000000000000 ) ;
#172199 = AXIS2_PLACEMENT_3D ( 'NONE', #67973, #113192, #14114 ) ;
#172200 = CIRCLE ( 'NONE', #159672, 0.09999999999999414912 ) ;
#172201 = EDGE_CURVE ( 'NONE', #208557, #33915, #135999, .T. ) ;
#172202 = AXIS2_PLACEMENT_3D ( 'NONE', #42616, #86854, #146832 ) ;
#172203 = CARTESIAN_POINT ( 'NONE',  ( -22.50000000000000000, 0.000000000000000000, 0.000000000000000000 ) ) ;
#172204 = EDGE_CURVE ( 'NONE', #90335, #113100, #85023, .T. ) ;
#172205 = EDGE_CURVE ( 'NONE', #73109, #84197, #246229, .T. ) ;
#172206 = CARTESIAN_POINT ( 'NONE',  ( -22.48660254037843487, 64.25000000001193712, -103.0731074845243711 ) ) ;
#172207 = CARTESIAN_POINT ( 'NONE',  ( -20.54999999999999716, 85.00000000001222134, -146.4170766071767389 ) ) ;
#172208 = CARTESIAN_POINT ( 'NONE',  ( 12.42718393586866732, 9.370655051134638924, -84.52582325598092439 ) ) ;
#172209 = DIRECTION ( 'NONE',  ( -1.000000000000000000, -0.000000000000000000, -0.000000000000000000 ) ) ;
#172210 = AXIS2_PLACEMENT_3D ( 'NONE', #137968, #197950, #3602 ) ;
#172211 = CIRCLE ( 'NONE', #163786, 0.1000000000000002554 ) ;
#172212 = AXIS2_PLACEMENT_3D ( 'NONE', #25737, #180966, #2299 ) ;
#172214 = DIRECTION ( 'NONE',  ( -0.000000000000000000, -0.8814952561688430555, 0.4721928772777346239 ) ) ;
#172213 = AXIS2_PLACEMENT_3D ( 'NONE', #42781, #122319, #201849 ) ;
#172215 = FACE_OUTER_BOUND ( 'NONE', #166702, .T. ) ;
#172216 = CARTESIAN_POINT ( 'NONE',  ( -16.89020380669786903, 66.05000000001157900, -56.76569633641382495 ) ) ;
#172217 = VERTEX_POINT ( 'NONE', #165413 ) ;
#172218 = CARTESIAN_POINT ( 'NONE',  ( 21.07928932188134397, 1.115600667400684642E-11, -33.50000000000000000 ) ) ;
#172220 = VERTEX_POINT ( 'NONE', #184966 ) ;
#172219 = CARTESIAN_POINT ( 'NONE',  ( 21.51976009735019346, 69.08954155835317579, -170.0231074845243882 ) ) ;
#172221 = CARTESIAN_POINT ( 'NONE',  ( 23.15000000000000213, -11.48912529306489816, -164.4000000000000057 ) ) ;
#172222 = DIRECTION ( 'NONE',  ( 1.000000000000000000, 0.000000000000000000, 0.000000000000000000 ) ) ;
#172223 = ORIENTED_EDGE ( 'NONE', *, *, #236360, .T. ) ;
#172224 = CARTESIAN_POINT ( 'NONE',  ( 19.90000000000000568, 1.350000000000000089, 16.60000000000000142 ) ) ;
#172225 = SHAPE_DEFINITION_REPRESENTATION ( #114014, #125202 ) ;
#172226 = DIRECTION ( 'NONE',  ( -0.000000000000000000, 1.000000000000000000, -0.000000000000000000 ) ) ;
#172227 = CARTESIAN_POINT ( 'NONE',  ( -21.05000000000000071, -11.48912529307605546, -30.39999999999999503 ) ) ;
#172228 = ORIENTED_EDGE ( 'NONE', *, *, #250710, .T. ) ;
#172229 = DIRECTION ( 'NONE',  ( 0.000000000000000000, 0.000000000000000000, -1.000000000000000000 ) ) ;
#172230 = DIRECTION ( 'NONE',  ( -1.000000000000000000, -0.000000000000000000, -0.000000000000000000 ) ) ;
#172231 = TOROIDAL_SURFACE ( 'NONE', #38920, 0.2000000000000000111, 0.1000000000000000056 ) ;
#172232 = CARTESIAN_POINT ( 'NONE',  ( -21.64999999999999858, 13.57274425111693539, -219.3827531532722048 ) ) ;
#172233 = ORIENTED_EDGE ( 'NONE', *, *, #202378, .T. ) ;
#172234 = ORIENTED_EDGE ( 'NONE', *, *, #234663, .T. ) ;
#172235 = DIRECTION ( 'NONE',  ( 1.000000000000000000, 0.000000000000000000, 0.000000000000000000 ) ) ;
#172236 = CARTESIAN_POINT ( 'NONE',  ( -20.94999999999999929, 4.898587196589411843E-16, -37.50000000000000000 ) ) ;
#172237 = DIRECTION ( 'NONE',  ( -0.000000000000000000, -0.000000000000000000, 1.000000000000000000 ) ) ;
#172238 = ADVANCED_FACE ( 'NONE', ( #127563 ), #69406, .F. ) ;
#172239 = CARTESIAN_POINT ( 'NONE',  ( -21.14999999999999858, 12.76524917372336709, -223.4223513401831553 ) ) ;
#172241 = DIRECTION ( 'NONE',  ( -0.000000000000000000, -0.1350103645451945777, 0.9908441862701590219 ) ) ;
#172240 = DIRECTION ( 'NONE',  ( -0.000000000000000000, -1.000000000000000000, -6.982962677686266711E-15 ) ) ;
#172242 = CARTESIAN_POINT ( 'NONE',  ( 21.05000000000000071, 76.00000000001213607, -136.5231074845243313 ) ) ;
#172243 = EDGE_CURVE ( 'NONE', #240530, #147657, #102670, .T. ) ;
#172244 = DIRECTION ( 'NONE',  ( 1.000000000000000000, 0.000000000000000000, 0.000000000000000000 ) ) ;
#172245 = FACE_OUTER_BOUND ( 'NONE', #196707, .T. ) ;
#172246 = ORIENTED_EDGE ( 'NONE', *, *, #55565, .T. ) ;
#172247 = AXIS2_PLACEMENT_3D ( 'NONE', #14458, #57386, #136941 ) ;
#172249 = VERTEX_POINT ( 'NONE', #170593 ) ;
#172248 = CARTESIAN_POINT ( 'NONE',  ( -22.50000000000000000, 0.000000000000000000, 6.249999999999998224 ) ) ;
#172250 = CARTESIAN_POINT ( 'NONE',  ( 20.12500000000000000, 9.750000000011153745, -88.15000000000004832 ) ) ;
#172251 = CARTESIAN_POINT ( 'NONE',  ( -21.07933241753356413, -1.255501372899540780, -194.7964368633462300 ) ) ;
#172254 = CARTESIAN_POINT ( 'NONE',  ( -20.94999999999999929, 1.115650877919449413E-11, -171.6000000000000227 ) ) ;
#172253 = DIRECTION ( 'NONE',  ( -0.000000000000000000, -6.982962677686266711E-15, 1.000000000000000000 ) ) ;
#172252 = AXIS2_PLACEMENT_3D ( 'NONE', #125888, #26834, #202865 ) ;
#172255 = EDGE_CURVE ( 'NONE', #51370, #205761, #67584, .T. ) ;
#172256 = ADVANCED_FACE ( 'NONE', ( #229241 ), #130117, .T. ) ;
#172257 = EDGE_LOOP ( 'NONE', ( #108912, #215931, #51180, #42193 ) ) ;
#172258 = DIRECTION ( 'NONE',  ( 0.000000000000000000, 0.000000000000000000, 1.000000000000000000 ) ) ;
#172259 = LINE ( 'NONE', #153982, #137325 ) ;
#172260 = CARTESIAN_POINT ( 'NONE',  ( 20.27550659511088682, 9.216043722520002035, -46.15000000000000568 ) ) ;
#172261 = CARTESIAN_POINT ( 'NONE',  ( 13.88638282980483929, 13.17763673189382523, -217.0637590370182011 ) ) ;
#172262 = VERTEX_POINT ( 'NONE', #25905 ) ;
#172263 = VERTEX_POINT ( 'NONE', #8899 ) ;
#172265 = CIRCLE ( 'NONE', #47108, 12.77500000000000391 ) ;
#172264 = DIRECTION ( 'NONE',  ( 0.000000000000000000, -0.6936040289657786628, -0.7203564749500342979 ) ) ;
#172266 = EDGE_LOOP ( 'NONE', ( #106529, #235611 ) ) ;
#172267 = CARTESIAN_POINT ( 'NONE',  ( 21.05000000000000071, 23.68770167995059239, -252.8127582590406348 ) ) ;
#172268 = AXIS2_PLACEMENT_3D ( 'NONE', #37272, #54234, #38541 ) ;
#172269 = DIRECTION ( 'NONE',  ( 0.000000000000000000, 0.000000000000000000, -1.000000000000000000 ) ) ;
#172270 = EDGE_CURVE ( 'NONE', #116826, #185664, #231905, .T. ) ;
#172272 = CARTESIAN_POINT ( 'NONE',  ( -21.13498764882296044, 65.52942838307841100, -242.1238406827027063 ) ) ;
#172271 = AXIS2_PLACEMENT_3D ( 'NONE', #53777, #132031, #211579 ) ;
#172273 = CIRCLE ( 'NONE', #126235, 0.1999999999999996503 ) ;
#172274 = VERTEX_POINT ( 'NONE', #88404 ) ;
#172275 = CARTESIAN_POINT ( 'NONE',  ( 20.94999999999999929, 36.18002604163306302, -236.0784499204090991 ) ) ;
#172276 = CARTESIAN_POINT ( 'NONE',  ( 18.59999999999998721, 19.85039924724470950, -35.78030305780136189 ) ) ;
#172277 = SPHERICAL_SURFACE ( 'NONE', #70215, 0.1000000000000000056 ) ;
#172278 = AXIS2_PLACEMENT_3D ( 'NONE', #130060, #186204, #167951 ) ;
#172280 = CARTESIAN_POINT ( 'NONE',  ( -21.05000000000000071, -1.162701749926853712, -41.60000000000000142 ) ) ;
#172279 = AXIS2_PLACEMENT_3D ( 'NONE', #428, #163383, #64274 ) ;
#172281 = DIRECTION ( 'NONE',  ( 0.000000000000000000, 0.8068669527897506244, 0.5907332058516622242 ) ) ;
#172282 = EDGE_CURVE ( 'NONE', #245381, #190040, #77930, .T. ) ;
#172285 = DIRECTION ( 'NONE',  ( 1.000000000000000000, 0.000000000000000000, 0.000000000000000000 ) ) ;
#172284 = AXIS2_PLACEMENT_3D ( 'NONE', #137269, #138532, #36937 ) ;
#172283 = DIRECTION ( 'NONE',  ( 0.000000000000000000, -0.5000000000000004441, -0.8660254037844384856 ) ) ;
#172286 = CARTESIAN_POINT ( 'NONE',  ( -16.80621392010912629, 66.05779742250453523, -149.2126994499415957 ) ) ;
#172288 = ORIENTED_EDGE ( 'NONE', *, *, #180711, .F. ) ;
#172287 = EDGE_CURVE ( 'NONE', #127248, #10248, #128856, .T. ) ;
#172290 = CARTESIAN_POINT ( 'NONE',  ( -16.81744102076749314, 9.950000000011142376, -180.1499999999999773 ) ) ;
#172289 = CARTESIAN_POINT ( 'NONE',  ( -23.25000000000000355, 70.35000000001210196, -127.2731074845243313 ) ) ;
#172291 = VERTEX_POINT ( 'NONE', #29782 ) ;
#172293 = ORIENTED_EDGE ( 'NONE', *, *, #25923, .F. ) ;
#172292 = DIRECTION ( 'NONE',  ( 0.000000000000000000, -0.2128009952263485993, 0.9770955615653341697 ) ) ;
#172294 = ORIENTED_EDGE ( 'NONE', *, *, #230732, .F. ) ;
#172295 = CARTESIAN_POINT ( 'NONE',  ( -16.89797118371580353, 9.976380722655672884, -146.5627066324414045 ) ) ;
#172296 = LINE ( 'NONE', #109689, #180051 ) ;
#172297 = LINE ( 'NONE', #34059, #234776 ) ;
#172298 = CIRCLE ( 'NONE', #51403, 0.6000000000000033085 ) ;
#172299 = CARTESIAN_POINT ( 'NONE',  ( 21.05000000000000071, 65.39167043205810614, -128.9314224712280179 ) ) ;
#172300 = ORIENTED_EDGE ( 'NONE', *, *, #78639, .T. ) ;
#172301 = LINE ( 'NONE', #32780, #47256 ) ;
#172302 = CARTESIAN_POINT ( 'NONE',  ( -18.50000000000000000, 64.25000000001246292, -181.7731074845244450 ) ) ;
#172303 = ADVANCED_FACE ( 'NONE', ( #109263 ), #10193, .T. ) ;
#172304 = VECTOR ( 'NONE', #22441, 1000.000000000000000 ) ;
#172305 = ORIENTED_EDGE ( 'NONE', *, *, #78191, .T. ) ;
#172306 = AXIS2_PLACEMENT_3D ( 'NONE', #105568, #207295, #3940 ) ;
#172307 = CIRCLE ( 'NONE', #51412, 0.1000000000000116629 ) ;
#172308 = ADVANCED_FACE ( 'NONE', ( #132706 ), #53154, .T. ) ;
#172309 = FACE_BOUND ( 'NONE', #122987, .T. ) ;
#172310 = AXIS2_PLACEMENT_3D ( 'NONE', #29197, #31752, #68285 ) ;
#172311 = CARTESIAN_POINT ( 'NONE',  ( -22.39999999999999858, 68.20922040163854660, -103.1231074845243540 ) ) ;
#172312 = ADVANCED_FACE ( 'NONE', ( #116983 ), #248625, .F. ) ;
#172313 = ORIENTED_EDGE ( 'NONE', *, *, #210642, .T. ) ;
#172314 = LINE ( 'NONE', #147563, #27026 ) ;
#172315 = VERTEX_POINT ( 'NONE', #96114 ) ;
#172316 = LINE ( 'NONE', #212687, #67279 ) ;
#172317 = VERTEX_POINT ( 'NONE', #12771 ) ;
#172318 = CARTESIAN_POINT ( 'NONE',  ( 23.14999999999998437, 7.128833340093095217, -233.7327013124392749 ) ) ;
#172319 = DIRECTION ( 'NONE',  ( 1.000000000000000000, 0.000000000000000000, 0.000000000000000000 ) ) ;
#172320 = PLANE ( 'NONE',  #180776 ) ;
#172321 = ADVANCED_FACE ( 'NONE', ( #135243 ), #93563, .T. ) ;
#172322 = PLANE ( 'NONE',  #249476 ) ;
#172323 = EDGE_CURVE ( 'NONE', #199385, #34439, #251345, .T. ) ;
#172324 = CIRCLE ( 'NONE', #218043, 0.1000000000000028644 ) ;
#172325 = CIRCLE ( 'NONE', #39022, 0.09999999999998898659 ) ;
#172326 = CARTESIAN_POINT ( 'NONE',  ( 20.94999999999999574, 1.249999999999999334, -8.000000000000000000 ) ) ;
#172327 = CARTESIAN_POINT ( 'NONE',  ( -21.64999999999999858, 7.249999999999992895, -21.25000000000000000 ) ) ;
#172328 = DIRECTION ( 'NONE',  ( 0.000000000000000000, 0.8814952561688320642, -0.4721928772777551075 ) ) ;
#172329 = AXIS2_PLACEMENT_3D ( 'NONE', #221599, #181242, #2564 ) ;
#172330 = VERTEX_POINT ( 'NONE', #36182 ) ;
#172331 = DIRECTION ( 'NONE',  ( 2.952720810173289112E-16, -1.000000000000000000, 0.000000000000000000 ) ) ;
#172332 = ORIENTED_EDGE ( 'NONE', *, *, #217294, .F. ) ;
#172335 = ORIENTED_EDGE ( 'NONE', *, *, #220919, .F. ) ;
#172334 = DIRECTION ( 'NONE',  ( 0.000000000000000000, -1.000000000000000000, 0.000000000000000000 ) ) ;
#172333 = DIRECTION ( 'NONE',  ( 1.387778780781405791E-13, 0.9999176327611370985, 0.01283462868040226822 ) ) ;
#172336 = ORIENTED_EDGE ( 'NONE', *, *, #178662, .F. ) ;
#172337 = DIRECTION ( 'NONE',  ( 1.000000000000000000, -0.000000000000000000, -0.000000000000000000 ) ) ;
#172338 = CARTESIAN_POINT ( 'NONE',  ( 20.94999999999999929, 65.70729864260985664, -64.06574559737245522 ) ) ;
